#172339 = AXIS2_PLACEMENT_3D ( 'NONE', #233506, #150121, #113537 ) ;
#172340 = DIRECTION ( 'NONE',  ( 1.000000000000000000, -0.000000000000000000, -0.000000000000000000 ) ) ;
#172341 = DIRECTION ( 'NONE',  ( -1.000000000000000000, 0.000000000000000000, 0.000000000000000000 ) ) ;
#172342 = AXIS2_PLACEMENT_3D ( 'NONE', #204774, #242622, #26169 ) ;
#172343 = ORIENTED_EDGE ( 'NONE', *, *, #73923, .T. ) ;
#172345 = ORIENTED_EDGE ( 'NONE', *, *, #60269, .T. ) ;
#172344 = CARTESIAN_POINT ( 'NONE',  ( -23.25000000000000000, 77.83585931145600512, -158.5186683157258187 ) ) ;
#172346 = AXIS2_PLACEMENT_3D ( 'NONE', #93611, #216114, #253949 ) ;
#172348 = DIRECTION ( 'NONE',  ( 0.000000000000000000, -0.1350103645451876944, 0.9908441862701601321 ) ) ;
#172347 = FACE_OUTER_BOUND ( 'NONE', #215733, .T. ) ;
#172350 = ORIENTED_EDGE ( 'NONE', *, *, #214625, .T. ) ;
#172349 = DIRECTION ( 'NONE',  ( 0.000000000000000000, 6.982962677686266711E-15, -1.000000000000000000 ) ) ;
#172351 = AXIS2_PLACEMENT_3D ( 'NONE', #103361, #64261, #61691 ) ;
#172352 = AXIS2_PLACEMENT_3D ( 'NONE', #238424, #257930, #220154 ) ;
#172353 = PRODUCT ( 'Snap Open Cable Crossbars 13', 'Snap Open Cable Crossbars 13', '', ( #71807 ) ) ;
#172354 = VERTEX_POINT ( 'NONE', #236925 ) ;
#172355 = AXIS2_PLACEMENT_3D ( 'NONE', #38921, #81840, #158879 ) ;
#172356 = CARTESIAN_POINT ( 'NONE',  ( 20.94999999999999929, 68.00366762990589109, -224.2307594727497815 ) ) ;
#172357 = CARTESIAN_POINT ( 'NONE',  ( 21.04999999999999716, 67.10527618163416719, -94.53602316137545358 ) ) ;
#172358 = ORIENTED_EDGE ( 'NONE', *, *, #188461, .F. ) ;
#172359 = SPHERICAL_SURFACE ( 'NONE', #30966, 0.1000000000000000056 ) ;
#172360 = ORIENTED_EDGE ( 'NONE', *, *, #226378, .F. ) ;
#172361 = DIRECTION ( 'NONE',  ( 0.000000000000000000, 0.4721928772777345129, 0.8814952561688430555 ) ) ;
#172362 = DIRECTION ( 'NONE',  ( 1.000000000000000000, 0.000000000000000000, 0.000000000000000000 ) ) ;
#172363 = AXIS2_PLACEMENT_3D ( 'NONE', #152629, #16950, #211288 ) ;
#172364 = ORIENTED_EDGE ( 'NONE', *, *, #113359, .F. ) ;
#172365 = DIRECTION ( 'NONE',  ( 0.000000000000000000, -0.9915357197604792727, 0.1298341882520473722 ) ) ;
#172366 = CIRCLE ( 'NONE', #205611, 1.900000000000012790 ) ;
#172367 = EDGE_CURVE ( 'NONE', #5245, #196258, #133966, .T. ) ;
#172368 = CARTESIAN_POINT ( 'NONE',  ( -20.65000000000000568, 7.250000000011138646, -46.15000000000000568 ) ) ;
#172369 = AXIS2_PLACEMENT_3D ( 'NONE', #64588, #45035, #226199 ) ;
#172370 = ORIENTED_EDGE ( 'NONE', *, *, #153929, .F. ) ;
#172371 = ORIENTED_EDGE ( 'NONE', *, *, #205890, .T. ) ;
#172372 = CARTESIAN_POINT ( 'NONE',  ( 20.53930447207944354, 18.80980900407904599, -229.8058790690892010 ) ) ;
#172373 = ORIENTED_EDGE ( 'NONE', *, *, #163812, .F. ) ;
#172374 = DIRECTION ( 'NONE',  ( 1.000000000000000000, 0.000000000000000000, 0.000000000000000000 ) ) ;
#172376 = EDGE_CURVE ( 'NONE', #44715, #221017, #136522, .T. ) ;
#172375 = ORIENTED_EDGE ( 'NONE', *, *, #168149, .T. ) ;
#172378 = ORIENTED_EDGE ( 'NONE', *, *, #29266, .T. ) ;
#172377 = DIRECTION ( 'NONE',  ( 0.000000000000000000, -0.8700118002898359348, 0.4930308989875165082 ) ) ;
#172379 = ORIENTED_EDGE ( 'NONE', *, *, #140521, .F. ) ;
#172380 = ADVANCED_FACE ( 'NONE', ( #74040 ), #115349, .T. ) ;
#172381 = DIRECTION ( 'NONE',  ( 0.000000000000000000, 0.000000000000000000, 1.000000000000000000 ) ) ;
#172382 = ADVANCED_FACE ( 'NONE', ( #16616 ), #256954, .T. ) ;
#172383 = EDGE_LOOP ( 'NONE', ( #49237, #222006, #53394, #171688 ) ) ;
#172386 = VERTEX_POINT ( 'NONE', #14048 ) ;
#172385 = EDGE_LOOP ( 'NONE', ( #113952, #226325, #183930, #13272, #231283, #205450, #22290, #206003, #151842, #215005, #10987 ) ) ;
#172384 = DIRECTION ( 'NONE',  ( 0.7071067811865475727, -0.7071067811865475727, -5.142139384388981164E-15 ) ) ;
#172388 = ORIENTED_EDGE ( 'NONE', *, *, #192555, .F. ) ;
#172387 = CIRCLE ( 'NONE', #59885, 0.1999999999999987899 ) ;
#172389 = AXIS2_PLACEMENT_3D ( 'NONE', #91781, #209148, #30544 ) ;
#172390 = CIRCLE ( 'NONE', #151520, 0.09999999999999939493 ) ;
#172391 = CIRCLE ( 'NONE', #93216, 4.000000000000003553 ) ;
#172392 = DIRECTION ( 'NONE',  ( 2.952720810173289112E-16, -1.000000000000000000, 0.000000000000000000 ) ) ;
#172393 = ORIENTED_EDGE ( 'NONE', *, *, #25148, .T. ) ;
#172394 = ADVANCED_FACE ( 'NONE', ( #173158 ), #123747, .F. ) ;
#172395 = CARTESIAN_POINT ( 'NONE',  ( -16.93860193097148326, 9.993107767340401182, -154.9001383673068801 ) ) ;
#172397 = ORIENTED_EDGE ( 'NONE', *, *, #8599, .T. ) ;
#172396 = DIRECTION ( 'NONE',  ( 1.000000000000000000, 0.000000000000000000, 0.000000000000000000 ) ) ;
#172398 = LINE ( 'NONE', #173691, #208963 ) ;
#172399 = ORIENTED_EDGE ( 'NONE', *, *, #202443, .F. ) ;
#172400 = ORIENTED_EDGE ( 'NONE', *, *, #35913, .F. ) ;
#172401 = DIRECTION ( 'NONE',  ( -1.000000000000000000, 0.000000000000000000, 0.000000000000000000 ) ) ;
#172402 = CARTESIAN_POINT ( 'NONE',  ( 20.12500000000000355, 66.74195072709427734, -61.15976864738194507 ) ) ;
#172403 = VERTEX_POINT ( 'NONE', #97378 ) ;
#172405 = ORIENTED_EDGE ( 'NONE', *, *, #73337, .T. ) ;
#172404 = CARTESIAN_POINT ( 'NONE',  ( 21.05000000000000071, 40.68212387350988735, -238.0221676322813096 ) ) ;
#172406 = CARTESIAN_POINT ( 'NONE',  ( -23.15000000000000213, 11.65000000001115588, -193.9851942293460070 ) ) ;
#172408 = ORIENTED_EDGE ( 'NONE', *, *, #138632, .F. ) ;
#172407 = ORIENTED_EDGE ( 'NONE', *, *, #183283, .T. ) ;
#172409 = AXIS2_PLACEMENT_3D ( 'NONE', #71581, #6440, #85951 ) ;
#172410 = EDGE_LOOP ( 'NONE', ( #252859, #194089, #164678, #19111 ) ) ;
#172411 = DIRECTION ( 'NONE',  ( 1.000000000000000000, 0.000000000000000000, 0.000000000000000000 ) ) ;
#172413 = EDGE_LOOP ( 'NONE', ( #145543, #91311, #191367, #139950 ) ) ;
#172412 = EDGE_CURVE ( 'NONE', #29232, #12856, #44630, .T. ) ;
#172414 = VERTEX_POINT ( 'NONE', #233105 ) ;
#172415 = EDGE_CURVE ( 'NONE', #197986, #36418, #61197, .T. ) ;
#172416 = DIRECTION ( 'NONE',  ( -0.000000000000000000, 0.1350103645451807555, 0.9908441862701610203 ) ) ;
#172417 = EDGE_LOOP ( 'NONE', ( #102168, #195300, #587, #115904 ) ) ;
#172418 = DIRECTION ( 'NONE',  ( 0.000000000000000000, 8.267618268485201230E-15, -1.000000000000000000 ) ) ;
#172419 = DIRECTION ( 'NONE',  ( -3.265361837132813093E-16, 1.000000000000000000, 0.000000000000000000 ) ) ;
#172420 = ORIENTED_EDGE ( 'NONE', *, *, #185625, .F. ) ;
#172422 = ADVANCED_FACE ( 'NONE', ( #114417 ), #156140, .T. ) ;
#172421 = VERTEX_POINT ( 'NONE', #34915 ) ;
#172423 = DIRECTION ( 'NONE',  ( -2.952720810173288619E-16, 1.000000000000000000, 0.000000000000000000 ) ) ;
#172424 = AXIS2_PLACEMENT_3D ( 'NONE', #251840, #108483, #227137 ) ;
#172425 = ORIENTED_EDGE ( 'NONE', *, *, #62259, .T. ) ;
#172426 = AXIS2_PLACEMENT_3D ( 'NONE', #225638, #168314, #47007 ) ;
#172427 = DIRECTION ( 'NONE',  ( 0.000000000000000000, -0.8660254037844411501, -0.4999999999999956701 ) ) ;
#172428 = ORIENTED_EDGE ( 'NONE', *, *, #233841, .T. ) ;
#172429 = VERTEX_POINT ( 'NONE', #111855 ) ;
#172430 = CARTESIAN_POINT ( 'NONE',  ( -20.94999999999999929, 77.36242903720467723, -28.13422623660311217 ) ) ;
#172432 = ORIENTED_EDGE ( 'NONE', *, *, #91685, .T. ) ;
#172431 = CARTESIAN_POINT ( 'NONE',  ( 18.50000000000000000, 85.40000000001231228, -162.7258477248610120 ) ) ;
#172433 = CARTESIAN_POINT ( 'NONE',  ( 23.25000000000000000, -6.688413578037176066, -212.5825622730469036 ) ) ;
#172434 = CARTESIAN_POINT ( 'NONE',  ( 21.30000000000002558, 1.115600667400684642E-11, -167.4999999999999716 ) ) ;
#172435 = DIRECTION ( 'NONE',  ( -1.000000000000000000, 0.000000000000000000, 0.000000000000000000 ) ) ;
#172436 = CARTESIAN_POINT ( 'NONE',  ( -21.05000000000000071, 76.00000000001253397, -181.8231074845243711 ) ) ;
#172437 = DIRECTION ( 'NONE',  ( 1.284434275755705296E-16, -0.7071067811865471286, -0.7071067811865479058 ) ) ;
#172438 = LINE ( 'NONE', #52428, #69184 ) ;
#172439 = DIRECTION ( 'NONE',  ( 0.000000000000000000, 6.982962677686266711E-15, -1.000000000000000000 ) ) ;
#172440 = CARTESIAN_POINT ( 'NONE',  ( -21.14999999999999858, 11.65000000001115588, -140.7838656629781724 ) ) ;
#172441 = CARTESIAN_POINT ( 'NONE',  ( 18.39999999999999858, 38.27493434228539826, -261.1939574891503639 ) ) ;
#172442 = TOROIDAL_SURFACE ( 'NONE', #209819, 2.100000000000002309, 0.1000000000000000056 ) ;
#172443 = CARTESIAN_POINT ( 'NONE',  ( -18.40000000000000213, 33.92901942162173157, -235.0579290632217067 ) ) ;
#172444 = CARTESIAN_POINT ( 'NONE',  ( -23.25000000000000000, -1.835859311443637010, -45.00443916879852679 ) ) ;
#172445 = ORIENTED_EDGE ( 'NONE', *, *, #157210, .T. ) ;
#172446 = VECTOR ( 'NONE', #11293, 1000.000000000000000 ) ;
#172447 = CIRCLE ( 'NONE', #64069, 12.97500000000000320 ) ;
#172448 = EDGE_CURVE ( 'NONE', #174523, #190881, #77355, .T. ) ;
#172450 = ORIENTED_EDGE ( 'NONE', *, *, #6282, .T. ) ;
#172449 = ORIENTED_EDGE ( 'NONE', *, *, #227211, .F. ) ;
#172452 = ORIENTED_EDGE ( 'NONE', *, *, #147724, .T. ) ;
#172451 = EDGE_CURVE ( 'NONE', #217355, #161618, #125642, .T. ) ;
#172453 = DIRECTION ( 'NONE',  ( 0.000000000000000000, 0.000000000000000000, -1.000000000000000000 ) ) ;
#172454 = FACE_OUTER_BOUND ( 'NONE', #38515, .T. ) ;
#172455 = EDGE_CURVE ( 'NONE', #252694, #137777, #157065, .T. ) ;
#172456 = EDGE_CURVE ( 'NONE', #86769, #228950, #79114, .T. ) ;
#172458 = DIRECTION ( 'NONE',  ( -1.000000000000000000, 0.000000000000000000, 0.000000000000000000 ) ) ;
#172457 = PLANE ( 'NONE',  #182628 ) ;
#172459 = ORIENTED_EDGE ( 'NONE', *, *, #167949, .F. ) ;
#172460 = ORIENTED_EDGE ( 'NONE', *, *, #12626, .F. ) ;
#172461 = CIRCLE ( 'NONE', #55668, 0.09999999999999892308 ) ;
#172463 = AXIS2_PLACEMENT_3D ( 'NONE', #161026, #1916, #237969 ) ;
#172462 =( LENGTH_UNIT ( ) NAMED_UNIT ( * ) SI_UNIT ( .MILLI., .METRE. ) );
#172465 = CIRCLE ( 'NONE', #109858, 11.75000000000001066 ) ;
#172464 = CARTESIAN_POINT ( 'NONE',  ( 20.97239005616515328, 67.12515615866146845, -57.27295468237120701 ) ) ;
#172466 = ADVANCED_FACE ( 'NONE', ( #199087 ), #110698, .T. ) ;
#172467 = CARTESIAN_POINT ( 'NONE',  ( -20.05000000000000426, 66.75000000001185185, -90.67310748452436542 ) ) ;
#172469 = EDGE_LOOP ( 'NONE', ( #147840, #149538, #77541, #165957 ) ) ;
#172468 = AXIS2_PLACEMENT_3D ( 'NONE', #103321, #21268, #142457 ) ;
#172470 = ORIENTED_EDGE ( 'NONE', *, *, #153062, .F. ) ;
#172471 = EDGE_CURVE ( 'NONE', #38015, #169538, #102281, .T. ) ;
#172472 = LINE ( 'NONE', #94158, #146604 ) ;
#172474 = EDGE_CURVE ( 'NONE', #208598, #101037, #120865, .T. ) ;
#172473 = EDGE_CURVE ( 'NONE', #229500, #231654, #57065, .T. ) ;
#172475 = CARTESIAN_POINT ( 'NONE',  ( -33.72168855820451938, 9.950000000011156587, -146.6499999999999773 ) ) ;
#172476 = CIRCLE ( 'NONE', #80828, 11.65000000000000391 ) ;
#172477 = DIRECTION ( 'NONE',  ( 1.000000000000000000, -0.000000000000000000, -0.000000000000000000 ) ) ;
#172479 = VERTEX_POINT ( 'NONE', #257713 ) ;
#172478 = LINE ( 'NONE', #192014, #168800 ) ;
#172480 = EDGE_CURVE ( 'NONE', #155936, #97513, #2912, .T. ) ;
#172481 = DIRECTION ( 'NONE',  ( -0.000000000000000000, -0.000000000000000000, -1.000000000000000000 ) ) ;
#172482 = DIRECTION ( 'NONE',  ( 0.7071067811865463515, 0.7071067811865487940, 4.937700262164540154E-15 ) ) ;
#172483 = VECTOR ( 'NONE', #93732, 1000.000000000000000 ) ;
#172484 = CARTESIAN_POINT ( 'NONE',  ( 18.40000000000000568, 85.50000000001192291, -96.02374538734412113 ) ) ;
#172486 = ORIENTED_EDGE ( 'NONE', *, *, #246273, .T. ) ;
#172485 = AXIS2_PLACEMENT_3D ( 'NONE', #246648, #88845, #129285 ) ;
#172487 = CARTESIAN_POINT ( 'NONE',  ( 15.69410316191959254, 66.64325398293360081, -85.81974776316017994 ) ) ;
#172488 = DIRECTION ( 'NONE',  ( 0.000000000000000000, -1.000000000000000000, -7.105427357601001859E-15 ) ) ;
#172489 = DIRECTION ( 'NONE',  ( -0.000000000000000000, 0.000000000000000000, -1.000000000000000000 ) ) ;
#172490 = CIRCLE ( 'NONE', #18316, 3.900000000000000799 ) ;
#172491 = EDGE_CURVE ( 'NONE', #147024, #220397, #190399, .T. ) ;
#172493 = CARTESIAN_POINT ( 'NONE',  ( 18.79999999999999716, 0.000000000000000000, 0.000000000000000000 ) ) ;
#172492 = CARTESIAN_POINT ( 'NONE',  ( -16.87331047859649757, 66.05000000001255955, -182.6731074845244223 ) ) ;
#172494 = CYLINDRICAL_SURFACE ( 'NONE', #62220, 0.1000000000000028644 ) ;
#172495 = DIRECTION ( 'NONE',  ( 0.000000000000000000, -0.1332476588733448597, -0.9910827722268067408 ) ) ;
#172496 = FACE_OUTER_BOUND ( 'NONE', #71422, .T. ) ;
#172497 = CARTESIAN_POINT ( 'NONE',  ( 18.58719872626880942, 85.56664439761105712, -163.2006292881272884 ) ) ;
#172498 = CARTESIAN_POINT ( 'NONE',  ( -21.09610168723073542, 69.62104428478737361, -136.5566969914158051 ) ) ;
#172499 = EDGE_CURVE ( 'NONE', #223845, #109477, #66951, .T. ) ;
#172500 = ADVANCED_FACE ( 'NONE', ( #60844 ), #223668, .T. ) ;
#172501 = EDGE_LOOP ( 'NONE', ( #235523, #190362, #10645, #55775 ) ) ;
#172502 = ORIENTED_EDGE ( 'NONE', *, *, #158908, .T. ) ;
#172503 = EDGE_LOOP ( 'NONE', ( #60402, #92733, #14643, #166578 ) ) ;
#172504 = ADVANCED_FACE ( 'NONE', ( #47371 ), #41324, .F. ) ;
#172505 = DIRECTION ( 'NONE',  ( -1.000000000000000000, 0.000000000000000000, 0.000000000000000000 ) ) ;
#172506 = CARTESIAN_POINT ( 'NONE',  ( -23.49999999999994316, 77.85126707825561709, -47.62635315998165453 ) ) ;
#172507 = ORIENTED_EDGE ( 'NONE', *, *, #248824, .F. ) ;
#172508 = DIRECTION ( 'NONE',  ( -0.000000000000000000, 0.000000000000000000, 1.000000000000000000 ) ) ;
#172509 = EDGE_CURVE ( 'NONE', #176334, #89225, #135630, .T. ) ;
#172510 = ORIENTED_EDGE ( 'NONE', *, *, #148500, .F. ) ;
#172511 = AXIS2_PLACEMENT_3D ( 'NONE', #113740, #132022, #96717 ) ;
#172512 =( LENGTH_UNIT ( ) NAMED_UNIT ( * ) SI_UNIT ( .MILLI., .METRE. ) );
#172513 = ADVANCED_FACE ( 'NONE', ( #85193 ), #65663, .F. ) ;
#172514 = VECTOR ( 'NONE', #137610, 1000.000000000000000 ) ;
#172515 = VERTEX_POINT ( 'NONE', #145193 ) ;
#172516 = AXIS2_PLACEMENT_3D ( 'NONE', #73828, #232897, #133761 ) ;
#172517 = CARTESIAN_POINT ( 'NONE',  ( 21.05000000000000071, 76.08559286337390404, -109.4367702193939351 ) ) ;
#172518 = ORIENTED_EDGE ( 'NONE', *, *, #194129, .T. ) ;
#172519 = CARTESIAN_POINT ( 'NONE',  ( -16.83794479845802172, 30.05980643715662382, -234.7553781105508790 ) ) ;
#172520 = LINE ( 'NONE', #232463, #56852 ) ;
#172521 = CIRCLE ( 'NONE', #14269, 0.1999999999999987899 ) ;
#172522 = CARTESIAN_POINT ( 'NONE',  ( -18.79999999999999716, 4.513204987021263825, 22.10000000000000142 ) ) ;
#172523 = DIRECTION ( 'NONE',  ( 0.000000000000000000, -0.9915357197604971473, 0.1298341882519111479 ) ) ;
#172525 = ORIENTED_EDGE ( 'NONE', *, *, #15667, .F. ) ;
#172524 = CARTESIAN_POINT ( 'NONE',  ( -16.88705144915422096, 29.95864726180315429, -234.6743689137096567 ) ) ;
#172527 = CYLINDRICAL_SURFACE ( 'NONE', #254339, 0.09999999999999939493 ) ;
#172526 = CARTESIAN_POINT ( 'NONE',  ( 21.05000000000000071, 6.164605728109038729, -199.6790125993524043 ) ) ;
#172528 = ADVANCED_FACE ( 'NONE', ( #224728 ), #140271, .F. ) ;
#172529 = CARTESIAN_POINT ( 'NONE',  ( -16.91049119928363709, 9.949999999999985079, -20.88172039319084305 ) ) ;
#172530 = DIRECTION ( 'NONE',  ( 0.000000000000000000, 0.000000000000000000, -1.000000000000000000 ) ) ;
#172531 = VECTOR ( 'NONE', #194992, 1000.000000000000000 ) ;
#172532 = CARTESIAN_POINT ( 'NONE',  ( -16.97683809663753607, 66.05000000001183480, -82.79463665241381420 ) ) ;
#172533 = DIRECTION ( 'NONE',  ( 1.000000000000000000, 0.000000000000000000, 0.000000000000000000 ) ) ;
#172534 = EDGE_LOOP ( 'NONE', ( #108152, #244705, #65010, #209455 ) ) ;
#172535 = AXIS2_PLACEMENT_3D ( 'NONE', #139487, #5090, #224164 ) ;
#172536 = DIRECTION ( 'NONE',  ( -1.000000000000000000, -0.000000000000000000, -0.000000000000000000 ) ) ;
#172537 = CIRCLE ( 'NONE', #93360, 0.09999999999999414912 ) ;
#172538 = ORIENTED_EDGE ( 'NONE', *, *, #254464, .F. ) ;
#172539 = DIRECTION ( 'NONE',  ( 0.000000000000000000, 0.9126074666063770380, 0.4088369013363281068 ) ) ;
#172540 = ORIENTED_EDGE ( 'NONE', *, *, #160963, .F. ) ;
#172541 = TOROIDAL_SURFACE ( 'NONE', #26761, 0.2000000000000000111, 0.1000000000000000056 ) ;
#172542 = CARTESIAN_POINT ( 'NONE',  ( 21.72449340488910607, 65.71604372252076587, -93.77310748452438816 ) ) ;
#172543 = CARTESIAN_POINT ( 'NONE',  ( 21.05000000000000071, 1.115600667400684642E-11, -33.50000000000000000 ) ) ;
#172544 = CARTESIAN_POINT ( 'NONE',  ( -18.59999999999999787, 11.65000000001115232, -174.5148057706539930 ) ) ;
#172545 = VERTEX_POINT ( 'NONE', #225990 ) ;
#172546 = VECTOR ( 'NONE', #140730, 1000.000000000000000 ) ;
#172547 = ORIENTED_EDGE ( 'NONE', *, *, #46742, .F. ) ;
#172548 = CARTESIAN_POINT ( 'NONE',  ( -21.05000000000000071, 69.60000000001230092, -160.0926828544628222 ) ) ;
#172550 = CIRCLE ( 'NONE', #43506, 12.87500000000000178 ) ;
#172549 = CARTESIAN_POINT ( 'NONE',  ( 23.14999999999999858, 1.115600667400684642E-11, -171.5000000000000284 ) ) ;
#172551 = EDGE_CURVE ( 'NONE', #54944, #110818, #94495, .T. ) ;
#172552 = DIRECTION ( 'NONE',  ( -1.000000000000000000, 0.000000000000000000, 0.000000000000000000 ) ) ;
#172553 = DIRECTION ( 'NONE',  ( 1.000000000000000000, 1.875376730785737719E-16, 0.000000000000000000 ) ) ;
#172554 = LINE ( 'NONE', #152974, #150048 ) ;
#172555 = DIRECTION ( 'NONE',  ( 1.186688945009009831E-16, -1.000000000000000000, 0.000000000000000000 ) ) ;
#172556 = ADVANCED_FACE ( 'NONE', ( #167369 ), #58271, .F. ) ;
#172557 = CARTESIAN_POINT ( 'NONE',  ( 21.14999999999999858, 65.28660755661196902, -90.77310748452438816 ) ) ;
#172558 = CARTESIAN_POINT ( 'NONE',  ( -18.50000000000000000, 64.35000000001245724, -170.0231074845244166 ) ) ;
#172559 = ORIENTED_EDGE ( 'NONE', *, *, #18403, .T. ) ;
#172560 = CIRCLE ( 'NONE', #226662, 0.1000000000000028644 ) ;
#172562 = VERTEX_POINT ( 'NONE', #13413 ) ;
#172561 = CARTESIAN_POINT ( 'NONE',  ( -23.25000000000000000, 4.150000000011156764, -79.35000000000005116 ) ) ;
#172563 = VECTOR ( 'NONE', #30470, 1000.000000000000000 ) ;
#172564 = CARTESIAN_POINT ( 'NONE',  ( 17.74533788810829904, 10.81849979148194763, -190.6863773250524048 ) ) ;
#172565 = DIRECTION ( 'NONE',  ( 0.000000000000000000, -0.6728971962617102953, -0.7397360091702507301 ) ) ;
#172567 = CARTESIAN_POINT ( 'NONE',  ( -18.59999999999999787, -0.7124800764063081715, -242.4837965912295772 ) ) ;
#172566 = FACE_OUTER_BOUND ( 'NONE', #38724, .T. ) ;
#172568 = EDGE_CURVE ( 'NONE', #133901, #153430, #194491, .T. ) ;
#172569 = ADVANCED_FACE ( 'NONE', ( #112514 ), #182001, .T. ) ;
#172570 = DIRECTION ( 'NONE',  ( 2.465190328815662439E-32, -0.2617529984165030132, -0.9651348961777158619 ) ) ;
#172572 = EDGE_LOOP ( 'NONE', ( #137647, #105307, #51598, #21095, #62879, #96229, #145063, #175360, #43139 ) ) ;
#172571 = DIRECTION ( 'NONE',  ( 0.000000000000000000, 1.000000000000000000, 1.156482317317864980E-14 ) ) ;
#172573 = DIRECTION ( 'NONE',  ( -0.000000000000000000, -0.000000000000000000, -1.000000000000000000 ) ) ;
#172574 = FACE_OUTER_BOUND ( 'NONE', #170394, .T. ) ;
#172575 = FACE_OUTER_BOUND ( 'NONE', #142491, .T. ) ;
#172576 = DIRECTION ( 'NONE',  ( -0.000000000000000000, 0.000000000000000000, -1.000000000000000000 ) ) ;
#172577 = CARTESIAN_POINT ( 'NONE',  ( 20.85000000000000142, 6.933893972137497030, -137.7856458343736108 ) ) ;
#172578 = ORIENTED_EDGE ( 'NONE', *, *, #220377, .T. ) ;
#172579 = FACE_OUTER_BOUND ( 'NONE', #60487, .T. ) ;
#172580 = EDGE_LOOP ( 'NONE', ( #97975, #217948, #171463, #41268 ) ) ;
#172581 = DIRECTION ( 'NONE',  ( 0.000000000000000000, -0.000000000000000000, 1.000000000000000000 ) ) ;
#172582 = ORIENTED_EDGE ( 'NONE', *, *, #127990, .T. ) ;
#172583 = DIRECTION ( 'NONE',  ( 8.565286242868724116E-15, -0.1575546449569727447, 0.9875102702516478370 ) ) ;
#172584 = CIRCLE ( 'NONE', #118367, 12.87499999999999112 ) ;
#172585 = VECTOR ( 'NONE', #249373, 1000.000000000000000 ) ;
#172586 = ORIENTED_EDGE ( 'NONE', *, *, #202590, .F. ) ;
#172587 = EDGE_CURVE ( 'NONE', #121176, #62147, #128220, .T. ) ;
#172588 = DIRECTION ( 'NONE',  ( 0.000000000000000000, -1.000000000000000000, 0.000000000000000000 ) ) ;
#172589 = DIRECTION ( 'NONE',  ( 0.000000000000000000, 0.2617529984165021806, 0.9651348961777159730 ) ) ;
#172590 = CARTESIAN_POINT ( 'NONE',  ( 21.14999999999999503, 64.35000000001237197, -170.0231074845244166 ) ) ;
#172591 = ORIENTED_EDGE ( 'NONE', *, *, #18668, .F. ) ;
#172592 = CARTESIAN_POINT ( 'NONE',  ( -23.15000000000000213, -11.64999999998884483, -164.4000000000000057 ) ) ;
#172593 = DIRECTION ( 'NONE',  ( -1.000000000000000000, -3.265361837132813093E-16, 0.000000000000000000 ) ) ;
#172594 = CARTESIAN_POINT ( 'NONE',  ( -20.94999999999999929, -1.162701749926853712, -142.1000000000000227 ) ) ;
#172595 = CARTESIAN_POINT ( 'NONE',  ( -21.05000000000000071, 47.95459712139159336, -246.5019368548292675 ) ) ;
#172596 = CARTESIAN_POINT ( 'NONE',  ( -18.59999999999999787, 74.16465844978715438, -57.96795619196135618 ) ) ;
#172598 = EDGE_LOOP ( 'NONE', ( #238925, #234227, #250246, #124259 ) ) ;
#172597 = EDGE_CURVE ( 'NONE', #50827, #256542, #215310, .T. ) ;
#172599 = CARTESIAN_POINT ( 'NONE',  ( -18.52309608778507766, 85.64247632006726008, -129.8085111433545649 ) ) ;
#172600 = VERTEX_POINT ( 'NONE', #190790 ) ;
#172602 = ORIENTED_EDGE ( 'NONE', *, *, #245579, .F. ) ;
#172601 = CARTESIAN_POINT ( 'NONE',  ( 21.04999999999908411, 67.22371710472118878, -90.86519848187187165 ) ) ;
#172603 = ORIENTED_EDGE ( 'NONE', *, *, #3886, .T. ) ;
#172604 = PRESENTATION_LAYER_ASSIGNMENT (  '', '', ( #255886 ) ) ;
#172605 = DIRECTION ( 'NONE',  ( 1.000000000000000000, 2.952720810173289112E-16, -0.000000000000000000 ) ) ;
#172606 = DIRECTION ( 'NONE',  ( 0.000000000000000000, -0.4166553800442105437, 0.9090645160164456673 ) ) ;
#172607 = DIRECTION ( 'NONE',  ( 0.000000000000000000, -1.000000000000000000, 0.000000000000000000 ) ) ;
#172608 = DIRECTION ( 'NONE',  ( 0.000000000000000000, -6.938893903907222067E-15, 1.000000000000000000 ) ) ;
#172609 = EDGE_LOOP ( 'NONE', ( #132291, #133123, #31979, #127009 ) ) ;
#172610 = CARTESIAN_POINT ( 'NONE',  ( -21.05000000000000071, 14.05000000001115623, -139.5136950707610026 ) ) ;
#172611 = DIRECTION ( 'NONE',  ( 0.000000000000000000, -1.000000000000000000, 0.000000000000000000 ) ) ;
#172612 = EDGE_CURVE ( 'NONE', #168680, #93005, #136163, .T. ) ;
#172613 = ORIENTED_EDGE ( 'NONE', *, *, #59113, .T. ) ;
#172615 = VERTEX_POINT ( 'NONE', #68242 ) ;
#172614 = CARTESIAN_POINT ( 'NONE',  ( -16.94878442675511465, 66.00827089702099215, -115.6348879088864976 ) ) ;
#172617 = ADVANCED_FACE ( 'NONE', ( #231189 ), #252325, .F. ) ;
#172616 = CARTESIAN_POINT ( 'NONE',  ( -22.47071067811865319, 36.65892442174472876, -249.5511627012454596 ) ) ;
#172618 = LINE ( 'NONE', #154337, #23238 ) ;
#172620 = VECTOR ( 'NONE', #95025, 999.9999999999998863 ) ;
#172619 = CARTESIAN_POINT ( 'NONE',  ( 21.13461538461538325, 44.29694026544699170, -236.3931290369747842 ) ) ;
#172621 = ORIENTED_EDGE ( 'NONE', *, *, #192225, .T. ) ;
#172622 = VECTOR ( 'NONE', #123488, 1000.000000000000000 ) ;
#172623 = ORIENTED_EDGE ( 'NONE', *, *, #194139, .T. ) ;
#172624 = VECTOR ( 'NONE', #22045, 1000.000000000000000 ) ;
#172626 = DIRECTION ( 'NONE',  ( 1.836970198721029934E-16, 1.000000000000000000, 6.982962677686266711E-15 ) ) ;
#172625 = CIRCLE ( 'NONE', #60120, 0.09999999999999867328 ) ;
#172627 = EDGE_CURVE ( 'NONE', #254024, #111950, #2535, .T. ) ;
#172628 = DIRECTION ( 'NONE',  ( -1.000000000000000000, -0.000000000000000000, -0.000000000000000000 ) ) ;
#172629 = VERTEX_POINT ( 'NONE', #171242 ) ;
#172630 = DIRECTION ( 'NONE',  ( -1.000000000000000000, 0.000000000000000000, -0.000000000000000000 ) ) ;
#172631 = EDGE_CURVE ( 'NONE', #248447, #79198, #106573, .T. ) ;
#172632 = PLANE ( 'NONE',  #193078 ) ;
#172633 = ADVANCED_FACE ( 'NONE', ( #94208 ), #10840, .F. ) ;
#172634 = DIRECTION ( 'NONE',  ( 0.000000000000000000, 0.9229812358755983270, -0.3848449534832869001 ) ) ;
#172635 = AXIS2_PLACEMENT_3D ( 'NONE', #221943, #43347, #6776 ) ;
#172636 = EDGE_CURVE ( 'NONE', #119280, #55681, #25948, .T. ) ;
#172637 = VECTOR ( 'NONE', #100203, 1000.000000000000000 ) ;
#172638 = AXIS2_PLACEMENT_3D ( 'NONE', #108478, #168503, #69370 ) ;
#172639 = VERTEX_POINT ( 'NONE', #18540 ) ;
#172640 = CARTESIAN_POINT ( 'NONE',  ( 20.94999999999999929, 67.07338541492450190, -61.05142446530125966 ) ) ;
#172641 = AXIS2_PLACEMENT_3D ( 'NONE', #64886, #80576, #160176 ) ;
#172642 = AXIS2_PLACEMENT_3D ( 'NONE', #22450, #60259, #104500 ) ;
#172643 = ORIENTED_EDGE ( 'NONE', *, *, #88736, .T. ) ;
#172644 = CARTESIAN_POINT ( 'NONE',  ( 21.00000000000000000, 9.750000000011153745, -112.8500000000000369 ) ) ;
#172646 = EDGE_CURVE ( 'NONE', #11036, #62328, #185719, .T. ) ;
#172645 = CARTESIAN_POINT ( 'NONE',  ( 22.39999999999999503, 11.75000000001115552, -167.3999999999999773 ) ) ;
#172648 = ORIENTED_EDGE ( 'NONE', *, *, #168424, .T. ) ;
#172647 = CARTESIAN_POINT ( 'NONE',  ( -18.59999999999999787, 22.43030315632513094, -231.3223027016406093 ) ) ;
#172649 = CARTESIAN_POINT ( 'NONE',  ( 23.14999999999999503, 60.99662849158838895, -205.1669373764474642 ) ) ;
#172650 = LINE ( 'NONE', #34396, #119982 ) ;
#172651 = CARTESIAN_POINT ( 'NONE',  ( -18.59999999999999787, 77.83585931145546510, -91.41866831572575336 ) ) ;
#172652 = DIRECTION ( 'NONE',  ( 0.000000000000000000, 0.000000000000000000, 1.000000000000000000 ) ) ;
#172653 = CARTESIAN_POINT ( 'NONE',  ( 21.05000000000000071, 6.413978881499668994, -33.58579911627400350 ) ) ;
#172654 = VECTOR ( 'NONE', #198723, 1000.000000000000000 ) ;
#172655 = FACE_OUTER_BOUND ( 'NONE', #122001, .T. ) ;
#172656 = AXIS2_PLACEMENT_3D ( 'NONE', #236045, #216481, #101634 ) ;
#172657 = DIRECTION ( 'NONE',  ( 0.000000000000000000, -1.299197156476247485E-14, 1.000000000000000000 ) ) ;
#172659 = ORIENTED_EDGE ( 'NONE', *, *, #188829, .F. ) ;
#172658 = CARTESIAN_POINT ( 'NONE',  ( -22.49917693094574389, 75.91477003579036875, -114.6729032690549701 ) ) ;
#172660 = AXIS2_PLACEMENT_3D ( 'NONE', #232888, #114194, #29559 ) ;
#172661 = DIRECTION ( 'NONE',  ( -1.000000000000000000, 0.000000000000000000, 0.000000000000000000 ) ) ;
#172662 = AXIS2_PLACEMENT_3D ( 'NONE', #44031, #122287, #81829 ) ;
#172663 = CARTESIAN_POINT ( 'NONE',  ( -18.38817693311004575, 16.37893853458640692, -222.2512945466943108 ) ) ;
#172664 = CARTESIAN_POINT ( 'NONE',  ( 21.14999999999999858, 11.65000000001116298, -88.75000000000004263 ) ) ;
#172665 = TOROIDAL_SURFACE ( 'NONE', #51787, 11.65000000000000036, 0.1000000000000000056 ) ;
#172667 = ORIENTED_EDGE ( 'NONE', *, *, #33000, .F. ) ;
#172666 = AXIS2_PLACEMENT_3D ( 'NONE', #23489, #3889, #224207 ) ;
#172668 = DIRECTION ( 'NONE',  ( 0.000000000000000000, 0.000000000000000000, -1.000000000000000000 ) ) ;
#172669 = CIRCLE ( 'NONE', #192905, 0.1000000000000028644 ) ;
#172670 = DIRECTION ( 'NONE',  ( 1.000000000000000000, 0.000000000000000000, -0.000000000000000000 ) ) ;
#172671 = SPHERICAL_SURFACE ( 'NONE', #40989, 0.1000000000000000056 ) ;
#172672 = ORIENTED_EDGE ( 'NONE', *, *, #75887, .T. ) ;
#172673 = FACE_OUTER_BOUND ( 'NONE', #197475, .T. ) ;
#172674 = CARTESIAN_POINT ( 'NONE',  ( -22.47071067811866385, 59.75442326890419764, -233.9300113800878762 ) ) ;
#172675 = VERTEX_POINT ( 'NONE', #237589 ) ;
#172676 = DIRECTION ( 'NONE',  ( -1.000000000000000000, 0.000000000000000000, -0.000000000000000000 ) ) ;
#172677 = ORIENTED_EDGE ( 'NONE', *, *, #245411, .F. ) ;
#172679 = EDGE_CURVE ( 'NONE', #220385, #22057, #160795, .T. ) ;
#172678 = CARTESIAN_POINT ( 'NONE',  ( 21.04999999999999716, 65.37127968600771055, -124.3731074845243540 ) ) ;
#172681 = EDGE_LOOP ( 'NONE', ( #117367, #98429, #29006, #181252 ) ) ;
#172680 = DIRECTION ( 'NONE',  ( 1.000000000000000000, 0.000000000000000000, 0.000000000000000000 ) ) ;
#172682 = CARTESIAN_POINT ( 'NONE',  ( 18.59999999999999787, -1.835859311432481045, -112.0044391687985694 ) ) ;
#172683 = ORIENTED_EDGE ( 'NONE', *, *, #243784, .F. ) ;
#172684 = VECTOR ( 'NONE', #140820, 1000.000000000000000 ) ;
#172685 = EDGE_CURVE ( 'NONE', #234219, #168502, #198180, .T. ) ;
#172686 = CARTESIAN_POINT ( 'NONE',  ( -0.8999999999999994671, -8.250000000000005329, 30.04142135623731136 ) ) ;
#172687 = ADVANCED_FACE ( 'NONE', ( #98035 ), #176348, .T. ) ;
#172688 = VERTEX_POINT ( 'NONE', #57642 ) ;
#172689 = AXIS2_PLACEMENT_3D ( 'NONE', #18347, #256907, #23522 ) ;
#172691 = ORIENTED_EDGE ( 'NONE', *, *, #143065, .T. ) ;
#172690 = EDGE_LOOP ( 'NONE', ( #202809, #188051, #203099, #56960 ) ) ;
#172693 = VERTEX_POINT ( 'NONE', #17266 ) ;
#172692 = PLANE ( 'NONE',  #118172 ) ;
#172694 = TOROIDAL_SURFACE ( 'NONE', #31223, 11.90000000000000391, 0.1000000000000000056 ) ;
#172695 = CARTESIAN_POINT ( 'NONE',  ( 20.94999027547553894, 65.70673848566956110, -64.06382523348288771 ) ) ;
#172696 = VERTEX_POINT ( 'NONE', #39414 ) ;
#172697 = VECTOR ( 'NONE', #134750, 1000.000000000000000 ) ;
#172698 = VERTEX_POINT ( 'NONE', #253281 ) ;
#172699 = EDGE_CURVE ( 'NONE', #203823, #119804, #189989, .T. ) ;
#172700 = CARTESIAN_POINT ( 'NONE',  ( -20.54999999999999716, 73.60000000001230092, -156.7984855617622770 ) ) ;
#172701 = SPHERICAL_SURFACE ( 'NONE', #63779, 0.1000000000000000056 ) ;
#172702 = CARTESIAN_POINT ( 'NONE',  ( 21.05000000000000071, 70.50000000001158185, -57.11784146561126363 ) ) ;
#172703 = ORIENTED_EDGE ( 'NONE', *, *, #22271, .T. ) ;
#172704 = EDGE_CURVE ( 'NONE', #95681, #254324, #55065, .T. ) ;
#172705 = CARTESIAN_POINT ( 'NONE',  ( 18.39999999999999503, 64.52683809664958403, -123.8731074845243683 ) ) ;
#172706 = DIRECTION ( 'NONE',  ( -1.000000000000000000, 0.000000000000000000, 0.000000000000000000 ) ) ;
#172707 = DIRECTION ( 'NONE',  ( 0.000000000000000000, -6.982962677686266711E-15, 1.000000000000000000 ) ) ;
#172708 = AXIS2_PLACEMENT_3D ( 'NONE', #128466, #185865, #149337 ) ;
#172709 = VERTEX_POINT ( 'NONE', #137194 ) ;
#172710 = DIRECTION ( 'NONE',  ( 0.000000000000000000, 0.9998779222360096863, -0.01562500000001061998 ) ) ;
#172711 = AXIS2_PLACEMENT_3D ( 'NONE', #197238, #177712, #90735 ) ;
#172712 = DIRECTION ( 'NONE',  ( 0.000000000000000000, 1.000000000000000000, 0.000000000000000000 ) ) ;
#172713 = FILL_AREA_STYLE_COLOUR ( '', #236409 ) ;
#172714 = VERTEX_POINT ( 'NONE', #198451 ) ;
#172715 = CARTESIAN_POINT ( 'NONE',  ( 18.59999999999999076, 6.400000000000003020, -9.930424630061574831 ) ) ;
#172716 = ORIENTED_EDGE ( 'NONE', *, *, #103501, .T. ) ;
#172717 = CARTESIAN_POINT ( 'NONE',  ( -18.46093223321777899, -7.755933848802606612, -209.9397816339188125 ) ) ;
#172718 = ORIENTED_EDGE ( 'NONE', *, *, #19353, .T. ) ;
#172719 = DIRECTION ( 'NONE',  ( 1.000000000000000000, 1.541880601228652843E-16, 2.878400969107353907E-16 ) ) ;
#172720 = EDGE_CURVE ( 'NONE', #112369, #156851, #202462, .T. ) ;
#172721 = ORIENTED_EDGE ( 'NONE', *, *, #37632, .F. ) ;
#172722 = VERTEX_POINT ( 'NONE', #15997 ) ;
#172723 = CARTESIAN_POINT ( 'NONE',  ( -22.49231231312463208, 11.37015642645466684, -198.4612171126308624 ) ) ;
#172724 = EDGE_CURVE ( 'NONE', #21983, #156407, #156703, .T. ) ;
#172725 = FACE_OUTER_BOUND ( 'NONE', #205454, .T. ) ;
#172726 = EDGE_LOOP ( 'NONE', ( #106927, #15207, #121817, #81525 ) ) ;
#172727 = ADVANCED_FACE ( 'NONE', ( #173817 ), #233746, .F. ) ;
#172728 = ORIENTED_EDGE ( 'NONE', *, *, #154474, .F. ) ;
#172729 = FACE_OUTER_BOUND ( 'NONE', #248026, .T. ) ;
#172730 = ORIENTED_EDGE ( 'NONE', *, *, #132175, .T. ) ;
#172731 = AXIS2_PLACEMENT_3D ( 'NONE', #224655, #241660, #3031 ) ;
#172732 = EDGE_CURVE ( 'NONE', #57247, #11158, #134605, .T. ) ;
#172734 = ORIENTED_EDGE ( 'NONE', *, *, #150642, .T. ) ;
#172733 = CIRCLE ( 'NONE', #135254, 0.1000000000000028644 ) ;
#172735 = VECTOR ( 'NONE', #178177, 1000.000000000000000 ) ;
#172736 = VECTOR ( 'NONE', #220652, 1000.000000000000000 ) ;
#172737 = DIRECTION ( 'NONE',  ( -0.000000000000000000, -0.000000000000000000, -1.000000000000000000 ) ) ;
#172738 = CARTESIAN_POINT ( 'NONE',  ( -21.05000000000000071, 76.00000000001170974, -69.52310748452431710 ) ) ;
#172739 = CARTESIAN_POINT ( 'NONE',  ( -16.89268316805466341, 9.951721813253341153, -46.14424752145445296 ) ) ;
#172741 = ORIENTED_EDGE ( 'NONE', *, *, #1400, .F. ) ;
#172740 = DIRECTION ( 'NONE',  ( 1.000000000000000000, 0.000000000000000000, 0.000000000000000000 ) ) ;
#172742 = FACE_OUTER_BOUND ( 'NONE', #62999, .T. ) ;
#172743 = DIRECTION ( 'NONE',  ( 1.000000000000000000, 0.000000000000000000, 0.000000000000000000 ) ) ;
#172745 = EDGE_CURVE ( 'NONE', #116862, #57200, #35560, .T. ) ;
#172744 = CARTESIAN_POINT ( 'NONE',  ( 21.05000000000000071, 76.00000000001155342, -56.54810748452432279 ) ) ;
#172747 = DIRECTION ( 'NONE',  ( 0.000000000000000000, 1.000000000000000000, -1.224646799147353207E-16 ) ) ;
#172746 = CARTESIAN_POINT ( 'NONE',  ( 18.59999999999999787, -8.175168544775697654, 10.42878401658402510 ) ) ;
#172748 = DIRECTION ( 'NONE',  ( -1.000000000000000000, 0.000000000000000000, 0.000000000000000000 ) ) ;
#172749 = DIRECTION ( 'NONE',  ( 0.000000000000000000, -6.240597636138643358E-14, -1.000000000000000000 ) ) ;
#172750 = DIRECTION ( 'NONE',  ( 0.000000000000000000, 1.000000000000000000, 0.000000000000000000 ) ) ;
#172751 = DIRECTION ( 'NONE',  ( 0.000000000000000000, -1.000000000000000000, -6.982962677686265922E-15 ) ) ;
#172752 = AXIS2_PLACEMENT_3D ( 'NONE', #163118, #223062, #182679 ) ;
#172753 = ORIENTED_EDGE ( 'NONE', *, *, #57374, .T. ) ;
#172754 = EDGE_CURVE ( 'NONE', #224952, #14895, #219969, .T. ) ;
#172755 =( BOUNDED_SURFACE ( )  B_SPLINE_SURFACE ( 3, 2, ( 
 ( #96047, #115629, #196437 ),
 ( #17793, #54364, #37394 ),
 ( #178195, #175618, #19087 ),
 ( #99877, #154783, #76487 ) ),
 .UNSPECIFIED., .F., .F., .F. ) 
 B_SPLINE_SURFACE_WITH_KNOTS ( ( 4, 4 ),
 ( 3, 3 ),
 ( 0.04058434257139457990, 0.04256401539001584966 ),
 ( 0.000000000000000000, 1.000000000000000000 ),
 .UNSPECIFIED. ) 
 GEOMETRIC_REPRESENTATION_ITEM ( )  RATIONAL_B_SPLINE_SURFACE ( (
 ( 1.000000000000000000, 0.7103081912008166743, 1.000000000000000000),
 ( 1.000000000000000000, 0.7104998333555226919, 1.000000000000000000),
 ( 1.000000000000000000, 0.7107238315754937918, 1.000000000000000000),
 ( 1.000000000000000000, 0.7110073749539386201, 1.000000000000000000) ) ) 
 REPRESENTATION_ITEM ( '' )  SURFACE ( )  );
#172756 = ORIENTED_EDGE ( 'NONE', *, *, #79345, .F. ) ;
#172757 = B_SPLINE_CURVE_WITH_KNOTS ( 'NONE', 3,
 ( #241926, #24190, #26770, #145394 ),
 .UNSPECIFIED., .F., .F.,
 ( 4, 4 ),
 ( 0.000000000000000000, 7.713889350929220882E-05 ),
 .UNSPECIFIED. ) ;
#172758 = CARTESIAN_POINT ( 'NONE',  ( 20.94999999999999574, 4.252251777740766236, -211.8999245327126744 ) ) ;
#172759 = EDGE_CURVE ( 'NONE', #130702, #105736, #77525, .T. ) ;
#172760 = EDGE_CURVE ( 'NONE', #111770, #218845, #172142, .T. ) ;
#172761 = DIRECTION ( 'NONE',  ( -0.000000000000000000, -0.000000000000000000, 1.000000000000000000 ) ) ;
#172762 = EDGE_LOOP ( 'NONE', ( #24674, #254230, #125669, #180244 ) ) ;
#172763 = DIRECTION ( 'NONE',  ( 0.000000000000000000, 1.000000000000000000, 0.000000000000000000 ) ) ;
#172764 = DIRECTION ( 'NONE',  ( 1.000000000000000000, 0.000000000000000000, 0.000000000000000000 ) ) ;
#172765 = ORIENTED_EDGE ( 'NONE', *, *, #70372, .F. ) ;
#172766 = EDGE_LOOP ( 'NONE', ( #109449, #105198, #73347, #246406 ) ) ;
#172767 = EDGE_CURVE ( 'NONE', #6746, #166854, #155140, .T. ) ;
#172769 = CARTESIAN_POINT ( 'NONE',  ( -18.59999999999999787, 66.75000000001223555, -148.7731074845244166 ) ) ;
#172768 = VECTOR ( 'NONE', #113919, 1000.000000000000000 ) ;
#172770 = PRESENTATION_LAYER_ASSIGNMENT (  '', '', ( #218487 ) ) ;
#172771 = CARTESIAN_POINT ( 'NONE',  ( -23.15000000000000213, 87.65000000001269598, -203.5231074845243029 ) ) ;
#172772 = EDGE_CURVE ( 'NONE', #75809, #55862, #6645, .T. ) ;
#172773 = FACE_OUTER_BOUND ( 'NONE', #175123, .T. ) ;
#172775 = ORIENTED_EDGE ( 'NONE', *, *, #26808, .F. ) ;
#172774 = CARTESIAN_POINT ( 'NONE',  ( 17.23472005113827166, 10.30788195451192379, -89.04657686006872552 ) ) ;
#172776 = DIRECTION ( 'NONE',  ( -1.000000000000000000, 1.646408749285562691E-14, 1.149681084847720908E-28 ) ) ;
#172778 = ORIENTED_EDGE ( 'NONE', *, *, #25351, .T. ) ;
#172777 = LINE ( 'NONE', #208026, #102119 ) ;
#172779 = DIRECTION ( 'NONE',  ( -1.836970198721029934E-16, 1.000000000000000000, 0.000000000000000000 ) ) ;
#172780 = CYLINDRICAL_SURFACE ( 'NONE', #245619, 0.1000000000000124678 ) ;
#172781 = DIRECTION ( 'NONE',  ( -1.000000000000000000, -0.000000000000000000, -0.000000000000000000 ) ) ;
#172782 = DIRECTION ( 'NONE',  ( 0.000000000000000000, 0.000000000000000000, -1.000000000000000000 ) ) ;
#172783 = EDGE_CURVE ( 'NONE', #13860, #146959, #31620, .T. ) ;
#172785 = CARTESIAN_POINT ( 'NONE',  ( 20.44999100639894962, 10.43971070322319683, -108.2590757259705612 ) ) ;
#172784 = DIRECTION ( 'NONE',  ( -0.000000000000000000, -1.000000000000000000, 6.308085367188393199E-16 ) ) ;
#172786 = DIRECTION ( 'NONE',  ( 0.000000000000000000, -0.1686199900910312910, 0.9856811345164826488 ) ) ;
#172787 = VECTOR ( 'NONE', #17726, 1000.000000000000000 ) ;
#172788 = CARTESIAN_POINT ( 'NONE',  ( -19.99999999999999645, 11.61130914238355771, 16.50000000000000000 ) ) ;
#172789 = CARTESIAN_POINT ( 'NONE',  ( 18.49999999999998934, 6.550000000011156231, -121.6500000000000341 ) ) ;
#172790 = CARTESIAN_POINT ( 'NONE',  ( -23.15000000000000213, 1.115600667400684642E-11, -67.00000000000000000 ) ) ;
#172791 = DIRECTION ( 'NONE',  ( 0.000000000000000000, 0.000000000000000000, 1.000000000000000000 ) ) ;
#172792 = ADVANCED_FACE ( 'NONE', ( #173441 ), #127445, .T. ) ;
#172793 = AXIS2_PLACEMENT_3D ( 'NONE', #153257, #211926, #32013 ) ;
#172794 = VERTEX_POINT ( 'NONE', #252910 ) ;
#172795 = TOROIDAL_SURFACE ( 'NONE', #255903, 6.258578643762700899, 0.1000000000000000056 ) ;
#172796 = CARTESIAN_POINT ( 'NONE',  ( -16.87036670365549540, 9.989418819312804843, -79.52043988269798547 ) ) ;
#172797 = ORIENTED_EDGE ( 'NONE', *, *, #250955, .F. ) ;
#172798 = ORIENTED_EDGE ( 'NONE', *, *, #170377, .F. ) ;
#172799 = EDGE_CURVE ( 'NONE', #92855, #49052, #153875, .T. ) ;
#172800 = CARTESIAN_POINT ( 'NONE',  ( 20.94999999999999929, 51.66758181523423588, -231.0768342483179083 ) ) ;
#172801 = DIRECTION ( 'NONE',  ( 1.000000000000000000, -0.000000000000000000, -0.000000000000000000 ) ) ;
#172802 = ADVANCED_FACE ( 'NONE', ( #36469 ), #229513, .T. ) ;
#172803 = VERTEX_POINT ( 'NONE', #190401 ) ;
#172804 = CARTESIAN_POINT ( 'NONE',  ( 20.85000000000000142, 87.65000000001170122, -69.52310748452423184 ) ) ;
#172805 =( NAMED_UNIT ( * ) PLANE_ANGLE_UNIT ( ) SI_UNIT ( $, .RADIAN. ) );
#172806 = EDGE_CURVE ( 'NONE', #18434, #94251, #64892, .T. ) ;
#172807 = AXIS2_PLACEMENT_3D ( 'NONE', #183630, #47949, #67521 ) ;
#172808 = ORIENTED_EDGE ( 'NONE', *, *, #196909, .F. ) ;
#172809 = VECTOR ( 'NONE', #211127, 1000.000000000000000 ) ;
#172810 = EDGE_LOOP ( 'NONE', ( #4572, #95013, #6620, #29529 ) ) ;
#172811 = AXIS2_PLACEMENT_3D ( 'NONE', #243876, #80939, #105629 ) ;
#172812 = FACE_OUTER_BOUND ( 'NONE', #24316, .T. ) ;
#172813 = CARTESIAN_POINT ( 'NONE',  ( 21.05000000000000071, 10.68429367439828859, -41.02667393863730183 ) ) ;
#172814 = CARTESIAN_POINT ( 'NONE',  ( 20.73486653747088582, 7.250000000000026645, -12.65000000000000568 ) ) ;
#172815 = AXIS2_PLACEMENT_3D ( 'NONE', #118674, #160377, #179927 ) ;
#172816 = CARTESIAN_POINT ( 'NONE',  ( 12.60873083341397027, 27.26868795068922680, -233.8692014934036081 ) ) ;
#172817 = DIRECTION ( 'NONE',  ( 0.000000000000000000, 6.982962677686266711E-15, -1.000000000000000000 ) ) ;
#172819 = DIRECTION ( 'NONE',  ( 1.000000000000000000, 0.000000000000000000, -0.000000000000000000 ) ) ;
#172818 = CARTESIAN_POINT ( 'NONE',  ( 21.05000000000000071, 5.000000000011153745, -79.40526601891313874 ) ) ;
#172820 = CARTESIAN_POINT ( 'NONE',  ( -14.23072895065543264, 9.455987233623899257, -82.01153116689789613 ) ) ;
#172822 = VERTEX_POINT ( 'NONE', #35196 ) ;
#172821 = DIRECTION ( 'NONE',  ( -1.000000000000000000, 0.000000000000000000, 0.000000000000000000 ) ) ;
#172824 = DIRECTION ( 'NONE',  ( -2.952720810173289112E-16, 1.000000000000000000, 0.000000000000000000 ) ) ;
#172823 = CARTESIAN_POINT ( 'NONE',  ( -22.60000000000080789, 0.04781698046536793367, 11.75002243115275036 ) ) ;
#172825 = ADVANCED_FACE ( 'NONE', ( #131689 ), #234637, .T. ) ;
#172826 = CARTESIAN_POINT ( 'NONE',  ( -21.05000000000000071, 36.65892442174472876, -249.5511627012454596 ) ) ;
#172827 =( BOUNDED_SURFACE ( )  B_SPLINE_SURFACE ( 3, 2, ( 
 ( #141497, #16447, #236737 ),
 ( #235457, #56796, #101036 ),
 ( #257537, #60664, #140195 ),
 ( #136334, #97192, #217168 ) ),
 .UNSPECIFIED., .F., .F., .F. ) 
 B_SPLINE_SURFACE_WITH_KNOTS ( ( 4, 4 ),
 ( 3, 3 ),
 ( -5.204170427930421283E-18, 0.001979672783031571903 ),
 ( 0.000000000000000000, 1.000000000000000000 ),
 .UNSPECIFIED. ) 
 GEOMETRIC_REPRESENTATION_ITEM ( )  RATIONAL_B_SPLINE_SURFACE ( (
 ( 1.000000000000000000, 0.7103081912007942478, 1.000000000000000000),
 ( 1.000000000000000000, 0.7104998333557805967, 1.000000000000000000),
 ( 1.000000000000000000, 0.7107238315756059244, 1.000000000000000000),
 ( 1.000000000000000000, 0.7110073749539113086, 1.000000000000000000) ) ) 
 REPRESENTATION_ITEM ( '' )  SURFACE ( )  );
#172828 = EDGE_CURVE ( 'NONE', #159529, #104826, #113410, .T. ) ;
#172829 = ORIENTED_EDGE ( 'NONE', *, *, #66209, .F. ) ;
#172830 = CYLINDRICAL_SURFACE ( 'NONE', #158850, 11.80000000000000426 ) ;
#172831 = AXIS2_PLACEMENT_3D ( 'NONE', #51295, #128309, #110009 ) ;
#172832 = PLANE ( 'NONE',  #39685 ) ;
#172833 = DIRECTION ( 'NONE',  ( 1.000000000000000000, 0.000000000000000000, 0.000000000000000000 ) ) ;
#172834 = CIRCLE ( 'NONE', #185260, 0.09999999999999939493 ) ;
#172835 = ORIENTED_EDGE ( 'NONE', *, *, #126075, .F. ) ;
#172836 = VECTOR ( 'NONE', #134725, 1000.000000000000000 ) ;
#172837 = CARTESIAN_POINT ( 'NONE',  ( -18.40000000000000213, 5.650000000011139001, -154.8500000000000227 ) ) ;
#172838 = VECTOR ( 'NONE', #62771, 999.9999999999998863 ) ;
#172839 = CARTESIAN_POINT ( 'NONE',  ( -21.64999999999999858, 7.250000000011148416, -112.7500000000000284 ) ) ;
#172840 = CARTESIAN_POINT ( 'NONE',  ( -21.05000000000000071, 1.115600667400684642E-11, -134.0000000000000284 ) ) ;
#172841 = ORIENTED_EDGE ( 'NONE', *, *, #163327, .T. ) ;
#172842 = ORIENTED_EDGE ( 'NONE', *, *, #163168, .T. ) ;
#172843 = CIRCLE ( 'NONE', #76924, 0.3999999999999979683 ) ;
#172844 = CARTESIAN_POINT ( 'NONE',  ( 22.40000000000020819, 64.25313205997866817, -247.2214437328679537 ) ) ;
#172845 = CIRCLE ( 'NONE', #68744, 4.300000000000032685 ) ;
#172846 = CARTESIAN_POINT ( 'NONE',  ( -18.58222699835055280, 10.33200063080771969, -173.0931674956643178 ) ) ;
#172847 = CARTESIAN_POINT ( 'NONE',  ( -18.50000000000000000, 74.36282728704223643, -191.9409541190523498 ) ) ;
#172848 = CARTESIAN_POINT ( 'NONE',  ( -16.27683809663750480, 66.65000000001255387, -182.5731074845244279 ) ) ;
#172849 = ORIENTED_EDGE ( 'NONE', *, *, #63600, .F. ) ;
#172850 = CIRCLE ( 'NONE', #35467, 0.09999999999999939493 ) ;
#172851 = AXIS2_PLACEMENT_3D ( 'NONE', #66116, #86932, #169108 ) ;
#172852 = DIRECTION ( 'NONE',  ( 0.000000000000000000, 0.8814952561688438326, -0.4721928772777330696 ) ) ;
#172853 = DIRECTION ( 'NONE',  ( 0.000000000000000000, 0.9947597004326491632, -0.1022405907413782566 ) ) ;
#172854 = DIRECTION ( 'NONE',  ( 0.000000000000000000, 0.8814952561688437216, -0.4721928772777334582 ) ) ;
#172855 = FACE_OUTER_BOUND ( 'NONE', #143207, .T. ) ;
#172856 = EDGE_CURVE ( 'NONE', #254732, #98712, #75592, .T. ) ;
#172857 = DIRECTION ( 'NONE',  ( 1.000000000000000000, 0.000000000000000000, 0.000000000000000000 ) ) ;
#172858 =( BOUNDED_SURFACE ( )  B_SPLINE_SURFACE ( 3, 2, ( 
 ( #126174, #203156, #84444 ),
 ( #167919, #64922, #207015 ),
 ( #165320, #244841, #87035 ),
 ( #162769, #246144, #147020 ),
 ( #66222, #204429, #23271 ),
 ( #45368, #63644, #67493 ) ),
 .UNSPECIFIED., .F., .F., .F. ) 
 B_SPLINE_SURFACE_WITH_KNOTS ( ( 4, 2, 4 ),
 ( 3, 3 ),
 ( 0.0001300404313046710908, 0.0003183318589266637198, 0.0005066232865486563217 ),
 ( 0.000000000000000000, 1.000000000000000000 ),
 .UNSPECIFIED. ) 
 GEOMETRIC_REPRESENTATION_ITEM ( )  RATIONAL_B_SPLINE_SURFACE ( (
 ( 1.000000000000000000, 0.7071067811865475727, 1.000000000000000000),
 ( 1.000000000000000000, 0.7625113560541042501, 1.000000000000000000),
 ( 1.000000000000000000, 0.8126073484687571513, 1.000000000000000000),
 ( 1.000000000000000000, 0.8923049332733655747, 1.000000000000000000),
 ( 1.000000000000000000, 0.9231914937768425089, 1.000000000000000000),
 ( 1.000000000000000000, 0.9238795325112945100, 1.000000000000000000) ) ) 
 REPRESENTATION_ITEM ( '' )  SURFACE ( )  );
#172860 = ORIENTED_EDGE ( 'NONE', *, *, #196890, .T. ) ;
#172859 = CARTESIAN_POINT ( 'NONE',  ( -16.94445028196807002, 66.00793639031407167, -82.13043766294282477 ) ) ;
#172861 = CARTESIAN_POINT ( 'NONE',  ( 19.97071067811864609, 11.72071067812981404, -54.85000000000000142 ) ) ;
#172862 = DIRECTION ( 'NONE',  ( 0.000000000000000000, 0.4721928772777351790, 0.8814952561688427224 ) ) ;
#172863 = DIRECTION ( 'NONE',  ( 0.000000000000000000, -0.2128009952263602567, 0.9770955615653315052 ) ) ;
#172864 = FACE_OUTER_BOUND ( 'NONE', #94062, .T. ) ;
#172865 = CARTESIAN_POINT ( 'NONE',  ( -23.15000000000000213, 14.08768503992705057, -210.4690089352671123 ) ) ;
#172867 = ORIENTED_EDGE ( 'NONE', *, *, #162695, .T. ) ;
#172866 = CARTESIAN_POINT ( 'NONE',  ( -21.44999999999999929, 21.39776787615277343, -233.0380739262505472 ) ) ;
#172868 = CARTESIAN_POINT ( 'NONE',  ( -23.49999999999994316, 76.00000000001119815, -36.02310748452479316 ) ) ;
#172869 = CARTESIAN_POINT ( 'NONE',  ( -18.40000000000000213, 11.48667500175766953, -9.250000000000001776 ) ) ;
#172870 = ORIENTED_EDGE ( 'NONE', *, *, #197557, .T. ) ;
#172871 = DIRECTION ( 'NONE',  ( -1.000000000000000000, 0.000000000000000000, 0.000000000000000000 ) ) ;
#172872 = AXIS2_PLACEMENT_3D ( 'NONE', #62253, #182208, #24436 ) ;
#172873 = CARTESIAN_POINT ( 'NONE',  ( -18.59999999999999787, 80.78317333349157536, -192.9003134612048882 ) ) ;
#172874 = DIRECTION ( 'NONE',  ( 0.000000000000000000, 0.8814952561688476074, -0.4721928772777262417 ) ) ;
#172876 = CIRCLE ( 'NONE', #255968, 0.1000000000000106498 ) ;
#172875 = LINE ( 'NONE', #17586, #4565 ) ;
#172877 = EDGE_CURVE ( 'NONE', #60863, #51379, #210649, .T. ) ;
#172878 = CIRCLE ( 'NONE', #2116, 12.87499999999999822 ) ;
#172879 = DIRECTION ( 'NONE',  ( 0.000000000000000000, 0.000000000000000000, 1.000000000000000000 ) ) ;
#172880 = DIRECTION ( 'NONE',  ( 0.000000000000000000, 1.000000000000000000, 0.000000000000000000 ) ) ;
#172881 = ORIENTED_EDGE ( 'NONE', *, *, #38029, .T. ) ;
#172882 = ORIENTED_EDGE ( 'NONE', *, *, #183936, .F. ) ;
#172883 = VECTOR ( 'NONE', #121657, 1000.000000000000000 ) ;
#172884 = DIRECTION ( 'NONE',  ( 0.000000000000000000, -1.000000000000000000, -7.272083257015735086E-15 ) ) ;
#172885 = AXIS2_PLACEMENT_3D ( 'NONE', #31982, #209301, #57601 ) ;
#172886 = CARTESIAN_POINT ( 'NONE',  ( -16.92209698673680052, 66.05000000001201954, -115.7337430515765533 ) ) ;
#172887 = DIRECTION ( 'NONE',  ( -1.000000000000000000, -1.652117596168391700E-15, -1.153667551319263085E-29 ) ) ;
#172888 = DIRECTION ( 'NONE',  ( 1.000000000000000000, -0.000000000000000000, -0.000000000000000000 ) ) ;
#172890 = CIRCLE ( 'NONE', #206166, 4.000000000000003553 ) ;
#172889 = DIRECTION ( 'NONE',  ( -1.000000000000000000, 0.000000000000000000, 0.000000000000000000 ) ) ;
#172891 = DIRECTION ( 'NONE',  ( -0.000000000000000000, 0.9126074666063772600, 0.4088369013363276072 ) ) ;
#172892 = AXIS2_PLACEMENT_3D ( 'NONE', #125178, #204685, #165596 ) ;
#172893 = CARTESIAN_POINT ( 'NONE',  ( -21.04999999999994387, 77.16254490893143725, -43.92310748452479885 ) ) ;
#172895 = CIRCLE ( 'NONE', #139522, 0.1000000000000028644 ) ;
#172894 = DIRECTION ( 'NONE',  ( 1.000000000000000000, 0.000000000000000000, 0.000000000000000000 ) ) ;
#172896 = ORIENTED_EDGE ( 'NONE', *, *, #114845, .T. ) ;
#172897 = LINE ( 'NONE', #133713, #190297 ) ;
#172898 = VERTEX_POINT ( 'NONE', #170875 ) ;
#172899 = LINE ( 'NONE', #30799, #5429 ) ;
#172900 = CARTESIAN_POINT ( 'NONE',  ( 20.95512820512820085, 10.62384868371188062, -7.664913569087606682 ) ) ;
#172903 = ORIENTED_EDGE ( 'NONE', *, *, #69103, .T. ) ;
#172902 = AXIS2_PLACEMENT_3D ( 'NONE', #117368, #255534, #236022 ) ;
#172901 = DIRECTION ( 'NONE',  ( 0.000000000000000000, 0.2128009952263600624, -0.9770955615653316162 ) ) ;
#172904 = CARTESIAN_POINT ( 'NONE',  ( -22.50485643085238863, -3.265757507883099375, -228.2539816168355742 ) ) ;
#172905 = CARTESIAN_POINT ( 'NONE',  ( -20.54999999999999716, 87.75000000001180922, -81.87310748452422615 ) ) ;
#172906 = DIRECTION ( 'NONE',  ( -0.000000000000000000, 0.8814952561688430555, -0.4721928772777346239 ) ) ;
#172907 = DIRECTION ( 'NONE',  ( 0.000000000000000000, -0.9126074666063764829, -0.4088369013363293281 ) ) ;
#172908 = EDGE_LOOP ( 'NONE', ( #85793, #170031, #16649, #135074 ) ) ;
#172909 = CARTESIAN_POINT ( 'NONE',  ( 20.94999999999999929, 64.35000000001218723, -143.3069731475025037 ) ) ;
#172910 = CARTESIAN_POINT ( 'NONE',  ( -18.50000000000000000, 11.65000000001115232, -112.6500000000000341 ) ) ;
#172912 = EDGE_CURVE ( 'NONE', #204996, #118577, #15035, .T. ) ;
#172911 = DIRECTION ( 'NONE',  ( 1.284434275755705296E-16, -0.7071067811865471286, 0.7071067811865479058 ) ) ;
#172913 = FACE_OUTER_BOUND ( 'NONE', #196178, .T. ) ;
#172914 = CARTESIAN_POINT ( 'NONE',  ( 18.59999999999997655, 76.00000000001126921, -203.5231074845248997 ) ) ;
#172915 = AXIS2_PLACEMENT_3D ( 'NONE', #43773, #244530, #145428 ) ;
#172916 = CIRCLE ( 'NONE', #77190, 7.900000000000003908 ) ;
#172917 = ORIENTED_EDGE ( 'NONE', *, *, #169834, .T. ) ;
#172918 = DIRECTION ( 'NONE',  ( 1.000000000000000000, 0.000000000000000000, 0.000000000000000000 ) ) ;
#172920 = EDGE_CURVE ( 'NONE', #102643, #204472, #152422, .T. ) ;
#172919 = CYLINDRICAL_SURFACE ( 'NONE', #62886, 0.1000000000000028644 ) ;
#172921 = ORIENTED_EDGE ( 'NONE', *, *, #58101, .F. ) ;
#172922 = ORIENTED_EDGE ( 'NONE', *, *, #2659, .T. ) ;
#172924 = ADVANCED_FACE ( 'NONE', ( #194261 ), #92547, .T. ) ;
#172923 = CARTESIAN_POINT ( 'NONE',  ( -18.59999999999999787, 66.75000000001199396, -115.2731074845243597 ) ) ;
#172925 = CARTESIAN_POINT ( 'NONE',  ( 20.94999999999999929, 1.115624548013267999E-11, -165.6000000000000227 ) ) ;
#172926 = ORIENTED_EDGE ( 'NONE', *, *, #178984, .T. ) ;
#172927 = DIRECTION ( 'NONE',  ( 0.000000000000000000, 0.000000000000000000, 1.000000000000000000 ) ) ;
#172928 = CARTESIAN_POINT ( 'NONE',  ( -16.97683810757273193, 9.950000000011137047, -147.2635767124612869 ) ) ;
#172929 = EDGE_CURVE ( 'NONE', #59708, #222143, #211226, .T. ) ;
#172930 = ORIENTED_EDGE ( 'NONE', *, *, #241327, .F. ) ;
#172931 = AXIS2_PLACEMENT_3D ( 'NONE', #33257, #129751, #151910 ) ;
#172932 = CIRCLE ( 'NONE', #185369, 4.000000000000003553 ) ;
#172933 = VERTEX_POINT ( 'NONE', #73036 ) ;
#172934 = DIRECTION ( 'NONE',  ( 1.000000000000000000, 0.000000000000000000, 0.000000000000000000 ) ) ;
#172936 = ADVANCED_FACE ( 'NONE', ( #53436 ), #132989, .F. ) ;
#172935 = DIRECTION ( 'NONE',  ( 1.000000000000000000, 0.000000000000000000, 0.000000000000000000 ) ) ;
#172938 = ORIENTED_EDGE ( 'NONE', *, *, #74709, .F. ) ;
#172937 = DIRECTION ( 'NONE',  ( 1.000000000000000000, 0.000000000000000000, 0.000000000000000000 ) ) ;
#172940 = CARTESIAN_POINT ( 'NONE',  ( -23.15000000000000213, 4.350000000011156054, -54.85000000000000142 ) ) ;
#172939 = UNCERTAINTY_MEASURE_WITH_UNIT (LENGTH_MEASURE( 1.000000000000000082E-05 ), #26815, 'distance_accuracy_value', 'NONE');
#172941 = DIRECTION ( 'NONE',  ( -3.265361837132813586E-16, 1.000000000000000000, 0.000000000000000000 ) ) ;
#172942 = CARTESIAN_POINT ( 'NONE',  ( -18.40000000000000213, 11.48667500176882328, -76.25000000000004263 ) ) ;
#172943 = CARTESIAN_POINT ( 'NONE',  ( -18.50000000000000000, 64.35000000001205933, -124.3731074845243825 ) ) ;
#172944 = FACE_OUTER_BOUND ( 'NONE', #153519, .T. ) ;
#172945 = DIRECTION ( 'NONE',  ( 1.000000000000000000, 0.000000000000000000, 0.000000000000000000 ) ) ;
#172947 = ORIENTED_EDGE ( 'NONE', *, *, #234518, .T. ) ;
#172946 = CARTESIAN_POINT ( 'NONE',  ( 23.14999999999999858, 73.90000000001244018, -170.0231074845243882 ) ) ;
#172948 = VERTEX_POINT ( 'NONE', #196782 ) ;
#172950 = CARTESIAN_POINT ( 'NONE',  ( -16.87401514999233498, 51.55499682964786246, -231.9750802427320764 ) ) ;
#172949 = DIRECTION ( 'NONE',  ( 2.952720810173289112E-16, 1.000000000000000000, 6.982962677686266711E-15 ) ) ;
#172952 = ORIENTED_EDGE ( 'NONE', *, *, #241800, .T. ) ;
#172951 = FACE_OUTER_BOUND ( 'NONE', #44418, .T. ) ;
#172953 = ORIENTED_EDGE ( 'NONE', *, *, #32660, .F. ) ;
#172954 = CARTESIAN_POINT ( 'NONE',  ( -21.53699400387654350, 1.145497594121937190, -230.5275921506975294 ) ) ;
#172955 = DIRECTION ( 'NONE',  ( 0.000000000000000000, -1.000000000000000000, 0.000000000000000000 ) ) ;
#172956 = TOROIDAL_SURFACE ( 'NONE', #231371, 12.97499999999999787, 0.1000000000000000056 ) ;
#172957 = TOROIDAL_SURFACE ( 'NONE', #98045, 11.90000000000000391, 0.1000000000000000056 ) ;
#172958 = CARTESIAN_POINT ( 'NONE',  ( -22.39999999999999503, 7.790779598384560245, -33.39999999999999858 ) ) ;
#172959 = CARTESIAN_POINT ( 'NONE',  ( 19.80993210785492309, 11.75000000001021228, -58.26711774888664053 ) ) ;
#172960 = DIRECTION ( 'NONE',  ( 0.000000000000000000, -1.000000000000000000, -0.000000000000000000 ) ) ;
#172961 = CARTESIAN_POINT ( 'NONE',  ( 20.94999999999999574, 48.05114133249968944, -246.4758750954581785 ) ) ;
#172962 = LINE ( 'NONE', #33451, #185458 ) ;
#172963 = EDGE_LOOP ( 'NONE', ( #78508, #70154, #51900, #13275 ) ) ;
#172964 = ORIENTED_EDGE ( 'NONE', *, *, #199435, .T. ) ;
#172965 = SPHERICAL_SURFACE ( 'NONE', #244016, 0.1000000000000000056 ) ;
#172966 = AXIS2_PLACEMENT_3D ( 'NONE', #83482, #23589, #6542 ) ;
#172967 = AXIS2_PLACEMENT_3D ( 'NONE', #228085, #12905, #168147 ) ;
#172968 = ORIENTED_EDGE ( 'NONE', *, *, #241128, .T. ) ;
#172969 = FACE_OUTER_BOUND ( 'NONE', #99213, .T. ) ;
#172970 = EDGE_LOOP ( 'NONE', ( #17550, #230536, #43653, #209194 ) ) ;
#172971 = DIRECTION ( 'NONE',  ( -0.000000000000000000, -0.000000000000000000, 1.000000000000000000 ) ) ;
#172972 = AXIS2_PLACEMENT_3D ( 'NONE', #153901, #174744, #95157 ) ;
#172973 = EDGE_CURVE ( 'NONE', #254080, #175526, #15109, .T. ) ;
#172974 = CARTESIAN_POINT ( 'NONE',  ( -23.15000000000000213, 4.350000000011156054, -121.8500000000000369 ) ) ;
#172975 = CARTESIAN_POINT ( 'NONE',  ( -23.25000000000000000, 19.73066058418984170, -238.2142830767208466 ) ) ;
#172976 = VERTEX_POINT ( 'NONE', #2423 ) ;
#172978 = EDGE_CURVE ( 'NONE', #166638, #194720, #136811, .T. ) ;
#172977 = DIRECTION ( 'NONE',  ( 0.000000000000000000, 0.000000000000000000, 1.000000000000000000 ) ) ;
#172979 = EDGE_LOOP ( 'NONE', ( #238474, #125968, #60336, #190593 ) ) ;
#172980 = CARTESIAN_POINT ( 'NONE',  ( 18.59999999999999787, 72.02722222756958104, -225.1832529173024398 ) ) ;
#172981 = CARTESIAN_POINT ( 'NONE',  ( 18.54147908293618130, 8.873963602870817979, -245.4029850331302498 ) ) ;
#172982 = EDGE_CURVE ( 'NONE', #162643, #125420, #37746, .T. ) ;
#172983 = EDGE_CURVE ( 'NONE', #113, #155129, #257996, .T. ) ;
#172984 = ORIENTED_EDGE ( 'NONE', *, *, #186013, .F. ) ;
#172985 = DIRECTION ( 'NONE',  ( -1.000000000000000000, 0.000000000000000000, 0.000000000000000000 ) ) ;
#172986 = VERTEX_POINT ( 'NONE', #141947 ) ;
#172989 = ORIENTED_EDGE ( 'NONE', *, *, #59876, .T. ) ;
#172988 = FACE_OUTER_BOUND ( 'NONE', #36235, .T. ) ;
#172987 = DIRECTION ( 'NONE',  ( 0.7071067811865475727, -0.7071067811865475727, 0.000000000000000000 ) ) ;
#172990 = B_SPLINE_CURVE_WITH_KNOTS ( 'NONE', 3,
 ( #41300, #135215, #157405, #136493, #140353, #60813, #219903, #36152, #235604, #236897 ),
 .UNSPECIFIED., .F., .F.,
 ( 4, 3, 3, 4 ),
 ( 1.887726692324194669E-15, 3.877043166999659889E-05, 7.336897548475921900E-05, 7.659383120240320164E-05 ),
 .UNSPECIFIED. ) ;
#172991 = CARTESIAN_POINT ( 'NONE',  ( -21.04999999999999716, -0.08574093702224486191, -27.08617371118702977 ) ) ;
#172993 = VERTEX_POINT ( 'NONE', #22023 ) ;
#172992 = VECTOR ( 'NONE', #123578, 1000.000000000000000 ) ;
#172994 = VECTOR ( 'NONE', #233335, 1000.000000000000000 ) ;
#172995 = VERTEX_POINT ( 'NONE', #160266 ) ;
#172996 = VECTOR ( 'NONE', #46485, 1000.000000000000000 ) ;
#172998 = EDGE_CURVE ( 'NONE', #231078, #84586, #110889, .T. ) ;
#172997 = CARTESIAN_POINT ( 'NONE',  ( -21.05000000000000071, -2.576841150532142244, -189.6381168072880428 ) ) ;
#172999 = EDGE_LOOP ( 'NONE', ( #216380, #179486, #88087, #70998 ) ) ;
#173000 = EDGE_CURVE ( 'NONE', #24899, #113044, #39996, .T. ) ;
#173001 = DIRECTION ( 'NONE',  ( 1.000000000000000000, 0.000000000000000000, 0.000000000000000000 ) ) ;
#173002 = CARTESIAN_POINT ( 'NONE',  ( 22.48508240969612615, 64.13718632996433655, -247.0868454141091490 ) ) ;
#173003 = CARTESIAN_POINT ( 'NONE',  ( -23.15000000000000213, 73.50000000001205080, -123.2984855617622202 ) ) ;
#173004 = CARTESIAN_POINT ( 'NONE',  ( -21.14999999999999858, 76.00000000001195133, -103.0231074845243171 ) ) ;
#173005 = AXIS2_PLACEMENT_3D ( 'NONE', #223225, #104542, #60302 ) ;
#173006 = EDGE_CURVE ( 'NONE', #79058, #38302, #241075, .T. ) ;
#173007 = CIRCLE ( 'NONE', #114707, 0.5000000000000004441 ) ;
#173008 = CIRCLE ( 'NONE', #81349, 0.1999999999999987899 ) ;
#173009 = CARTESIAN_POINT ( 'NONE',  ( 18.59999999999999076, 5.950000000011100632, -43.80570230503486329 ) ) ;
#173010 = ORIENTED_EDGE ( 'NONE', *, *, #161338, .T. ) ;
#173011 = CARTESIAN_POINT ( 'NONE',  ( -20.94999999999999929, 48.05114133249968944, -246.4758750954581785 ) ) ;
#173012 = CARTESIAN_POINT ( 'NONE',  ( -20.96077737575320654, 64.37609936600745186, -109.8823155274178163 ) ) ;
#173013 = CARTESIAN_POINT ( 'NONE',  ( -20.94999999999999929, 11.63687328911532859, -160.6782407866750475 ) ) ;
#173014 = VERTEX_POINT ( 'NONE', #239779 ) ;
#173015 = CARTESIAN_POINT ( 'NONE',  ( -23.15000000000000213, 11.65000000001115588, -112.6500000000000341 ) ) ;
#173016 = VERTEX_POINT ( 'NONE', #81942 ) ;
#173017 = DIRECTION ( 'NONE',  ( 0.000000000000000000, -0.2128009952263604232, 0.9770955615653316162 ) ) ;
#173018 = VERTEX_POINT ( 'NONE', #220220 ) ;
#173019 = AXIS2_PLACEMENT_3D ( 'NONE', #81524, #22896, #102368 ) ;
#173020 = AXIS2_PLACEMENT_3D ( 'NONE', #2986, #139924, #81230 ) ;
#173021 = SPHERICAL_SURFACE ( 'NONE', #155945, 0.1000000000000000056 ) ;
#173022 = CARTESIAN_POINT ( 'NONE',  ( -18.59999999999999787, 64.25000000001277556, -215.2731074845244450 ) ) ;
#173023 = EDGE_CURVE ( 'NONE', #16177, #111684, #178678, .T. ) ;
#173025 = ORIENTED_EDGE ( 'NONE', *, *, #238300, .T. ) ;
#173024 = DIRECTION ( 'NONE',  ( 1.000000000000000000, -0.000000000000000000, -0.000000000000000000 ) ) ;
#173026 = EDGE_CURVE ( 'NONE', #41250, #86050, #148490, .T. ) ;
#173027 = DIRECTION ( 'NONE',  ( -1.000000000000000000, -0.000000000000000000, -0.000000000000000000 ) ) ;
#173028 = ORIENTED_EDGE ( 'NONE', *, *, #32553, .F. ) ;
#173029 = EDGE_CURVE ( 'NONE', #233085, #52293, #177263, .T. ) ;
#173030 = VECTOR ( 'NONE', #182166, 1000.000000000000000 ) ;
#173031 = DIRECTION ( 'NONE',  ( 0.000000000000000000, 0.000000000000000000, 1.000000000000000000 ) ) ;
#173032 = CARTESIAN_POINT ( 'NONE',  ( -16.87333278164142314, 9.882609784590052016, -113.6331678061527128 ) ) ;
#173033 = VERTEX_POINT ( 'NONE', #255432 ) ;
#173034 = DIRECTION ( 'NONE',  ( 0.000000000000000000, -0.3896596508880098009, -0.9209589331071360574 ) ) ;
#173035 = VERTEX_POINT ( 'NONE', #61131 ) ;
#173036 = CARTESIAN_POINT ( 'NONE',  ( -16.93583594267724379, 10.00862343506335961, -146.5593908393207982 ) ) ;
#173037 = EDGE_LOOP ( 'NONE', ( #27796, #82233, #45617, #254941, #177013 ) ) ;
#173038 = CARTESIAN_POINT ( 'NONE',  ( 12.26145404764308644, 9.351413679112543065, -117.4803435675489993 ) ) ;
#173039 = CARTESIAN_POINT ( 'NONE',  ( 18.59999999999999432, 1.162701749949165642, -41.60000000000000142 ) ) ;
#173040 = EDGE_CURVE ( 'NONE', #59053, #55818, #102649, .T. ) ;
#173041 = EDGE_CURVE ( 'NONE', #233644, #11074, #40174, .T. ) ;
#173043 = ORIENTED_EDGE ( 'NONE', *, *, #143168, .T. ) ;
#173042 = DIRECTION ( 'NONE',  ( 0.000000000000000000, 0.000000000000000000, -1.000000000000000000 ) ) ;
#173044 = AXIS2_PLACEMENT_3D ( 'NONE', #236100, #157903, #216536 ) ;
#173045 = CARTESIAN_POINT ( 'NONE',  ( -21.05000000000000071, -1.162701749926853712, -41.50000000000000000 ) ) ;
#173046 = CARTESIAN_POINT ( 'NONE',  ( -22.50000000000000000, 0.09263750062063520752, -155.8503027929592122 ) ) ;
#173047 = VECTOR ( 'NONE', #94372, 1000.000000000000000 ) ;
#173049 = ADVANCED_FACE ( 'NONE', ( #119850 ), #169374, .F. ) ;
#173048 = CARTESIAN_POINT ( 'NONE',  ( -16.93433913041102912, 10.00597842152393824, -20.93536542739516548 ) ) ;
#173051 = DIRECTION ( 'NONE',  ( 0.000000000000000000, -1.000000000000000000, 0.000000000000000000 ) ) ;
#173050 = CARTESIAN_POINT ( 'NONE',  ( 21.05000000000000071, 5.000000000011153745, -188.9947339810868812 ) ) ;
#173052 = TOROIDAL_SURFACE ( 'NONE', #60567, 2.100000000000002309, 0.1000000000000000056 ) ;
#173053 = FACE_OUTER_BOUND ( 'NONE', #172572, .T. ) ;
#173054 = DIRECTION ( 'NONE',  ( 0.000000000000000000, 0.000000000000000000, 1.000000000000000000 ) ) ;
#173055 = DIRECTION ( 'NONE',  ( 0.000000000000000000, 0.9126074666063771490, 0.4088369013363281623 ) ) ;
#173056 = ORIENTED_EDGE ( 'NONE', *, *, #224938, .T. ) ;
#173058 = ORIENTED_EDGE ( 'NONE', *, *, #54708, .F. ) ;
#173057 = CIRCLE ( 'NONE', #131497, 4.000000000000003553 ) ;
#173059 = CARTESIAN_POINT ( 'NONE',  ( -23.25000000000000000, 36.65892442174935439, -249.5511627012433848 ) ) ;
#173060 = AXIS2_PLACEMENT_3D ( 'NONE', #133017, #230844, #114727 ) ;
#173062 = ORIENTED_EDGE ( 'NONE', *, *, #57309, .T. ) ;
#173061 = CARTESIAN_POINT ( 'NONE',  ( -18.59999999999999787, 77.16412189325360771, -162.3082593989527425 ) ) ;
#173063 = ORIENTED_EDGE ( 'NONE', *, *, #77195, .T. ) ;
#173064 = CARTESIAN_POINT ( 'NONE',  ( -20.85000000000000142, 87.65000000001144542, -38.92310748452424463 ) ) ;
#173065 = VERTEX_POINT ( 'NONE', #238485 ) ;
#173066 = CARTESIAN_POINT ( 'NONE',  ( 20.95512820512820440, 43.40368376489742275, -234.8883907171572787 ) ) ;
#173067 = AXIS2_PLACEMENT_3D ( 'NONE', #99544, #457, #56562 ) ;
#173068 = AXIS2_PLACEMENT_3D ( 'NONE', #143240, #124982, #155477 ) ;
#173069 = ADVANCED_FACE ( 'NONE', ( #179816 ), #235960, .T. ) ;
#173070 = ORIENTED_EDGE ( 'NONE', *, *, #7509, .F. ) ;
#173071 = AXIS2_PLACEMENT_3D ( 'NONE', #201988, #186285, #122460 ) ;
#173072 =( NAMED_UNIT ( * ) SI_UNIT ( $, .STERADIAN. ) SOLID_ANGLE_UNIT ( ) );
#173074 = EDGE_CURVE ( 'NONE', #222383, #7645, #177560, .T. ) ;
#173073 = DIRECTION ( 'NONE',  ( 0.000000000000000000, 0.000000000000000000, -1.000000000000000000 ) ) ;
#173076 = ORIENTED_EDGE ( 'NONE', *, *, #253432, .F. ) ;
#173075 = ORIENTED_EDGE ( 'NONE', *, *, #242793, .T. ) ;
#173077 = ORIENTED_EDGE ( 'NONE', *, *, #134582, .T. ) ;
#173078 = ORIENTED_EDGE ( 'NONE', *, *, #134286, .F. ) ;
#173079 = ORIENTED_EDGE ( 'NONE', *, *, #158867, .F. ) ;
#173080 = EDGE_CURVE ( 'NONE', #5885, #221119, #27714, .T. ) ;
#173081 = CARTESIAN_POINT ( 'NONE',  ( -21.55000000000000426, 7.750000000000003553, -21.15000000000000213 ) ) ;
#173082 = CARTESIAN_POINT ( 'NONE',  ( 21.12769345151713196, 43.45362607442633873, -234.7614388166508093 ) ) ;
#173083 = CARTESIAN_POINT ( 'NONE',  ( -15.31895204843005232, 9.396533993965075382, -185.4059397791733090 ) ) ;
#173086 = EDGE_CURVE ( 'NONE', #135164, #247253, #6276, .T. ) ;
#173085 = ORIENTED_EDGE ( 'NONE', *, *, #212065, .F. ) ;
#173084 = FACE_OUTER_BOUND ( 'NONE', #34972, .T. ) ;
#173087 = CIRCLE ( 'NONE', #223101, 0.1999999999999987899 ) ;
#173088 = DIRECTION ( 'NONE',  ( 0.000000000000000000, -0.000000000000000000, -1.000000000000000000 ) ) ;
#173089 = CARTESIAN_POINT ( 'NONE',  ( 21.00023020733438273, 6.390869245278871347, -167.4999999999999432 ) ) ;
#173091 = ORIENTED_EDGE ( 'NONE', *, *, #138796, .F. ) ;
#173090 = CARTESIAN_POINT ( 'NONE',  ( -21.98333005346336932, 0.000000000000000000, 7.374075329056680950 ) ) ;
#173092 = CYLINDRICAL_SURFACE ( 'NONE', #212528, 0.09999999999999939493 ) ;
#173093 = VERTEX_POINT ( 'NONE', #165378 ) ;
#173094 = ADVANCED_FACE ( 'NONE', ( #68854 ), #7580, .F. ) ;
#173095 = DIRECTION ( 'NONE',  ( -3.265361837132813093E-16, 1.000000000000000000, 0.000000000000000000 ) ) ;
#173096 = ORIENTED_EDGE ( 'NONE', *, *, #248160, .F. ) ;
#173097 = DIRECTION ( 'NONE',  ( 1.000000000000000000, 0.000000000000000000, 0.000000000000000000 ) ) ;
#173098 = CARTESIAN_POINT ( 'NONE',  ( 21.14999999999999858, 69.74218538953603286, -136.6208977758331287 ) ) ;
#173099 = ORIENTED_EDGE ( 'NONE', *, *, #172195, .T. ) ;
#173101 = CARTESIAN_POINT ( 'NONE',  ( 18.59999999999999787, 77.73670573947921980, -58.00568489690056850 ) ) ;
#173100 = CARTESIAN_POINT ( 'NONE',  ( -18.40000000000000213, 67.23581240663841641, -214.2531594801197627 ) ) ;
#173102 = DIRECTION ( 'NONE',  ( -1.000000000000000000, 0.000000000000000000, 0.000000000000000000 ) ) ;
#173103 = ADVANCED_FACE ( 'NONE', ( #44146 ), #148375, .T. ) ;
#173104 = CARTESIAN_POINT ( 'NONE',  ( 21.72449340488910252, 65.71604372252147641, -190.8731074845244393 ) ) ;
#173105 = CIRCLE ( 'NONE', #60607, 0.1000000000000028644 ) ;
#173106 = DIRECTION ( 'NONE',  ( -0.000000000000000000, -1.000000000000000000, 6.308085367188393199E-16 ) ) ;
#173107 = ADVANCED_FACE ( 'NONE', ( #123685 ), #13589, .T. ) ;
#173108 = ORIENTED_EDGE ( 'NONE', *, *, #22513, .T. ) ;
#173109 = EDGE_LOOP ( 'NONE', ( #191347, #138185, #153509, #55288 ) ) ;
#173110 = CARTESIAN_POINT ( 'NONE',  ( -21.09096482362077651, 0.03944827878506227542, -127.6364556345950518 ) ) ;
#173111 = CARTESIAN_POINT ( 'NONE',  ( 23.14999999999999503, 64.35000000001254250, -182.2731074845244450 ) ) ;
#173112 = ORIENTED_EDGE ( 'NONE', *, *, #64866, .T. ) ;
#173113 = CARTESIAN_POINT ( 'NONE',  ( 20.94999999999999929, 10.38178547073510316, -173.0078453638842007 ) ) ;
#173114 = EDGE_LOOP ( 'NONE', ( #98934, #108422, #218862, #99880 ) ) ;
#173115 = EDGE_CURVE ( 'NONE', #135659, #172263, #35496, .T. ) ;
#173116 = DIRECTION ( 'NONE',  ( -0.000000000000000000, -0.4791956752371546169, -0.8777080977375152360 ) ) ;
#173117 = CARTESIAN_POINT ( 'NONE',  ( 21.03670563405603033, 60.20313529934050223, -221.1782316337949794 ) ) ;
#173118 = CARTESIAN_POINT ( 'NONE',  ( -20.64999999999999858, 1.115600667400684642E-11, -54.12500000000000711 ) ) ;
#173119 = ORIENTED_EDGE ( 'NONE', *, *, #83640, .T. ) ;
#173120 = DIRECTION ( 'NONE',  ( 0.000000000000000000, 0.000000000000000000, -1.000000000000000000 ) ) ;
#173121 =( NAMED_UNIT ( * ) PLANE_ANGLE_UNIT ( ) SI_UNIT ( $, .RADIAN. ) );
#173122 = ADVANCED_FACE ( 'NONE', ( #212215 ), #113099, .T. ) ;
#173123 = AXIS2_PLACEMENT_3D ( 'NONE', #125592, #180437, #184279 ) ;
#173124 = ORIENTED_EDGE ( 'NONE', *, *, #29263, .T. ) ;
#173125 = ORIENTED_EDGE ( 'NONE', *, *, #169525, .F. ) ;
#173126 = EDGE_LOOP ( 'NONE', ( #247707, #77624, #253819, #55798 ) ) ;
#173127 = EDGE_CURVE ( 'NONE', #128036, #134983, #53119, .T. ) ;
#173128 = CARTESIAN_POINT ( 'NONE',  ( -21.05000000000000071, 74.75000000001207923, -128.5231074845243029 ) ) ;
#173129 = DIRECTION ( 'NONE',  ( 0.000000000000000000, -6.853228547068871147E-15, 1.000000000000000000 ) ) ;
#173130 = AXIS2_PLACEMENT_3D ( 'NONE', #171614, #72497, #174191 ) ;
#173131 = CARTESIAN_POINT ( 'NONE',  ( -23.15000000000000213, 69.16514130714681130, -247.7543978865853660 ) ) ;
#173132 = CARTESIAN_POINT ( 'NONE',  ( -21.05000000000000071, 5.900000000011102586, -43.71909976465641989 ) ) ;
#173133 = CARTESIAN_POINT ( 'NONE',  ( 12.84435279558020149, 66.58929125296495499, -118.4538990786802941 ) ) ;
#173135 = CARTESIAN_POINT ( 'NONE',  ( -23.25000000000000000, -0.8831241301779060304, -196.9450534195053706 ) ) ;
#173134 = CARTESIAN_POINT ( 'NONE',  ( -20.54999999999999716, 1.115600667400684642E-11, -67.00000000000000000 ) ) ;
#173136 = ADVANCED_FACE ( 'NONE', ( #133932 ), #250039, .F. ) ;
#173138 = ORIENTED_EDGE ( 'NONE', *, *, #61425, .T. ) ;
#173137 = CARTESIAN_POINT ( 'NONE',  ( 23.14999999999999858, 76.00000000001213607, -136.5231074845243313 ) ) ;
#173139 = LINE ( 'NONE', #252609, #12592 ) ;
#173140 = ORIENTED_EDGE ( 'NONE', *, *, #235401, .T. ) ;
#173141 = CARTESIAN_POINT ( 'NONE',  ( -12.47155713865591764, 9.375669526436929857, -149.8677900093859705 ) ) ;
#173142 = ADVANCED_FACE ( 'NONE', ( #153560 ), #111824, .F. ) ;
#173143 = ORIENTED_EDGE ( 'NONE', *, *, #222511, .F. ) ;
#173144 = ORIENTED_EDGE ( 'NONE', *, *, #193337, .T. ) ;
#173145 = FACE_OUTER_BOUND ( 'NONE', #100481, .T. ) ;
#173146 = CARTESIAN_POINT ( 'NONE',  ( -16.93583594267724024, 10.00862343506335783, -46.05939083932076272 ) ) ;
#173147 = DIRECTION ( 'NONE',  ( -3.265361837132813093E-16, 1.000000000000000000, -0.000000000000000000 ) ) ;
#173148 = DIRECTION ( 'NONE',  ( 0.7071067811864846231, 0.2890913453341779626, -0.6453109281989296564 ) ) ;
#173149 = AXIS2_PLACEMENT_3D ( 'NONE', #160840, #176552, #155718 ) ;
#173150 = CIRCLE ( 'NONE', #155980, 12.87499999999999822 ) ;
#173151 = CARTESIAN_POINT ( 'NONE',  ( 18.49999999999999289, 6.650000000011155876, -155.1500000000000057 ) ) ;
#173152 = ORIENTED_EDGE ( 'NONE', *, *, #44573, .T. ) ;
#173153 = VERTEX_POINT ( 'NONE', #191382 ) ;
#173154 = CARTESIAN_POINT ( 'NONE',  ( -20.54999999999999716, 2.400000000011155432, -154.2753780772379173 ) ) ;
#173156 = EDGE_CURVE ( 'NONE', #45997, #207660, #244135, .T. ) ;
#173155 = VERTEX_POINT ( 'NONE', #12741 ) ;
#173157 = DIRECTION ( 'NONE',  ( 0.000000000000000000, 0.6728388485993083146, -0.7397890806274158848 ) ) ;
#173158 = FACE_OUTER_BOUND ( 'NONE', #173706, .T. ) ;
#173159 = ORIENTED_EDGE ( 'NONE', *, *, #84131, .T. ) ;
#173160 = CARTESIAN_POINT ( 'NONE',  ( 23.15000000000000213, -11.48912529306489994, -130.9000000000000341 ) ) ;
#173161 = DIRECTION ( 'NONE',  ( 0.000000000000000000, 0.2128009952263485993, -0.9770955615653341697 ) ) ;
#173162 = CARTESIAN_POINT ( 'NONE',  ( -22.48660254037843487, 64.35000000001166143, -69.57310748452438531 ) ) ;
#173163 = DIRECTION ( 'NONE',  ( 1.000000000000000000, 0.000000000000000000, 0.000000000000000000 ) ) ;
#173164 = VERTEX_POINT ( 'NONE', #192642 ) ;
#173165 = LINE ( 'NONE', #17875, #237698 ) ;
#173166 = CYLINDRICAL_SURFACE ( 'NONE', #228884, 0.09999999999999939493 ) ;
#173167 = CIRCLE ( 'NONE', #244012, 0.09999999999999538425 ) ;
#173168 = CARTESIAN_POINT ( 'NONE',  ( -21.00219873199061738, 57.83991513803482576, -226.1457439616172849 ) ) ;
#173169 = TOROIDAL_SURFACE ( 'NONE', #68905, 7.800000000000000711, 0.1000000000000000056 ) ;
#173170 = TOROIDAL_SURFACE ( 'NONE', #148163, 0.4000000000000017431, 0.1000000000000000056 ) ;
#173171 = CIRCLE ( 'NONE', #73197, 0.1000000000000000472 ) ;
#173172 = ORIENTED_EDGE ( 'NONE', *, *, #78356, .F. ) ;
#173173 = PRESENTATION_LAYER_ASSIGNMENT (  '', '', ( #23306 ) ) ;
#173175 = EDGE_CURVE ( 'NONE', #140050, #185475, #110521, .T. ) ;
#173174 = DIRECTION ( 'NONE',  ( 0.000000000000000000, -1.000000000000000000, 0.000000000000000000 ) ) ;
#173176 = EDGE_LOOP ( 'NONE', ( #29174, #122277, #166691, #244497 ) ) ;
#173177 = CARTESIAN_POINT ( 'NONE',  ( 15.15590539855245922, 66.58931770574432107, -154.5919640425761941 ) ) ;
#173178 = CARTESIAN_POINT ( 'NONE',  ( -16.93353400591625757, 14.22995845551265681, -219.3242416127272065 ) ) ;
#173179 = CARTESIAN_POINT ( 'NONE',  ( -18.59999999999999787, 11.65000000001115232, -179.6499999999999773 ) ) ;
#173180 = CARTESIAN_POINT ( 'NONE',  ( 21.05000000000000071, 77.84908441863888129, -91.36709696307717365 ) ) ;
#173181 = CARTESIAN_POINT ( 'NONE',  ( -20.54999999999999716, 1.115600667400684642E-11, -134.0000000000000284 ) ) ;
#173182 = DIRECTION ( 'NONE',  ( 1.000000000000000000, 0.000000000000000000, 0.000000000000000000 ) ) ;
#173183 = VERTEX_POINT ( 'NONE', #170561 ) ;
#173184 = CARTESIAN_POINT ( 'NONE',  ( -23.25000000000000355, 10.05000000001113847, -146.7500000000000284 ) ) ;
#173185 = CARTESIAN_POINT ( 'NONE',  ( 20.94999999999999929, 48.40874555430183790, -244.2873875965402704 ) ) ;
#173186 = DIRECTION ( 'NONE',  ( 1.020425574104004196E-15, 6.982962677686266711E-15, -1.000000000000000000 ) ) ;
#173187 = DIRECTION ( 'NONE',  ( 1.000000000000000000, 0.000000000000000000, 0.000000000000000000 ) ) ;
#173188 = EDGE_CURVE ( 'NONE', #168456, #201338, #127641, .T. ) ;
#173189 = CIRCLE ( 'NONE', #43947, 0.9000000000000014655 ) ;
#173190 = CARTESIAN_POINT ( 'NONE',  ( 20.94999999999999574, 74.16465844978745281, -91.46795619196133487 ) ) ;
#173191 =( BOUNDED_SURFACE ( )  B_SPLINE_SURFACE ( 3, 2, ( 
 ( #121796, #20123, #235296 ),
 ( #120525, #38393, #176639 ),
 ( #159627, #37131, #77485 ),
 ( #175365, #39704, #99614 ) ),
 .UNSPECIFIED., .F., .F., .T. ) 
 B_SPLINE_SURFACE_WITH_KNOTS ( ( 4, 4 ),
 ( 3, 3 ),
 ( 0.000000000000000000, 0.001979672783031562362 ),
 ( 0.000000000000000000, 1.000000000000000000 ),
 .UNSPECIFIED. ) 
 GEOMETRIC_REPRESENTATION_ITEM ( )  RATIONAL_B_SPLINE_SURFACE ( (
 ( 1.000000000000000000, 0.7103081912008196719, 1.000000000000000000),
 ( 1.000000000000000000, 0.7104998333558700807, 1.000000000000000000),
 ( 1.000000000000000000, 0.7107238315755209923, 1.000000000000000000),
 ( 1.000000000000000000, 0.7110073749539376209, 1.000000000000000000) ) ) 
 REPRESENTATION_ITEM ( '' )  SURFACE ( )  );
#173192 = AXIS2_PLACEMENT_3D ( 'NONE', #30981, #244845, #68798 ) ;
#173193 = AXIS2_PLACEMENT_3D ( 'NONE', #50698, #89842, #128995 ) ;
#173194 = ORIENTED_EDGE ( 'NONE', *, *, #174793, .F. ) ;
#173195 = ORIENTED_EDGE ( 'NONE', *, *, #235833, .T. ) ;
#173196 = DIRECTION ( 'NONE',  ( 0.000000000000000000, 0.9651348961777157509, -0.2617529984165031243 ) ) ;
#173197 = DIRECTION ( 'NONE',  ( -0.000000000000000000, -0.000000000000000000, 1.000000000000000000 ) ) ;
#173198 = CARTESIAN_POINT ( 'NONE',  ( -18.40000000000000213, 11.33174054712517886, -20.85000000000000142 ) ) ;
#173199 =( NAMED_UNIT ( * ) PLANE_ANGLE_UNIT ( ) SI_UNIT ( $, .RADIAN. ) );
#173200 = CYLINDRICAL_SURFACE ( 'NONE', #99605, 0.1000000000000028644 ) ;
#173201 = CIRCLE ( 'NONE', #206458, 4.099999999999992539 ) ;
#173202 = VERTEX_POINT ( 'NONE', #132669 ) ;
#173203 = AXIS2_PLACEMENT_3D ( 'NONE', #73187, #155293, #118719 ) ;
#173204 = ITEM_DEFINED_TRANSFORMATION ( 'NONE', 'NONE', #190248,  #2425 ) ;
#173205 = CIRCLE ( 'NONE', #42755, 0.1000000000000028644 ) ;
#173206 = EDGE_LOOP ( 'NONE', ( #204449, #250752, #191059 ) ) ;
#173207 = DIRECTION ( 'NONE',  ( 1.000000000000000000, -2.952720810173289112E-16, -2.061873921506763405E-30 ) ) ;
#173208 = VECTOR ( 'NONE', #6857, 999.9999999999998863 ) ;
#173209 = ORIENTED_EDGE ( 'NONE', *, *, #218066, .F. ) ;
#173211 = AXIS2_PLACEMENT_3D ( 'NONE', #66685, #212303, #207495 ) ;
#173210 = CARTESIAN_POINT ( 'NONE',  ( -20.94999999999999929, 12.80863705670245878, -205.3010250813005655 ) ) ;
#173212 = EDGE_LOOP ( 'NONE', ( #55792, #216259, #66414 ) ) ;
#173213 = CARTESIAN_POINT ( 'NONE',  ( -21.05000000000000071, 76.00000000001195133, -103.0231074845243171 ) ) ;
#173214 = AXIS2_PLACEMENT_3D ( 'NONE', #53551, #32744, #156537 ) ;
#173215 = DIRECTION ( 'NONE',  ( 1.000000000000000000, 0.000000000000000000, 0.000000000000000000 ) ) ;
#173216 = CARTESIAN_POINT ( 'NONE',  ( 21.04116576186302368, 10.62466307876251292, -112.8285817686274299 ) ) ;
#173217 = AXIS2_PLACEMENT_3D ( 'NONE', #1530, #122797, #22416 ) ;
#173218 = LINE ( 'NONE', #235695, #36531 ) ;
#173219 = DIRECTION ( 'NONE',  ( 1.000000000000000000, 0.000000000000000000, 0.000000000000000000 ) ) ;
#173220 = DIRECTION ( 'NONE',  ( 1.000000000000000000, 0.000000000000000000, -0.000000000000000000 ) ) ;
#173221 = DIRECTION ( 'NONE',  ( 1.000000000000000000, -0.000000000000000000, -0.000000000000000000 ) ) ;
#173222 = EDGE_CURVE ( 'NONE', #193731, #201172, #91350, .T. ) ;
#173223 = FACE_OUTER_BOUND ( 'NONE', #98379, .T. ) ;
#173225 = CARTESIAN_POINT ( 'NONE',  ( 21.30000000000002558, 1.115600667400684642E-11, -67.00000000000004263 ) ) ;
#173224 = CARTESIAN_POINT ( 'NONE',  ( 20.04999999999999716, 67.25000000001222134, -149.1731074845244223 ) ) ;
#173226 = DIRECTION ( 'NONE',  ( 1.000000000000000000, 0.000000000000000000, 0.000000000000000000 ) ) ;
#173227 = DIRECTION ( 'NONE',  ( 0.000000000000000000, -0.01562499999996560217, -0.9998779222360102414 ) ) ;
#173228 = EDGE_LOOP ( 'NONE', ( #865, #215324, #168959, #203473, #103846 ) ) ;
#173229 = CARTESIAN_POINT ( 'NONE',  ( -18.49372193242250972, -9.442484523357896009, -40.26478126003478764 ) ) ;
#173230 = CYLINDRICAL_SURFACE ( 'NONE', #66322, 0.09999999999999939493 ) ;
#173231 = CARTESIAN_POINT ( 'NONE',  ( -20.94999999999999929, 68.97833521811159585, -65.68954208262705663 ) ) ;
#173232 = ORIENTED_EDGE ( 'NONE', *, *, #14773, .T. ) ;
#173233 = CARTESIAN_POINT ( 'NONE',  ( -21.05000000000000071, 7.128833340093095217, -233.7327013124392749 ) ) ;
#173235 = EDGE_CURVE ( 'NONE', #12612, #117026, #106774, .T. ) ;
#173234 = CARTESIAN_POINT ( 'NONE',  ( -21.64999999999999858, 7.350000000011155166, -121.6500000000000341 ) ) ;
#173236 = CARTESIAN_POINT ( 'NONE',  ( -23.15000000000000213, 23.38726701055792745, -229.1122755113798632 ) ) ;
#173237 =( BOUNDED_CURVE ( )  B_SPLINE_CURVE ( 3, ( #117074, #256510, #255237, #132805 ),
 .UNSPECIFIED., .F., .F. ) 
 B_SPLINE_CURVE_WITH_KNOTS ( ( 4, 4 ),
 ( 1.570796326794895448, 3.141592653589791784 ),
 .UNSPECIFIED. ) 
 CURVE ( )  GEOMETRIC_REPRESENTATION_ITEM ( )  RATIONAL_B_SPLINE_CURVE ( ( 1.000000000000000000, 0.8047378541243650485, 0.8047378541243650485, 1.000000000000000000 ) ) 
 REPRESENTATION_ITEM ( '' )  );
#173238 = ORIENTED_EDGE ( 'NONE', *, *, #242076, .F. ) ;
#173239 = EDGE_CURVE ( 'NONE', #164655, #162415, #210913, .T. ) ;
#173240 = CIRCLE ( 'NONE', #248212, 11.80000000000000959 ) ;
#173241 = AXIS2_PLACEMENT_3D ( 'NONE', #93095, #153126, #227464 ) ;
#173242 = CYLINDRICAL_SURFACE ( 'NONE', #126461, 7.900000000000000355 ) ;
#173243 = ORIENTED_EDGE ( 'NONE', *, *, #9337, .F. ) ;
#173245 = CIRCLE ( 'NONE', #152374, 2.699999999999999289 ) ;
#173244 = DIRECTION ( 'NONE',  ( 0.000000000000000000, 0.000000000000000000, 1.000000000000000000 ) ) ;
#173246 = FACE_OUTER_BOUND ( 'NONE', #215808, .T. ) ;
#173247 = CIRCLE ( 'NONE', #6780, 0.5000000000000004441 ) ;
#173248 = EDGE_CURVE ( 'NONE', #196564, #87303, #81768, .T. ) ;
#173249 = CIRCLE ( 'NONE', #160761, 4.100000000000008527 ) ;
#173250 = EDGE_LOOP ( 'NONE', ( #189255, #100307, #81758, #8950 ) ) ;
#173251 = DIRECTION ( 'NONE',  ( -0.000000000000000000, 0.000000000000000000, -1.000000000000000000 ) ) ;
#173252 = ORIENTED_EDGE ( 'NONE', *, *, #36735, .F. ) ;
#173253 = EDGE_CURVE ( 'NONE', #220738, #245391, #56855, .T. ) ;
#173255 = AXIS2_PLACEMENT_3D ( 'NONE', #158014, #117555, #19760 ) ;
#173254 = DIRECTION ( 'NONE',  ( 1.000000000000000000, 0.000000000000000000, 0.000000000000000000 ) ) ;
#173257 = AXIS2_PLACEMENT_3D ( 'NONE', #173137, #157412, #97358 ) ;
#173256 = CARTESIAN_POINT ( 'NONE',  ( 21.05000000000000071, -11.39257802169451139, -130.9260504201681101 ) ) ;
#173259 = CARTESIAN_POINT ( 'NONE',  ( -23.25000000000000000, 70.05000000001221849, -146.8288097895591875 ) ) ;
#173258 = UNCERTAINTY_MEASURE_WITH_UNIT (LENGTH_MEASURE( 1.000000000000000082E-05 ), #7251, 'distance_accuracy_value', 'NONE');
#173260 = CARTESIAN_POINT ( 'NONE',  ( -20.64999999999999858, 20.06933876993645782, -235.7297789824848451 ) ) ;
#173261 = CARTESIAN_POINT ( 'NONE',  ( -16.83794237512074332, 9.926359221107476927, -12.80354215869896173 ) ) ;
#173262 = CARTESIAN_POINT ( 'NONE',  ( -23.25000000000000000, 76.00000000001213607, -136.5231074845243313 ) ) ;
#173263 = ADVANCED_FACE ( 'NONE', ( #109230 ), #234315, .F. ) ;
#173264 = VECTOR ( 'NONE', #243036, 1000.000000000000000 ) ;
#173265 = FACE_OUTER_BOUND ( 'NONE', #187902, .T. ) ;
#173266 = DIRECTION ( 'NONE',  ( -1.000000000000000000, -7.304098846218134667E-16, 0.000000000000000000 ) ) ;
#173268 = ORIENTED_EDGE ( 'NONE', *, *, #258032, .T. ) ;
#173267 = CARTESIAN_POINT ( 'NONE',  ( 18.50000000000000711, -0.6576273345615416543, -242.5323337003319182 ) ) ;
#173270 = CARTESIAN_POINT ( 'NONE',  ( -21.05439746398122836, 64.25000000001161027, -62.53319099703981720 ) ) ;
#173269 = CARTESIAN_POINT ( 'NONE',  ( -22.50000000000000000, 76.00000000001237765, -170.0231074845243597 ) ) ;
#173271 = ORIENTED_EDGE ( 'NONE', *, *, #169441, .F. ) ;
#173273 = ORIENTED_EDGE ( 'NONE', *, *, #117927, .T. ) ;
#173272 = CARTESIAN_POINT ( 'NONE',  ( 20.94999999999999574, 74.83729825007360148, -61.42310748452432989 ) ) ;
#173274 = B_SPLINE_CURVE_WITH_KNOTS ( 'NONE', 3,
 ( #181280, #123861, #62599, #202109, #183821, #41771, #102983, #182560, #5152, #242509, #203395, #143409, #126411, #65149, #205949, #44326, #125147, #24782, #104263 ),
 .UNSPECIFIED., .F., .F.,
 ( 4, 3, 3, 3, 3, 3, 4 ),
 ( 0.000000000000000000, 1.655171619025856859E-05, 2.773500582849416576E-05, 5.941817267376708916E-05, 0.0001114174635873553602, 0.0001914169455916492238, 0.0002627181070750875128 ),
 .UNSPECIFIED. ) ;
#173275 = EDGE_LOOP ( 'NONE', ( #224323, #75654, #129303, #169212, #151245 ) ) ;
#173276 = DIRECTION ( 'NONE',  ( 0.000000000000000000, 0.2128009952263605065, -0.9770955615653315052 ) ) ;
#173277 = DIRECTION ( 'NONE',  ( 0.000000000000000000, -1.000000000000000000, -0.000000000000000000 ) ) ;
#173278 = CARTESIAN_POINT ( 'NONE',  ( 21.05000000000000071, 62.08591502004790641, -248.5699171172615820 ) ) ;
#173279 = DIRECTION ( 'NONE',  ( -0.000000000000000000, -0.9651348961777157509, 0.2617529984165031243 ) ) ;
#173281 = DIRECTION ( 'NONE',  ( 2.952720810173289112E-16, -1.000000000000000000, -0.000000000000000000 ) ) ;
#173280 = AXIS2_PLACEMENT_3D ( 'NONE', #21949, #102726, #160195 ) ;
#173282 = CARTESIAN_POINT ( 'NONE',  ( -18.59999999999999787, 64.35000000001190301, -96.10830171387040366 ) ) ;
#173283 = CARTESIAN_POINT ( 'NONE',  ( -18.50000000000000000, 1.340746217944851715, -157.2271374945787841 ) ) ;
#173284 = EDGE_CURVE ( 'NONE', #177501, #729, #115168, .T. ) ;
#173285 = CARTESIAN_POINT ( 'NONE',  ( 20.94999999999999929, -11.64999999998883595, -100.5000000000000284 ) ) ;
#173286 = ORIENTED_EDGE ( 'NONE', *, *, #14946, .T. ) ;
#173287 = EDGE_LOOP ( 'NONE', ( #145482, #240585, #116201, #51310 ) ) ;
#173288 = DIRECTION ( 'NONE',  ( -1.000000000000000000, -0.000000000000000000, 0.000000000000000000 ) ) ;
#173289 = AXIS2_PLACEMENT_3D ( 'NONE', #251656, #11794, #233405 ) ;
#173290 = AXIS2_PLACEMENT_3D ( 'NONE', #46678, #221454, #81928 ) ;
#173291 = ORIENTED_EDGE ( 'NONE', *, *, #7022, .F. ) ;
#173292 = AXIS2_PLACEMENT_3D ( 'NONE', #164565, #61603, #65445 ) ;
#173294 = DIRECTION ( 'NONE',  ( 0.000000000000000000, -1.000000000000000000, -6.982962677686265922E-15 ) ) ;
#173293 = VECTOR ( 'NONE', #18155, 999.9999999999998863 ) ;
#173295 = VERTEX_POINT ( 'NONE', #179508 ) ;
#173296 = CARTESIAN_POINT ( 'NONE',  ( 18.58725287972291795, -9.566626910691692132, -40.32250480576551865 ) ) ;
#173297 = EDGE_CURVE ( 'NONE', #149228, #227874, #198360, .T. ) ;
#173298 = CARTESIAN_POINT ( 'NONE',  ( -20.85000000000000142, 87.65000000001192859, -105.9231074845242091 ) ) ;
#173299 = DIRECTION ( 'NONE',  ( -0.7071067811865487940, -0.7071067811865463515, -4.216150419019404490E-15 ) ) ;
#173300 = LINE ( 'NONE', #254049, #127340 ) ;
#173301 = FACE_OUTER_BOUND ( 'NONE', #163741, .T. ) ;
#173302 = ORIENTED_EDGE ( 'NONE', *, *, #162400, .T. ) ;
#173304 = EDGE_CURVE ( 'NONE', #236886, #2978, #152617, .T. ) ;
#173303 = CARTESIAN_POINT ( 'NONE',  ( -18.41809261886920623, -9.682403314745256395, -207.6568435500914234 ) ) ;
#173305 = DIRECTION ( 'NONE',  ( 1.000000000000000000, 0.000000000000000000, 0.000000000000000000 ) ) ;
#173306 = DIRECTION ( 'NONE',  ( 0.000000000000000000, -0.9941044884914571611, 0.1084263158146499262 ) ) ;
#173307 = AXIS2_PLACEMENT_3D ( 'NONE', #102506, #256757, #156469 ) ;
#173308 = CARTESIAN_POINT ( 'NONE',  ( -20.94999999999999929, 0.000000000000000000, -33.50000000000000000 ) ) ;
#173309 = EDGE_CURVE ( 'NONE', #141325, #165624, #252510, .T. ) ;
#173310 = ORIENTED_EDGE ( 'NONE', *, *, #1141, .T. ) ;
#173311 = CIRCLE ( 'NONE', #139913, 0.09999999999999892308 ) ;
#173312 = LINE ( 'NONE', #254062, #249913 ) ;
#173313 = ORIENTED_EDGE ( 'NONE', *, *, #45882, .F. ) ;
#173316 = ORIENTED_EDGE ( 'NONE', *, *, #166951, .T. ) ;
#173315 = DIRECTION ( 'NONE',  ( 1.000000000000000000, 0.000000000000000000, 0.000000000000000000 ) ) ;
#173314 = DIRECTION ( 'NONE',  ( 0.000000000000000000, 0.000000000000000000, -1.000000000000000000 ) ) ;
#173317 = EDGE_CURVE ( 'NONE', #7520, #87561, #98619, .T. ) ;
#173318 = DIRECTION ( 'NONE',  ( 0.000000000000000000, -0.000000000000000000, 1.000000000000000000 ) ) ;
#173319 = DIRECTION ( 'NONE',  ( 3.469446951953515108E-14, -1.000000000000000000, 0.000000000000000000 ) ) ;
#173320 = CIRCLE ( 'NONE', #81637, 0.1000000000000028644 ) ;
#173321 = VERTEX_POINT ( 'NONE', #235595 ) ;
#173322 = LINE ( 'NONE', #130277, #117988 ) ;
#173324 = EDGE_CURVE ( 'NONE', #171093, #121226, #240067, .T. ) ;
#173323 = CARTESIAN_POINT ( 'NONE',  ( 20.94999999999999574, 69.45000000001158469, -59.67928539484123718 ) ) ;
#173325 = CARTESIAN_POINT ( 'NONE',  ( -22.50000000000000000, -3.096576715760142484, -228.1501377515016884 ) ) ;
#173327 = ORIENTED_EDGE ( 'NONE', *, *, #205645, .T. ) ;
#173326 = FACE_OUTER_BOUND ( 'NONE', #123970, .T. ) ;
#173328 = EDGE_CURVE ( 'NONE', #88949, #12989, #58489, .T. ) ;
#173329 = EDGE_CURVE ( 'NONE', #18136, #140605, #23620, .T. ) ;
#173330 = VERTEX_POINT ( 'NONE', #137771 ) ;
#173331 = CYLINDRICAL_SURFACE ( 'NONE', #215939, 0.1000000000000046685 ) ;
#173332 = DIRECTION ( 'NONE',  ( 1.000000000000000000, 0.000000000000000000, 0.000000000000000000 ) ) ;
#173333 = CARTESIAN_POINT ( 'NONE',  ( -20.64999999999999858, 68.85000000001186038, -90.67310748452435121 ) ) ;
#173334 = VECTOR ( 'NONE', #238769, 1000.000000000000114 ) ;
#173335 = DIRECTION ( 'NONE',  ( -1.000000000000000000, -0.000000000000000000, -0.000000000000000000 ) ) ;
#173336 = ORIENTED_EDGE ( 'NONE', *, *, #224314, .F. ) ;
#173337 = CARTESIAN_POINT ( 'NONE',  ( -21.64999999999999858, 65.95000000001206786, -123.7731074845243739 ) ) ;
#173338 = EDGE_CURVE ( 'NONE', #145079, #243577, #160961, .T. ) ;
#173339 = DIRECTION ( 'NONE',  ( 0.000000000000000000, -0.1686199900910313187, 0.9856811345164828708 ) ) ;
#173340 = LINE ( 'NONE', #237112, #222597 ) ;
#173341 = EDGE_LOOP ( 'NONE', ( #255368, #167468, #79780, #151807, #77829 ) ) ;
#173342 = CARTESIAN_POINT ( 'NONE',  ( 20.12518398540832010, 59.69712022869846635, -225.5262535407554765 ) ) ;
#173343 = EDGE_CURVE ( 'NONE', #108404, #191917, #48513, .T. ) ;
#173344 = CARTESIAN_POINT ( 'NONE',  ( 18.49999999999999289, 64.25000000001161027, -61.42310748452440095 ) ) ;
#173345 = VERTEX_POINT ( 'NONE', #56931 ) ;
#173346 = AXIS2_PLACEMENT_3D ( 'NONE', #224456, #167098, #25007 ) ;
#173347 = DIRECTION ( 'NONE',  ( -1.000000000000000000, -2.952720810173289112E-16, 0.000000000000000000 ) ) ;
#173348 = DIRECTION ( 'NONE',  ( 0.000000000000000000, 0.000000000000000000, -1.000000000000000000 ) ) ;
#173349 = CIRCLE ( 'NONE', #23301, 0.1000000000000026007 ) ;
#173350 = ORIENTED_EDGE ( 'NONE', *, *, #54012, .T. ) ;
#173351 = ORIENTED_EDGE ( 'NONE', *, *, #132450, .T. ) ;
#173352 = CARTESIAN_POINT ( 'NONE',  ( 21.05000000000000071, 71.00000000001151079, -48.02837350343745015 ) ) ;
#173353 = ORIENTED_EDGE ( 'NONE', *, *, #211524, .F. ) ;
#173355 = ORIENTED_EDGE ( 'NONE', *, *, #21090, .T. ) ;
#173354 = LINE ( 'NONE', #175894, #159492 ) ;
#173356 = EDGE_CURVE ( 'NONE', #245034, #77679, #257674, .T. ) ;
#173357 = EDGE_CURVE ( 'NONE', #204919, #208058, #79074, .T. ) ;
#173360 = ORIENTED_EDGE ( 'NONE', *, *, #131031, .F. ) ;
#173359 = ORIENTED_EDGE ( 'NONE', *, *, #173852, .T. ) ;
#173358 = FACE_OUTER_BOUND ( 'NONE', #64721, .T. ) ;
#173362 = ADVANCED_FACE ( 'NONE', ( #180777 ), #81630, .F. ) ;
#173361 = CARTESIAN_POINT ( 'NONE',  ( -23.25000000000000000, -8.999999999988844479, -57.10603087734755690 ) ) ;
#173363 = CARTESIAN_POINT ( 'NONE',  ( 20.94999999999999929, 76.00000000001244871, -170.0231074845243597 ) ) ;
#173364 = CARTESIAN_POINT ( 'NONE',  ( 21.08750232978087524, 10.72486338602132250, -112.7288581729996224 ) ) ;
#173365 = CIRCLE ( 'NONE', #77604, 0.1000000000000028644 ) ;
#173366 = DIRECTION ( 'NONE',  ( 1.000000000000000000, 0.000000000000000000, 0.000000000000000000 ) ) ;
#173367 = DIRECTION ( 'NONE',  ( 0.000000000000000000, -1.000000000000000000, -6.982962677686266711E-15 ) ) ;
#173368 = CARTESIAN_POINT ( 'NONE',  ( -22.59999970745345976, 25.93914356428276591, -254.3637448099888445 ) ) ;
#173370 = ORIENTED_EDGE ( 'NONE', *, *, #133833, .F. ) ;
#173369 = AXIS2_PLACEMENT_3D ( 'NONE', #90811, #167828, #226459 ) ;
#173371 = VERTEX_POINT ( 'NONE', #55647 ) ;
#173372 = ORIENTED_EDGE ( 'NONE', *, *, #46095, .F. ) ;
#173373 = DIRECTION ( 'NONE',  ( 1.000000000000000000, 0.000000000000000000, 0.000000000000000000 ) ) ;
#173375 = ORIENTED_EDGE ( 'NONE', *, *, #50910, .T. ) ;
#173374 = CARTESIAN_POINT ( 'NONE',  ( 21.14999999999999858, 69.45934304831071415, -103.0231074845243597 ) ) ;
#173377 = CARTESIAN_POINT ( 'NONE',  ( 23.14999999999998437, 76.00000000001213607, -136.5231074845242745 ) ) ;
#173376 = CIRCLE ( 'NONE', #235853, 2.000000000000001776 ) ;
#173378 = ORIENTED_EDGE ( 'NONE', *, *, #219956, .F. ) ;
#173379 = ORIENTED_EDGE ( 'NONE', *, *, #59327, .T. ) ;
#173380 = CARTESIAN_POINT ( 'NONE',  ( -18.42637059832564717, -0.7441716900925177125, -242.2113608637883146 ) ) ;
#173381 = CIRCLE ( 'NONE', #60891, 0.09999999999998898659 ) ;
#173382 = ADVANCED_FACE ( 'NONE', ( #17828 ), #36144, .T. ) ;
#173383 = EDGE_LOOP ( 'NONE', ( #6206, #17206, #202837, #44641 ) ) ;
#173384 = DIRECTION ( 'NONE',  ( 1.000000000000000000, 0.000000000000000000, 0.000000000000000000 ) ) ;
#173386 = EDGE_CURVE ( 'NONE', #256406, #247600, #76523, .T. ) ;
#173385 = CARTESIAN_POINT ( 'NONE',  ( 20.94999999999999929, 81.91411460262999356, -215.0718681741873013 ) ) ;
#173389 = VERTEX_POINT ( 'NONE', #139033 ) ;
#173388 = EDGE_LOOP ( 'NONE', ( #166839, #118324, #117810, #190448, #14151 ) ) ;
#173387 = AXIS2_PLACEMENT_3D ( 'NONE', #2044, #234242, #116876 ) ;
#173390 = ORIENTED_EDGE ( 'NONE', *, *, #234340, .F. ) ;
#173391 = CARTESIAN_POINT ( 'NONE',  ( -22.39999999999999858, 11.75000000001115552, -66.90000000000004832 ) ) ;
#173392 = AXIS2_PLACEMENT_3D ( 'NONE', #105030, #102473, #222424 ) ;
#173393 = ORIENTED_EDGE ( 'NONE', *, *, #257421, .T. ) ;
#173394 = AXIS2_PLACEMENT_3D ( 'NONE', #153655, #14105, #59590 ) ;
#173395 = ORIENTED_EDGE ( 'NONE', *, *, #87458, .T. ) ;
#173396 = CARTESIAN_POINT ( 'NONE',  ( -28.12018973533754362, 11.62642356364895413, -347.0000000000001137 ) ) ;
#173399 = ADVANCED_FACE ( 'NONE', ( #218589 ), #176949, .T. ) ;
#173398 = ORIENTED_EDGE ( 'NONE', *, *, #153955, .F. ) ;
#173397 = LINE ( 'NONE', #212487, #210121 ) ;
#173400 = FACE_OUTER_BOUND ( 'NONE', #58577, .T. ) ;
#173401 = AXIS2_PLACEMENT_3D ( 'NONE', #37337, #25475, #162420 ) ;
#173403 = CARTESIAN_POINT ( 'NONE',  ( -23.15000000000000213, 62.08591502004791352, -248.5699171172615820 ) ) ;
#173402 = FACE_BOUND ( 'NONE', #213903, .T. ) ;
#173404 = DIRECTION ( 'NONE',  ( -1.000000000000000000, -0.000000000000000000, 0.000000000000000000 ) ) ;
#173405 = DIRECTION ( 'NONE',  ( 0.000000000000000000, 0.000000000000000000, -1.000000000000000000 ) ) ;
#173406 = FACE_BOUND ( 'NONE', #216480, .T. ) ;
#173407 = ORIENTED_EDGE ( 'NONE', *, *, #5235, .T. ) ;
#173408 = ADVANCED_FACE ( 'NONE', ( #197760 ), #65091, .T. ) ;
#173409 = ORIENTED_EDGE ( 'NONE', *, *, #81930, .F. ) ;
#173410 = CARTESIAN_POINT ( 'NONE',  ( 18.54271179734060127, 85.62408429011072997, -96.28214263182411514 ) ) ;
#173411 = DIRECTION ( 'NONE',  ( -0.000000000000000000, 0.9274965247785350586, 0.3738317757009704811 ) ) ;
#173412 = DIRECTION ( 'NONE',  ( 0.000000000000000000, 0.4099100576504394744, 0.9121259477928547188 ) ) ;
#173413 = ADVANCED_FACE ( 'NONE', ( #82918 ), #166377, .T. ) ;
#173414 = VECTOR ( 'NONE', #107241, 1000.000000000000000 ) ;
#173415 = EDGE_LOOP ( 'NONE', ( #211671, #197550, #104632 ) ) ;
#173416 = CARTESIAN_POINT ( 'NONE',  ( 18.39999999999999503, 50.99613813938697149, -230.5564200897905778 ) ) ;
#173417 = ADVANCED_FACE ( 'NONE', ( #183346 ), #124656, .F. ) ;
#173418 = DIRECTION ( 'NONE',  ( -1.000000000000000000, -2.952720810173289112E-16, 0.000000000000000000 ) ) ;
#173419 = LINE ( 'NONE', #194240, #238358 ) ;
#173421 = EDGE_CURVE ( 'NONE', #156346, #57105, #211028, .T. ) ;
#173420 = EDGE_CURVE ( 'NONE', #27566, #10248, #84172, .T. ) ;
#173422 = ORIENTED_EDGE ( 'NONE', *, *, #125456, .T. ) ;
#173423 = ORIENTED_EDGE ( 'NONE', *, *, #71642, .T. ) ;
#173424 = CARTESIAN_POINT ( 'NONE',  ( 20.85000000000000142, 80.78317333349157536, -192.9003134612049166 ) ) ;
#173425 = FACE_OUTER_BOUND ( 'NONE', #99491, .T. ) ;
#173426 = VERTEX_POINT ( 'NONE', #206750 ) ;
#173427 = DIRECTION ( 'NONE',  ( -2.940209281316621016E-16, -1.000000000000000000, -7.056502275159890832E-15 ) ) ;
#173428 = ORIENTED_EDGE ( 'NONE', *, *, #195714, .T. ) ;
#173429 = CARTESIAN_POINT ( 'NONE',  ( 18.59999999999999076, 6.650000000011155876, -88.25000000000005684 ) ) ;
#173430 = CARTESIAN_POINT ( 'NONE',  ( 18.39999999999999858, -0.7490476236415681832, -242.2033265267442061 ) ) ;
#173432 = LINE ( 'NONE', #31336, #233096 ) ;
#173431 = CARTESIAN_POINT ( 'NONE',  ( -23.25000000000000000, 1.910280373842936141, -113.1313678551989739 ) ) ;
#173433 = TOROIDAL_SURFACE ( 'NONE', #210975, 0.2000000000000000111, 0.1000000000000000056 ) ;
#173434 = CARTESIAN_POINT ( 'NONE',  ( -14.77538296656415184, 66.56333706821271790, -84.70007075222947890 ) ) ;
#173435 = DIRECTION ( 'NONE',  ( -1.000000000000000000, -0.000000000000000000, 0.000000000000000000 ) ) ;
#173436 = CIRCLE ( 'NONE', #98310, 0.1000000000000028644 ) ;
#173437 = CARTESIAN_POINT ( 'NONE',  ( 23.14999999999999858, 1.115600667400684642E-11, -67.00000000000000000 ) ) ;
#173438 = AXIS2_PLACEMENT_3D ( 'NONE', #209620, #28458, #8855 ) ;
#173439 = CIRCLE ( 'NONE', #27672, 0.1000000000000028644 ) ;
#173440 = B_SPLINE_CURVE_WITH_KNOTS ( 'NONE', 3,
 ( #197401, #77438, #99565, #201254, #240398, #22652, #61751, #21368, #155752, #180422, #98269, #141293, #219527, #81283, #39654, #116592 ),
 .UNSPECIFIED., .F., .F.,
 ( 4, 3, 3, 3, 3, 4 ),
 ( 0.000000000000000000, 2.209075297431153384E-05, 5.594258369009587762E-05, 8.979524372342081605E-05, 0.0001236472815274580067, 0.0001574990747609520314 ),
 .UNSPECIFIED. ) ;
#173441 = FACE_OUTER_BOUND ( 'NONE', #163787, .T. ) ;
#173442 = ADVANCED_FACE ( 'NONE', ( #23009 ), #46372, .T. ) ;
#173443 = EDGE_CURVE ( 'NONE', #56540, #184760, #7252, .T. ) ;
#173444 = TOROIDAL_SURFACE ( 'NONE', #60936, 0.2000000000000000111, 0.1000000000000000056 ) ;
#173446 = ORIENTED_EDGE ( 'NONE', *, *, #1970, .F. ) ;
#173445 = VERTEX_POINT ( 'NONE', #45112 ) ;
#173447 = ORIENTED_EDGE ( 'NONE', *, *, #112126, .T. ) ;
#173448 = EDGE_CURVE ( 'NONE', #1689, #90736, #61181, .T. ) ;
#173449 = CARTESIAN_POINT ( 'NONE',  ( -16.92507428761702215, 12.42752446970227176, -211.3048343277114895 ) ) ;
#173450 = CARTESIAN_POINT ( 'NONE',  ( 23.15000000000000213, 61.88149656937974896, -248.1136133839584090 ) ) ;
#173451 = DIRECTION ( 'NONE',  ( -1.000000000000000000, -0.000000000000000000, -0.000000000000000000 ) ) ;
#173452 = VECTOR ( 'NONE', #89329, 1000.000000000000000 ) ;
#173454 = CARTESIAN_POINT ( 'NONE',  ( -22.49533356619860314, 11.65000000631534149, -33.43487741967728510 ) ) ;
#173453 = DIRECTION ( 'NONE',  ( -0.000000000000000000, 6.982962677686266711E-15, -1.000000000000000000 ) ) ;
#173455 = EDGE_CURVE ( 'NONE', #204007, #41254, #64668, .T. ) ;
#173456 = DIRECTION ( 'NONE',  ( 0.000000000000000000, 6.982962677686266711E-15, -1.000000000000000000 ) ) ;
#173457 = VERTEX_POINT ( 'NONE', #51493 ) ;
#173458 = CARTESIAN_POINT ( 'NONE',  ( 20.95512820512820440, 10.62384868372303615, -74.66491356908764487 ) ) ;
#173459 = CIRCLE ( 'NONE', #165007, 0.1999999999999987899 ) ;
#173460 = ADVANCED_FACE ( 'NONE', ( #48949 ), #168955, .F. ) ;
#173461 = ORIENTED_EDGE ( 'NONE', *, *, #169020, .T. ) ;
#173462 = ORIENTED_EDGE ( 'NONE', *, *, #67050, .F. ) ;
#173463 = CARTESIAN_POINT ( 'NONE',  ( -21.05000000000000071, 1.250000000011155299, -108.5000000000000426 ) ) ;
#173464 = AXIS2_PLACEMENT_3D ( 'NONE', #48379, #228320, #163214 ) ;
#173465 = CARTESIAN_POINT ( 'NONE',  ( 21.05000000000000071, 0.000000000000000000, -12.15000000000000036 ) ) ;
#173466 = CARTESIAN_POINT ( 'NONE',  ( -23.25000000000000355, 11.75000000001113953, -54.35000000000000142 ) ) ;
#173467 = DIRECTION ( 'NONE',  ( 1.000000000000000000, 0.000000000000000000, 0.000000000000000000 ) ) ;
#173468 = CARTESIAN_POINT ( 'NONE',  ( -20.85000000000000142, 68.11287320386161070, -224.1382462126928488 ) ) ;
#173469 = ORIENTED_EDGE ( 'NONE', *, *, #66649, .T. ) ;
#173470 = ORIENTED_EDGE ( 'NONE', *, *, #138522, .F. ) ;
#173471 = CARTESIAN_POINT ( 'NONE',  ( -23.15000000000000213, -9.499999999988846255, -157.6060308773475924 ) ) ;
#173472 = VECTOR ( 'NONE', #228830, 1000.000000000000000 ) ;
#173473 = FACE_OUTER_BOUND ( 'NONE', #216622, .T. ) ;
#173474 = EDGE_CURVE ( 'NONE', #75249, #129055, #186075, .T. ) ;
#173475 = DIRECTION ( 'NONE',  ( -1.000000000000000000, 1.836970198721029934E-16, 1.282749433769087757E-30 ) ) ;
#173476 = DIRECTION ( 'NONE',  ( 1.000000000000000000, 0.000000000000000000, 0.000000000000000000 ) ) ;
#173477 = DIRECTION ( 'NONE',  ( 1.000000000000000000, 0.000000000000000000, 0.000000000000000000 ) ) ;
#173478 = DIRECTION ( 'NONE',  ( -1.000000000000000000, 0.000000000000000000, 0.000000000000000000 ) ) ;
#173479 = CARTESIAN_POINT ( 'NONE',  ( -22.00411653962166980, 7.253442868381237751, -33.40096189421771555 ) ) ;
#173481 = CARTESIAN_POINT ( 'NONE',  ( 20.10000000000000853, 4.547418889303921574, 21.90000000000000213 ) ) ;
#173480 = CARTESIAN_POINT ( 'NONE',  ( -22.44366136229477249, 0.009341569486069218817, 11.64971855747391061 ) ) ;
#173482 = LINE ( 'NONE', #250389, #112487 ) ;
#173484 = ADVANCED_FACE ( 'NONE', ( #9831 ), #93211, .T. ) ;
#173483 = CARTESIAN_POINT ( 'NONE',  ( 21.05000000000000071, 65.27628289530409234, -61.85819391543678591 ) ) ;
#173485 = DIRECTION ( 'NONE',  ( 0.000000000000000000, 0.000000000000000000, 1.000000000000000000 ) ) ;
#173486 = CARTESIAN_POINT ( 'NONE',  ( 20.94999999999999929, 10.29288807859936838, -139.4580020160122160 ) ) ;
#173487 = VECTOR ( 'NONE', #159630, 1000.000000000000000 ) ;
#173490 = ORIENTED_EDGE ( 'NONE', *, *, #241961, .F. ) ;
#173489 = AXIS2_PLACEMENT_3D ( 'NONE', #196164, #18806, #157058 ) ;
#173488 = CARTESIAN_POINT ( 'NONE',  ( -6.000000000000003553, -11.25000000000000000, 10.10000000000000142 ) ) ;
#173491 = AXIS2_PLACEMENT_3D ( 'NONE', #37903, #133133, #193116 ) ;
#173492 = AXIS2_PLACEMENT_3D ( 'NONE', #84495, #124969, #67549 ) ;
#173494 = EDGE_CURVE ( 'NONE', #212474, #225666, #223649, .T. ) ;
#173493 = DIRECTION ( 'NONE',  ( 1.000000000000000000, -3.469446951953718318E-14, 2.003086131649645455E-14 ) ) ;
#173495 = DIRECTION ( 'NONE',  ( 1.000000000000000000, 0.000000000000000000, 0.000000000000000000 ) ) ;
#173496 = FACE_OUTER_BOUND ( 'NONE', #178994, .T. ) ;
#173497 = AXIS2_PLACEMENT_3D ( 'NONE', #128530, #249760, #88082 ) ;
#173498 = CARTESIAN_POINT ( 'NONE',  ( 12.26145404764308644, 9.351413679112543065, -83.98034356754899932 ) ) ;
#173499 = CARTESIAN_POINT ( 'NONE',  ( 23.24999999999999645, 70.40000000001229807, -157.6178414656113205 ) ) ;
#173500 = CIRCLE ( 'NONE', #60998, 0.1000000000000002554 ) ;
#173501 = VECTOR ( 'NONE', #96576, 1000.000000000000000 ) ;
#173502 = B_SPLINE_CURVE_WITH_KNOTS ( 'NONE', 3,
 ( #81590, #45070, #182020, #142857, #22971, #145442, #101138, #106303, #124615, #204128, #4638, #43792, #239430, #202852, #104995, #221124, #103727, #25522, #243255 ),
 .UNSPECIFIED., .F., .F.,
 ( 4, 3, 3, 3, 3, 3, 4 ),
 ( 0.000000000000000000, 1.655171619026205498E-05, 2.773500582849481967E-05, 5.941817267378896972E-05, 0.0001114174635873639254, 0.0001914169455916358881, 0.0002627181070750633351 ),
 .UNSPECIFIED. ) ;
#173503 = FACE_OUTER_BOUND ( 'NONE', #196799, .T. ) ;
#173504 = CARTESIAN_POINT ( 'NONE',  ( -13.40000000000000036, -9.650000000000005684, 12.40000000000000391 ) ) ;
#173505 = CARTESIAN_POINT ( 'NONE',  ( 21.05000000000000071, 1.115625160336667635E-11, -132.0000000000000284 ) ) ;
#173506 = VECTOR ( 'NONE', #200479, 1000.000000000000000 ) ;
#173507 = ORIENTED_EDGE ( 'NONE', *, *, #117492, .F. ) ;
#173508 = FACE_OUTER_BOUND ( 'NONE', #103223, .T. ) ;
#173510 = EDGE_LOOP ( 'NONE', ( #192772, #68712, #86828, #110157, #78643 ) ) ;
#173509 = CARTESIAN_POINT ( 'NONE',  ( 18.59999999999999432, -1.162701749926853712, -75.00000000000004263 ) ) ;
#173511 = FACE_OUTER_BOUND ( 'NONE', #169191, .T. ) ;
#173512 = CARTESIAN_POINT ( 'NONE',  ( -21.12642695952773764, 69.62434007797720881, -170.1220107677137605 ) ) ;
#173513 = CARTESIAN_POINT ( 'NONE',  ( -22.57320508075685694, 31.85509083104292571, -238.8280249686205252 ) ) ;
#173514 = EDGE_LOOP ( 'NONE', ( #46876, #78406, #23867, #114357, #232195 ) ) ;
#173515 = CARTESIAN_POINT ( 'NONE',  ( -18.69999999999999929, -18.98805597050104410, -9.034413349721665654 ) ) ;
#173516 = PRODUCT_CONTEXT ( 'NONE', #145654, 'mechanical' ) ;
#173517 = CARTESIAN_POINT ( 'NONE',  ( 22.59999985501178799, 11.46678616150633268, -198.4355198451642650 ) ) ;
#173518 = CARTESIAN_POINT ( 'NONE',  ( 22.50927854361890113, -2.598867553876332614, -189.5410128092696311 ) ) ;
#173519 = ORIENTED_EDGE ( 'NONE', *, *, #10222, .T. ) ;
#173520 = DIRECTION ( 'NONE',  ( 1.000000000000000000, 7.304098846218134667E-16, -0.000000000000000000 ) ) ;
#173521 = CARTESIAN_POINT ( 'NONE',  ( -18.59999999999999787, 23.34004772283015328, -229.2004250369967338 ) ) ;
#173522 = AXIS2_PLACEMENT_3D ( 'NONE', #148666, #13019, #208645 ) ;
#173523 = DIRECTION ( 'NONE',  ( -3.265361837132813586E-16, 1.000000000000000000, 0.000000000000000000 ) ) ;
#173524 = VERTEX_POINT ( 'NONE', #248449 ) ;
#173525 = ORIENTED_EDGE ( 'NONE', *, *, #148579, .T. ) ;
#173526 = CIRCLE ( 'NONE', #78166, 12.87500000000000178 ) ;
#173527 = DIRECTION ( 'NONE',  ( 0.000000000000000000, -1.186135710069611419E-15, 1.000000000000000000 ) ) ;
#173528 = FACE_OUTER_BOUND ( 'NONE', #53552, .T. ) ;
#173529 = DIRECTION ( 'NONE',  ( 0.000000000000000000, 0.000000000000000000, -1.000000000000000000 ) ) ;
#173530 = CARTESIAN_POINT ( 'NONE',  ( -17.11825945287481687, 30.25354784785470841, -234.7188954791831748 ) ) ;
#173531 = EDGE_CURVE ( 'NONE', #165019, #116521, #15407, .T. ) ;
#173534 = CARTESIAN_POINT ( 'NONE',  ( -18.40000000000000213, 64.51332499825454647, -145.7731074845244450 ) ) ;
#173533 = AXIS2_PLACEMENT_3D ( 'NONE', #83329, #189842, #90725 ) ;
#173532 = FACE_OUTER_BOUND ( 'NONE', #124531, .T. ) ;
#173535 = CARTESIAN_POINT ( 'NONE',  ( -18.40000000000000213, 11.47316190337364183, -121.4500000000000313 ) ) ;
#173536 = CARTESIAN_POINT ( 'NONE',  ( -22.39999999999999858, 56.01362831242966678, -232.7091905853083347 ) ) ;
#173537 = DIRECTION ( 'NONE',  ( 0.000000000000000000, 0.000000000000000000, 1.000000000000000000 ) ) ;
#173538 = CARTESIAN_POINT ( 'NONE',  ( -17.22361732159832215, 12.52791994134343234, -209.9088836718198650 ) ) ;
#173539 = ORIENTED_EDGE ( 'NONE', *, *, #148122, .T. ) ;
#173540 = AXIS2_PLACEMENT_3D ( 'NONE', #219821, #85412, #41225 ) ;
#173541 = ORIENTED_EDGE ( 'NONE', *, *, #223110, .T. ) ;
#173542 = CARTESIAN_POINT ( 'NONE',  ( -18.59999999999999787, 85.48068669529138219, -163.0819923157664562 ) ) ;
#173543 = CARTESIAN_POINT ( 'NONE',  ( 22.39999999999999503, 29.50811709945092076, -252.6450601445781103 ) ) ;
#173545 = CARTESIAN_POINT ( 'NONE',  ( -20.64999999999999858, 29.14863708059993286, -237.4168895852561434 ) ) ;
#173544 = DIRECTION ( 'NONE',  ( 0.000000000000000000, -0.9274965247785504907, -0.3738317757009320674 ) ) ;
#173546 = ORIENTED_EDGE ( 'NONE', *, *, #148301, .F. ) ;
#173547 = CARTESIAN_POINT ( 'NONE',  ( 21.05000000000000071, -11.64999999999999147, -30.59999999999999432 ) ) ;
#173549 = EDGE_CURVE ( 'NONE', #150544, #237840, #140258, .T. ) ;
#173548 = CARTESIAN_POINT ( 'NONE',  ( 23.14999999999998792, 11.65000000001115588, -33.50000000000000000 ) ) ;
#173550 = CARTESIAN_POINT ( 'NONE',  ( 21.05000000000000071, 10.68863688179707694, -222.5873974249509217 ) ) ;
#173551 = VERTEX_POINT ( 'NONE', #129774 ) ;
#173552 = ORIENTED_EDGE ( 'NONE', *, *, #104147, .T. ) ;
#173553 = EDGE_CURVE ( 'NONE', #179315, #200421, #189754, .T. ) ;
#173554 = ORIENTED_EDGE ( 'NONE', *, *, #106997, .T. ) ;
#173555 = DIRECTION ( 'NONE',  ( 0.000000000000000000, 0.9770955615653315052, 0.2128009952263603954 ) ) ;
#173557 = EDGE_CURVE ( 'NONE', #213725, #152168, #48690, .T. ) ;
#173556 = VECTOR ( 'NONE', #90375, 1000.000000000000000 ) ;
#173558 = DIRECTION ( 'NONE',  ( 0.000000000000000000, 1.000000000000000000, 7.116814260417668513E-15 ) ) ;
#173559 = CIRCLE ( 'NONE', #169456, 0.09999999999998898659 ) ;
#173560 = DIRECTION ( 'NONE',  ( 0.000000000000000000, 6.982962677686266711E-15, -1.000000000000000000 ) ) ;
#173561 = EDGE_CURVE ( 'NONE', #5814, #31606, #91930, .T. ) ;
#173562 = AXIS2_PLACEMENT_3D ( 'NONE', #205115, #162183, #241695 ) ;
#173563 = EDGE_CURVE ( 'NONE', #230071, #199924, #252277, .T. ) ;
#173564 = ORIENTED_EDGE ( 'NONE', *, *, #143356, .F. ) ;
#173565 = LINE ( 'NONE', #253037, #76600 ) ;
#173566 =( BOUNDED_SURFACE ( )  B_SPLINE_SURFACE ( 3, 2, ( 
 ( #130933, #172678, #188340 ),
 ( #52667, #132218, #112662 ),
 ( #192211, #87927, #167522 ),
 ( #27582, #125363, #147489 ),
 ( #88773, #182779, #206180 ),
 ( #244005, #7991, #65379 ) ),
 .UNSPECIFIED., .F., .F., .F. ) 
 B_SPLINE_SURFACE_WITH_KNOTS ( ( 4, 2, 4 ),
 ( 3, 3 ),
 ( 0.0001342700090130014186, 0.0002909192928057377698, 0.0004475685765984741210 ),
 ( 0.000000000000000000, 1.000000000000000000 ),
 .UNSPECIFIED. ) 
 GEOMETRIC_REPRESENTATION_ITEM ( )  RATIONAL_B_SPLINE_SURFACE ( (
 ( 1.000000000000000000, 0.7250110520819876836, 1.000000000000000000),
 ( 1.000000000000000000, 0.7257599279135071857, 1.000000000000000000),
 ( 1.000000000000000000, 0.7137594617282845277, 1.000000000000000000),
 ( 1.000000000000000000, 0.6959270178810901264, 1.000000000000000000),
 ( 1.000000000000000000, 0.6919879549338453506, 1.000000000000000000),
 ( 1.000000000000000000, 0.7071067811865494601, 1.000000000000000000) ) ) 
 REPRESENTATION_ITEM ( '' )  SURFACE ( )  );
#173567 = AXIS2_PLACEMENT_3D ( 'NONE', #111654, #35988, #54236 ) ;
#173568 = EDGE_CURVE ( 'NONE', #60065, #151804, #123733, .T. ) ;
#173569 = FACE_OUTER_BOUND ( 'NONE', #100711, .T. ) ;
#173570 = DIRECTION ( 'NONE',  ( 1.000000000000000000, 0.000000000000000000, 0.000000000000000000 ) ) ;
#173571 = LINE ( 'NONE', #53571, #124890 ) ;
#173572 = CARTESIAN_POINT ( 'NONE',  ( 21.05000000000000071, 65.49889199258034012, -241.8691648588986425 ) ) ;
#173574 = DIRECTION ( 'NONE',  ( 0.000000000000000000, 0.000000000000000000, -1.000000000000000000 ) ) ;
#173573 = FACE_OUTER_BOUND ( 'NONE', #110471, .T. ) ;
#173575 = ADVANCED_FACE ( 'NONE', ( #230161 ), #254928, .T. ) ;
#173576 = CARTESIAN_POINT ( 'NONE',  ( -16.83233564386387471, 66.06977820342763152, -149.2985868210483318 ) ) ;
#173577 = ORIENTED_EDGE ( 'NONE', *, *, #180845, .T. ) ;
#173579 = DIRECTION ( 'NONE',  ( 0.000000000000000000, -0.8777080977375715243, 0.4791956752370512551 ) ) ;
#173578 = DIRECTION ( 'NONE',  ( 1.000000000000000000, 0.000000000000000000, 0.000000000000000000 ) ) ;
#173580 = ORIENTED_EDGE ( 'NONE', *, *, #44973, .T. ) ;
#173582 = ORIENTED_EDGE ( 'NONE', *, *, #228544, .T. ) ;
#173581 = CARTESIAN_POINT ( 'NONE',  ( -20.64999999999999858, 73.50000000001151079, -49.24772940728643533 ) ) ;
#173583 = AXIS2_PLACEMENT_3D ( 'NONE', #115282, #155732, #138663 ) ;
#173584 = ORIENTED_EDGE ( 'NONE', *, *, #64486, .T. ) ;
#173585 = CARTESIAN_POINT ( 'NONE',  ( 22.59080734064468032, 12.64999392629033359, -223.3606122593135979 ) ) ;
#173586 = VECTOR ( 'NONE', #61797, 1000.000000000000000 ) ;
#173587 = EDGE_CURVE ( 'NONE', #141245, #154382, #19502, .T. ) ;
#173588 = CARTESIAN_POINT ( 'NONE',  ( 18.56579813702275317, 10.33025634372637924, -72.58709292826388548 ) ) ;
#173589 = CIRCLE ( 'NONE', #73601, 0.9750000000000036415 ) ;
#173590 = CARTESIAN_POINT ( 'NONE',  ( -18.59999999999999787, -0.5913595841389547303, -242.4574432119242999 ) ) ;
#173591 = FACE_OUTER_BOUND ( 'NONE', #148704, .T. ) ;
#173592 = ORIENTED_EDGE ( 'NONE', *, *, #99609, .T. ) ;
#173593 = ADVANCED_FACE ( 'NONE', ( #68532, #23679 ), #182738, .F. ) ;
#173594 = LINE ( 'NONE', #117417, #122491 ) ;
#173595 = FACE_OUTER_BOUND ( 'NONE', #16656, .T. ) ;
#173596 = VERTEX_POINT ( 'NONE', #1500 ) ;
#173598 = EDGE_CURVE ( 'NONE', #118767, #111624, #23528, .T. ) ;
#173597 = CYLINDRICAL_SURFACE ( 'NONE', #15034, 0.1000000000000028644 ) ;
#173599 = CIRCLE ( 'NONE', #148432, 0.1000000000000028644 ) ;
#173600 = CARTESIAN_POINT ( 'NONE',  ( 21.05000000000000071, 13.71992543034163958, -238.5823796952984992 ) ) ;
#173601 = ORIENTED_EDGE ( 'NONE', *, *, #88905, .T. ) ;
#173602 = CARTESIAN_POINT ( 'NONE',  ( 21.14999999999999858, 45.25174493058054281, -238.5244480634700324 ) ) ;
#173603 = ORIENTED_EDGE ( 'NONE', *, *, #226370, .F. ) ;
#173604 = DIRECTION ( 'NONE',  ( -2.952720810173289112E-16, 1.000000000000000000, -0.000000000000000000 ) ) ;
#173605 = EDGE_LOOP ( 'NONE', ( #154076, #23168, #49778 ) ) ;
#173606 = CARTESIAN_POINT ( 'NONE',  ( 23.14999999999999503, 21.13195309841794867, -243.6318585593223816 ) ) ;
#173607 = ADVANCED_FACE ( 'NONE', ( #17519 ), #235197, .T. ) ;
#173608 = CARTESIAN_POINT ( 'NONE',  ( -1.739115166359751801E-14, 64.35000000001224407, -148.6731074845244507 ) ) ;
#173609 = CARTESIAN_POINT ( 'NONE',  ( 22.16821283564876666, 68.44102665923192319, -203.5231074845243882 ) ) ;
#173610 = LINE ( 'NONE', #129298, #74548 ) ;
#173611 = VECTOR ( 'NONE', #5533, 1000.000000000000000 ) ;
#173612 = AXIS2_PLACEMENT_3D ( 'NONE', #20325, #708, #75172 ) ;
#173613 = TOROIDAL_SURFACE ( 'NONE', #115289, 12.97499999999999787, 0.1000000000000000056 ) ;
#173614 = AXIS2_PLACEMENT_3D ( 'NONE', #185474, #5526, #85050 ) ;
#173615 = CARTESIAN_POINT ( 'NONE',  ( 23.14999999999998792, 31.89597452117651244, -238.9192857152811769 ) ) ;
#173616 = DIRECTION ( 'NONE',  ( 0.000000000000000000, 0.9126074666063769270, 0.4088369013363281623 ) ) ;
#173617 = DIRECTION ( 'NONE',  ( 0.000000000000000000, 0.5000000000000078826, -0.8660254037844340447 ) ) ;
#173618 = ORIENTED_EDGE ( 'NONE', *, *, #17769, .T. ) ;
#173620 = FACE_OUTER_BOUND ( 'NONE', #127983, .T. ) ;
#173619 = DIRECTION ( 'NONE',  ( -1.000000000000000000, -0.000000000000000000, -0.000000000000000000 ) ) ;
#173621 = ORIENTED_EDGE ( 'NONE', *, *, #103009, .F. ) ;
#173624 = VERTEX_POINT ( 'NONE', #240135 ) ;
#173623 = FACE_OUTER_BOUND ( 'NONE', #245501, .T. ) ;
#173622 = DIRECTION ( 'NONE',  ( -3.265361837132813093E-16, 1.000000000000000000, 0.000000000000000000 ) ) ;
#173625 = VECTOR ( 'NONE', #35150, 1000.000000000000000 ) ;
#173626 = EDGE_CURVE ( 'NONE', #46494, #120853, #61492, .T. ) ;
#173627 = EDGE_LOOP ( 'NONE', ( #72614, #70332, #204168, #196961 ) ) ;
#173628 = DIRECTION ( 'NONE',  ( 0.000000000000000000, 1.000000000000000000, 7.116814260417668513E-15 ) ) ;
#173629 = CARTESIAN_POINT ( 'NONE',  ( 21.14999999999999858, 1.115486826172573664E-11, -60.45934304829879835 ) ) ;
#173630 = CYLINDRICAL_SURFACE ( 'NONE', #73515, 12.87500000000000355 ) ;
#173631 = CARTESIAN_POINT ( 'NONE',  ( -23.15000000000000213, -8.999999999988846255, -43.39396912265245021 ) ) ;
#173632 = ORIENTED_EDGE ( 'NONE', *, *, #25985, .T. ) ;
#173634 = ORIENTED_EDGE ( 'NONE', *, *, #199661, .F. ) ;
#173633 = CARTESIAN_POINT ( 'NONE',  ( -16.87304349924914604, 66.03825492205483272, -115.6340408094791172 ) ) ;
#173636 = EDGE_CURVE ( 'NONE', #79296, #135320, #22383, .T. ) ;
#173635 = AXIS2_PLACEMENT_3D ( 'NONE', #193590, #194887, #14963 ) ;
#173638 = CARTESIAN_POINT ( 'NONE',  ( 18.49999999999999289, 10.20857864377385127, -155.3500000000000227 ) ) ;
#173637 = CARTESIAN_POINT ( 'NONE',  ( 20.94999999999999929, 10.72371710471868056, -146.1500000000000341 ) ) ;
#173639 = AXIS2_PLACEMENT_3D ( 'NONE', #109962, #166132, #228658 ) ;
#173641 = ORIENTED_EDGE ( 'NONE', *, *, #89401, .F. ) ;
#173640 = FACE_OUTER_BOUND ( 'NONE', #203838, .T. ) ;
#173642 = CIRCLE ( 'NONE', #52752, 11.80000000000000426 ) ;
#173643 = EDGE_CURVE ( 'NONE', #21068, #17724, #57047, .T. ) ;
#173644 = ADVANCED_FACE ( 'NONE', ( #56620 ), #81992, .F. ) ;
#173645 = EDGE_LOOP ( 'NONE', ( #156587, #211213, #180024, #29965 ) ) ;
#173646 = EDGE_CURVE ( 'NONE', #235108, #98003, #82301, .T. ) ;
#173647 = EDGE_CURVE ( 'NONE', #253337, #79099, #115333, .T. ) ;
#173648 = CARTESIAN_POINT ( 'NONE',  ( 20.95265033839679347, 11.88147568740731330, -206.1554567466520780 ) ) ;
#173649 = DIRECTION ( 'NONE',  ( -1.000000000000000000, -0.000000000000000000, -0.000000000000000000 ) ) ;
#173650 = VERTEX_POINT ( 'NONE', #142299 ) ;
#173651 = DIRECTION ( 'NONE',  ( 1.000000000000000000, 0.000000000000000000, 0.000000000000000000 ) ) ;
#173652 = VERTEX_POINT ( 'NONE', #221816 ) ;
#173653 = ADVANCED_FACE ( 'NONE', ( #44507 ), #122769, .F. ) ;
#173654 = CARTESIAN_POINT ( 'NONE',  ( -18.47690164073607022, -9.464844538001083052, -107.2013809398361843 ) ) ;
#173655 = CARTESIAN_POINT ( 'NONE',  ( 20.46382478191414833, 18.90138345391644847, -228.0154769769863492 ) ) ;
#173656 = ORIENTED_EDGE ( 'NONE', *, *, #44114, .F. ) ;
#173657 = CARTESIAN_POINT ( 'NONE',  ( -18.40000000000000213, 64.25000000001253397, -179.2731074845244450 ) ) ;
#173658 = VECTOR ( 'NONE', #251997, 1000.000000000000000 ) ;
#173659 = CIRCLE ( 'NONE', #98536, 0.1000000000000001305 ) ;
#173660 = DIRECTION ( 'NONE',  ( 0.000000000000000000, 0.000000000000000000, -1.000000000000000000 ) ) ;
#173661 = VECTOR ( 'NONE', #102312, 1000.000000000000000 ) ;
#173662 = CIRCLE ( 'NONE', #211203, 0.09999999999998898659 ) ;
#173663 = EDGE_CURVE ( 'NONE', #229490, #227815, #190379, .T. ) ;
#173664 = EDGE_LOOP ( 'NONE', ( #167156, #25508, #66295, #35198, #174439 ) ) ;
#173665 = VERTEX_POINT ( 'NONE', #203568 ) ;
#173666 = CARTESIAN_POINT ( 'NONE',  ( -22.94999999999999929, -11.64999999999999858, 12.09999999999999609 ) ) ;
#173667 =( BOUNDED_SURFACE ( )  B_SPLINE_SURFACE ( 3, 2, ( 
 ( #55493, #13845, #175506 ),
 ( #132507, #172959, #15134 ),
 ( #71270, #191225, #195069 ),
 ( #174244, #16431, #33447 ),
 ( #154666, #93368, #112948 ),
 ( #155948, #131213, #150783 ) ),
 .UNSPECIFIED., .F., .F., .T. ) 
 B_SPLINE_SURFACE_WITH_KNOTS ( ( 4, 2, 4 ),
 ( 3, 3 ),
 ( 4.712388980384689674, 5.497787143782137953, 6.283185307179586232 ),
 ( 0.000000000000000000, 1.000000000000000000 ),
 .UNSPECIFIED. ) 
 GEOMETRIC_REPRESENTATION_ITEM ( )  RATIONAL_B_SPLINE_SURFACE ( (
 ( 1.000000000000000000, 0.7071067811865536790, 1.000000000000000000),
 ( 1.000000000000000000, 0.7727932973488890189, 1.000000000000000000),
 ( 1.000000000000000000, 0.8282379607652868847, 1.000000000000000000),
 ( 1.000000000000000000, 0.9038128468036029650, 1.000000000000000000),
 ( 1.000000000000000000, 0.9240297172246195734, 1.000000000000000000),
 ( 1.000000000000000000, 0.9238795325112914014, 1.000000000000000000) ) ) 
 REPRESENTATION_ITEM ( '' )  SURFACE ( )  );
#173668 = ORIENTED_EDGE ( 'NONE', *, *, #210428, .T. ) ;
#173669 = CARTESIAN_POINT ( 'NONE',  ( -21.05000000000000071, 61.95000000001234497, -164.5094124137634708 ) ) ;
#173670 = VERTEX_POINT ( 'NONE', #94494 ) ;
#173672 = ORIENTED_EDGE ( 'NONE', *, *, #18240, .F. ) ;
#173671 = FACE_OUTER_BOUND ( 'NONE', #67254, .T. ) ;
#173673 = ADVANCED_FACE ( 'NONE', ( #154516 ), #115347, .F. ) ;
#173674 = ADVANCED_FACE ( 'NONE', ( #76208 ), #126599, .T. ) ;
#173675 = ORIENTED_EDGE ( 'NONE', *, *, #41970, .T. ) ;
#173676 = FACE_OUTER_BOUND ( 'NONE', #90392, .T. ) ;
#173677 = ORIENTED_EDGE ( 'NONE', *, *, #14568, .F. ) ;
#173680 = VERTEX_POINT ( 'NONE', #49628 ) ;
#173679 = ORIENTED_EDGE ( 'NONE', *, *, #167437, .T. ) ;
#173678 = CARTESIAN_POINT ( 'NONE',  ( 18.49999999999999645, -1.299733671219632791, -124.0281295228694347 ) ) ;
#173681 = CIRCLE ( 'NONE', #215309, 0.1999999999999996503 ) ;
#173682 = AXIS2_PLACEMENT_3D ( 'NONE', #217342, #29161, #70838 ) ;
#173683 = CIRCLE ( 'NONE', #40394, 0.1000000000000013933 ) ;
#173684 = ORIENTED_EDGE ( 'NONE', *, *, #132107, .T. ) ;
#173685 = AXIS2_PLACEMENT_3D ( 'NONE', #251131, #116774, #174228 ) ;
#173686 = CARTESIAN_POINT ( 'NONE',  ( -20.94999999999999929, 87.29603075034701476, -72.57100664418810254 ) ) ;
#173687 = ORIENTED_EDGE ( 'NONE', *, *, #241190, .F. ) ;
#173688 = DIRECTION ( 'NONE',  ( -1.073024830501117528E-15, 0.8814952561688430555, -0.4721928772777346239 ) ) ;
#173690 = ORIENTED_EDGE ( 'NONE', *, *, #209446, .T. ) ;
#173689 = CYLINDRICAL_SURFACE ( 'NONE', #245118, 0.1000000000000028644 ) ;
#173691 = CARTESIAN_POINT ( 'NONE',  ( -20.94999999999999929, 11.60000000001115517, -194.0717967697244717 ) ) ;
#173692 = ORIENTED_EDGE ( 'NONE', *, *, #251668, .T. ) ;
#173693 = ORIENTED_EDGE ( 'NONE', *, *, #97213, .T. ) ;
#173694 = CARTESIAN_POINT ( 'NONE',  ( -20.54999999999999716, 2.000000000011154189, -180.7246219227620543 ) ) ;
#173695 = CARTESIAN_POINT ( 'NONE',  ( 24.30000000000000071, -12.79999999999999716, 33.00000000000000000 ) ) ;
#173696 = ORIENTED_EDGE ( 'NONE', *, *, #43524, .F. ) ;
#173697 = ORIENTED_EDGE ( 'NONE', *, *, #131816, .T. ) ;
#173698 = AXIS2_PLACEMENT_3D ( 'NONE', #174686, #117230, #136776 ) ;
#173700 = VERTEX_POINT ( 'NONE', #167044 ) ;
#173699 = ORIENTED_EDGE ( 'NONE', *, *, #154628, .T. ) ;
#173701 = ORIENTED_EDGE ( 'NONE', *, *, #256549, .F. ) ;
#173702 = DIRECTION ( 'NONE',  ( -3.890533409366484652E-14, 0.1298341882520054891, 0.9915357197604850459 ) ) ;
#173703 = ORIENTED_EDGE ( 'NONE', *, *, #195440, .T. ) ;
#173704 = ORIENTED_EDGE ( 'NONE', *, *, #52095, .F. ) ;
#173705 = CARTESIAN_POINT ( 'NONE',  ( -20.94999999999999929, 77.25000000001232081, -162.0231074845243313 ) ) ;
#173706 = EDGE_LOOP ( 'NONE', ( #147688, #234627, #163561, #155324 ) ) ;
#173707 = CARTESIAN_POINT ( 'NONE',  ( -20.07928932188135107, 66.77928932189364275, -157.6731074845244223 ) ) ;
#173708 = AXIS2_PLACEMENT_3D ( 'NONE', #127586, #168036, #205836 ) ;
#173709 = CARTESIAN_POINT ( 'NONE',  ( 21.14999999999999858, 76.00000000001169553, -76.06376443622556849 ) ) ;
#173710 = ORIENTED_EDGE ( 'NONE', *, *, #16442, .T. ) ;
#173711 = ADVANCED_FACE ( 'NONE', ( #208723 ), #45771, .F. ) ;
#173712 = EDGE_LOOP ( 'NONE', ( #9156, #132878, #197666, #37664 ) ) ;
#173713 = VECTOR ( 'NONE', #221563, 1000.000000000000000 ) ;
#173714 = FACE_OUTER_BOUND ( 'NONE', #89447, .T. ) ;
#173715 = ADVANCED_FACE ( 'NONE', ( #150035 ), #68417, .F. ) ;
#173716 = ORIENTED_EDGE ( 'NONE', *, *, #242148, .T. ) ;
#173717 = AXIS2_PLACEMENT_3D ( 'NONE', #181392, #1426, #60114 ) ;
#173718 = AXIS2_PLACEMENT_3D ( 'NONE', #136788, #234615, #76819 ) ;
#173719 = ADVANCED_FACE ( 'NONE', ( #144863 ), #44622, .T. ) ;
#173720 = CARTESIAN_POINT ( 'NONE',  ( 21.05000000000000071, 8.826429739528350638, -108.9140547129437380 ) ) ;
#173721 = EDGE_CURVE ( 'NONE', #113, #84120, #164452, .T. ) ;
#173722 = ORIENTED_EDGE ( 'NONE', *, *, #176930, .T. ) ;
#173723 = VERTEX_POINT ( 'NONE', #125320 ) ;
#173724 = LINE ( 'NONE', #134522, #125327 ) ;
#173725 = VECTOR ( 'NONE', #90993, 1000.000000000000000 ) ;
#173727 = ORIENTED_EDGE ( 'NONE', *, *, #35103, .F. ) ;
#173726 = CARTESIAN_POINT ( 'NONE',  ( -16.97683809663752186, 9.950000000011138823, -120.5976359818037196 ) ) ;
#173728 = CARTESIAN_POINT ( 'NONE',  ( 18.57071067811864040, 10.17928932189250091, -88.25000000000005684 ) ) ;
#173729 = DIRECTION ( 'NONE',  ( 1.000000000000000000, 0.000000000000000000, 0.000000000000000000 ) ) ;
#173730 = CARTESIAN_POINT ( 'NONE',  ( 20.95325940946048249, 65.47660992931579926, -128.9586453552842897 ) ) ;
#173731 = FACE_OUTER_BOUND ( 'NONE', #60299, .T. ) ;
#173732 = CARTESIAN_POINT ( 'NONE',  ( -18.59999999999999787, -1.164121893241208960, -41.41484808557160591 ) ) ;
#173733 = DIRECTION ( 'NONE',  ( 0.000000000000000000, 0.000000000000000000, -1.000000000000000000 ) ) ;
#173734 = FACE_OUTER_BOUND ( 'NONE', #103657, .T. ) ;
#173735 = CARTESIAN_POINT ( 'NONE',  ( 22.16821283564877021, 33.56853718381600515, -242.6527871905703932 ) ) ;
#173736 = DIRECTION ( 'NONE',  ( 1.000000000000000000, -0.000000000000000000, -0.000000000000000000 ) ) ;
#173737 = CYLINDRICAL_SURFACE ( 'NONE', #82615, 0.09999999999999939493 ) ;
#173738 = CARTESIAN_POINT ( 'NONE',  ( 20.94999999999999929, 6.846123162363745074, -104.2377262668499043 ) ) ;
#173739 = VECTOR ( 'NONE', #60236, 1000.000000000000000 ) ;
#173740 = ORIENTED_EDGE ( 'NONE', *, *, #35076, .F. ) ;
#173741 = EDGE_CURVE ( 'NONE', #87859, #242592, #26229, .T. ) ;
#173743 = ADVANCED_FACE ( 'NONE', ( #147444 ), #86155, .F. ) ;
#173742 = VECTOR ( 'NONE', #12640, 1000.000000000000114 ) ;
#173746 = VERTEX_POINT ( 'NONE', #104435 ) ;
#173745 = ORIENTED_EDGE ( 'NONE', *, *, #14181, .T. ) ;
#173744 = VECTOR ( 'NONE', #72065, 1000.000000000000000 ) ;
#173747 = VERTEX_POINT ( 'NONE', #229563 ) ;
#173748 = AXIS2_PLACEMENT_3D ( 'NONE', #252113, #232592, #197282 ) ;
#173749 = DIRECTION ( 'NONE',  ( -0.000000000000000000, 0.2617529984165031243, 0.9651348961777157509 ) ) ;
#173750 = DIRECTION ( 'NONE',  ( -1.020425574104004196E-15, 6.982962677686266711E-15, -1.000000000000000000 ) ) ;
#173751 = AXIS2_PLACEMENT_3D ( 'NONE', #12942, #11650, #209837 ) ;
#173752 = VECTOR ( 'NONE', #64322, 1000.000000000000114 ) ;
#173754 = LINE ( 'NONE', #13345, #44657 ) ;
#173753 = DIRECTION ( 'NONE',  ( 1.000000000000000000, 0.000000000000000000, 0.000000000000000000 ) ) ;
#173755 = ORIENTED_EDGE ( 'NONE', *, *, #221902, .T. ) ;
#173756 = ORIENTED_EDGE ( 'NONE', *, *, #219693, .T. ) ;
#173757 = ADVANCED_FACE ( 'NONE', ( #206138 ), #27540, .T. ) ;
#173758 = DIRECTION ( 'NONE',  ( 0.000000000000000000, -1.000000000000000000, 0.000000000000000000 ) ) ;
#173759 = CARTESIAN_POINT ( 'NONE',  ( -18.39999999999999858, -9.599999999988849453, -207.6001893912220169 ) ) ;
#173760 = EDGE_CURVE ( 'NONE', #178267, #248809, #173662, .T. ) ;
#173761 = DIRECTION ( 'NONE',  ( 0.000000000000000000, 0.000000000000000000, -1.000000000000000000 ) ) ;
#173762 = ORIENTED_EDGE ( 'NONE', *, *, #182879, .F. ) ;
#173763 = ORIENTED_EDGE ( 'NONE', *, *, #73889, .T. ) ;
#173764 = AXIS2_PLACEMENT_3D ( 'NONE', #120165, #41898, #82244 ) ;
#173765 = CARTESIAN_POINT ( 'NONE',  ( -23.15000000000000213, -9.499999999988848032, -43.39396912265245021 ) ) ;
#173766 = CIRCLE ( 'NONE', #23896, 0.09999999999998898659 ) ;
#173767 = DIRECTION ( 'NONE',  ( 1.000000000000000000, 0.000000000000000000, 0.000000000000000000 ) ) ;
#173768 = ORIENTED_EDGE ( 'NONE', *, *, #156479, .F. ) ;
#173769 = DIRECTION ( 'NONE',  ( 0.000000000000000000, 0.000000000000000000, 1.000000000000000000 ) ) ;
#173771 = EDGE_LOOP ( 'NONE', ( #60142, #69612, #103, #122380 ) ) ;
#173770 = CARTESIAN_POINT ( 'NONE',  ( 18.40916198585723151, 77.13860745477401792, -241.8264963619319872 ) ) ;
#173772 = CARTESIAN_POINT ( 'NONE',  ( 23.24999999999999645, 67.17743825834565996, -123.8731074845243683 ) ) ;
#173773 = ADVANCED_FACE ( 'NONE', ( #207438 ), #189140, .F. ) ;
#173774 = CARTESIAN_POINT ( 'NONE',  ( -21.05000000000000071, 69.70000000001266471, -203.4231074845244223 ) ) ;
#173775 = DIRECTION ( 'NONE',  ( 1.000000000000000000, 0.000000000000000000, 0.000000000000000000 ) ) ;
#173776 = ORIENTED_EDGE ( 'NONE', *, *, #30916, .T. ) ;
#173777 = DIRECTION ( 'NONE',  ( -1.000000000000000000, -0.000000000000000000, -0.000000000000000000 ) ) ;
#173778 = ADVANCED_FACE ( 'NONE', ( #169626 ), #50884, .F. ) ;
#173779 = DIRECTION ( 'NONE',  ( -0.000000000000000000, -1.000000000000000000, 6.308085367188393199E-16 ) ) ;
#173781 = CARTESIAN_POINT ( 'NONE',  ( 18.49999999999999289, 6.846123162363745074, -70.73772626684986164 ) ) ;
#173780 = DIRECTION ( 'NONE',  ( 0.000000000000000000, 0.000000000000000000, 1.000000000000000000 ) ) ;
#173782 = DIRECTION ( 'NONE',  ( -2.827886303505249259E-16, 0.8660254037844412611, 0.4999999999999956701 ) ) ;
#173783 = AXIS2_PLACEMENT_3D ( 'NONE', #161153, #240676, #141576 ) ;
#173785 = EDGE_CURVE ( 'NONE', #23430, #94061, #184001, .T. ) ;
#173784 = DIRECTION ( 'NONE',  ( 0.000000000000000000, 0.4088369013363783999, -0.9126074666063545004 ) ) ;
#173786 = CARTESIAN_POINT ( 'NONE',  ( 18.60000000000000142, 85.52394631233008226, -163.1410794891860974 ) ) ;
#173787 = LINE ( 'NONE', #13380, #243321 ) ;
#173788 = VERTEX_POINT ( 'NONE', #250393 ) ;
#173789 = CIRCLE ( 'NONE', #252823, 0.3999999999999952482 ) ;
#173790 = VERTEX_POINT ( 'NONE', #153921 ) ;
#173791 = DIRECTION ( 'NONE',  ( 0.000000000000000000, -0.8814952561688425003, 0.4721928772777359007 ) ) ;
#173792 = CARTESIAN_POINT ( 'NONE',  ( -21.95218792049438861, 75.90097156021228386, -143.7246150457709746 ) ) ;
#173793 = ORIENTED_EDGE ( 'NONE', *, *, #144813, .F. ) ;
#173794 = ADVANCED_FACE ( 'NONE', ( #174761 ), #156470, .F. ) ;
#173795 = DIRECTION ( 'NONE',  ( 0.000000000000000000, 1.000000000000000000, -1.224646799147353207E-16 ) ) ;
#173796 = VECTOR ( 'NONE', #134157, 1000.000000000000000 ) ;
#173797 = TOROIDAL_SURFACE ( 'NONE', #15543, 0.2000000000000000111, 0.1000000000000000056 ) ;
#173798 = ORIENTED_EDGE ( 'NONE', *, *, #227585, .F. ) ;
#173799 = EDGE_CURVE ( 'NONE', #36655, #169538, #32360, .T. ) ;
#173800 =( NAMED_UNIT ( * ) SI_UNIT ( $, .STERADIAN. ) SOLID_ANGLE_UNIT ( ) );
#173801 = AXIS2_PLACEMENT_3D ( 'NONE', #101852, #100559, #86136 ) ;
#173802 = AXIS2_PLACEMENT_3D ( 'NONE', #188786, #124977, #167981 ) ;
#173803 = ORIENTED_EDGE ( 'NONE', *, *, #46805, .T. ) ;
#173804 = DIRECTION ( 'NONE',  ( -0.000000000000000000, 1.000000000000000000, 6.982962677686267499E-15 ) ) ;
#173805 = ORIENTED_EDGE ( 'NONE', *, *, #42375, .T. ) ;
#173806 = AXIS2_PLACEMENT_3D ( 'NONE', #81893, #44093, #186176 ) ;
#173807 = FACE_OUTER_BOUND ( 'NONE', #65740, .T. ) ;
#173808 = SPHERICAL_SURFACE ( 'NONE', #115846, 0.1000000000000000056 ) ;
#173809 = DIRECTION ( 'NONE',  ( -1.000000000000000000, -2.952720810173289112E-16, 0.000000000000000000 ) ) ;
#173810 = CARTESIAN_POINT ( 'NONE',  ( 18.42555734704284731, 85.49715836194880580, -129.4832769867893205 ) ) ;
#173811 = CARTESIAN_POINT ( 'NONE',  ( 21.05000000000000071, 7.554435330547283556, -235.6868924355707691 ) ) ;
#173813 = EDGE_LOOP ( 'NONE', ( #141420, #155142, #114341, #229239 ) ) ;
#173812 = CARTESIAN_POINT ( 'NONE',  ( -16.87683809663752399, 29.62235354460948500, -234.5896431630760617 ) ) ;
#173815 = DIRECTION ( 'NONE',  ( 0.000000000000000000, -1.000000000000000000, -8.609265936414504429E-15 ) ) ;
#173814 = CARTESIAN_POINT ( 'NONE',  ( 23.24999999999999289, 45.21086124044690280, -238.4331873168094091 ) ) ;
#173816 = DIRECTION ( 'NONE',  ( 1.000000000000000000, 0.000000000000000000, 0.000000000000000000 ) ) ;
#173817 = FACE_OUTER_BOUND ( 'NONE', #49028, .T. ) ;
#173818 = CARTESIAN_POINT ( 'NONE',  ( 20.04142135623730070, 11.65000000001115943, -155.3500000000000227 ) ) ;
#173819 = DIRECTION ( 'NONE',  ( -1.000000000000000000, 0.000000000000000000, 0.000000000000000000 ) ) ;
#173821 = EDGE_LOOP ( 'NONE', ( #206347, #49897, #25580, #71476 ) ) ;
#173820 = CIRCLE ( 'NONE', #39939, 4.000000000000000000 ) ;
#173822 = AXIS2_PLACEMENT_3D ( 'NONE', #231880, #70247, #130170 ) ;
#173823 = DIRECTION ( 'NONE',  ( 0.000000000000000000, 0.9126074666063773710, 0.4088369013363274962 ) ) ;
#173824 = ORIENTED_EDGE ( 'NONE', *, *, #231933, .F. ) ;
#173825 = VERTEX_POINT ( 'NONE', #131732 ) ;
#173826 = DIRECTION ( 'NONE',  ( 1.000000000000000000, -3.965082230804126670E-15, 0.000000000000000000 ) ) ;
#173827 = DIRECTION ( 'NONE',  ( 0.000000000000000000, 6.938893903907222067E-15, -1.000000000000000000 ) ) ;
#173828 = ORIENTED_EDGE ( 'NONE', *, *, #67912, .T. ) ;
#173829 = ORIENTED_EDGE ( 'NONE', *, *, #183240, .T. ) ;
#173830 = CARTESIAN_POINT ( 'NONE',  ( -20.15000000000000568, 66.70857864377528301, -191.2731074845244166 ) ) ;
#173831 = CARTESIAN_POINT ( 'NONE',  ( 23.14999999999998437, 38.31471387215685809, -253.2472229410012687 ) ) ;
#173832 = CARTESIAN_POINT ( 'NONE',  ( 20.87600722750343252, 65.66887361445387228, -164.4329845918269939 ) ) ;
#173833 = LINE ( 'NONE', #36875, #232091 ) ;
#173834 = EDGE_CURVE ( 'NONE', #41988, #94854, #200164, .T. ) ;
#173836 = LINE ( 'NONE', #194662, #8560 ) ;
#173835 = DIRECTION ( 'NONE',  ( 0.000000000000000000, 0.000000000000000000, 1.000000000000000000 ) ) ;
#173837 = CIRCLE ( 'NONE', #248816, 0.1000000000000000611 ) ;
#173838 = AXIS2_PLACEMENT_3D ( 'NONE', #174444, #71463, #231813 ) ;
#173839 = CARTESIAN_POINT ( 'NONE',  ( 21.07971444708685738, 6.329792081637700463, -167.4121765636820669 ) ) ;
#173841 = VECTOR ( 'NONE', #117759, 1000.000000000000000 ) ;
#173840 = CARTESIAN_POINT ( 'NONE',  ( 21.04999999999999716, 65.37127968600751160, -90.87310748452436826 ) ) ;
#173842 = VECTOR ( 'NONE', #212570, 1000.000000000000000 ) ;
#173843 = DIRECTION ( 'NONE',  ( -1.000000000000000000, -1.836970198721029934E-16, 0.000000000000000000 ) ) ;
#173844 = ORIENTED_EDGE ( 'NONE', *, *, #44470, .T. ) ;
#173845 = DIRECTION ( 'NONE',  ( 1.000000000000000000, 7.492892343619937423E-30, -1.073024830501117725E-15 ) ) ;
#173847 = EDGE_LOOP ( 'NONE', ( #4443, #145643, #195917, #248437 ) ) ;
#173846 = DIRECTION ( 'NONE',  ( 1.000000000000000000, 0.000000000000000000, 0.000000000000000000 ) ) ;
#173848 = DIRECTION ( 'NONE',  ( 0.000000000000000000, -1.000000000000000000, -6.982962677686265922E-15 ) ) ;
#173849 = DIRECTION ( 'NONE',  ( 1.000000000000000000, -0.000000000000000000, 0.000000000000000000 ) ) ;
#173851 = CARTESIAN_POINT ( 'NONE',  ( -18.69999999999999929, -8.350000000000004974, 10.52591260281975138 ) ) ;
#173850 = DIRECTION ( 'NONE',  ( 0.7071067811865474617, 0.7071067811865474617, 0.000000000000000000 ) ) ;
#173852 = EDGE_CURVE ( 'NONE', #255984, #177874, #170915, .T. ) ;
#173853 = VERTEX_POINT ( 'NONE', #75634 ) ;
#173854 = CARTESIAN_POINT ( 'NONE',  ( 23.25000000000000355, 98.45632476063556737, -196.7292090367925823 ) ) ;
#173855 = DIRECTION ( 'NONE',  ( -0.000000000000000000, 0.000000000000000000, 1.000000000000000000 ) ) ;
#173856 = DIRECTION ( 'NONE',  ( 0.000000000000000000, 0.9770955615653388326, 0.2128009952263264781 ) ) ;
#173857 = DIRECTION ( 'NONE',  ( -0.000000000000000000, 6.938893903907270030E-14, 1.000000000000000000 ) ) ;
#173858 = CARTESIAN_POINT ( 'NONE',  ( -23.15000000000000213, 64.35000000001222986, -148.7731074845244450 ) ) ;
#173859 = ORIENTED_EDGE ( 'NONE', *, *, #107210, .T. ) ;
#173860 = PLANE ( 'NONE',  #88803 ) ;
#173862 = EDGE_CURVE ( 'NONE', #127795, #106375, #115509, .T. ) ;
#173861 = ORIENTED_EDGE ( 'NONE', *, *, #65097, .F. ) ;
#173863 = VECTOR ( 'NONE', #62607, 1000.000000000000000 ) ;
#173865 = AXIS2_PLACEMENT_3D ( 'NONE', #110632, #11550, #231887 ) ;
#173864 = CARTESIAN_POINT ( 'NONE',  ( -20.85000000000000142, 1.115600667400684642E-11, -134.0000000000000284 ) ) ;
#173866 = EDGE_LOOP ( 'NONE', ( #55649, #118988, #173656, #111205 ) ) ;
#173867 = CARTESIAN_POINT ( 'NONE',  ( -20.91682497891422798, 46.43483777265581836, -243.0774829958280918 ) ) ;
#173868 = ORIENTED_EDGE ( 'NONE', *, *, #243343, .T. ) ;
#173870 = CARTESIAN_POINT ( 'NONE',  ( -23.25000000000000000, 71.75000000001156764, -57.37310748452435405 ) ) ;
#173869 = AXIS2_PLACEMENT_3D ( 'NONE', #237715, #42103, #176475 ) ;
#173871 = DIRECTION ( 'NONE',  ( 0.000000000000000000, 0.8660254037844419273, -0.4999999999999942824 ) ) ;
#173872 = EDGE_CURVE ( 'NONE', #253910, #113736, #119636, .T. ) ;
#173873 = ADVANCED_FACE ( 'NONE', ( #16933, #191741, #91334 ), #113451, .T. ) ;
#173874 = EDGE_LOOP ( 'NONE', ( #66816, #43387, #56850, #154037 ) ) ;
#173875 = CARTESIAN_POINT ( 'NONE',  ( -16.97683810757273193, 9.949999999999983302, -13.26357671246047687 ) ) ;
#173876 = DIRECTION ( 'NONE',  ( 0.000000000000000000, -0.2128009952263485993, 0.9770955615653341697 ) ) ;
#173877 = CARTESIAN_POINT ( 'NONE',  ( -21.05000000000000071, 1.162701749949165642, -41.50000000000000000 ) ) ;
#173878 = DIRECTION ( 'NONE',  ( 1.000000000000000000, 0.000000000000000000, 0.000000000000000000 ) ) ;
#173879 = CARTESIAN_POINT ( 'NONE',  ( -16.94445028196807002, 66.00793639031427062, -115.6304376629428106 ) ) ;
#173880 = ORIENTED_EDGE ( 'NONE', *, *, #248339, .T. ) ;
#173881 = CARTESIAN_POINT ( 'NONE',  ( -18.39999999999999858, 85.50000000001210765, -129.9229180933022576 ) ) ;
#173882 = VERTEX_POINT ( 'NONE', #151318 ) ;
#173884 = ORIENTED_EDGE ( 'NONE', *, *, #245442, .F. ) ;
#173883 = DIRECTION ( 'NONE',  ( -1.000000000000000000, 0.000000000000000000, 0.000000000000000000 ) ) ;
#173885 = VERTEX_POINT ( 'NONE', #133031 ) ;
#173886 = CARTESIAN_POINT ( 'NONE',  ( 18.50000000000000000, 85.40000000001263913, -196.2258477248609836 ) ) ;
#173887 = ADVANCED_FACE ( 'NONE', ( #33967 ), #14384, .F. ) ;
#173888 = DIRECTION ( 'NONE',  ( -3.469446951953515108E-14, 0.000000000000000000, -1.000000000000000000 ) ) ;
#173889 = CARTESIAN_POINT ( 'NONE',  ( 22.59080734064468032, 11.75000000000000000, 0.03074970809707019623 ) ) ;
#173890 = CARTESIAN_POINT ( 'NONE',  ( -22.50000000000094147, 75.89914163091312105, -81.27267460801373034 ) ) ;
#173891 = VERTEX_POINT ( 'NONE', #213836 ) ;
#173892 = DIRECTION ( 'NONE',  ( 1.000000000000000000, 0.000000000000000000, 0.000000000000000000 ) ) ;
#173893 = CIRCLE ( 'NONE', #223696, 0.1000000000000028644 ) ;
#173894 = CARTESIAN_POINT ( 'NONE',  ( 21.00000000000000000, 12.15477401631902232, -210.9923204818763622 ) ) ;
#173895 = ORIENTED_EDGE ( 'NONE', *, *, #249887, .T. ) ;
#173897 = VERTEX_POINT ( 'NONE', #233424 ) ;
#173896 = LINE ( 'NONE', #132151, #221826 ) ;
#173898 = DIRECTION ( 'NONE',  ( 1.000000000000000000, -0.000000000000000000, 0.000000000000000000 ) ) ;
#173899 = EDGE_CURVE ( 'NONE', #20074, #166706, #230858, .T. ) ;
#173900 = AXIS2_PLACEMENT_3D ( 'NONE', #223508, #224794, #128291 ) ;
#173901 = CARTESIAN_POINT ( 'NONE',  ( -20.94999999999999929, 74.16465844978787914, -158.4679561919613775 ) ) ;
#173902 = AXIS2_PLACEMENT_3D ( 'NONE', #41439, #182220, #160105 ) ;
#173903 = ORIENTED_EDGE ( 'NONE', *, *, #102361, .T. ) ;
#173904 = VECTOR ( 'NONE', #247447, 1000.000000000000000 ) ;
#173905 = ORIENTED_EDGE ( 'NONE', *, *, #137171, .F. ) ;
#173906 = PRODUCT_DEFINITION_FORMATION_WITH_SPECIFIED_SOURCE ( 'ANY', '', #257766, .NOT_KNOWN. ) ;
#173907 = CARTESIAN_POINT ( 'NONE',  ( -20.89878130938411616, 18.40663661316795441, -236.9846611508999388 ) ) ;
#173909 = ORIENTED_EDGE ( 'NONE', *, *, #156808, .T. ) ;
#173908 = CIRCLE ( 'NONE', #23854, 4.099999999999992539 ) ;
#173910 = DIRECTION ( 'NONE',  ( -3.265361837132812600E-16, -0.4088369013363246096, 0.9126074666063785923 ) ) ;
#173911 = CIRCLE ( 'NONE', #153061, 0.5000000000000004441 ) ;
#173912 = CARTESIAN_POINT ( 'NONE',  ( 15.66039659514495419, 66.63925083009641526, -52.20853734391710077 ) ) ;
#173913 = DIRECTION ( 'NONE',  ( 0.000000000000000000, 0.000000000000000000, -1.000000000000000000 ) ) ;
#173914 = EDGE_CURVE ( 'NONE', #82512, #244339, #54753, .T. ) ;
#173915 = AXIS2_PLACEMENT_3D ( 'NONE', #250139, #145885, #7685 ) ;
#173916 = AXIS2_PLACEMENT_3D ( 'NONE', #116852, #196378, #138941 ) ;
#173917 = ORIENTED_EDGE ( 'NONE', *, *, #221020, .F. ) ;
#173918 = CARTESIAN_POINT ( 'NONE',  ( 20.93284271247462414, 11.75000000001116085, -59.98519422934605672 ) ) ;
#173919 = ADVANCED_FACE ( 'NONE', ( #252950 ), #96433, .F. ) ;
#173920 = CIRCLE ( 'NONE', #182256, 0.09999999999999939493 ) ;
#173922 = EDGE_CURVE ( 'NONE', #236987, #244761, #234686, .T. ) ;
#173921 = AXIS2_PLACEMENT_3D ( 'NONE', #201502, #22901, #197647 ) ;
#173923 = ORIENTED_EDGE ( 'NONE', *, *, #22318, .F. ) ;
#173924 = CIRCLE ( 'NONE', #15692, 0.5000000000000005551 ) ;
#173925 = DIRECTION ( 'NONE',  ( 1.000000000000000000, 0.000000000000000000, 0.000000000000000000 ) ) ;
#173926 = CARTESIAN_POINT ( 'NONE',  ( -16.91256925476571027, 9.985731158139330432, -79.53235751099477113 ) ) ;
#173928 = ORIENTED_EDGE ( 'NONE', *, *, #75555, .F. ) ;
#173927 = SPHERICAL_SURFACE ( 'NONE', #224961, 0.1000000000000000056 ) ;
#173929 = DIRECTION ( 'NONE',  ( -0.000000000000000000, -0.000000000000000000, 1.000000000000000000 ) ) ;
#173930 = CYLINDRICAL_SURFACE ( 'NONE', #86595, 11.74999999999999645 ) ;
#173932 = EDGE_CURVE ( 'NONE', #53335, #176751, #227962, .T. ) ;
#173931 = DIRECTION ( 'NONE',  ( 0.000000000000000000, 0.000000000000000000, 1.000000000000000000 ) ) ;
#173934 = EDGE_CURVE ( 'NONE', #45881, #108241, #110885, .T. ) ;
#173933 = DIRECTION ( 'NONE',  ( 1.000000000000000000, 0.000000000000000000, 0.000000000000000000 ) ) ;
#173935 = FACE_OUTER_BOUND ( 'NONE', #69132, .T. ) ;
#173936 = CYLINDRICAL_SURFACE ( 'NONE', #10023, 0.1000000000000001443 ) ;
#173937 = CARTESIAN_POINT ( 'NONE',  ( -20.64999999999999858, 7.250000000011155521, -79.25000000000004263 ) ) ;
#173939 = VERTEX_POINT ( 'NONE', #11817 ) ;
#173938 = CARTESIAN_POINT ( 'NONE',  ( -13.39999999999994529, 64.35000000001120668, -23.72310748452479245 ) ) ;
#173940 = EDGE_CURVE ( 'NONE', #80924, #131461, #2472, .T. ) ;
#173941 = EDGE_CURVE ( 'NONE', #94115, #197918, #152979, .T. ) ;
#173942 = CIRCLE ( 'NONE', #182272, 0.5000000000000004441 ) ;
#173945 = EDGE_CURVE ( 'NONE', #216320, #158092, #244508, .T. ) ;
#173944 = ADVANCED_FACE ( 'NONE', ( #160309 ), #81989, .F. ) ;
#173943 = CIRCLE ( 'NONE', #98836, 0.09999999999998898659 ) ;
#173946 = AXIS2_PLACEMENT_3D ( 'NONE', #60535, #235325, #176665 ) ;
#173947 = DIRECTION ( 'NONE',  ( -0.000000000000000000, 0.9770955615653313941, 0.2128009952263603954 ) ) ;
#173948 = CARTESIAN_POINT ( 'NONE',  ( 18.59999999999999076, 65.79142135624880439, -48.17310748452439384 ) ) ;
#173949 = DIRECTION ( 'NONE',  ( 0.000000000000000000, 0.8700118002898322711, -0.4930308989875231140 ) ) ;
#173950 = ORIENTED_EDGE ( 'NONE', *, *, #6170, .T. ) ;
#173951 = DIRECTION ( 'NONE',  ( -2.602085213965226419E-14, 6.982962677686266711E-15, -1.000000000000000000 ) ) ;
#173952 = EDGE_CURVE ( 'NONE', #119072, #40566, #7170, .T. ) ;
#173953 = DIRECTION ( 'NONE',  ( 0.000000000000000000, 0.000000000000000000, -1.000000000000000000 ) ) ;
#173954 = AXIS2_PLACEMENT_3D ( 'NONE', #28786, #250349, #27496 ) ;
#173955 = CARTESIAN_POINT ( 'NONE',  ( 23.25000000000000000, -11.64999999998884483, -33.50000000000000000 ) ) ;
#173957 = ORIENTED_EDGE ( 'NONE', *, *, #243618, .T. ) ;
#173956 = CIRCLE ( 'NONE', #215583, 0.1000000000000004496 ) ;
#173958 = EDGE_CURVE ( 'NONE', #30387, #182622, #207124, .T. ) ;
#173959 = ADVANCED_FACE ( 'NONE', ( #237259 ), #3774, .T. ) ;
#173960 = CARTESIAN_POINT ( 'NONE',  ( -20.85000000000000142, 78.06784868750165174, -195.8985418047209350 ) ) ;
#173961 = CARTESIAN_POINT ( 'NONE',  ( -16.94062896051973865, 9.992719105111833144, -79.60251654211884897 ) ) ;
#173962 = EDGE_CURVE ( 'NONE', #172562, #48651, #198724, .T. ) ;
#173963 = ORIENTED_EDGE ( 'NONE', *, *, #90233, .F. ) ;
#173964 = CARTESIAN_POINT ( 'NONE',  ( -18.40000000000000213, 65.06382255409391746, -210.1412732845728897 ) ) ;
#173965 = ORIENTED_EDGE ( 'NONE', *, *, #149391, .T. ) ;
#173966 = EDGE_LOOP ( 'NONE', ( #188792, #75825, #147803, #67466 ) ) ;
#173967 = EDGE_CURVE ( 'NONE', #253024, #22668, #39072, .T. ) ;
#173968 = AXIS2_PLACEMENT_3D ( 'NONE', #86345, #100143, #256622 ) ;
#173969 = CARTESIAN_POINT ( 'NONE',  ( 22.50000000000000000, 68.25000000001236344, -170.1231074845244109 ) ) ;
#173970 = ORIENTED_EDGE ( 'NONE', *, *, #15605, .T. ) ;
#173971 = DIRECTION ( 'NONE',  ( 1.000000000000000000, -0.000000000000000000, -0.000000000000000000 ) ) ;
#173972 = VECTOR ( 'NONE', #113437, 1000.000000000000000 ) ;
#173973 = AXIS2_PLACEMENT_3D ( 'NONE', #156116, #120839, #179518 ) ;
#173974 = ORIENTED_EDGE ( 'NONE', *, *, #134636, .F. ) ;
#173976 = ORIENTED_EDGE ( 'NONE', *, *, #166267, .T. ) ;
#173975 = ORIENTED_EDGE ( 'NONE', *, *, #167549, .T. ) ;
#173977 = CARTESIAN_POINT ( 'NONE',  ( -18.59999999999999787, 7.675662554762638479, -241.7139905447625381 ) ) ;
#173978 = AXIS2_PLACEMENT_3D ( 'NONE', #234140, #157212, #214575 ) ;
#173980 = VERTEX_POINT ( 'NONE', #161589 ) ;
#173979 = CARTESIAN_POINT ( 'NONE',  ( 15.52844286134408058, 9.375669526436928081, -49.36779000938593498 ) ) ;
#173981 = CARTESIAN_POINT ( 'NONE',  ( 20.89878130938411616, 65.67252876774509218, -63.94570419949945261 ) ) ;
#173982 = ORIENTED_EDGE ( 'NONE', *, *, #103304, .T. ) ;
#173983 = AXIS2_PLACEMENT_3D ( 'NONE', #244535, #204121, #142849 ) ;
#173984 = ORIENTED_EDGE ( 'NONE', *, *, #164262, .T. ) ;
#173985 = DIRECTION ( 'NONE',  ( -0.000000000000000000, 0.000000000000000000, 1.000000000000000000 ) ) ;
#173986 = DIRECTION ( 'NONE',  ( 0.000000000000000000, -0.000000000000000000, 1.000000000000000000 ) ) ;
#173987 = CARTESIAN_POINT ( 'NONE',  ( 20.94999999999999929, 4.813084112149524252, -11.94151775652382419 ) ) ;
#173988 = ORIENTED_EDGE ( 'NONE', *, *, #2031, .T. ) ;
#173989 = DIRECTION ( 'NONE',  ( 1.020425574104004196E-15, -6.982962677686266711E-15, 1.000000000000000000 ) ) ;
#173990 = DIRECTION ( 'NONE',  ( 0.000000000000000000, 0.9126074666063805907, 0.4088369013363201132 ) ) ;
#173991 = CARTESIAN_POINT ( 'NONE',  ( -18.79999999999999716, -1.885425182446133885, -11.49641995933507843 ) ) ;
#173992 = VECTOR ( 'NONE', #106140, 1000.000000000000000 ) ;
#173993 = ORIENTED_EDGE ( 'NONE', *, *, #98559, .T. ) ;
#173994 = FACE_OUTER_BOUND ( 'NONE', #167274, .T. ) ;
#173995 = CARTESIAN_POINT ( 'NONE',  ( -18.44204374631829424, 38.01828962671714862, -261.0463112980073674 ) ) ;
#173996 = DIRECTION ( 'NONE',  ( 0.000000000000000000, -7.056502275159894776E-15, 1.000000000000000000 ) ) ;
#173997 = ORIENTED_EDGE ( 'NONE', *, *, #52047, .T. ) ;
#173998 = CARTESIAN_POINT ( 'NONE',  ( 21.05000000000000071, 87.29603075034795268, -200.4752083248604038 ) ) ;
#173999 = ORIENTED_EDGE ( 'NONE', *, *, #226229, .F. ) ;
#174001 = EDGE_LOOP ( 'NONE', ( #95795, #179935, #11327, #19216 ) ) ;
#174000 = CIRCLE ( 'NONE', #228131, 0.09999999999999939493 ) ;
#174002 = CARTESIAN_POINT ( 'NONE',  ( 20.95512820512820440, 65.37615131630076348, -195.8581939154368285 ) ) ;
#174003 = ORIENTED_EDGE ( 'NONE', *, *, #43926, .F. ) ;
#174004 = ORIENTED_EDGE ( 'NONE', *, *, #20214, .F. ) ;
#174005 = DIRECTION ( 'NONE',  ( -0.000000000000000000, 1.000000000000000000, -0.000000000000000000 ) ) ;
#174006 = CARTESIAN_POINT ( 'NONE',  ( -18.59999999999999787, 0.000000000000000000, -33.50000000000000000 ) ) ;
#174007 = ORIENTED_EDGE ( 'NONE', *, *, #149282, .F. ) ;
#174008 = ORIENTED_EDGE ( 'NONE', *, *, #26756, .T. ) ;
#174009 = FACE_OUTER_BOUND ( 'NONE', #252610, .T. ) ;
#174010 = DIRECTION ( 'NONE',  ( -1.000000000000000000, 0.000000000000000000, 0.000000000000000000 ) ) ;
#174011 = ORIENTED_EDGE ( 'NONE', *, *, #192762, .T. ) ;
#174012 = ADVANCED_FACE ( 'NONE', ( #182429 ), #62477, .F. ) ;
#174013 = AXIS2_PLACEMENT_3D ( 'NONE', #98688, #77870, #177020 ) ;
#174014 = CIRCLE ( 'NONE', #40731, 11.75000000000000000 ) ;
#174015 = ADVANCED_FACE ( 'NONE', ( #196831 ), #73861, .T. ) ;
#174016 = EDGE_LOOP ( 'NONE', ( #125857, #228192, #13855, #100421, #163307 ) ) ;
#174017 = FACE_OUTER_BOUND ( 'NONE', #86535, .T. ) ;
#174018 = EDGE_CURVE ( 'NONE', #143707, #128967, #140453, .T. ) ;
#174019 = DIRECTION ( 'NONE',  ( 1.000000000000000000, 0.000000000000000000, -0.000000000000000000 ) ) ;
#174020 = ADVANCED_FACE ( 'NONE', ( #179862 ), #85127, .T. ) ;
#174021 = CARTESIAN_POINT ( 'NONE',  ( -23.25000000000000000, 6.982009704867601307, -70.69615211825629331 ) ) ;
#174022 = DIRECTION ( 'NONE',  ( -1.000000000000000000, 0.000000000000000000, 0.000000000000000000 ) ) ;
#174023 = CARTESIAN_POINT ( 'NONE',  ( -20.54999999999999716, 7.249999999999999112, -12.25000000000000000 ) ) ;
#174024 = DIRECTION ( 'NONE',  ( 0.000000000000000000, 1.000000000000000000, 0.000000000000000000 ) ) ;
#174025 = CARTESIAN_POINT ( 'NONE',  ( 22.47071067811865319, 7.522163794833003791, -199.2603376134759117 ) ) ;
#174028 = FACE_OUTER_BOUND ( 'NONE', #119113, .T. ) ;
#174027 = AXIS2_PLACEMENT_3D ( 'NONE', #199247, #240934, #38891 ) ;
#174026 = FACE_OUTER_BOUND ( 'NONE', #243213, .T. ) ;
#174029 = CARTESIAN_POINT ( 'NONE',  ( -21.05000000000000071, -11.64999999998884483, -103.4000000000000341 ) ) ;
#174030 = DIRECTION ( 'NONE',  ( -2.952720810173288619E-16, 1.000000000000000000, 0.000000000000000000 ) ) ;
#174031 = AXIS2_PLACEMENT_3D ( 'NONE', #248233, #228685, #47438 ) ;
#174032 = CARTESIAN_POINT ( 'NONE',  ( -23.25000000000000000, 76.00000000001213607, -136.5231074845243313 ) ) ;
#174033 = CARTESIAN_POINT ( 'NONE',  ( -21.05000000000000071, 76.10000000001242881, -176.5637644362255969 ) ) ;
#174034 = VERTEX_POINT ( 'NONE', #139410 ) ;
#174035 = ADVANCED_FACE ( 'NONE', ( #218960 ), #121192, .T. ) ;
#174036 = CIRCLE ( 'NONE', #86652, 0.1000000000000124678 ) ;
#174037 = EDGE_CURVE ( 'NONE', #51264, #19031, #220274, .T. ) ;
#174039 = ORIENTED_EDGE ( 'NONE', *, *, #131008, .F. ) ;
#174038 = CARTESIAN_POINT ( 'NONE',  ( 18.59999999999999076, 6.650000000011155876, -88.35000000000003695 ) ) ;
#174040 = DIRECTION ( 'NONE',  ( 0.000000000000000000, -0.8814952561688476074, 0.4721928772777262417 ) ) ;
#174041 = LINE ( 'NONE', #230113, #244361 ) ;
#174042 = ORIENTED_EDGE ( 'NONE', *, *, #234524, .F. ) ;
#174043 =( NAMED_UNIT ( * ) PLANE_ANGLE_UNIT ( ) SI_UNIT ( $, .RADIAN. ) );
#174044 = EDGE_CURVE ( 'NONE', #235986, #118225, #206339, .T. ) ;
#174045 = CARTESIAN_POINT ( 'NONE',  ( 20.94999999999999929, 10.29288807859936838, -206.4580020160121592 ) ) ;
#174046 = AXIS2_PLACEMENT_3D ( 'NONE', #137143, #120186, #216674 ) ;
#174047 = ADVANCED_FACE ( 'NONE', ( #44200 ), #165427, .T. ) ;
#174048 = CARTESIAN_POINT ( 'NONE',  ( -23.25000000000000000, 64.25000000001206502, -124.3731074845243825 ) ) ;
#174049 = ORIENTED_EDGE ( 'NONE', *, *, #54348, .F. ) ;
#174050 = VECTOR ( 'NONE', #8146, 1000.000000000000000 ) ;
#174051 = DIRECTION ( 'NONE',  ( -1.000000000000000000, 0.000000000000000000, -0.000000000000000000 ) ) ;
#174052 = DIRECTION ( 'NONE',  ( 1.441126678808781001E-14, 0.9316174814283004757, 0.3634403228828503307 ) ) ;
#174053 = FACE_OUTER_BOUND ( 'NONE', #141682, .T. ) ;
#174055 = ORIENTED_EDGE ( 'NONE', *, *, #58797, .T. ) ;
#174054 = CARTESIAN_POINT ( 'NONE',  ( -21.14999999999999858, 11.65000000001115588, -33.50000000000000000 ) ) ;
#174056 = CARTESIAN_POINT ( 'NONE',  ( -16.87683809663752399, 66.15000000001229807, -156.6207434663281219 ) ) ;
#174057 = VECTOR ( 'NONE', #188231, 1000.000000000000000 ) ;
#174058 = EDGE_CURVE ( 'NONE', #61597, #182833, #61357, .T. ) ;
#174060 = ORIENTED_EDGE ( 'NONE', *, *, #152309, .T. ) ;
#174059 = CARTESIAN_POINT ( 'NONE',  ( -18.36527282681991124, 85.50000060000968460, -96.10095852002184813 ) ) ;
#174061 = CARTESIAN_POINT ( 'NONE',  ( 18.59999999999999076, 8.980461154494401299, -187.0187154576991304 ) ) ;
#174062 = DIRECTION ( 'NONE',  ( -1.000000000000000000, -0.000000000000000000, -0.000000000000000000 ) ) ;
#174063 = FACE_OUTER_BOUND ( 'NONE', #111389, .T. ) ;
#174064 = EDGE_CURVE ( 'NONE', #181106, #213843, #240427, .T. ) ;
#174065 = CARTESIAN_POINT ( 'NONE',  ( 20.12500000000000355, 65.75804927292921320, -95.16290375743827212 ) ) ;
#174067 = CARTESIAN_POINT ( 'NONE',  ( -23.15000000000000213, 76.00000000001213607, -136.5231074845243313 ) ) ;
#174066 = CARTESIAN_POINT ( 'NONE',  ( -16.82055514392377304, 9.950000000011137047, -154.8232019254577949 ) ) ;
#174068 = DIRECTION ( 'NONE',  ( 1.000000000000000000, -0.000000000000000000, -0.000000000000000000 ) ) ;
#174070 = EDGE_CURVE ( 'NONE', #207953, #144953, #236324, .T. ) ;
#174069 = FACE_OUTER_BOUND ( 'NONE', #40388, .T. ) ;
#174071 = DIRECTION ( 'NONE',  ( 0.000000000000000000, 0.000000000000000000, 1.000000000000000000 ) ) ;
#174072 = CIRCLE ( 'NONE', #94908, 0.2000000000000057288 ) ;
#174073 = AXIS2_PLACEMENT_3D ( 'NONE', #103448, #3066, #162186 ) ;
#174074 = DIRECTION ( 'NONE',  ( -1.000000000000000000, 0.000000000000000000, 0.000000000000000000 ) ) ;
#174075 = FACE_OUTER_BOUND ( 'NONE', #91431, .T. ) ;
#174076 = TOROIDAL_SURFACE ( 'NONE', #61610, 0.4000000000000005773, 0.1000000000000000056 ) ;
#174077 = VERTEX_POINT ( 'NONE', #222803 ) ;
#174078 = EDGE_CURVE ( 'NONE', #146439, #199102, #82172, .T. ) ;
#174079 = CARTESIAN_POINT ( 'NONE',  ( -20.07928932188135107, 66.77928932189388433, -182.3731074845244393 ) ) ;
#174080 = CIRCLE ( 'NONE', #61613, 0.5000000000000179856 ) ;
#174081 = ORIENTED_EDGE ( 'NONE', *, *, #140754, .T. ) ;
#174082 = EDGE_LOOP ( 'NONE', ( #68748, #33282, #78295, #87028 ) ) ;
#174084 = CARTESIAN_POINT ( 'NONE',  ( -23.15000000000000213, 84.66355140188075268, -59.99900636645695329 ) ) ;
#174083 = CIRCLE ( 'NONE', #98406, 0.2000000000000111688 ) ;
#174085 = CARTESIAN_POINT ( 'NONE',  ( 18.59999999999999076, 69.45000000001188312, -93.00608031408432907 ) ) ;
#174086 = ORIENTED_EDGE ( 'NONE', *, *, #222075, .F. ) ;
#174087 = EDGE_CURVE ( 'NONE', #68761, #119183, #161332, .T. ) ;
#174088 = VERTEX_POINT ( 'NONE', #184980 ) ;
#174089 = EDGE_CURVE ( 'NONE', #15679, #107177, #95069, .T. ) ;
#174090 = DIRECTION ( 'NONE',  ( 0.000000000000000000, -0.4999999999999348299, 0.8660254037844762331 ) ) ;
#174091 = PRESENTATION_STYLE_ASSIGNMENT (( #252278 ) ) ;
#174092 = VECTOR ( 'NONE', #92997, 1000.000000000000114 ) ;
#174093 = ORIENTED_EDGE ( 'NONE', *, *, #13256, .F. ) ;
#174094 = EDGE_LOOP ( 'NONE', ( #238511, #199140, #17447, #233578 ) ) ;
#174096 = FACE_OUTER_BOUND ( 'NONE', #213379, .T. ) ;
#174095 = AXIS2_PLACEMENT_3D ( 'NONE', #226571, #186189, #200614 ) ;
#174097 = CARTESIAN_POINT ( 'NONE',  ( -18.59999999999999787, -1.835341550213255957, -145.5551512925629822 ) ) ;
#174098 = DIRECTION ( 'NONE',  ( 0.000000000000000000, 0.000000000000000000, 1.000000000000000000 ) ) ;
#174099 = CIRCLE ( 'NONE', #203089, 0.09999999999999939493 ) ;
#174100 = CARTESIAN_POINT ( 'NONE',  ( 17.74533788810829904, 10.81849979148195118, -123.6863773250524616 ) ) ;
#174101 = AXIS2_PLACEMENT_3D ( 'NONE', #122272, #218783, #118432 ) ;
#174102 = EDGE_CURVE ( 'NONE', #176861, #243814, #48879, .T. ) ;
#174104 = CARTESIAN_POINT ( 'NONE',  ( 18.39999999999999858, 85.60000000001137721, -29.42291809330221142 ) ) ;
#174103 = CARTESIAN_POINT ( 'NONE',  ( 18.57071067811864040, 51.89016398296629973, -231.5736831079530020 ) ) ;
#174105 = CARTESIAN_POINT ( 'NONE',  ( -22.39999999999999858, 59.71212129423881976, -233.8158665866020272 ) ) ;
#174107 = VERTEX_POINT ( 'NONE', #85842 ) ;
#174106 = CARTESIAN_POINT ( 'NONE',  ( 20.94999999999999929, 5.850000000011105428, -177.6324972242779268 ) ) ;
#174109 = CARTESIAN_POINT ( 'NONE',  ( -20.85000000000000142, -1.263275465217258198, -41.40186466674640542 ) ) ;
#174108 = FACE_OUTER_BOUND ( 'NONE', #42201, .T. ) ;
#174110 = AXIS2_PLACEMENT_3D ( 'NONE', #129953, #70029, #88252 ) ;
#174111 = CARTESIAN_POINT ( 'NONE',  ( -23.15000000000000213, 17.01923898301589944, -224.3994341343041867 ) ) ;
#174112 = ORIENTED_EDGE ( 'NONE', *, *, #199032, .T. ) ;
#174113 = CARTESIAN_POINT ( 'NONE',  ( -23.15000000000000213, 4.350000000011156054, -54.64999999999999858 ) ) ;
#174114 = CARTESIAN_POINT ( 'NONE',  ( -18.39999999999999858, -9.399999999988850163, -21.75000000000000355 ) ) ;
#174115 = ORIENTED_EDGE ( 'NONE', *, *, #221092, .T. ) ;
#174116 = DIRECTION ( 'NONE',  ( -1.000000000000000000, -0.000000000000000000, -0.000000000000000000 ) ) ;
#174117 = AXIS2_PLACEMENT_3D ( 'NONE', #175332, #254785, #198712 ) ;
#174118 = FACE_OUTER_BOUND ( 'NONE', #205086, .T. ) ;
#174119 = AXIS2_PLACEMENT_3D ( 'NONE', #255952, #77349, #78633 ) ;
#174121 = ORIENTED_EDGE ( 'NONE', *, *, #225104, .F. ) ;
#174120 = AXIS2_PLACEMENT_3D ( 'NONE', #90371, #70852, #51223 ) ;
#174122 = EDGE_LOOP ( 'NONE', ( #105888, #154114, #1403, #149712 ) ) ;
#174123 = FACE_OUTER_BOUND ( 'NONE', #214127, .T. ) ;
#174124 = CARTESIAN_POINT ( 'NONE',  ( -22.39999999999999858, -0.1008583690875579364, -55.25043287651065782 ) ) ;
#174125 = FACE_OUTER_BOUND ( 'NONE', #177062, .T. ) ;
#174126 = DIRECTION ( 'NONE',  ( 0.000000000000000000, -0.008583690987162452199, 0.9999631594459053030 ) ) ;
#174127 = EDGE_LOOP ( 'NONE', ( #241015, #216855, #102504, #239769 ) ) ;
#174128 = DIRECTION ( 'NONE',  ( 0.000000000000000000, 1.000000000000000000, 0.000000000000000000 ) ) ;
#174129 = PRESENTATION_LAYER_ASSIGNMENT (  '', '', ( #240721 ) ) ;
#174130 = CARTESIAN_POINT ( 'NONE',  ( -22.59999985501179154, 64.25013020700939137, -170.0887061543239724 ) ) ;
#174131 = AXIS2_PLACEMENT_3D ( 'NONE', #250036, #150941, #27175 ) ;
#174132 = CARTESIAN_POINT ( 'NONE',  ( -18.44085059012131822, 11.51401249349495970, -124.7403053191215747 ) ) ;
#174133 = CARTESIAN_POINT ( 'NONE',  ( 18.59999999999999787, -1.249999999988843369, -175.3004807544151049 ) ) ;
#174134 = CIRCLE ( 'NONE', #99240, 0.1000000000000028644 ) ;
#174135 = CYLINDRICAL_SURFACE ( 'NONE', #167812, 0.09999999999998898659 ) ;
#174136 = CIRCLE ( 'NONE', #203328, 11.80000000000000426 ) ;
#174138 = ORIENTED_EDGE ( 'NONE', *, *, #129670, .T. ) ;
#174137 = DIRECTION ( 'NONE',  ( 0.000000000000000000, 0.000000000000000000, -1.000000000000000000 ) ) ;
#174139 = CARTESIAN_POINT ( 'NONE',  ( 18.60000000000000142, 85.40000000001184333, -95.72584772486095517 ) ) ;
#174140 = DIRECTION ( 'NONE',  ( -2.952720810173289112E-16, -0.9651348961777157509, 0.2617529984165031243 ) ) ;
#174141 = DIRECTION ( 'NONE',  ( 0.000000000000000000, 0.000000000000000000, -1.000000000000000000 ) ) ;
#174142 = DIRECTION ( 'NONE',  ( 0.000000000000000000, -0.6728971962617172897, 0.7397360091702445128 ) ) ;
#174143 = EDGE_CURVE ( 'NONE', #32549, #62345, #23968, .T. ) ;
#174144 = CARTESIAN_POINT ( 'NONE',  ( -20.94999999999999929, 0.000000000000000000, -33.50000000000000000 ) ) ;
#174146 = VERTEX_POINT ( 'NONE', #226659 ) ;
#174145 = DIRECTION ( 'NONE',  ( 0.000000000000000000, 0.2128009952263403282, -0.9770955615653358350 ) ) ;
#174147 = FACE_OUTER_BOUND ( 'NONE', #256044, .T. ) ;
#174148 = CIRCLE ( 'NONE', #124047, 11.80000000000000426 ) ;
#174149 = CARTESIAN_POINT ( 'NONE',  ( -20.90000000000000213, 1.899104650876408451, -11.59795743183152972 ) ) ;
#174150 = CARTESIAN_POINT ( 'NONE',  ( 23.24999999999999645, 70.40000000001150227, -48.42837350343745584 ) ) ;
#174151 = VERTEX_POINT ( 'NONE', #225370 ) ;
#174152 = DIRECTION ( 'NONE',  ( 0.000000000000000000, -0.5954378521545836689, -0.8034013718071036925 ) ) ;
#174153 = CARTESIAN_POINT ( 'NONE',  ( -21.65000000000000213, 9.950000000011140600, -180.2499999999999716 ) ) ;
#174155 = EDGE_CURVE ( 'NONE', #130783, #237011, #169735, .T. ) ;
#174154 = DIRECTION ( 'NONE',  ( -3.265361837132813093E-16, 1.000000000000000000, 0.000000000000000000 ) ) ;
#174157 = EDGE_CURVE ( 'NONE', #51518, #8358, #46737, .T. ) ;
#174156 = AXIS2_PLACEMENT_3D ( 'NONE', #174438, #36178, #93559 ) ;
#174158 = AXIS2_PLACEMENT_3D ( 'NONE', #219582, #95776, #17528 ) ;
#174159 = CARTESIAN_POINT ( 'NONE',  ( 20.94999999999999574, 70.10000000001193143, -92.80400771986793984 ) ) ;
#174160 = CIRCLE ( 'NONE', #236462, 0.09999999999999939493 ) ;
#174161 = VECTOR ( 'NONE', #127779, 1000.000000000000000 ) ;
#174162 = FACE_OUTER_BOUND ( 'NONE', #82699, .T. ) ;
#174163 = ORIENTED_EDGE ( 'NONE', *, *, #105184, .F. ) ;
#174164 = ORIENTED_EDGE ( 'NONE', *, *, #250821, .F. ) ;
#174165 = CARTESIAN_POINT ( 'NONE',  ( -20.85000000000000142, 11.75000000001115197, -160.7161343370219129 ) ) ;
#174166 = CARTESIAN_POINT ( 'NONE',  ( -23.25000000000000000, 76.00000000001165290, -69.52310748452431710 ) ) ;
#174167 = EDGE_CURVE ( 'NONE', #514, #10605, #78097, .T. ) ;
#174168 = CARTESIAN_POINT ( 'NONE',  ( 20.94999999999999929, 7.128833340094563376, -233.7327013124401276 ) ) ;
#174169 = CARTESIAN_POINT ( 'NONE',  ( 20.94999999999999574, 65.57661458509942065, -162.5310555606543232 ) ) ;
#174170 = FACE_OUTER_BOUND ( 'NONE', #238831, .T. ) ;
#174171 = VECTOR ( 'NONE', #119992, 1000.000000000000000 ) ;
#174172 = DIRECTION ( 'NONE',  ( 1.000000000000000000, 2.952720810173289112E-16, -0.000000000000000000 ) ) ;
#174173 = CYLINDRICAL_SURFACE ( 'NONE', #153729, 11.79999999999999538 ) ;
#174174 = AXIS2_PLACEMENT_3D ( 'NONE', #17040, #136963, #216501 ) ;
#174175 = CARTESIAN_POINT ( 'NONE',  ( -20.07928932188135107, 9.220710678129810489, -188.7499999999999716 ) ) ;
#174176 = EDGE_LOOP ( 'NONE', ( #71410, #62029, #165983, #252504, #42384 ) ) ;
#174177 = DIRECTION ( 'NONE',  ( 0.000000000000000000, 1.000000000000000000, -3.469446951953635015E-14 ) ) ;
#174178 = ORIENTED_EDGE ( 'NONE', *, *, #147656, .F. ) ;
#174179 = ORIENTED_EDGE ( 'NONE', *, *, #90356, .T. ) ;
#174180 = EDGE_CURVE ( 'NONE', #136982, #208398, #186452, .T. ) ;
#174181 = DIRECTION ( 'NONE',  ( -0.000000000000000000, 1.000000000000000000, 6.982962677686266711E-15 ) ) ;
#174182 = CARTESIAN_POINT ( 'NONE',  ( 20.90000000000000213, 0.000000000000000000, 0.000000000000000000 ) ) ;
#174183 = ADVANCED_FACE ( 'NONE', ( #49316 ), #94851, .F. ) ;
#174184 = CARTESIAN_POINT ( 'NONE',  ( 21.05000000000000071, 10.42338541491290549, -7.492051923870094221 ) ) ;
#174185 = ORIENTED_EDGE ( 'NONE', *, *, #101413, .F. ) ;
#174186 = DIRECTION ( 'NONE',  ( 1.000000000000000000, 7.049440681616514931E-16, -1.911869773728115948E-16 ) ) ;
#174187 = FILL_AREA_STYLE ('',( #193713 ) ) ;
#174188 = CARTESIAN_POINT ( 'NONE',  ( 18.48197441911473504, 85.51795479471654460, -62.63289584231627316 ) ) ;
#174189 = VERTEX_POINT ( 'NONE', #253921 ) ;
#174190 = CARTESIAN_POINT ( 'NONE',  ( 21.05000000000000071, 1.115600667400684642E-11, -134.0000000000000000 ) ) ;
#174191 = DIRECTION ( 'NONE',  ( 0.000000000000000000, 0.000000000000000000, -1.000000000000000000 ) ) ;
#174193 = EDGE_CURVE ( 'NONE', #106895, #4548, #207309, .T. ) ;
#174192 = CARTESIAN_POINT ( 'NONE',  ( -18.47079683080353973, 85.47166410525711910, -162.9142469435320777 ) ) ;
#174194 = AXIS2_PLACEMENT_3D ( 'NONE', #75981, #133394, #253323 ) ;
#174195 = CIRCLE ( 'NONE', #49245, 0.1000000000000028644 ) ;
#174196 = CIRCLE ( 'NONE', #120577, 0.09999999999999739653 ) ;
#174197 = TOROIDAL_SURFACE ( 'NONE', #7754, 7.791421356237335338, 0.1000000000000000056 ) ;
#174198 = DIRECTION ( 'NONE',  ( -1.000000000000000000, 0.000000000000000000, 0.000000000000000000 ) ) ;
#174199 = ORIENTED_EDGE ( 'NONE', *, *, #162181, .F. ) ;
#174200 = CYLINDRICAL_SURFACE ( 'NONE', #152129, 0.09999999999998898659 ) ;
#174201 = CARTESIAN_POINT ( 'NONE',  ( 22.39999999999999858, 7.790779598384538929, -66.90000000000004832 ) ) ;
#174202 = EDGE_LOOP ( 'NONE', ( #29653, #140079, #222415, #201133, #4556 ) ) ;
#174203 = CARTESIAN_POINT ( 'NONE',  ( 21.14250536705908345, 6.518172176891880554, -134.0000000000000000 ) ) ;
#174204 = DIRECTION ( 'NONE',  ( 0.000000000000000000, 0.000000000000000000, -1.000000000000000000 ) ) ;
#174205 = CARTESIAN_POINT ( 'NONE',  ( 20.85000000000000142, 77.73670573947940454, -91.50568489690056140 ) ) ;
#174206 = ADVANCED_FACE ( 'NONE', ( #132719 ), #229255, .T. ) ;
#174207 = ORIENTED_EDGE ( 'NONE', *, *, #207474, .T. ) ;
#174208 = CIRCLE ( 'NONE', #199114, 11.65000000000000213 ) ;
#174209 = DIRECTION ( 'NONE',  ( 0.000000000000000000, 0.9651348961777157509, -0.2617529984165031243 ) ) ;
#174210 = CARTESIAN_POINT ( 'NONE',  ( -16.87683809663752754, 9.865889849342865503, -147.2674268070695689 ) ) ;
#174211 = EDGE_LOOP ( 'NONE', ( #118887, #173058, #183298, #12641 ) ) ;
#174212 = AXIS2_PLACEMENT_3D ( 'NONE', #144463, #42827, #28436 ) ;
#174213 = EDGE_CURVE ( 'NONE', #56768, #208166, #240601, .T. ) ;
#174214 = ORIENTED_EDGE ( 'NONE', *, *, #142404, .F. ) ;
#174215 = FACE_OUTER_BOUND ( 'NONE', #72191, .T. ) ;
#174216 = CYLINDRICAL_SURFACE ( 'NONE', #208588, 0.09999999999999982514 ) ;
#174218 = ORIENTED_EDGE ( 'NONE', *, *, #22678, .F. ) ;
#174217 = LINE ( 'NONE', #256201, #79024 ) ;
#174219 = DIRECTION ( 'NONE',  ( -0.000000000000000000, 0.3848449534832963370, 0.9229812358755945523 ) ) ;
#174220 = CARTESIAN_POINT ( 'NONE',  ( -16.92507428761700439, 9.950000000011138823, -113.2133974596215893 ) ) ;
#174221 = EDGE_CURVE ( 'NONE', #22954, #118580, #36193, .T. ) ;
#174223 = EDGE_CURVE ( 'NONE', #231873, #255695, #132457, .T. ) ;
#174222 = CARTESIAN_POINT ( 'NONE',  ( -20.92356734117541706, 65.68026841930924320, -130.9725740131889893 ) ) ;
#174224 = CARTESIAN_POINT ( 'NONE',  ( -20.85000000000000142, 18.41524492703432614, -237.0006385043383546 ) ) ;
#174225 = CARTESIAN_POINT ( 'NONE',  ( -20.54999999999999716, 7.150000000011155876, -50.25000000000000000 ) ) ;
#174226 = CARTESIAN_POINT ( 'NONE',  ( -0.8999999999999437339, 64.35000000001120668, -10.02310748452479139 ) ) ;
#174227 = CARTESIAN_POINT ( 'NONE',  ( 20.85000000000000142, 75.83895117929300511, -69.80729732888453043 ) ) ;
#174229 = VERTEX_POINT ( 'NONE', #210967 ) ;
#174228 = DIRECTION ( 'NONE',  ( 0.000000000000000000, -7.304098846218139203E-15, 1.000000000000000000 ) ) ;
#174230 = ORIENTED_EDGE ( 'NONE', *, *, #86956, .F. ) ;
#174232 = CARTESIAN_POINT ( 'NONE',  ( -16.89268316805465986, 66.04827818676933759, -48.66735500597884823 ) ) ;
#174231 = DIRECTION ( 'NONE',  ( -1.000000000000000000, 3.265361837132813093E-16, 2.280189983783949500E-30 ) ) ;
#174234 = EDGE_LOOP ( 'NONE', ( #190898, #57575, #232361, #170995 ) ) ;
#174233 = CARTESIAN_POINT ( 'NONE',  ( 18.59999999999999432, 77.26178616857734482, -161.9366085209788650 ) ) ;
#174235 = TOROIDAL_SURFACE ( 'NONE', #28497, 7.800000000000000711, 0.1000000000000000056 ) ;
#174236 = VERTEX_POINT ( 'NONE', #32357 ) ;
#174237 = CARTESIAN_POINT ( 'NONE',  ( -18.57399277249657032, 10.33112638556969465, -106.0901228926975222 ) ) ;
#174239 = DIRECTION ( 'NONE',  ( 1.000000000000000000, 0.000000000000000000, 0.000000000000000000 ) ) ;
#174238 = AXIS2_PLACEMENT_3D ( 'NONE', #211475, #112384, #191944 ) ;
#174240 = VECTOR ( 'NONE', #154913, 1000.000000000000000 ) ;
#174241 = EDGE_CURVE ( 'NONE', #4255, #85481, #232259, .T. ) ;
#174242 = EDGE_CURVE ( 'NONE', #67087, #134912, #165614, .T. ) ;
#174243 = CARTESIAN_POINT ( 'NONE',  ( -22.50000000000000000, 64.35042919246716053, -103.1231074845243825 ) ) ;
#174244 = CARTESIAN_POINT ( 'NONE',  ( 19.94784844284962944, 11.71308993304009682, -58.20219871729849359 ) ) ;
#174245 = AXIS2_PLACEMENT_3D ( 'NONE', #180235, #290, #22455 ) ;
#174246 = EDGE_CURVE ( 'NONE', #200055, #72387, #219742, .T. ) ;
#174247 = DIRECTION ( 'NONE',  ( 0.000000000000000000, 0.000000000000000000, -1.000000000000000000 ) ) ;
#174248 = DIRECTION ( 'NONE',  ( 0.000000000000000000, 1.000000000000000000, 6.982962677686266711E-15 ) ) ;
#174250 = EDGE_LOOP ( 'NONE', ( #38074, #160429, #83398, #121427 ) ) ;
#174249 = EDGE_CURVE ( 'NONE', #75011, #229956, #99119, .T. ) ;
#174251 = ORIENTED_EDGE ( 'NONE', *, *, #44126, .T. ) ;
#174252 = DIRECTION ( 'NONE',  ( 0.000000000000000000, -0.9651348961777157509, 0.2617529984165031243 ) ) ;
#174253 = VECTOR ( 'NONE', #18673, 999.9999999999998863 ) ;
#174254 = CIRCLE ( 'NONE', #136787, 0.09999999999998712696 ) ;
#174255 = ORIENTED_EDGE ( 'NONE', *, *, #138600, .F. ) ;
#174256 = EDGE_CURVE ( 'NONE', #174426, #194720, #171874, .T. ) ;
#174257 = DIRECTION ( 'NONE',  ( -1.000000000000000000, -0.000000000000000000, -0.000000000000000000 ) ) ;
#174259 = EDGE_CURVE ( 'NONE', #219341, #44711, #74052, .T. ) ;
#174258 = ORIENTED_EDGE ( 'NONE', *, *, #245202, .T. ) ;
#174261 = DIRECTION ( 'NONE',  ( 0.000000000000000000, -0.2617529984165031243, -0.9651348961777157509 ) ) ;
#174260 = TOROIDAL_SURFACE ( 'NONE', #149293, 12.97499999999999609, 0.1000000000000000056 ) ;
#174262 = CIRCLE ( 'NONE', #74300, 0.1999999999999987899 ) ;
#174263 = CARTESIAN_POINT ( 'NONE',  ( -16.94389599338512298, 9.991197989766199328, -79.60764480181029512 ) ) ;
#174264 = EDGE_CURVE ( 'NONE', #71372, #123899, #244878, .T. ) ;
#174265 = ORIENTED_EDGE ( 'NONE', *, *, #164322, .F. ) ;
#174266 = CARTESIAN_POINT ( 'NONE',  ( -13.11924609551135212, 66.56831044948793874, -118.2438174522883116 ) ) ;
#174267 = ORIENTED_EDGE ( 'NONE', *, *, #256793, .F. ) ;
#174268 = DIRECTION ( 'NONE',  ( -1.000000000000000000, -0.000000000000000000, -0.000000000000000000 ) ) ;
#174269 = ORIENTED_EDGE ( 'NONE', *, *, #243030, .F. ) ;
#174270 = ADVANCED_FACE ( 'NONE', ( #154864 ), #165138, .T. ) ;
#174271 = CIRCLE ( 'NONE', #178731, 0.09999999999999520384 ) ;
#174272 = LINE ( 'NONE', #54260, #110652 ) ;
#174273 = EDGE_CURVE ( 'NONE', #201532, #7052, #149052, .T. ) ;
#174274 = FACE_OUTER_BOUND ( 'NONE', #146266, .T. ) ;
#174276 = VERTEX_POINT ( 'NONE', #177000 ) ;
#174275 = EDGE_CURVE ( 'NONE', #131987, #109174, #107327, .T. ) ;
#174277 = FACE_OUTER_BOUND ( 'NONE', #247471, .T. ) ;
#174278 = EDGE_LOOP ( 'NONE', ( #109093, #177957, #216173, #246953, #216618 ) ) ;
#174281 = ORIENTED_EDGE ( 'NONE', *, *, #226337, .F. ) ;
#174280 = PLANE ( 'NONE',  #130458 ) ;
#174279 = DIRECTION ( 'NONE',  ( 0.000000000000000000, -1.000000000000000000, -0.000000000000000000 ) ) ;
#174282 = FACE_OUTER_BOUND ( 'NONE', #56216, .T. ) ;
#174283 = CIRCLE ( 'NONE', #53438, 0.09999999999999939493 ) ;
#174284 = ORIENTED_EDGE ( 'NONE', *, *, #124699, .T. ) ;
#174285 = ORIENTED_EDGE ( 'NONE', *, *, #184144, .F. ) ;
#174286 = CIRCLE ( 'NONE', #203468, 0.09999999999998898659 ) ;
#174287 = CIRCLE ( 'NONE', #70223, 0.09999999999999781286 ) ;
#174289 = DIRECTION ( 'NONE',  ( 0.000000000000000000, 1.000000000000000000, 6.982962677686266711E-15 ) ) ;
#174288 =( BOUNDED_SURFACE ( )  B_SPLINE_SURFACE ( 3, 2, ( 
 ( #69718, #188364, #231361 ),
 ( #149259, #50126, #52693 ),
 ( #132243, #74876, #119110 ),
 ( #56527, #213055, #34463 ),
 ( #113954, #255986, #37023 ),
 ( #233910, #116541, #177820 ),
 ( #193517, #194814, #99507 ),
 ( #137365, #16175, #14887 ) ),
 .UNSPECIFIED., .F., .F., .F. ) 
 B_SPLINE_SURFACE_WITH_KNOTS ( ( 4, 2, 2, 4 ),
 ( 3, 3 ),
 ( 0.0001723339234021445073, 0.0002782939632049938328, 0.0003842540030078432124, 0.0005961740826135418633 ),
 ( 0.000000000000000000, 1.000000000000000000 ),
 .UNSPECIFIED. ) 
 GEOMETRIC_REPRESENTATION_ITEM ( )  RATIONAL_B_SPLINE_SURFACE ( (
 ( 1.000000000000000000, 0.9504532311154628710, 1.000000000000000000),
 ( 1.000000000000000000, 0.9506023220710236865, 1.000000000000000000),
 ( 1.000000000000000000, 0.9395774818181227284, 1.000000000000000000),
 ( 1.000000000000000000, 0.9079328464647767882, 1.000000000000000000),
 ( 1.000000000000000000, 0.8875702416206470158, 1.000000000000000000),
 ( 1.000000000000000000, 0.8205919608038449997, 1.000000000000000000),
 ( 1.000000000000000000, 0.7666842783599741029, 1.000000000000000000),
 ( 1.000000000000000000, 0.7071067811864506503, 1.000000000000000000) ) ) 
 REPRESENTATION_ITEM ( '' )  SURFACE ( )  );
#174290 = ORIENTED_EDGE ( 'NONE', *, *, #143343, .F. ) ;
#174291 = ADVANCED_FACE ( 'NONE', ( #141680 ), #120875, .F. ) ;
#174293 = AXIS2_PLACEMENT_3D ( 'NONE', #62840, #141574, #7184 ) ;
#174292 = CARTESIAN_POINT ( 'NONE',  ( 20.94999999999999929, 76.00000000001172396, -71.42310748452430857 ) ) ;
#174294 = CARTESIAN_POINT ( 'NONE',  ( 21.05000000000000071, 69.69548367074806094, -69.50200417646566109 ) ) ;
#174295 = DIRECTION ( 'NONE',  ( 0.000000000000000000, 0.000000000000000000, -1.000000000000000000 ) ) ;
#174296 = LINE ( 'NONE', #115542, #56064 ) ;
#174297 = DIRECTION ( 'NONE',  ( -1.000000000000000000, -0.000000000000000000, -0.000000000000000000 ) ) ;
#174298 = ORIENTED_EDGE ( 'NONE', *, *, #257091, .F. ) ;
#174299 = DIRECTION ( 'NONE',  ( 1.000000000000000000, 0.000000000000000000, 0.000000000000000000 ) ) ;
#174300 = DIRECTION ( 'NONE',  ( 1.000000000000000000, -0.000000000000000000, -0.000000000000000000 ) ) ;
#174301 = CARTESIAN_POINT ( 'NONE',  ( 18.57399277249656322, 10.33112638556969820, -139.5901228926975080 ) ) ;
#174302 = EDGE_LOOP ( 'NONE', ( #61113, #196742, #94204, #2593 ) ) ;
#174303 = CARTESIAN_POINT ( 'NONE',  ( 21.46681500593092196, 6.700443717232642982, -199.5407148005082547 ) ) ;
#174304 = ORIENTED_EDGE ( 'NONE', *, *, #93877, .F. ) ;
#174306 = CIRCLE ( 'NONE', #215924, 0.1000000000000002554 ) ;
#174305 = DIRECTION ( 'NONE',  ( -1.000000000000000000, -0.000000000000000000, -0.000000000000000000 ) ) ;
#174307 = EDGE_LOOP ( 'NONE', ( #200159, #20008, #171469, #200815 ) ) ;
#174308 = CARTESIAN_POINT ( 'NONE',  ( -20.94999999999999929, -11.64999999998884483, -70.00000000000004263 ) ) ;
#174309 = FACE_OUTER_BOUND ( 'NONE', #91152, .T. ) ;
#174311 = ORIENTED_EDGE ( 'NONE', *, *, #183283, .F. ) ;
#174310 = CARTESIAN_POINT ( 'NONE',  ( -23.15000000000000213, 76.00000000001179501, -81.32310748452431426 ) ) ;
#174312 = DIRECTION ( 'NONE',  ( 0.000000000000000000, 0.000000000000000000, -1.000000000000000000 ) ) ;
#174313 = ORIENTED_EDGE ( 'NONE', *, *, #256841, .T. ) ;
#174314 = CARTESIAN_POINT ( 'NONE',  ( -22.19999999999999929, -11.65000000000000036, 12.09999999999999609 ) ) ;
#174315 = AXIS2_PLACEMENT_3D ( 'NONE', #176026, #76887, #53488 ) ;
#174316 = CARTESIAN_POINT ( 'NONE',  ( -16.80621392010904103, 9.942202577518958861, -113.1895919654167670 ) ) ;
#174317 = CIRCLE ( 'NONE', #220057, 0.09999999999999967248 ) ;
#174318 = ORIENTED_EDGE ( 'NONE', *, *, #140843, .T. ) ;
#174319 = EDGE_CURVE ( 'NONE', #143659, #96682, #212343, .T. ) ;
#174320 = CARTESIAN_POINT ( 'NONE',  ( -21.53699400384953577, 1.355070199499284871E-11, -127.2122882067625653 ) ) ;
#174321 = CARTESIAN_POINT ( 'NONE',  ( 18.49999999999999645, 1.115600667400684642E-11, -33.50000000000000000 ) ) ;
#174322 = AXIS2_PLACEMENT_3D ( 'NONE', #65092, #164208, #222873 ) ;
#174323 = ORIENTED_EDGE ( 'NONE', *, *, #38468, .T. ) ;
#174324 = CARTESIAN_POINT ( 'NONE',  ( 18.59999999999999787, -1.835341550213255957, -45.15515129256298366 ) ) ;
#174325 = EDGE_CURVE ( 'NONE', #62507, #93087, #198902, .T. ) ;
#174326 = ORIENTED_EDGE ( 'NONE', *, *, #17536, .T. ) ;
#174327 = AXIS2_PLACEMENT_3D ( 'NONE', #165036, #86760, #248428 ) ;
#174328 = DIRECTION ( 'NONE',  ( 0.000000000000000000, -0.2617529984165152257, -0.9651348961777124202 ) ) ;
#174329 = DIRECTION ( 'NONE',  ( 0.000000000000000000, -0.03181660087581671820, 0.9994937237965574317 ) ) ;
#174330 = AXIS2_PLACEMENT_3D ( 'NONE', #23936, #121746, #83833 ) ;
#174332 = ORIENTED_EDGE ( 'NONE', *, *, #217999, .F. ) ;
#174331 = DIRECTION ( 'NONE',  ( 1.000000000000000000, -0.000000000000000000, -0.000000000000000000 ) ) ;
#174333 = CIRCLE ( 'NONE', #153488, 4.000000000000003553 ) ;
#174334 = CARTESIAN_POINT ( 'NONE',  ( -22.49072729836729678, 0.05648193274477467801, -155.8499917508450210 ) ) ;
#174335 = CIRCLE ( 'NONE', #149190, 0.6000000000000033085 ) ;
#174336 = CARTESIAN_POINT ( 'NONE',  ( 20.90000000000000213, 7.986648289447971116, -1.311673547813416718 ) ) ;
#174337 = CIRCLE ( 'NONE', #170427, 0.4000000000000114575 ) ;
#174339 = DIRECTION ( 'NONE',  ( 1.000000000000000000, 0.000000000000000000, 0.000000000000000000 ) ) ;
#174338 = CARTESIAN_POINT ( 'NONE',  ( -21.05000000000000071, -11.39257802170566691, -30.42605042016806394 ) ) ;
#174341 = ADVANCED_FACE ( 'NONE', ( #56986 ), #38748, .F. ) ;
#174340 = DIRECTION ( 'NONE',  ( -0.000000000000000000, -0.1298341882520022694, -0.9915357197604853789 ) ) ;
#174342 = CARTESIAN_POINT ( 'NONE',  ( -18.40000000000000213, 5.650000000011139001, -54.35000000000000142 ) ) ;
#174343 = CARTESIAN_POINT ( 'NONE',  ( -18.59999999999999787, 1.637172712970381694, -11.58215336547201879 ) ) ;
#174344 = VECTOR ( 'NONE', #90579, 999.9999999999998863 ) ;
#174345 = FACE_OUTER_BOUND ( 'NONE', #100085, .T. ) ;
#174346 = VERTEX_POINT ( 'NONE', #58281 ) ;
#174347 = EDGE_LOOP ( 'NONE', ( #153194, #7886 ) ) ;
#174348 = DIRECTION ( 'NONE',  ( 1.000000000000000000, 0.000000000000000000, 0.000000000000000000 ) ) ;
#174350 = ORIENTED_EDGE ( 'NONE', *, *, #49919, .T. ) ;
#174349 = SPHERICAL_SURFACE ( 'NONE', #208560, 0.1000000000000000056 ) ;
#174351 = ORIENTED_EDGE ( 'NONE', *, *, #17839, .T. ) ;
#174352 = DIRECTION ( 'NONE',  ( 0.000000000000000000, 0.5000000000000078826, 0.8660254037844340447 ) ) ;
#174353 = ORIENTED_EDGE ( 'NONE', *, *, #95387, .T. ) ;
#174354 = CARTESIAN_POINT ( 'NONE',  ( 22.00411653962185099, 33.60306640061018868, -242.9721070132476939 ) ) ;
#174355 = TOROIDAL_SURFACE ( 'NONE', #57771, 12.97499999999999787, 0.1000000000000000056 ) ;
#174356 = ORIENTED_EDGE ( 'NONE', *, *, #100838, .T. ) ;
#174357 = SHAPE_REPRESENTATION_RELATIONSHIP ( 'NONE' , 'NONE' ,  #18588, #132074 ) ;
#174358 = CARTESIAN_POINT ( 'NONE',  ( 18.59999999999999787, -10.64999999999999325, 31.59999999999999787 ) ) ;
#174360 = ORIENTED_EDGE ( 'NONE', *, *, #124966, .F. ) ;
#174359 = ORIENTED_EDGE ( 'NONE', *, *, #20520, .F. ) ;
#174361 = ORIENTED_EDGE ( 'NONE', *, *, #206247, .T. ) ;
#174362 = EDGE_LOOP ( 'NONE', ( #60292, #129881, #238490, #174527, #187982 ) ) ;
#174363 = ORIENTED_EDGE ( 'NONE', *, *, #227037, .F. ) ;
#174364 = CARTESIAN_POINT ( 'NONE',  ( 21.05000000000005400, 83.80000000001119531, -51.02310748452479316 ) ) ;
#174365 = CARTESIAN_POINT ( 'NONE',  ( 18.59999999999999787, 70.10000000001193143, -92.80400771986793984 ) ) ;
#174366 = DIRECTION ( 'NONE',  ( 1.000000000000000000, 0.000000000000000000, 0.000000000000000000 ) ) ;
#174368 = ORIENTED_EDGE ( 'NONE', *, *, #127975, .F. ) ;
#174367 = DIRECTION ( 'NONE',  ( 0.000000000000000000, -6.982962677686266711E-15, 1.000000000000000000 ) ) ;
#174369 = DIRECTION ( 'NONE',  ( 1.000000000000000000, 0.000000000000000000, 0.000000000000000000 ) ) ;
#174370 = CARTESIAN_POINT ( 'NONE',  ( -23.15000000000000213, 0.000000000000000000, -33.50000000000000000 ) ) ;
#174372 = ORIENTED_EDGE ( 'NONE', *, *, #1658, .T. ) ;
#174371 = CARTESIAN_POINT ( 'NONE',  ( -18.40000000000000213, 62.49385230547966330, -209.4698601954371213 ) ) ;
#174373 = LINE ( 'NONE', #253843, #41840 ) ;
#174374 = ORIENTED_EDGE ( 'NONE', *, *, #170471, .F. ) ;
#174375 = ADVANCED_FACE ( 'NONE', ( #158719 ), #137820, .T. ) ;
#174377 = ORIENTED_EDGE ( 'NONE', *, *, #164177, .F. ) ;
#174376 = DIRECTION ( 'NONE',  ( 2.952720810173289112E-16, -1.000000000000000000, -0.000000000000000000 ) ) ;
#174378 = DIRECTION ( 'NONE',  ( 0.000000000000000000, 0.000000000000000000, 1.000000000000000000 ) ) ;
#174379 = CYLINDRICAL_SURFACE ( 'NONE', #233073, 0.09999999999999939493 ) ;
#174380 = ADVANCED_FACE ( 'NONE', ( #98665 ), #94853, .F. ) ;
#174381 = ORIENTED_EDGE ( 'NONE', *, *, #219539, .F. ) ;
#174382 = AXIS2_PLACEMENT_3D ( 'NONE', #254289, #135634, #112251 ) ;
#174385 = CARTESIAN_POINT ( 'NONE',  ( 21.05000000000000071, 19.68370618165487329, -225.3554403480446240 ) ) ;
#174384 = AXIS2_PLACEMENT_3D ( 'NONE', #201232, #103399, #199973 ) ;
#174383 = CARTESIAN_POINT ( 'NONE',  ( -16.80891096016334529, 9.950000000011137047, -46.13233719273200251 ) ) ;
#174386 = DIRECTION ( 'NONE',  ( -1.000000000000000000, -0.000000000000000000, -0.000000000000000000 ) ) ;
#174387 = CARTESIAN_POINT ( 'NONE',  ( 21.14999999999999503, -0.09999999999999939493, 11.64957080754479968 ) ) ;
#174388 = CARTESIAN_POINT ( 'NONE',  ( -20.64999999999999858, 76.00000000001212186, -134.6231074845243256 ) ) ;
#174389 = ORIENTED_EDGE ( 'NONE', *, *, #134713, .T. ) ;
#174390 = ORIENTED_EDGE ( 'NONE', *, *, #188316, .F. ) ;
#174391 =( BOUNDED_SURFACE ( )  B_SPLINE_SURFACE ( 3, 2, ( 
 ( #143584, #124032, #206130 ),
 ( #105708, #23670, #243961 ),
 ( #82293, #203558, #24946 ),
 ( #181445, #2769, #241412 ),
 ( #104428, #65324, #122760 ),
 ( #224391, #183991, #7937 ) ),
 .UNSPECIFIED., .F., .F., .F. ) 
 B_SPLINE_SURFACE_WITH_KNOTS ( ( 4, 2, 4 ),
 ( 3, 3 ),
 ( 0.0001792624049599542341, 0.0003686986002124689049, 0.0005581347954649835486 ),
 ( 0.000000000000000000, 1.000000000000000000 ),
 .UNSPECIFIED. ) 
 GEOMETRIC_REPRESENTATION_ITEM ( )  RATIONAL_B_SPLINE_SURFACE ( (
 ( 1.000000000000000000, 0.9238795325112860723, 1.000000000000000000),
 ( 1.000000000000000000, 0.9229318695238166725, 1.000000000000000000),
 ( 1.000000000000000000, 0.8926288119231142737, 1.000000000000000000),
 ( 1.000000000000000000, 0.8123777807271115314, 1.000000000000000000),
 ( 1.000000000000000000, 0.7629087100931926102, 1.000000000000000000),
 ( 1.000000000000000000, 0.7071067811865475727, 1.000000000000000000) ) ) 
 REPRESENTATION_ITEM ( '' )  SURFACE ( )  );
#174392 = EDGE_CURVE ( 'NONE', #60331, #203538, #19865, .T. ) ;
#174393 = CARTESIAN_POINT ( 'NONE',  ( 21.05000000000000071, 70.50000000001180922, -81.92837350343744163 ) ) ;
#174394 = VECTOR ( 'NONE', #129789, 999.9999999999998863 ) ;
#174395 = CARTESIAN_POINT ( 'NONE',  ( -18.38817693311004575, 62.49759664249535263, -209.4452904435883625 ) ) ;
#174396 = ORIENTED_EDGE ( 'NONE', *, *, #159550, .T. ) ;
#174397 = CARTESIAN_POINT ( 'NONE',  ( -23.15000000000000213, 71.65000000001187175, -90.77310748452434552 ) ) ;
#174398 = VERTEX_POINT ( 'NONE', #863 ) ;
#174399 = DIRECTION ( 'NONE',  ( 0.000000000000000000, 0.000000000000000000, 1.000000000000000000 ) ) ;
#174400 = CARTESIAN_POINT ( 'NONE',  ( -20.94999999999999574, 56.21213088740040575, -228.0580413555848622 ) ) ;
#174401 = EDGE_CURVE ( 'NONE', #250992, #23181, #82352, .T. ) ;
#174402 = EDGE_CURVE ( 'NONE', #127492, #140147, #194842, .T. ) ;
#174403 = AXIS2_PLACEMENT_3D ( 'NONE', #44713, #188068, #68119 ) ;
#174404 = VECTOR ( 'NONE', #119862, 1000.000000000000000 ) ;
#174405 = ORIENTED_EDGE ( 'NONE', *, *, #101296, .F. ) ;
#174406 = AXIS2_PLACEMENT_3D ( 'NONE', #180920, #161366, #240895 ) ;
#174407 = EDGE_CURVE ( 'NONE', #163227, #126808, #3254, .T. ) ;
#174408 = CARTESIAN_POINT ( 'NONE',  ( 21.05000000000000071, 67.12338541492499644, -128.1380270056797031 ) ) ;
#174409 = EDGE_LOOP ( 'NONE', ( #228187, #59688 ) ) ;
#174410 = AXIS2_PLACEMENT_3D ( 'NONE', #110174, #89319, #132308 ) ;
#174411 = ORIENTED_EDGE ( 'NONE', *, *, #18277, .T. ) ;
#174412 = ORIENTED_EDGE ( 'NONE', *, *, #76075, .F. ) ;
#174413 = CARTESIAN_POINT ( 'NONE',  ( 21.15000000000005187, 74.25000000001119815, -47.64205752314703801 ) ) ;
#174414 = LINE ( 'NONE', #190078, #178389 ) ;
#174415 = DIRECTION ( 'NONE',  ( 1.073024830501117725E-15, -0.000000000000000000, -1.000000000000000000 ) ) ;
#174416 = CARTESIAN_POINT ( 'NONE',  ( 13.99999999999999822, 9.850000000011137402, -150.7500000000000284 ) ) ;
#174417 = LINE ( 'NONE', #196480, #84298 ) ;
#174418 = ADVANCED_FACE ( 'NONE', ( #221210 ), #20047, .F. ) ;
#174420 = DIRECTION ( 'NONE',  ( 0.000000000000000000, -6.982962677686266711E-15, 1.000000000000000000 ) ) ;
#174419 = CARTESIAN_POINT ( 'NONE',  ( 21.05000000000000071, 76.00000000001195133, -103.0231074845243171 ) ) ;
#174422 = VERTEX_POINT ( 'NONE', #62159 ) ;
#174421 = DIRECTION ( 'NONE',  ( 0.000000000000000000, -6.982962677686266711E-15, 1.000000000000000000 ) ) ;
#174423 = DIRECTION ( 'NONE',  ( -0.000000000000000000, -1.000000000000000000, -0.000000000000000000 ) ) ;
#174424 = ORIENTED_EDGE ( 'NONE', *, *, #118413, .T. ) ;
#174425 = CARTESIAN_POINT ( 'NONE',  ( -21.14999999999999858, 11.65000000001115588, -67.10000000000005116 ) ) ;
#174426 = VERTEX_POINT ( 'NONE', #66000 ) ;
#174427 = ORIENTED_EDGE ( 'NONE', *, *, #178311, .F. ) ;
#174428 = DIRECTION ( 'NONE',  ( -3.265361837132813093E-16, 1.000000000000000000, 0.000000000000000000 ) ) ;
#174429 = CARTESIAN_POINT ( 'NONE',  ( -17.11825945287481332, 10.05000000001113847, -121.2500000000000426 ) ) ;
#174430 = DIRECTION ( 'NONE',  ( 0.000000000000000000, -0.4088369013363280513, 0.9126074666063769270 ) ) ;
#174431 = CARTESIAN_POINT ( 'NONE',  ( -18.40000000000000213, 5.650000000011139001, -180.1499999999999773 ) ) ;
#174432 = CIRCLE ( 'NONE', #99336, 1.900000000000012790 ) ;
#174433 = AXIS2_PLACEMENT_3D ( 'NONE', #217561, #119792, #199316 ) ;
#174434 = CIRCLE ( 'NONE', #124311, 11.80000000000000249 ) ;
#174435 = CARTESIAN_POINT ( 'NONE',  ( -21.65000000000000213, 9.950000000011140600, -146.7500000000000284 ) ) ;
#174436 = ORIENTED_EDGE ( 'NONE', *, *, #223879, .F. ) ;
#174437 = ORIENTED_EDGE ( 'NONE', *, *, #82656, .T. ) ;
#174438 = CARTESIAN_POINT ( 'NONE',  ( 20.85000000000000142, 31.15787740146373608, -259.8205824356103903 ) ) ;
#174439 = ORIENTED_EDGE ( 'NONE', *, *, #210476, .F. ) ;
#174440 = DIRECTION ( 'NONE',  ( 0.000000000000000000, 0.000000000000000000, -1.000000000000000000 ) ) ;
#174441 = DIRECTION ( 'NONE',  ( -1.000000000000000000, 0.000000000000000000, 0.000000000000000000 ) ) ;
#174442 = ORIENTED_EDGE ( 'NONE', *, *, #17747, .F. ) ;
#174444 = CARTESIAN_POINT ( 'NONE',  ( -23.25000000000000355, 11.75000000001113953, -143.2500000000000284 ) ) ;
#174443 = AXIS2_PLACEMENT_3D ( 'NONE', #124939, #148345, #203178 ) ;
#174445 = CARTESIAN_POINT ( 'NONE',  ( 21.05000000000000071, 87.48912529308798014, -106.1231074845242262 ) ) ;
#174446 = CARTESIAN_POINT ( 'NONE',  ( -18.58735405345342784, -9.566478620325430171, -207.8227146462658652 ) ) ;
#174447 = DIRECTION ( 'NONE',  ( 1.020425574104003999E-15, 0.8814952561688430555, -0.4721928772777346239 ) ) ;
#174448 = ORIENTED_EDGE ( 'NONE', *, *, #42060, .T. ) ;
#174449 = CYLINDRICAL_SURFACE ( 'NONE', #121022, 0.09999999999999950595 ) ;
#174450 = DIRECTION ( 'NONE',  ( 0.000000000000000000, 1.000000000000000000, 6.982962677686266711E-15 ) ) ;
#174451 = VECTOR ( 'NONE', #46900, 1000.000000000000000 ) ;
#174452 = DIRECTION ( 'NONE',  ( 0.000000000000000000, 0.000000000000000000, 1.000000000000000000 ) ) ;
#174453 = CIRCLE ( 'NONE', #49500, 0.1000000000000028644 ) ;
#174454 = CIRCLE ( 'NONE', #61972, 0.1000000000000000472 ) ;
#174455 = EDGE_CURVE ( 'NONE', #56953, #194835, #202940, .T. ) ;
#174456 = ORIENTED_EDGE ( 'NONE', *, *, #128582, .T. ) ;
#174457 = AXIS2_PLACEMENT_3D ( 'NONE', #128916, #209734, #132782 ) ;
#174458 = CARTESIAN_POINT ( 'NONE',  ( 21.04999999999999716, -0.08561306079281304215, -161.0862402661896624 ) ) ;
#174459 = ORIENTED_EDGE ( 'NONE', *, *, #161251, .F. ) ;
#174460 = DIRECTION ( 'NONE',  ( 1.000000000000000000, 0.000000000000000000, 0.000000000000000000 ) ) ;
#174461 = EDGE_CURVE ( 'NONE', #131148, #103069, #203187, .T. ) ;
#174462 = DIRECTION ( 'NONE',  ( -0.000000000000000000, 6.982962677686266711E-15, -1.000000000000000000 ) ) ;
#174463 = CYLINDRICAL_SURFACE ( 'NONE', #71403, 0.09999999999999939493 ) ;
#174465 = AXIS2_PLACEMENT_3D ( 'NONE', #4358, #83863, #163452 ) ;
#174464 = DIRECTION ( 'NONE',  ( 1.000000000000000000, 0.000000000000000000, 0.000000000000000000 ) ) ;
#174466 = CARTESIAN_POINT ( 'NONE',  ( 21.05000000000000071, 76.00000000001237765, -169.9231074845243654 ) ) ;
#174467 = DIRECTION ( 'NONE',  ( 0.000000000000000000, -7.429790795770644761E-15, 1.000000000000000000 ) ) ;
#174468 = ORIENTED_EDGE ( 'NONE', *, *, #254475, .F. ) ;
#174469 = CARTESIAN_POINT ( 'NONE',  ( -16.93262454970420094, 65.99797953208170043, -123.9501837107616780 ) ) ;
#174470 = DIRECTION ( 'NONE',  ( 0.000000000000000000, 0.000000000000000000, 1.000000000000000000 ) ) ;
#174471 = EDGE_CURVE ( 'NONE', #122271, #181631, #10017, .T. ) ;
#174472 = EDGE_CURVE ( 'NONE', #173790, #27558, #103212, .T. ) ;
#174473 = CARTESIAN_POINT ( 'NONE',  ( -18.40000000000000213, 64.52683809664958403, -123.8731074845243683 ) ) ;
#174474 = CARTESIAN_POINT ( 'NONE',  ( -18.59999999999999787, 70.10000000001235776, -159.8040077198679683 ) ) ;
#174475 = CIRCLE ( 'NONE', #157898, 0.1000000000000001860 ) ;
#174476 = DIRECTION ( 'NONE',  ( 0.000000000000000000, -0.1686199900910312910, 0.9856811345164826488 ) ) ;
#174477 = AXIS2_PLACEMENT_3D ( 'NONE', #143551, #186550, #44473 ) ;
#174478 = AXIS2_PLACEMENT_3D ( 'NONE', #44554, #204883, #225719 ) ;
#174480 = ORIENTED_EDGE ( 'NONE', *, *, #245811, .F. ) ;
#174479 = CIRCLE ( 'NONE', #32819, 0.09999999999999939493 ) ;
#174481 = ORIENTED_EDGE ( 'NONE', *, *, #167983, .T. ) ;
#174482 = CARTESIAN_POINT ( 'NONE',  ( 21.05000000000000071, 76.49733069700262433, -201.6893511817872309 ) ) ;
#174483 = AXIS2_PLACEMENT_3D ( 'NONE', #198354, #100508, #19738 ) ;
#174484 = CARTESIAN_POINT ( 'NONE',  ( -21.00983514138059860, 6.346420624576638581, 11.97684634237457502 ) ) ;
#174485 = CARTESIAN_POINT ( 'NONE',  ( 18.47149038651511077, -9.671457158006703025, -40.17278633473840443 ) ) ;
#174486 = CARTESIAN_POINT ( 'NONE',  ( -20.85000000000000142, 74.83909925395606422, -233.7225145625711491 ) ) ;
#174487 = DIRECTION ( 'NONE',  ( 0.000000000000000000, -2.498001805406600196E-13, -1.000000000000000000 ) ) ;
#174488 = EDGE_CURVE ( 'NONE', #93529, #201917, #245931, .T. ) ;
#174489 = CIRCLE ( 'NONE', #191198, 0.1000000000000028644 ) ;
#174490 = EDGE_LOOP ( 'NONE', ( #55648, #163135, #63708, #183047, #94364, #208828, #104181, #249923, #13695 ) ) ;
#174491 = CARTESIAN_POINT ( 'NONE',  ( -20.94999999999994600, 66.15000000001120384, -6.023107484524794941 ) ) ;
#174492 = EDGE_CURVE ( 'NONE', #160578, #137086, #142945, .T. ) ;
#174493 = DIRECTION ( 'NONE',  ( 1.000000000000000000, -0.000000000000000000, -0.000000000000000000 ) ) ;
#174494 = ORIENTED_EDGE ( 'NONE', *, *, #179990, .T. ) ;
#174495 = DIRECTION ( 'NONE',  ( 0.000000000000000000, -0.2617529984165031243, -0.9651348961777157509 ) ) ;
#174496 = LINE ( 'NONE', #247873, #211946 ) ;
#174497 = AXIS2_PLACEMENT_3D ( 'NONE', #125815, #187110, #87954 ) ;
#174498 = VECTOR ( 'NONE', #71189, 1000.000000000000000 ) ;
#174499 = AXIS2_PLACEMENT_3D ( 'NONE', #29893, #205932, #145950 ) ;
#174500 = VERTEX_POINT ( 'NONE', #84222 ) ;
#174501 = CARTESIAN_POINT ( 'NONE',  ( -21.03571358705754335, 12.93326237266432877, -205.1683698891342829 ) ) ;
#174502 = EDGE_CURVE ( 'NONE', #258000, #136982, #178280, .T. ) ;
#174503 = ORIENTED_EDGE ( 'NONE', *, *, #176096, .F. ) ;
#174504 = ADVANCED_FACE ( 'NONE', ( #242064 ), #157443, .T. ) ;
#174505 = CARTESIAN_POINT ( 'NONE',  ( -18.59999999999999787, -1.851028230129704522, -112.1539132694225316 ) ) ;
#174506 = EDGE_CURVE ( 'NONE', #227495, #81505, #128545, .T. ) ;
#174507 = DIRECTION ( 'NONE',  ( 2.840903330521631775E-16, 0.8700118002898354908, -0.4930308989875170078 ) ) ;
#174508 = CARTESIAN_POINT ( 'NONE',  ( -20.94999999999999929, 9.685169582982728897, -235.1020606565447224 ) ) ;
#174509 = DIRECTION ( 'NONE',  ( 0.000000000000000000, 0.06835365183351375939, -0.9976611540402997580 ) ) ;
#174511 = CIRCLE ( 'NONE', #37100, 0.1000000000000028644 ) ;
#174510 = CYLINDRICAL_SURFACE ( 'NONE', #223615, 0.1000000000000028644 ) ;
#174512 = DIRECTION ( 'NONE',  ( 1.000000000000000000, 0.000000000000000000, 0.000000000000000000 ) ) ;
#174513 = B_SPLINE_CURVE_WITH_KNOTS ( 'NONE', 3,
 ( #24401, #201728, #41397, #3517, #924, #80457, #160065, #200453, #43938, #21821, #242132, #140462, #239584, #180893, #141747, #103888 ),
 .UNSPECIFIED., .F., .F.,
 ( 4, 3, 3, 3, 3, 4 ),
 ( 0.000000000000000000, 2.209075297430740031E-05, 5.594258369009624354E-05, 8.979524372342015197E-05, 0.0001236472815274586301, 0.0001574990747609555279 ),
 .UNSPECIFIED. ) ;
#174514 = DIRECTION ( 'NONE',  ( 0.000000000000000000, 1.000000000000000000, 6.982962677686266711E-15 ) ) ;
#174515 = DIRECTION ( 'NONE',  ( 1.000000000000000000, 0.000000000000000000, 0.000000000000000000 ) ) ;
#174517 = DIRECTION ( 'NONE',  ( 0.000000000000000000, 0.000000000000000000, 1.000000000000000000 ) ) ;
#174516 = DIRECTION ( 'NONE',  ( -7.304098846217608103E-16, 0.4721928772776973204, 0.8814952561688629284 ) ) ;
#174518 = CARTESIAN_POINT ( 'NONE',  ( 18.50000000000000000, -7.631834139421004970, -210.1304494778856053 ) ) ;
#174519 = AXIS2_PLACEMENT_3D ( 'NONE', #243409, #239574, #64771 ) ;
#174520 = CARTESIAN_POINT ( 'NONE',  ( 12.25000000000000000, 9.850000000011137402, -150.7500000000000284 ) ) ;
#174521 = DIRECTION ( 'NONE',  ( 1.000000000000000000, 0.000000000000000000, 0.000000000000000000 ) ) ;
#174522 = CARTESIAN_POINT ( 'NONE',  ( 20.95556889135987788, 18.88117369740709961, -227.9781925454673512 ) ) ;
#174523 = VERTEX_POINT ( 'NONE', #243350 ) ;
#174524 = CARTESIAN_POINT ( 'NONE',  ( -18.59999999999999787, 1.835341550235567887, -45.15515129256298366 ) ) ;
#174525 = CARTESIAN_POINT ( 'NONE',  ( 20.94999999999999929, 1.115600667400684642E-11, -67.00000000000004263 ) ) ;
#174526 = AXIS2_PLACEMENT_3D ( 'NONE', #16263, #31971, #90617 ) ;
#174527 = ORIENTED_EDGE ( 'NONE', *, *, #39399, .F. ) ;
#174528 = LINE ( 'NONE', #156215, #193619 ) ;
#174529 = CARTESIAN_POINT ( 'NONE',  ( -16.98495255085916611, 65.99443563401675306, -48.65772469074489948 ) ) ;
#174530 = LINE ( 'NONE', #74121, #110229 ) ;
#174531 = ORIENTED_EDGE ( 'NONE', *, *, #174143, .T. ) ;
#174532 = AXIS2_PLACEMENT_3D ( 'NONE', #145866, #45495, #25944 ) ;
#174533 = AXIS2_PLACEMENT_3D ( 'NONE', #29490, #7315, #121211 ) ;
#174534 = EDGE_CURVE ( 'NONE', #225362, #223565, #111613, .T. ) ;
#174535 = DIRECTION ( 'NONE',  ( 0.000000000000000000, -0.6728971962617102953, -0.7397360091702507301 ) ) ;
#174536 = AXIS2_PLACEMENT_3D ( 'NONE', #47538, #107527, #167540 ) ;
#174537 = ORIENTED_EDGE ( 'NONE', *, *, #63148, .T. ) ;
#174538 = CARTESIAN_POINT ( 'NONE',  ( -18.69999999999999929, 4.513204987021268266, 22.10000000000000142 ) ) ;
#174539 = DIRECTION ( 'NONE',  ( 0.000000000000000000, -1.000000000000000000, 0.000000000000000000 ) ) ;
#174540 = ORIENTED_EDGE ( 'NONE', *, *, #221857, .F. ) ;
#174541 = EDGE_CURVE ( 'NONE', #201784, #142525, #211581, .T. ) ;
#174542 = ORIENTED_EDGE ( 'NONE', *, *, #101475, .F. ) ;
#174543 = DIRECTION ( 'NONE',  ( 1.000000000000000000, 0.000000000000000000, 0.000000000000000000 ) ) ;
#174544 = FACE_OUTER_BOUND ( 'NONE', #131267, .T. ) ;
#174545 = DIRECTION ( 'NONE',  ( 0.000000000000000000, -0.2128009952261809279, 0.9770955615653705850 ) ) ;
#174546 = ADVANCED_FACE ( 'NONE', ( #127261 ), #7306, .T. ) ;
#174547 = DIRECTION ( 'NONE',  ( -4.701977403289178058E-30, 1.734723475976807094E-14, -1.000000000000000000 ) ) ;
#174548 = CYLINDRICAL_SURFACE ( 'NONE', #184728, 0.1000000000000028644 ) ;
#174549 = CARTESIAN_POINT ( 'NONE',  ( -15.39946565075089957, 47.12508421510194268, -234.5737628866445732 ) ) ;
#174550 = CARTESIAN_POINT ( 'NONE',  ( 18.59999999999999076, 55.11435547888746811, -226.8560373590520101 ) ) ;
#174551 = DIRECTION ( 'NONE',  ( -0.000000000000000000, -6.982962677686266711E-15, 1.000000000000000000 ) ) ;
#174552 = EDGE_CURVE ( 'NONE', #163287, #117533, #228330, .T. ) ;
#174554 = EDGE_LOOP ( 'NONE', ( #213707, #3921, #95585, #134252 ) ) ;
#174553 = CARTESIAN_POINT ( 'NONE',  ( 21.04999999999879279, 69.50331341424386267, -103.0084513660114993 ) ) ;
#174555 = EDGE_LOOP ( 'NONE', ( #189495, #247941, #242338, #52490 ) ) ;
#174557 = CARTESIAN_POINT ( 'NONE',  ( -20.97625342178413277, 64.39999999919147911, -62.59490425472234421 ) ) ;
#174556 = DIRECTION ( 'NONE',  ( 2.715809747126117987E-16, 1.000000000000000000, 5.431619494252235382E-15 ) ) ;
#174558 = ORIENTED_EDGE ( 'NONE', *, *, #12864, .T. ) ;
#174560 = VERTEX_POINT ( 'NONE', #64715 ) ;
#174559 = LINE ( 'NONE', #35031, #177636 ) ;
#174561 = ORIENTED_EDGE ( 'NONE', *, *, #115041, .F. ) ;
#174562 = LINE ( 'NONE', #75435, #37435 ) ;
#174563 = PLANE ( 'NONE',  #146875 ) ;
#174564 = EDGE_CURVE ( 'NONE', #85588, #80694, #95036, .T. ) ;
#174565 = ADVANCED_FACE ( 'NONE', ( #205500 ), #223777, .T. ) ;
#174566 = CARTESIAN_POINT ( 'NONE',  ( 20.96428641294277995, 62.87317279473580811, -207.0346585172396487 ) ) ;
#174567 = LINE ( 'NONE', #256550, #126753 ) ;
#174568 = LINE ( 'NONE', #171986, #223201 ) ;
#174569 = CARTESIAN_POINT ( 'NONE',  ( 21.05000000000000071, 9.997527148596393687, -228.1702915402975407 ) ) ;
#174570 = LINE ( 'NONE', #135368, #23678 ) ;
#174571 = CYLINDRICAL_SURFACE ( 'NONE', #168767, 0.8750000000000007772 ) ;
#174572 = AXIS2_PLACEMENT_3D ( 'NONE', #173231, #114489, #190193 ) ;
#174573 = ORIENTED_EDGE ( 'NONE', *, *, #252526, .F. ) ;
#174574 = ORIENTED_EDGE ( 'NONE', *, *, #108189, .T. ) ;
#174575 = AXIS2_PLACEMENT_3D ( 'NONE', #177569, #38044, #22335 ) ;
#174576 = CARTESIAN_POINT ( 'NONE',  ( 22.16821283564876666, 7.385839301279039759, -199.3914429501938343 ) ) ;
#174577 = CIRCLE ( 'NONE', #245449, 0.1000000000000024342 ) ;
#174578 = EDGE_CURVE ( 'NONE', #80026, #216286, #195019, .T. ) ;
#174579 = EDGE_LOOP ( 'NONE', ( #245752, #208914, #231660, #6237 ) ) ;
#174580 = CYLINDRICAL_SURFACE ( 'NONE', #134272, 0.1000000000000124678 ) ;
#174582 = EDGE_CURVE ( 'NONE', #144465, #208590, #53349, .T. ) ;
#174581 = VERTEX_POINT ( 'NONE', #106387 ) ;
#174583 = DIRECTION ( 'NONE',  ( -1.000000000000000000, -2.952720810173289112E-16, 0.000000000000000000 ) ) ;
#174584 = CIRCLE ( 'NONE', #49801, 0.09999999999999939493 ) ;
#174585 = SPHERICAL_SURFACE ( 'NONE', #9429, 0.1000000000000000056 ) ;
#174586 = DIRECTION ( 'NONE',  ( -0.000000000000000000, 0.3848449534832868446, 0.9229812358755982160 ) ) ;
#174587 = EDGE_CURVE ( 'NONE', #226630, #71383, #186641, .T. ) ;
#174589 = EDGE_LOOP ( 'NONE', ( #195176, #255118, #252155, #132237 ) ) ;
#174588 = CARTESIAN_POINT ( 'NONE',  ( -18.59999999999999787, 64.35000000001264198, -196.5083017138704236 ) ) ;
#174590 = DIRECTION ( 'NONE',  ( 1.000000000000000000, 0.000000000000000000, 0.000000000000000000 ) ) ;
#174591 = ORIENTED_EDGE ( 'NONE', *, *, #208411, .F. ) ;
#174592 = CARTESIAN_POINT ( 'NONE',  ( -20.64999999999999858, 68.85000000001186038, -90.67310748452435121 ) ) ;
#174594 = DIRECTION ( 'NONE',  ( 0.000000000000000000, -0.4930308989875575865, -0.8700118002898125091 ) ) ;
#174593 = AXIS2_PLACEMENT_3D ( 'NONE', #61051, #143143, #141874 ) ;
#174595 = AXIS2_PLACEMENT_3D ( 'NONE', #254223, #191738, #54751 ) ;
#174596 = CARTESIAN_POINT ( 'NONE',  ( -21.05000000000000071, 76.10000000001170406, -76.06376443622556849 ) ) ;
#174597 = EDGE_CURVE ( 'NONE', #227850, #153040, #45154, .T. ) ;
#174599 = VECTOR ( 'NONE', #20261, 999.9999999999998863 ) ;
#174598 = CARTESIAN_POINT ( 'NONE',  ( -21.76363531954647357, 75.90099812571328641, -210.5360440323960916 ) ) ;
#174600 = CYLINDRICAL_SURFACE ( 'NONE', #128199, 11.80000000000000959 ) ;
#174602 = ORIENTED_EDGE ( 'NONE', *, *, #49283, .F. ) ;
#174601 = EDGE_CURVE ( 'NONE', #148962, #9861, #224213, .T. ) ;
#174604 = CARTESIAN_POINT ( 'NONE',  ( -18.37151313414656784, 85.57101412579008581, -29.20644457528533877 ) ) ;
#174603 = CARTESIAN_POINT ( 'NONE',  ( 21.05000000000000071, 58.76097767208403866, -233.5579081436841022 ) ) ;
#174605 = ORIENTED_EDGE ( 'NONE', *, *, #73466, .T. ) ;
#174607 = VERTEX_POINT ( 'NONE', #248492 ) ;
#174606 = CARTESIAN_POINT ( 'NONE',  ( -21.05000000000000426, 64.40000000001234071, -163.0949042542488883 ) ) ;
#174608 = AXIS2_PLACEMENT_3D ( 'NONE', #89022, #126882, #249406 ) ;
#174609 = CARTESIAN_POINT ( 'NONE',  ( 18.59999999999999076, 11.75000000001115907, -125.3500000000000512 ) ) ;
#174610 = ADVANCED_FACE ( 'NONE', ( #251037 ), #134924, .T. ) ;
#174611 = CARTESIAN_POINT ( 'NONE',  ( -23.25000000000000000, 24.21659883365190069, -253.0960739854072870 ) ) ;
#174612 = EDGE_LOOP ( 'NONE', ( #35210, #47983, #24694, #50296 ) ) ;
#174613 = DIRECTION ( 'NONE',  ( 0.7071067811865388020, -0.7071067811865561215, 0.000000000000000000 ) ) ;
#174614 = CARTESIAN_POINT ( 'NONE',  ( -20.85000000000000142, 68.92903212821255465, -32.27654326265606954 ) ) ;
#174615 = CARTESIAN_POINT ( 'NONE',  ( -16.77683809663752257, 9.945835743215301505, -146.6639490191042228 ) ) ;
#174616 = EDGE_CURVE ( 'NONE', #136892, #145413, #71157, .T. ) ;
#174618 = ORIENTED_EDGE ( 'NONE', *, *, #19713, .T. ) ;
#174617 = SPHERICAL_SURFACE ( 'NONE', #101856, 0.1000000000000000056 ) ;
#174619 = ORIENTED_EDGE ( 'NONE', *, *, #184738, .F. ) ;
#174620 = DIRECTION ( 'NONE',  ( 0.000000000000000000, 0.000000000000000000, 1.000000000000000000 ) ) ;
#174621 = CYLINDRICAL_SURFACE ( 'NONE', #92005, 0.09999999999999691080 ) ;
#174622 = AXIS2_PLACEMENT_3D ( 'NONE', #83662, #227058, #245360 ) ;
#174623 = DIRECTION ( 'NONE',  ( 0.000000000000000000, 0.2128009952263403282, -0.9770955615653358350 ) ) ;
#174624 = ORIENTED_EDGE ( 'NONE', *, *, #217371, .T. ) ;
#174625 = CARTESIAN_POINT ( 'NONE',  ( 18.59999999999999432, 77.83585931145526615, -58.01866831572577610 ) ) ;
#174626 = DIRECTION ( 'NONE',  ( -0.000000000000000000, -0.000000000000000000, 1.000000000000000000 ) ) ;
#174627 = DIRECTION ( 'NONE',  ( 0.000000000000000000, 0.000000000000000000, 1.000000000000000000 ) ) ;
#174628 = ORIENTED_EDGE ( 'NONE', *, *, #249421, .T. ) ;
#174629 = CARTESIAN_POINT ( 'NONE',  ( 20.30466543256828160, 60.41185174759706911, -225.4538167435136415 ) ) ;
#174630 = DIRECTION ( 'NONE',  ( 0.000000000000000000, 0.2617529984165030132, 0.9651348961777157509 ) ) ;
#174631 = VERTEX_POINT ( 'NONE', #91975 ) ;
#174633 = AXIS2_PLACEMENT_3D ( 'NONE', #103495, #102196, #24004 ) ;
#174632 = DIRECTION ( 'NONE',  ( 1.000000000000000000, 0.000000000000000000, 0.000000000000000000 ) ) ;
#174634 = FACE_OUTER_BOUND ( 'NONE', #237987, .T. ) ;
#174635 = CARTESIAN_POINT ( 'NONE',  ( -18.79999999999999716, -1.212568896937008089, -8.000000000000000000 ) ) ;
#174636 = AXIS2_PLACEMENT_3D ( 'NONE', #87815, #199124, #124411 ) ;
#174637 = ORIENTED_EDGE ( 'NONE', *, *, #166807, .T. ) ;
#174638 = EDGE_LOOP ( 'NONE', ( #78728, #60676, #83763, #218275 ) ) ;
#174639 = AXIS2_PLACEMENT_3D ( 'NONE', #172595, #132134, #171315 ) ;
#174640 = FACE_OUTER_BOUND ( 'NONE', #61387, .T. ) ;
#174641 = EDGE_CURVE ( 'NONE', #221167, #257696, #66002, .T. ) ;
#174642 = EDGE_LOOP ( 'NONE', ( #157370, #253055, #201325, #252424 ) ) ;
#174644 = VERTEX_POINT ( 'NONE', #69876 ) ;
#174643 = DIRECTION ( 'NONE',  ( 0.000000000000000000, 2.891205793294679805E-16, -1.000000000000000000 ) ) ;
#174645 = CIRCLE ( 'NONE', #162137, 0.1000000000000024342 ) ;
#174646 = AXIS2_PLACEMENT_3D ( 'NONE', #196572, #77903, #160047 ) ;
#174649 = ORIENTED_EDGE ( 'NONE', *, *, #67450, .T. ) ;
#174648 = EDGE_LOOP ( 'NONE', ( #156595, #215900, #241285, #121627 ) ) ;
#174647 = FACE_OUTER_BOUND ( 'NONE', #145841, .T. ) ;
#174650 = DIRECTION ( 'NONE',  ( 0.000000000000000000, 0.000000000000000000, -1.000000000000000000 ) ) ;
#174651 = CARTESIAN_POINT ( 'NONE',  ( 22.20000000000000284, 6.223900101154161923, 12.09999999999999964 ) ) ;
#174653 = ADVANCED_FACE ( 'NONE', ( #149414 ), #30752, .F. ) ;
#174652 = CARTESIAN_POINT ( 'NONE',  ( 21.13507111622890022, 10.71768338700954537, -112.7491685863608382 ) ) ;
#174654 = CARTESIAN_POINT ( 'NONE',  ( 21.05000000000000071, 65.39167043205863195, -195.9314224712280748 ) ) ;
#174655 = CIRCLE ( 'NONE', #12311, 0.6000000000000033085 ) ;
#174656 = CARTESIAN_POINT ( 'NONE',  ( -21.14999999999994174, 74.94272479589878344, -3.123107484524795474 ) ) ;
#174657 = DIRECTION ( 'NONE',  ( 0.000000000000000000, 0.000000000000000000, 1.000000000000000000 ) ) ;
#174658 = ORIENTED_EDGE ( 'NONE', *, *, #174791, .F. ) ;
#174659 = ORIENTED_EDGE ( 'NONE', *, *, #213451, .F. ) ;
#174660 = TOROIDAL_SURFACE ( 'NONE', #207943, 0.2000000000000000111, 0.1000000000000000056 ) ;
#174661 = ORIENTED_EDGE ( 'NONE', *, *, #167062, .F. ) ;
#174662 = LINE ( 'NONE', #172078, #229011 ) ;
#174664 = VERTEX_POINT ( 'NONE', #52841 ) ;
#174663 = DIRECTION ( 'NONE',  ( 0.5932847527679299127, 0.8049926720990051576, 4.984624513800587583E-15 ) ) ;
#174665 = DIRECTION ( 'NONE',  ( 0.000000000000000000, -7.116814260417668513E-15, 1.000000000000000000 ) ) ;
#174666 = EDGE_LOOP ( 'NONE', ( #78059, #60599, #98043, #161181 ) ) ;
#174667 = AXIS2_PLACEMENT_3D ( 'NONE', #46666, #159272, #60136 ) ;
#174668 = FACE_OUTER_BOUND ( 'NONE', #228537, .T. ) ;
#174669 = VERTEX_POINT ( 'NONE', #213198 ) ;
#174670 = DIRECTION ( 'NONE',  ( -1.000000000000000000, -0.000000000000000000, -0.000000000000000000 ) ) ;
#174671 = ORIENTED_EDGE ( 'NONE', *, *, #12069, .T. ) ;
#174672 = PLANE ( 'NONE',  #60496 ) ;
#174673 = FACE_OUTER_BOUND ( 'NONE', #166309, .T. ) ;
#174674 = AXIS2_PLACEMENT_3D ( 'NONE', #221761, #180113, #177571 ) ;
#174676 = EDGE_LOOP ( 'NONE', ( #28172, #52418, #108208, #131099 ) ) ;
#174675 = EDGE_LOOP ( 'NONE', ( #4947, #35277, #235515, #160533 ) ) ;
#174677 = ORIENTED_EDGE ( 'NONE', *, *, #11065, .T. ) ;
#174678 = CARTESIAN_POINT ( 'NONE',  ( -23.25000000000000000, 67.49222854868494892, -195.4187676019683693 ) ) ;
#174679 = ORIENTED_EDGE ( 'NONE', *, *, #192729, .T. ) ;
#174680 = ORIENTED_EDGE ( 'NONE', *, *, #226498, .T. ) ;
#174681 = CARTESIAN_POINT ( 'NONE',  ( 23.14999999999999503, 15.92646454033040371, -219.3818586450342423 ) ) ;
#174683 = VERTEX_POINT ( 'NONE', #151988 ) ;
#174682 = CARTESIAN_POINT ( 'NONE',  ( 18.40000000000000568, -9.499999999988890664, -107.4221498493303955 ) ) ;
#174684 = DIRECTION ( 'NONE',  ( 1.000000000000000000, 3.265361837132813093E-16, -0.000000000000000000 ) ) ;
#174686 = CARTESIAN_POINT ( 'NONE',  ( 23.40000000000005542, 87.50449464844290048, -34.18759587077607165 ) ) ;
#174685 = CARTESIAN_POINT ( 'NONE',  ( -22.39999999999999503, 7.790779598384560245, -167.3999999999999773 ) ) ;
#174687 = DIRECTION ( 'NONE',  ( 1.000000000000000000, -2.952720810173289112E-16, -2.061873921506763405E-30 ) ) ;
#174688 = CARTESIAN_POINT ( 'NONE',  ( 18.59999999999999432, 77.73625713160897988, -57.95445515550681392 ) ) ;
#174689 = FACE_BOUND ( 'NONE', #162593, .T. ) ;
#174690 = ORIENTED_EDGE ( 'NONE', *, *, #79484, .F. ) ;
#174691 = CIRCLE ( 'NONE', #128867, 12.87499999999999822 ) ;
#174692 = ORIENTED_EDGE ( 'NONE', *, *, #148433, .F. ) ;
#174693 = CARTESIAN_POINT ( 'NONE',  ( -18.59999999999999787, 11.75000000001115552, -167.5000000000000284 ) ) ;
#174694 = DIRECTION ( 'NONE',  ( 0.000000000000000000, 0.000000000000000000, -1.000000000000000000 ) ) ;
#174695 = FACE_BOUND ( 'NONE', #122554, .T. ) ;
#174696 = VECTOR ( 'NONE', #194267, 1000.000000000000000 ) ;
#174697 = EDGE_CURVE ( 'NONE', #248011, #149564, #61726, .T. ) ;
#174698 = ORIENTED_EDGE ( 'NONE', *, *, #150400, .F. ) ;
#174699 = DIRECTION ( 'NONE',  ( 1.000000000000000000, -0.000000000000000000, -0.000000000000000000 ) ) ;
#174700 = DIRECTION ( 'NONE',  ( 0.000000000000000000, 1.000000000000000000, 0.000000000000000000 ) ) ;
#174701 = ORIENTED_EDGE ( 'NONE', *, *, #118809, .F. ) ;
#174702 = EDGE_LOOP ( 'NONE', ( #161634, #125232, #197224, #107039 ) ) ;
#174703 = ADVANCED_FACE ( 'NONE', ( #94534 ), #29481, .F. ) ;
#174704 = DIRECTION ( 'NONE',  ( 0.000000000000000000, 0.000000000000000000, -1.000000000000000000 ) ) ;
#174705 = CARTESIAN_POINT ( 'NONE',  ( -16.78055652883087134, 66.05322308388670649, -123.8623156469319326 ) ) ;
#174706 = ORIENTED_EDGE ( 'NONE', *, *, #146497, .F. ) ;
#174707 = CYLINDRICAL_SURFACE ( 'NONE', #218054, 0.09999999999999939493 ) ;
#174708 = ORIENTED_EDGE ( 'NONE', *, *, #225856, .T. ) ;
#174709 = FACE_OUTER_BOUND ( 'NONE', #238017, .T. ) ;
#174710 = LINE ( 'NONE', #74310, #74793 ) ;
#174712 = DIRECTION ( 'NONE',  ( -1.000000000000000000, 0.000000000000000000, 0.000000000000000000 ) ) ;
#174711 = DIRECTION ( 'NONE',  ( 0.7071067811865475727, -0.7071067811865475727, -5.142139384388981164E-15 ) ) ;
#174713 = EDGE_CURVE ( 'NONE', #222383, #178251, #192371, .T. ) ;
#174714 = VECTOR ( 'NONE', #94881, 1000.000000000000000 ) ;
#174715 = CARTESIAN_POINT ( 'NONE',  ( -21.07928932188134041, 61.09751618602744827, -234.2940654522722639 ) ) ;
#174716 = CARTESIAN_POINT ( 'NONE',  ( 21.13507111622890022, 65.28231661301347799, -90.77393889816359263 ) ) ;
#174717 = AXIS2_PLACEMENT_3D ( 'NONE', #156669, #234898, #56226 ) ;
#174718 = EDGE_CURVE ( 'NONE', #210671, #203969, #36827, .T. ) ;
#174719 = CARTESIAN_POINT ( 'NONE',  ( 20.94999999999999574, 70.53171716061257257, -228.4612385850772682 ) ) ;
#174720 = VECTOR ( 'NONE', #145005, 1000.000000000000000 ) ;
#174721 =( BOUNDED_SURFACE ( )  B_SPLINE_SURFACE ( 3, 2, ( 
 ( #17259, #96748, #255808 ),
 ( #77206, #177637, #78485 ),
 ( #198446, #219289, #236287 ),
 ( #19833, #158091, #99321 ),
 ( #178926, #79756, #159345 ),
 ( #40704, #120238, #127911 ),
 ( #87475, #105738, #226998 ),
 ( #242702, #7968, #88751 ),
 ( #125340, #246551, #224424 ),
 ( #108349, #23700, #26249 ) ),
 .UNSPECIFIED., .F., .F., .F. ) 
 B_SPLINE_SURFACE_WITH_KNOTS ( ( 4, 2, 2, 2, 4 ),
 ( 3, 3 ),
 ( 0.002161241639767248670, 0.002579950749615825267, 0.002789305304540113349, 0.002893982582002257390, 0.002998659859464401431 ),
 ( 0.000000000000000000, 1.000000000000000000 ),
 .UNSPECIFIED. ) 
 GEOMETRIC_REPRESENTATION_ITEM ( )  RATIONAL_B_SPLINE_SURFACE ( (
 ( 1.000000000000000000, 0.7071067811865536790, 1.000000000000000000),
 ( 1.000000000000000000, 0.7632447400667790038, 1.000000000000000000),
 ( 1.000000000000000000, 0.8158073005105432873, 1.000000000000000000),
 ( 1.000000000000000000, 0.8906973462398217745, 1.000000000000000000),
 ( 1.000000000000000000, 0.9149408947797255109, 1.000000000000000000),
 ( 1.000000000000000000, 0.9493368785277334077, 1.000000000000000000),
 ( 1.000000000000000000, 0.9605194247158570509, 1.000000000000000000),
 ( 1.000000000000000000, 0.9803630264779448211, 1.000000000000000000),
 ( 1.000000000000000000, 0.9900844824272494460, 1.000000000000000000),
 ( 1.000000000000000000, 0.9894588281429256282, 1.000000000000000000) ) ) 
 REPRESENTATION_ITEM ( '' )  SURFACE ( )  );
#174723 = ORIENTED_EDGE ( 'NONE', *, *, #38838, .T. ) ;
#174722 = ORIENTED_EDGE ( 'NONE', *, *, #255749, .F. ) ;
#174724 = EDGE_LOOP ( 'NONE', ( #3060, #164822, #50759 ) ) ;
#174725 = DIRECTION ( 'NONE',  ( 1.000000000000000000, 0.000000000000000000, 0.000000000000000000 ) ) ;
#174726 = CARTESIAN_POINT ( 'NONE',  ( -18.40000000000000213, 64.66825945288681510, -115.6731074845243796 ) ) ;
#174727 = DIRECTION ( 'NONE',  ( -0.000000000000000000, 0.000000000000000000, 1.000000000000000000 ) ) ;
#174728 = DIRECTION ( 'NONE',  ( 1.000000000000000000, 0.000000000000000000, 0.000000000000000000 ) ) ;
#174729 = EDGE_CURVE ( 'NONE', #35701, #109083, #75016, .T. ) ;
#174731 = CARTESIAN_POINT ( 'NONE',  ( -12.25000000000000178, 66.65000000001185754, -86.27310748452437394 ) ) ;
#174730 = DIRECTION ( 'NONE',  ( 1.000000000000000000, 0.000000000000000000, 0.000000000000000000 ) ) ;
#174732 = DIRECTION ( 'NONE',  ( 0.000000000000000000, -1.000000000000000000, 0.000000000000000000 ) ) ;
#174733 = EDGE_LOOP ( 'NONE', ( #17606, #199656, #40280, #52677, #194276, #206704, #89924 ) ) ;
#174734 = CARTESIAN_POINT ( 'NONE',  ( -18.50000000000000000, 77.16412189325330928, -128.8082593989527425 ) ) ;
#174735 = ORIENTED_EDGE ( 'NONE', *, *, #146295, .T. ) ;
#174736 = ORIENTED_EDGE ( 'NONE', *, *, #180932, .F. ) ;
#174737 = CARTESIAN_POINT ( 'NONE',  ( -21.14999999999999503, 69.45934304831041572, -69.52310748452437394 ) ) ;
#174738 = DIRECTION ( 'NONE',  ( 1.000000000000000000, -0.000000000000000000, -0.000000000000000000 ) ) ;
#174739 = DIRECTION ( 'NONE',  ( 0.000000000000000000, -6.982962677686266711E-15, 1.000000000000000000 ) ) ;
#174740 = CYLINDRICAL_SURFACE ( 'NONE', #119073, 0.09999999999999939493 ) ;
#174741 = DIRECTION ( 'NONE',  ( -5.603264701231743991E-32, 1.897661533703519897E-16, -1.000000000000000000 ) ) ;
#174742 = ORIENTED_EDGE ( 'NONE', *, *, #40458, .F. ) ;
#174743 = EDGE_LOOP ( 'NONE', ( #156654, #172132, #113469, #55961 ) ) ;
#174744 = DIRECTION ( 'NONE',  ( -1.000000000000000000, 0.000000000000000000, -0.000000000000000000 ) ) ;
#174745 = DIRECTION ( 'NONE',  ( 0.000000000000000000, 0.000000000000000000, -1.000000000000000000 ) ) ;
#174746 = DIRECTION ( 'NONE',  ( 0.000000000000000000, 0.000000000000000000, -1.000000000000000000 ) ) ;
#174747 = DIRECTION ( 'NONE',  ( 1.000000000000000000, 0.000000000000000000, 0.000000000000000000 ) ) ;
#174748 = DIRECTION ( 'NONE',  ( -1.000000000000000000, 0.000000000000000000, -0.000000000000000000 ) ) ;
#174750 = EDGE_CURVE ( 'NONE', #81073, #115527, #24333, .T. ) ;
#174749 = DIRECTION ( 'NONE',  ( 0.000000000000000000, 0.4930308989875230585, 0.8700118002898322711 ) ) ;
#174752 = FACE_OUTER_BOUND ( 'NONE', #255018, .T. ) ;
#174751 = LINE ( 'NONE', #230850, #245134 ) ;
#174753 = DIRECTION ( 'NONE',  ( -0.7070776581709311559, 4.937903618720164857E-15, -0.7071359030027479786 ) ) ;
#174754 = DIRECTION ( 'NONE',  ( 1.000000000000000000, 0.000000000000000000, -0.000000000000000000 ) ) ;
#174755 = CIRCLE ( 'NONE', #187185, 0.1000000000000013933 ) ;
#174756 = AXIS2_PLACEMENT_3D ( 'NONE', #20736, #181094, #178538 ) ;
#174757 = DIRECTION ( 'NONE',  ( 0.000000000000000000, -6.982962677686266711E-15, 1.000000000000000000 ) ) ;
#174758 = DIRECTION ( 'NONE',  ( -1.073024830501117725E-15, 0.000000000000000000, 1.000000000000000000 ) ) ;
#174759 = TOROIDAL_SURFACE ( 'NONE', #33270, 2.100000000000002309, 0.1000000000000000056 ) ;
#174760 = AXIS2_PLACEMENT_3D ( 'NONE', #216364, #40346, #195551 ) ;
#174762 = ORIENTED_EDGE ( 'NONE', *, *, #80024, .T. ) ;
#174761 = FACE_OUTER_BOUND ( 'NONE', #253013, .T. ) ;
#174763 = ADVANCED_FACE ( 'NONE', ( #172855 ), #153280, .T. ) ;
#174764 = TOROIDAL_SURFACE ( 'NONE', #128932, 11.65000000000000036, 0.1000000000000000056 ) ;
#174765 = DIRECTION ( 'NONE',  ( 0.000000000000000000, 0.000000000000000000, 1.000000000000000000 ) ) ;
#174766 = ORIENTED_EDGE ( 'NONE', *, *, #87536, .F. ) ;
#174767 = ADVANCED_FACE ( 'NONE', ( #34598 ), #3450, .T. ) ;
#174768 = DIRECTION ( 'NONE',  ( 0.000000000000000000, -1.000000000000000000, -6.982962677686265922E-15 ) ) ;
#174769 = AXIS2_PLACEMENT_3D ( 'NONE', #154742, #16509, #73930 ) ;
#174770 = AXIS2_PLACEMENT_3D ( 'NONE', #257722, #116993, #42583 ) ;
#174771 = ORIENTED_EDGE ( 'NONE', *, *, #57925, .F. ) ;
#174773 = AXIS2_PLACEMENT_3D ( 'NONE', #246993, #48797, #35377 ) ;
#174772 = DIRECTION ( 'NONE',  ( 1.000000000000000000, 7.116814260417643269E-15, 0.000000000000000000 ) ) ;
#174774 = ADVANCED_FACE ( 'NONE', ( #234053 ), #117957, .T. ) ;
#174775 = CARTESIAN_POINT ( 'NONE',  ( 12.30626653967340900, 9.356790025057035720, -84.20482650861391960 ) ) ;
#174776 = CARTESIAN_POINT ( 'NONE',  ( 22.49806830649814060, 0.07746431633666321648, -21.85011034516092465 ) ) ;
#174777 = AXIS2_PLACEMENT_3D ( 'NONE', #166391, #25574, #201626 ) ;
#174778 = CARTESIAN_POINT ( 'NONE',  ( -21.65000000000000213, 12.41403342719998548, -211.2428889513006993 ) ) ;
#174779 = CARTESIAN_POINT ( 'NONE',  ( -18.39999999999999858, 37.99112772578902764, -261.0419300540664835 ) ) ;
#174780 = CARTESIAN_POINT ( 'NONE',  ( -20.64999999999999858, -8.999999999988844479, -90.60603087734760663 ) ) ;
#174781 = VERTEX_POINT ( 'NONE', #61848 ) ;
#174782 = CYLINDRICAL_SURFACE ( 'NONE', #220509, 1.749999999999999778 ) ;
#174784 = ORIENTED_EDGE ( 'NONE', *, *, #208089, .T. ) ;
#174783 = DIRECTION ( 'NONE',  ( -1.000000000000000000, 0.000000000000000000, 0.000000000000000000 ) ) ;
#174785 = CARTESIAN_POINT ( 'NONE',  ( -20.94999999999999929, 36.65892442174935439, -249.5511627012433848 ) ) ;
#174786 = EDGE_CURVE ( 'NONE', #103882, #159242, #179245, .T. ) ;
#174787 = CARTESIAN_POINT ( 'NONE',  ( -22.01447462590972748, 68.73619979878245090, -170.1221444845839699 ) ) ;
#174788 = FACE_OUTER_BOUND ( 'NONE', #171878, .T. ) ;
#174789 = ORIENTED_EDGE ( 'NONE', *, *, #29438, .T. ) ;
#174790 = DIRECTION ( 'NONE',  ( 1.000000000000000000, 0.000000000000000000, 0.000000000000000000 ) ) ;
#174791 = EDGE_CURVE ( 'NONE', #84480, #23304, #95808, .T. ) ;
#174792 = SHAPE_DEFINITION_REPRESENTATION ( #84581, #168659 ) ;
#174793 = EDGE_CURVE ( 'NONE', #92561, #187599, #80077, .T. ) ;
#174794 = CARTESIAN_POINT ( 'NONE',  ( 21.05000000000000071, 10.72371710471867701, -112.6500000000000341 ) ) ;
#174795 = CARTESIAN_POINT ( 'NONE',  ( -5.899999999999938183, 64.35000000001120668, -21.92310748452479174 ) ) ;
#174796 = VERTEX_POINT ( 'NONE', #16318 ) ;
#174797 = CARTESIAN_POINT ( 'NONE',  ( 20.94999999999999929, 69.05648948627111849, -235.0374527038057977 ) ) ;
#174798 = CARTESIAN_POINT ( 'NONE',  ( -18.59999999999999787, 11.65000000001115232, -121.8500000000000369 ) ) ;
#174799 = CIRCLE ( 'NONE', #241399, 0.09999999999999939493 ) ;
#174800 = ADVANCED_FACE ( 'NONE', ( #196212 ), #18857, .F. ) ;
#174801 = PLANE ( 'NONE',  #186747 ) ;
#174802 = VERTEX_POINT ( 'NONE', #39741 ) ;
#174803 = AXIS2_PLACEMENT_3D ( 'NONE', #207708, #34226, #29101 ) ;
#174804 = VERTEX_POINT ( 'NONE', #254844 ) ;
#174805 = EDGE_CURVE ( 'NONE', #241985, #91860, #17563, .T. ) ;
#174806 = EDGE_CURVE ( 'NONE', #76854, #186448, #82534, .T. ) ;
#174807 = DIRECTION ( 'NONE',  ( 0.000000000000000000, 0.2128009952263403282, -0.9770955615653358350 ) ) ;
#174808 = CARTESIAN_POINT ( 'NONE',  ( -20.64999999999999858, -8.999999999988846255, -76.89396912265249284 ) ) ;
#174809 = CYLINDRICAL_SURFACE ( 'NONE', #256532, 0.09999999999999609201 ) ;
#174810 = DIRECTION ( 'NONE',  ( 0.000000000000000000, 0.000000000000000000, -1.000000000000000000 ) ) ;
#174812 = CYLINDRICAL_SURFACE ( 'NONE', #207941, 0.09999999999999939493 ) ;
#174811 = CARTESIAN_POINT ( 'NONE',  ( 23.15000000000000213, 82.22731448072437388, -214.9453318841612486 ) ) ;
#174813 = LINE ( 'NONE', #148792, #169234 ) ;
#174814 = CARTESIAN_POINT ( 'NONE',  ( -16.94389599338512298, 9.991197989766199328, -113.1076448018102809 ) ) ;
#174815 = DIRECTION ( 'NONE',  ( -1.000000000000000000, 0.000000000000000000, 0.000000000000000000 ) ) ;
#174816 = CARTESIAN_POINT ( 'NONE',  ( -21.55000000000000426, 68.29142135624888965, -57.17310748452437963 ) ) ;
#174817 = VECTOR ( 'NONE', #39141, 1000.000000000000000 ) ;
#174818 = VERTEX_POINT ( 'NONE', #155828 ) ;
#174819 = VERTEX_POINT ( 'NONE', #257411 ) ;
#174820 = FACE_OUTER_BOUND ( 'NONE', #98574, .T. ) ;
#174821 = CIRCLE ( 'NONE', #249603, 0.09999999999999939493 ) ;
#174822 = DIRECTION ( 'NONE',  ( 0.000000000000000000, -1.000000000000000000, 0.000000000000000000 ) ) ;
#174824 = DIRECTION ( 'NONE',  ( 0.000000000000000000, 0.000000000000000000, -1.000000000000000000 ) ) ;
#174823 = DIRECTION ( 'NONE',  ( 1.000000000000000000, 0.000000000000000000, 0.000000000000000000 ) ) ;
#174825 = EDGE_CURVE ( 'NONE', #85729, #229669, #245070, .T. ) ;
#174826 = CIRCLE ( 'NONE', #145710, 11.65000000000000746 ) ;
#174827 = DIRECTION ( 'NONE',  ( -1.000000000000000000, -1.836970198721029934E-16, 0.000000000000000000 ) ) ;
#174829 = EDGE_CURVE ( 'NONE', #75051, #118692, #56665, .T. ) ;
#174828 = LINE ( 'NONE', #117374, #104196 ) ;
#174830 = CARTESIAN_POINT ( 'NONE',  ( 15.73863059295127798, 12.75047551130876933, -215.6006359250795299 ) ) ;
#174831 = ORIENTED_EDGE ( 'NONE', *, *, #154816, .T. ) ;
#174832 = AXIS2_PLACEMENT_3D ( 'NONE', #179857, #182424, #59863 ) ;
#174833 = AXIS2_PLACEMENT_3D ( 'NONE', #124136, #18912, #203658 ) ;
#174834 = VERTEX_POINT ( 'NONE', #59225 ) ;
#174835 = EDGE_CURVE ( 'NONE', #138529, #257629, #120553, .T. ) ;
#174836 = DIRECTION ( 'NONE',  ( -1.000000000000000000, 2.952720810173289112E-16, 2.061873921506763405E-30 ) ) ;
#174837 = ORIENTED_EDGE ( 'NONE', *, *, #186639, .F. ) ;
#174838 = FACE_OUTER_BOUND ( 'NONE', #85526, .T. ) ;
#174839 = AXIS2_PLACEMENT_3D ( 'NONE', #174419, #175663, #199065 ) ;
#174840 = CARTESIAN_POINT ( 'NONE',  ( -21.05000000000000071, 87.29603075034775372, -173.0710066441881452 ) ) ;
#174841 = CIRCLE ( 'NONE', #216282, 11.74999999999999645 ) ;
#174843 = MECHANICAL_DESIGN_GEOMETRIC_PRESENTATION_REPRESENTATION (  '', ( #87290 ), #137349 ) ;
#174842 = CARTESIAN_POINT ( 'NONE',  ( -21.07933241753356413, 65.48460859884913532, -241.9386811690302181 ) ) ;
#174844 = AXIS2_PLACEMENT_3D ( 'NONE', #110181, #245856, #210579 ) ;
#174845 = AXIS2_PLACEMENT_3D ( 'NONE', #42690, #24440, #25700 ) ;
#174846 = ORIENTED_EDGE ( 'NONE', *, *, #5805, .F. ) ;
#174847 = LINE ( 'NONE', #134361, #43299 ) ;
#174848 = VECTOR ( 'NONE', #21687, 1000.000000000000114 ) ;
#174849 = DIRECTION ( 'NONE',  ( 1.000000000000000000, -3.265361837132813093E-16, -2.280189983783949500E-30 ) ) ;
#174850 = LINE ( 'NONE', #93965, #240874 ) ;
#174851 = CARTESIAN_POINT ( 'NONE',  ( -20.64999999999999858, 63.46669608621377279, -222.0380013001639270 ) ) ;
#174852 = EDGE_CURVE ( 'NONE', #44347, #97848, #90940, .T. ) ;
#174853 = CARTESIAN_POINT ( 'NONE',  ( -23.25000000000000000, 76.00000000001210765, -132.4731074845242915 ) ) ;
#174854 = CARTESIAN_POINT ( 'NONE',  ( 21.07954640115354294, 65.51085817920615284, -241.9464652145973957 ) ) ;
#174856 = DIRECTION ( 'NONE',  ( -1.000000000000000000, 0.000000000000000000, 0.000000000000000000 ) ) ;
#174855 = DIRECTION ( 'NONE',  ( 0.000000000000000000, 0.000000000000000000, -1.000000000000000000 ) ) ;
#174857 = LINE ( 'NONE', #229647, #107372 ) ;
#174858 = EDGE_CURVE ( 'NONE', #28425, #106299, #81366, .T. ) ;
#174859 = EDGE_LOOP ( 'NONE', ( #237954, #145064, #184950, #151557 ) ) ;
#174861 = CARTESIAN_POINT ( 'NONE',  ( -16.85312964099708566, 66.08639531794429445, -115.9202917780939686 ) ) ;
#174860 = CARTESIAN_POINT ( 'NONE',  ( -23.25000000000000000, 11.65000000000000036, -26.48519422934604961 ) ) ;
#174862 = ORIENTED_EDGE ( 'NONE', *, *, #160066, .T. ) ;
#174864 = ORIENTED_EDGE ( 'NONE', *, *, #156253, .F. ) ;
#174863 = CARTESIAN_POINT ( 'NONE',  ( 23.15000000000000213, -11.48912529307605368, -30.39999999999999503 ) ) ;
#174865 = ORIENTED_EDGE ( 'NONE', *, *, #186006, .T. ) ;
#174866 = CARTESIAN_POINT ( 'NONE',  ( -20.94999999999999929, 18.71344899777637494, -226.7788045585494103 ) ) ;
#174867 = CARTESIAN_POINT ( 'NONE',  ( -21.55000000000000426, 7.750000000011159074, -54.65000000000000568 ) ) ;
#174868 = LINE ( 'NONE', #36624, #35090 ) ;
#174869 = DIRECTION ( 'NONE',  ( -1.000000000000000000, -2.952720810173289112E-16, 0.000000000000000000 ) ) ;
#174870 = EDGE_LOOP ( 'NONE', ( #8160, #162644, #226227, #115250 ) ) ;
#174871 = ADVANCED_FACE ( 'NONE', ( #1838 ), #157626, .T. ) ;
#174872 = CARTESIAN_POINT ( 'NONE',  ( 22.57320508075688537, 31.89597452117651244, -238.9192857152811769 ) ) ;
#174873 = FACE_OUTER_BOUND ( 'NONE', #157037, .T. ) ;
#174874 = CARTESIAN_POINT ( 'NONE',  ( 22.49999999999999645, 64.35012909624849442, -203.6056273753973187 ) ) ;
#174875 = EDGE_CURVE ( 'NONE', #252537, #252512, #218318, .T. ) ;
#174876 = ORIENTED_EDGE ( 'NONE', *, *, #208493, .F. ) ;
#174877 = AXIS2_PLACEMENT_3D ( 'NONE', #227764, #146929, #49127 ) ;
#174878 = DIRECTION ( 'NONE',  ( 0.000000000000000000, 0.9654727137038715545, -0.2605042016806676242 ) ) ;
#174879 = EDGE_CURVE ( 'NONE', #246415, #22816, #182552, .T. ) ;
#174880 = CIRCLE ( 'NONE', #4124, 0.09999999999999939493 ) ;
#174881 = FACE_OUTER_BOUND ( 'NONE', #122860, .T. ) ;
#174882 = ORIENTED_EDGE ( 'NONE', *, *, #239377, .T. ) ;
#174883 = ORIENTED_EDGE ( 'NONE', *, *, #216561, .T. ) ;
#174884 = PLANE ( 'NONE',  #60311 ) ;
#174885 = AXIS2_PLACEMENT_3D ( 'NONE', #157763, #79435, #76876 ) ;
#174886 = EDGE_CURVE ( 'NONE', #159228, #183385, #124279, .T. ) ;
#174887 = EDGE_LOOP ( 'NONE', ( #118668, #235166, #26027, #135899 ) ) ;
#174888 = DIRECTION ( 'NONE',  ( -0.000000000000000000, 1.000000000000000000, 6.982962677686266711E-15 ) ) ;
#174891 = EDGE_CURVE ( 'NONE', #239804, #143336, #199099, .T. ) ;
#174890 = EDGE_CURVE ( 'NONE', #242995, #249989, #219616, .T. ) ;
#174889 = ORIENTED_EDGE ( 'NONE', *, *, #42676, .T. ) ;
#174892 = DIRECTION ( 'NONE',  ( 0.000000000000000000, -0.9770955615653318382, -0.2128009952263588411 ) ) ;
#174893 = CARTESIAN_POINT ( 'NONE',  ( -18.40000000000000213, 11.47316190337364183, -191.6740539331919990 ) ) ;
#174894 = DIRECTION ( 'NONE',  ( 0.000000000000000000, 0.9856811345164829818, 0.1686199900910294314 ) ) ;
#174895 = ADVANCED_FACE ( 'NONE', ( #63107 ), #174197, .F. ) ;
#174896 = CARTESIAN_POINT ( 'NONE',  ( 20.94999999999999574, 60.83337574417771521, -225.3422414619149095 ) ) ;
#174897 = AXIS2_PLACEMENT_3D ( 'NONE', #60575, #41054, #120587 ) ;
#174898 = VECTOR ( 'NONE', #11699, 1000.000000000000000 ) ;
#174899 = CARTESIAN_POINT ( 'NONE',  ( -21.30740335185486245, 0.09893452578700702438, -26.94334207797199809 ) ) ;
#174900 = CARTESIAN_POINT ( 'NONE',  ( 18.36493879433266940, -9.500000806178647395, -73.92214866035172349 ) ) ;
#174901 = FACE_OUTER_BOUND ( 'NONE', #85811, .T. ) ;
#174903 = ORIENTED_EDGE ( 'NONE', *, *, #32100, .F. ) ;
#174902 = ADVANCED_FACE ( 'NONE', ( #163512 ), #111993, .T. ) ;
#174907 = EDGE_CURVE ( 'NONE', #93493, #153949, #128547, .T. ) ;
#174906 = CARTESIAN_POINT ( 'NONE',  ( 23.25000000000000000, -11.64999999999999147, -30.39999999999999503 ) ) ;
#174905 = FACE_OUTER_BOUND ( 'NONE', #228236, .T. ) ;
#174904 = CIRCLE ( 'NONE', #228838, 0.1000000000000028644 ) ;
#174908 = EDGE_LOOP ( 'NONE', ( #222990, #198038, #124658, #224723 ) ) ;
#174911 = ORIENTED_EDGE ( 'NONE', *, *, #54084, .F. ) ;
#174910 = CARTESIAN_POINT ( 'NONE',  ( 18.49999999999999289, 28.91254064196106910, -237.8576372133405528 ) ) ;
#174909 = LINE ( 'NONE', #13224, #103124 ) ;
#174912 = VERTEX_POINT ( 'NONE', #5688 ) ;
#174913 = DIRECTION ( 'NONE',  ( -1.000000000000000000, 0.000000000000000000, -0.000000000000000000 ) ) ;
#174914 = FACE_OUTER_BOUND ( 'NONE', #228670, .T. ) ;
#174915 = DIRECTION ( 'NONE',  ( -0.000000000000000000, -6.982962677686266711E-15, 1.000000000000000000 ) ) ;
#174916 = EDGE_CURVE ( 'NONE', #223761, #209328, #157818, .T. ) ;
#174917 = CARTESIAN_POINT ( 'NONE',  ( -16.85939591225058365, 9.905226478398999390, -113.4600682464690777 ) ) ;
#174918 = ORIENTED_EDGE ( 'NONE', *, *, #147617, .T. ) ;
#174920 = VERTEX_POINT ( 'NONE', #106070 ) ;
#174919 = PLANE ( 'NONE',  #151140 ) ;
#174921 = EDGE_CURVE ( 'NONE', #47997, #211866, #191111, .T. ) ;
#174923 = CARTESIAN_POINT ( 'NONE',  ( 20.95556889135987788, 10.62194358773509606, -7.642394221857522929 ) ) ;
#174922 = CARTESIAN_POINT ( 'NONE',  ( 23.14999999999999858, 69.05648948627110428, -235.0374527038057977 ) ) ;
#174924 = EDGE_CURVE ( 'NONE', #15448, #105294, #143936, .T. ) ;
#174926 = EDGE_LOOP ( 'NONE', ( #196049, #128268 ) ) ;
#174925 = DIRECTION ( 'NONE',  ( 0.000000000000000000, 0.000000000000000000, -1.000000000000000000 ) ) ;
#174927 = CIRCLE ( 'NONE', #41622, 12.97499999999999964 ) ;
#174928 = AXIS2_PLACEMENT_3D ( 'NONE', #216841, #141173, #255922 ) ;
#174929 = ORIENTED_EDGE ( 'NONE', *, *, #237819, .T. ) ;
#174930 = CARTESIAN_POINT ( 'NONE',  ( 20.95496329884391784, 11.93721277456621799, -206.1520643135125397 ) ) ;
#174931 = CARTESIAN_POINT ( 'NONE',  ( -21.98333005346336577, 65.30108822512866595, -242.9721039335941555 ) ) ;
#174932 = ORIENTED_EDGE ( 'NONE', *, *, #20721, .F. ) ;
#174933 = CARTESIAN_POINT ( 'NONE',  ( 23.24999999999999645, 1.115600667400684642E-11, -100.5000000000000426 ) ) ;
#174934 = EDGE_LOOP ( 'NONE', ( #106888, #251264, #61413, #257692 ) ) ;
#174936 = ADVANCED_FACE ( 'NONE', ( #82649 ), #222167, .F. ) ;
#174935 = CARTESIAN_POINT ( 'NONE',  ( 20.04999999999999716, 8.750000000011173285, -42.75000000000000000 ) ) ;
#174937 = LINE ( 'NONE', #236134, #226512 ) ;
#174938 = EDGE_LOOP ( 'NONE', ( #125423, #40944 ) ) ;
#174939 = DIRECTION ( 'NONE',  ( -0.000000000000000000, 0.9651348961777157509, -0.2617529984165031243 ) ) ;
#174940 = EDGE_CURVE ( 'NONE', #185056, #231683, #162247, .T. ) ;
#174941 = AXIS2_PLACEMENT_3D ( 'NONE', #129583, #31797, #10926 ) ;
#174942 = AXIS2_PLACEMENT_3D ( 'NONE', #183653, #123676, #83222 ) ;
#174943 = AXIS2_PLACEMENT_3D ( 'NONE', #103736, #142865, #205419 ) ;
#174944 = CIRCLE ( 'NONE', #241527, 0.09999999999999134581 ) ;
#174945 = CARTESIAN_POINT ( 'NONE',  ( -16.85312964099708921, 9.913604682078871022, -54.10281570643046223 ) ) ;
#174946 = ORIENTED_EDGE ( 'NONE', *, *, #62855, .T. ) ;
#174947 = AXIS2_PLACEMENT_3D ( 'NONE', #132752, #111902, #253942 ) ;
#174948 = ORIENTED_EDGE ( 'NONE', *, *, #50445, .T. ) ;
#174949 = CARTESIAN_POINT ( 'NONE',  ( 20.97438252431638972, 18.81170931721642603, -229.8655759255429700 ) ) ;
#174950 = ORIENTED_EDGE ( 'NONE', *, *, #205971, .T. ) ;
#174951 = ADVANCED_FACE ( 'NONE', ( #26586 ), #123111, .F. ) ;
#174952 = ORIENTED_EDGE ( 'NONE', *, *, #186895, .T. ) ;
#174954 = EDGE_LOOP ( 'NONE', ( #164973, #85835, #93209, #47648, #232947, #29385, #103164 ) ) ;
#174953 = DIRECTION ( 'NONE',  ( 0.000000000000000000, 0.000000000000000000, -1.000000000000000000 ) ) ;
#174955 = ORIENTED_EDGE ( 'NONE', *, *, #209231, .F. ) ;
#174956 = DIRECTION ( 'NONE',  ( 0.000000000000000000, 0.9770955615653316162, 0.2128009952263604232 ) ) ;
#174957 = EDGE_LOOP ( 'NONE', ( #155290, #151359, #211375 ) ) ;
#174960 = VERTEX_POINT ( 'NONE', #184344 ) ;
#174959 = ORIENTED_EDGE ( 'NONE', *, *, #72927, .T. ) ;
#174958 = DIRECTION ( 'NONE',  ( -0.000000000000000000, -0.000000000000000000, 1.000000000000000000 ) ) ;
#174961 = CIRCLE ( 'NONE', #141572, 7.900000000000003908 ) ;
#174962 = ORIENTED_EDGE ( 'NONE', *, *, #198600, .T. ) ;
#174963 = DIRECTION ( 'NONE',  ( 0.000000000000000000, 0.8814952561688476074, -0.4721928772777262417 ) ) ;
#174964 = EDGE_CURVE ( 'NONE', #163061, #14704, #27886, .T. ) ;
#174965 = FACE_OUTER_BOUND ( 'NONE', #207809, .T. ) ;
#174966 = ORIENTED_EDGE ( 'NONE', *, *, #38611, .F. ) ;
#174967 = CARTESIAN_POINT ( 'NONE',  ( -0.8999999999999993561, -8.250000000000005329, 26.00000000000000355 ) ) ;
#174969 = VERTEX_POINT ( 'NONE', #85215 ) ;
#174968 = CARTESIAN_POINT ( 'NONE',  ( 20.85000000000000142, -1.835859311432481045, -179.0044391687985410 ) ) ;
#174970 = DIRECTION ( 'NONE',  ( 1.000000000000000000, 0.000000000000000000, 0.000000000000000000 ) ) ;
#174971 = ORIENTED_EDGE ( 'NONE', *, *, #146178, .F. ) ;
#174972 = ORIENTED_EDGE ( 'NONE', *, *, #146597, .F. ) ;
#174973 = CYLINDRICAL_SURFACE ( 'NONE', #211348, 0.5000000000000004441 ) ;
#174974 =( NAMED_UNIT ( * ) SI_UNIT ( $, .STERADIAN. ) SOLID_ANGLE_UNIT ( ) );
#174975 = ORIENTED_EDGE ( 'NONE', *, *, #234141, .F. ) ;
#174976 = ORIENTED_EDGE ( 'NONE', *, *, #203372, .F. ) ;
#174978 = AXIS2_PLACEMENT_3D ( 'NONE', #213286, #30839, #50346 ) ;
#174977 = LINE ( 'NONE', #138340, #135146 ) ;
#174979 = CARTESIAN_POINT ( 'NONE',  ( -18.59999999999999787, 64.35000000001161879, -62.50830171387040934 ) ) ;
#174981 = ORIENTED_EDGE ( 'NONE', *, *, #112784, .T. ) ;
#174980 = ORIENTED_EDGE ( 'NONE', *, *, #220058, .F. ) ;
#174982 = ORIENTED_EDGE ( 'NONE', *, *, #173636, .F. ) ;
#174983 = CARTESIAN_POINT ( 'NONE',  ( -18.59999999999999787, 77.83585931145526615, -58.01866831572577610 ) ) ;
#174984 = ORIENTED_EDGE ( 'NONE', *, *, #250436, .F. ) ;
#174985 = ORIENTED_EDGE ( 'NONE', *, *, #175943, .F. ) ;
#174986 = CARTESIAN_POINT ( 'NONE',  ( 23.15000000000000213, -4.656943609564678788, -233.1535107627236414 ) ) ;
#174987 = CIRCLE ( 'NONE', #79034, 0.09999999999999484301 ) ;
#174988 = EDGE_LOOP ( 'NONE', ( #184729, #128202, #21704, #227164 ) ) ;
#174989 = CARTESIAN_POINT ( 'NONE',  ( 20.85000000000000142, 45.99141771592758943, -256.5205054824189119 ) ) ;
#174990 = DIRECTION ( 'NONE',  ( -1.000000000000000000, -0.000000000000000000, -0.000000000000000000 ) ) ;
#174991 = ORIENTED_EDGE ( 'NONE', *, *, #64924, .T. ) ;
#174992 = EDGE_CURVE ( 'NONE', #136640, #254397, #4421, .T. ) ;
#174993 = ORIENTED_EDGE ( 'NONE', *, *, #162712, .F. ) ;
#174994 = DIRECTION ( 'NONE',  ( -6.938893903907222856E-15, 1.000000000000000000, 2.891205793294679805E-16 ) ) ;
#174996 = EDGE_LOOP ( 'NONE', ( #229974, #167146, #11507, #141421 ) ) ;
#174995 = CIRCLE ( 'NONE', #91749, 0.09999999999999939493 ) ;
#174997 = VECTOR ( 'NONE', #205910, 1000.000000000000000 ) ;
#174998 = DIRECTION ( 'NONE',  ( 7.589415207398575214E-15, -0.4721928772777346239, -0.8814952561688430555 ) ) ;
#174999 = VERTEX_POINT ( 'NONE', #164800 ) ;
#175000 = ORIENTED_EDGE ( 'NONE', *, *, #37645, .F. ) ;
#175001 = VECTOR ( 'NONE', #185624, 999.9999999999998863 ) ;
#175002 = EDGE_CURVE ( 'NONE', #7289, #218161, #28648, .T. ) ;
#175003 = CARTESIAN_POINT ( 'NONE',  ( -23.15000000000000213, 64.25000000001186606, -90.77310748452440237 ) ) ;
#175005 = VERTEX_POINT ( 'NONE', #6995 ) ;
#175004 = DIRECTION ( 'NONE',  ( 0.000000000000000000, 0.000000000000000000, -1.000000000000000000 ) ) ;
#175006 = DIRECTION ( 'NONE',  ( 0.000000000000000000, -0.000000000000000000, 1.000000000000000000 ) ) ;
#175007 = DIRECTION ( 'NONE',  ( 1.000000000000000000, 0.000000000000000000, 0.000000000000000000 ) ) ;
#175008 = ORIENTED_EDGE ( 'NONE', *, *, #153335, .F. ) ;
#175009 = AXIS2_PLACEMENT_3D ( 'NONE', #218955, #220266, #24650 ) ;
#175010 = DIRECTION ( 'NONE',  ( 0.000000000000000000, -0.5000000000000016653, 0.8660254037844377084 ) ) ;
#175012 = TOROIDAL_SURFACE ( 'NONE', #16761, 7.791421356237316687, 0.1000000000000000056 ) ;
#175011 = CARTESIAN_POINT ( 'NONE',  ( 18.49999999999907985, 33.73043529525261874, -236.3544816891452740 ) ) ;
#175013 = DIRECTION ( 'NONE',  ( -1.000000000000000000, 0.000000000000000000, 0.000000000000000000 ) ) ;
#175014 = ADVANCED_FACE ( 'NONE', ( #145214 ), #167389, .F. ) ;
#175015 = CARTESIAN_POINT ( 'NONE',  ( 20.95512820512820440, 65.37615131630040821, -157.8731074845244393 ) ) ;
#175016 = FACE_OUTER_BOUND ( 'NONE', #62954, .T. ) ;
#175017 = CARTESIAN_POINT ( 'NONE',  ( 20.94999999999999929, 6.550000000011156231, -179.7499999999999716 ) ) ;
#175018 = CARTESIAN_POINT ( 'NONE',  ( -22.01447462590972748, 68.73619979878172614, -69.62214448458389882 ) ) ;
#175019 = CARTESIAN_POINT ( 'NONE',  ( -18.40000000000000213, 33.85569253519368260, -235.0339796035492554 ) ) ;
#175020 = LINE ( 'NONE', #233670, #18181 ) ;
#175021 = ADVANCED_FACE ( 'NONE', ( #42285 ), #153540, .F. ) ;
#175022 = EDGE_LOOP ( 'NONE', ( #127704, #135769, #246399, #180124, #105904 ) ) ;
#175023 = TOROIDAL_SURFACE ( 'NONE', #191756, 12.97499999999999787, 0.1000000000000000056 ) ;
#175024 = CIRCLE ( 'NONE', #75048, 0.2000000000000057288 ) ;
#175025 = CIRCLE ( 'NONE', #45969, 0.1000000000000028644 ) ;
#175026 = CIRCLE ( 'NONE', #179281, 0.1000000000000002554 ) ;
#175027 = AXIS2_PLACEMENT_3D ( 'NONE', #9204, #169617, #50872 ) ;
#175028 = EDGE_CURVE ( 'NONE', #120409, #31046, #224748, .T. ) ;
#175030 = EDGE_LOOP ( 'NONE', ( #75805, #99115, #58986, #141639, #69160 ) ) ;
#175029 = ORIENTED_EDGE ( 'NONE', *, *, #204015, .F. ) ;
#175031 = ORIENTED_EDGE ( 'NONE', *, *, #44922, .F. ) ;
#175032 = EDGE_CURVE ( 'NONE', #237997, #212805, #99472, .T. ) ;
#175033 = CARTESIAN_POINT ( 'NONE',  ( -21.08035267497491816, 0.08268862478717949049, -94.16829316021699015 ) ) ;
#175034 = EDGE_CURVE ( 'NONE', #217417, #216635, #193396, .T. ) ;
#175036 = CARTESIAN_POINT ( 'NONE',  ( 18.49999999999998934, 10.25000000001115552, -192.1499999999999488 ) ) ;
#175035 = LINE ( 'NONE', #32945, #111691 ) ;
#175037 = ORIENTED_EDGE ( 'NONE', *, *, #196329, .T. ) ;
#175038 = ORIENTED_EDGE ( 'NONE', *, *, #241854, .F. ) ;
#175039 = CARTESIAN_POINT ( 'NONE',  ( 21.13736287352038445, 67.95335762362756782, -56.87310748452437537 ) ) ;
#175040 = DIRECTION ( 'NONE',  ( 0.000000000000000000, -0.8774096236503307056, 0.4797419643160112934 ) ) ;
#175041 = EDGE_CURVE ( 'NONE', #18414, #221149, #48683, .T. ) ;
#175042 = DIRECTION ( 'NONE',  ( -1.000000000000000000, 0.000000000000000000, 0.000000000000000000 ) ) ;
#175043 = DIRECTION ( 'NONE',  ( 0.000000000000000000, 0.000000000000000000, 1.000000000000000000 ) ) ;
#175044 = ORIENTED_EDGE ( 'NONE', *, *, #25832, .T. ) ;
#175045 = EDGE_LOOP ( 'NONE', ( #140120, #89729, #64248, #13657, #34138, #78140, #113957, #41927, #124640, #95636, #212002 ) ) ;
#175046 = DIRECTION ( 'NONE',  ( -0.000000000000000000, 6.982962677686266711E-15, -1.000000000000000000 ) ) ;
#175047 = CARTESIAN_POINT ( 'NONE',  ( 18.59999999999999787, 1.866714910057309273, -11.75267524628200633 ) ) ;
#175048 = VERTEX_POINT ( 'NONE', #169975 ) ;
#175049 = CARTESIAN_POINT ( 'NONE',  ( 23.14999999999999858, 70.50000000001158185, -57.11784146561126363 ) ) ;
#175050 = CARTESIAN_POINT ( 'NONE',  ( -20.64999999999999858, 2.500000000011154633, -53.77537807723790309 ) ) ;
#175051 = DIRECTION ( 'NONE',  ( 0.000000000000000000, -0.6728971962617102953, -0.7397360091702507301 ) ) ;
#175052 = DIRECTION ( 'NONE',  ( 1.000000000000000000, 0.000000000000000000, 0.000000000000000000 ) ) ;
#175053 = CARTESIAN_POINT ( 'NONE',  ( 23.24999999999999645, 1.115600667400684642E-11, -67.00000000000000000 ) ) ;
#175054 = EDGE_LOOP ( 'NONE', ( #239500, #6539, #136905, #10026, #136537, #96352, #152000 ) ) ;
#175055 = DIRECTION ( 'NONE',  ( 1.000000000000000000, 0.000000000000000000, 0.000000000000000000 ) ) ;
#175056 = CARTESIAN_POINT ( 'NONE',  ( -18.50000000000000000, 9.250000000011157297, -146.3500000000000227 ) ) ;
#175057 = AXIS2_PLACEMENT_3D ( 'NONE', #53651, #229720, #112354 ) ;
#175059 = ADVANCED_FACE ( 'NONE', ( #69560 ), #149099, .F. ) ;
#175058 = CARTESIAN_POINT ( 'NONE',  ( -5.899999999999938183, 64.35000000001120668, -22.12310748452479103 ) ) ;
#175061 = DIRECTION ( 'NONE',  ( 1.000000000000000000, 0.000000000000000000, 0.000000000000000000 ) ) ;
#175060 = DIRECTION ( 'NONE',  ( 0.000000000000000000, -0.000000000000000000, 1.000000000000000000 ) ) ;
#175062 = DIRECTION ( 'NONE',  ( 1.000000000000000000, 0.000000000000000000, 0.000000000000000000 ) ) ;
#175063 = CIRCLE ( 'NONE', #91797, 0.09999999999999839573 ) ;
#175064 = DIRECTION ( 'NONE',  ( 1.000000000000000000, 0.000000000000000000, 0.000000000000000000 ) ) ;
#175065 = FACE_OUTER_BOUND ( 'NONE', #87362, .T. ) ;
#175066 = CARTESIAN_POINT ( 'NONE',  ( 20.94999999999999929, -11.48912529307605546, -30.39999999999999503 ) ) ;
#175068 = ORIENTED_EDGE ( 'NONE', *, *, #69932, .T. ) ;
#175067 = AXIS2_PLACEMENT_3D ( 'NONE', #222798, #46733, #67593 ) ;
#175069 = ORIENTED_EDGE ( 'NONE', *, *, #78623, .F. ) ;
#175070 = ADVANCED_FACE ( 'NONE', ( #49974 ), #249479, .F. ) ;
#175071 = DIRECTION ( 'NONE',  ( 0.000000000000000000, 0.000000000000000000, 1.000000000000000000 ) ) ;
#175072 = ORIENTED_EDGE ( 'NONE', *, *, #206515, .T. ) ;
#175073 = DIRECTION ( 'NONE',  ( 1.000000000000000000, 0.000000000000000000, 0.000000000000000000 ) ) ;
#175074 = ORIENTED_EDGE ( 'NONE', *, *, #48403, .T. ) ;
#175075 = VECTOR ( 'NONE', #3658, 1000.000000000000114 ) ;
#175076 = SHAPE_REPRESENTATION_RELATIONSHIP ( 'NONE' , 'NONE' ,  #100031, #178764 ) ;
#175077 = FACE_OUTER_BOUND ( 'NONE', #139941, .T. ) ;
#175078 = CIRCLE ( 'NONE', #187525, 0.1000000000000060701 ) ;
#175079 = ORIENTED_EDGE ( 'NONE', *, *, #121669, .F. ) ;
#175080 = EDGE_CURVE ( 'NONE', #4874, #132890, #216009, .T. ) ;
#175081 = AXIS2_PLACEMENT_3D ( 'NONE', #57166, #158888, #23229 ) ;
#175082 = CARTESIAN_POINT ( 'NONE',  ( 18.39999999999999503, 64.25000000001253397, -179.2731074845244450 ) ) ;
#175083 = CARTESIAN_POINT ( 'NONE',  ( -12.68215100488889213, 9.396630376328872103, -51.40705739281828812 ) ) ;
#175084 = CARTESIAN_POINT ( 'NONE',  ( 21.14999999999999858, 64.25000000001165290, -69.42310748452440805 ) ) ;
#175085 = LINE ( 'NONE', #113769, #33110 ) ;
#175087 = EDGE_LOOP ( 'NONE', ( #50923, #221130, #219432, #97940 ) ) ;
#175086 = CARTESIAN_POINT ( 'NONE',  ( -16.93710578446422588, 29.96937912356857225, -234.6801176782661571 ) ) ;
#175089 = CARTESIAN_POINT ( 'NONE',  ( -20.94999999999999929, 7.128833340093095217, -233.7327013124392749 ) ) ;
#175088 = DIRECTION ( 'NONE',  ( 1.000000000000000000, 0.000000000000000000, 0.000000000000000000 ) ) ;
#175090 = CARTESIAN_POINT ( 'NONE',  ( -18.59999999999999787, 70.56573376625485139, -228.3808404818380779 ) ) ;
#175092 = EDGE_CURVE ( 'NONE', #81149, #135406, #125036, .T. ) ;
#175091 =( BOUNDED_SURFACE ( )  B_SPLINE_SURFACE ( 3, 2, ( 
 ( #236413, #16112, #153075 ),
 ( #95614, #133467, #175212 ),
 ( #254656, #216842, #155634 ),
 ( #197286, #212997, #96865 ),
 ( #18654, #240283, #182887 ),
 ( #44644, #220708, #143729 ) ),
 .UNSPECIFIED., .F., .F., .F. ) 
 B_SPLINE_SURFACE_WITH_KNOTS ( ( 4, 2, 4 ),
 ( 3, 3 ),
 ( 0.0001342700090130150253, 0.0002909192928057470397, 0.0004475685765984790000 ),
 ( 0.000000000000000000, 1.000000000000000000 ),
 .UNSPECIFIED. ) 
 GEOMETRIC_REPRESENTATION_ITEM ( )  RATIONAL_B_SPLINE_SURFACE ( (
 ( 1.000000000000000000, 0.7250110520819876836, 1.000000000000000000),
 ( 1.000000000000000000, 0.7257599279136505155, 1.000000000000000000),
 ( 1.000000000000000000, 0.7137594617280778042, 1.000000000000000000),
 ( 1.000000000000000000, 0.6959270178813201646, 1.000000000000000000),
 ( 1.000000000000000000, 0.6919879549336411806, 1.000000000000000000),
 ( 1.000000000000000000, 0.7071067811865475727, 1.000000000000000000) ) ) 
 REPRESENTATION_ITEM ( '' )  SURFACE ( )  );
#175093 = CARTESIAN_POINT ( 'NONE',  ( 20.94999999999999574, 64.37928932189329601, -109.8915241368653284 ) ) ;
#175094 = CARTESIAN_POINT ( 'NONE',  ( 18.58719872626881298, 87.01890647199485329, -199.4425935546263986 ) ) ;
#175095 = DIRECTION ( 'NONE',  ( 1.000000000000000000, -0.000000000000000000, -0.000000000000000000 ) ) ;
#175096 = ORIENTED_EDGE ( 'NONE', *, *, #204205, .T. ) ;
#175097 = ADVANCED_FACE ( 'NONE', ( #152972 ), #151685, .T. ) ;
#175098 = FILL_AREA_STYLE ('',( #95504 ) ) ;
#175099 = CARTESIAN_POINT ( 'NONE',  ( -18.59999999999999787, 77.85161776048073534, -91.41991776492061206 ) ) ;
#175100 = ADVANCED_FACE ( 'NONE', ( #73426 ), #136920, .T. ) ;
#175101 = VECTOR ( 'NONE', #127182, 1000.000000000000000 ) ;
#175102 = AXIS2_PLACEMENT_3D ( 'NONE', #165581, #63899, #66466 ) ;
#175103 = ORIENTED_EDGE ( 'NONE', *, *, #250771, .F. ) ;
#175104 = CARTESIAN_POINT ( 'NONE',  ( -2.995603634470891112E-16, -11.74999999998884448, -112.7500000000000284 ) ) ;
#175105 = EDGE_LOOP ( 'NONE', ( #182644, #107446, #139944, #148618 ) ) ;
#175106 = DIRECTION ( 'NONE',  ( 1.000000000000000000, -0.000000000000000000, -0.000000000000000000 ) ) ;
#175107 = EDGE_CURVE ( 'NONE', #81073, #217454, #16143, .T. ) ;
#175108 = CARTESIAN_POINT ( 'NONE',  ( -16.90987985657661596, 9.957807518179730977, -20.86928708888364170 ) ) ;
#175109 = CARTESIAN_POINT ( 'NONE',  ( 20.94999999999999574, 69.60000000001230092, -160.0926828544628222 ) ) ;
#175110 = ORIENTED_EDGE ( 'NONE', *, *, #220027, .T. ) ;
#175111 = ORIENTED_EDGE ( 'NONE', *, *, #234695, .F. ) ;
#175112 = DIRECTION ( 'NONE',  ( -1.000000000000000000, 2.952720810173289112E-16, 2.061873921506763405E-30 ) ) ;
#175113 = LINE ( 'NONE', #231205, #35861 ) ;
#175114 = AXIS2_PLACEMENT_3D ( 'NONE', #223222, #4178, #180267 ) ;
#175115 = CARTESIAN_POINT ( 'NONE',  ( -16.87683809663752044, 62.88879881541065942, -213.8537543555185607 ) ) ;
#175117 = CARTESIAN_POINT ( 'NONE',  ( -16.89797118371604867, 66.02361927736649250, -90.46040085208208836 ) ) ;
#175116 = CIRCLE ( 'NONE', #112532, 0.2000000000000005107 ) ;
#175119 = DIRECTION ( 'NONE',  ( 0.000000000000000000, 0.000000000000000000, -1.000000000000000000 ) ) ;
#175118 = CARTESIAN_POINT ( 'NONE',  ( -23.25000000000000000, 76.00000000001260503, -190.7481074845243256 ) ) ;
#175120 = DIRECTION ( 'NONE',  ( 0.000000000000000000, 1.734723475976998188E-13, 1.000000000000000000 ) ) ;
#175121 = CARTESIAN_POINT ( 'NONE',  ( 21.05000012384952868, 65.37127970113623121, -90.84513015448881390 ) ) ;
#175122 = CARTESIAN_POINT ( 'NONE',  ( 21.05000000000000782, 30.90959765417966665, -252.1452208208993966 ) ) ;
#175123 = EDGE_LOOP ( 'NONE', ( #26183, #73840, #146396, #137076 ) ) ;
#175124 = SPHERICAL_SURFACE ( 'NONE', #19026, 0.1000000000000000056 ) ;
#175125 = EDGE_CURVE ( 'NONE', #64347, #209723, #68266, .T. ) ;
#175127 = VERTEX_POINT ( 'NONE', #135917 ) ;
#175126 = LINE ( 'NONE', #141091, #248719 ) ;
#175128 = CIRCLE ( 'NONE', #54252, 0.1000000000000028644 ) ;
#175129 = CARTESIAN_POINT ( 'NONE',  ( 22.49999999999999645, 11.64987090376337875, 0.08251989087297323389 ) ) ;
#175130 = DIRECTION ( 'NONE',  ( 0.000000000000000000, 0.000000000000000000, 1.000000000000000000 ) ) ;
#175132 = FACE_OUTER_BOUND ( 'NONE', #67514, .T. ) ;
#175131 = CARTESIAN_POINT ( 'NONE',  ( -21.05000000000000071, 74.73821383144687047, -94.93660852097883662 ) ) ;
#175133 = ADVANCED_FACE ( 'NONE', ( #57662 ), #128579, .F. ) ;
#175135 = ORIENTED_EDGE ( 'NONE', *, *, #107365, .T. ) ;
#175134 = CARTESIAN_POINT ( 'NONE',  ( -15.06774609480954474, 62.16217865953741750, -218.5667261927900995 ) ) ;
#175137 = DIRECTION ( 'NONE',  ( 0.000000000000000000, 0.000000000000000000, -1.000000000000000000 ) ) ;
#175136 = CARTESIAN_POINT ( 'NONE',  ( -20.94999999999999929, 1.115600667400684642E-11, -167.5000000000000284 ) ) ;
#175139 = ADVANCED_FACE ( 'NONE', ( #257113 ), #198472, .T. ) ;
#175138 = CARTESIAN_POINT ( 'NONE',  ( 23.14999999999999858, 11.65000000001116298, -193.9851942293460070 ) ) ;
#175140 = DIRECTION ( 'NONE',  ( 0.000000000000000000, -6.982962677686266711E-15, 1.000000000000000000 ) ) ;
#175141 = DIRECTION ( 'NONE',  ( 1.000000000000000000, 0.000000000000000000, 0.000000000000000000 ) ) ;
#175142 = CARTESIAN_POINT ( 'NONE',  ( -18.50000000000000000, 10.29270135741298375, -139.4573618871519614 ) ) ;
#175143 = VERTEX_POINT ( 'NONE', #21155 ) ;
#175144 = DIRECTION ( 'NONE',  ( 1.000000000000000000, -0.000000000000000000, -0.000000000000000000 ) ) ;
#175146 = ORIENTED_EDGE ( 'NONE', *, *, #13916, .T. ) ;
#175145 = CIRCLE ( 'NONE', #187584, 0.09999999999998898659 ) ;
#175147 = EDGE_CURVE ( 'NONE', #62255, #207350, #99351, .T. ) ;
#175148 = FACE_OUTER_BOUND ( 'NONE', #6475, .T. ) ;
#175149 = ORIENTED_EDGE ( 'NONE', *, *, #27641, .F. ) ;
#175150 = DIRECTION ( 'NONE',  ( 0.000000000000000000, 0.1332476588733448597, -0.9910827722268067408 ) ) ;
#175151 = ORIENTED_EDGE ( 'NONE', *, *, #131737, .T. ) ;
#175152 = CARTESIAN_POINT ( 'NONE',  ( -21.12642695952773764, 6.375659922046319927, -167.4010967168105708 ) ) ;
#175153 = CARTESIAN_POINT ( 'NONE',  ( -23.25000000000000000, 76.00000000001126921, -203.5231074845248997 ) ) ;
#175154 = PLANE ( 'NONE',  #114201 ) ;
#175155 = ORIENTED_EDGE ( 'NONE', *, *, #98087, .F. ) ;
#175156 = DIRECTION ( 'NONE',  ( 1.000000000000000000, 0.000000000000000000, 0.000000000000000000 ) ) ;
#175157 = EDGE_CURVE ( 'NONE', #142715, #219313, #36874, .T. ) ;
#175158 = DIRECTION ( 'NONE',  ( 1.000000000000000000, 0.000000000000000000, 0.000000000000000000 ) ) ;
#175159 = CARTESIAN_POINT ( 'NONE',  ( 23.14999999999999858, 56.16603649944111254, -228.1013850343386480 ) ) ;
#175160 = LINE ( 'NONE', #112580, #116343 ) ;
#175162 = CARTESIAN_POINT ( 'NONE',  ( -12.25000000000000178, 9.850000000011133849, -184.2499999999999716 ) ) ;
#175161 = AXIS2_PLACEMENT_3D ( 'NONE', #135019, #15110, #56754 ) ;
#175163 = ADVANCED_FACE ( 'NONE', ( #18564 ), #98053, .F. ) ;
#175164 = ORIENTED_EDGE ( 'NONE', *, *, #209051, .T. ) ;
#175165 = CARTESIAN_POINT ( 'NONE',  ( -18.37151313414648612, 85.57101412579075372, -129.7064445752858717 ) ) ;
#175166 = ORIENTED_EDGE ( 'NONE', *, *, #197098, .F. ) ;
#175168 = ORIENTED_EDGE ( 'NONE', *, *, #123858, .F. ) ;
#175167 = DIRECTION ( 'NONE',  ( 0.000000000000000000, 0.9999631594459055250, 0.008583690987131395445 ) ) ;
#175169 = ORIENTED_EDGE ( 'NONE', *, *, #253117, .T. ) ;
#175170 = CARTESIAN_POINT ( 'NONE',  ( 18.44364597020195973, 85.49048731717491023, -196.4651295948403913 ) ) ;
#175171 = DIRECTION ( 'NONE',  ( 0.000000000000000000, 1.000000000000000000, 6.938893903907222067E-15 ) ) ;
#175172 = DIRECTION ( 'NONE',  ( -1.000000000000000000, -0.000000000000000000, -0.000000000000000000 ) ) ;
#175173 = DIRECTION ( 'NONE',  ( 0.000000000000000000, 0.2128009952263618110, -0.9770955615653311721 ) ) ;
#175174 = AXIS2_PLACEMENT_3D ( 'NONE', #220864, #235622, #136512 ) ;
#175175 = ORIENTED_EDGE ( 'NONE', *, *, #104635, .T. ) ;
#175176 = ADVANCED_FACE ( 'NONE', ( #77230 ), #24512, .F. ) ;
#175177 = DIRECTION ( 'NONE',  ( 0.000000000000000000, -1.000000000000000000, 0.000000000000000000 ) ) ;
#175178 = CARTESIAN_POINT ( 'NONE',  ( 23.14999999999999858, 76.00000000001190870, -103.0231074845243029 ) ) ;
#175179 = VERTEX_POINT ( 'NONE', #156818 ) ;
#175180 = ADVANCED_FACE ( 'NONE', ( #253305 ), #55083, .T. ) ;
#175182 = ORIENTED_EDGE ( 'NONE', *, *, #215818, .F. ) ;
#175181 = CARTESIAN_POINT ( 'NONE',  ( 11.60000000000006182, 64.25000000001119815, -23.72310748452479601 ) ) ;
#175183 = CARTESIAN_POINT ( 'NONE',  ( 20.30531438145591139, 65.90309893892202808, -128.7270896772505466 ) ) ;
#175184 = DIRECTION ( 'NONE',  ( 2.952720810173289112E-16, -1.000000000000000000, 0.000000000000000000 ) ) ;
#175185 = ADVANCED_FACE ( 'NONE', ( #154265 ), #181884, .F. ) ;
#175186 = CYLINDRICAL_SURFACE ( 'NONE', #251357, 0.1000000000000002554 ) ;
#175187 = AXIS2_PLACEMENT_3D ( 'NONE', #119641, #54514, #117065 ) ;
#175188 = ORIENTED_EDGE ( 'NONE', *, *, #23486, .T. ) ;
#175189 = AXIS2_PLACEMENT_3D ( 'NONE', #208190, #111638, #29569 ) ;
#175190 = ADVANCED_FACE ( 'NONE', ( #4122 ), #41992, .F. ) ;
#175191 = CARTESIAN_POINT ( 'NONE',  ( 21.04999999999999716, 64.25000000001195133, -109.8647081744214375 ) ) ;
#175193 = EDGE_CURVE ( 'NONE', #198825, #114655, #245315, .T. ) ;
#175192 = ORIENTED_EDGE ( 'NONE', *, *, #86411, .T. ) ;
#175194 = CARTESIAN_POINT ( 'NONE',  ( -33.72168855820451938, 9.950000000011156587, -154.8500000000000796 ) ) ;
#175195 = CIRCLE ( 'NONE', #91919, 0.1000000000000027117 ) ;
#175196 = CARTESIAN_POINT ( 'NONE',  ( 12.48201962039795809, 66.62334006147798959, -51.89491493630711716 ) ) ;
#175197 = AXIS2_PLACEMENT_3D ( 'NONE', #229891, #169960, #250725 ) ;
#175198 = CYLINDRICAL_SURFACE ( 'NONE', #242636, 0.09999999999999939493 ) ;
#175199 = CIRCLE ( 'NONE', #237696, 0.09999999999999939493 ) ;
#175200 = EDGE_CURVE ( 'NONE', #104969, #163802, #121543, .T. ) ;
#175202 = ADVANCED_FACE ( 'NONE', ( #101913 ), #240185, .F. ) ;
#175201 = CIRCLE ( 'NONE', #162690, 0.2000000000000057288 ) ;
#175203 = CIRCLE ( 'NONE', #75219, 0.1000000000000028644 ) ;
#175204 = ORIENTED_EDGE ( 'NONE', *, *, #142931, .T. ) ;
#175206 = CARTESIAN_POINT ( 'NONE',  ( -23.25000000000000000, 77.85161776048025217, -24.41991776492064758 ) ) ;
#175205 = AXIS2_PLACEMENT_3D ( 'NONE', #257700, #79102, #58264 ) ;
#175207 = CIRCLE ( 'NONE', #71119, 0.09999999999998898659 ) ;
#175208 = VERTEX_POINT ( 'NONE', #82345 ) ;
#175209 = CARTESIAN_POINT ( 'NONE',  ( -16.94107738177415712, 12.45552124806248706, -211.1315092113344463 ) ) ;
#175210 = EDGE_CURVE ( 'NONE', #77508, #122635, #74422, .T. ) ;
#175211 = LINE ( 'NONE', #136006, #199832 ) ;
#175213 = ORIENTED_EDGE ( 'NONE', *, *, #54810, .F. ) ;
#175212 = CARTESIAN_POINT ( 'NONE',  ( 21.05000000000000071, 10.72371711693665652, -146.1762396011381497 ) ) ;
#175214 = DIRECTION ( 'NONE',  ( -1.000000000000000000, 0.000000000000000000, 0.000000000000000000 ) ) ;
#175215 = DIRECTION ( 'NONE',  ( 0.000000000000000000, -2.428612866367527723E-14, -1.000000000000000000 ) ) ;
#175216 = CARTESIAN_POINT ( 'NONE',  ( -20.54999999999999716, 7.150000000011155876, -54.65000000000000568 ) ) ;
#175217 = DIRECTION ( 'NONE',  ( -0.000000000000000000, -0.000000000000000000, -1.000000000000000000 ) ) ;
#175218 = CARTESIAN_POINT ( 'NONE',  ( 15.48841904831874849, 67.43841904833035983, -56.87310748452438247 ) ) ;
#175219 = CARTESIAN_POINT ( 'NONE',  ( -21.14999999999999858, 11.65000000000000036, -3.469446951953614189E-15 ) ) ;
#175221 = ADVANCED_FACE ( 'NONE', ( #241462 ), #182783, .F. ) ;
#175220 = CARTESIAN_POINT ( 'NONE',  ( 21.08134388332232234, 6.334680580529113314, -66.92418108249302122 ) ) ;
#175222 = CIRCLE ( 'NONE', #29465, 0.09999999999999939493 ) ;
#175224 = ORIENTED_EDGE ( 'NONE', *, *, #90006, .T. ) ;
#175223 = CYLINDRICAL_SURFACE ( 'NONE', #86278, 12.87500000000000000 ) ;
#175225 = EDGE_CURVE ( 'NONE', #223079, #243012, #23728, .T. ) ;
#175227 = EDGE_CURVE ( 'NONE', #213743, #45676, #236867, .T. ) ;
#175226 = CARTESIAN_POINT ( 'NONE',  ( -18.38204789744325396, 16.37699364664935331, -222.2517181225500451 ) ) ;
#175228 = CARTESIAN_POINT ( 'NONE',  ( -18.43473496883410334, 85.49495241101196541, -196.4772359122960665 ) ) ;
#175229 = ORIENTED_EDGE ( 'NONE', *, *, #109988, .T. ) ;
#175230 = FACE_OUTER_BOUND ( 'NONE', #206676, .T. ) ;
#175231 = AXIS2_PLACEMENT_3D ( 'NONE', #79611, #198293, #17115 ) ;
#175232 = FACE_OUTER_BOUND ( 'NONE', #122139, .T. ) ;
#175233 = FACE_OUTER_BOUND ( 'NONE', #146810, .T. ) ;
#175234 = EDGE_CURVE ( 'NONE', #100848, #22587, #243234, .T. ) ;
#175235 = ORIENTED_EDGE ( 'NONE', *, *, #171094, .T. ) ;
#175236 = CIRCLE ( 'NONE', #137754, 12.97499999999999964 ) ;
#175237 = CARTESIAN_POINT ( 'NONE',  ( -23.15000000000000213, 69.16514130714681130, -247.7543978865853660 ) ) ;
#175238 = CARTESIAN_POINT ( 'NONE',  ( -16.93339986808596720, 65.99489607144667502, -190.9571138127115830 ) ) ;
#175239 = ORIENTED_EDGE ( 'NONE', *, *, #146107, .F. ) ;
#175240 = CARTESIAN_POINT ( 'NONE',  ( -18.35668295345803713, 11.47316190337363118, -124.7500000000000426 ) ) ;
#175241 = ORIENTED_EDGE ( 'NONE', *, *, #190670, .T. ) ;
#175243 = EDGE_CURVE ( 'NONE', #13199, #55509, #174496, .T. ) ;
#175242 = CARTESIAN_POINT ( 'NONE',  ( 20.94999999999999929, -9.399999999988846611, -76.89396912265249284 ) ) ;
#175245 = ORIENTED_EDGE ( 'NONE', *, *, #163360, .T. ) ;
#175244 = CARTESIAN_POINT ( 'NONE',  ( -21.05000000000000071, 1.835341550235567887, -78.55515129256302487 ) ) ;
#175246 = DIRECTION ( 'NONE',  ( 1.000000000000000000, -2.849773892568378313E-16, 7.728835255496647986E-17 ) ) ;
#175247 = ORIENTED_EDGE ( 'NONE', *, *, #84618, .T. ) ;
#175248 = AXIS2_PLACEMENT_3D ( 'NONE', #43157, #63994, #44448 ) ;
#175249 = CARTESIAN_POINT ( 'NONE',  ( 18.39999999999999858, 77.27075167199318173, -241.8768735168259241 ) ) ;
#175250 = ORIENTED_EDGE ( 'NONE', *, *, #182284, .F. ) ;
#175252 = ORIENTED_EDGE ( 'NONE', *, *, #757, .T. ) ;
#175251 = ORIENTED_EDGE ( 'NONE', *, *, #157653, .F. ) ;
#175253 = CARTESIAN_POINT ( 'NONE',  ( 18.42595409746874680, 85.49999981257707304, -129.5237451327773215 ) ) ;
#175254 = ORIENTED_EDGE ( 'NONE', *, *, #35354, .T. ) ;
#175255 = CARTESIAN_POINT ( 'NONE',  ( -21.44999999999999929, 7.150000000011155876, -188.7499999999999716 ) ) ;
#175256 = EDGE_LOOP ( 'NONE', ( #35108, #192539, #38979, #95214 ) ) ;
#175257 = CIRCLE ( 'NONE', #133518, 0.1999999999999987899 ) ;
#175258 = EDGE_LOOP ( 'NONE', ( #92196, #217680, #247188, #91190 ) ) ;
#175259 = CARTESIAN_POINT ( 'NONE',  ( -20.94999999999999929, 87.48912529308798014, -106.1231074845242262 ) ) ;
#175260 = CARTESIAN_POINT ( 'NONE',  ( -18.59999999999999787, 76.00000000001244871, -170.0231074845243597 ) ) ;
#175261 = LINE ( 'NONE', #52688, #103254 ) ;
#175262 = EDGE_LOOP ( 'NONE', ( #182006, #252472, #219665, #25709, #52380, #180021 ) ) ;
#175263 = CARTESIAN_POINT ( 'NONE',  ( 21.05000000000000071, 44.00266445878927613, -258.8505972146074896 ) ) ;
#175264 = CARTESIAN_POINT ( 'NONE',  ( 20.95512820512820795, 67.12384868372417657, -157.8229346253956749 ) ) ;
#175265 = DIRECTION ( 'NONE',  ( 1.000000000000000000, -2.824170522722115425E-14, 2.841386468225606068E-14 ) ) ;
#175266 = ORIENTED_EDGE ( 'NONE', *, *, #104062, .F. ) ;
#175267 = DIRECTION ( 'NONE',  ( 0.000000000000000000, 0.000000000000000000, -1.000000000000000000 ) ) ;
#175268 = CARTESIAN_POINT ( 'NONE',  ( -18.47130263965424390, 38.07810181029199015, -261.0557975469300800 ) ) ;
#175269 = DIRECTION ( 'NONE',  ( 4.336808689942128177E-15, 0.8660254037844330455, -0.5000000000000096589 ) ) ;
#175270 = AXIS2_PLACEMENT_3D ( 'NONE', #6160, #122279, #141828 ) ;
#175271 = ORIENTED_EDGE ( 'NONE', *, *, #120677, .F. ) ;
#175272 = CARTESIAN_POINT ( 'NONE',  ( -18.50000000000000000, 69.15387683765983695, -166.2853812176745691 ) ) ;
#175273 = VERTEX_POINT ( 'NONE', #235683 ) ;
#175274 = VERTEX_POINT ( 'NONE', #74088 ) ;
#175275 = CARTESIAN_POINT ( 'NONE',  ( -21.44999999999999929, 53.12864924257549148, -234.3382351616128858 ) ) ;
#175276 = ORIENTED_EDGE ( 'NONE', *, *, #247831, .F. ) ;
#175277 = ORIENTED_EDGE ( 'NONE', *, *, #28417, .T. ) ;
#175278 = DIRECTION ( 'NONE',  ( 1.000000000000000000, 0.000000000000000000, 0.000000000000000000 ) ) ;
#175279 = DIRECTION ( 'NONE',  ( 0.000000000000000000, 6.982962677686266711E-15, -1.000000000000000000 ) ) ;
#175280 = ORIENTED_EDGE ( 'NONE', *, *, #104654, .F. ) ;
#175281 = EDGE_LOOP ( 'NONE', ( #51786, #117796, #5248, #217068, #124071 ) ) ;
#175282 = CARTESIAN_POINT ( 'NONE',  ( -18.50000000000000000, -9.499999999988849808, -55.25000000000004974 ) ) ;
#175283 = CARTESIAN_POINT ( 'NONE',  ( -20.54999999999999716, 2.400000000011155432, -90.60603087734760663 ) ) ;
#175284 = ORIENTED_EDGE ( 'NONE', *, *, #35548, .T. ) ;
#175285 = AXIS2_PLACEMENT_3D ( 'NONE', #250826, #232595, #55169 ) ;
#175286 = VECTOR ( 'NONE', #233415, 1000.000000000000000 ) ;
#175287 = ADVANCED_FACE ( 'NONE', ( #88776 ), #57023, .T. ) ;
#175288 = CIRCLE ( 'NONE', #183636, 0.09999999999999939493 ) ;
#175289 = ORIENTED_EDGE ( 'NONE', *, *, #214298, .T. ) ;
#175290 = TOROIDAL_SURFACE ( 'NONE', #62830, 0.4000000000000005773, 0.1000000000000000056 ) ;
#175291 = DIRECTION ( 'NONE',  ( 0.000000000000000000, 0.9126074666063660468, 0.4088369013363524762 ) ) ;
#175292 = DIRECTION ( 'NONE',  ( 0.000000000000000000, 6.982962677686267499E-15, -1.000000000000000000 ) ) ;
#175293 = DIRECTION ( 'NONE',  ( 0.000000000000000000, -1.000000000000000000, 0.000000000000000000 ) ) ;
#175294 = PLANE ( 'NONE',  #180724 ) ;
#175295 = DIRECTION ( 'NONE',  ( 0.000000000000000000, 0.4999999999999689138, -0.8660254037844565822 ) ) ;
#175297 = ADVANCED_FACE ( 'NONE', ( #53205 ), #161896, .T. ) ;
#175296 = CIRCLE ( 'NONE', #162818, 0.1999999999999987899 ) ;
#175298 = CARTESIAN_POINT ( 'NONE',  ( -22.50000000000000000, 11.64957080755595520, -66.90000000000004832 ) ) ;
#175299 = LINE ( 'NONE', #177852, #231872 ) ;
#175301 = DIRECTION ( 'NONE',  ( 0.000000000000000000, 1.224646799142185182E-16, 1.000000000000000000 ) ) ;
#175300 = CARTESIAN_POINT ( 'NONE',  ( -16.86337532320262156, 9.979967204224358568, -12.55107553101719198 ) ) ;
#175302 = DIRECTION ( 'NONE',  ( -1.000000000000000000, 0.000000000000000000, 0.000000000000000000 ) ) ;
#175303 = CARTESIAN_POINT ( 'NONE',  ( -16.87683809663752399, 23.59405348476696318, -231.3784738672519836 ) ) ;
#175304 = DIRECTION ( 'NONE',  ( -1.000000000000000000, -1.394253735153569469E-16, -2.602809386958778209E-16 ) ) ;
#175305 = LINE ( 'NONE', #155741, #42678 ) ;
#175306 = ORIENTED_EDGE ( 'NONE', *, *, #71219, .T. ) ;
#175307 = EDGE_CURVE ( 'NONE', #126912, #136449, #49439, .T. ) ;
#175309 = ORIENTED_EDGE ( 'NONE', *, *, #253639, .T. ) ;
#175308 = CARTESIAN_POINT ( 'NONE',  ( 23.24999999999999289, 5.950000000011163692, -90.19429769496522908 ) ) ;
#175310 = EDGE_CURVE ( 'NONE', #129965, #241817, #232622, .T. ) ;
#175311 = AXIS2_PLACEMENT_3D ( 'NONE', #73132, #92650, #104804 ) ;
#175312 = CARTESIAN_POINT ( 'NONE',  ( 23.24999999999999289, 56.01362831242965967, -232.7091905853083347 ) ) ;
#175313 = EDGE_CURVE ( 'NONE', #38011, #226695, #45526, .T. ) ;
#175314 = CARTESIAN_POINT ( 'NONE',  ( -16.77683809663752257, 66.05416425680809311, -149.1870565036286109 ) ) ;
#175315 = ORIENTED_EDGE ( 'NONE', *, *, #195020, .F. ) ;
#175316 = CIRCLE ( 'NONE', #141967, 11.90000000000000213 ) ;
#175317 = DIRECTION ( 'NONE',  ( 0.000000000000000000, -0.2128009952263403282, 0.9770955615653358350 ) ) ;
#175318 = ADVANCED_FACE ( 'NONE', ( #153649 ), #96163, .T. ) ;
#175319 = CIRCLE ( 'NONE', #62864, 0.09999999999999939493 ) ;
#175320 = CARTESIAN_POINT ( 'NONE',  ( -17.04295772865528846, 10.02489942527129507, -54.35000000000000853 ) ) ;
#175321 = VERTEX_POINT ( 'NONE', #127935 ) ;
#175322 = CARTESIAN_POINT ( 'NONE',  ( 21.12769345151713196, 60.09153065753968548, -221.2288501437841717 ) ) ;
#175323 = CARTESIAN_POINT ( 'NONE',  ( 20.94999999999999574, 87.41227409416181615, -133.6231074845242119 ) ) ;
#175324 = EDGE_CURVE ( 'NONE', #37214, #95308, #187912, .T. ) ;
#175325 = CIRCLE ( 'NONE', #216967, 11.80000000000000426 ) ;
#175326 = CARTESIAN_POINT ( 'NONE',  ( 21.14999999999999858, 17.83900070254454562, -239.4698447713637677 ) ) ;
#175328 = VERTEX_POINT ( 'NONE', #252676 ) ;
#175327 = CYLINDRICAL_SURFACE ( 'NONE', #210090, 0.1000000000000028644 ) ;
#175330 = VERTEX_POINT ( 'NONE', #93617 ) ;
#175329 = CARTESIAN_POINT ( 'NONE',  ( -18.43459694179558639, 85.49421012500988581, -96.40610228186316988 ) ) ;
#175331 = DIRECTION ( 'NONE',  ( -0.000000000000000000, 0.4721928772777345684, 0.8814952561688429444 ) ) ;
#175332 = CARTESIAN_POINT ( 'NONE',  ( -20.64999999999999858, 4.350000000011156054, -112.8500000000000369 ) ) ;
#175334 = EDGE_CURVE ( 'NONE', #175005, #69752, #99652, .T. ) ;
#175333 = CARTESIAN_POINT ( 'NONE',  ( -23.25000000000000000, 4.350000000011156054, -146.1500000000000341 ) ) ;
#175336 = DIRECTION ( 'NONE',  ( -1.000000000000000000, 0.000000000000000000, 0.000000000000000000 ) ) ;
#175335 = CARTESIAN_POINT ( 'NONE',  ( -16.85697194749122829, 9.908543714134735225, -154.5649957323862225 ) ) ;
#175337 = LINE ( 'NONE', #91909, #28768 ) ;
#175339 = CARTESIAN_POINT ( 'NONE',  ( -23.25000000000000000, 1.115600667400684642E-11, -67.00000000000004263 ) ) ;
#175338 = CIRCLE ( 'NONE', #212739, 0.09999999999999939493 ) ;
#175340 = CARTESIAN_POINT ( 'NONE',  ( -20.00857864376270001, 9.150000000011157653, -188.7499999999999716 ) ) ;
#175341 = CARTESIAN_POINT ( 'NONE',  ( -23.25000000000000000, 76.00000000001165290, -69.52310748452431710 ) ) ;
#175342 = CIRCLE ( 'NONE', #237682, 0.09999999999998898659 ) ;
#175343 = VERTEX_POINT ( 'NONE', #108373 ) ;
#175345 = FACE_OUTER_BOUND ( 'NONE', #94929, .T. ) ;
#175344 = AXIS2_PLACEMENT_3D ( 'NONE', #99433, #224531, #108445 ) ;
#175346 = VERTEX_POINT ( 'NONE', #54482 ) ;
#175347 = AXIS2_PLACEMENT_3D ( 'NONE', #22101, #220300, #182459 ) ;
#175348 = ORIENTED_EDGE ( 'NONE', *, *, #111619, .F. ) ;
#175349 = CYLINDRICAL_SURFACE ( 'NONE', #140072, 7.900000000000010125 ) ;
#175350 = FACE_OUTER_BOUND ( 'NONE', #179652, .T. ) ;
#175351 = EDGE_LOOP ( 'NONE', ( #26171, #71705, #50811 ) ) ;
#175352 = AXIS2_PLACEMENT_3D ( 'NONE', #219300, #100603, #1529 ) ;
#175353 = VERTEX_POINT ( 'NONE', #195314 ) ;
#175354 = CARTESIAN_POINT ( 'NONE',  ( -21.45000000000000284, 7.708578643773852157, -45.85000000000000142 ) ) ;
#175355 =( LENGTH_UNIT ( ) NAMED_UNIT ( * ) SI_UNIT ( .MILLI., .METRE. ) );
#175357 = EDGE_LOOP ( 'NONE', ( #202383, #243471, #110854, #48252 ) ) ;
#175356 = AXIS2_PLACEMENT_3D ( 'NONE', #169009, #248502, #33346 ) ;
#175358 = AXIS2_PLACEMENT_3D ( 'NONE', #62615, #142138, #183836 ) ;
#175359 = TOROIDAL_SURFACE ( 'NONE', #83712, 0.2000000000000000111, 0.1000000000000000056 ) ;
#175360 = ORIENTED_EDGE ( 'NONE', *, *, #126718, .T. ) ;
#175361 = AXIS2_PLACEMENT_3D ( 'NONE', #210625, #91957, #166400 ) ;
#175362 = CIRCLE ( 'NONE', #221111, 0.1000000000000001305 ) ;
#175363 = EDGE_CURVE ( 'NONE', #221901, #80949, #231867, .T. ) ;
#175364 = CARTESIAN_POINT ( 'NONE',  ( -21.65000000000000213, 60.96553306590055854, -220.9452142459683159 ) ) ;
#175365 = CARTESIAN_POINT ( 'NONE',  ( -21.07094088545368749, 0.09889370255222154626, 6.320167221917132316 ) ) ;
#175366 = DIRECTION ( 'NONE',  ( 0.000000000000000000, 0.2617529984165031243, 0.9651348961777157509 ) ) ;
#175367 = EDGE_CURVE ( 'NONE', #248733, #79511, #213554, .T. ) ;
#175368 = DIRECTION ( 'NONE',  ( 0.000000000000000000, 0.8814952561688430555, -0.4721928772777347350 ) ) ;
#175369 = CARTESIAN_POINT ( 'NONE',  ( 16.87683809663749557, 9.950000000011131718, -121.3500000000000369 ) ) ;
#175370 = DIRECTION ( 'NONE',  ( 0.000000000000000000, 0.000000000000000000, -1.000000000000000000 ) ) ;
#175371 = CARTESIAN_POINT ( 'NONE',  ( 21.04999999999999361, 76.01759718702061264, -142.9638783781856830 ) ) ;
#175373 = ORIENTED_EDGE ( 'NONE', *, *, #64122, .T. ) ;
#175372 = CARTESIAN_POINT ( 'NONE',  ( -20.86777300164945004, 10.33200063080771969, -139.5931674956643462 ) ) ;
#175375 = CARTESIAN_POINT ( 'NONE',  ( -18.59999999999999787, 13.63177590472475487, -238.5351604075707144 ) ) ;
#175374 = CARTESIAN_POINT ( 'NONE',  ( -21.64999999999999858, 68.75000000001152500, -48.27310748452437394 ) ) ;
#175376 = ADVANCED_FACE ( 'NONE', ( #207483, #234398, #28879 ), #114461, .F. ) ;
#175377 = LINE ( 'NONE', #13698, #40224 ) ;
#175378 = EDGE_CURVE ( 'NONE', #128048, #251815, #33105, .T. ) ;
#175379 = EDGE_LOOP ( 'NONE', ( #135151, #161800, #43161, #205727 ) ) ;
#175380 = CYLINDRICAL_SURFACE ( 'NONE', #52111, 0.5000000000000004441 ) ;
#175381 = DIRECTION ( 'NONE',  ( 0.000000000000000000, -0.1575844902526687130, -0.9875055080513762684 ) ) ;
#175382 = ORIENTED_EDGE ( 'NONE', *, *, #231957, .T. ) ;
#175383 = ADVANCED_FACE ( 'NONE', ( #255198 ), #107070, .F. ) ;
#175384 = DIRECTION ( 'NONE',  ( -1.000000000000000000, -0.000000000000000000, -0.000000000000000000 ) ) ;
#175385 = EDGE_CURVE ( 'NONE', #13609, #120046, #78810, .T. ) ;
#175386 = LINE ( 'NONE', #155815, #185897 ) ;
#175387 = CARTESIAN_POINT ( 'NONE',  ( 20.85000000000000142, 1.115600667400684642E-11, -167.5000000000000284 ) ) ;
#175388 = ADVANCED_FACE ( 'NONE', ( #177034, #137856 ), #161310, .F. ) ;
#175389 = ORIENTED_EDGE ( 'NONE', *, *, #154920, .F. ) ;
#175390 = VERTEX_POINT ( 'NONE', #120912 ) ;
#175391 = LINE ( 'NONE', #75006, #236636 ) ;
#175392 = EDGE_CURVE ( 'NONE', #119943, #144042, #74602, .T. ) ;
#175393 = CARTESIAN_POINT ( 'NONE',  ( -18.31572283045012384, -0.7430829278780020086, -242.4583343033048379 ) ) ;
#175394 = PLANE ( 'NONE',  #257225 ) ;
#175395 = DIRECTION ( 'NONE',  ( -0.000000000000000000, -1.000000000000000000, 4.336808689942043611E-14 ) ) ;
#175396 = VERTEX_POINT ( 'NONE', #221244 ) ;
#175397 = DIRECTION ( 'NONE',  ( 1.000000000000000000, -0.000000000000000000, -0.000000000000000000 ) ) ;
#175398 = ADVANCED_FACE ( 'NONE', ( #17918 ), #133029, .T. ) ;
#175399 = FACE_OUTER_BOUND ( 'NONE', #8750, .T. ) ;
#175400 = DIRECTION ( 'NONE',  ( -0.000000000000000000, -0.2128009952263603677, 0.9770955615653313941 ) ) ;
#175401 = EDGE_CURVE ( 'NONE', #236185, #102720, #256473, .T. ) ;
#175402 = EDGE_CURVE ( 'NONE', #129497, #191603, #216192, .T. ) ;
#175403 = CARTESIAN_POINT ( 'NONE',  ( -23.25000000000000000, 73.40000000001185754, -89.79848556176223440 ) ) ;
#175404 = EDGE_CURVE ( 'NONE', #156098, #33432, #20597, .T. ) ;
#175405 = CIRCLE ( 'NONE', #62945, 0.09999999999999817368 ) ;
#175406 = VERTEX_POINT ( 'NONE', #140429 ) ;
#175407 = DIRECTION ( 'NONE',  ( 1.000000000000000000, 0.000000000000000000, 0.000000000000000000 ) ) ;
#175408 = CARTESIAN_POINT ( 'NONE',  ( -16.87683809663750623, 66.05000000001187743, -89.62074346632789457 ) ) ;
#175409 = CARTESIAN_POINT ( 'NONE',  ( 18.59999999999999787, 77.40560538581968331, -241.7331240221339783 ) ) ;
#175410 = CARTESIAN_POINT ( 'NONE',  ( -22.59999999999999787, 0.1008583691098682150, -122.2504328765106294 ) ) ;
#175411 = LINE ( 'NONE', #254854, #79632 ) ;
#175412 = EDGE_CURVE ( 'NONE', #131827, #127173, #21794, .T. ) ;
#175414 = EDGE_LOOP ( 'NONE', ( #101784, #66474, #73757, #211079 ) ) ;
#175413 = DIRECTION ( 'NONE',  ( -1.000000000000000000, -0.000000000000000000, 0.000000000000000000 ) ) ;
#175415 = DIRECTION ( 'NONE',  ( 0.000000000000000000, 1.000000000000000000, -6.308085367188393199E-16 ) ) ;
#175416 = EDGE_CURVE ( 'NONE', #107466, #191501, #81711, .T. ) ;
#175417 = DIRECTION ( 'NONE',  ( -1.000000000000000000, -0.000000000000000000, -0.000000000000000000 ) ) ;
#175418 = CARTESIAN_POINT ( 'NONE',  ( 21.05000000000000071, 69.35000000001231513, -160.0060803140843859 ) ) ;
#175419 = VERTEX_POINT ( 'NONE', #240833 ) ;
#175420 = FACE_OUTER_BOUND ( 'NONE', #159713, .T. ) ;
#175421 = DIRECTION ( 'NONE',  ( 1.000000000000000000, -0.000000000000000000, -0.000000000000000000 ) ) ;
#175422 = DIRECTION ( 'NONE',  ( 0.000000000000000000, 0.000000000000000000, -1.000000000000000000 ) ) ;
#175423 = CYLINDRICAL_SURFACE ( 'NONE', #204296, 0.5000000000000014433 ) ;
#175425 = AXIS2_PLACEMENT_3D ( 'NONE', #45443, #207093, #124990 ) ;
#175424 = DIRECTION ( 'NONE',  ( 0.000000000000000000, 0.8700118002898321601, -0.4930308989875230030 ) ) ;
#175427 = AXIS2_PLACEMENT_3D ( 'NONE', #210569, #33249, #233971 ) ;
#175426 = DIRECTION ( 'NONE',  ( 0.000000000000000000, -0.2128009952263479332, 0.9770955615653342807 ) ) ;
#175428 = VERTEX_POINT ( 'NONE', #160033 ) ;
#175429 = ORIENTED_EDGE ( 'NONE', *, *, #145854, .T. ) ;
#175430 = AXIS2_PLACEMENT_3D ( 'NONE', #169420, #49430, #191541 ) ;
#175431 = DIRECTION ( 'NONE',  ( -0.000000000000000000, 0.000000000000000000, -1.000000000000000000 ) ) ;
#175432 = DIRECTION ( 'NONE',  ( 0.000000000000000000, 0.2128009952263601456, -0.9770955615653316162 ) ) ;
#175433 = CARTESIAN_POINT ( 'NONE',  ( -18.50000000000000000, 11.75000000001115552, -146.1500000000000341 ) ) ;
#175434 = DIRECTION ( 'NONE',  ( 0.000000000000000000, 0.000000000000000000, -1.000000000000000000 ) ) ;
#175435 = CYLINDRICAL_SURFACE ( 'NONE', #100750, 4.000000000000003553 ) ;
#175436 = AXIS2_PLACEMENT_3D ( 'NONE', #113634, #90195, #91510 ) ;
#175437 = CARTESIAN_POINT ( 'NONE',  ( -21.05000000000000071, 36.65892442174472876, -249.5511627012454596 ) ) ;
#175438 = CARTESIAN_POINT ( 'NONE',  ( -18.59999999999999787, 61.45319073932094511, -212.2704122313080006 ) ) ;
#175439 = EDGE_LOOP ( 'NONE', ( #124489, #81945, #206395, #253403 ) ) ;
#175440 = DIRECTION ( 'NONE',  ( 1.000000000000000000, -0.000000000000000000, -0.000000000000000000 ) ) ;
#175441 = VERTEX_POINT ( 'NONE', #122174 ) ;
#175442 = ORIENTED_EDGE ( 'NONE', *, *, #144185, .T. ) ;
#175443 = DIRECTION ( 'NONE',  ( 0.000000000000000000, -6.982962677686266711E-15, 1.000000000000000000 ) ) ;
#175444 = CARTESIAN_POINT ( 'NONE',  ( -21.14999999999999858, 6.540656951712399803, -100.5000000000000284 ) ) ;
#175445 = DIRECTION ( 'NONE',  ( 1.000000000000000000, 0.000000000000000000, 0.000000000000000000 ) ) ;
#175447 = ORIENTED_EDGE ( 'NONE', *, *, #175632, .F. ) ;
#175446 = DIRECTION ( 'NONE',  ( -0.000000000000000000, 7.272083257015735086E-15, -1.000000000000000000 ) ) ;
#175448 = CARTESIAN_POINT ( 'NONE',  ( -22.50000000000000000, 11.48087284840413425, -198.4995883060917947 ) ) ;
#175449 = FACE_OUTER_BOUND ( 'NONE', #57592, .T. ) ;
#175450 = DIRECTION ( 'NONE',  ( -0.000000000000000000, 1.000000000000000000, -0.000000000000000000 ) ) ;
#175451 = ORIENTED_EDGE ( 'NONE', *, *, #237595, .F. ) ;
#175452 = DIRECTION ( 'NONE',  ( 1.000000000000000000, 0.000000000000000000, 0.000000000000000000 ) ) ;
#175453 = EDGE_CURVE ( 'NONE', #112954, #191992, #120556, .T. ) ;
#175454 = DIRECTION ( 'NONE',  ( 1.000000000000000000, -0.000000000000000000, 0.000000000000000000 ) ) ;
#175455 = CIRCLE ( 'NONE', #92213, 0.09999999999999939493 ) ;
#175456 = AXIS2_PLACEMENT_3D ( 'NONE', #204288, #25674, #187327 ) ;
#175457 = CARTESIAN_POINT ( 'NONE',  ( -23.25000000000000355, 5.650000000011139001, -76.25000000000004263 ) ) ;
#175458 = DIRECTION ( 'NONE',  ( 0.000000000000000000, -0.9908441862701782288, 0.1350103645450542456 ) ) ;
#175459 = AXIS2_PLACEMENT_3D ( 'NONE', #182117, #42600, #222492 ) ;
#175460 = EDGE_CURVE ( 'NONE', #135788, #158987, #219974, .T. ) ;
#175461 = ORIENTED_EDGE ( 'NONE', *, *, #203124, .F. ) ;
#175462 = FACE_OUTER_BOUND ( 'NONE', #202200, .T. ) ;
#175464 = ADVANCED_FACE ( 'NONE', ( #179591 ), #87197, .T. ) ;
#175463 = CARTESIAN_POINT ( 'NONE',  ( -20.94999999999999929, 11.65000000001115232, -100.5000000000000426 ) ) ;
#175466 = EDGE_CURVE ( 'NONE', #147427, #136008, #218677, .T. ) ;
#175465 = ORIENTED_EDGE ( 'NONE', *, *, #1595, .T. ) ;
#175467 = DIRECTION ( 'NONE',  ( 2.952720810173289112E-16, -1.000000000000000000, 0.000000000000000000 ) ) ;
#175468 = DIRECTION ( 'NONE',  ( 3.469446951953492389E-14, 0.9228863568391486583, 0.3850724248244262182 ) ) ;
#175469 = LINE ( 'NONE', #97144, #247217 ) ;
#175470 = AXIS2_PLACEMENT_3D ( 'NONE', #11527, #55729, #231866 ) ;
#175471 = ORIENTED_EDGE ( 'NONE', *, *, #172699, .T. ) ;
#175472 = CARTESIAN_POINT ( 'NONE',  ( 20.95263205890719149, 8.895740107905213634, -41.98950840694161712 ) ) ;
#175473 = ORIENTED_EDGE ( 'NONE', *, *, #195071, .F. ) ;
#175474 = EDGE_CURVE ( 'NONE', #25862, #235134, #141719, .T. ) ;
#175475 = EDGE_LOOP ( 'NONE', ( #132739, #6704, #118045, #194589 ) ) ;
#175476 = LINE ( 'NONE', #217119, #176712 ) ;
#175477 = DIRECTION ( 'NONE',  ( 0.000000000000000000, 0.000000000000000000, -1.000000000000000000 ) ) ;
#175478 = CIRCLE ( 'NONE', #125408, 3.999999999999996447 ) ;
#175480 = ORIENTED_EDGE ( 'NONE', *, *, #65889, .F. ) ;
#175479 = CARTESIAN_POINT ( 'NONE',  ( -21.05000000000000071, -1.162701749926853712, -41.40000000000000568 ) ) ;
#175481 = CARTESIAN_POINT ( 'NONE',  ( -20.54999999999999716, 9.350000000011156942, -188.7499999999999716 ) ) ;
#175482 = DIRECTION ( 'NONE',  ( -3.469446951953995998E-14, 0.000000000000000000, -1.000000000000000000 ) ) ;
#175483 = CARTESIAN_POINT ( 'NONE',  ( -20.94999999999999929, 65.70729864261026876, -131.0657455973724836 ) ) ;
#175484 = FACE_OUTER_BOUND ( 'NONE', #130370, .T. ) ;
#175485 = CARTESIAN_POINT ( 'NONE',  ( -21.05000000000000071, 7.128833340093095217, -233.7327013124392749 ) ) ;
#175486 = AXIS2_PLACEMENT_3D ( 'NONE', #5697, #27896, #44855 ) ;
#175487 = DIRECTION ( 'NONE',  ( 0.000000000000000000, 0.000000000000000000, -1.000000000000000000 ) ) ;
#175488 = CARTESIAN_POINT ( 'NONE',  ( 21.15000000000004476, 84.00000000001119815, -37.18565239344504647 ) ) ;
#175491 = ORIENTED_EDGE ( 'NONE', *, *, #55179, .F. ) ;
#175490 = ADVANCED_FACE ( 'NONE', ( #40093 ), #19213, .T. ) ;
#175489 = DIRECTION ( 'NONE',  ( 0.000000000000000000, 0.000000000000000000, -1.000000000000000000 ) ) ;
#175493 = EDGE_LOOP ( 'NONE', ( #39026, #9100 ) ) ;
#175492 = CARTESIAN_POINT ( 'NONE',  ( -20.94999999999999929, 87.65000000001163016, -66.42310748452423752 ) ) ;
#175495 = DIRECTION ( 'NONE',  ( 1.000000000000000000, 0.000000000000000000, 0.000000000000000000 ) ) ;
#175494 = FACE_OUTER_BOUND ( 'NONE', #19313, .T. ) ;
#175497 = ORIENTED_EDGE ( 'NONE', *, *, #240741, .F. ) ;
#175496 = CARTESIAN_POINT ( 'NONE',  ( 23.14999999999998437, 76.00000000001195133, -103.0231074845243171 ) ) ;
#175498 = AXIS2_PLACEMENT_3D ( 'NONE', #153419, #75149, #169121 ) ;
#175499 = ORIENTED_EDGE ( 'NONE', *, *, #9090, .F. ) ;
#175500 = ADVANCED_FACE ( 'NONE', ( #201698 ), #227672, .F. ) ;
#175501 = FACE_OUTER_BOUND ( 'NONE', #145759, .T. ) ;
#175502 = FACE_OUTER_BOUND ( 'NONE', #227582, .T. ) ;
#175503 = AXIS2_PLACEMENT_3D ( 'NONE', #10836, #51205, #8274 ) ;
#175504 = CARTESIAN_POINT ( 'NONE',  ( -23.25000000000000000, 64.25000000001165290, -69.52310748452440237 ) ) ;
#175505 = VECTOR ( 'NONE', #80735, 1000.000000000000000 ) ;
#175506 = CARTESIAN_POINT ( 'NONE',  ( 19.75857864376269291, 11.75000000001116263, -58.35000000000000853 ) ) ;
#175507 = CARTESIAN_POINT ( 'NONE',  ( -23.25000000000000000, 77.14957036958705316, -28.20719500002235236 ) ) ;
#175509 = ADVANCED_FACE ( 'NONE', ( #185987 ), #124739, .F. ) ;
#175508 = DIRECTION ( 'NONE',  ( 0.000000000000000000, -0.2128009952263603954, 0.9770955615653315052 ) ) ;
#175510 = CIRCLE ( 'NONE', #150554, 0.09999999999998898659 ) ;
#175511 = EDGE_CURVE ( 'NONE', #203548, #179043, #205534, .T. ) ;
#175512 = DIRECTION ( 'NONE',  ( 0.000000000000000000, -0.9371753822965326330, 0.3488585713686107592 ) ) ;
#175513 = ORIENTED_EDGE ( 'NONE', *, *, #237466, .T. ) ;
#175514 = ORIENTED_EDGE ( 'NONE', *, *, #227545, .F. ) ;
#175515 = CARTESIAN_POINT ( 'NONE',  ( -22.10000000000000142, -11.75000000000000000, 32.89999999999999858 ) ) ;
#175517 = EDGE_CURVE ( 'NONE', #61798, #256256, #165146, .T. ) ;
#175516 = AXIS2_PLACEMENT_3D ( 'NONE', #76994, #136968, #117416 ) ;
#175518 = VERTEX_POINT ( 'NONE', #184694 ) ;
#175519 = AXIS2_PLACEMENT_3D ( 'NONE', #38890, #80532, #216213 ) ;
#175520 = FACE_OUTER_BOUND ( 'NONE', #241055, .T. ) ;
#175521 = FACE_OUTER_BOUND ( 'NONE', #121436, .T. ) ;
#175522 = AXIS2_PLACEMENT_3D ( 'NONE', #17585, #116696, #137529 ) ;
#175523 = FACE_OUTER_BOUND ( 'NONE', #257567, .T. ) ;
#175524 = ORIENTED_EDGE ( 'NONE', *, *, #144821, .F. ) ;
#175525 = CARTESIAN_POINT ( 'NONE',  ( -12.92414019175886430, 66.58236703690573677, -118.3741590187920565 ) ) ;
#175526 = VERTEX_POINT ( 'NONE', #204254 ) ;
#175527 = ADVANCED_FACE ( 'NONE', ( #9913 ), #50123, .T. ) ;
#175529 = AXIS2_PLACEMENT_3D ( 'NONE', #114563, #156289, #208855 ) ;
#175528 = LINE ( 'NONE', #60669, #13004 ) ;
#175530 = ORIENTED_EDGE ( 'NONE', *, *, #88795, .F. ) ;
#175531 = FACE_OUTER_BOUND ( 'NONE', #117686, .T. ) ;
#175532 = CARTESIAN_POINT ( 'NONE',  ( -2.995603634470891112E-16, 69.35000000001222986, -148.8731074845244109 ) ) ;
#175533 = EDGE_CURVE ( 'NONE', #116556, #204714, #106421, .T. ) ;
#175534 = DIRECTION ( 'NONE',  ( -1.000000000000000000, 0.000000000000000000, 0.000000000000000000 ) ) ;
#175535 = ORIENTED_EDGE ( 'NONE', *, *, #200275, .T. ) ;
#175536 = LINE ( 'NONE', #73880, #77662 ) ;
#175538 = ORIENTED_EDGE ( 'NONE', *, *, #179562, .F. ) ;
#175537 = CARTESIAN_POINT ( 'NONE',  ( 23.40000000000005542, 77.83551161375993388, -47.52760213295649550 ) ) ;
#175539 = AXIS2_PLACEMENT_3D ( 'NONE', #203928, #240492, #3141 ) ;
#175540 = DIRECTION ( 'NONE',  ( 1.000000000000000000, 0.000000000000000000, 0.000000000000000000 ) ) ;
#175541 = CIRCLE ( 'NONE', #63074, 0.09999999999999939493 ) ;
#175543 = VERTEX_POINT ( 'NONE', #144262 ) ;
#175542 = VECTOR ( 'NONE', #160347, 1000.000000000000000 ) ;
#175544 = AXIS2_PLACEMENT_3D ( 'NONE', #81731, #223826, #910 ) ;
#175545 = ORIENTED_EDGE ( 'NONE', *, *, #81848, .F. ) ;
#175546 = FACE_BOUND ( 'NONE', #183931, .T. ) ;
#175547 = ORIENTED_EDGE ( 'NONE', *, *, #26231, .F. ) ;
#175548 = CARTESIAN_POINT ( 'NONE',  ( 20.94999999999999929, 76.00000000001141132, -34.02310748452431710 ) ) ;
#175549 = CARTESIAN_POINT ( 'NONE',  ( 21.00000000000000000, 1.410778198689825347, -7.973296578895943121 ) ) ;
#175550 = DIRECTION ( 'NONE',  ( 0.000000000000000000, -0.4930308989875170078, -0.8700118002898356018 ) ) ;
#175551 = CARTESIAN_POINT ( 'NONE',  ( -21.11927991906891577, 0.009083679485028523307, -60.55150688150853711 ) ) ;
#175552 = VERTEX_POINT ( 'NONE', #127298 ) ;
#175553 = CARTESIAN_POINT ( 'NONE',  ( -21.05000000000000071, 1.835341550235567887, -78.55515129256302487 ) ) ;
#175554 = DIRECTION ( 'NONE',  ( 0.000000000000000000, 0.000000000000000000, -1.000000000000000000 ) ) ;
#175555 = FACE_OUTER_BOUND ( 'NONE', #191413, .T. ) ;
#175556 = EDGE_LOOP ( 'NONE', ( #84237, #177814, #115696, #87435 ) ) ;
#175557 = LINE ( 'NONE', #193822, #130339 ) ;
#175558 = EDGE_LOOP ( 'NONE', ( #175733, #188284, #243265, #143527 ) ) ;
#175559 = FACE_OUTER_BOUND ( 'NONE', #75984, .T. ) ;
#175560 = ORIENTED_EDGE ( 'NONE', *, *, #176133, .T. ) ;
#175561 = DIRECTION ( 'NONE',  ( -1.000000000000000000, -0.000000000000000000, 0.000000000000000000 ) ) ;
#175563 = ORIENTED_EDGE ( 'NONE', *, *, #89946, .T. ) ;
#175562 = DIRECTION ( 'NONE',  ( -0.000000000000000000, -0.000000000000000000, -1.000000000000000000 ) ) ;
#175564 = CARTESIAN_POINT ( 'NONE',  ( -18.49719636458566896, 8.901920981062144023, -245.3987932648529693 ) ) ;
#175565 = ORIENTED_EDGE ( 'NONE', *, *, #80246, .T. ) ;
#175566 = VECTOR ( 'NONE', #248661, 1000.000000000000114 ) ;
#175567 = DIRECTION ( 'NONE',  ( -1.000000000000000000, -1.652117596168391700E-15, -1.153667551319263085E-29 ) ) ;
#175568 = CARTESIAN_POINT ( 'NONE',  ( -20.54999999999999716, 26.34635675162282098, -241.8429480539297174 ) ) ;
#175569 = ORIENTED_EDGE ( 'NONE', *, *, #32023, .T. ) ;
#175570 = FACE_OUTER_BOUND ( 'NONE', #37691, .T. ) ;
#175571 = CARTESIAN_POINT ( 'NONE',  ( -20.85000000106584750, 11.75000000001115197, -194.1555046564733971 ) ) ;
#175572 = EDGE_LOOP ( 'NONE', ( #187846, #9391, #159867, #191271, #201481 ) ) ;
#175573 = ORIENTED_EDGE ( 'NONE', *, *, #49121, .F. ) ;
#175575 = CARTESIAN_POINT ( 'NONE',  ( 22.50000000000000000, 1.115600667400684642E-11, -134.0000000000000000 ) ) ;
#175574 = CIRCLE ( 'NONE', #204595, 0.09999999999999520384 ) ;
#175576 = CARTESIAN_POINT ( 'NONE',  ( -18.39999999999999858, -9.499999999988849808, -73.60018939122203108 ) ) ;
#175577 = EDGE_CURVE ( 'NONE', #235224, #100823, #116271, .T. ) ;
#175579 = EDGE_LOOP ( 'NONE', ( #198438, #97813, #135675, #158647 ) ) ;
#175578 = DIRECTION ( 'NONE',  ( 1.000000000000000000, -7.304098846218134667E-16, -5.100424963727255829E-30 ) ) ;
#175580 = EDGE_CURVE ( 'NONE', #226215, #82768, #146221, .T. ) ;
#175581 = CARTESIAN_POINT ( 'NONE',  ( -20.64999999999999858, 7.150000000011155876, -179.8499999999999943 ) ) ;
#175582 = EDGE_CURVE ( 'NONE', #101028, #85681, #3832, .T. ) ;
#175583 = CARTESIAN_POINT ( 'NONE',  ( 20.12500000000000000, 66.25000000001189449, -94.91133620241009794 ) ) ;
#175585 = LINE ( 'NONE', #217238, #92763 ) ;
#175584 = DIRECTION ( 'NONE',  ( 0.000000000000000000, 0.4930308989875575865, 0.8700118002898125091 ) ) ;
#175586 = DIRECTION ( 'NONE',  ( 0.000000000000000000, 1.000000000000000000, 6.982962677686266711E-15 ) ) ;
#175587 = DIRECTION ( 'NONE',  ( 0.000000000000000000, -1.000000000000000000, -6.982962677686265922E-15 ) ) ;
#175588 = VECTOR ( 'NONE', #81035, 1000.000000000000000 ) ;
#175589 = CARTESIAN_POINT ( 'NONE',  ( 18.46858270002953262, -9.474202674699412796, -40.60202193470386334 ) ) ;
#175590 = AXIS2_PLACEMENT_3D ( 'NONE', #156430, #55979, #213797 ) ;
#175591 = CARTESIAN_POINT ( 'NONE',  ( -18.59999999999999787, 74.13328508995527955, -191.7704322382423641 ) ) ;
#175593 = ORIENTED_EDGE ( 'NONE', *, *, #20523, .F. ) ;
#175592 = AXIS2_PLACEMENT_3D ( 'NONE', #233486, #76947, #238594 ) ;
#175594 = ORIENTED_EDGE ( 'NONE', *, *, #75089, .F. ) ;
#175595 = CARTESIAN_POINT ( 'NONE',  ( 18.47654891039379166, 85.46527494839465078, -162.8971315793296526 ) ) ;
#175597 = ORIENTED_EDGE ( 'NONE', *, *, #85959, .F. ) ;
#175596 = CARTESIAN_POINT ( 'NONE',  ( -18.35668295345803713, 33.92263863280957281, -235.0698407953532296 ) ) ;
#175598 = ORIENTED_EDGE ( 'NONE', *, *, #54344, .F. ) ;
#175599 = ADVANCED_FACE ( 'NONE', ( #128584 ), #29517, .T. ) ;
#175600 = LINE ( 'NONE', #114327, #22867 ) ;
#175601 = ORIENTED_EDGE ( 'NONE', *, *, #215019, .F. ) ;
#175602 = CARTESIAN_POINT ( 'NONE',  ( 20.95083306685154056, 8.916842641890202259, -8.477324853258354054 ) ) ;
#175603 = ORIENTED_EDGE ( 'NONE', *, *, #44357, .T. ) ;
#175604 = AXIS2_PLACEMENT_3D ( 'NONE', #141725, #179599, #122182 ) ;
#175605 =( LENGTH_UNIT ( ) NAMED_UNIT ( * ) SI_UNIT ( .MILLI., .METRE. ) );
#175606 = CARTESIAN_POINT ( 'NONE',  ( 23.14999999999999858, 1.115600667400684642E-11, -200.9999999999999432 ) ) ;
#175608 = VERTEX_POINT ( 'NONE', #92017 ) ;
#175607 = VERTEX_POINT ( 'NONE', #222526 ) ;
#175609 = ORIENTED_EDGE ( 'NONE', *, *, #119989, .T. ) ;
#175610 = ORIENTED_EDGE ( 'NONE', *, *, #194827, .F. ) ;
#175611 = ORIENTED_EDGE ( 'NONE', *, *, #105266, .F. ) ;
#175612 = CARTESIAN_POINT ( 'NONE',  ( 20.94999999999999574, 68.48451787451661232, -224.2224406095231757 ) ) ;
#175613 = FACE_OUTER_BOUND ( 'NONE', #189459, .T. ) ;
#175615 = EDGE_LOOP ( 'NONE', ( #156841, #174735, #14284 ) ) ;
#175614 = FACE_OUTER_BOUND ( 'NONE', #126475, .T. ) ;
#175616 = EDGE_CURVE ( 'NONE', #14870, #107983, #230276, .T. ) ;
#175617 = EDGE_CURVE ( 'NONE', #113573, #10751, #191147, .T. ) ;
#175618 = CARTESIAN_POINT ( 'NONE',  ( -21.53699400384685703, 33.88385736502569756, -243.3566462376632842 ) ) ;
#175619 = CARTESIAN_POINT ( 'NONE',  ( 12.25000000000000355, 12.65163926562330410, -215.1534139431609560 ) ) ;
#175621 = ORIENTED_EDGE ( 'NONE', *, *, #74619, .F. ) ;
#175620 = CARTESIAN_POINT ( 'NONE',  ( -16.94333152886236249, 60.88942040374450215, -221.0717341904871489 ) ) ;
#175622 = CARTESIAN_POINT ( 'NONE',  ( -18.50000000000000000, -1.164121893241208960, -41.41484808557160591 ) ) ;
#175623 = EDGE_LOOP ( 'NONE', ( #233604, #197785, #13058, #230057 ) ) ;
#175624 = DIRECTION ( 'NONE',  ( 1.000000000000000000, 0.000000000000000000, 0.000000000000000000 ) ) ;
#175626 = ORIENTED_EDGE ( 'NONE', *, *, #50165, .T. ) ;
#175625 = CARTESIAN_POINT ( 'NONE',  ( -18.39999999999999858, 85.51932773110476660, -163.0501311079649440 ) ) ;
#175627 = CARTESIAN_POINT ( 'NONE',  ( -18.59999999999999787, 7.675662554762638479, -241.7139905447625381 ) ) ;
#175628 = DIRECTION ( 'NONE',  ( 0.000000000000000000, -1.000000000000000000, 0.000000000000000000 ) ) ;
#175629 = AXIS2_PLACEMENT_3D ( 'NONE', #164574, #244088, #47155 ) ;
#175630 = AXIS2_PLACEMENT_3D ( 'NONE', #229849, #169926, #48633 ) ;
#175632 = EDGE_CURVE ( 'NONE', #229722, #42531, #205317, .T. ) ;
#175631 = CARTESIAN_POINT ( 'NONE',  ( 20.01093837587850288, 11.75000000001116263, -91.75439743459725150 ) ) ;
#175633 = CIRCLE ( 'NONE', #42511, 0.1000000000000028644 ) ;
#175634 = VERTEX_POINT ( 'NONE', #52884 ) ;
#175635 = CARTESIAN_POINT ( 'NONE',  ( -16.79270642812324965, 9.946244216949034822, -46.16106672143809675 ) ) ;
#175636 = CARTESIAN_POINT ( 'NONE',  ( 18.46932045258653332, 85.67068520027807210, -163.3492471115275464 ) ) ;
#175637 = LINE ( 'NONE', #216012, #205531 ) ;
#175638 = EDGE_LOOP ( 'NONE', ( #44145, #117269, #232785, #255501 ) ) ;
#175639 = ORIENTED_EDGE ( 'NONE', *, *, #89467, .F. ) ;
#175640 = CARTESIAN_POINT ( 'NONE',  ( -20.64999999999999858, -9.000000000000001776, -24.10603087734756045 ) ) ;
#175641 = DIRECTION ( 'NONE',  ( 0.000000000000000000, -0.9908441862701782288, 0.1350103645450542456 ) ) ;
#175642 = ORIENTED_EDGE ( 'NONE', *, *, #176756, .F. ) ;
#175643 = DIRECTION ( 'NONE',  ( 0.000000000000000000, -0.1335171055202867274, 0.9910465087640865089 ) ) ;
#175644 = ORIENTED_EDGE ( 'NONE', *, *, #141587, .F. ) ;
#175645 = PLANE ( 'NONE',  #94117 ) ;
#175646 = CARTESIAN_POINT ( 'NONE',  ( -22.00356870070476489, 76.00000000000328271, -177.2773498462649968 ) ) ;
#175647 = AXIS2_PLACEMENT_3D ( 'NONE', #80425, #101258, #77888 ) ;
#175648 = ADVANCED_FACE ( 'NONE', ( #150716 ), #51574, .T. ) ;
#175649 = ORIENTED_EDGE ( 'NONE', *, *, #73348, .F. ) ;
#175650 = CARTESIAN_POINT ( 'NONE',  ( -16.87036670365548474, 65.91505003675624152, -48.57310748452439952 ) ) ;
#175651 = ORIENTED_EDGE ( 'NONE', *, *, #135049, .F. ) ;
#175652 = ORIENTED_EDGE ( 'NONE', *, *, #230271, .F. ) ;
#175653 = ORIENTED_EDGE ( 'NONE', *, *, #166800, .T. ) ;
#175654 = EDGE_CURVE ( 'NONE', #248221, #4663, #149597, .T. ) ;
#175655 = LINE ( 'NONE', #16592, #4493 ) ;
#175656 = DIRECTION ( 'NONE',  ( -0.000000000000000000, 0.1350103645451626311, 0.9908441862701635738 ) ) ;
#175657 = CARTESIAN_POINT ( 'NONE',  ( -23.15000000000000213, 76.00000000001190870, -103.0231074845243029 ) ) ;
#175658 = ADVANCED_FACE ( 'NONE', ( #94578 ), #174173, .F. ) ;
#175659 = DIRECTION ( 'NONE',  ( -7.304098846218134667E-16, -1.000000000000000000, 0.000000000000000000 ) ) ;
#175661 = B_SPLINE_CURVE_WITH_KNOTS ( 'NONE', 3,
 ( #121947, #44977, #202758, #224873, #227449, #82770, #124519, #46244, #244446, #162370 ),
 .UNSPECIFIED., .F., .F.,
 ( 4, 2, 2, 2, 4 ),
 ( 0.000000000000000000, 4.221631689684808797E-05, 8.443263379369617594E-05, 0.0001688652675874713902, 0.0003377305351750226319 ),
 .UNSPECIFIED. ) ;
#175660 = DIRECTION ( 'NONE',  ( 0.000000000000000000, -0.2617529984165031243, -0.9651348961777157509 ) ) ;
#175662 = AXIS2_PLACEMENT_3D ( 'NONE', #51075, #250591, #193212 ) ;
#175664 = DIRECTION ( 'NONE',  ( -1.000000000000000000, -3.190570557967288949E-16, -6.948722487160392945E-17 ) ) ;
#175663 = DIRECTION ( 'NONE',  ( 1.000000000000000000, 0.000000000000000000, 0.000000000000000000 ) ) ;
#175666 = ORIENTED_EDGE ( 'NONE', *, *, #160933, .F. ) ;
#175665 = LINE ( 'NONE', #92250, #139685 ) ;
#175667 = DIRECTION ( 'NONE',  ( 0.000000000000000000, 1.000000000000000000, 6.982962677686266711E-15 ) ) ;
#175668 = EDGE_LOOP ( 'NONE', ( #101745, #132158, #7572, #205875, #32394 ) ) ;
#175669 = EDGE_CURVE ( 'NONE', #12539, #139324, #131144, .T. ) ;
#175670 = CARTESIAN_POINT ( 'NONE',  ( -13.54795643572457919, 9.450668889178686527, -149.0555464902073481 ) ) ;
#175671 = EDGE_CURVE ( 'NONE', #132129, #234753, #24709, .T. ) ;
#175672 = EDGE_LOOP ( 'NONE', ( #159267, #74774, #256407, #41211 ) ) ;
#175673 = ORIENTED_EDGE ( 'NONE', *, *, #83653, .T. ) ;
#175674 = CARTESIAN_POINT ( 'NONE',  ( 18.59999999999997655, 0.000000000000000000, -33.50000000000000000 ) ) ;
#175675 = CIRCLE ( 'NONE', #229815, 0.1000000000000000749 ) ;
#175676 = DIRECTION ( 'NONE',  ( 0.000000000000000000, 0.000000000000000000, 1.000000000000000000 ) ) ;
#175677 = LINE ( 'NONE', #119557, #16956 ) ;
#175678 = VERTEX_POINT ( 'NONE', #153321 ) ;
#175679 = DIRECTION ( 'NONE',  ( -0.7071067811865475727, 0.2890913453342130457, -0.6453109281988448354 ) ) ;
#175680 = AXIS2_PLACEMENT_3D ( 'NONE', #13566, #250866, #89229 ) ;
#175681 = ADVANCED_FACE ( 'NONE', ( #234088 ), #149452, .F. ) ;
#175682 = DIRECTION ( 'NONE',  ( 1.000000000000000000, 0.000000000000000000, 0.000000000000000000 ) ) ;
#175685 = EDGE_CURVE ( 'NONE', #212201, #252532, #66375, .T. ) ;
#175684 = EDGE_CURVE ( 'NONE', #12615, #194376, #112873, .T. ) ;
#175683 = AXIS2_PLACEMENT_3D ( 'NONE', #174785, #73106, #210025 ) ;
#175686 = ORIENTED_EDGE ( 'NONE', *, *, #3574, .T. ) ;
#175687 = ORIENTED_EDGE ( 'NONE', *, *, #122426, .T. ) ;
#175688 = VECTOR ( 'NONE', #129835, 1000.000000000000000 ) ;
#175689 = FACE_OUTER_BOUND ( 'NONE', #154534, .T. ) ;
#175690 = ORIENTED_EDGE ( 'NONE', *, *, #129473, .T. ) ;
#175691 = DIRECTION ( 'NONE',  ( 0.000000000000000000, 0.000000000000000000, -1.000000000000000000 ) ) ;
#175692 = CARTESIAN_POINT ( 'NONE',  ( -1.820710678118657944, -9.929289321870186313, -192.2499999999999716 ) ) ;
#175693 = ORIENTED_EDGE ( 'NONE', *, *, #196282, .T. ) ;
#175694 = CARTESIAN_POINT ( 'NONE',  ( 21.05000000000000071, 67.17357026049469937, -94.60905277158067861 ) ) ;
#175695 = EDGE_CURVE ( 'NONE', #157545, #145044, #170326, .T. ) ;
#175696 = CARTESIAN_POINT ( 'NONE',  ( -21.05000000000000071, 6.412126976762837494, -199.7058512474018244 ) ) ;
#175697 = CARTESIAN_POINT ( 'NONE',  ( 21.05000012384952868, 65.37127970113776598, -157.8451301544894534 ) ) ;
#175698 = ORIENTED_EDGE ( 'NONE', *, *, #250324, .F. ) ;
#175699 = TOROIDAL_SURFACE ( 'NONE', #238391, 0.2000000000000000111, 0.1000000000000000056 ) ;
#175701 = AXIS2_PLACEMENT_3D ( 'NONE', #248154, #44819, #86479 ) ;
#175700 = CARTESIAN_POINT ( 'NONE',  ( 20.94999999999999574, 35.88801296822693843, -234.5558624753690538 ) ) ;
#175702 = EDGE_CURVE ( 'NONE', #30427, #40157, #232800, .T. ) ;
#175703 = CARTESIAN_POINT ( 'NONE',  ( 18.59999999999999076, 6.650000000011155876, -188.8499999999999659 ) ) ;
#175704 = AXIS2_PLACEMENT_3D ( 'NONE', #122240, #25703, #201760 ) ;
#175705 = CARTESIAN_POINT ( 'NONE',  ( -22.48479450179659977, 26.00783696130147504, -254.2712270987252339 ) ) ;
#175706 = EDGE_CURVE ( 'NONE', #6907, #16586, #7948, .T. ) ;
#175708 = EDGE_CURVE ( 'NONE', #70203, #197443, #112357, .T. ) ;
#175707 = AXIS2_PLACEMENT_3D ( 'NONE', #195096, #97201, #55516 ) ;
#175709 = ORIENTED_EDGE ( 'NONE', *, *, #40577, .T. ) ;
#175710 = VECTOR ( 'NONE', #193993, 1000.000000000000000 ) ;
#175711 = EDGE_CURVE ( 'NONE', #51418, #208604, #116456, .T. ) ;
#175712 = CARTESIAN_POINT ( 'NONE',  ( -20.64999999999999858, 85.40000000001148805, -45.91707660717669626 ) ) ;
#175713 = ORIENTED_EDGE ( 'NONE', *, *, #215305, .T. ) ;
#175714 = DIRECTION ( 'NONE',  ( 0.000000000000000000, 0.000000000000000000, 1.000000000000000000 ) ) ;
#175715 = AXIS2_PLACEMENT_3D ( 'NONE', #64209, #143734, #164600 ) ;
#175716 = CARTESIAN_POINT ( 'NONE',  ( 20.94999999999999574, -1.249999999988843369, -41.50000000000000000 ) ) ;
#175717 = CARTESIAN_POINT ( 'NONE',  ( 20.94999999999999574, -1.162701749938009677, -8.000000000000000000 ) ) ;
#175718 = ADVANCED_FACE ( 'NONE', ( #37204 ), #121870, .F. ) ;
#175719 = CARTESIAN_POINT ( 'NONE',  ( -20.85000000000000142, 87.65000000001245439, -170.0231074845242745 ) ) ;
#175720 = CARTESIAN_POINT ( 'NONE',  ( -16.89797118371614459, 9.976380722655427746, -46.06270663244127661 ) ) ;
#175721 = CARTESIAN_POINT ( 'NONE',  ( -23.15000000000000213, 1.115600667400684642E-11, -167.4999999999999716 ) ) ;
#175722 = ORIENTED_EDGE ( 'NONE', *, *, #89824, .F. ) ;
#175723 = DIRECTION ( 'NONE',  ( 0.000000000000000000, 1.000000000000000000, 0.000000000000000000 ) ) ;
#175724 = CARTESIAN_POINT ( 'NONE',  ( 21.04999999999908411, 67.22371710472138773, -124.3651984818718574 ) ) ;
#175726 = EDGE_CURVE ( 'NONE', #11088, #227300, #137280, .T. ) ;
#175725 = DIRECTION ( 'NONE',  ( 0.000000000000000000, -1.000000000000000000, 0.000000000000000000 ) ) ;
#175727 = CARTESIAN_POINT ( 'NONE',  ( -20.85000000000000142, 1.115600667400684642E-11, -100.5000000000000426 ) ) ;
#175728 = AXIS2_PLACEMENT_3D ( 'NONE', #100988, #22817, #59305 ) ;
#175729 = AXIS2_PLACEMENT_3D ( 'NONE', #58310, #33690, #97426 ) ;
#175730 = CARTESIAN_POINT ( 'NONE',  ( -23.15000000000000213, -11.64999999998884483, -21.75000000000000355 ) ) ;
#175731 = VECTOR ( 'NONE', #52905, 1000.000000000000000 ) ;
#175732 = AXIS2_PLACEMENT_3D ( 'NONE', #128849, #243647, #248796 ) ;
#175733 = ORIENTED_EDGE ( 'NONE', *, *, #186952, .F. ) ;
#175734 = ORIENTED_EDGE ( 'NONE', *, *, #47184, .T. ) ;
#175735 = CARTESIAN_POINT ( 'NONE',  ( 20.73486653747088582, 45.23934133962701765, -237.7629717664446503 ) ) ;
#175736 = DIRECTION ( 'NONE',  ( 0.000000000000000000, 0.000000000000000000, 1.000000000000000000 ) ) ;
#175737 = DIRECTION ( 'NONE',  ( -1.652117596168391700E-15, -1.000000000000000000, 0.000000000000000000 ) ) ;
#175738 = CARTESIAN_POINT ( 'NONE',  ( 18.59999999999999076, 65.79142135624930177, -115.1731074845243796 ) ) ;
#175739 = CYLINDRICAL_SURFACE ( 'NONE', #237017, 0.09999999999999939493 ) ;
#175740 = ADVANCED_FACE ( 'NONE', ( #200114 ), #18898, .F. ) ;
#175741 = EDGE_LOOP ( 'NONE', ( #111075, #167482, #98068, #210889 ) ) ;
#175742 = DIRECTION ( 'NONE',  ( 1.000000000000000000, -3.265361837132813093E-16, -2.280189983783949500E-30 ) ) ;
#175743 = CARTESIAN_POINT ( 'NONE',  ( -23.25000000000000000, 7.021664781911246322, -137.8335654018973457 ) ) ;
#175744 = VERTEX_POINT ( 'NONE', #21494 ) ;
#175745 = CYLINDRICAL_SURFACE ( 'NONE', #242075, 0.09999999999999939493 ) ;
#175746 = CARTESIAN_POINT ( 'NONE',  ( -18.59999999999999787, 0.5876173420563349792, -209.1618981382189588 ) ) ;
#175747 = VECTOR ( 'NONE', #168310, 1000.000000000000000 ) ;
#175748 = ORIENTED_EDGE ( 'NONE', *, *, #167567, .F. ) ;
#175749 = FACE_OUTER_BOUND ( 'NONE', #71024, .T. ) ;
#175750 = ORIENTED_EDGE ( 'NONE', *, *, #186996, .F. ) ;
#175751 = DIRECTION ( 'NONE',  ( -1.000000000000000000, 0.000000000000000000, 0.000000000000000000 ) ) ;
#175752 = CARTESIAN_POINT ( 'NONE',  ( 21.07928932188134397, 69.67148334361907303, -170.1220026301788266 ) ) ;
#175753 = LINE ( 'NONE', #156196, #28687 ) ;
#175754 = CARTESIAN_POINT ( 'NONE',  ( 21.22070241538126467, 75.90108096947739114, -176.4930537573939944 ) ) ;
#175755 = DIRECTION ( 'NONE',  ( 0.000000000000000000, 1.000000000000000000, 6.982962677686266711E-15 ) ) ;
#175756 = CARTESIAN_POINT ( 'NONE',  ( 20.94999999999999929, 76.00000000001142553, -36.02310748452432421 ) ) ;
#175757 = DIRECTION ( 'NONE',  ( 0.000000000000000000, -0.8814952561688390587, 0.4721928772777421734 ) ) ;
#175758 = FACE_OUTER_BOUND ( 'NONE', #167323, .T. ) ;
#175759 = ADVANCED_FACE ( 'NONE', ( #236658 ), #99692, .F. ) ;
#175760 = CARTESIAN_POINT ( 'NONE',  ( 18.44364597020196683, -7.771168315469450860, -209.9159040159132417 ) ) ;
#175761 = DIRECTION ( 'NONE',  ( -1.000000000000000000, 0.000000000000000000, 0.000000000000000000 ) ) ;
#175762 = CARTESIAN_POINT ( 'NONE',  ( -16.92507428761700083, 30.15044400021737658, -234.7771091759292688 ) ) ;
#175763 = CARTESIAN_POINT ( 'NONE',  ( 21.05000000000000071, 18.94908112497232011, -227.8991131484155517 ) ) ;
#175764 = ORIENTED_EDGE ( 'NONE', *, *, #20918, .F. ) ;
#175765 = EDGE_CURVE ( 'NONE', #153726, #66771, #62270, .T. ) ;
#175766 = CARTESIAN_POINT ( 'NONE',  ( 21.05000000000000071, 10.72371710471867701, -79.15000000000004832 ) ) ;
#175767 = DIRECTION ( 'NONE',  ( 0.000000000000000000, 0.8814952561688440547, -0.4721928772777327921 ) ) ;
#175768 = AXIS2_PLACEMENT_3D ( 'NONE', #129209, #190488, #146186 ) ;
#175769 = ORIENTED_EDGE ( 'NONE', *, *, #10222, .F. ) ;
#175770 = FACE_OUTER_BOUND ( 'NONE', #241493, .T. ) ;
#175772 = ADVANCED_FACE ( 'NONE', ( #138808 ), #174759, .T. ) ;
#175771 = LINE ( 'NONE', #96197, #171080 ) ;
#175773 = LINE ( 'NONE', #111948, #189356 ) ;
#175774 = ADVANCED_FACE ( 'NONE', ( #201386 ), #199855, .F. ) ;
#175775 = APPLICATION_CONTEXT ( 'automotive_design' ) ;
#175776 = ORIENTED_EDGE ( 'NONE', *, *, #69972, .F. ) ;
#175777 = CARTESIAN_POINT ( 'NONE',  ( 21.06025298249095457, 6.342459739380975847, 12.00000000173893078 ) ) ;
#175778 = DIRECTION ( 'NONE',  ( 0.000000000000000000, 0.000000000000000000, 1.000000000000000000 ) ) ;
#175779 = ORIENTED_EDGE ( 'NONE', *, *, #13722, .T. ) ;
#175780 = DIRECTION ( 'NONE',  ( 1.000000000000000000, 0.000000000000000000, 0.000000000000000000 ) ) ;
#175781 = DIRECTION ( 'NONE',  ( 0.000000000000000000, 0.9126074666063545004, 0.4088369013363783999 ) ) ;
#175782 = AXIS2_PLACEMENT_3D ( 'NONE', #218972, #82001, #40389 ) ;
#175783 = AXIS2_PLACEMENT_3D ( 'NONE', #143984, #5744, #226072 ) ;
#175784 = VERTEX_POINT ( 'NONE', #159708 ) ;
#175785 = CARTESIAN_POINT ( 'NONE',  ( 20.94999999999999929, 45.93587830916155212, -239.9163948487882863 ) ) ;
#175786 =( BOUNDED_SURFACE ( )  B_SPLINE_SURFACE ( 3, 2, ( 
 ( #85328, #67082, #187054 ),
 ( #164899, #127056, #147915 ),
 ( #207902, #50079, #25404 ),
 ( #166216, #84018, #227431 ),
 ( #48794, #209149, #146588 ),
 ( #65793, #47496, #103607 ),
 ( #145317, #7096, #183188 ),
 ( #206589, #128352, #46220 ) ),
 .UNSPECIFIED., .F., .F., .F. ) 
 B_SPLINE_SURFACE_WITH_KNOTS ( ( 4, 2, 2, 4 ),
 ( 3, 3 ),
 ( 0.0001723339234021411192, 0.0002782939632049912849, 0.0003842540030078414777, 0.0005961740826135418633 ),
 ( 0.000000000000000000, 1.000000000000000000 ),
 .UNSPECIFIED. ) 
 GEOMETRIC_REPRESENTATION_ITEM ( )  RATIONAL_B_SPLINE_SURFACE ( (
 ( 1.000000000000000000, 0.9504532311154628710, 1.000000000000000000),
 ( 1.000000000000000000, 0.9506023220709669541, 1.000000000000000000),
 ( 1.000000000000000000, 0.9395774818181893417, 1.000000000000000000),
 ( 1.000000000000000000, 0.9079328464647246077, 1.000000000000000000),
 ( 1.000000000000000000, 0.8875702416203912204, 1.000000000000000000),
 ( 1.000000000000000000, 0.8205919608043565905, 1.000000000000000000),
 ( 1.000000000000000000, 0.7666842783596220512, 1.000000000000000000),
 ( 1.000000000000000000, 0.7071067811864205632, 1.000000000000000000) ) ) 
 REPRESENTATION_ITEM ( '' )  SURFACE ( )  );
#175787 = EDGE_LOOP ( 'NONE', ( #174055, #64787, #89678, #162508 ) ) ;
#175788 = FACE_OUTER_BOUND ( 'NONE', #4472, .T. ) ;
#175789 = CARTESIAN_POINT ( 'NONE',  ( 20.95512820512820440, 67.12384868372393498, -124.3731074845243683 ) ) ;
#175791 = LINE ( 'NONE', #40143, #120189 ) ;
#175790 = UNCERTAINTY_MEASURE_WITH_UNIT (LENGTH_MEASURE( 1.000000000000000082E-05 ), #56340, 'distance_accuracy_value', 'NONE');
#175792 = DIRECTION ( 'NONE',  ( -1.000000000000000000, -2.952720810173289112E-16, 0.000000000000000000 ) ) ;
#175793 = CARTESIAN_POINT ( 'NONE',  ( -16.77683809663752257, 9.945835743204145984, -12.66394901910421034 ) ) ;
#175794 = CARTESIAN_POINT ( 'NONE',  ( -14.11697426661281440, 46.48157447062519765, -234.7876710066568648 ) ) ;
#175795 = AXIS2_PLACEMENT_3D ( 'NONE', #180722, #2051, #41230 ) ;
#175796 = DIRECTION ( 'NONE',  ( -0.8049926720990043805, 0.2425566999317304295, -0.5414360951997322369 ) ) ;
#175797 = CARTESIAN_POINT ( 'NONE',  ( -18.34374000495059676, 64.52683809664929981, -78.77310748452438816 ) ) ;
#175799 = EDGE_LOOP ( 'NONE', ( #198559, #32570, #41210, #46124 ) ) ;
#175798 = CARTESIAN_POINT ( 'NONE',  ( -18.44362607810620602, -9.490496158073668198, -40.55795386684712156 ) ) ;
#175800 = ORIENTED_EDGE ( 'NONE', *, *, #52665, .F. ) ;
#175802 = CARTESIAN_POINT ( 'NONE',  ( -20.54999999999999716, 74.00000000001229239, -156.7984855617622770 ) ) ;
#175801 = LINE ( 'NONE', #122231, #182748 ) ;
#175804 = VERTEX_POINT ( 'NONE', #180555 ) ;
#175803 = CARTESIAN_POINT ( 'NONE',  ( -23.25000000000000000, 1.115600667400684642E-11, -134.0000000000000284 ) ) ;
#175805 = ORIENTED_EDGE ( 'NONE', *, *, #106766, .F. ) ;
#175806 = EDGE_CURVE ( 'NONE', #226856, #236861, #1885, .T. ) ;
#175807 = CARTESIAN_POINT ( 'NONE',  ( -16.94445028196807002, 66.00793639031451221, -149.1304376629428816 ) ) ;
#175808 = FACE_OUTER_BOUND ( 'NONE', #187509, .T. ) ;
#175809 = DIRECTION ( 'NONE',  ( -0.000000000000000000, 0.6132151058540549204, -0.7899159663865520375 ) ) ;
#175810 = DIRECTION ( 'NONE',  ( -1.000000000000000000, -1.541880601228652843E-16, -2.878400969107353907E-16 ) ) ;
#175811 = CARTESIAN_POINT ( 'NONE',  ( 20.94999999999999929, 54.23099463892082639, -236.2002849323373539 ) ) ;
#175812 = LINE ( 'NONE', #255271, #143620 ) ;
#175814 = EDGE_CURVE ( 'NONE', #209877, #196735, #161971, .T. ) ;
#175813 = DIRECTION ( 'NONE',  ( -1.000000000000000000, 0.000000000000000000, -0.000000000000000000 ) ) ;
#175815 = AXIS2_PLACEMENT_3D ( 'NONE', #20922, #17063, #234808 ) ;
#175816 = AXIS2_PLACEMENT_3D ( 'NONE', #170005, #249510, #70891 ) ;
#175817 = EDGE_CURVE ( 'NONE', #42405, #21500, #198819, .T. ) ;
#175819 = CIRCLE ( 'NONE', #96654, 0.1999999999999966804 ) ;
#175818 = CARTESIAN_POINT ( 'NONE',  ( 18.59999999999999787, 1.115600667400684642E-11, -100.5000000000000284 ) ) ;
#175820 = ORIENTED_EDGE ( 'NONE', *, *, #131739, .F. ) ;
#175821 = EDGE_LOOP ( 'NONE', ( #240441, #130328, #90812, #166931 ) ) ;
#175822 = DIRECTION ( 'NONE',  ( -0.000000000000000000, 1.000000000000000000, -0.000000000000000000 ) ) ;
#175823 = ORIENTED_EDGE ( 'NONE', *, *, #206393, .F. ) ;
#175824 = CARTESIAN_POINT ( 'NONE',  ( -23.49999999999994316, 74.63923853664559260, -43.99645795275012006 ) ) ;
#175825 = ORIENTED_EDGE ( 'NONE', *, *, #50527, .T. ) ;
#175826 = DIRECTION ( 'NONE',  ( 0.000000000000000000, -4.019398425746649671E-14, 1.000000000000000000 ) ) ;
#175827 = EDGE_CURVE ( 'NONE', #127487, #22210, #145255, .T. ) ;
#175828 = CARTESIAN_POINT ( 'NONE',  ( 23.14999999999999858, 4.000000000011155521, -100.5000000000000426 ) ) ;
#175829 = CARTESIAN_POINT ( 'NONE',  ( -20.54999999999999716, 76.00000000001179501, -82.39810748452430289 ) ) ;
#175831 = VERTEX_POINT ( 'NONE', #104820 ) ;
#175830 = CARTESIAN_POINT ( 'NONE',  ( -22.39999999999999858, 0.1000000000111554016, -59.20922040162664501 ) ) ;
#175832 = EDGE_CURVE ( 'NONE', #243059, #125420, #58147, .T. ) ;
#175833 = LINE ( 'NONE', #235776, #24999 ) ;
#175834 = ORIENTED_EDGE ( 'NONE', *, *, #27402, .T. ) ;
#175835 = EDGE_CURVE ( 'NONE', #217887, #174781, #162249, .T. ) ;
#175836 = FACE_OUTER_BOUND ( 'NONE', #212789, .T. ) ;
#175837 = AXIS2_PLACEMENT_3D ( 'NONE', #86244, #182836, #245361 ) ;
#175838 = CYLINDRICAL_SURFACE ( 'NONE', #238033, 0.09999999999999976963 ) ;
#175839 = DIRECTION ( 'NONE',  ( -0.000000000000000000, -0.000000000000000000, 1.000000000000000000 ) ) ;
#175840 = CARTESIAN_POINT ( 'NONE',  ( -20.90000000000000213, -1.410778198689825347, -7.973296578895943121 ) ) ;
#175841 = EDGE_CURVE ( 'NONE', #92780, #124945, #258048, .T. ) ;
#175842 = CARTESIAN_POINT ( 'NONE',  ( -21.14999999999999858, 11.75000000000000000, -3.469446951953614189E-15 ) ) ;
#175843 = ORIENTED_EDGE ( 'NONE', *, *, #59822, .F. ) ;
#175844 = CARTESIAN_POINT ( 'NONE',  ( -18.46154800491001069, 85.48020627425343321, -29.36565664614284898 ) ) ;
#175845 = ORIENTED_EDGE ( 'NONE', *, *, #42362, .F. ) ;
#175848 = ORIENTED_EDGE ( 'NONE', *, *, #138721, .F. ) ;
#175847 = CARTESIAN_POINT ( 'NONE',  ( -21.05000000000000071, 77.26178616857662007, -61.43660852097883662 ) ) ;
#175846 = CARTESIAN_POINT ( 'NONE',  ( -20.65000000000000568, 68.75000000001233502, -160.7731074845244166 ) ) ;
#175849 = CIRCLE ( 'NONE', #188865, 2.100000000000004530 ) ;
#175850 = CARTESIAN_POINT ( 'NONE',  ( -22.42357213249529480, 0.09908696401271366305, -159.8270676136400539 ) ) ;
#175851 = CARTESIAN_POINT ( 'NONE',  ( -22.59999999999999787, 64.25043287652226809, -69.62396585362311896 ) ) ;
#175852 = EDGE_LOOP ( 'NONE', ( #241835, #101072, #232591, #71627 ) ) ;
#175853 = FACE_OUTER_BOUND ( 'NONE', #47919, .T. ) ;
#175854 = EDGE_CURVE ( 'NONE', #116279, #109234, #120746, .T. ) ;
#175855 = CARTESIAN_POINT ( 'NONE',  ( -23.15000000000000213, 2.000000000011154189, -120.7753780772379315 ) ) ;
#175856 = DIRECTION ( 'NONE',  ( 1.000000000000000000, 0.000000000000000000, 0.000000000000000000 ) ) ;
#175858 = ORIENTED_EDGE ( 'NONE', *, *, #180196, .T. ) ;
#175857 = DIRECTION ( 'NONE',  ( 0.000000000000000000, -1.000000000000000000, -6.982962677686265922E-15 ) ) ;
#175859 = VECTOR ( 'NONE', #132713, 1000.000000000000000 ) ;
#175860 = DIRECTION ( 'NONE',  ( 0.000000000000000000, 0.9893560106964510714, -0.1455152366551481502 ) ) ;
#175861 = CIRCLE ( 'NONE', #96695, 0.1000000000000028644 ) ;
#175862 = VERTEX_POINT ( 'NONE', #206532 ) ;
#175863 = TOROIDAL_SURFACE ( 'NONE', #17602, 0.6000000000000004219, 0.1000000000000000056 ) ;
#175864 = AXIS2_PLACEMENT_3D ( 'NONE', #162118, #215949, #85089 ) ;
#175865 = DIRECTION ( 'NONE',  ( -1.000000000000000000, 0.000000000000000000, 0.000000000000000000 ) ) ;
#175866 = CARTESIAN_POINT ( 'NONE',  ( 20.94999999999999574, 18.74932170447730329, -227.9057176861678613 ) ) ;
#175867 = CARTESIAN_POINT ( 'NONE',  ( 20.85000000000000142, -1.749999999988843813, -212.6189500386222164 ) ) ;
#175868 = ORIENTED_EDGE ( 'NONE', *, *, #161876, .F. ) ;
#175869 = LINE ( 'NONE', #255326, #254995 ) ;
#175871 = EDGE_LOOP ( 'NONE', ( #180209, #87101, #44060, #179664 ) ) ;
#175870 = CIRCLE ( 'NONE', #46640, 11.74999999999999822 ) ;
#175872 = LINE ( 'NONE', #152464, #147843 ) ;
#175873 = CARTESIAN_POINT ( 'NONE',  ( -20.94999999999999929, 77.84915357198811137, -124.9171408647273012 ) ) ;
#175874 = EDGE_LOOP ( 'NONE', ( #141743, #45478, #13986, #99756 ) ) ;
#175875 = CARTESIAN_POINT ( 'NONE',  ( 21.05193202509564543, 22.92263105335900164, -230.0273867217252075 ) ) ;
#175876 = B_SPLINE_CURVE_WITH_KNOTS ( 'NONE', 3,
 ( #175807, #255265, #100068, #214909, #178379, #958, #197905, #77953, #76674, #21853, #257833, #216180, #199207 ),
 .UNSPECIFIED., .F., .F.,
 ( 4, 3, 3, 3, 4 ),
 ( -3.224855718275878119E-06, -4.235164736271501695E-22, 6.199515528669195097E-06, 4.034952380127538728E-05, 7.452715123699865944E-05 ),
 .UNSPECIFIED. ) ;
#175877 = AXIS2_PLACEMENT_3D ( 'NONE', #122097, #162522, #2123 ) ;
#175878 = DIRECTION ( 'NONE',  ( -3.265361837132813093E-16, -1.000000000000000000, -6.982962677686266711E-15 ) ) ;
#175879 = AXIS2_PLACEMENT_3D ( 'NONE', #74696, #233739, #134599 ) ;
#175880 = ORIENTED_EDGE ( 'NONE', *, *, #28187, .F. ) ;
#175881 = CIRCLE ( 'NONE', #84219, 0.09999999999999854838 ) ;
#175882 = AXIS2_PLACEMENT_3D ( 'NONE', #247765, #5271, #30034 ) ;
#175883 = DIRECTION ( 'NONE',  ( 1.000000000000000000, -0.000000000000000000, 0.000000000000000000 ) ) ;
#175884 = DIRECTION ( 'NONE',  ( 1.875376730785737719E-16, -1.000000000000000000, 0.000000000000000000 ) ) ;
#175886 = CARTESIAN_POINT ( 'NONE',  ( 21.14999999999999858, 0.000000000000000000, 11.64957080754479968 ) ) ;
#175885 = AXIS2_PLACEMENT_3D ( 'NONE', #94236, #212913, #168700 ) ;
#175887 = B_SPLINE_CURVE_WITH_KNOTS ( 'NONE', 3,
 ( #152468, #130297, #28691, #231998, #91183, #250254, #208583, #29954 ),
 .UNSPECIFIED., .F., .F.,
 ( 4, 2, 2, 4 ),
 ( 0.000000000000000000, 0.0002114466876441993754, 0.0003171700314663004590, 0.0004228933752884015697 ),
 .UNSPECIFIED. ) ;
#175888 = EDGE_CURVE ( 'NONE', #109188, #201244, #145641, .T. ) ;
#175889 = ORIENTED_EDGE ( 'NONE', *, *, #24163, .T. ) ;
#175891 =( BOUNDED_CURVE ( )  B_SPLINE_CURVE ( 3, ( #13445, #92964, #172564, #252041 ),
 .UNSPECIFIED., .F., .F. ) 
 B_SPLINE_CURVE_WITH_KNOTS ( ( 4, 4 ),
 ( 3.432212674861196522, 3.693332928900581624 ),
 .UNSPECIFIED. ) 
 CURVE ( )  GEOMETRIC_REPRESENTATION_ITEM ( )  RATIONAL_B_SPLINE_CURVE ( ( 1.000000000000000000, 0.9943260843901261525, 0.9943260843901261525, 1.000000000000000000 ) ) 
 REPRESENTATION_ITEM ( '' )  );
#175890 = VECTOR ( 'NONE', #249790, 1000.000000000000000 ) ;
#175892 = CARTESIAN_POINT ( 'NONE',  ( 23.24999999999999645, 1.115600667400684642E-11, -134.0000000000000000 ) ) ;
#175893 = ORIENTED_EDGE ( 'NONE', *, *, #129478, .F. ) ;
#175895 = ORIENTED_EDGE ( 'NONE', *, *, #230443, .F. ) ;
#175894 = CARTESIAN_POINT ( 'NONE',  ( -21.37071067811865532, 12.40787673083931431, -220.0458254187771558 ) ) ;
#175897 = EDGE_CURVE ( 'NONE', #195865, #110389, #43610, .T. ) ;
#175896 = CIRCLE ( 'NONE', #213272, 0.1000000000000028644 ) ;
#175900 = EDGE_LOOP ( 'NONE', ( #201628, #25172, #20190, #37, #144519 ) ) ;
#175899 = VERTEX_POINT ( 'NONE', #123149 ) ;
#175898 = CARTESIAN_POINT ( 'NONE',  ( 21.87500000000000355, 66.25000000001151079, -48.37310748452438958 ) ) ;
#175901 = EDGE_CURVE ( 'NONE', #131047, #192117, #167431, .T. ) ;
#175902 = LINE ( 'NONE', #70713, #74621 ) ;
#175903 = ADVANCED_FACE ( 'NONE', ( #163554 ), #148390, .F. ) ;
#175904 = CARTESIAN_POINT ( 'NONE',  ( -20.85882249326303040, 65.66751761918619934, -30.42826094061123854 ) ) ;
#175905 = DIRECTION ( 'NONE',  ( 0.000000000000000000, 0.000000000000000000, -1.000000000000000000 ) ) ;
#175906 = DIRECTION ( 'NONE',  ( 0.000000000000000000, 0.000000000000000000, 1.000000000000000000 ) ) ;
#175907 = CARTESIAN_POINT ( 'NONE',  ( 23.15000000000000213, -3.770473190032740174, -225.9805569534692324 ) ) ;
#175908 = AXIS2_PLACEMENT_3D ( 'NONE', #211982, #93295, #172889 ) ;
#175909 = CARTESIAN_POINT ( 'NONE',  ( -20.94999999999999929, 1.115600667400684642E-11, -134.0000000000000284 ) ) ;
#175910 = CIRCLE ( 'NONE', #121913, 11.70000000000000284 ) ;
#175911 = CARTESIAN_POINT ( 'NONE',  ( -18.59999999999999787, 64.35000000001254250, -182.1731074845244507 ) ) ;
#175913 = CARTESIAN_POINT ( 'NONE',  ( -21.05000000000000071, 17.11694853917243364, -224.3781540347815451 ) ) ;
#175912 = TOROIDAL_SURFACE ( 'NONE', #205087, 4.099999999999999645, 0.1000000000000000056 ) ;
#175914 = VERTEX_POINT ( 'NONE', #46164 ) ;
#175915 = ORIENTED_EDGE ( 'NONE', *, *, #63221, .T. ) ;
#175916 = ORIENTED_EDGE ( 'NONE', *, *, #115887, .T. ) ;
#175917 = CARTESIAN_POINT ( 'NONE',  ( -5.900000000000003020, -11.34999999999999964, 10.10000000000000142 ) ) ;
#175919 = EDGE_LOOP ( 'NONE', ( #205215, #90763, #243576, #222266 ) ) ;
#175918 = CARTESIAN_POINT ( 'NONE',  ( -23.15000000000000213, -11.64999999998884483, -134.0000000000000000 ) ) ;
#175920 = LINE ( 'NONE', #220161, #21717 ) ;
#175921 = EDGE_LOOP ( 'NONE', ( #167767, #32632, #255709, #229220 ) ) ;
#175922 = EDGE_CURVE ( 'NONE', #154503, #202001, #49796, .T. ) ;
#175923 = FACE_OUTER_BOUND ( 'NONE', #58891, .T. ) ;
#175924 = ORIENTED_EDGE ( 'NONE', *, *, #210309, .F. ) ;
#175925 = DIRECTION ( 'NONE',  ( 1.000000000000000000, 0.000000000000000000, 0.000000000000000000 ) ) ;
#175926 = EDGE_CURVE ( 'NONE', #211251, #4726, #20792, .T. ) ;
#175928 = ORIENTED_EDGE ( 'NONE', *, *, #106158, .T. ) ;
#175927 = PRODUCT_RELATED_PRODUCT_CATEGORY ( 'part', '', ( #26382 ) ) ;
#175929 = DIRECTION ( 'NONE',  ( 0.000000000000000000, -1.000000000000000000, 0.000000000000000000 ) ) ;
#175930 = DIRECTION ( 'NONE',  ( 0.000000000000000000, 0.000000000000000000, -1.000000000000000000 ) ) ;
#175931 = AXIS2_PLACEMENT_3D ( 'NONE', #250367, #93853, #133003 ) ;
#175933 = ORIENTED_EDGE ( 'NONE', *, *, #189869, .F. ) ;
#175932 = ORIENTED_EDGE ( 'NONE', *, *, #138832, .T. ) ;
#175934 = ORIENTED_EDGE ( 'NONE', *, *, #231964, .F. ) ;
#175935 = DIRECTION ( 'NONE',  ( 1.000000000000000000, 0.000000000000000000, 0.000000000000000000 ) ) ;
#175936 = ORIENTED_EDGE ( 'NONE', *, *, #36400, .T. ) ;
#175937 = VERTEX_POINT ( 'NONE', #65734 ) ;
#175938 = EDGE_CURVE ( 'NONE', #68317, #48752, #224791, .T. ) ;
#175939 = DIRECTION ( 'NONE',  ( 0.000000000000000000, 0.000000000000000000, 1.000000000000000000 ) ) ;
#175941 = ORIENTED_EDGE ( 'NONE', *, *, #235077, .F. ) ;
#175940 = LINE ( 'NONE', #36430, #126902 ) ;
#175942 = EDGE_CURVE ( 'NONE', #140330, #141837, #166536, .T. ) ;
#175943 = EDGE_CURVE ( 'NONE', #26422, #102935, #34500, .T. ) ;
#175945 = CARTESIAN_POINT ( 'NONE',  ( 20.95052659398289308, 65.52017563223242291, -162.4478687286588183 ) ) ;
#175944 = CARTESIAN_POINT ( 'NONE',  ( 23.14999999999999858, 76.00000000001165290, -69.52310748452431710 ) ) ;
#175946 = DIRECTION ( 'NONE',  ( 0.000000000000000000, -7.086529944415893080E-15, 1.000000000000000000 ) ) ;
#175947 = DIRECTION ( 'NONE',  ( 0.000000000000000000, 1.000000000000000000, 0.000000000000000000 ) ) ;
#175948 = CARTESIAN_POINT ( 'NONE',  ( -33.72168855820452649, 64.52683809664901560, -45.27310748452439526 ) ) ;
#175949 = EDGE_LOOP ( 'NONE', ( #32984, #49725, #87898, #33191 ) ) ;
#175950 = ORIENTED_EDGE ( 'NONE', *, *, #52621, .F. ) ;
#175951 = CARTESIAN_POINT ( 'NONE',  ( 18.33683296300528198, 85.51114997114476068, -96.11740007181523993 ) ) ;
#175952 = DIRECTION ( 'NONE',  ( 0.000000000000000000, 0.2002428086779743377, -0.9797463026583749235 ) ) ;
#175953 = DIRECTION ( 'NONE',  ( 0.000000000000000000, -0.8660254037844387076, 0.4999999999999998335 ) ) ;
#175954 = ADVANCED_FACE ( 'NONE', ( #211689 ), #108075, .T. ) ;
#175955 = EDGE_LOOP ( 'NONE', ( #58458, #124301, #225865, #168562 ) ) ;
#175956 = CARTESIAN_POINT ( 'NONE',  ( 18.39999999999999503, 70.35000000001187459, -90.37310748452433984 ) ) ;
#175957 = AXIS2_PLACEMENT_3D ( 'NONE', #232827, #114128, #193685 ) ;
#175958 = DIRECTION ( 'NONE',  ( -0.000000000000000000, 1.000000000000000000, -1.224646799147352961E-16 ) ) ;
#175959 = CARTESIAN_POINT ( 'NONE',  ( 13.40000000000000036, -11.65000000000000036, 12.40000000000000391 ) ) ;
#175960 = EDGE_LOOP ( 'NONE', ( #64368, #150254, #223419, #208613 ) ) ;
#175961 = ORIENTED_EDGE ( 'NONE', *, *, #193351, .F. ) ;
#175962 = CARTESIAN_POINT ( 'NONE',  ( -23.15000000000000213, 11.65000000001115588, -155.3500000000000227 ) ) ;
#175963 = CARTESIAN_POINT ( 'NONE',  ( -20.64999999999999858, 4.350000000011156054, -155.1500000000000057 ) ) ;
#175964 = ORIENTED_EDGE ( 'NONE', *, *, #103832, .F. ) ;
#175965 = DIRECTION ( 'NONE',  ( 1.000000000000000000, -2.952720810173289112E-16, -2.061873921506763405E-30 ) ) ;
#175966 = ORIENTED_EDGE ( 'NONE', *, *, #103332, .T. ) ;
#175967 = FACE_OUTER_BOUND ( 'NONE', #235132, .T. ) ;
#175968 = LINE ( 'NONE', #213783, #187187 ) ;
#175970 = CARTESIAN_POINT ( 'NONE',  ( -23.25000000000000355, 5.650000000011139001, -87.85000000000003695 ) ) ;
#175969 = LINE ( 'NONE', #255423, #207227 ) ;
#175971 = CARTESIAN_POINT ( 'NONE',  ( -23.25000000000000000, -1.835859311443637010, -45.00443916879852679 ) ) ;
#175972 = ADVANCED_FACE ( 'NONE', ( #193409 ), #91721, .T. ) ;
#175973 = CYLINDRICAL_SURFACE ( 'NONE', #203650, 0.1000000000000028644 ) ;
#175974 = VECTOR ( 'NONE', #169326, 1000.000000000000000 ) ;
#175975 = CARTESIAN_POINT ( 'NONE',  ( 24.30000000000000071, -12.79999999999999716, -347.0000000000001137 ) ) ;
#175976 = TOROIDAL_SURFACE ( 'NONE', #63499, 0.2000000000000000111, 0.1000000000000000056 ) ;
#175978 = ORIENTED_EDGE ( 'NONE', *, *, #113230, .T. ) ;
#175977 = EDGE_LOOP ( 'NONE', ( #113509, #37145, #187526, #252868 ) ) ;
#175979 = VERTEX_POINT ( 'NONE', #150432 ) ;
#175980 = EDGE_CURVE ( 'NONE', #2240, #65925, #130842, .T. ) ;
#175981 = DIRECTION ( 'NONE',  ( -1.000000000000000000, 0.000000000000000000, 0.000000000000000000 ) ) ;
#175982 = CARTESIAN_POINT ( 'NONE',  ( -16.77828822508139694, 60.94630241056517406, -221.0305267419277868 ) ) ;
#175983 = DIRECTION ( 'NONE',  ( 1.000000000000000000, 0.000000000000000000, 0.000000000000000000 ) ) ;
#175984 = DIRECTION ( 'NONE',  ( -1.000000000000000000, 7.304098846218134667E-16, -4.217023435051678980E-16 ) ) ;
#175986 = CARTESIAN_POINT ( 'NONE',  ( -14.77738660682463312, 66.56344716000744199, -87.84515201176407118 ) ) ;
#175985 = PLANE ( 'NONE',  #224482 ) ;
#175987 = CARTESIAN_POINT ( 'NONE',  ( -16.85939681242906119, 66.09477481408619326, -48.98318552933291414 ) ) ;
#175988 = ORIENTED_EDGE ( 'NONE', *, *, #14079, .F. ) ;
#175989 = ADVANCED_FACE ( 'NONE', ( #30481 ), #195580, .F. ) ;
#175990 = DIRECTION ( 'NONE',  ( 0.000000000000000000, -0.000000000000000000, -1.000000000000000000 ) ) ;
#175991 = ORIENTED_EDGE ( 'NONE', *, *, #174992, .F. ) ;
#175992 = ORIENTED_EDGE ( 'NONE', *, *, #94177, .F. ) ;
#175993 = CARTESIAN_POINT ( 'NONE',  ( 23.14999999999998437, -4.049999999999998934, 0.000000000000000000 ) ) ;
#175995 = TOROIDAL_SURFACE ( 'NONE', #117696, 3.899999999999999467, 0.1000000000000000056 ) ;
#175994 = DIRECTION ( 'NONE',  ( 0.000000000000000000, 0.000000000000000000, -1.000000000000000000 ) ) ;
#175996 = CYLINDRICAL_SURFACE ( 'NONE', #50230, 0.09999999999998898659 ) ;
#175997 = CIRCLE ( 'NONE', #192533, 11.80000000000000426 ) ;
#175998 = CARTESIAN_POINT ( 'NONE',  ( 23.25000000000000000, 87.65000000001221281, -148.2731074845242176 ) ) ;
#175999 = EDGE_CURVE ( 'NONE', #146731, #18113, #132133, .T. ) ;
#176000 = CARTESIAN_POINT ( 'NONE',  ( 22.59999999999999432, 0.1008583691098678403, -155.7504328765105868 ) ) ;
#176001 = EDGE_CURVE ( 'NONE', #136430, #41111, #70903, .T. ) ;
#176002 = VERTEX_POINT ( 'NONE', #14783 ) ;
#176003 = VERTEX_POINT ( 'NONE', #250787 ) ;
#176004 = DIRECTION ( 'NONE',  ( 0.000000000000000000, 1.000000000000000000, 0.000000000000000000 ) ) ;
#176005 = CIRCLE ( 'NONE', #105186, 0.6000000000000033085 ) ;
#176006 = CARTESIAN_POINT ( 'NONE',  ( 18.59999999999999076, -1.835859311432481045, -179.1044391687985353 ) ) ;
#176007 = DIRECTION ( 'NONE',  ( 0.000000000000000000, 0.2617529984164955192, 0.9651348961777178603 ) ) ;
#176008 = CARTESIAN_POINT ( 'NONE',  ( 21.10000000000000142, 0.000000000000000000, -4.100000000000000533 ) ) ;
#176009 = FACE_OUTER_BOUND ( 'NONE', #58205, .T. ) ;
#176010 = CARTESIAN_POINT ( 'NONE',  ( -20.64999999999999858, 73.60000000001151932, -49.24772940728643533 ) ) ;
#176011 = FACE_OUTER_BOUND ( 'NONE', #233159, .T. ) ;
#176012 = CIRCLE ( 'NONE', #146911, 0.09999999999999939493 ) ;
#176015 = CARTESIAN_POINT ( 'NONE',  ( -21.05000000000000071, 76.10000000001276987, -215.1731074845243654 ) ) ;
#176014 = VECTOR ( 'NONE', #132521, 1000.000000000000000 ) ;
#176013 = CARTESIAN_POINT ( 'NONE',  ( -22.42253884134832020, 0.001932351135308873818, 11.64960569734842366 ) ) ;
#176017 = DIRECTION ( 'NONE',  ( -1.000000000000000000, 0.000000000000000000, 0.000000000000000000 ) ) ;
#176016 = VECTOR ( 'NONE', #138197, 1000.000000000000000 ) ;
#176018 = AXIS2_PLACEMENT_3D ( 'NONE', #89637, #169227, #190041 ) ;
#176019 = DIRECTION ( 'NONE',  ( 1.000000000000000000, 0.000000000000000000, 0.000000000000000000 ) ) ;
#176020 = CARTESIAN_POINT ( 'NONE',  ( 23.14999999999998437, 7.128833340093095217, -233.7327013124392749 ) ) ;
#176021 = CARTESIAN_POINT ( 'NONE',  ( 21.07928932188134397, 69.67148334361938566, -203.6220026301787982 ) ) ;
#176023 = VERTEX_POINT ( 'NONE', #72174 ) ;
#176022 = CARTESIAN_POINT ( 'NONE',  ( -20.54999999999999716, 70.12557831835937350, -215.6322690948981915 ) ) ;
#176024 = EDGE_CURVE ( 'NONE', #111063, #17499, #220505, .T. ) ;
#176025 = EDGE_CURVE ( 'NONE', #161437, #40449, #228869, .T. ) ;
#176026 = CARTESIAN_POINT ( 'NONE',  ( 20.85000000000000142, 1.115600667400684642E-11, -67.00000000000000000 ) ) ;
#176027 = VERTEX_POINT ( 'NONE', #94279 ) ;
#176028 = CARTESIAN_POINT ( 'NONE',  ( -18.35235881385853318, 11.47341900772405054, -109.7500000000000426 ) ) ;
#176029 = LINE ( 'NONE', #215130, #64568 ) ;
#176030 = ADVANCED_FACE ( 'NONE', ( #233811 ), #134675, .F. ) ;
#176031 = ORIENTED_EDGE ( 'NONE', *, *, #117071, .F. ) ;
#176032 = DIRECTION ( 'NONE',  ( 0.000000000000000000, 0.8068669527897009974, 0.5907332058517299478 ) ) ;
#176034 = EDGE_CURVE ( 'NONE', #82856, #147015, #52582, .T. ) ;
#176033 = CARTESIAN_POINT ( 'NONE',  ( -23.15000000000000213, 64.35000000001198828, -115.2731074845243739 ) ) ;
#176036 = CIRCLE ( 'NONE', #209308, 0.9750000000000036415 ) ;
#176035 = DIRECTION ( 'NONE',  ( 0.000000000000000000, 0.9651348961777157509, -0.2617529984165031243 ) ) ;
#176037 = AXIS2_PLACEMENT_3D ( 'NONE', #130373, #110813, #11746 ) ;
#176038 = DIRECTION ( 'NONE',  ( 0.000000000000000000, 0.9998779222360102414, 0.01562499999996356907 ) ) ;
#176039 = CARTESIAN_POINT ( 'NONE',  ( 18.52928932304149967, 10.27928932304150678, -24.67625343280360894 ) ) ;
#176040 = DIRECTION ( 'NONE',  ( -1.000000000000000000, 0.000000000000000000, 0.000000000000000000 ) ) ;
#176041 = VERTEX_POINT ( 'NONE', #231254 ) ;
#176042 = CARTESIAN_POINT ( 'NONE',  ( 18.59999999999999076, 15.24158151457507415, -223.0107194535042083 ) ) ;
#176044 = ORIENTED_EDGE ( 'NONE', *, *, #12970, .T. ) ;
#176043 = CARTESIAN_POINT ( 'NONE',  ( -21.05000000000000426, 11.60000000001115872, -40.42820323027555673 ) ) ;
#176045 = CARTESIAN_POINT ( 'NONE',  ( -21.05000000000000071, 16.44800918141279311, -240.8068063186265135 ) ) ;
#176046 = VECTOR ( 'NONE', #130996, 1000.000000000000000 ) ;
#176047 = FACE_OUTER_BOUND ( 'NONE', #179502, .T. ) ;
#176048 = EDGE_CURVE ( 'NONE', #224583, #135153, #248230, .T. ) ;
#176049 = CARTESIAN_POINT ( 'NONE',  ( -20.85000000000000142, 7.021664781900089913, -37.13356540189729316 ) ) ;
#176050 = ORIENTED_EDGE ( 'NONE', *, *, #148917, .T. ) ;
#176051 = CARTESIAN_POINT ( 'NONE',  ( -20.90000000000000213, 1.885425182446133885, -11.49641995933507843 ) ) ;
#176052 = EDGE_CURVE ( 'NONE', #213843, #239412, #133193, .T. ) ;
#176053 = AXIS2_PLACEMENT_3D ( 'NONE', #4714, #145521, #187247 ) ;
#176054 = APPLICATION_PROTOCOL_DEFINITION ( 'draft international standard', 'automotive_design', 1998, #190631 ) ;
#176055 = CARTESIAN_POINT ( 'NONE',  ( 22.48660254037843131, 11.47023279864282941, -198.4507335280135294 ) ) ;
#176057 = AXIS2_PLACEMENT_3D ( 'NONE', #16785, #216229, #15505 ) ;
#176056 = CARTESIAN_POINT ( 'NONE',  ( -18.50000000000000000, 70.22659352830977753, -197.9852579278363578 ) ) ;
#176058 = ORIENTED_EDGE ( 'NONE', *, *, #234538, .T. ) ;
#176059 = AXIS2_PLACEMENT_3D ( 'NONE', #199310, #117198, #237145 ) ;
#176060 = LINE ( 'NONE', #174797, #96138 ) ;
#176061 = FACE_OUTER_BOUND ( 'NONE', #241219, .T. ) ;
#176062 = CIRCLE ( 'NONE', #171780, 0.1000000000000013933 ) ;
#176063 = VECTOR ( 'NONE', #239638, 1000.000000000000000 ) ;
#176064 = CARTESIAN_POINT ( 'NONE',  ( -16.77779411440718604, 9.946101447118758543, -121.3369425829955048 ) ) ;
#176065 = VERTEX_POINT ( 'NONE', #51274 ) ;
#176066 = ORIENTED_EDGE ( 'NONE', *, *, #206427, .F. ) ;
#176067 = LINE ( 'NONE', #117351, #72315 ) ;
#176069 = AXIS2_PLACEMENT_3D ( 'NONE', #206452, #209023, #126921 ) ;
#176068 = CARTESIAN_POINT ( 'NONE',  ( 23.14999999999998437, 11.48087284840413425, -198.4995883060917663 ) ) ;
#176071 = CIRCLE ( 'NONE', #134325, 0.1000000000000028644 ) ;
#176070 = CARTESIAN_POINT ( 'NONE',  ( -20.94999999999999929, 11.70000000001115126, -127.2450018504814295 ) ) ;
#176072 = CYLINDRICAL_SURFACE ( 'NONE', #102824, 0.5000000000000008882 ) ;
#176073 = CARTESIAN_POINT ( 'NONE',  ( -16.93388492042257454, 30.26908302050733823, -234.7969376182378198 ) ) ;
#176075 = CARTESIAN_POINT ( 'NONE',  ( 21.14999999999999503, 30.69873658968802133, -264.9868732779115703 ) ) ;
#176074 = LINE ( 'NONE', #216444, #107753 ) ;
#176076 = AXIS2_PLACEMENT_3D ( 'NONE', #24494, #23215, #242221 ) ;
#176077 = FACE_OUTER_BOUND ( 'NONE', #139070, .T. ) ;
#176078 = CARTESIAN_POINT ( 'NONE',  ( -16.94333152886235894, 9.990342011461637028, -113.1079684689456286 ) ) ;
#176079 = CARTESIAN_POINT ( 'NONE',  ( 18.50016250449482413, 65.70233904877068198, -30.54874109119651848 ) ) ;
#176080 = DIRECTION ( 'NONE',  ( 0.000000000000000000, 0.000000000000000000, 1.000000000000000000 ) ) ;
#176081 = ORIENTED_EDGE ( 'NONE', *, *, #17025, .F. ) ;
#176082 = EDGE_CURVE ( 'NONE', #133593, #81511, #249715, .T. ) ;
#176083 = ORIENTED_EDGE ( 'NONE', *, *, #23373, .T. ) ;
#176084 = PLANE ( 'NONE',  #97816 ) ;
#176085 = CIRCLE ( 'NONE', #67723, 0.09999999999999939493 ) ;
#176086 = CARTESIAN_POINT ( 'NONE',  ( 21.05000000000000071, 76.00000000001237765, -170.0231074845243597 ) ) ;
#176088 = DIRECTION ( 'NONE',  ( 0.000000000000000000, 0.2617529984165035684, 0.9651348961777156399 ) ) ;
#176087 = CARTESIAN_POINT ( 'NONE',  ( 21.11927991906888025, 69.55150688152023974, -69.53219116399826305 ) ) ;
#176089 = AXIS2_PLACEMENT_3D ( 'NONE', #154291, #53859, #176393 ) ;
#176090 = CARTESIAN_POINT ( 'NONE',  ( -23.25000000000000000, 7.958757221477368304, -237.5433740025449083 ) ) ;
#176091 = CARTESIAN_POINT ( 'NONE',  ( 20.94999999999999929, 87.65000000001215597, -139.4231074845242802 ) ) ;
#176092 = ORIENTED_EDGE ( 'NONE', *, *, #59501, .F. ) ;
#176093 = ORIENTED_EDGE ( 'NONE', *, *, #111949, .T. ) ;
#176094 = CARTESIAN_POINT ( 'NONE',  ( 18.59999999999998366, 1.115600667400684642E-11, -200.9999999999999432 ) ) ;
#176095 = ORIENTED_EDGE ( 'NONE', *, *, #29325, .F. ) ;
#176096 = EDGE_CURVE ( 'NONE', #154148, #60110, #153919, .T. ) ;
#176097 = DIRECTION ( 'NONE',  ( 0.000000000000000000, 0.000000000000000000, 1.000000000000000000 ) ) ;
#176098 = VECTOR ( 'NONE', #199589, 1000.000000000000000 ) ;
#176099 = AXIS2_PLACEMENT_3D ( 'NONE', #165197, #204305, #141767 ) ;
#176100 = DIRECTION ( 'NONE',  ( -1.000000000000000000, 0.000000000000000000, -0.000000000000000000 ) ) ;
#176101 = VECTOR ( 'NONE', #24522, 1000.000000000000000 ) ;
#176102 = CARTESIAN_POINT ( 'NONE',  ( -23.25000000000000000, 1.148907358139439339E-11, -201.0000000000015064 ) ) ;
#176103 = ORIENTED_EDGE ( 'NONE', *, *, #219501, .T. ) ;
#176104 = CARTESIAN_POINT ( 'NONE',  ( 21.05000000000000071, 61.95000000001248708, -175.5368025552853624 ) ) ;
#176105 = ORIENTED_EDGE ( 'NONE', *, *, #30021, .T. ) ;
#176106 = DIRECTION ( 'NONE',  ( 0.000000000000000000, 0.2128009952263485993, -0.9770955615653341697 ) ) ;
#176107 = CARTESIAN_POINT ( 'NONE',  ( -18.59999999999999787, 61.57587952878036930, -212.2000740415318774 ) ) ;
#176108 = CARTESIAN_POINT ( 'NONE',  ( 21.14999999999999858, 69.45000000001186891, -90.67310748452435121 ) ) ;
#176109 = DIRECTION ( 'NONE',  ( 0.000000000000000000, 0.000000000000000000, -1.000000000000000000 ) ) ;
#176110 = CARTESIAN_POINT ( 'NONE',  ( -21.05000000000000071, 76.00000000001139711, -32.02310748452432421 ) ) ;
#176112 = CARTESIAN_POINT ( 'NONE',  ( -13.39999999999994529, 64.35000000001120668, -18.42310748452479174 ) ) ;
#176111 = DIRECTION ( 'NONE',  ( 1.000000000000000000, 0.000000000000000000, 0.000000000000000000 ) ) ;
#176113 = DIRECTION ( 'NONE',  ( 0.7071067811865463515, 0.7071067811865487940, 4.937700262164540154E-15 ) ) ;
#176114 = ORIENTED_EDGE ( 'NONE', *, *, #240635, .T. ) ;
#176115 = VECTOR ( 'NONE', #107627, 1000.000000000000000 ) ;
#176117 = DIRECTION ( 'NONE',  ( 1.000000000000000000, 0.000000000000000000, 0.000000000000000000 ) ) ;
#176116 = DIRECTION ( 'NONE',  ( 1.000000000000000000, -2.952720810173289112E-16, -2.061873921506763405E-30 ) ) ;
#176118 = ORIENTED_EDGE ( 'NONE', *, *, #32100, .T. ) ;
#176120 = ORIENTED_EDGE ( 'NONE', *, *, #113570, .F. ) ;
#176119 = CARTESIAN_POINT ( 'NONE',  ( -20.54999999999999716, 7.150000000011155876, -79.35000000000005116 ) ) ;
#176121 = ORIENTED_EDGE ( 'NONE', *, *, #140237, .F. ) ;
#176122 = FACE_OUTER_BOUND ( 'NONE', #27156, .T. ) ;
#176123 = CARTESIAN_POINT ( 'NONE',  ( -22.39999999999999503, 1.115541036281197940E-11, -25.70922040162659883 ) ) ;
#176124 = LINE ( 'NONE', #213942, #214118 ) ;
#176125 = DIRECTION ( 'NONE',  ( 0.000000000000000000, 0.000000000000000000, -1.000000000000000000 ) ) ;
#176126 = AXIS2_PLACEMENT_3D ( 'NONE', #223178, #26284, #245331 ) ;
#176127 = ORIENTED_EDGE ( 'NONE', *, *, #202970, .T. ) ;
#176128 = DIRECTION ( 'NONE',  ( 1.000000000000000000, 0.000000000000000000, 0.000000000000000000 ) ) ;
#176129 = LINE ( 'NONE', #39187, #35036 ) ;
#176130 = DIRECTION ( 'NONE',  ( 1.000000000000000000, 0.000000000000000000, 0.000000000000000000 ) ) ;
#176131 = VERTEX_POINT ( 'NONE', #175159 ) ;
#176132 = DIRECTION ( 'NONE',  ( 0.000000000000000000, -1.000000000000000000, 0.000000000000000000 ) ) ;
#176133 = EDGE_CURVE ( 'NONE', #179596, #168233, #74795, .T. ) ;
#176134 = LINE ( 'NONE', #139533, #35289 ) ;
#176135 = ORIENTED_EDGE ( 'NONE', *, *, #157635, .T. ) ;
#176136 = VERTEX_POINT ( 'NONE', #38184 ) ;
#176137 = CARTESIAN_POINT ( 'NONE',  ( -16.94878442675512886, 9.991729103002160883, -188.3882195756378337 ) ) ;
#176138 = CIRCLE ( 'NONE', #46908, 0.1000000000000032391 ) ;
#176139 = ORIENTED_EDGE ( 'NONE', *, *, #10859, .T. ) ;
#176140 = DIRECTION ( 'NONE',  ( 0.000000000000000000, 0.9998779222360096863, -0.01562500000001061998 ) ) ;
#176141 = EDGE_LOOP ( 'NONE', ( #98710, #234978, #199550, #21388 ) ) ;
#176142 = CARTESIAN_POINT ( 'NONE',  ( -21.05000000000000071, 74.83729825007462466, -195.5231074845243597 ) ) ;
#176143 = EDGE_CURVE ( 'NONE', #214669, #106265, #79187, .T. ) ;
#176144 = DIRECTION ( 'NONE',  ( 0.000000000000000000, 0.2617529984165174461, 0.9651348961777118651 ) ) ;
#176145 = LINE ( 'NONE', #77012, #101622 ) ;
#176146 = ADVANCED_FACE ( 'NONE', ( #236363 ), #120931, .T. ) ;
#176147 = CYLINDRICAL_SURFACE ( 'NONE', #95517, 0.1000000000000002554 ) ;
#176149 = CIRCLE ( 'NONE', #63690, 0.09999999999999939493 ) ;
#176148 = DIRECTION ( 'NONE',  ( 0.000000000000000000, 1.000000000000000000, -1.224646799147353207E-16 ) ) ;
#176150 = EDGE_CURVE ( 'NONE', #104084, #76475, #45891, .T. ) ;
#176151 = CARTESIAN_POINT ( 'NONE',  ( -23.15000000000000213, -4.756823075239757337, -233.1486023682345490 ) ) ;
#176152 = CARTESIAN_POINT ( 'NONE',  ( 20.94999999999999929, 1.115600667400684642E-11, -67.00000000000000000 ) ) ;
#176153 = ORIENTED_EDGE ( 'NONE', *, *, #223110, .F. ) ;
#176155 = CARTESIAN_POINT ( 'NONE',  ( 21.14999999999999858, 45.02833974712562792, -238.5149546970766892 ) ) ;
#176154 = SPHERICAL_SURFACE ( 'NONE', #174773, 0.1000000000000000056 ) ;
#176157 = ORIENTED_EDGE ( 'NONE', *, *, #16280, .T. ) ;
#176156 = AXIS2_PLACEMENT_3D ( 'NONE', #251466, #166841, #147235 ) ;
#176160 = ORIENTED_EDGE ( 'NONE', *, *, #198794, .F. ) ;
#176159 = CARTESIAN_POINT ( 'NONE',  ( -18.44362607810620958, 85.49049615809643399, -62.46515361767715291 ) ) ;
#176158 = CARTESIAN_POINT ( 'NONE',  ( -18.59999999999999787, 68.48451787451661232, -224.2224406095231757 ) ) ;
#176161 = ORIENTED_EDGE ( 'NONE', *, *, #43213, .F. ) ;
#176162 = FACE_OUTER_BOUND ( 'NONE', #98124, .T. ) ;
#176163 = CARTESIAN_POINT ( 'NONE',  ( 12.84233041328156055, 66.58946139148339682, -154.5904194873835706 ) ) ;
#176165 = FACE_OUTER_BOUND ( 'NONE', #162813, .T. ) ;
#176164 = AXIS2_PLACEMENT_3D ( 'NONE', #95476, #172508, #73388 ) ;
#176166 = CARTESIAN_POINT ( 'NONE',  ( -21.05000000000000071, 64.37928932189343811, -129.6546908321833484 ) ) ;
#176167 = ORIENTED_EDGE ( 'NONE', *, *, #190249, .T. ) ;
#176168 = CYLINDRICAL_SURFACE ( 'NONE', #55408, 0.09999999999999939493 ) ;
#176169 = EDGE_CURVE ( 'NONE', #242431, #13670, #212503, .T. ) ;
#176170 = DIRECTION ( 'NONE',  ( -1.000000000000000000, 0.000000000000000000, 0.000000000000000000 ) ) ;
#176172 = CARTESIAN_POINT ( 'NONE',  ( 20.95052659398289308, 10.47982436777990323, -7.575238755865602691 ) ) ;
#176171 = CARTESIAN_POINT ( 'NONE',  ( 21.05000000000000071, 78.47509609352879068, -238.9045489380306435 ) ) ;
#176174 = ORIENTED_EDGE ( 'NONE', *, *, #97391, .F. ) ;
#176173 = CARTESIAN_POINT ( 'NONE',  ( -21.05000000000000071, 0.000000000000000000, -4.299999999999956302 ) ) ;
#176175 = CIRCLE ( 'NONE', #209450, 0.1000000000000118433 ) ;
#176176 = AXIS2_PLACEMENT_3D ( 'NONE', #256279, #217205, #257572 ) ;
#176177 = ORIENTED_EDGE ( 'NONE', *, *, #136041, .F. ) ;
#176178 = DIRECTION ( 'NONE',  ( 1.000000000000000000, -3.265361837132813093E-16, -2.280189983783949500E-30 ) ) ;
#176179 = EDGE_LOOP ( 'NONE', ( #171054, #152344, #64233 ) ) ;
#176180 = DIRECTION ( 'NONE',  ( 1.000000000000000000, 2.952720810173289112E-16, -0.000000000000000000 ) ) ;
#176181 = ORIENTED_EDGE ( 'NONE', *, *, #148023, .F. ) ;
#176183 = AXIS2_PLACEMENT_3D ( 'NONE', #38689, #178220, #120813 ) ;
#176182 = DIRECTION ( 'NONE',  ( -0.000000000000000000, 0.000000000000000000, -1.000000000000000000 ) ) ;
#176184 = DIRECTION ( 'NONE',  ( 0.000000000000000000, 0.2617529984164915779, 0.9651348961777189706 ) ) ;
#176185 = CARTESIAN_POINT ( 'NONE',  ( 11.60000000000000320, -8.250000000000003553, 12.40000000000000391 ) ) ;
#176186 = EDGE_LOOP ( 'NONE', ( #29316, #186077, #34219, #26101 ) ) ;
#176187 = CARTESIAN_POINT ( 'NONE',  ( -21.05000000000000071, 30.73075574124490572, -252.3164853687435709 ) ) ;
#176188 = CIRCLE ( 'NONE', #109513, 0.1000000000000013933 ) ;
#176189 = AXIS2_PLACEMENT_3D ( 'NONE', #113613, #51032, #211431 ) ;
#176190 = CIRCLE ( 'NONE', #63739, 0.6000000000000033085 ) ;
#176191 = CIRCLE ( 'NONE', #59607, 0.5000000000000004441 ) ;
#176192 = CARTESIAN_POINT ( 'NONE',  ( -16.87372397896795562, 9.880599536652892922, -53.85072451003576077 ) ) ;
#176193 = EDGE_CURVE ( 'NONE', #21030, #134482, #204089, .T. ) ;
#176194 = VERTEX_POINT ( 'NONE', #310 ) ;
#176195 = EDGE_LOOP ( 'NONE', ( #163518, #13974 ) ) ;
#176196 = CARTESIAN_POINT ( 'NONE',  ( 20.12481660106788084, 18.87840997762110007, -229.2195997782433210 ) ) ;
#176197 = ORIENTED_EDGE ( 'NONE', *, *, #214449, .T. ) ;
#176198 = ORIENTED_EDGE ( 'NONE', *, *, #155678, .T. ) ;
#176200 = ORIENTED_EDGE ( 'NONE', *, *, #199562, .F. ) ;
#176199 = DIRECTION ( 'NONE',  ( -0.000000000000000000, 0.7106264324241465813, -0.7035695228903323661 ) ) ;
#176201 = EDGE_CURVE ( 'NONE', #46813, #172429, #85, .T. ) ;
#176202 = ORIENTED_EDGE ( 'NONE', *, *, #247643, .F. ) ;
#176203 = FACE_OUTER_BOUND ( 'NONE', #20246, .T. ) ;
#176205 = ORIENTED_EDGE ( 'NONE', *, *, #169195, .T. ) ;
#176204 = EDGE_LOOP ( 'NONE', ( #12348, #185315, #254496 ) ) ;
#176206 = CIRCLE ( 'NONE', #72737, 11.79999999999999716 ) ;
#176207 = EDGE_CURVE ( 'NONE', #78012, #89054, #145837, .T. ) ;
#176208 = CIRCLE ( 'NONE', #76210, 0.1000000000000001860 ) ;
#176209 = EDGE_LOOP ( 'NONE', ( #6572, #46182, #181092, #104588 ) ) ;
#176210 = DIRECTION ( 'NONE',  ( 1.000000000000000000, 3.265361837132813093E-16, -0.000000000000000000 ) ) ;
#176211 = DIRECTION ( 'NONE',  ( -0.000000000000000000, -0.1350103645451945777, 0.9908441862701590219 ) ) ;
#176212 = DIRECTION ( 'NONE',  ( -0.000000000000000000, 0.4721928772777343464, 0.8814952561688431665 ) ) ;
#176213 = ORIENTED_EDGE ( 'NONE', *, *, #113774, .T. ) ;
#176214 = AXIS2_PLACEMENT_3D ( 'NONE', #164962, #84083, #8467 ) ;
#176215 = CYLINDRICAL_SURFACE ( 'NONE', #16459, 0.09999999999999939493 ) ;
#176216 = AXIS2_PLACEMENT_3D ( 'NONE', #6887, #86394, #143818 ) ;
#176217 = EDGE_CURVE ( 'NONE', #18296, #133755, #100019, .T. ) ;
#176219 = ORIENTED_EDGE ( 'NONE', *, *, #140638, .F. ) ;
#176218 = FACE_OUTER_BOUND ( 'NONE', #81350, .T. ) ;
#176220 = DIRECTION ( 'NONE',  ( 0.000000000000000000, 0.000000000000000000, -1.000000000000000000 ) ) ;
#176222 = ORIENTED_EDGE ( 'NONE', *, *, #145605, .T. ) ;
#176221 = SPHERICAL_SURFACE ( 'NONE', #239570, 0.1000000000000000056 ) ;
#176223 = ORIENTED_EDGE ( 'NONE', *, *, #25046, .F. ) ;
#176224 = VECTOR ( 'NONE', #196207, 1000.000000000000000 ) ;
#176225 = ADVANCED_FACE ( 'NONE', ( #16067 ), #177711, .F. ) ;
#176226 = CARTESIAN_POINT ( 'NONE',  ( 22.47071067811864964, 0.09909245471376178227, -159.7799252555019223 ) ) ;
#176227 = CARTESIAN_POINT ( 'NONE',  ( -18.79999999999999716, 1.350000000000000089, 16.60000000000000142 ) ) ;
#176228 = AXIS2_PLACEMENT_3D ( 'NONE', #110099, #28033, #184491 ) ;
#176229 = CIRCLE ( 'NONE', #213610, 0.9750000000000036415 ) ;
#176231 = ORIENTED_EDGE ( 'NONE', *, *, #116503, .F. ) ;
#176230 = VECTOR ( 'NONE', #116907, 1000.000000000000000 ) ;
#176232 = VERTEX_POINT ( 'NONE', #257154 ) ;
#176233 = DIRECTION ( 'NONE',  ( 0.000000000000000000, 0.000000000000000000, -1.000000000000000000 ) ) ;
#176234 = FACE_OUTER_BOUND ( 'NONE', #78843, .T. ) ;
#176235 = CIRCLE ( 'NONE', #242847, 0.09999999999999939493 ) ;
#176236 = ADVANCED_FACE ( 'NONE', ( #78565 ), #158159, .F. ) ;
#176238 = EDGE_LOOP ( 'NONE', ( #54550, #62975, #83988, #247580, #191839 ) ) ;
#176237 = EDGE_LOOP ( 'NONE', ( #162176, #95325, #110772 ) ) ;
#176239 = ORIENTED_EDGE ( 'NONE', *, *, #241570, .T. ) ;
#176240 = VERTEX_POINT ( 'NONE', #95565 ) ;
#176241 = ORIENTED_EDGE ( 'NONE', *, *, #244313, .T. ) ;
#176242 = DIRECTION ( 'NONE',  ( 0.000000000000000000, 0.000000000000000000, -1.000000000000000000 ) ) ;
#176243 = VERTEX_POINT ( 'NONE', #176919 ) ;
#176244 = ADVANCED_FACE ( 'NONE', ( #21676 ), #12591, .F. ) ;
#176245 = CARTESIAN_POINT ( 'NONE',  ( -16.93440969289731157, 12.44567823802137241, -211.1758536839202804 ) ) ;
#176246 = EDGE_CURVE ( 'NONE', #54036, #34960, #137447, .T. ) ;
#176247 = CIRCLE ( 'NONE', #93017, 0.1000000000000002692 ) ;
#176249 = LINE ( 'NONE', #60109, #60835 ) ;
#176248 = LINE ( 'NONE', #198349, #73944 ) ;
#176251 = ORIENTED_EDGE ( 'NONE', *, *, #217371, .F. ) ;
#176250 = AXIS2_PLACEMENT_3D ( 'NONE', #39850, #60648, #240591 ) ;
#176252 = ORIENTED_EDGE ( 'NONE', *, *, #27834, .T. ) ;
#176253 = AXIS2_PLACEMENT_3D ( 'NONE', #140924, #58785, #217857 ) ;
#176254 = PLANE ( 'NONE',  #36916 ) ;
#176255 = ORIENTED_EDGE ( 'NONE', *, *, #232207, .T. ) ;
#176256 = AXIS2_PLACEMENT_3D ( 'NONE', #71345, #191307, #150858 ) ;
#176257 = TOROIDAL_SURFACE ( 'NONE', #242863, 0.2000000000000000111, 0.1000000000000000056 ) ;
#176258 = TOROIDAL_SURFACE ( 'NONE', #247134, 0.2000000000000000111, 0.1000000000000000056 ) ;
#176259 = AXIS2_PLACEMENT_3D ( 'NONE', #133368, #77223, #218004 ) ;
#176260 = DIRECTION ( 'NONE',  ( -1.000000000000000000, 0.000000000000000000, 0.000000000000000000 ) ) ;
#176261 = ORIENTED_EDGE ( 'NONE', *, *, #250772, .F. ) ;
#176262 = EDGE_CURVE ( 'NONE', #79923, #176243, #119495, .T. ) ;
#176263 = VERTEX_POINT ( 'NONE', #56906 ) ;
#176264 = ADVANCED_FACE ( 'NONE', ( #116917 ), #49977, .T. ) ;
#176265 = CARTESIAN_POINT ( 'NONE',  ( 23.14999999999998792, 55.98745301258801987, -232.8057040749261262 ) ) ;
#176267 = ORIENTED_EDGE ( 'NONE', *, *, #224227, .F. ) ;
#176266 = CARTESIAN_POINT ( 'NONE',  ( -16.90138253750127362, 9.950000000011138823, -121.2115627079046618 ) ) ;
#176268 = CARTESIAN_POINT ( 'NONE',  ( -23.15000000000000213, 76.00000000001126921, -203.5231074845248997 ) ) ;
#176269 = CARTESIAN_POINT ( 'NONE',  ( -18.41431012584570226, 33.94987820762823816, -235.0681983671880175 ) ) ;
#176270 = ORIENTED_EDGE ( 'NONE', *, *, #216228, .T. ) ;
#176271 = CARTESIAN_POINT ( 'NONE',  ( 20.99999999999998934, 7.986648289447971116, -1.311673547813416718 ) ) ;
#176272 = CARTESIAN_POINT ( 'NONE',  ( -21.05000000000000071, 67.23127455305841238, -235.8551265064783991 ) ) ;
#176273 = CYLINDRICAL_SURFACE ( 'NONE', #257044, 0.09999999999999957534 ) ;
#176274 = CARTESIAN_POINT ( 'NONE',  ( -20.64999999999999858, 84.66355140188112216, -112.5472086025915388 ) ) ;
#176275 = PLANE ( 'NONE',  #128831 ) ;
#176276 = DIRECTION ( 'NONE',  ( 0.000000000000000000, 0.000000000000000000, -1.000000000000000000 ) ) ;
#176277 = CARTESIAN_POINT ( 'NONE',  ( 21.30000000000002558, 1.115650265596050101E-11, -129.9500000000000171 ) ) ;
#176278 = EDGE_CURVE ( 'NONE', #166383, #81086, #253978, .T. ) ;
#176279 = CARTESIAN_POINT ( 'NONE',  ( 21.04999999999999716, 76.08561306081617204, -142.9368672183345552 ) ) ;
#176280 = DIRECTION ( 'NONE',  ( -1.000000000000000000, 0.000000000000000000, 0.000000000000000000 ) ) ;
#176282 = VERTEX_POINT ( 'NONE', #118202 ) ;
#176281 = AXIS2_PLACEMENT_3D ( 'NONE', #85327, #141472, #164898 ) ;
#176283 = AXIS2_PLACEMENT_3D ( 'NONE', #67424, #249918, #71301 ) ;
#176285 = EDGE_LOOP ( 'NONE', ( #222845, #41548, #120574 ) ) ;
#176284 = ORIENTED_EDGE ( 'NONE', *, *, #116228, .T. ) ;
#176286 = ORIENTED_EDGE ( 'NONE', *, *, #199348, .F. ) ;
#176287 = DIRECTION ( 'NONE',  ( 0.000000000000000000, 0.000000000000000000, -1.000000000000000000 ) ) ;
#176288 = DIRECTION ( 'NONE',  ( 1.000000000000000000, 0.000000000000000000, 0.000000000000000000 ) ) ;
#176290 = DIRECTION ( 'NONE',  ( 1.000000000000000000, -0.000000000000000000, -0.000000000000000000 ) ) ;
#176289 = DIRECTION ( 'NONE',  ( 0.000000000000000000, 0.8814952561688476074, -0.4721928772777262417 ) ) ;
#176291 = VERTEX_POINT ( 'NONE', #201578 ) ;
#176292 = EDGE_CURVE ( 'NONE', #238447, #42338, #54246, .T. ) ;
#176293 =( NAMED_UNIT ( * ) SI_UNIT ( $, .STERADIAN. ) SOLID_ANGLE_UNIT ( ) );
#176294 = DIRECTION ( 'NONE',  ( 1.000000000000000000, -0.000000000000000000, 0.000000000000000000 ) ) ;
#176295 = CARTESIAN_POINT ( 'NONE',  ( -16.89060415895970735, 9.951220762813354881, -180.1459202242704123 ) ) ;
#176296 = EDGE_CURVE ( 'NONE', #133079, #72361, #158352, .T. ) ;
#176297 = CARTESIAN_POINT ( 'NONE',  ( 18.44444291854883033, -9.490101180932070335, -73.62890396489098066 ) ) ;
#176298 = ORIENTED_EDGE ( 'NONE', *, *, #233943, .T. ) ;
#176299 = ORIENTED_EDGE ( 'NONE', *, *, #82869, .T. ) ;
#176300 = CARTESIAN_POINT ( 'NONE',  ( -22.39999999999999858, 68.20922040163927136, -203.6231074845244109 ) ) ;
#176301 = EDGE_CURVE ( 'NONE', #16177, #233882, #81600, .T. ) ;
#176302 = CIRCLE ( 'NONE', #63855, 0.1000000000000002831 ) ;
#176303 = ADVANCED_FACE ( 'NONE', ( #178201 ), #25075, .T. ) ;
#176304 = ORIENTED_EDGE ( 'NONE', *, *, #73190, .T. ) ;
#176305 = PLANE ( 'NONE',  #16348 ) ;
#176306 = DIRECTION ( 'NONE',  ( -1.000000000000000000, -0.000000000000000000, -0.000000000000000000 ) ) ;
#176307 = DIRECTION ( 'NONE',  ( 0.000000000000000000, 0.000000000000000000, 1.000000000000000000 ) ) ;
#176308 = DIRECTION ( 'NONE',  ( 0.000000000000000000, 0.000000000000000000, -1.000000000000000000 ) ) ;
#176309 = CYLINDRICAL_SURFACE ( 'NONE', #69042, 0.09999999999999939493 ) ;
#176310 = EDGE_CURVE ( 'NONE', #249247, #136022, #136453, .T. ) ;
#176311 = DIRECTION ( 'NONE',  ( 0.000000000000000000, 6.982962677686266711E-15, -1.000000000000000000 ) ) ;
#176312 = ORIENTED_EDGE ( 'NONE', *, *, #189619, .F. ) ;
#176313 = CARTESIAN_POINT ( 'NONE',  ( -21.07928932188134041, 1.115600667400684642E-11, -33.50000000000000000 ) ) ;
#176314 = DIRECTION ( 'NONE',  ( 0.000000000000000000, 0.4721928772777346239, 0.8814952561688430555 ) ) ;
#176315 = CARTESIAN_POINT ( 'NONE',  ( -21.37071067811865532, 8.070710678129811910, -54.65000000000000568 ) ) ;
#176317 = CARTESIAN_POINT ( 'NONE',  ( 21.05000000000000071, 76.00000000001244871, -170.0231074845243597 ) ) ;
#176316 = CARTESIAN_POINT ( 'NONE',  ( -16.85312841634287295, 66.08639382269184637, -123.6259343512318480 ) ) ;
#176318 = DIRECTION ( 'NONE',  ( 0.000000000000000000, 0.8814952561688430555, -0.4721928772777346239 ) ) ;
#176319 = DIRECTION ( 'NONE',  ( 0.000000000000000000, -0.7397360091702802620, 0.6728971962616779878 ) ) ;
#176320 = CARTESIAN_POINT ( 'NONE',  ( 18.52351027002947959, 85.64216290470756121, -163.3080605340145439 ) ) ;
#176321 = CARTESIAN_POINT ( 'NONE',  ( 22.49999999999999645, 75.91119002362509605, -114.6728704025562422 ) ) ;
#176322 = AXIS2_PLACEMENT_3D ( 'NONE', #241243, #26046, #202108 ) ;
#176323 = ORIENTED_EDGE ( 'NONE', *, *, #1682, .T. ) ;
#176324 = ADVANCED_FACE ( 'NONE', ( #17799 ), #87566, .T. ) ;
#176325 = TOROIDAL_SURFACE ( 'NONE', #105522, 0.4000000000000005773, 0.1000000000000000056 ) ;
#176326 = EDGE_CURVE ( 'NONE', #58209, #66400, #16685, .T. ) ;
#176327 = VERTEX_POINT ( 'NONE', #38667 ) ;
#176328 = DIRECTION ( 'NONE',  ( 0.000000000000000000, -0.8777080977375132376, 0.4791956752371582251 ) ) ;
#176329 = ORIENTED_EDGE ( 'NONE', *, *, #237813, .F. ) ;
#176330 = EDGE_CURVE ( 'NONE', #98991, #171186, #170849, .T. ) ;
#176331 = CARTESIAN_POINT ( 'NONE',  ( -20.85000000000000142, 74.74783850729542678, -233.7633982527047465 ) ) ;
#176332 = EDGE_CURVE ( 'NONE', #51404, #78551, #104135, .T. ) ;
#176333 = CARTESIAN_POINT ( 'NONE',  ( 20.94999999999999929, 1.115600667400684642E-11, -100.5000000000000426 ) ) ;
#176334 = VERTEX_POINT ( 'NONE', #20401 ) ;
#176335 = AXIS2_PLACEMENT_3D ( 'NONE', #236718, #58073, #118068 ) ;
#176336 = CARTESIAN_POINT ( 'NONE',  ( 18.59999999999999076, 64.35000000001220144, -145.1731074845244507 ) ) ;
#176337 = CARTESIAN_POINT ( 'NONE',  ( -14.87770893841226716, 9.430637101707896264, -51.76826061806094970 ) ) ;
#176338 = CARTESIAN_POINT ( 'NONE',  ( -18.59999999999999787, 66.75000000001260503, -191.1731074845244223 ) ) ;
#176339 = CIRCLE ( 'NONE', #43056, 12.87499999999999822 ) ;
#176340 = EDGE_CURVE ( 'NONE', #27168, #58719, #218411, .T. ) ;
#176341 = LINE ( 'NONE', #257086, #170479 ) ;
#176343 = ORIENTED_EDGE ( 'NONE', *, *, #207996, .F. ) ;
#176342 = CARTESIAN_POINT ( 'NONE',  ( -21.14999999999999858, 64.25000000001269029, -203.4231074845244507 ) ) ;
#176345 = DIRECTION ( 'NONE',  ( 0.000000000000000000, 0.000000000000000000, 1.000000000000000000 ) ) ;
#176344 = CARTESIAN_POINT ( 'NONE',  ( -20.64999999999999858, 74.00000000001223555, -149.7477294072864709 ) ) ;
#176346 = DIRECTION ( 'NONE',  ( 0.000000000000000000, 8.673617379884030739E-15, -1.000000000000000000 ) ) ;
#176347 = EDGE_CURVE ( 'NONE', #205644, #19990, #783, .T. ) ;
#176348 = CYLINDRICAL_SURFACE ( 'NONE', #169173, 0.09999999999999939493 ) ;
#176349 = CARTESIAN_POINT ( 'NONE',  ( -19.99999999999999645, 5.552655413246002425, 16.61686199900910310 ) ) ;
#176350 = DIRECTION ( 'NONE',  ( -0.000000000000000000, 0.8814952561688430555, -0.4721928772777346239 ) ) ;
#176351 = ORIENTED_EDGE ( 'NONE', *, *, #239012, .T. ) ;
#176352 = EDGE_CURVE ( 'NONE', #246137, #104540, #183263, .T. ) ;
#176353 = DIRECTION ( 'NONE',  ( 1.000000000000000000, 0.000000000000000000, 0.000000000000000000 ) ) ;
#176354 = CIRCLE ( 'NONE', #147096, 11.65000000000000036 ) ;
#176355 = AXIS2_PLACEMENT_3D ( 'NONE', #179015, #143691, #21217 ) ;
#176356 = EDGE_LOOP ( 'NONE', ( #189373, #238516, #40761, #80651 ) ) ;
#176357 = DIRECTION ( 'NONE',  ( 0.000000000000000000, -0.4088369013363281068, 0.9126074666063770380 ) ) ;
#176358 = ORIENTED_EDGE ( 'NONE', *, *, #250503, .F. ) ;
#176359 = LINE ( 'NONE', #172542, #63820 ) ;
#176360 = AXIS2_PLACEMENT_3D ( 'NONE', #145471, #26851, #127207 ) ;
#176361 = DIRECTION ( 'NONE',  ( -0.000000000000000000, 0.000000000000000000, -1.000000000000000000 ) ) ;
#176362 = CARTESIAN_POINT ( 'NONE',  ( -21.05000000000000071, 46.54514716347711101, -243.1111603596801842 ) ) ;
#176363 = EDGE_CURVE ( 'NONE', #152762, #74814, #88026, .T. ) ;
#176364 = ORIENTED_EDGE ( 'NONE', *, *, #113272, .T. ) ;
#176365 = EDGE_LOOP ( 'NONE', ( #106915, #207199, #215348, #84948, #248800 ) ) ;
#176366 = CIRCLE ( 'NONE', #55687, 0.09999999999998898659 ) ;
#176367 = AXIS2_PLACEMENT_3D ( 'NONE', #238695, #237417, #138287 ) ;
#176368 = AXIS2_PLACEMENT_3D ( 'NONE', #182183, #3521, #29550 ) ;
#176369 = AXIS2_PLACEMENT_3D ( 'NONE', #184355, #65701, #180526 ) ;
#176371 = EDGE_CURVE ( 'NONE', #216334, #201073, #33457, .T. ) ;
#176370 = DIRECTION ( 'NONE',  ( 0.000000000000000000, -1.776356839400271369E-15, 1.000000000000000000 ) ) ;
#176372 = CARTESIAN_POINT ( 'NONE',  ( 20.95224633520496127, 10.50403838541865831, -207.4047027453351006 ) ) ;
#176373 = CARTESIAN_POINT ( 'NONE',  ( -16.88783316861815109, 63.05896443345586277, -213.2263201824675889 ) ) ;
#176374 = CARTESIAN_POINT ( 'NONE',  ( -20.54999999999999716, 62.04503132991428060, -248.4786563706009588 ) ) ;
#176376 = CARTESIAN_POINT ( 'NONE',  ( 20.94999999999999929, 17.05609719657923407, -224.5686720499523119 ) ) ;
#176375 = DIRECTION ( 'NONE',  ( 1.000000000000000000, 0.000000000000000000, 0.000000000000000000 ) ) ;
#176377 = CARTESIAN_POINT ( 'NONE',  ( 20.85000000000000142, 64.25000000001175238, -76.30697314750248950 ) ) ;
#176378 = DIRECTION ( 'NONE',  ( 1.000000000000000000, 0.000000000000000000, 0.000000000000000000 ) ) ;
#176379 = CARTESIAN_POINT ( 'NONE',  ( 20.94999999999999929, 19.00443933019177223, -232.7770257915295531 ) ) ;
#176380 = VERTEX_POINT ( 'NONE', #26831 ) ;
#176381 = CYLINDRICAL_SURFACE ( 'NONE', #227319, 0.09999999999999939493 ) ;
#176383 = ORIENTED_EDGE ( 'NONE', *, *, #8298, .F. ) ;
#176382 = DIRECTION ( 'NONE',  ( 0.000000000000000000, -6.608470384673536035E-15, 1.000000000000000000 ) ) ;
#176384 = CARTESIAN_POINT ( 'NONE',  ( 20.94999999999999929, 63.62814136979439184, -224.4990371885399441 ) ) ;
#176385 = FACE_OUTER_BOUND ( 'NONE', #168312, .T. ) ;
#176387 = CARTESIAN_POINT ( 'NONE',  ( -23.25000000000000000, -9.682403433465239573, -73.65684337741279819 ) ) ;
#176386 = FACE_OUTER_BOUND ( 'NONE', #162931, .T. ) ;
#176388 = ADVANCED_FACE ( 'NONE', ( #145449 ), #62474, .F. ) ;
#176389 = ORIENTED_EDGE ( 'NONE', *, *, #167578, .F. ) ;
#176391 = CARTESIAN_POINT ( 'NONE',  ( 18.59999999999999787, 74.14897176987174987, -191.8691942151018850 ) ) ;
#176390 = CARTESIAN_POINT ( 'NONE',  ( 23.14999999999999503, 64.25000000001195133, -110.0379132551783243 ) ) ;
#176392 = CARTESIAN_POINT ( 'NONE',  ( -16.97683809663752186, 66.05000000001190585, -93.77310748452438816 ) ) ;
#176393 = DIRECTION ( 'NONE',  ( 0.000000000000000000, 0.000000000000000000, -1.000000000000000000 ) ) ;
#176394 = LINE ( 'NONE', #137239, #140898 ) ;
#176395 = CARTESIAN_POINT ( 'NONE',  ( -18.59117750673696889, 10.33248238083634796, -139.5948465439131780 ) ) ;
#176396 = EDGE_LOOP ( 'NONE', ( #192468, #66421, #237055 ) ) ;
#176397 = FACE_OUTER_BOUND ( 'NONE', #233337, .T. ) ;
#176398 = VERTEX_POINT ( 'NONE', #241992 ) ;
#176399 = AXIS2_PLACEMENT_3D ( 'NONE', #156746, #137150, #217945 ) ;
#176400 = CARTESIAN_POINT ( 'NONE',  ( 22.50046968639222200, 75.95483015287750561, -215.2731526389931105 ) ) ;
#176401 = ORIENTED_EDGE ( 'NONE', *, *, #15574, .T. ) ;
#176402 = ADVANCED_FACE ( 'NONE', ( #67209 ), #245851, .F. ) ;
#176403 = CARTESIAN_POINT ( 'NONE',  ( -20.89878130938411616, 46.45193731540633308, -243.0811559066744110 ) ) ;
#176404 = AXIS2_PLACEMENT_3D ( 'NONE', #171002, #208800, #147536 ) ;
#176405 = ORIENTED_EDGE ( 'NONE', *, *, #90568, .F. ) ;
#176406 = CARTESIAN_POINT ( 'NONE',  ( 20.85000000000000142, 1.115600667400684642E-11, -167.5000000000000284 ) ) ;
#176407 = AXIS2_PLACEMENT_3D ( 'NONE', #169750, #49758, #71908 ) ;
#176408 = VECTOR ( 'NONE', #44450, 999.9999999999998863 ) ;
#176409 = CARTESIAN_POINT ( 'NONE',  ( -20.64999999999999858, 68.75000000001230660, -157.7731074845244166 ) ) ;
#176410 = EDGE_LOOP ( 'NONE', ( #134260, #174389, #204428, #236732 ) ) ;
#176411 = CIRCLE ( 'NONE', #68056, 0.1000000000000058481 ) ;
#176412 = FACE_OUTER_BOUND ( 'NONE', #46914, .T. ) ;
#176414 = AXIS2_PLACEMENT_3D ( 'NONE', #85067, #207641, #6851 ) ;
#176413 = FACE_OUTER_BOUND ( 'NONE', #17268, .T. ) ;
#176415 = DIRECTION ( 'NONE',  ( 1.000000000000000000, 0.000000000000000000, -0.000000000000000000 ) ) ;
#176416 = AXIS2_PLACEMENT_3D ( 'NONE', #69451, #246769, #130680 ) ;
#176417 = AXIS2_PLACEMENT_3D ( 'NONE', #164194, #143326, #80769 ) ;
#176418 = DIRECTION ( 'NONE',  ( 0.000000000000000000, 0.000000000000000000, -1.000000000000000000 ) ) ;
#176419 = AXIS2_PLACEMENT_3D ( 'NONE', #6898, #70761, #68161 ) ;
#176420 = CARTESIAN_POINT ( 'NONE',  ( -16.94052228080551714, 66.01372026691315398, -115.6327319818549455 ) ) ;
#176421 = ORIENTED_EDGE ( 'NONE', *, *, #108436, .T. ) ;
#176422 = CARTESIAN_POINT ( 'NONE',  ( -18.44232395689948589, 85.55228255706195739, -129.6808554997166141 ) ) ;
#176423 = ORIENTED_EDGE ( 'NONE', *, *, #207560, .F. ) ;
#176425 = VERTEX_POINT ( 'NONE', #102447 ) ;
#176424 = CARTESIAN_POINT ( 'NONE',  ( 21.08832698747859169, 67.22463560659464576, -90.79439001806022702 ) ) ;
#176426 = VECTOR ( 'NONE', #87922, 1000.000000000000000 ) ;
#176427 = ORIENTED_EDGE ( 'NONE', *, *, #111064, .T. ) ;
#176428 = LINE ( 'NONE', #79842, #32334 ) ;
#176429 = DIRECTION ( 'NONE',  ( 0.000000000000000000, 0.000000000000000000, -1.000000000000000000 ) ) ;
#176430 = CARTESIAN_POINT ( 'NONE',  ( 23.15000000000000213, -11.64999999998883595, -63.89999999999999858 ) ) ;
#176431 = CARTESIAN_POINT ( 'NONE',  ( 23.14999999999999858, 5.600000000011153389, -54.59473398108690390 ) ) ;
#176432 = ORIENTED_EDGE ( 'NONE', *, *, #249196, .T. ) ;
#176433 = CARTESIAN_POINT ( 'NONE',  ( 23.24999999999999645, 8.822561741677553471, -54.34999999999999432 ) ) ;
#176435 = DIRECTION ( 'NONE',  ( 0.000000000000000000, 0.9908441862701596881, -0.1350103645451904977 ) ) ;
#176434 = CIRCLE ( 'NONE', #80710, 0.09999999999999939493 ) ;
#176436 = EDGE_LOOP ( 'NONE', ( #106059, #90228, #225746, #45003 ) ) ;
#176438 = VERTEX_POINT ( 'NONE', #106311 ) ;
#176437 = CARTESIAN_POINT ( 'NONE',  ( -23.49999999999994316, 76.00000000001119815, -36.02310748452479316 ) ) ;
#176439 = EDGE_CURVE ( 'NONE', #127497, #148843, #208215, .T. ) ;
#176440 = FACE_OUTER_BOUND ( 'NONE', #85085, .T. ) ;
#176441 = CIRCLE ( 'NONE', #209736, 0.09999999999999986677 ) ;
#176442 = CARTESIAN_POINT ( 'NONE',  ( 21.33487959338958362, 6.725558151922348848, -100.5000000000000284 ) ) ;
#176443 = ORIENTED_EDGE ( 'NONE', *, *, #87426, .F. ) ;
#176444 = AXIS2_PLACEMENT_3D ( 'NONE', #158590, #178153, #118155 ) ;
#176445 = CIRCLE ( 'NONE', #138961, 0.5000000000000014433 ) ;
#176446 = AXIS2_PLACEMENT_3D ( 'NONE', #184033, #220606, #5370 ) ;
#176447 = CARTESIAN_POINT ( 'NONE',  ( 21.05000000000000071, 64.25000000001195133, -110.0379132551783243 ) ) ;
#176448 = ORIENTED_EDGE ( 'NONE', *, *, #218391, .T. ) ;
#176449 = CARTESIAN_POINT ( 'NONE',  ( 18.59999999999999076, 46.45388641681647357, -243.1520440498138385 ) ) ;
#176450 = EDGE_CURVE ( 'NONE', #201052, #183877, #123341, .T. ) ;
#176451 = DIRECTION ( 'NONE',  ( 1.000000000000000000, -0.000000000000000000, 0.000000000000000000 ) ) ;
#176452 = LINE ( 'NONE', #79865, #51555 ) ;
#176453 = EDGE_CURVE ( 'NONE', #214434, #13316, #162428, .T. ) ;
#176454 = DIRECTION ( 'NONE',  ( -4.408576920032448588E-17, -0.1350103645451807555, -0.9908441862701609093 ) ) ;
#176456 = EDGE_CURVE ( 'NONE', #197503, #49384, #52431, .T. ) ;
#176455 = AXIS2_PLACEMENT_3D ( 'NONE', #245459, #26415, #207619 ) ;
#176457 = CIRCLE ( 'NONE', #64012, 0.1000000000000011990 ) ;
#176458 = CIRCLE ( 'NONE', #159696, 0.09999999999999939493 ) ;
#176459 = CIRCLE ( 'NONE', #138793, 11.64999999999999325 ) ;
#176460 = EDGE_LOOP ( 'NONE', ( #146224, #94380, #191962, #210797 ) ) ;
#176461 = DIRECTION ( 'NONE',  ( 6.484947573744954877E-15, -0.9274965247785555977, 0.3738317757009190223 ) ) ;
#176462 = EDGE_CURVE ( 'NONE', #207133, #133625, #124623, .T. ) ;
#176463 = ORIENTED_EDGE ( 'NONE', *, *, #35619, .T. ) ;
#176464 = CARTESIAN_POINT ( 'NONE',  ( -18.59999999999999787, -1.164121893230052995, -141.9148480855716343 ) ) ;
#176465 = PLANE ( 'NONE',  #220663 ) ;
#176467 = EDGE_LOOP ( 'NONE', ( #167161, #55093, #89374, #116627 ) ) ;
#176466 = DIRECTION ( 'NONE',  ( 1.000000000000000000, 0.000000000000000000, 0.000000000000000000 ) ) ;
#176468 = FACE_OUTER_BOUND ( 'NONE', #212790, .T. ) ;
#176469 = CARTESIAN_POINT ( 'NONE',  ( -20.64999999999999858, -8.999999999988846255, -143.3939691226524644 ) ) ;
#176470 = EDGE_CURVE ( 'NONE', #194529, #143771, #4186, .T. ) ;
#176471 = CARTESIAN_POINT ( 'NONE',  ( 19.99999999999998934, 15.90518444080776383, -219.2841490888777116 ) ) ;
#176472 = LINE ( 'NONE', #255929, #46489 ) ;
#176473 = LINE ( 'NONE', #255930, #56289 ) ;
#176474 = SPHERICAL_SURFACE ( 'NONE', #43351, 0.1000000000000000056 ) ;
#176475 = DIRECTION ( 'NONE',  ( 0.000000000000000000, 0.000000000000000000, -1.000000000000000000 ) ) ;
#176477 = ORIENTED_EDGE ( 'NONE', *, *, #18841, .T. ) ;
#176476 = DIRECTION ( 'NONE',  ( -1.000000000000000000, 0.000000000000000000, 0.000000000000000000 ) ) ;
#176478 = EDGE_CURVE ( 'NONE', #22276, #193833, #8525, .T. ) ;
#176479 = B_SPLINE_CURVE_WITH_KNOTS ( 'NONE', 3,
 ( #212714, #193154, #94024, #173633, #253098, #74523, #78311, #121347, #41795, #44348 ),
 .UNSPECIFIED., .F., .F.,
 ( 4, 3, 3, 4 ),
 ( 7.632826238681267430E-06, 4.756916949875584252E-05, 9.484459048150138379E-05, 0.0001435500935099836574 ),
 .UNSPECIFIED. ) ;
#176480 = CARTESIAN_POINT ( 'NONE',  ( -16.87683809663752399, 50.97313360171294505, -232.3453239361865315 ) ) ;
#176481 = AXIS2_PLACEMENT_3D ( 'NONE', #207542, #168458, #69317 ) ;
#176482 = DIRECTION ( 'NONE',  ( 1.000000000000000000, 0.000000000000000000, 0.000000000000000000 ) ) ;
#176483 = CARTESIAN_POINT ( 'NONE',  ( 21.53699400380198981, 69.21228820681629657, -103.0231074845243455 ) ) ;
#176484 = ORIENTED_EDGE ( 'NONE', *, *, #110658, .T. ) ;
#176485 = DIRECTION ( 'NONE',  ( -1.000000000000000000, -0.000000000000000000, 0.000000000000000000 ) ) ;
#176486 = EDGE_CURVE ( 'NONE', #161554, #97541, #204744, .T. ) ;
#176487 = CARTESIAN_POINT ( 'NONE',  ( -18.42609945526418258, 85.49999971050182523, -62.52374499427813959 ) ) ;
#176488 = ORIENTED_EDGE ( 'NONE', *, *, #120753, .T. ) ;
#176489 = CIRCLE ( 'NONE', #238842, 11.74999999999999822 ) ;
#176490 = FACE_OUTER_BOUND ( 'NONE', #19370, .T. ) ;
#176491 = AXIS2_PLACEMENT_3D ( 'NONE', #228034, #149806, #248889 ) ;
#176492 = VECTOR ( 'NONE', #94153, 1000.000000000000227 ) ;
#176493 = CARTESIAN_POINT ( 'NONE',  ( -21.14999999999999858, -11.64999999998884483, -170.3999999999999773 ) ) ;
#176494 = EDGE_CURVE ( 'NONE', #83651, #177470, #712, .T. ) ;
#176495 = ORIENTED_EDGE ( 'NONE', *, *, #29363, .F. ) ;
#176496 = DIRECTION ( 'NONE',  ( -0.000000000000000000, -0.8454177738465993297, -0.5341055959866553016 ) ) ;
#176497 = ORIENTED_EDGE ( 'NONE', *, *, #99967, .F. ) ;
#176498 = FACE_OUTER_BOUND ( 'NONE', #213034, .T. ) ;
#176500 = VERTEX_POINT ( 'NONE', #224974 ) ;
#176499 = CARTESIAN_POINT ( 'NONE',  ( 21.05000000000000071, 6.540656951712403355, -134.1000000000000227 ) ) ;
#176501 = CARTESIAN_POINT ( 'NONE',  ( -18.59999999999999787, -1.835859311443637010, -45.00443916879852679 ) ) ;
#176502 = VERTEX_POINT ( 'NONE', #22982 ) ;
#176503 = CARTESIAN_POINT ( 'NONE',  ( -20.94999999999999929, 76.00000000001189449, -95.12310748452431142 ) ) ;
#176504 = ORIENTED_EDGE ( 'NONE', *, *, #5499, .T. ) ;
#176506 = ORIENTED_EDGE ( 'NONE', *, *, #77597, .F. ) ;
#176505 = ORIENTED_EDGE ( 'NONE', *, *, #194278, .F. ) ;
#176508 = FACE_OUTER_BOUND ( 'NONE', #202138, .T. ) ;
#176507 = AXIS2_PLACEMENT_3D ( 'NONE', #50056, #93038, #171348 ) ;
#176509 = VERTEX_POINT ( 'NONE', #46347 ) ;
#176510 = ADVANCED_FACE ( 'NONE', ( #182030 ), #67391, .F. ) ;
#176511 = CARTESIAN_POINT ( 'NONE',  ( 21.05000000000000071, 71.00000000001230660, -157.6178414656113205 ) ) ;
#176512 = ORIENTED_EDGE ( 'NONE', *, *, #195180, .F. ) ;
#176513 = AXIS2_PLACEMENT_3D ( 'NONE', #150174, #233560, #189291 ) ;
#176514 = ADVANCED_FACE ( 'NONE', ( #3364 ), #179842, .T. ) ;
#176515 = AXIS2_PLACEMENT_3D ( 'NONE', #165225, #3572, #103939 ) ;
#176516 = VECTOR ( 'NONE', #222667, 999.9999999999998863 ) ;
#176517 = EDGE_LOOP ( 'NONE', ( #65214, #19817, #115301, #136339 ) ) ;
#176518 = CARTESIAN_POINT ( 'NONE',  ( 23.40000000000005187, 83.90000000001120384, -37.27310748452479316 ) ) ;
#176519 = CARTESIAN_POINT ( 'NONE',  ( 22.24259225415828567, 75.90093411655887223, -77.01504535508973959 ) ) ;
#176520 = ADVANCED_FACE ( 'NONE', ( #71082 ), #125648, .F. ) ;
#176521 = LINE ( 'NONE', #156965, #78322 ) ;
#176522 = LINE ( 'NONE', #158269, #168920 ) ;
#176523 = ORIENTED_EDGE ( 'NONE', *, *, #44465, .T. ) ;
#176524 = CARTESIAN_POINT ( 'NONE',  ( -21.14999999999999858, 64.25000000001210765, -129.7392418215462158 ) ) ;
#176525 = CARTESIAN_POINT ( 'NONE',  ( -16.87331047859651179, 9.950000000011142376, -146.6500000000000341 ) ) ;
#176526 = CARTESIAN_POINT ( 'NONE',  ( -18.40000000000000213, 67.17743825834568838, -127.2731074845243597 ) ) ;
#176527 = CIRCLE ( 'NONE', #218175, 0.5000000000000004441 ) ;
#176529 = ORIENTED_EDGE ( 'NONE', *, *, #247347, .F. ) ;
#176528 = EDGE_CURVE ( 'NONE', #134956, #16525, #238062, .T. ) ;
#176530 = VECTOR ( 'NONE', #164030, 1000.000000000000000 ) ;
#176532 = ADVANCED_FACE ( 'NONE', ( #189730 ), #149340, .T. ) ;
#176531 = LINE ( 'NONE', #35744, #67052 ) ;
#176533 = DIRECTION ( 'NONE',  ( 0.000000000000000000, 0.5000683049008540770, 0.8659859643398306606 ) ) ;
#176534 = CARTESIAN_POINT ( 'NONE',  ( 20.94999999999999929, 67.23127455305841238, -235.8551265064783991 ) ) ;
#176535 = VECTOR ( 'NONE', #61289, 1000.000000000000000 ) ;
#176536 = ORIENTED_EDGE ( 'NONE', *, *, #121171, .F. ) ;
#176537 = DIRECTION ( 'NONE',  ( 0.000000000000000000, -0.000000000000000000, -1.000000000000000000 ) ) ;
#176538 = EDGE_LOOP ( 'NONE', ( #37605, #139368, #189757, #41247 ) ) ;
#176539 = ORIENTED_EDGE ( 'NONE', *, *, #21799, .F. ) ;
#176540 = DIRECTION ( 'NONE',  ( 0.000000000000000000, 0.9126074666063769270, 0.4088369013363280513 ) ) ;
#176541 = EDGE_CURVE ( 'NONE', #105422, #214442, #167377, .T. ) ;
#176543 = EDGE_LOOP ( 'NONE', ( #198959, #43863, #47338, #116108 ) ) ;
#176542 = AXIS2_PLACEMENT_3D ( 'NONE', #64365, #225959, #223412 ) ;
#176544 = ORIENTED_EDGE ( 'NONE', *, *, #48973, .T. ) ;
#176545 = CARTESIAN_POINT ( 'NONE',  ( -22.50000000000000000, 11.36403278914770176, -198.4341430231427807 ) ) ;
#176546 = CARTESIAN_POINT ( 'NONE',  ( -23.25000000000000000, 76.00000000001170974, -69.52310748452431710 ) ) ;
#176547 = VERTEX_POINT ( 'NONE', #177592 ) ;
#176548 = ORIENTED_EDGE ( 'NONE', *, *, #189692, .F. ) ;
#176549 = CYLINDRICAL_SURFACE ( 'NONE', #239605, 11.75000000000001066 ) ;
#176550 = AXIS2_PLACEMENT_3D ( 'NONE', #130283, #204679, #49476 ) ;
#176551 = AXIS2_PLACEMENT_3D ( 'NONE', #43335, #143700, #64177 ) ;
#176552 = DIRECTION ( 'NONE',  ( 1.000000000000000000, 0.000000000000000000, 0.000000000000000000 ) ) ;
#176553 = AXIS2_PLACEMENT_3D ( 'NONE', #131465, #211011, #230579 ) ;
#176554 = EDGE_LOOP ( 'NONE', ( #130407, #121537, #17444, #86468 ) ) ;
#176555 = VERTEX_POINT ( 'NONE', #158039 ) ;
#176556 = EDGE_LOOP ( 'NONE', ( #212743, #209323, #195811, #99916 ) ) ;
#176557 = DIRECTION ( 'NONE',  ( 0.000000000000000000, -6.982962677686266711E-15, 1.000000000000000000 ) ) ;
#176558 = DIRECTION ( 'NONE',  ( 1.000000000000000000, -0.000000000000000000, 0.000000000000000000 ) ) ;
#176559 = EDGE_CURVE ( 'NONE', #45948, #206992, #63278, .T. ) ;
#176560 = ADVANCED_FACE ( 'NONE', ( #194579 ), #121594, .T. ) ;
#176561 = CARTESIAN_POINT ( 'NONE',  ( -20.94999999999999929, 74.16465844978745281, -91.46795619196133487 ) ) ;
#176562 = CARTESIAN_POINT ( 'NONE',  ( 20.85000000000000142, -1.835859311432481045, -112.0044391687985694 ) ) ;
#176563 = CARTESIAN_POINT ( 'NONE',  ( -16.94107738177415712, 10.01423928514777728, -113.0500000000000398 ) ) ;
#176564 = CARTESIAN_POINT ( 'NONE',  ( -23.15000000000000213, 64.25000000001195133, -109.8647081744214375 ) ) ;
#176565 = DIRECTION ( 'NONE',  ( -3.265361837132813093E-16, 1.000000000000000000, 0.000000000000000000 ) ) ;
#176566 = AXIS2_PLACEMENT_3D ( 'NONE', #628, #220978, #181872 ) ;
#176568 = DIRECTION ( 'NONE',  ( 0.000000000000000000, -0.000000000000000000, 1.000000000000000000 ) ) ;
#176567 = CARTESIAN_POINT ( 'NONE',  ( 20.05000000000002913, 7.250000000011171508, -146.6500000000000341 ) ) ;
#176569 = DIRECTION ( 'NONE',  ( -1.000000000000000000, 0.000000000000000000, 0.000000000000000000 ) ) ;
#176570 = DIRECTION ( 'NONE',  ( -0.5932847527679299127, -0.8049926720990051576, -6.257843056355997642E-15 ) ) ;
#176571 = CIRCLE ( 'NONE', #139101, 0.5000000000000004441 ) ;
#176572 = EDGE_CURVE ( 'NONE', #131693, #169929, #192293, .T. ) ;
#176573 = FACE_OUTER_BOUND ( 'NONE', #84763, .T. ) ;
#176575 = DIRECTION ( 'NONE',  ( 0.000000000000000000, 0.000000000000000000, -1.000000000000000000 ) ) ;
#176574 = CIRCLE ( 'NONE', #9956, 0.1000000000000028644 ) ;
#176576 = ORIENTED_EDGE ( 'NONE', *, *, #43814, .T. ) ;
#176577 = CIRCLE ( 'NONE', #26552, 0.1000000000000002554 ) ;
#176578 = AXIS2_PLACEMENT_3D ( 'NONE', #149670, #33603, #193923 ) ;
#176580 = VERTEX_POINT ( 'NONE', #175039 ) ;
#176579 = CARTESIAN_POINT ( 'NONE',  ( -18.50000000000000000, -0.5913595841389538421, -242.4574432119242999 ) ) ;
#176581 =( BOUNDED_CURVE ( )  B_SPLINE_CURVE ( 3, ( #160994, #75381, #159709, #99694 ),
 .UNSPECIFIED., .F., .F. ) 
 B_SPLINE_CURVE_WITH_KNOTS ( ( 4, 4 ),
 ( 3.141592653589793116, 4.712388980384689674 ),
 .UNSPECIFIED. ) 
 CURVE ( )  GEOMETRIC_REPRESENTATION_ITEM ( )  RATIONAL_B_SPLINE_CURVE ( ( 1.000000000000000000, 0.8047378541243649375, 0.8047378541243649375, 1.000000000000000000 ) ) 
 REPRESENTATION_ITEM ( '' )  );
#176582 = CYLINDRICAL_SURFACE ( 'NONE', #240162, 0.09999999999999939493 ) ;
#176583 = CIRCLE ( 'NONE', #134838, 0.2000000000000057288 ) ;
#176584 = CARTESIAN_POINT ( 'NONE',  ( 18.50000000000000000, -9.499999999988842703, -21.75000000000000355 ) ) ;
#176585 = VERTEX_POINT ( 'NONE', #15943 ) ;
#176586 = AXIS2_PLACEMENT_3D ( 'NONE', #247433, #187488, #227878 ) ;
#176587 =( NAMED_UNIT ( * ) PLANE_ANGLE_UNIT ( ) SI_UNIT ( $, .RADIAN. ) );
#176588 = AXIS2_PLACEMENT_3D ( 'NONE', #77904, #55747, #195328 ) ;
#176589 = CYLINDRICAL_SURFACE ( 'NONE', #24853, 0.1000000000000028644 ) ;
#176590 = CIRCLE ( 'NONE', #22480, 0.09999999999999939493 ) ;
#176591 = PRODUCT_DEFINITION_SHAPE ( 'NONE', 'NONE',  #258137 ) ;
#176592 = EDGE_CURVE ( 'NONE', #196380, #991, #242357, .T. ) ;
#176593 = CARTESIAN_POINT ( 'NONE',  ( -16.94878442675512886, 66.00827089702130479, -157.4113270601623071 ) ) ;
#176594 = VERTEX_POINT ( 'NONE', #77160 ) ;
#176595 = CARTESIAN_POINT ( 'NONE',  ( 21.05000000000000071, 65.27628289530511552, -195.8581939154368285 ) ) ;
#176596 = DIRECTION ( 'NONE',  ( -1.000000000000000000, -0.000000000000000000, -0.000000000000000000 ) ) ;
#176597 =( BOUNDED_CURVE ( )  B_SPLINE_CURVE ( 3, ( #176524, #72282, #151833, #52691 ),
 .UNSPECIFIED., .F., .F. ) 
 B_SPLINE_CURVE_WITH_KNOTS ( ( 4, 4 ),
 ( 1.570796326794895448, 3.141592653589791784 ),
 .UNSPECIFIED. ) 
 CURVE ( )  GEOMETRIC_REPRESENTATION_ITEM ( )  RATIONAL_B_SPLINE_CURVE ( ( 1.000000000000000000, 0.8047378541243650485, 0.8047378541243650485, 1.000000000000000000 ) ) 
 REPRESENTATION_ITEM ( '' )  );
#176598 = ADVANCED_FACE ( 'NONE', ( #18481, #30680 ), #254489, .T. ) ;
#176599 = DIRECTION ( 'NONE',  ( 1.224646799147353207E-16, 1.000000000000000000, 0.000000000000000000 ) ) ;
#176601 = EDGE_LOOP ( 'NONE', ( #197258, #116828, #172591, #213434 ) ) ;
#176600 = DIRECTION ( 'NONE',  ( 0.7071067811865474617, -0.7071067811865474617, -5.142139384388980375E-15 ) ) ;
#176602 = CIRCLE ( 'NONE', #160043, 0.5999999999999992006 ) ;
#176604 = ORIENTED_EDGE ( 'NONE', *, *, #120612, .T. ) ;
#176603 = CARTESIAN_POINT ( 'NONE',  ( -18.37151313414566545, 85.57101412579110900, -96.20644457528561588 ) ) ;
#176606 = EDGE_CURVE ( 'NONE', #215723, #172220, #195857, .T. ) ;
#176605 = CARTESIAN_POINT ( 'NONE',  ( -20.54999999999999716, 1.115600667400684642E-11, -132.0000000000000284 ) ) ;
#176607 = PLANE ( 'NONE',  #33266 ) ;
#176608 = CARTESIAN_POINT ( 'NONE',  ( -18.40000000000000213, 8.822561741677553471, -42.75000000000000000 ) ) ;
#176609 = CYLINDRICAL_SURFACE ( 'NONE', #106922, 1.749999999999998002 ) ;
#176610 = AXIS2_PLACEMENT_3D ( 'NONE', #226213, #51437, #47598 ) ;
#176612 = CARTESIAN_POINT ( 'NONE',  ( -21.05000000000000071, 68.49522935589659767, -224.1230159437372436 ) ) ;
#176611 = CARTESIAN_POINT ( 'NONE',  ( -22.39999999999999858, 64.35000000001166143, -69.42310748452440805 ) ) ;
#176614 = EDGE_CURVE ( 'NONE', #243325, #61948, #197104, .T. ) ;
#176613 = CYLINDRICAL_SURFACE ( 'NONE', #249488, 0.09999999999999939493 ) ;
#176615 = DIRECTION ( 'NONE',  ( 1.000000000000000000, 0.000000000000000000, 0.000000000000000000 ) ) ;
#176616 = CARTESIAN_POINT ( 'NONE',  ( -18.43459694179556152, 85.49421012501045425, -163.4061022818634683 ) ) ;
#176617 = CARTESIAN_POINT ( 'NONE',  ( 20.94999999999999929, 1.115649653272650466E-11, -130.0000000000000284 ) ) ;
#176618 =( BOUNDED_SURFACE ( )  B_SPLINE_SURFACE ( 3, 2, ( 
 ( #35081, #93726, #175851 ),
 ( #257879, #36344, #194136 ),
 ( #54593, #79274, #115862 ),
 ( #158858, #14218, #18035 ) ),
 .UNSPECIFIED., .F., .F., .F. ) 
 B_SPLINE_SURFACE_WITH_KNOTS ( ( 4, 4 ),
 ( 3, 3 ),
 ( 0.0006461284895273902403, 0.0007503702773986316125 ),
 ( 0.000000000000000000, 1.000000000000000000 ),
 .UNSPECIFIED. ) 
 GEOMETRIC_REPRESENTATION_ITEM ( )  RATIONAL_B_SPLINE_SURFACE ( (
 ( 1.000000000000000000, 0.7071067811865475727, 1.000000000000000000),
 ( 1.000000000000000000, 0.7076476444648814867, 1.000000000000000000),
 ( 1.000000000000000000, 0.7075727925191590550, 1.000000000000000000),
 ( 1.000000000000000000, 0.7071067811865581199, 1.000000000000000000) ) ) 
 REPRESENTATION_ITEM ( '' )  SURFACE ( )  );
#176620 = ORIENTED_EDGE ( 'NONE', *, *, #72883, .F. ) ;
#176619 = AXIS2_PLACEMENT_3D ( 'NONE', #52362, #152804, #74562 ) ;
#176621 = EDGE_CURVE ( 'NONE', #239496, #169204, #217204, .T. ) ;
#176622 = DIRECTION ( 'NONE',  ( -1.000000000000000000, 0.000000000000000000, 0.000000000000000000 ) ) ;
#176623 = VECTOR ( 'NONE', #124427, 1000.000000000000227 ) ;
#176625 = ADVANCED_FACE ( 'NONE', ( #168926 ), #257039, .F. ) ;
#176624 = ADVANCED_FACE ( 'NONE', ( #117577 ), #188199, .F. ) ;
#176626 = ORIENTED_EDGE ( 'NONE', *, *, #175888, .T. ) ;
#176627 = ORIENTED_EDGE ( 'NONE', *, *, #145870, .T. ) ;
#176628 = CARTESIAN_POINT ( 'NONE',  ( -23.25000000000000000, -1.835859311432481045, -78.50443916879852679 ) ) ;
#176629 = SPHERICAL_SURFACE ( 'NONE', #73600, 0.1000000000000000056 ) ;
#176630 = VERTEX_POINT ( 'NONE', #159293 ) ;
#176631 = ORIENTED_EDGE ( 'NONE', *, *, #5272, .F. ) ;
#176632 = ORIENTED_EDGE ( 'NONE', *, *, #188036, .T. ) ;
#176634 = EDGE_CURVE ( 'NONE', #237868, #154400, #60157, .T. ) ;
#176633 = CIRCLE ( 'NONE', #55771, 0.1000000000000124678 ) ;
#176635 = TOROIDAL_SURFACE ( 'NONE', #22519, 0.4000000000000009104, 0.1000000000000000056 ) ;
#176636 = ADVANCED_FACE ( 'NONE', ( #139688 ), #163143, .T. ) ;
#176637 = ORIENTED_EDGE ( 'NONE', *, *, #149231, .T. ) ;
#176638 = LINE ( 'NONE', #140034, #113020 ) ;
#176639 = CARTESIAN_POINT ( 'NONE',  ( -21.93340585898930328, -5.963111948670274387E-16, 7.324147022125356621 ) ) ;
#176640 = CARTESIAN_POINT ( 'NONE',  ( 23.15000000000000213, 79.08634564045904369, -228.8189404293001132 ) ) ;
#176641 = CARTESIAN_POINT ( 'NONE',  ( -21.14999999999999858, 11.65000000001115232, -134.0000000000000000 ) ) ;
#176642 = DIRECTION ( 'NONE',  ( -1.000000000000000000, -0.000000000000000000, 0.000000000000000000 ) ) ;
#176643 = EDGE_CURVE ( 'NONE', #96043, #14463, #104768, .T. ) ;
#176644 = DIRECTION ( 'NONE',  ( 0.000000000000000000, -6.938893903907222067E-15, 1.000000000000000000 ) ) ;
#176645 = CARTESIAN_POINT ( 'NONE',  ( -23.25000000000000000, 76.00000000001126921, -203.5231074845248997 ) ) ;
#176647 = ORIENTED_EDGE ( 'NONE', *, *, #175708, .T. ) ;
#176646 = DIRECTION ( 'NONE',  ( 0.000000000000000000, -0.9770955615653381665, -0.2128009952263304749 ) ) ;
#176649 = CYLINDRICAL_SURFACE ( 'NONE', #154271, 0.09999999999999939493 ) ;
#176648 = CARTESIAN_POINT ( 'NONE',  ( 20.85000000000000142, 77.75000000001182343, -91.40415744590204383 ) ) ;
#176650 = DIRECTION ( 'NONE',  ( 1.000000000000000000, -0.000000000000000000, 0.000000000000000000 ) ) ;
#176651 = VERTEX_POINT ( 'NONE', #180135 ) ;
#176652 = DIRECTION ( 'NONE',  ( -1.000000000000000000, 2.952720810173289112E-16, 2.061873921506763405E-30 ) ) ;
#176653 = DIRECTION ( 'NONE',  ( 0.000000000000000000, 0.8814952561688407240, -0.4721928772777390093 ) ) ;
#176654 = ORIENTED_EDGE ( 'NONE', *, *, #29598, .F. ) ;
#176655 = EDGE_CURVE ( 'NONE', #242065, #239290, #134018, .T. ) ;
#176657 = DIRECTION ( 'NONE',  ( -0.000000000000000000, 0.1350103645451835865, 0.9908441862701605762 ) ) ;
#176656 = CARTESIAN_POINT ( 'NONE',  ( 20.94999999999999574, 79.03126467873600802, -235.8703919547671717 ) ) ;
#176658 = EDGE_CURVE ( 'NONE', #6487, #197879, #1472, .T. ) ;
#176659 = CARTESIAN_POINT ( 'NONE',  ( -21.05000000000000071, -11.29603075033528548, -3.047899159663867152 ) ) ;
#176660 = ORIENTED_EDGE ( 'NONE', *, *, #224420, .F. ) ;
#176661 = ORIENTED_EDGE ( 'NONE', *, *, #248556, .T. ) ;
#176662 = AXIS2_PLACEMENT_3D ( 'NONE', #108121, #226773, #187676 ) ;
#176663 = CARTESIAN_POINT ( 'NONE',  ( 21.05000000000000071, 70.60000000001178933, -79.41707660717679573 ) ) ;
#176664 = CARTESIAN_POINT ( 'NONE',  ( 23.14999999999999503, 6.550000000011156231, -79.35000000000005116 ) ) ;
#176665 = DIRECTION ( 'NONE',  ( 0.000000000000000000, 0.000000000000000000, -1.000000000000000000 ) ) ;
#176667 = EDGE_CURVE ( 'NONE', #116965, #160646, #84833, .T. ) ;
#176666 = CARTESIAN_POINT ( 'NONE',  ( 17.74533788810830259, 10.81849979148194940, -144.3136226749475952 ) ) ;
#176668 = ORIENTED_EDGE ( 'NONE', *, *, #227153, .T. ) ;
#176669 = CARTESIAN_POINT ( 'NONE',  ( 18.59999999999999076, 6.982009704856455556, -37.19615211825629331 ) ) ;
#176670 = ADVANCED_FACE ( 'NONE', ( #120190 ), #62747, .T. ) ;
#176671 = DIRECTION ( 'NONE',  ( 1.000000000000000000, -0.000000000000000000, 0.000000000000000000 ) ) ;
#176672 = B_SPLINE_CURVE_WITH_KNOTS ( 'NONE', 3,
 ( #103667, #244484, #144085, #222327, #80240, #241911, #240636, #159837, #101071, #119419 ),
 .UNSPECIFIED., .F., .F.,
 ( 4, 3, 3, 4 ),
 ( 1.301042606982605321E-18, 0.0002000000000008467444, 0.001000000000082971845, 0.001967863649483304195 ),
 .UNSPECIFIED. ) ;
#176673 = AXIS2_PLACEMENT_3D ( 'NONE', #49788, #172362, #94047 ) ;
#176674 = CARTESIAN_POINT ( 'NONE',  ( -20.54999999999999716, 1.148907358139439339E-11, -201.0000000000015064 ) ) ;
#176675 = AXIS2_PLACEMENT_3D ( 'NONE', #42658, #20558, #122208 ) ;
#176676 = DIRECTION ( 'NONE',  ( -1.000000000000000000, 0.000000000000000000, 0.000000000000000000 ) ) ;
#176677 = AXIS2_PLACEMENT_3D ( 'NONE', #230831, #131708, #211245 ) ;
#176678 = VECTOR ( 'NONE', #173106, 1000.000000000000000 ) ;
#176680 = ORIENTED_EDGE ( 'NONE', *, *, #33820, .F. ) ;
#176679 = LINE ( 'NONE', #240483, #46269 ) ;
#176681 = FACE_OUTER_BOUND ( 'NONE', #148771, .T. ) ;
#176682 = DIRECTION ( 'NONE',  ( 1.000000000000000000, 0.000000000000000000, 0.000000000000000000 ) ) ;
#176683 = FACE_OUTER_BOUND ( 'NONE', #212485, .T. ) ;
#176684 = DIRECTION ( 'NONE',  ( 0.000000000000000000, 0.000000000000000000, -1.000000000000000000 ) ) ;
#176685 = EDGE_CURVE ( 'NONE', #47050, #163993, #225578, .T. ) ;
#176686 = CARTESIAN_POINT ( 'NONE',  ( 22.39999999999999503, 1.115600667400684642E-11, -126.2500000000000284 ) ) ;
#176688 = EDGE_LOOP ( 'NONE', ( #96083, #99622, #178400 ) ) ;
#176687 = DIRECTION ( 'NONE',  ( 1.000000000000000000, 0.000000000000000000, 0.000000000000000000 ) ) ;
#176689 = CARTESIAN_POINT ( 'NONE',  ( -23.25000000000000000, 10.33248238083634440, -106.0948465439131922 ) ) ;
#176690 = CARTESIAN_POINT ( 'NONE',  ( 20.94983749550516450, 67.49429988484537546, -195.5441618131978601 ) ) ;
#176691 = ORIENTED_EDGE ( 'NONE', *, *, #232815, .F. ) ;
#176692 = CARTESIAN_POINT ( 'NONE',  ( -21.05000000000000071, 1.162701749949165642, -74.90000000000004832 ) ) ;
#176693 = CARTESIAN_POINT ( 'NONE',  ( -26.01805557925458956, 8.624264858734566275, 33.00000000000000000 ) ) ;
#176694 = CYLINDRICAL_SURFACE ( 'NONE', #225372, 0.1000000000000028644 ) ;
#176695 = B_SPLINE_CURVE_WITH_KNOTS ( 'NONE', 3,
 ( #106673, #204498, #85809, #166705, #64994, #165394 ),
 .UNSPECIFIED., .F., .F.,
 ( 4, 2, 4 ),
 ( 0.000000000000000000, 0.0001496588209255828787, 0.0002993176418511657574 ),
 .UNSPECIFIED. ) ;
#176696 = AXIS2_PLACEMENT_3D ( 'NONE', #113579, #133146, #216526 ) ;
#176697 = CARTESIAN_POINT ( 'NONE',  ( -18.52186455169006152, 78.22055546782374336, -231.5567229729791165 ) ) ;
#176698 = DIRECTION ( 'NONE',  ( 0.000000000000000000, -6.982962677686266711E-15, 1.000000000000000000 ) ) ;
#176700 = ORIENTED_EDGE ( 'NONE', *, *, #177141, .F. ) ;
#176699 = AXIS2_PLACEMENT_3D ( 'NONE', #92755, #155346, #234856 ) ;
#176701 = ORIENTED_EDGE ( 'NONE', *, *, #129655, .T. ) ;
#176702 = AXIS2_PLACEMENT_3D ( 'NONE', #105264, #68756, #86995 ) ;
#176703 = CARTESIAN_POINT ( 'NONE',  ( 21.05000000000000071, 1.115600667400684642E-11, -134.0000000000000284 ) ) ;
#176704 = CARTESIAN_POINT ( 'NONE',  ( -23.15000000000000213, 71.65000000001253966, -182.3731074845244109 ) ) ;
#176705 = DIRECTION ( 'NONE',  ( -1.000000000000000000, 0.000000000000000000, 0.000000000000000000 ) ) ;
#176706 = DIRECTION ( 'NONE',  ( 1.000000000000000000, -0.000000000000000000, -0.000000000000000000 ) ) ;
#176707 = ORIENTED_EDGE ( 'NONE', *, *, #68793, .F. ) ;
#176708 = CARTESIAN_POINT ( 'NONE',  ( -23.25000000000000000, 78.00142589229885459, -228.9845759368473637 ) ) ;
#176709 = AXIS2_PLACEMENT_3D ( 'NONE', #119200, #63056, #121779 ) ;
#176710 = AXIS2_PLACEMENT_3D ( 'NONE', #81445, #197561, #217108 ) ;
#176711 = CARTESIAN_POINT ( 'NONE',  ( 20.21494484322213125, 10.86490356972843152, -207.1695121093801504 ) ) ;
#176712 = VECTOR ( 'NONE', #219706, 1000.000000000000114 ) ;
#176713 = CARTESIAN_POINT ( 'NONE',  ( 18.49999999999998934, 53.37395138337728895, -234.8857996415767104 ) ) ;
#176714 = AXIS2_PLACEMENT_3D ( 'NONE', #18669, #173947, #196035 ) ;
#176715 = FACE_OUTER_BOUND ( 'NONE', #38503, .T. ) ;
#176716 = VERTEX_POINT ( 'NONE', #79713 ) ;
#176717 = DIRECTION ( 'NONE',  ( -0.000000000000000000, 1.000000000000000000, 6.352154140967427193E-15 ) ) ;
#176718 = AXIS2_PLACEMENT_3D ( 'NONE', #118448, #76727, #235802 ) ;
#176719 = ORIENTED_EDGE ( 'NONE', *, *, #227022, .T. ) ;
#176720 = ORIENTED_EDGE ( 'NONE', *, *, #12428, .F. ) ;
#176721 = CARTESIAN_POINT ( 'NONE',  ( -21.05000000000000071, -0.02110330804785487402, -27.19548367073597461 ) ) ;
#176722 = CARTESIAN_POINT ( 'NONE',  ( -18.59999999999999787, 70.65875701002079268, -179.8297576910124178 ) ) ;
#176723 = FACE_OUTER_BOUND ( 'NONE', #217310, .T. ) ;
#176724 = ORIENTED_EDGE ( 'NONE', *, *, #90568, .T. ) ;
#176726 = VECTOR ( 'NONE', #252477, 1000.000000000000000 ) ;
#176725 = DIRECTION ( 'NONE',  ( -1.000000000000000000, 0.000000000000000000, 0.000000000000000000 ) ) ;
#176727 = FACE_OUTER_BOUND ( 'NONE', #30794, .T. ) ;
#176728 = DIRECTION ( 'NONE',  ( 0.000000000000000000, 0.000000000000000000, 1.000000000000000000 ) ) ;
#176729 = CIRCLE ( 'NONE', #172666, 0.09999999999999939493 ) ;
#176730 = VERTEX_POINT ( 'NONE', #23652 ) ;
#176732 = DIRECTION ( 'NONE',  ( -1.000000000000000000, -0.000000000000000000, 0.000000000000000000 ) ) ;
#176731 = AXIS2_PLACEMENT_3D ( 'NONE', #165154, #67328, #66040 ) ;
#176734 = ORIENTED_EDGE ( 'NONE', *, *, #92283, .T. ) ;
#176733 = CARTESIAN_POINT ( 'NONE',  ( 18.56308993302918964, 65.61930884468851843, -145.2838848455861580 ) ) ;
#176735 = EDGE_CURVE ( 'NONE', #230941, #163525, #5772, .T. ) ;
#176736 = DIRECTION ( 'NONE',  ( 0.000000000000000000, 0.7116622890665382783, 0.7025217336998015316 ) ) ;
#176737 = DIRECTION ( 'NONE',  ( 0.000000000000000000, 3.552713678800499352E-15, -1.000000000000000000 ) ) ;
#176738 = ORIENTED_EDGE ( 'NONE', *, *, #172978, .T. ) ;
#176739 = CARTESIAN_POINT ( 'NONE',  ( -16.77732147278574715, 9.945966932584587639, -79.66350875687584221 ) ) ;
#176740 = CARTESIAN_POINT ( 'NONE',  ( -18.59999999999999787, 66.65000000001187175, -90.77310748452437394 ) ) ;
#176741 = CARTESIAN_POINT ( 'NONE',  ( 21.14999999999999858, 1.627786319807486892, -244.0021210468063089 ) ) ;
#176742 = ORIENTED_EDGE ( 'NONE', *, *, #253422, .F. ) ;
#176743 = CARTESIAN_POINT ( 'NONE',  ( 21.07928932188134397, 6.328516656404459262, -133.9011048543456184 ) ) ;
#176744 = ADVANCED_FACE ( 'NONE', ( #188 ), #4045, .F. ) ;
#176745 = DIRECTION ( 'NONE',  ( -1.000000000000000000, 0.000000000000000000, 0.000000000000000000 ) ) ;
#176746 = DIRECTION ( 'NONE',  ( 1.000000000000000000, 2.683427030341257327E-17, -8.429776912874271752E-16 ) ) ;
#176747 = EDGE_CURVE ( 'NONE', #223317, #6603, #54903, .T. ) ;
#176748 = AXIS2_PLACEMENT_3D ( 'NONE', #36814, #233707, #74664 ) ;
#176749 = ORIENTED_EDGE ( 'NONE', *, *, #86801, .T. ) ;
#176750 = CIRCLE ( 'NONE', #89235, 0.09999999999998898659 ) ;
#176751 = VERTEX_POINT ( 'NONE', #241393 ) ;
#176752 = AXIS2_PLACEMENT_3D ( 'NONE', #50707, #155961, #91148 ) ;
#176753 = ADVANCED_FACE ( 'NONE', ( #221783 ), #142398, .F. ) ;
#176754 = AXIS2_PLACEMENT_3D ( 'NONE', #195223, #98612, #96071 ) ;
#176755 = ORIENTED_EDGE ( 'NONE', *, *, #217476, .F. ) ;
#176756 = EDGE_CURVE ( 'NONE', #189704, #140720, #42436, .T. ) ;
#176757 = PLANE ( 'NONE',  #60161 ) ;
#176758 = CARTESIAN_POINT ( 'NONE',  ( -18.34374000495059676, 64.52683809665003878, -179.2731074845244450 ) ) ;
#176760 = VERTEX_POINT ( 'NONE', #187847 ) ;
#176759 = CARTESIAN_POINT ( 'NONE',  ( 18.59999999999999076, 10.49142135624846439, -158.7500000000000284 ) ) ;
#176761 = PLANE ( 'NONE',  #57485 ) ;
#176763 = AXIS2_PLACEMENT_3D ( 'NONE', #228677, #109982, #13471 ) ;
#176762 = DIRECTION ( 'NONE',  ( 1.000000000000000000, 0.000000000000000000, 0.000000000000000000 ) ) ;
#176764 = EDGE_CURVE ( 'NONE', #224755, #114130, #206105, .T. ) ;
#176765 = CARTESIAN_POINT ( 'NONE',  ( -22.59066674512270012, 11.47438154053713966, -198.4697828622833811 ) ) ;
#176766 = CARTESIAN_POINT ( 'NONE',  ( -18.47690164073607377, 85.46484453802391101, -62.82172654468813278 ) ) ;
#176767 = DIRECTION ( 'NONE',  ( 1.000000000000000000, 0.000000000000000000, 0.000000000000000000 ) ) ;
#176768 = TOROIDAL_SURFACE ( 'NONE', #201693, 0.2000000000000000111, 0.1000000000000000056 ) ;
#176769 = CARTESIAN_POINT ( 'NONE',  ( -21.14999999999999858, 64.35000000001238618, -170.0231074845244166 ) ) ;
#176770 = AXIS2_PLACEMENT_3D ( 'NONE', #157493, #83012, #179606 ) ;
#176771 = VERTEX_POINT ( 'NONE', #6613 ) ;
#176773 = EDGE_LOOP ( 'NONE', ( #105052, #92811, #141073, #111762 ) ) ;
#176772 = CARTESIAN_POINT ( 'NONE',  ( 23.25000000000000000, -13.98128454229088291, -192.0195388455185821 ) ) ;
#176775 = DIRECTION ( 'NONE',  ( 0.000000000000000000, 0.000000000000000000, 1.000000000000000000 ) ) ;
#176774 = DIRECTION ( 'NONE',  ( -0.5932847527679298016, -0.8049926720990051576, -5.621233785078291429E-15 ) ) ;
#176776 = ADVANCED_FACE ( 'NONE', ( #91300 ), #254772, .T. ) ;
#176777 = TOROIDAL_SURFACE ( 'NONE', #255821, 2.699999999999999734, 0.1000000000000000056 ) ;
#176779 = VERTEX_POINT ( 'NONE', #209970 ) ;
#176778 = LINE ( 'NONE', #22730, #96898 ) ;
#176780 = ORIENTED_EDGE ( 'NONE', *, *, #251161, .F. ) ;
#176781 = CARTESIAN_POINT ( 'NONE',  ( -21.14999999999999858, -1.391858308744747807, -194.6091531227727955 ) ) ;
#176782 = CARTESIAN_POINT ( 'NONE',  ( -20.94999999999999929, 74.16465844978765176, -124.9679561919613207 ) ) ;
#176783 = EDGE_CURVE ( 'NONE', #240530, #221551, #146124, .T. ) ;
#176784 = CYLINDRICAL_SURFACE ( 'NONE', #67713, 0.09999999999998898659 ) ;
#176785 = PLANE ( 'NONE',  #169278 ) ;
#176786 = DIRECTION ( 'NONE',  ( -1.000000000000000000, 0.000000000000000000, 0.000000000000000000 ) ) ;
#176787 = AXIS2_PLACEMENT_3D ( 'NONE', #126655, #48393, #207498 ) ;
#176788 = CYLINDRICAL_SURFACE ( 'NONE', #182226, 0.09999999999999939493 ) ;
#176789 = EDGE_CURVE ( 'NONE', #122058, #206647, #125290, .T. ) ;
#176790 = CARTESIAN_POINT ( 'NONE',  ( -20.64999999999999858, 1.115625160336667635E-11, -202.9999999999999716 ) ) ;
#176791 = CIRCLE ( 'NONE', #22861, 0.1000000000000052097 ) ;
#176792 = VERTEX_POINT ( 'NONE', #190415 ) ;
#176793 = ORIENTED_EDGE ( 'NONE', *, *, #179608, .F. ) ;
#176794 = CYLINDRICAL_SURFACE ( 'NONE', #144045, 0.09999999999998898659 ) ;
#176795 = ORIENTED_EDGE ( 'NONE', *, *, #87811, .F. ) ;
#176796 = DIRECTION ( 'NONE',  ( 0.000000000000000000, -0.000000000000000000, -1.000000000000000000 ) ) ;
#176798 = AXIS2_PLACEMENT_3D ( 'NONE', #79358, #80635, #160228 ) ;
#176797 = DIRECTION ( 'NONE',  ( 2.694716079187273439E-16, 1.000000000000000000, 6.467318590049456648E-15 ) ) ;
#176799 = AXIS2_PLACEMENT_3D ( 'NONE', #41547, #87033, #204427 ) ;
#176800 = DIRECTION ( 'NONE',  ( 0.000000000000000000, 0.000000000000000000, -1.000000000000000000 ) ) ;
#176801 = AXIS2_PLACEMENT_3D ( 'NONE', #210385, #227364, #250778 ) ;
#176802 = CARTESIAN_POINT ( 'NONE',  ( -18.59999999999999787, 77.16412189325305349, -95.10825939895268277 ) ) ;
#176803 = VERTEX_POINT ( 'NONE', #49599 ) ;
#176804 = CARTESIAN_POINT ( 'NONE',  ( -15.15564720441981095, 66.58929125296495499, -118.4538990786802799 ) ) ;
#176805 = ORIENTED_EDGE ( 'NONE', *, *, #247632, .F. ) ;
#176806 = SPHERICAL_SURFACE ( 'NONE', #233753, 0.1000000000000000056 ) ;
#176807 = ORIENTED_EDGE ( 'NONE', *, *, #251298, .T. ) ;
#176808 = CARTESIAN_POINT ( 'NONE',  ( -20.85000000000000142, 67.23127455305835554, -235.8551265064784559 ) ) ;
#176809 = CARTESIAN_POINT ( 'NONE',  ( -17.11825945287481332, 65.95000000001181206, -82.27310748452437394 ) ) ;
#176810 = CARTESIAN_POINT ( 'NONE',  ( 23.25000000000000000, -9.600000000000003197, -9.893969122652443104 ) ) ;
#176811 = EDGE_LOOP ( 'NONE', ( #172623, #124765, #222712, #7155 ) ) ;
#176812 = FACE_OUTER_BOUND ( 'NONE', #150437, .T. ) ;
#176814 = ORIENTED_EDGE ( 'NONE', *, *, #6391, .F. ) ;
#176813 = CARTESIAN_POINT ( 'NONE',  ( 20.94999999999999929, 76.00000000001145395, -40.12310748452431852 ) ) ;
#176815 = FACE_OUTER_BOUND ( 'NONE', #21915, .T. ) ;
#176816 = CIRCLE ( 'NONE', #110156, 11.80000000000000426 ) ;
#176817 = ORIENTED_EDGE ( 'NONE', *, *, #4404, .T. ) ;
#176818 = EDGE_CURVE ( 'NONE', #33783, #15704, #117288, .T. ) ;
#176819 = VECTOR ( 'NONE', #27592, 1000.000000000000000 ) ;
#176820 = DIRECTION ( 'NONE',  ( 0.000000000000000000, 0.9274965247785529332, 0.3738317757009255171 ) ) ;
#176821 = ORIENTED_EDGE ( 'NONE', *, *, #242167, .F. ) ;
#176822 = CARTESIAN_POINT ( 'NONE',  ( 22.39999999999999858, 10.71943444926881561, -226.8179467668883547 ) ) ;
#176823 = ADVANCED_FACE ( 'NONE', ( #105687 ), #38191, .T. ) ;
#176824 = CARTESIAN_POINT ( 'NONE',  ( 22.47110162079220785, 64.15407550225560840, -247.0913484080595026 ) ) ;
#176825 = ADVANCED_FACE ( 'NONE', ( #169596 ), #249102, .F. ) ;
#176826 = CARTESIAN_POINT ( 'NONE',  ( -20.94999999999999929, 68.48451787451661232, -224.2224406095231757 ) ) ;
#176827 = DIRECTION ( 'NONE',  ( 0.000000000000000000, -6.982962677686266711E-15, 1.000000000000000000 ) ) ;
#176828 = DIRECTION ( 'NONE',  ( 1.000000000000000000, 0.000000000000000000, 0.000000000000000000 ) ) ;
#176830 = ORIENTED_EDGE ( 'NONE', *, *, #54816, .F. ) ;
#176829 = ADVANCED_FACE ( 'NONE', ( #70486 ), #165717, .F. ) ;
#176831 = EDGE_CURVE ( 'NONE', #2697, #120409, #204928, .T. ) ;
#176832 = LINE ( 'NONE', #236771, #106902 ) ;
#176833 = CARTESIAN_POINT ( 'NONE',  ( -28.12018973533754362, 11.62642356364895413, 33.00000000000000000 ) ) ;
#176834 = DIRECTION ( 'NONE',  ( 0.000000000000000000, -0.000000000000000000, -1.000000000000000000 ) ) ;
#176835 = ADVANCED_FACE ( 'NONE', ( #7921 ), #253457, .T. ) ;
#176836 = VERTEX_POINT ( 'NONE', #69190 ) ;
#176837 = CARTESIAN_POINT ( 'NONE',  ( -12.25000000000000178, 9.349999999999983658, -16.75000000000000000 ) ) ;
#176839 = EDGE_CURVE ( 'NONE', #143032, #71381, #228248, .T. ) ;
#176838 = ORIENTED_EDGE ( 'NONE', *, *, #6940, .T. ) ;
#176840 = LINE ( 'NONE', #180678, #239780 ) ;
#176841 = ORIENTED_EDGE ( 'NONE', *, *, #175854, .T. ) ;
#176842 = AXIS2_PLACEMENT_3D ( 'NONE', #256232, #77647, #135055 ) ;
#176843 = TOROIDAL_SURFACE ( 'NONE', #210158, 0.2000000000000000111, 0.1000000000000000056 ) ;
#176844 = CARTESIAN_POINT ( 'NONE',  ( 23.24999999999999289, 12.76524917372336887, -223.4223513401831269 ) ) ;
#176845 = CARTESIAN_POINT ( 'NONE',  ( 21.14999999999999858, 87.75000000001259082, -191.2731074845242745 ) ) ;
#176846 = EDGE_CURVE ( 'NONE', #182323, #235498, #104941, .T. ) ;
#176848 = ORIENTED_EDGE ( 'NONE', *, *, #98695, .F. ) ;
#176847 = LINE ( 'NONE', #58132, #48776 ) ;
#176849 = CARTESIAN_POINT ( 'NONE',  ( -17.71734398241073549, 10.84235722847571637, -123.7251382530056105 ) ) ;
#176850 = ORIENTED_EDGE ( 'NONE', *, *, #91159, .F. ) ;
#176851 = DIRECTION ( 'NONE',  ( 0.000000000000000000, 0.000000000000000000, -1.000000000000000000 ) ) ;
#176852 = CARTESIAN_POINT ( 'NONE',  ( -21.65000000000000213, 68.75000000001188027, -90.37310748452435405 ) ) ;
#176853 = ORIENTED_EDGE ( 'NONE', *, *, #146274, .T. ) ;
#176854 = VERTEX_POINT ( 'NONE', #174734 ) ;
#176855 = DIRECTION ( 'NONE',  ( -1.000000000000000000, 2.775557561562908012E-13, 5.551115123125816024E-13 ) ) ;
#176856 = CARTESIAN_POINT ( 'NONE',  ( 20.95224633520496127, 67.09947783345465666, -94.52983103660311315 ) ) ;
#176857 = ORIENTED_EDGE ( 'NONE', *, *, #96078, .F. ) ;
#176859 = CARTESIAN_POINT ( 'NONE',  ( -18.59999999999999787, 13.65786464920749843, -219.7735913778983559 ) ) ;
#176858 = CIRCLE ( 'NONE', #22740, 0.5999999999999894307 ) ;
#176860 = AXIS2_PLACEMENT_3D ( 'NONE', #254920, #215835, #76324 ) ;
#176861 = VERTEX_POINT ( 'NONE', #97680 ) ;
#176862 = VERTEX_POINT ( 'NONE', #194274 ) ;
#176863 = AXIS2_PLACEMENT_3D ( 'NONE', #60830, #196495, #137796 ) ;
#176864 = CIRCLE ( 'NONE', #180945, 1.999999999999997335 ) ;
#176865 = ADVANCED_FACE ( 'NONE', ( #114706 ), #96407, .F. ) ;
#176866 = CARTESIAN_POINT ( 'NONE',  ( -17.04295772865458858, 65.97510057475003009, -48.67310748452439384 ) ) ;
#176867 = LINE ( 'NONE', #256307, #76442 ) ;
#176868 =( GEOMETRIC_REPRESENTATION_CONTEXT ( 3 ) GLOBAL_UNCERTAINTY_ASSIGNED_CONTEXT ( ( #172939 ) ) GLOBAL_UNIT_ASSIGNED_CONTEXT ( ( #26815, #153191, #233966 ) ) REPRESENTATION_CONTEXT ( 'NONE', 'WORKASPACE' ) );
#176869 = EDGE_CURVE ( 'NONE', #12754, #246027, #238252, .T. ) ;
#176870 = EDGE_CURVE ( 'NONE', #10632, #22319, #34290, .T. ) ;
#176872 = ORIENTED_EDGE ( 'NONE', *, *, #231915, .T. ) ;
#176871 = CARTESIAN_POINT ( 'NONE',  ( 21.14999999999999858, 64.35000000001186038, -90.87310748452438247 ) ) ;
#176873 = DIRECTION ( 'NONE',  ( 0.000000000000000000, -0.6728971962616412394, -0.7397360091703134577 ) ) ;
#176874 = LINE ( 'NONE', #257604, #144091 ) ;
#176875 = CARTESIAN_POINT ( 'NONE',  ( 20.94999999999999574, 18.81166555858608902, -229.8642012822692777 ) ) ;
#176877 = CARTESIAN_POINT ( 'NONE',  ( -22.49072729836729678, 75.94351806727883059, -181.6731157336792819 ) ) ;
#176876 = DIRECTION ( 'NONE',  ( 1.000000000000000000, 0.000000000000000000, 0.000000000000000000 ) ) ;
#176878 = LINE ( 'NONE', #116880, #182112 ) ;
#176879 = CARTESIAN_POINT ( 'NONE',  ( 21.05000000000000071, 6.650000000011155876, -79.15000000000004832 ) ) ;
#176880 = DIRECTION ( 'NONE',  ( 0.000000000000000000, 0.9908441862701596881, 0.1350103645451904977 ) ) ;
#176881 = TOROIDAL_SURFACE ( 'NONE', #218522, 11.65000000000000036, 0.1000000000000000056 ) ;
#176882 = FACE_OUTER_BOUND ( 'NONE', #77404, .T. ) ;
#176883 = AXIS2_PLACEMENT_3D ( 'NONE', #75, #44365, #118768 ) ;
#176884 = VERTEX_POINT ( 'NONE', #112164 ) ;
#176885 = ORIENTED_EDGE ( 'NONE', *, *, #67547, .F. ) ;
#176886 = CIRCLE ( 'NONE', #64448, 12.87499999999999822 ) ;
#176887 = DIRECTION ( 'NONE',  ( -1.000000000000000000, -0.000000000000000000, 0.000000000000000000 ) ) ;
#176888 = AXIS2_PLACEMENT_3D ( 'NONE', #242437, #63821, #143345 ) ;
#176890 = ORIENTED_EDGE ( 'NONE', *, *, #123252, .T. ) ;
#176889 = DIRECTION ( 'NONE',  ( -0.000000000000000000, 6.982962677686266711E-15, -1.000000000000000000 ) ) ;
#176891 = VERTEX_POINT ( 'NONE', #136828 ) ;
#176892 = CARTESIAN_POINT ( 'NONE',  ( -18.59999999999999787, 69.06610602788535402, -65.73746165015079157 ) ) ;
#176893 = ORIENTED_EDGE ( 'NONE', *, *, #42483, .T. ) ;
#176894 = CARTESIAN_POINT ( 'NONE',  ( 21.72449340488910252, 65.71604372252073745, -90.37310748452436826 ) ) ;
#176895 = CIRCLE ( 'NONE', #239418, 0.1000000000000028644 ) ;
#176896 = CIRCLE ( 'NONE', #110232, 0.1000000000000028644 ) ;
#176897 = VERTEX_POINT ( 'NONE', #191711 ) ;
#176898 = AXIS2_PLACEMENT_3D ( 'NONE', #71919, #206280, #130581 ) ;
#176899 = DIRECTION ( 'NONE',  ( 1.000000000000000000, 0.000000000000000000, -0.000000000000000000 ) ) ;
#176900 = CIRCLE ( 'NONE', #93476, 12.87499999999999822 ) ;
#176902 = ORIENTED_EDGE ( 'NONE', *, *, #121254, .F. ) ;
#176901 = ORIENTED_EDGE ( 'NONE', *, *, #34634, .T. ) ;
#176903 = VERTEX_POINT ( 'NONE', #131702 ) ;
#176904 = EDGE_LOOP ( 'NONE', ( #223481, #169152, #119909, #163134 ) ) ;
#176905 = ORIENTED_EDGE ( 'NONE', *, *, #61213, .T. ) ;
#176907 = DIRECTION ( 'NONE',  ( 1.000000000000000000, 0.000000000000000000, 0.000000000000000000 ) ) ;
#176906 = CIRCLE ( 'NONE', #193645, 0.09999999999999939493 ) ;
#176908 = LINE ( 'NONE', #197721, #13567 ) ;
#176910 = ORIENTED_EDGE ( 'NONE', *, *, #99719, .T. ) ;
#176909 = DIRECTION ( 'NONE',  ( -1.000000000000000000, 0.000000000000000000, 0.000000000000000000 ) ) ;
#176911 = CIRCLE ( 'NONE', #135362, 0.09999999999998898659 ) ;
#176912 = CARTESIAN_POINT ( 'NONE',  ( 20.94999999999999929, 8.776282895303628706, -75.55862899514100661 ) ) ;
#176913 = CARTESIAN_POINT ( 'NONE',  ( 12.60053434924909688, 12.51008756600233340, -214.3176843001242275 ) ) ;
#176915 = ORIENTED_EDGE ( 'NONE', *, *, #226144, .F. ) ;
#176914 = DIRECTION ( 'NONE',  ( 0.000000000000000000, 0.000000000000000000, 1.000000000000000000 ) ) ;
#176916 = DIRECTION ( 'NONE',  ( 0.000000000000000000, 0.1568667991644863147, 0.9876197685951252359 ) ) ;
#176917 = ORIENTED_EDGE ( 'NONE', *, *, #210933, .F. ) ;
#176918 = AXIS2_PLACEMENT_3D ( 'NONE', #134467, #57499, #233603 ) ;
#176919 = CARTESIAN_POINT ( 'NONE',  ( 21.05000000000000071, -11.64999999998883595, -64.00000000000000000 ) ) ;
#176920 = AXIS2_PLACEMENT_3D ( 'NONE', #170407, #110367, #244733 ) ;
#176922 = ORIENTED_EDGE ( 'NONE', *, *, #137301, .F. ) ;
#176921 = LINE ( 'NONE', #80320, #51881 ) ;
#176923 = CARTESIAN_POINT ( 'NONE',  ( 23.15000000000000213, -8.999999999988842703, -157.6060308773475640 ) ) ;
#176925 = EDGE_CURVE ( 'NONE', #246004, #228778, #142563, .T. ) ;
#176924 = DIRECTION ( 'NONE',  ( -1.000000000000000000, -1.541880601228652843E-16, -2.878400969107353907E-16 ) ) ;
#176926 = CARTESIAN_POINT ( 'NONE',  ( -23.15000000000000213, 64.25000000001158185, -57.37310748452440379 ) ) ;
#176927 = VERTEX_POINT ( 'NONE', #15642 ) ;
#176929 = DIRECTION ( 'NONE',  ( 0.000000000000000000, -0.01283462868041947667, -0.9999176327611367654 ) ) ;
#176928 = CARTESIAN_POINT ( 'NONE',  ( -16.87401514999235275, 9.950000000011137047, -46.21998200746781293 ) ) ;
#176930 = EDGE_CURVE ( 'NONE', #82405, #58814, #76787, .T. ) ;
#176931 = CARTESIAN_POINT ( 'NONE',  ( 21.95218792049437795, 7.201507561257818324, -133.9009715602001052 ) ) ;
#176932 = DIRECTION ( 'NONE',  ( 1.000000000000000000, 0.000000000000000000, 0.000000000000000000 ) ) ;
#176933 = CARTESIAN_POINT ( 'NONE',  ( 21.05000000000000071, 74.16465844978745281, -91.46795619196133487 ) ) ;
#176934 = ORIENTED_EDGE ( 'NONE', *, *, #162221, .F. ) ;
#176935 = ORIENTED_EDGE ( 'NONE', *, *, #54911, .T. ) ;
#176936 = ORIENTED_EDGE ( 'NONE', *, *, #138214, .F. ) ;
#176937 = EDGE_CURVE ( 'NONE', #110864, #193738, #234157, .T. ) ;
#176938 = DIRECTION ( 'NONE',  ( 1.000000000000000000, 0.000000000000000000, 0.000000000000000000 ) ) ;
#176940 = EDGE_CURVE ( 'NONE', #247867, #172688, #5186, .T. ) ;
#176939 = FACE_OUTER_BOUND ( 'NONE', #254420, .T. ) ;
#176941 = VERTEX_POINT ( 'NONE', #92560 ) ;
#176942 = DIRECTION ( 'NONE',  ( 0.000000000000000000, -0.9126074666063622720, -0.4088369013363611360 ) ) ;
#176943 = VERTEX_POINT ( 'NONE', #117281 ) ;
#176944 = DIRECTION ( 'NONE',  ( -1.000000000000000000, 0.000000000000000000, -0.000000000000000000 ) ) ;
#176945 = DIRECTION ( 'NONE',  ( 0.000000000000000000, 0.8814952561688428334, -0.4721928772777350125 ) ) ;
#176946 = VECTOR ( 'NONE', #220365, 1000.000000000000227 ) ;
#176947 = AXIS2_PLACEMENT_3D ( 'NONE', #156301, #18033, #98816 ) ;
#176948 = EDGE_LOOP ( 'NONE', ( #183285, #187056, #234620, #102822 ) ) ;
#176949 = CYLINDRICAL_SURFACE ( 'NONE', #98353, 0.09999999999999939493 ) ;
#176950 = FILL_AREA_STYLE ('',( #137772 ) ) ;
#176951 = VECTOR ( 'NONE', #241558, 1000.000000000000000 ) ;
#176952 = ORIENTED_EDGE ( 'NONE', *, *, #115538, .F. ) ;
#176953 = ADVANCED_FACE ( 'NONE', ( #172159 ), #251649, .F. ) ;
#176954 = ORIENTED_EDGE ( 'NONE', *, *, #125220, .F. ) ;
#176955 = EDGE_CURVE ( 'NONE', #112934, #251883, #138286, .T. ) ;
#176956 = EDGE_LOOP ( 'NONE', ( #60514, #104575 ) ) ;
#176957 = AXIS2_PLACEMENT_3D ( 'NONE', #55203, #115213, #70984 ) ;
#176958 = CARTESIAN_POINT ( 'NONE',  ( -22.94999999999999929, 4.611773100472912112, 22.11686199900910665 ) ) ;
#176959 = FACE_OUTER_BOUND ( 'NONE', #217597, .T. ) ;
#176960 = AXIS2_PLACEMENT_3D ( 'NONE', #208709, #165732, #28819 ) ;
#176961 = CARTESIAN_POINT ( 'NONE',  ( 23.24999999999999645, 76.00000000001165290, -69.52310748452431710 ) ) ;
#176962 = DIRECTION ( 'NONE',  ( 1.000000000000000000, 0.000000000000000000, 0.000000000000000000 ) ) ;
#176963 = CARTESIAN_POINT ( 'NONE',  ( 15.31784899511110076, 66.60336962369433422, -118.6160500917061000 ) ) ;
#176965 = CARTESIAN_POINT ( 'NONE',  ( -23.25000000000000000, 11.75000000001115552, -167.4999999999999716 ) ) ;
#176964 = DIRECTION ( 'NONE',  ( 0.000000000000000000, 0.000000000000000000, 1.000000000000000000 ) ) ;
#176966 = CARTESIAN_POINT ( 'NONE',  ( -20.54999999999999716, 85.00000000001159606, -59.62913836187181715 ) ) ;
#176968 = ORIENTED_EDGE ( 'NONE', *, *, #111867, .T. ) ;
#176967 = CYLINDRICAL_SURFACE ( 'NONE', #81407, 0.09999999999999693856 ) ;
#176969 = LINE ( 'NONE', #24305, #8306 ) ;
#176970 = EDGE_LOOP ( 'NONE', ( #210931, #190246, #222742, #25114 ) ) ;
#176971 = PLANE ( 'NONE',  #15676 ) ;
#176972 = ORIENTED_EDGE ( 'NONE', *, *, #97100, .F. ) ;
#176973 = EDGE_LOOP ( 'NONE', ( #249896, #75176, #44578, #15737 ) ) ;
#176974 = CARTESIAN_POINT ( 'NONE',  ( -18.59999999999999787, 6.982009704867601307, -204.6961521182562649 ) ) ;
#176975 = CIRCLE ( 'NONE', #247678, 0.09999999999999939493 ) ;
#176976 = DIRECTION ( 'NONE',  ( -1.000000000000000000, -0.000000000000000000, -0.000000000000000000 ) ) ;
#176977 = LINE ( 'NONE', #114405, #46156 ) ;
#176978 = EDGE_LOOP ( 'NONE', ( #208899, #55569 ) ) ;
#176979 = EDGE_CURVE ( 'NONE', #35530, #210115, #167554, .T. ) ;
#176980 = AXIS2_PLACEMENT_3D ( 'NONE', #252800, #12949, #228130 ) ;
#176981 = EDGE_CURVE ( 'NONE', #22494, #164329, #55074, .T. ) ;
#176982 = CARTESIAN_POINT ( 'NONE',  ( -20.64999999999999858, 1.115600667400684642E-11, -100.5000000000000426 ) ) ;
#176983 = EDGE_LOOP ( 'NONE', ( #209487, #4208, #78933, #244787 ) ) ;
#176984 = ORIENTED_EDGE ( 'NONE', *, *, #131418, .F. ) ;
#176985 = FACE_OUTER_BOUND ( 'NONE', #56519, .T. ) ;
#176986 = EDGE_LOOP ( 'NONE', ( #215149, #193642, #24996 ) ) ;
#176987 = CARTESIAN_POINT ( 'NONE',  ( 20.10000000000000497, 5.552655413246002425, 16.61686199900910310 ) ) ;
#176988 = DIRECTION ( 'NONE',  ( 1.000000000000000000, 0.000000000000000000, 0.000000000000000000 ) ) ;
#176989 = EDGE_LOOP ( 'NONE', ( #210805, #250460, #30741, #128942 ) ) ;
#176990 = CARTESIAN_POINT ( 'NONE',  ( -18.40000000000000213, 11.47316190337364183, -158.2500000000000284 ) ) ;
#176991 = CIRCLE ( 'NONE', #31428, 0.09999999999999939493 ) ;
#176992 = DIRECTION ( 'NONE',  ( 1.000000000000000000, 0.000000000000000000, 0.000000000000000000 ) ) ;
#176994 = ADVANCED_FACE ( 'NONE', ( #16904 ), #6732, .F. ) ;
#176993 = LINE ( 'NONE', #24324, #55178 ) ;
#176995 = VERTEX_POINT ( 'NONE', #20763 ) ;
#176996 = ADVANCED_FACE ( 'NONE', ( #58562 ), #103419, .T. ) ;
#176997 = FACE_OUTER_BOUND ( 'NONE', #159705, .T. ) ;
#176998 = DIRECTION ( 'NONE',  ( 0.000000000000000000, 0.6728971962616697722, 0.7397360091702875895 ) ) ;
#176999 = EDGE_CURVE ( 'NONE', #108506, #64218, #96763, .T. ) ;
#177000 = CARTESIAN_POINT ( 'NONE',  ( -23.15000000000000213, 55.89093952297024970, -232.7795287750844579 ) ) ;
#177001 = CIRCLE ( 'NONE', #43688, 0.5000000000000004441 ) ;
#177002 = VERTEX_POINT ( 'NONE', #157736 ) ;
#177003 = CIRCLE ( 'NONE', #210303, 0.09999999999999939493 ) ;
#177004 = CARTESIAN_POINT ( 'NONE',  ( 20.94999999999999929, 1.835341550235569663, -78.55515129256303908 ) ) ;
#177005 = EDGE_LOOP ( 'NONE', ( #256342, #103275, #97147, #230859 ) ) ;
#177006 = DIRECTION ( 'NONE',  ( 0.000000000000000000, 0.000000000000000000, -1.000000000000000000 ) ) ;
#177007 = EDGE_CURVE ( 'NONE', #165391, #153112, #242350, .T. ) ;
#177008 = CARTESIAN_POINT ( 'NONE',  ( -20.94999999999999929, -10.76604040606817847, -206.3127087229280789 ) ) ;
#177009 = CARTESIAN_POINT ( 'NONE',  ( -22.19999999999999929, -11.65000000000000036, 9.900000000000002132 ) ) ;
#177010 = DIRECTION ( 'NONE',  ( 0.000000000000000000, -0.2128009952263603677, 0.9770955615653313941 ) ) ;
#177011 = DIRECTION ( 'NONE',  ( 0.000000000000000000, 6.982962677686266711E-15, -1.000000000000000000 ) ) ;
#177012 = DIRECTION ( 'NONE',  ( -1.000000000000000000, 0.000000000000000000, 0.000000000000000000 ) ) ;
#177013 = ORIENTED_EDGE ( 'NONE', *, *, #18480, .F. ) ;
#177014 = CARTESIAN_POINT ( 'NONE',  ( -16.93255653858138388, 66.00154854603491117, -123.9414641165346893 ) ) ;
#177015 = ADVANCED_FACE ( 'NONE', ( #160284 ), #241096, .F. ) ;
#177016 = CARTESIAN_POINT ( 'NONE',  ( -16.88853107394619357, 66.04912151666482600, -82.17017113763215264 ) ) ;
#177017 = DIRECTION ( 'NONE',  ( 0.000000000000000000, 2.664535259100376091E-15, 1.000000000000000000 ) ) ;
#177018 = FACE_OUTER_BOUND ( 'NONE', #238952, .T. ) ;
#177019 = CIRCLE ( 'NONE', #222759, 12.87500000000000178 ) ;
#177020 = DIRECTION ( 'NONE',  ( 0.000000000000000000, 0.000000000000000000, 1.000000000000000000 ) ) ;
#177021 = VERTEX_POINT ( 'NONE', #218927 ) ;
#177022 = VERTEX_POINT ( 'NONE', #62444 ) ;
#177023 = FACE_OUTER_BOUND ( 'NONE', #143133, .T. ) ;
#177024 = CARTESIAN_POINT ( 'NONE',  ( 21.72449340488910252, 12.74034062369345399, -211.1718227230884963 ) ) ;
#177025 = CARTESIAN_POINT ( 'NONE',  ( -23.25000000000000355, 5.650000000011139001, -54.35000000000000142 ) ) ;
#177027 = DIRECTION ( 'NONE',  ( -1.000000000000000000, 0.000000000000000000, 0.000000000000000000 ) ) ;
#177026 = AXIS2_PLACEMENT_3D ( 'NONE', #139472, #20851, #140775 ) ;
#177028 = DIRECTION ( 'NONE',  ( 1.000000000000000000, 0.000000000000000000, 0.000000000000000000 ) ) ;
#177029 = ORIENTED_EDGE ( 'NONE', *, *, #143030, .F. ) ;
#177030 = DIRECTION ( 'NONE',  ( 0.000000000000000000, 0.000000000000000000, 1.000000000000000000 ) ) ;
#177031 = DIRECTION ( 'NONE',  ( 0.000000000000000000, 0.9525900758537773072, -0.3042567129660331271 ) ) ;
#177032 = EDGE_LOOP ( 'NONE', ( #250568, #21851, #185995, #104659 ) ) ;
#177033 = CARTESIAN_POINT ( 'NONE',  ( 18.59999999999999076, 69.55000000001230376, -160.0060803140843859 ) ) ;
#177034 = FACE_BOUND ( 'NONE', #209357, .T. ) ;
#177035 = COLOUR_RGB ( '', 0.31764706, 0.68627451, 0.89019608) ;
#177036 = ORIENTED_EDGE ( 'NONE', *, *, #111081, .T. ) ;
#177037 = DIRECTION ( 'NONE',  ( 0.000000000000000000, 0.9126074666063764829, 0.4088369013363290505 ) ) ;
#177038 = ORIENTED_EDGE ( 'NONE', *, *, #135682, .T. ) ;
#177039 = DIRECTION ( 'NONE',  ( -1.000000000000000000, -0.000000000000000000, -0.000000000000000000 ) ) ;
#177040 = FACE_OUTER_BOUND ( 'NONE', #188628, .T. ) ;
#177041 = CARTESIAN_POINT ( 'NONE',  ( -21.05000000000000071, 87.39257802171802325, -166.9491579046923277 ) ) ;
#177042 = CARTESIAN_POINT ( 'NONE',  ( 20.85000000000000142, 17.16609282392354174, -224.6038045889790453 ) ) ;
#177043 = DIRECTION ( 'NONE',  ( -1.000000000000000000, 0.000000000000000000, 0.000000000000000000 ) ) ;
#177044 = CARTESIAN_POINT ( 'NONE',  ( -16.87683809663752399, 21.23804903843306491, -12.65000000000000213 ) ) ;
#177045 = FACE_OUTER_BOUND ( 'NONE', #93962, .T. ) ;
#177046 = FACE_OUTER_BOUND ( 'NONE', #83307, .T. ) ;
#177047 = DIRECTION ( 'NONE',  ( -1.000000000000000000, 0.000000000000000000, -0.000000000000000000 ) ) ;
#177048 = EDGE_CURVE ( 'NONE', #233528, #152504, #46715, .T. ) ;
#177049 = CARTESIAN_POINT ( 'NONE',  ( 21.00000000000000000, 9.750000000011153745, -88.25000000000005684 ) ) ;
#177050 = CARTESIAN_POINT ( 'NONE',  ( -23.25000000000000355, 53.98582189624752914, -228.9137301112145622 ) ) ;
#177052 = CARTESIAN_POINT ( 'NONE',  ( 18.58222699835054570, 10.33200063080772324, -206.5931674956642610 ) ) ;
#177051 = AXIS2_PLACEMENT_3D ( 'NONE', #24186, #238070, #257579 ) ;
#177053 = AXIS2_PLACEMENT_3D ( 'NONE', #153728, #173288, #134093 ) ;
#177054 = DIRECTION ( 'NONE',  ( 0.000000000000000000, -2.168404344970984413E-15, -1.000000000000000000 ) ) ;
#177056 = DIRECTION ( 'NONE',  ( -0.000000000000000000, 1.000000000000000000, -0.000000000000000000 ) ) ;
#177055 = CIRCLE ( 'NONE', #156211, 0.09999999999998898659 ) ;
#177057 = ORIENTED_EDGE ( 'NONE', *, *, #69337, .T. ) ;
#177058 = CARTESIAN_POINT ( 'NONE',  ( 21.05000000000000071, 6.257814610476131634, 0.09779029130878996723 ) ) ;
#177059 = DIRECTION ( 'NONE',  ( 0.000000000000000000, -1.000000000000000000, 1.387778780781442047E-14 ) ) ;
#177061 = ADVANCED_FACE ( 'NONE', ( #221487 ), #81960, .T. ) ;
#177060 = CARTESIAN_POINT ( 'NONE',  ( 20.41140022480507454, 10.41043084241319683, -41.11500130363457117 ) ) ;
#177062 = EDGE_LOOP ( 'NONE', ( #202686, #234166, #138028, #100931 ) ) ;
#177063 = DIRECTION ( 'NONE',  ( 1.000000000000000000, 6.938893903907222067E-15, 0.000000000000000000 ) ) ;
#177064 = EDGE_CURVE ( 'NONE', #21148, #224911, #189148, .T. ) ;
#177065 = ADVANCED_FACE ( 'NONE', ( #179834 ), #88396, .T. ) ;
#177066 = DIRECTION ( 'NONE',  ( 1.000000000000000000, 0.000000000000000000, 0.000000000000000000 ) ) ;
#177067 = EDGE_LOOP ( 'NONE', ( #149019, #201320, #184129, #168300 ) ) ;
#177068 = FACE_OUTER_BOUND ( 'NONE', #246649, .T. ) ;
#177069 = DIRECTION ( 'NONE',  ( -1.000000000000000000, 0.000000000000000000, 0.000000000000000000 ) ) ;
#177070 = ORIENTED_EDGE ( 'NONE', *, *, #12196, .F. ) ;
#177071 = VECTOR ( 'NONE', #21919, 1000.000000000000000 ) ;
#177072 = AXIS2_PLACEMENT_3D ( 'NONE', #83179, #4927, #222709 ) ;
#177073 = CIRCLE ( 'NONE', #89550, 0.09999999999998898659 ) ;
#177074 = ORIENTED_EDGE ( 'NONE', *, *, #75002, .F. ) ;
#177075 = DIRECTION ( 'NONE',  ( 1.000000000000000000, 7.304098846218105085E-16, 4.217023435051677501E-16 ) ) ;
#177076 = EDGE_CURVE ( 'NONE', #239074, #154564, #100246, .T. ) ;
#177077 = ORIENTED_EDGE ( 'NONE', *, *, #137657, .F. ) ;
#177078 = CARTESIAN_POINT ( 'NONE',  ( -22.59999999999999787, 75.89914163091405896, -215.2726746080137445 ) ) ;
#177079 = CARTESIAN_POINT ( 'NONE',  ( 21.13461538461538325, 67.11458296203758778, -124.2731074845243597 ) ) ;
#177081 = CIRCLE ( 'NONE', #127169, 0.4000000000000114575 ) ;
#177080 = DIRECTION ( 'NONE',  ( 0.000000000000000000, 0.2617529984165152257, 0.9651348961777124202 ) ) ;
#177083 = DIRECTION ( 'NONE',  ( 0.000000000000000000, 0.2128009952263485993, -0.9770955615653341697 ) ) ;
#177082 = AXIS2_PLACEMENT_3D ( 'NONE', #43346, #240268, #202407 ) ;
#177084 = AXIS2_PLACEMENT_3D ( 'NONE', #198655, #254733, #96951 ) ;
#177085 = CARTESIAN_POINT ( 'NONE',  ( -20.85000000000000142, 80.78317333349157536, -192.9003134612049166 ) ) ;
#177086 = CARTESIAN_POINT ( 'NONE',  ( -20.65000000000000568, 68.75000000001209344, -127.2731074845243597 ) ) ;
#177087 = CARTESIAN_POINT ( 'NONE',  ( 21.00000000000000000, 66.25000000001253397, -182.2731074845244450 ) ) ;
#177088 = CARTESIAN_POINT ( 'NONE',  ( 23.24999999999999289, 31.89597452117650533, -238.9192857152811484 ) ) ;
#177090 = EDGE_LOOP ( 'NONE', ( #123850, #100435, #117537 ) ) ;
#177089 = FACE_OUTER_BOUND ( 'NONE', #123607, .T. ) ;
#177091 = ORIENTED_EDGE ( 'NONE', *, *, #51935, .T. ) ;
#177093 = CARTESIAN_POINT ( 'NONE',  ( -21.05000000000000071, 64.36312671090715298, -62.70134827119954934 ) ) ;
#177092 = CARTESIAN_POINT ( 'NONE',  ( 18.58719872626879877, 38.15560524319364077, -261.2056399649021046 ) ) ;
#177095 = ORIENTED_EDGE ( 'NONE', *, *, #245146, .F. ) ;
#177094 = CARTESIAN_POINT ( 'NONE',  ( -18.59999999999999787, 11.64999999999999680, 11.75000000000000000 ) ) ;
#177096 = B_SPLINE_CURVE_WITH_KNOTS ( 'NONE', 3,
 ( #201947, #3735, #83245, #130093, #93538, #192656, #213484, #230494, #148391, #92248, #170575, #133943, #227923, #209642, #250053, #114394 ),
 .UNSPECIFIED., .F., .F.,
 ( 4, 3, 3, 3, 3, 4 ),
 ( 0.000000000000000000, 2.209833635978364789E-05, 5.595056164120505162E-05, 8.979992002657522703E-05, 0.0001236482757199150722, 0.0001574984039363133280 ),
 .UNSPECIFIED. ) ;
#177097 = ORIENTED_EDGE ( 'NONE', *, *, #214054, .F. ) ;
#177098 = FACE_OUTER_BOUND ( 'NONE', #113630, .T. ) ;
#177099 = CARTESIAN_POINT ( 'NONE',  ( 20.53930447207977039, 8.977148687535430938, -175.9425071415753621 ) ) ;
#177100 = AXIS2_PLACEMENT_3D ( 'NONE', #201204, #2991, #202494 ) ;
#177101 = ADVANCED_FACE ( 'NONE', ( #161558 ), #19466, .F. ) ;
#177102 = VECTOR ( 'NONE', #102578, 1000.000000000000000 ) ;
#177103 = CARTESIAN_POINT ( 'NONE',  ( 20.94999999999998508, 62.88396779178383156, -206.9948552354528886 ) ) ;
#177104 = DIRECTION ( 'NONE',  ( -2.978066053179069723E-16, 0.4721928772777349015, 0.8814952561688428334 ) ) ;
#177105 = FACE_OUTER_BOUND ( 'NONE', #241317, .T. ) ;
#177106 = AXIS2_PLACEMENT_3D ( 'NONE', #126021, #184714, #222545 ) ;
#177107 = CARTESIAN_POINT ( 'NONE',  ( -18.39999999999999858, 20.74413403641815989, -228.0104766523929243 ) ) ;
#177108 = AXIS2_PLACEMENT_3D ( 'NONE', #247309, #49110, #208210 ) ;
#177109 = DIRECTION ( 'NONE',  ( 0.000000000000000000, 0.9651348961776958779, -0.2617529984165761214 ) ) ;
#177110 = EDGE_CURVE ( 'NONE', #232095, #34141, #80003, .T. ) ;
#177111 = DIRECTION ( 'NONE',  ( 0.000000000000000000, 1.000000000000000000, 0.000000000000000000 ) ) ;
#177112 = EDGE_LOOP ( 'NONE', ( #81209, #72714, #45994, #212184 ) ) ;
#177113 = ORIENTED_EDGE ( 'NONE', *, *, #52191, .T. ) ;
#177114 = CYLINDRICAL_SURFACE ( 'NONE', #6510, 0.1000000000000024342 ) ;
#177115 = EDGE_LOOP ( 'NONE', ( #118703, #203491, #162587, #99519 ) ) ;
#177116 = CARTESIAN_POINT ( 'NONE',  ( -18.59999999999999787, 57.82359945636609666, -226.0354702357591350 ) ) ;
#177117 = ORIENTED_EDGE ( 'NONE', *, *, #167862, .T. ) ;
#177118 = CARTESIAN_POINT ( 'NONE',  ( -16.89021194854739960, 14.13613997954251289, -219.1501013543562522 ) ) ;
#177119 = CARTESIAN_POINT ( 'NONE',  ( -15.66061380678752535, 48.63273434562353970, -233.9299239298079840 ) ) ;
#177120 = FACE_OUTER_BOUND ( 'NONE', #166054, .T. ) ;
#177122 = ORIENTED_EDGE ( 'NONE', *, *, #155463, .F. ) ;
#177121 = DIRECTION ( 'NONE',  ( 1.000000000000000000, -3.265361837132813093E-16, -2.280189983783949500E-30 ) ) ;
#177123 = FACE_OUTER_BOUND ( 'NONE', #170582, .T. ) ;
#177124 = EDGE_LOOP ( 'NONE', ( #3105, #106513, #68766 ) ) ;
#177125 = DIRECTION ( 'NONE',  ( 0.000000000000000000, -1.000000000000000000, 0.000000000000000000 ) ) ;
#177126 = AXIS2_PLACEMENT_3D ( 'NONE', #217452, #119671, #199201 ) ;
#177127 = EDGE_CURVE ( 'NONE', #115296, #129552, #9310, .T. ) ;
#177128 = DIRECTION ( 'NONE',  ( 1.000000000000000000, 0.000000000000000000, 0.000000000000000000 ) ) ;
#177129 = DIRECTION ( 'NONE',  ( 0.000000000000000000, 1.000000000000000000, 0.000000000000000000 ) ) ;
#177130 = AXIS2_PLACEMENT_3D ( 'NONE', #21588, #81509, #157264 ) ;
#177131 = CARTESIAN_POINT ( 'NONE',  ( -22.14074124539699540, 75.90094710416866519, -210.9131853355681301 ) ) ;
#177132 = DIRECTION ( 'NONE',  ( 0.000000000000000000, 1.000000000000000000, -6.308085367188393199E-16 ) ) ;
#177133 = ORIENTED_EDGE ( 'NONE', *, *, #73316, .F. ) ;
#177134 = CARTESIAN_POINT ( 'NONE',  ( -23.15000000000000213, 36.65892442174935439, -249.5511627012433848 ) ) ;
#177135 = ORIENTED_EDGE ( 'NONE', *, *, #165586, .T. ) ;
#177138 = ORIENTED_EDGE ( 'NONE', *, *, #34975, .T. ) ;
#177137 = CARTESIAN_POINT ( 'NONE',  ( -18.59999999999999787, 45.93315328338058379, -256.6017782078560003 ) ) ;
#177136 = CARTESIAN_POINT ( 'NONE',  ( 20.95512820512820440, 62.54007867304706281, -212.5651857150171224 ) ) ;
#177139 = DIRECTION ( 'NONE',  ( 1.000000000000000000, 0.000000000000000000, 0.000000000000000000 ) ) ;
#177140 = AXIS2_PLACEMENT_3D ( 'NONE', #167216, #104600, #146320 ) ;
#177141 = EDGE_CURVE ( 'NONE', #123153, #211510, #66294, .T. ) ;
#177142 = CARTESIAN_POINT ( 'NONE',  ( -18.50000000000000711, 57.72708596674832648, -226.0092949359174952 ) ) ;
#177143 = VECTOR ( 'NONE', #3759, 1000.000000000000000 ) ;
#177144 = ORIENTED_EDGE ( 'NONE', *, *, #39106, .F. ) ;
#177146 = ADVANCED_FACE ( 'NONE', ( #164114 ), #150971, .F. ) ;
#177145 = CARTESIAN_POINT ( 'NONE',  ( 18.41815437325351823, 85.49870985315352812, -129.9191616457220277 ) ) ;
#177147 = FACE_OUTER_BOUND ( 'NONE', #63910, .T. ) ;
#177148 = EDGE_CURVE ( 'NONE', #220110, #63695, #225336, .T. ) ;
#177149 = CARTESIAN_POINT ( 'NONE',  ( -16.93388492042258875, 9.988541822515902169, -12.59945487681382836 ) ) ;
#177151 = EDGE_CURVE ( 'NONE', #39117, #32631, #144520, .T. ) ;
#177150 = AXIS2_PLACEMENT_3D ( 'NONE', #34495, #72327, #91871 ) ;
#177153 = ORIENTED_EDGE ( 'NONE', *, *, #214807, .T. ) ;
#177152 = CARTESIAN_POINT ( 'NONE',  ( -22.94999999999999929, -11.75000000000000178, 0.000000000000000000 ) ) ;
#177154 = CIRCLE ( 'NONE', #222896, 0.09999999999998708533 ) ;
#177155 = DIRECTION ( 'NONE',  ( 0.000000000000000000, 0.000000000000000000, -1.000000000000000000 ) ) ;
#177157 = VERTEX_POINT ( 'NONE', #243636 ) ;
#177156 = ADVANCED_FACE ( 'NONE', ( #7595 ), #224061, .T. ) ;
#177158 = CARTESIAN_POINT ( 'NONE',  ( -16.85718274719485166, 9.976142314632857833, -180.0633463321825616 ) ) ;
#177159 = CARTESIAN_POINT ( 'NONE',  ( 18.51997666896878059, -9.392332131507778570, -74.14340618748370559 ) ) ;
#177160 = CARTESIAN_POINT ( 'NONE',  ( -16.80438519320023616, 44.13624578021552480, -235.2988313683356409 ) ) ;
#177161 = ADVANCED_FACE ( 'NONE', ( #25893 ), #180022, .T. ) ;
#177162 = ORIENTED_EDGE ( 'NONE', *, *, #149128, .T. ) ;
#177163 = LINE ( 'NONE', #217519, #59210 ) ;
#177166 = EDGE_CURVE ( 'NONE', #189338, #11593, #75956, .T. ) ;
#177165 = EDGE_CURVE ( 'NONE', #4043, #255700, #227929, .T. ) ;
#177164 = ORIENTED_EDGE ( 'NONE', *, *, #246360, .F. ) ;
#177167 = CARTESIAN_POINT ( 'NONE',  ( 18.49999999999999289, 7.021664781911246322, -104.3335654018973315 ) ) ;
#177168 = CARTESIAN_POINT ( 'NONE',  ( 18.39999999999999858, -9.399999999988843058, -55.25000000000004974 ) ) ;
#177169 = CARTESIAN_POINT ( 'NONE',  ( -17.11825945287482753, 10.05000000001113847, -46.14999999999999858 ) ) ;
#177170 = CIRCLE ( 'NONE', #64707, 11.75000000000000000 ) ;
#177171 = ORIENTED_EDGE ( 'NONE', *, *, #116110, .T. ) ;
#177172 = DIRECTION ( 'NONE',  ( -0.000000000000000000, -0.000000000000000000, -1.000000000000000000 ) ) ;
#177173 = PLANE ( 'NONE',  #93099 ) ;
#177174 = EDGE_CURVE ( 'NONE', #72109, #254577, #30182, .T. ) ;
#177175 = FACE_OUTER_BOUND ( 'NONE', #38042, .T. ) ;
#177176 = ORIENTED_EDGE ( 'NONE', *, *, #242572, .T. ) ;
#177177 = DIRECTION ( 'NONE',  ( -1.000000000000000000, -0.000000000000000000, -0.000000000000000000 ) ) ;
#177178 = DIRECTION ( 'NONE',  ( 6.938893903907222856E-15, 0.4088369013363281068, -0.9126074666063770380 ) ) ;
#177179 = EDGE_CURVE ( 'NONE', #85475, #27168, #124987, .T. ) ;
#177181 = EDGE_CURVE ( 'NONE', #16604, #61134, #176695, .T. ) ;
#177180 = DIRECTION ( 'NONE',  ( 0.000000000000000000, -6.982962677686266711E-15, 1.000000000000000000 ) ) ;
#177182 = TOROIDAL_SURFACE ( 'NONE', #35708, 0.2000000000000000111, 0.1000000000000000056 ) ;
#177183 = AXIS2_PLACEMENT_3D ( 'NONE', #195015, #78874, #95879 ) ;
#177184 = ORIENTED_EDGE ( 'NONE', *, *, #130371, .T. ) ;
#177185 = EDGE_CURVE ( 'NONE', #225500, #70632, #84261, .T. ) ;
#177186 = CYLINDRICAL_SURFACE ( 'NONE', #112649, 2.000000000000001776 ) ;
#177187 = EDGE_LOOP ( 'NONE', ( #140750, #78687, #155001 ) ) ;
#177189 = ORIENTED_EDGE ( 'NONE', *, *, #113998, .F. ) ;
#177188 = DIRECTION ( 'NONE',  ( 0.000000000000000000, 0.4088369013363287729, -0.9126074666063767049 ) ) ;
#177190 = EDGE_CURVE ( 'NONE', #45677, #38476, #184093, .T. ) ;
#177193 = ORIENTED_EDGE ( 'NONE', *, *, #72059, .T. ) ;
#177192 = ORIENTED_EDGE ( 'NONE', *, *, #163640, .T. ) ;
#177191 = CARTESIAN_POINT ( 'NONE',  ( -20.54999999999999716, -8.999999999988846255, -110.3939691226524786 ) ) ;
#177194 = CARTESIAN_POINT ( 'NONE',  ( 18.49999999999998934, 56.14960075277838314, -100.7428044267230973 ) ) ;
#177195 = CARTESIAN_POINT ( 'NONE',  ( -16.77683809663752257, 52.34166666667851331, -86.27310748452447342 ) ) ;
#177196 = CARTESIAN_POINT ( 'NONE',  ( -16.83558968593874994, 12.41665198337125098, -211.2549122955051359 ) ) ;
#177197 = LINE ( 'NONE', #205699, #257439 ) ;
#177198 = AXIS2_PLACEMENT_3D ( 'NONE', #82883, #106313, #127193 ) ;
#177199 = DIRECTION ( 'NONE',  ( 0.000000000000000000, 0.000000000000000000, -1.000000000000000000 ) ) ;
#177200 = CARTESIAN_POINT ( 'NONE',  ( -37.88850191057539973, -9.849999999999994316, 30.09999999999999076 ) ) ;
#177202 = FACE_OUTER_BOUND ( 'NONE', #137621, .T. ) ;
#177201 = DIRECTION ( 'NONE',  ( -1.000000000000000000, -0.000000000000000000, -0.000000000000000000 ) ) ;
#177203 = ORIENTED_EDGE ( 'NONE', *, *, #186846, .T. ) ;
#177204 = ORIENTED_EDGE ( 'NONE', *, *, #256516, .T. ) ;
#177205 = ORIENTED_EDGE ( 'NONE', *, *, #124761, .F. ) ;
#177206 = DIRECTION ( 'NONE',  ( -1.000000000000000000, 0.000000000000000000, 0.000000000000000000 ) ) ;
#177207 = AXIS2_PLACEMENT_3D ( 'NONE', #28251, #226391, #243406 ) ;
#177209 = ORIENTED_EDGE ( 'NONE', *, *, #35244, .T. ) ;
#177208 = DIRECTION ( 'NONE',  ( -0.000000000000000000, -0.8814952561688430555, 0.4721928772777346239 ) ) ;
#177210 = DIRECTION ( 'NONE',  ( -0.000000000000000000, 1.000000000000000000, -0.000000000000000000 ) ) ;
#177211 = VERTEX_POINT ( 'NONE', #188795 ) ;
#177212 = CARTESIAN_POINT ( 'NONE',  ( 18.39999999999999858, 77.17949092533254429, -241.9177572069595783 ) ) ;
#177213 = ORIENTED_EDGE ( 'NONE', *, *, #189302, .F. ) ;
#177214 = LINE ( 'NONE', #138033, #54538 ) ;
#177215 = ORIENTED_EDGE ( 'NONE', *, *, #238624, .F. ) ;
#177216 = LINE ( 'NONE', #237166, #172994 ) ;
#177217 = DIRECTION ( 'NONE',  ( -1.000000000000000000, 0.000000000000000000, 0.000000000000000000 ) ) ;
#177219 = EDGE_LOOP ( 'NONE', ( #64620, #216516, #218997, #9396, #13243 ) ) ;
#177218 = ORIENTED_EDGE ( 'NONE', *, *, #133215, .F. ) ;
#177220 = AXIS2_PLACEMENT_3D ( 'NONE', #237273, #22084, #101567 ) ;
#177221 = ORIENTED_EDGE ( 'NONE', *, *, #196069, .F. ) ;
#177222 = DIRECTION ( 'NONE',  ( -1.000000000000000000, 0.000000000000000000, 0.000000000000000000 ) ) ;
#177223 = ORIENTED_EDGE ( 'NONE', *, *, #197709, .F. ) ;
#177224 = ORIENTED_EDGE ( 'NONE', *, *, #6391, .T. ) ;
#177225 = DIRECTION ( 'NONE',  ( 0.7071067811865475727, 0.7071067811865475727, -0.000000000000000000 ) ) ;
#177227 = ORIENTED_EDGE ( 'NONE', *, *, #163174, .T. ) ;
#177226 = CARTESIAN_POINT ( 'NONE',  ( 18.40916198585730967, -9.499999999988844479, -107.1001896318234543 ) ) ;
#177229 = CARTESIAN_POINT ( 'NONE',  ( 20.95265033839679347, 65.48774916754517506, -162.4573437284944646 ) ) ;
#177228 = CARTESIAN_POINT ( 'NONE',  ( 19.58285714285715073, 60.73471314953822997, -225.3683569544359671 ) ) ;
#177230 = CARTESIAN_POINT ( 'NONE',  ( 21.15000000000005187, 77.83551161375991967, -47.62760213295649692 ) ) ;
#177231 = CARTESIAN_POINT ( 'NONE',  ( -18.39999999999999858, 11.47867410001043709, -42.77469321634066546 ) ) ;
#177232 = LINE ( 'NONE', #256685, #105196 ) ;
#177233 = ORIENTED_EDGE ( 'NONE', *, *, #108050, .T. ) ;
#177234 = VERTEX_POINT ( 'NONE', #149702 ) ;
#177235 = CARTESIAN_POINT ( 'NONE',  ( -20.65000000000000568, 28.93140779147704933, -237.1870821964559184 ) ) ;
#177236 = CARTESIAN_POINT ( 'NONE',  ( -18.59999999999999787, 64.35000000001234355, -163.0083017138704236 ) ) ;
#177238 = ADVANCED_FACE ( 'NONE', ( #10173 ), #248785, .F. ) ;
#177237 = DIRECTION ( 'NONE',  ( 1.000000000000000000, 0.000000000000000000, 0.000000000000000000 ) ) ;
#177239 = AXIS2_PLACEMENT_3D ( 'NONE', #207965, #244492, #29347 ) ;
#177240 = ORIENTED_EDGE ( 'NONE', *, *, #191899, .T. ) ;
#177241 = CARTESIAN_POINT ( 'NONE',  ( 20.94999999999999574, 74.83729825007388570, -94.92310748452432279 ) ) ;
#177242 = EDGE_CURVE ( 'NONE', #33031, #195816, #104103, .T. ) ;
#177243 = VECTOR ( 'NONE', #9998, 1000.000000000000000 ) ;
#177244 = CIRCLE ( 'NONE', #210532, 0.09999999999999520384 ) ;
#177245 = AXIS2_PLACEMENT_3D ( 'NONE', #173363, #129059, #113337 ) ;
#177246 = CARTESIAN_POINT ( 'NONE',  ( -16.93211319090181632, 51.66459555148166061, -231.8712077822809761 ) ) ;
#177247 = DIRECTION ( 'NONE',  ( 0.000000000000000000, -0.4930308989875248349, -0.8700118002898312719 ) ) ;
#177248 = ORIENTED_EDGE ( 'NONE', *, *, #211216, .F. ) ;
#177249 = EDGE_LOOP ( 'NONE', ( #231098, #233979, #205020, #159725 ) ) ;
#177250 = EDGE_CURVE ( 'NONE', #132941, #147015, #11463, .T. ) ;
#177251 = DIRECTION ( 'NONE',  ( 0.000000000000000000, 0.000000000000000000, 1.000000000000000000 ) ) ;
#177253 = ADVANCED_FACE ( 'NONE', ( #252611 ), #171845, .T. ) ;
#177252 = LINE ( 'NONE', #114679, #252856 ) ;
#177254 = ORIENTED_EDGE ( 'NONE', *, *, #103779, .T. ) ;
#177255 = CARTESIAN_POINT ( 'NONE',  ( -20.64999999999999858, 74.00000000001151079, -48.74772940728643533 ) ) ;
#177256 = VERTEX_POINT ( 'NONE', #74027 ) ;
#177257 = FACE_OUTER_BOUND ( 'NONE', #100758, .T. ) ;
#177258 = DIRECTION ( 'NONE',  ( 0.7071067811865388020, -0.7071067811865561215, 0.000000000000000000 ) ) ;
#177260 = CARTESIAN_POINT ( 'NONE',  ( -22.48660254037844552, 55.87785187304944401, -232.8277855198933253 ) ) ;
#177259 = LINE ( 'NONE', #136804, #111530 ) ;
#177261 = LINE ( 'NONE', #152566, #69687 ) ;
#177262 = CARTESIAN_POINT ( 'NONE',  ( -20.54999999999999716, 68.85000000001259934, -191.2731074845244166 ) ) ;
#177263 = LINE ( 'NONE', #175975, #210834 ) ;
#177264 = VECTOR ( 'NONE', #20333, 1000.000000000000000 ) ;
#177265 = PRESENTATION_LAYER_ASSIGNMENT (  '', '', ( #185604 ) ) ;
#177266 = EDGE_CURVE ( 'NONE', #132961, #175526, #170580, .T. ) ;
#177268 = ORIENTED_EDGE ( 'NONE', *, *, #70279, .F. ) ;
#177267 = VERTEX_POINT ( 'NONE', #114399 ) ;
#177269 = ORIENTED_EDGE ( 'NONE', *, *, #205051, .F. ) ;
#177271 = EDGE_CURVE ( 'NONE', #31535, #203363, #2547, .T. ) ;
#177270 = AXIS2_PLACEMENT_3D ( 'NONE', #243796, #82124, #63878 ) ;
#177272 = CARTESIAN_POINT ( 'NONE',  ( -18.47653818581422058, -7.732071902224467941, -209.9769657719527629 ) ) ;
#177273 = DIRECTION ( 'NONE',  ( -1.000000000000000000, -0.000000000000000000, -0.000000000000000000 ) ) ;
#177274 = TOROIDAL_SURFACE ( 'NONE', #85607, 0.4000000000000003553, 0.1000000000000000056 ) ;
#177275 = FACE_OUTER_BOUND ( 'NONE', #181191, .T. ) ;
#177277 = DIRECTION ( 'NONE',  ( 0.000000000000000000, -1.000000000000000000, 0.000000000000000000 ) ) ;
#177276 = CARTESIAN_POINT ( 'NONE',  ( 20.13684514580102913, 9.495855392750403468, -8.143031685684873011 ) ) ;
#177278 = CARTESIAN_POINT ( 'NONE',  ( -21.45000000000000284, 7.708578643773852157, -179.7499999999999716 ) ) ;
#177279 = ORIENTED_EDGE ( 'NONE', *, *, #153278, .T. ) ;
#177280 = CIRCLE ( 'NONE', #168904, 14.30833333333333890 ) ;
#177281 = CARTESIAN_POINT ( 'NONE',  ( -21.14999999999999858, 76.00000000001267608, -203.5231074845243597 ) ) ;
#177282 = CIRCLE ( 'NONE', #214641, 0.1000000000000028644 ) ;
#177283 = TOROIDAL_SURFACE ( 'NONE', #148017, 0.2000000000000000111, 0.1000000000000000056 ) ;
#177284 = VERTEX_POINT ( 'NONE', #12757 ) ;
#177285 = ORIENTED_EDGE ( 'NONE', *, *, #225449, .F. ) ;
#177286 = CARTESIAN_POINT ( 'NONE',  ( -20.64999999999999858, 74.00000000001254818, -183.2477294072864709 ) ) ;
#177287 = CARTESIAN_POINT ( 'NONE',  ( -22.44366136229477249, 0.009341569497225227225, -88.85028144252612492 ) ) ;
#177288 = DIRECTION ( 'NONE',  ( 0.000000000000000000, 1.000000000000000000, 6.982962677686266711E-15 ) ) ;
#177289 = CARTESIAN_POINT ( 'NONE',  ( 21.05000000000000071, 5.850000000011105428, -43.63249722427796939 ) ) ;
#177290 = EDGE_CURVE ( 'NONE', #34419, #82189, #28137, .T. ) ;
#177291 = VECTOR ( 'NONE', #84424, 1000.000000000000000 ) ;
#177292 = CARTESIAN_POINT ( 'NONE',  ( -20.85000000000000497, 56.11297552314564285, -227.9607914937810733 ) ) ;
#177293 = ORIENTED_EDGE ( 'NONE', *, *, #170498, .T. ) ;
#177294 = VERTEX_POINT ( 'NONE', #16605 ) ;
#177295 = VECTOR ( 'NONE', #65534, 1000.000000000000000 ) ;
#177296 = DIRECTION ( 'NONE',  ( 0.000000000000000000, -3.469446951953635015E-14, 1.000000000000000000 ) ) ;
#177297 = CARTESIAN_POINT ( 'NONE',  ( -16.97683809663752186, 61.03587125567668181, -221.0679030354277188 ) ) ;
#177298 = ORIENTED_EDGE ( 'NONE', *, *, #227507, .T. ) ;
#177299 = DIRECTION ( 'NONE',  ( -1.000000000000000000, -0.000000000000000000, -0.000000000000000000 ) ) ;
#177300 = DIRECTION ( 'NONE',  ( 0.000000000000000000, 6.938893903907222067E-15, -1.000000000000000000 ) ) ;
#177301 = AXIS2_PLACEMENT_3D ( 'NONE', #88798, #247894, #69278 ) ;
#177302 = FACE_OUTER_BOUND ( 'NONE', #194465, .T. ) ;
#177303 = VECTOR ( 'NONE', #172226, 1000.000000000000000 ) ;
#177305 = EDGE_CURVE ( 'NONE', #88949, #176903, #148926, .T. ) ;
#177304 = DIRECTION ( 'NONE',  ( 1.000000000000000000, -0.000000000000000000, -0.000000000000000000 ) ) ;
#177306 = CARTESIAN_POINT ( 'NONE',  ( -21.04999999999999716, -0.08574093703340139594, 6.413826288812968457 ) ) ;
#177308 = CARTESIAN_POINT ( 'NONE',  ( -13.40000000000000036, -8.250000000000007105, 17.60000000000000497 ) ) ;
#177307 = DIRECTION ( 'NONE',  ( 0.000000000000000000, -1.000000000000000000, 0.000000000000000000 ) ) ;
#177309 = CARTESIAN_POINT ( 'NONE',  ( -23.25000000000000000, 76.00000000001234923, -165.9731074845243768 ) ) ;
#177310 = ADVANCED_FACE ( 'NONE', ( #255133 ), #140514, .T. ) ;
#177311 = CARTESIAN_POINT ( 'NONE',  ( -21.05000000000000071, 5.899999999999947065, -10.21909976465641456 ) ) ;
#177312 = DIRECTION ( 'NONE',  ( 0.000000000000000000, -1.000000000000000000, 0.000000000000000000 ) ) ;
#177313 = LINE ( 'NONE', #97705, #252521 ) ;
#177314 = B_SPLINE_CURVE_WITH_KNOTS ( 'NONE', 3,
 ( #141648, #99926, #823, #101194 ),
 .UNSPECIFIED., .F., .F.,
 ( 4, 4 ),
 ( 0.000000000000000000, 0.0001048066582182725291 ),
 .UNSPECIFIED. ) ;
#177316 = ORIENTED_EDGE ( 'NONE', *, *, #241478, .T. ) ;
#177315 = CARTESIAN_POINT ( 'NONE',  ( -23.25000000000000000, 14.80545736607782814, -235.9842437978701639 ) ) ;
#177317 = B_SPLINE_CURVE_WITH_KNOTS ( 'NONE', 3,
 ( #7226, #106317, #183318, #50203, #185874, #47627, #5933, #245858, #146723, #68508 ),
 .UNSPECIFIED., .F., .F.,
 ( 4, 2, 2, 2, 4 ),
 ( 0.000000000000000000, 0.0003916577441626822214, 0.0005874866162440240368, 0.0006854010522846949987, 0.0007833154883253658522 ),
 .UNSPECIFIED. ) ;
#177318 = EDGE_CURVE ( 'NONE', #70602, #237528, #32223, .T. ) ;
#177319 = DIRECTION ( 'NONE',  ( 0.000000000000000000, 0.000000000000000000, 1.000000000000000000 ) ) ;
#177320 = ORIENTED_EDGE ( 'NONE', *, *, #189619, .T. ) ;
#177321 = APPLICATION_CONTEXT ( 'automotive_design' ) ;
#177322 = EDGE_CURVE ( 'NONE', #108947, #41838, #11825, .T. ) ;
#177324 = AXIS2_PLACEMENT_3D ( 'NONE', #189285, #92726, #229691 ) ;
#177323 = CARTESIAN_POINT ( 'NONE',  ( -18.40000000000000213, 54.09347887257330711, -229.1540424707546322 ) ) ;
#177325 = CARTESIAN_POINT ( 'NONE',  ( -23.25000000000000000, 0.000000000000000000, 0.000000000000000000 ) ) ;
#177327 = EDGE_LOOP ( 'NONE', ( #16109, #153110, #108742, #68129 ) ) ;
#177326 = AXIS2_PLACEMENT_3D ( 'NONE', #57810, #35730, #253450 ) ;
#177328 = CARTESIAN_POINT ( 'NONE',  ( -21.05000000000000071, 86.58125133469155799, -209.3975964148341973 ) ) ;
#177329 = EDGE_CURVE ( 'NONE', #94706, #151867, #2135, .T. ) ;
#177330 = DIRECTION ( 'NONE',  ( 1.000000000000000000, 0.000000000000000000, 0.000000000000000000 ) ) ;
#177331 = CARTESIAN_POINT ( 'NONE',  ( 22.44352723754029810, 0.009277095054436624438, -21.85027865465129437 ) ) ;
#177332 = CARTESIAN_POINT ( 'NONE',  ( -20.94999999999999929, 1.115600667400684642E-11, -67.00000000000004263 ) ) ;
#177333 = DIRECTION ( 'NONE',  ( 0.000000000000000000, 0.000000000000000000, -1.000000000000000000 ) ) ;
#177334 = DIRECTION ( 'NONE',  ( 1.000000000000000000, 0.000000000000000000, 0.000000000000000000 ) ) ;
#177335 = ORIENTED_EDGE ( 'NONE', *, *, #160699, .T. ) ;
#177336 = LINE ( 'NONE', #56038, #237262 ) ;
#177338 = VERTEX_POINT ( 'NONE', #242039 ) ;
#177337 = FACE_OUTER_BOUND ( 'NONE', #210881, .T. ) ;
#177339 = FACE_OUTER_BOUND ( 'NONE', #171791, .T. ) ;
#177340 = EDGE_CURVE ( 'NONE', #50990, #251678, #245105, .T. ) ;
#177341 =( BOUNDED_SURFACE ( )  B_SPLINE_SURFACE ( 3, 2, ( 
 ( #139099, #137837, #879 ),
 ( #217373, #2176, #102540 ),
 ( #37490, #40073, #136552 ),
 ( #140410, #3467, #256447 ),
 ( #257744, #117013, #119600 ),
 ( #219959, #158736, #118303 ),
 ( #21774, #141697, #197819 ),
 ( #200401, #201674, #199115 ),
 ( #60874, #236957, #157458 ),
 ( #160013, #20496, #19193 ) ),
 .UNSPECIFIED., .F., .F., .F. ) 
 B_SPLINE_SURFACE_WITH_KNOTS ( ( 4, 2, 2, 2, 4 ),
 ( 3, 3 ),
 ( 0.0001836757140118967866, 0.0004000170051583450668, 0.0005081876507315692204, 0.0005622729735181812702, 0.0006163582963047933199 ),
 ( 0.000000000000000000, 1.000000000000000000 ),
 .UNSPECIFIED. ) 
 GEOMETRIC_REPRESENTATION_ITEM ( )  RATIONAL_B_SPLINE_SURFACE ( (
 ( 1.000000000000000000, 0.7071067811865475727, 1.000000000000000000),
 ( 1.000000000000000000, 0.6461995200041559251, 1.000000000000000000),
 ( 1.000000000000000000, 0.5776453529532865616, 1.000000000000000000),
 ( 1.000000000000000000, 0.4585233068360237696, 1.000000000000000000),
 ( 1.000000000000000000, 0.4154092989944294656, 1.000000000000000000),
 ( 1.000000000000000000, 0.3550093145832801111, 1.000000000000000000),
 ( 1.000000000000000000, 0.3354498651690954736, 1.000000000000000000),
 ( 1.000000000000000000, 0.3060347992252003824, 1.000000000000000000),
 ( 1.000000000000000000, 0.2963555829628572447, 1.000000000000000000),
 ( 1.000000000000000000, 0.2966190024561997651, 1.000000000000000000) ) ) 
 REPRESENTATION_ITEM ( '' )  SURFACE ( )  );
#177342 = DIRECTION ( 'NONE',  ( -1.000000000000000000, -0.000000000000000000, -0.000000000000000000 ) ) ;
#177343 = DIRECTION ( 'NONE',  ( 1.000000000000000000, -0.000000000000000000, -0.000000000000000000 ) ) ;
#177344 = CIRCLE ( 'NONE', #64862, 0.1000000000000028644 ) ;
#177345 = ORIENTED_EDGE ( 'NONE', *, *, #152182, .T. ) ;
#177346 = CARTESIAN_POINT ( 'NONE',  ( -16.83558968593882099, 66.05000000001261640, -190.8608022969076785 ) ) ;
#177347 = AXIS2_PLACEMENT_3D ( 'NONE', #209322, #129790, #170260 ) ;
#177348 = PRODUCT_CONTEXT ( 'NONE', #190631, 'mechanical' ) ;
#177349 = CARTESIAN_POINT ( 'NONE',  ( -18.47079683080346513, 85.47166410525677804, -95.91424694353177927 ) ) ;
#177350 = AXIS2_PLACEMENT_3D ( 'NONE', #167388, #68264, #244312 ) ;
#177351 = VERTEX_POINT ( 'NONE', #101203 ) ;
#177352 = DIRECTION ( 'NONE',  ( 1.000000000000000000, 0.000000000000000000, 0.000000000000000000 ) ) ;
#177353 = LINE ( 'NONE', #117345, #46543 ) ;
#177354 = SURFACE_STYLE_FILL_AREA ( #116073 ) ;
#177355 = ORIENTED_EDGE ( 'NONE', *, *, #113697, .F. ) ;
#177356 = CIRCLE ( 'NONE', #152220, 4.299999999999970512 ) ;
#177357 = VERTEX_POINT ( 'NONE', #80371 ) ;
#177358 = DIRECTION ( 'NONE',  ( -1.000000000000000000, -7.709882115452463178E-15, 0.000000000000000000 ) ) ;
#177359 = CARTESIAN_POINT ( 'NONE',  ( 21.05281448260627641, 8.776010158548784190, -45.67355791181142166 ) ) ;
#177360 = CARTESIAN_POINT ( 'NONE',  ( -18.50000000000000000, 14.80545736607782814, -235.9842437978701639 ) ) ;
#177361 = DIRECTION ( 'NONE',  ( -0.000000000000000000, 0.9126074666063770380, 0.4088369013363281068 ) ) ;
#177362 = CARTESIAN_POINT ( 'NONE',  ( 18.49999999999999289, 10.37342005529114886, -125.2657881246251037 ) ) ;
#177364 = DIRECTION ( 'NONE',  ( 0.000000000000000000, 1.000000000000000000, 0.000000000000000000 ) ) ;
#177363 = CARTESIAN_POINT ( 'NONE',  ( 21.04999999999999716, -1.391858308744753359, -194.6091531227728524 ) ) ;
#177365 = DIRECTION ( 'NONE',  ( 0.000000000000000000, 0.000000000000000000, 1.000000000000000000 ) ) ;
#177366 = PLANE ( 'NONE',  #43710 ) ;
#177367 = CARTESIAN_POINT ( 'NONE',  ( 18.57399277249656322, 65.66887361445283489, -30.43298459182692639 ) ) ;
#177368 = DIRECTION ( 'NONE',  ( -1.000000000000000000, -0.000000000000000000, -0.000000000000000000 ) ) ;
#177369 = ORIENTED_EDGE ( 'NONE', *, *, #15029, .T. ) ;
#177370 = AXIS2_PLACEMENT_3D ( 'NONE', #40006, #119527, #199049 ) ;
#177371 = ADVANCED_FACE ( 'NONE', ( #17850 ), #176971, .F. ) ;
#177372 = EDGE_LOOP ( 'NONE', ( #4437, #51714, #138998, #193244 ) ) ;
#177373 = CIRCLE ( 'NONE', #119076, 0.1000000000000028644 ) ;
#177375 = DIRECTION ( 'NONE',  ( 0.000000000000000000, 1.000000000000000000, 0.000000000000000000 ) ) ;
#177374 = VECTOR ( 'NONE', #75947, 1000.000000000000000 ) ;
#177376 = CARTESIAN_POINT ( 'NONE',  ( 21.05000000000000071, 1.115600667400684642E-11, -163.1999999999999602 ) ) ;
#177378 = LINE ( 'NONE', #44262, #257648 ) ;
#177377 = FACE_OUTER_BOUND ( 'NONE', #46053, .T. ) ;
#177379 = CYLINDRICAL_SURFACE ( 'NONE', #147643, 0.1000000000000078187 ) ;
#177380 = DIRECTION ( 'NONE',  ( 1.000000000000000000, 0.000000000000000000, 0.000000000000000000 ) ) ;
#177382 = ADVANCED_FACE ( 'NONE', ( #217325 ), #256405, .F. ) ;
#177381 = CARTESIAN_POINT ( 'NONE',  ( 13.12229106158773639, 13.10213769539062412, -216.8429874065679144 ) ) ;
#177383 = EDGE_LOOP ( 'NONE', ( #137059, #245474, #64933, #205660 ) ) ;
#177384 = EDGE_LOOP ( 'NONE', ( #103980, #11688, #110124, #70899 ) ) ;
#177385 = EDGE_CURVE ( 'NONE', #203793, #256334, #115582, .T. ) ;
#177386 = EDGE_CURVE ( 'NONE', #165923, #220397, #94733, .T. ) ;
#177387 = LINE ( 'NONE', #134352, #176016 ) ;
#177388 = EDGE_LOOP ( 'NONE', ( #74844, #77272, #173844, #113575 ) ) ;
#177389 = AXIS2_PLACEMENT_3D ( 'NONE', #83854, #81296, #121768 ) ;
#177390 = CARTESIAN_POINT ( 'NONE',  ( -33.72168855820452649, 64.52683809664941350, -93.77310748452440237 ) ) ;
#177391 = CIRCLE ( 'NONE', #98028, 0.9750000000000036415 ) ;
#177392 = ORIENTED_EDGE ( 'NONE', *, *, #245653, .F. ) ;
#177393 = CARTESIAN_POINT ( 'NONE',  ( -17.11825945287482753, 66.05000000001260219, -190.8731074845243825 ) ) ;
#177394 = EDGE_CURVE ( 'NONE', #118040, #178378, #36523, .T. ) ;
#177395 = VERTEX_POINT ( 'NONE', #196490 ) ;
#177396 = DIRECTION ( 'NONE',  ( 1.000000000000000000, 0.000000000000000000, 0.000000000000000000 ) ) ;
#177397 = CARTESIAN_POINT ( 'NONE',  ( 21.05000000000000071, -0.09999999998884338825, -26.95934304829875927 ) ) ;
#177398 = DIRECTION ( 'NONE',  ( 0.000000000000000000, 6.982962677686266711E-15, -1.000000000000000000 ) ) ;
#177399 = DIRECTION ( 'NONE',  ( 1.000000000000000000, 0.000000000000000000, -0.000000000000000000 ) ) ;
#177400 = CARTESIAN_POINT ( 'NONE',  ( 21.04999999999978755, 65.55631946098660023, -241.9747880272848022 ) ) ;
#177402 = CARTESIAN_POINT ( 'NONE',  ( -20.54999999999999716, 74.00000000001259082, -190.2984855617622770 ) ) ;
#177401 = FACE_OUTER_BOUND ( 'NONE', #240362, .T. ) ;
#177403 = CARTESIAN_POINT ( 'NONE',  ( 18.59999999999999076, 6.650000000011155876, -155.2500000000000284 ) ) ;
#177404 = ORIENTED_EDGE ( 'NONE', *, *, #157665, .T. ) ;
#177406 = DIRECTION ( 'NONE',  ( 0.000000000000000000, -0.9651348961780373825, 0.2617529984153167399 ) ) ;
#177405 = DIRECTION ( 'NONE',  ( 0.000000000000000000, 0.000000000000000000, -1.000000000000000000 ) ) ;
#177407 = ORIENTED_EDGE ( 'NONE', *, *, #212202, .F. ) ;
#177409 = ORIENTED_EDGE ( 'NONE', *, *, #197116, .T. ) ;
#177408 = DIRECTION ( 'NONE',  ( 1.000000000000000000, 0.000000000000000000, 0.000000000000000000 ) ) ;
#177410 = AXIS2_PLACEMENT_3D ( 'NONE', #129394, #128116, #13304 ) ;
#177411 = VERTEX_POINT ( 'NONE', #58258 ) ;
#177412 = FACE_OUTER_BOUND ( 'NONE', #25825, .T. ) ;
#177413 = CARTESIAN_POINT ( 'NONE',  ( -21.53699400385237794, 1.034126895667923527E-11, -26.71228820676542526 ) ) ;
#177414 = CARTESIAN_POINT ( 'NONE',  ( -23.15000000000000213, 85.00000000001179501, -78.81707660717668773 ) ) ;
#177415 = CARTESIAN_POINT ( 'NONE',  ( -17.27223548802031061, 22.03327853370796419, -229.9804127912456693 ) ) ;
#177416 = VERTEX_POINT ( 'NONE', #182082 ) ;
#177417 = EDGE_CURVE ( 'NONE', #239144, #104754, #116968, .T. ) ;
#177419 = EDGE_CURVE ( 'NONE', #158708, #134756, #44686, .T. ) ;
#177418 = CARTESIAN_POINT ( 'NONE',  ( -23.15000000000000213, 76.00000000001213607, -136.5231074845243313 ) ) ;
#177420 = CARTESIAN_POINT ( 'NONE',  ( 21.04105312098514347, 8.875332623054768888, -112.8285067472120602 ) ) ;
#177421 = CARTESIAN_POINT ( 'NONE',  ( 22.59066674512274986, 64.25000000001267608, -203.5536116081545970 ) ) ;
#177422 = ORIENTED_EDGE ( 'NONE', *, *, #105509, .F. ) ;
#177423 = LINE ( 'NONE', #251789, #210833 ) ;
#177424 = ADVANCED_FACE ( 'NONE', ( #98640 ), #21969, .T. ) ;
#177426 = TOROIDAL_SURFACE ( 'NONE', #35763, 11.90000000000000213, 0.1000000000000000056 ) ;
#177425 = DIRECTION ( 'NONE',  ( -1.000000000000000000, -0.000000000000000000, -0.000000000000000000 ) ) ;
#177427 = ORIENTED_EDGE ( 'NONE', *, *, #185841, .T. ) ;
#177428 = VERTEX_POINT ( 'NONE', #85496 ) ;
#177430 = CARTESIAN_POINT ( 'NONE',  ( -23.15000000000000213, 1.148907358139439339E-11, -201.0000000000015064 ) ) ;
#177429 = VECTOR ( 'NONE', #217159, 1000.000000000000000 ) ;
#177431 = CIRCLE ( 'NONE', #193980, 0.5000000000000004441 ) ;
#177432 = AXIS2_PLACEMENT_3D ( 'NONE', #72964, #148633, #49520 ) ;
#177433 = ORIENTED_EDGE ( 'NONE', *, *, #126812, .F. ) ;
#177434 = CARTESIAN_POINT ( 'NONE',  ( -18.44085059012131822, 11.51401249348379530, -9.259694680878462592 ) ) ;
#177435 = ORIENTED_EDGE ( 'NONE', *, *, #257364, .T. ) ;
#177436 = FACE_OUTER_BOUND ( 'NONE', #137383, .T. ) ;
#177437 =( BOUNDED_CURVE ( )  B_SPLINE_CURVE ( 3, ( #151461, #251819, #250534, #190589 ),
 .UNSPECIFIED., .F., .T. ) 
 B_SPLINE_CURVE_WITH_KNOTS ( ( 4, 4 ),
 ( 0.3000847527772366186, 0.5497968875596810356 ),
 .UNSPECIFIED. ) 
 CURVE ( )  GEOMETRIC_REPRESENTATION_ITEM ( )  RATIONAL_B_SPLINE_CURVE ( ( 1.000000000000000000, 0.9948104011409419911, 0.9948104011409419911, 1.000000000000000000 ) ) 
 REPRESENTATION_ITEM ( '' )  );
#177438 = COLOUR_RGB ( '', 0.08235294, 0.09019608, 0.10196078) ;
#177439 = CARTESIAN_POINT ( 'NONE',  ( -20.65000000000000568, 7.250000000011138646, -79.65000000000004832 ) ) ;
#177440 = CARTESIAN_POINT ( 'NONE',  ( -20.94999999999999929, 77.26178616857734482, -161.9366085209788650 ) ) ;
#177441 = PLANE ( 'NONE',  #103871 ) ;
#177442 = EDGE_CURVE ( 'NONE', #236989, #208046, #119701, .T. ) ;
#177443 = DIRECTION ( 'NONE',  ( 0.000000000000000000, 0.9651348961777157509, -0.2617529984165031243 ) ) ;
#177444 = CARTESIAN_POINT ( 'NONE',  ( -21.08198257630413508, 0.07264332379574613141, -27.16340326598493604 ) ) ;
#177445 = PLANE ( 'NONE',  #193322 ) ;
#177446 = ORIENTED_EDGE ( 'NONE', *, *, #179705, .T. ) ;
#177448 = CARTESIAN_POINT ( 'NONE',  ( 23.14999999999999858, 53.62064951147646497, -235.8162552129080609 ) ) ;
#177447 = CARTESIAN_POINT ( 'NONE',  ( -23.25000000000000000, 87.75000000001192291, -99.92310748452422331 ) ) ;
#177449 = ORIENTED_EDGE ( 'NONE', *, *, #17876, .T. ) ;
#177452 = ORIENTED_EDGE ( 'NONE', *, *, #32247, .F. ) ;
#177451 = DIRECTION ( 'NONE',  ( -1.000000000000000000, -1.541880601228652843E-16, -2.878400969107353907E-16 ) ) ;
#177450 = CARTESIAN_POINT ( 'NONE',  ( -18.59999999999999787, 66.65000000001222702, -148.6731074845244223 ) ) ;
#177453 = VERTEX_POINT ( 'NONE', #165076 ) ;
#177454 = DIRECTION ( 'NONE',  ( -1.000000000000000000, 0.000000000000000000, 0.000000000000000000 ) ) ;
#177455 = AXIS2_PLACEMENT_3D ( 'NONE', #172975, #152112, #37293 ) ;
#177456 = DIRECTION ( 'NONE',  ( 0.000000000000000000, 0.2617529984165031243, 0.9651348961777157509 ) ) ;
#177457 = ADVANCED_FACE ( 'NONE', ( #67257 ), #47674, .T. ) ;
#177458 = DIRECTION ( 'NONE',  ( 0.000000000000000000, 0.000000000000000000, 1.000000000000000000 ) ) ;
#177459 = ORIENTED_EDGE ( 'NONE', *, *, #6445, .T. ) ;
#177460 = CARTESIAN_POINT ( 'NONE',  ( -23.15000000000000213, -11.41227409413852811, -131.0000000000000284 ) ) ;
#177461 = CIRCLE ( 'NONE', #19205, 0.09999999999998898659 ) ;
#177462 = CYLINDRICAL_SURFACE ( 'NONE', #190284, 0.09999999999998898659 ) ;
#177463 = AXIS2_PLACEMENT_3D ( 'NONE', #186061, #248599, #25704 ) ;
#177464 = EDGE_CURVE ( 'NONE', #22716, #107478, #123389, .T. ) ;
#177466 = CARTESIAN_POINT ( 'NONE',  ( 20.95265033839679347, 10.51225083246715819, -7.565763756029960874 ) ) ;
#177465 = LINE ( 'NONE', #256915, #67909 ) ;
#177467 = EDGE_CURVE ( 'NONE', #254486, #246750, #215546, .T. ) ;
#177468 = AXIS2_PLACEMENT_3D ( 'NONE', #186502, #249052, #152536 ) ;
#177470 = VERTEX_POINT ( 'NONE', #226307 ) ;
#177469 = CARTESIAN_POINT ( 'NONE',  ( 20.94999999999999929, 1.835341550235569663, -112.0551512925630249 ) ) ;
#177471 = VERTEX_POINT ( 'NONE', #168974 ) ;
#177474 = EDGE_CURVE ( 'NONE', #163992, #163656, #225025, .T. ) ;
#177473 = EDGE_CURVE ( 'NONE', #15038, #212171, #173911, .T. ) ;
#177472 = B_SPLINE_CURVE_WITH_KNOTS ( 'NONE', 3,
 ( #38049, #194559, #97965, #160565, #134531, #96673, #177574, #78421, #158019, #237517, #217917, #101813, #242631, #121446, #6592, #144806 ),
 .UNSPECIFIED., .F., .F.,
 ( 4, 3, 3, 3, 3, 4 ),
 ( 0.000000000000000000, 3.357088238235017585E-05, 6.714213034886951743E-05, 0.0001007408646120965597, 0.0001343627955914321564, 0.0001573956632896059723 ),
 .UNSPECIFIED. ) ;
#177475 = TOROIDAL_SURFACE ( 'NONE', #210753, 11.70000000000000639, 0.1000000000000000056 ) ;
#177476 = DIRECTION ( 'NONE',  ( -1.000000000000000000, -0.000000000000000000, 0.000000000000000000 ) ) ;
#177478 = EDGE_CURVE ( 'NONE', #120061, #24865, #187230, .T. ) ;
#177477 = EDGE_LOOP ( 'NONE', ( #166448, #52440, #211877, #103073 ) ) ;
#177479 = DIRECTION ( 'NONE',  ( 0.000000000000000000, 0.000000000000000000, -1.000000000000000000 ) ) ;
#177480 = ORIENTED_EDGE ( 'NONE', *, *, #123595, .T. ) ;
#177481 = TOROIDAL_SURFACE ( 'NONE', #139832, 1.900000000000002576, 0.1000000000000000056 ) ;
#177482 = DIRECTION ( 'NONE',  ( 0.7071067811865493491, -0.7071067811865456854, -4.937700262164518065E-15 ) ) ;
#177483 = DIRECTION ( 'NONE',  ( -2.952720810173288619E-16, 0.4721928772777346239, 0.8814952561688430555 ) ) ;
#177484 = LINE ( 'NONE', #79, #68340 ) ;
#177485 = ADVANCED_FACE ( 'NONE', ( #107663 ), #77979, .F. ) ;
#177487 = VERTEX_POINT ( 'NONE', #163806 ) ;
#177486 = AXIS2_PLACEMENT_3D ( 'NONE', #81547, #21619, #161127 ) ;
#177488 = CYLINDRICAL_SURFACE ( 'NONE', #125313, 11.80000000000000426 ) ;
#177489 = EDGE_CURVE ( 'NONE', #257228, #162975, #82236, .T. ) ;
#177490 = AXIS2_PLACEMENT_3D ( 'NONE', #181364, #28401, #120122 ) ;
#177491 = CARTESIAN_POINT ( 'NONE',  ( 20.94999999999999929, -11.64999999998883595, -167.5000000000000000 ) ) ;
#177492 = EDGE_CURVE ( 'NONE', #139895, #116521, #65510, .T. ) ;
#177493 = EDGE_CURVE ( 'NONE', #23304, #200329, #182236, .T. ) ;
#177494 = ORIENTED_EDGE ( 'NONE', *, *, #98510, .F. ) ;
#177495 = ORIENTED_EDGE ( 'NONE', *, *, #100397, .F. ) ;
#177496 = DIRECTION ( 'NONE',  ( 0.000000000000000000, -1.000000000000000000, -1.734723475976807292E-15 ) ) ;
#177497 = ORIENTED_EDGE ( 'NONE', *, *, #240113, .F. ) ;
#177498 = EDGE_CURVE ( 'NONE', #108264, #65247, #68551, .T. ) ;
#177499 = ORIENTED_EDGE ( 'NONE', *, *, #21791, .F. ) ;
#177501 = VERTEX_POINT ( 'NONE', #245907 ) ;
#177500 = CARTESIAN_POINT ( 'NONE',  ( 18.59999999999998721, 6.846123162363745074, -171.2377262668498759 ) ) ;
#177503 = EDGE_CURVE ( 'NONE', #241360, #57517, #219631, .T. ) ;
#177502 = ORIENTED_EDGE ( 'NONE', *, *, #185848, .T. ) ;
#177504 = AXIS2_PLACEMENT_3D ( 'NONE', #41470, #6148, #85661 ) ;
#177505 = EDGE_CURVE ( 'NONE', #120691, #154671, #227608, .T. ) ;
#177506 = CIRCLE ( 'NONE', #227522, 11.75000000000000178 ) ;
#177509 = ORIENTED_EDGE ( 'NONE', *, *, #178791, .T. ) ;
#177508 = ORIENTED_EDGE ( 'NONE', *, *, #55907, .T. ) ;
#177507 = SPHERICAL_SURFACE ( 'NONE', #27081, 0.1000000000000000056 ) ;
#177510 = CIRCLE ( 'NONE', #194258, 0.1000000000000003525 ) ;
#177511 = AXIS2_PLACEMENT_3D ( 'NONE', #257545, #241888, #159807 ) ;
#177512 = EDGE_CURVE ( 'NONE', #232566, #219655, #223749, .T. ) ;
#177513 = ORIENTED_EDGE ( 'NONE', *, *, #218457, .T. ) ;
#177514 = DIRECTION ( 'NONE',  ( 0.000000000000000000, 0.000000000000000000, -1.000000000000000000 ) ) ;
#177515 = CARTESIAN_POINT ( 'NONE',  ( -18.59999999999999787, 74.25000000001229239, -158.3535959266227451 ) ) ;
#177516 = CIRCLE ( 'NONE', #252283, 3.900000000000000799 ) ;
#177517 = CARTESIAN_POINT ( 'NONE',  ( -16.80621392010919735, 14.14295755150341627, -219.2180467217198725 ) ) ;
#177518 = VERTEX_POINT ( 'NONE', #205474 ) ;
#177519 = FACE_OUTER_BOUND ( 'NONE', #244042, .T. ) ;
#177521 = ORIENTED_EDGE ( 'NONE', *, *, #129763, .F. ) ;
#177520 = DIRECTION ( 'NONE',  ( 1.000000000000000000, 0.000000000000000000, 0.000000000000000000 ) ) ;
#177522 = DIRECTION ( 'NONE',  ( 1.000000000000000000, -0.000000000000000000, -0.000000000000000000 ) ) ;
#177524 = VERTEX_POINT ( 'NONE', #5984 ) ;
#177523 = DIRECTION ( 'NONE',  ( 1.000000000000000000, 0.000000000000000000, 0.000000000000000000 ) ) ;
#177525 = EDGE_CURVE ( 'NONE', #250352, #210177, #252958, .T. ) ;
#177526 = CIRCLE ( 'NONE', #123321, 0.1000000000000028644 ) ;
#177527 = ORIENTED_EDGE ( 'NONE', *, *, #185221, .F. ) ;
#177528 = ADVANCED_FACE ( 'NONE', ( #26879 ), #24033, .T. ) ;
#177529 = AXIS2_PLACEMENT_3D ( 'NONE', #61862, #64431, #141383 ) ;
#177530 = CARTESIAN_POINT ( 'NONE',  ( 23.14999999999999147, 0.000000000000000000, 0.000000000000000000 ) ) ;
#177531 = DIRECTION ( 'NONE',  ( 0.000000000000000000, 0.000000000000000000, -1.000000000000000000 ) ) ;
#177532 = TOROIDAL_SURFACE ( 'NONE', #165009, 11.65000000000000036, 0.1000000000000000056 ) ;
#177533 = ORIENTED_EDGE ( 'NONE', *, *, #244501, .T. ) ;
#177534 = ORIENTED_EDGE ( 'NONE', *, *, #252009, .T. ) ;
#177535 = DIRECTION ( 'NONE',  ( -1.000000000000000000, 0.000000000000000000, 0.000000000000000000 ) ) ;
#177536 = DIRECTION ( 'NONE',  ( -1.000000000000000000, 0.000000000000000000, 0.000000000000000000 ) ) ;
#177538 = ORIENTED_EDGE ( 'NONE', *, *, #124477, .F. ) ;
#177537 = VERTEX_POINT ( 'NONE', #30732 ) ;
#177539 = ORIENTED_EDGE ( 'NONE', *, *, #185193, .F. ) ;
#177540 = CARTESIAN_POINT ( 'NONE',  ( 21.12802099929860944, 61.96285729424215560, -221.7356349687620138 ) ) ;
#177541 = ORIENTED_EDGE ( 'NONE', *, *, #29759, .T. ) ;
#177542 = ORIENTED_EDGE ( 'NONE', *, *, #173421, .F. ) ;
#177543 = FACE_OUTER_BOUND ( 'NONE', #132531, .T. ) ;
#177544 = AXIS2_PLACEMENT_3D ( 'NONE', #118491, #139292, #179741 ) ;
#177545 = ORIENTED_EDGE ( 'NONE', *, *, #168214, .F. ) ;
#177546 = CARTESIAN_POINT ( 'NONE',  ( -18.40000000000000213, 5.649999999999983480, -20.85000000000000142 ) ) ;
#177548 = FACE_OUTER_BOUND ( 'NONE', #223411, .T. ) ;
#177547 = CARTESIAN_POINT ( 'NONE',  ( 23.14999999999998437, 1.115600667400684642E-11, -167.4999999999999716 ) ) ;
#177549 = EDGE_LOOP ( 'NONE', ( #191086, #183906, #65962, #44333 ) ) ;
#177551 = VERTEX_POINT ( 'NONE', #133649 ) ;
#177550 = ORIENTED_EDGE ( 'NONE', *, *, #216681, .T. ) ;
#177552 = CARTESIAN_POINT ( 'NONE',  ( -21.05000000000000071, 76.10000000001272724, -210.0637644362255969 ) ) ;
#177554 = ADVANCED_FACE ( 'NONE', ( #210619 ), #61429, .T. ) ;
#177553 = DIRECTION ( 'NONE',  ( 0.000000000000000000, -1.000000000000000000, 0.000000000000000000 ) ) ;
#177555 = ORIENTED_EDGE ( 'NONE', *, *, #81865, .F. ) ;
#177556 = VECTOR ( 'NONE', #103478, 1000.000000000000000 ) ;
#177557 = AXIS2_PLACEMENT_3D ( 'NONE', #34868, #253866, #154814 ) ;
#177558 = EDGE_CURVE ( 'NONE', #164661, #250321, #161396, .T. ) ;
#177559 = CIRCLE ( 'NONE', #10941, 11.89999999999999858 ) ;
#177560 = CIRCLE ( 'NONE', #135991, 0.09999999999998898659 ) ;
#177561 = DIRECTION ( 'NONE',  ( -1.000000000000000000, 2.952720810173289112E-16, 2.061873921506763405E-30 ) ) ;
#177562 = EDGE_LOOP ( 'NONE', ( #189153, #105247, #41311, #26184 ) ) ;
#177563 = ORIENTED_EDGE ( 'NONE', *, *, #171593, .F. ) ;
#177564 = DIRECTION ( 'NONE',  ( 0.000000000000000000, -0.5341055959866798375, 0.8454177738465836756 ) ) ;
#177565 = VERTEX_POINT ( 'NONE', #131078 ) ;
#177566 = CARTESIAN_POINT ( 'NONE',  ( -21.05000000000000071, 0.000000000000000000, 0.000000000000000000 ) ) ;
#177567 = ORIENTED_EDGE ( 'NONE', *, *, #53986, .T. ) ;
#177568 = DIRECTION ( 'NONE',  ( 1.000000000000000000, 0.000000000000000000, 0.000000000000000000 ) ) ;
#177569 = CARTESIAN_POINT ( 'NONE',  ( -20.94999999999999929, -1.835341550213255957, -145.5551512925629822 ) ) ;
#177571 = DIRECTION ( 'NONE',  ( -1.000000000000000000, -0.000000000000000000, 0.000000000000000000 ) ) ;
#177570 = CARTESIAN_POINT ( 'NONE',  ( -20.54999999999999716, 1.925233644870972816, -46.23024353312612789 ) ) ;
#177572 = FACE_OUTER_BOUND ( 'NONE', #55777, .T. ) ;
#177573 = LINE ( 'NONE', #154162, #224665 ) ;
#177574 = CARTESIAN_POINT ( 'NONE',  ( 21.07189867249812210, 65.27501972991913703, -157.8106560422477003 ) ) ;
#177575 = CARTESIAN_POINT ( 'NONE',  ( -16.85312964099708566, 66.08639531794450761, -149.4202917780939686 ) ) ;
#177576 = DIRECTION ( 'NONE',  ( 0.000000000000000000, 0.000000000000000000, -1.000000000000000000 ) ) ;
#177577 = CARTESIAN_POINT ( 'NONE',  ( 20.95000000000005258, 64.25000000001119815, -6.123107484524794586 ) ) ;
#177578 = TOROIDAL_SURFACE ( 'NONE', #181643, 3.899999999999999467, 0.1000000000000000056 ) ;
#177579 = EDGE_CURVE ( 'NONE', #138331, #201908, #169801, .T. ) ;
#177580 = CIRCLE ( 'NONE', #252348, 0.1999999999999987899 ) ;
#177581 = ORIENTED_EDGE ( 'NONE', *, *, #201790, .F. ) ;
#177583 = ORIENTED_EDGE ( 'NONE', *, *, #75736, .T. ) ;
#177582 = ORIENTED_EDGE ( 'NONE', *, *, #166259, .T. ) ;
#177584 = CIRCLE ( 'NONE', #2555, 0.09999999999999939493 ) ;
#177585 = ORIENTED_EDGE ( 'NONE', *, *, #178669, .F. ) ;
#177586 = VERTEX_POINT ( 'NONE', #150651 ) ;
#177587 = CYLINDRICAL_SURFACE ( 'NONE', #82110, 0.09999999999999939493 ) ;
#177588 = DIRECTION ( 'NONE',  ( -1.000000000000000000, 0.000000000000000000, 0.000000000000000000 ) ) ;
#177590 = CARTESIAN_POINT ( 'NONE',  ( 18.59999999999999076, 63.62814136979439184, -224.4990371885399441 ) ) ;
#177589 = CARTESIAN_POINT ( 'NONE',  ( -21.55000000000000426, 68.29142135624881860, -48.37310748452437537 ) ) ;
#177591 = ORIENTED_EDGE ( 'NONE', *, *, #93729, .F. ) ;
#177592 = CARTESIAN_POINT ( 'NONE',  ( -23.15000000000000213, 85.00000000001149658, -45.41707660717669626 ) ) ;
#177593 = PRESENTATION_STYLE_ASSIGNMENT (( #38066 ) ) ;
#177594 = DIRECTION ( 'NONE',  ( 1.186688945009009831E-16, 1.000000000000000000, 6.982962677686266711E-15 ) ) ;
#177595 = DIRECTION ( 'NONE',  ( 1.000000000000000000, 0.000000000000000000, -0.000000000000000000 ) ) ;
#177596 = DIRECTION ( 'NONE',  ( 0.000000000000000000, 0.000000000000000000, -1.000000000000000000 ) ) ;
#177597 = ORIENTED_EDGE ( 'NONE', *, *, #244473, .T. ) ;
#177598 = AXIS2_PLACEMENT_3D ( 'NONE', #106942, #108249, #186504 ) ;
#177599 = EDGE_LOOP ( 'NONE', ( #222085, #165787, #147772, #205850 ) ) ;
#177600 = CYLINDRICAL_SURFACE ( 'NONE', #245476, 0.1000000000000028644 ) ;
#177601 = CARTESIAN_POINT ( 'NONE',  ( 20.05000000000002913, 7.250000000000015099, -12.65000000000000391 ) ) ;
#177602 = DIRECTION ( 'NONE',  ( 0.000000000000000000, -7.086529944415886769E-15, 1.000000000000000000 ) ) ;
#177603 = CYLINDRICAL_SURFACE ( 'NONE', #158519, 1.749999999999998002 ) ;
#177604 = ORIENTED_EDGE ( 'NONE', *, *, #209430, .F. ) ;
#177605 = LINE ( 'NONE', #56320, #219457 ) ;
#177607 = EDGE_CURVE ( 'NONE', #50042, #138896, #190456, .T. ) ;
#177606 = DIRECTION ( 'NONE',  ( -1.000000000000000000, -0.000000000000000000, 0.000000000000000000 ) ) ;
#177608 = DIRECTION ( 'NONE',  ( -1.000000000000000000, -0.000000000000000000, -0.000000000000000000 ) ) ;
#177609 = CARTESIAN_POINT ( 'NONE',  ( 23.24999999999999645, 67.17743825834622839, -194.2731074845244166 ) ) ;
#177610 = LINE ( 'NONE', #135860, #41392 ) ;
#177611 = EDGE_CURVE ( 'NONE', #7452, #197017, #194929, .T. ) ;
#177612 = TOROIDAL_SURFACE ( 'NONE', #77587, 0.2000000000000000111, 0.1000000000000000056 ) ;
#177613 = CARTESIAN_POINT ( 'NONE',  ( -21.44999999999999929, 63.37018259659601682, -222.0118260003222872 ) ) ;
#177614 = DIRECTION ( 'NONE',  ( 0.000000000000000000, 0.2128009952263485993, -0.9770955615653341697 ) ) ;
#177615 = DIRECTION ( 'NONE',  ( 0.000000000000000000, -0.1495327102803078179, 0.9887567792719429427 ) ) ;
#177616 = AXIS2_PLACEMENT_3D ( 'NONE', #191130, #175421, #72457 ) ;
#177617 = VERTEX_POINT ( 'NONE', #230180 ) ;
#177618 = CIRCLE ( 'NONE', #90076, 0.09999999999999976963 ) ;
#177620 = VERTEX_POINT ( 'NONE', #90660 ) ;
#177619 = PRESENTATION_LAYER_ASSIGNMENT (  '', '', ( #256625 ) ) ;
#177621 = EDGE_CURVE ( 'NONE', #121432, #211306, #157311, .T. ) ;
#177622 = LINE ( 'NONE', #257069, #90383 ) ;
#177623 = VERTEX_POINT ( 'NONE', #171527 ) ;
#177624 = EDGE_CURVE ( 'NONE', #75581, #86050, #175377, .T. ) ;
#177625 = DIRECTION ( 'NONE',  ( -0.000000000000000000, 0.4088369013363281623, -0.9126074666063771490 ) ) ;
#177626 = CARTESIAN_POINT ( 'NONE',  ( -18.58693740092132884, -9.406432150241801793, -174.6248164565013496 ) ) ;
#177627 = ADVANCED_FACE ( 'NONE', ( #149392 ), #91953, .T. ) ;
#177628 = LINE ( 'NONE', #216714, #133589 ) ;
#177629 = CIRCLE ( 'NONE', #73575, 0.1000000000000009492 ) ;
#177630 = VERTEX_POINT ( 'NONE', #251006 ) ;
#177631 = PLANE ( 'NONE',  #155604 ) ;
#177632 = VECTOR ( 'NONE', #55208, 1000.000000000000000 ) ;
#177633 = DIRECTION ( 'NONE',  ( 1.000000000000000000, 0.000000000000000000, -0.000000000000000000 ) ) ;
#177634 = CARTESIAN_POINT ( 'NONE',  ( -20.85000000000000142, 1.115600667400684642E-11, -167.5000000000000284 ) ) ;
#177635 = CARTESIAN_POINT ( 'NONE',  ( -21.05000000000000071, 76.10000000001245724, -181.6726782920691505 ) ) ;
#177638 = ORIENTED_EDGE ( 'NONE', *, *, #30353, .F. ) ;
#177637 = CARTESIAN_POINT ( 'NONE',  ( -16.89155683852479228, 9.950000000011138823, -187.7226281504588599 ) ) ;
#177636 = VECTOR ( 'NONE', #229355, 1000.000000000000000 ) ;
#177640 = CARTESIAN_POINT ( 'NONE',  ( 20.85000000000000142, 11.75000000001115907, -200.9999999999999432 ) ) ;
#177639 = FACE_OUTER_BOUND ( 'NONE', #73422, .T. ) ;
#177641 = EDGE_CURVE ( 'NONE', #121114, #81429, #65702, .T. ) ;
#177642 = PLANE ( 'NONE',  #44494 ) ;
#177643 = DIRECTION ( 'NONE',  ( -1.000000000000000000, -0.000000000000000000, -0.000000000000000000 ) ) ;
#177644 = CIRCLE ( 'NONE', #181889, 0.09999999999999939493 ) ;
#177645 = DIRECTION ( 'NONE',  ( -3.265361837132813093E-16, -1.000000000000000000, -6.982962677686266711E-15 ) ) ;
#177646 = LINE ( 'NONE', #55067, #4241 ) ;
#177648 = ORIENTED_EDGE ( 'NONE', *, *, #62336, .F. ) ;
#177647 = AXIS2_PLACEMENT_3D ( 'NONE', #16855, #96353, #179456 ) ;
#177649 =( NAMED_UNIT ( * ) PLANE_ANGLE_UNIT ( ) SI_UNIT ( $, .RADIAN. ) );
#177650 = CARTESIAN_POINT ( 'NONE',  ( -23.25000000000000000, 78.57160958314655375, -238.9307242378722833 ) ) ;
#177651 = VERTEX_POINT ( 'NONE', #50243 ) ;
#177652 = LINE ( 'NONE', #237599, #248623 ) ;
#177653 = ORIENTED_EDGE ( 'NONE', *, *, #95664, .T. ) ;
#177654 = CIRCLE ( 'NONE', #115259, 4.000000000000002665 ) ;
#177655 = CARTESIAN_POINT ( 'NONE',  ( 18.53691006697114929, 54.99043569302317280, -230.0501718883048738 ) ) ;
#177656 = AXIS2_PLACEMENT_3D ( 'NONE', #145477, #46369, #202891 ) ;
#177657 = AXIS2_PLACEMENT_3D ( 'NONE', #118332, #197845, #137860 ) ;
#177658 = FACE_OUTER_BOUND ( 'NONE', #23230, .T. ) ;
#177659 = DIRECTION ( 'NONE',  ( -0.000000000000000000, -0.4088369013363283844, 0.9126074666063769270 ) ) ;
#177660 = ORIENTED_EDGE ( 'NONE', *, *, #40866, .F. ) ;
#177661 = VERTEX_POINT ( 'NONE', #114075 ) ;
#177662 = DIRECTION ( 'NONE',  ( 0.000000000000000000, -0.4999999999999478195, -0.8660254037844686836 ) ) ;
#177663 = CYLINDRICAL_SURFACE ( 'NONE', #60950, 0.09999999999999939493 ) ;
#177664 = CARTESIAN_POINT ( 'NONE',  ( 18.39999999999999503, 70.35000000001261355, -190.8731074845244109 ) ) ;
#177665 = CARTESIAN_POINT ( 'NONE',  ( 21.00000000000000000, 0.000000000000000000, 0.000000000000000000 ) ) ;
#177666 = CIRCLE ( 'NONE', #206855, 0.09999999999999939493 ) ;
#177668 = CARTESIAN_POINT ( 'NONE',  ( -21.00000000000000000, 6.644425182197215562, 9.641788261573355001 ) ) ;
#177667 = CARTESIAN_POINT ( 'NONE',  ( -20.85000000000000142, 7.021664781911246322, -137.8335654018973457 ) ) ;
#177669 = LINE ( 'NONE', #2829, #156585 ) ;
#177670 = B_SPLINE_CURVE_WITH_KNOTS ( 'NONE', 3,
 ( #203472, #27437, #165638, #26123, #105615, #185186, #16835, #53376, #93775, #229451, #170812, #211167, #194192, #32569, #172079, #114631 ),
 .UNSPECIFIED., .F., .F.,
 ( 4, 3, 3, 3, 3, 4 ),
 ( 0.000000000000000000, 1.810570668010599751E-05, 2.740575833570006129E-05, 4.256816319434536945E-05, 5.213463471025743496E-05, 6.641585710718904932E-05 ),
 .UNSPECIFIED. ) ;
#177671 = CARTESIAN_POINT ( 'NONE',  ( 21.13461538461538325, 65.38541703798631488, -90.77310748452440237 ) ) ;
#177672 = DIRECTION ( 'NONE',  ( 0.000000000000000000, 4.440892098500570153E-15, -1.000000000000000000 ) ) ;
#177673 = ORIENTED_EDGE ( 'NONE', *, *, #25746, .F. ) ;
#177674 = LINE ( 'NONE', #182795, #202391 ) ;
#177675 = EDGE_CURVE ( 'NONE', #145277, #219574, #206793, .T. ) ;
#177677 = ORIENTED_EDGE ( 'NONE', *, *, #45405, .T. ) ;
#177676 = DIRECTION ( 'NONE',  ( 0.000000000000000000, -6.982962677686266711E-15, 1.000000000000000000 ) ) ;
#177678 = DIRECTION ( 'NONE',  ( 0.000000000000000000, 0.000000000000000000, 1.000000000000000000 ) ) ;
#177679 = DIRECTION ( 'NONE',  ( 0.000000000000000000, 0.000000000000000000, -1.000000000000000000 ) ) ;
#177680 = DIRECTION ( 'NONE',  ( 1.000000000000000000, 0.000000000000000000, 0.000000000000000000 ) ) ;
#177681 = ORIENTED_EDGE ( 'NONE', *, *, #185943, .T. ) ;
#177683 = DIRECTION ( 'NONE',  ( -1.000000000000000000, 0.000000000000000000, 0.000000000000000000 ) ) ;
#177682 = FACE_OUTER_BOUND ( 'NONE', #111159, .T. ) ;
#177684 = DIRECTION ( 'NONE',  ( -0.000000000000000000, -0.000000000000000000, -1.000000000000000000 ) ) ;
#177685 = DIRECTION ( 'NONE',  ( -0.000000000000000000, 0.1332476588733589318, -0.9910827722268049644 ) ) ;
#177686 = DIRECTION ( 'NONE',  ( -1.000000000000000000, 0.000000000000000000, -0.000000000000000000 ) ) ;
#177688 = ADVANCED_FACE ( 'NONE', ( #34572, #33309 ), #112809, .T. ) ;
#177687 = CARTESIAN_POINT ( 'NONE',  ( -18.54148534481894472, 10.32532329027886320, -139.5699343018359855 ) ) ;
#177689 = ORIENTED_EDGE ( 'NONE', *, *, #255406, .F. ) ;
#177690 = CARTESIAN_POINT ( 'NONE',  ( -22.49806830649814415, 31.82532512087596288, -238.9510566881495777 ) ) ;
#177691 = CIRCLE ( 'NONE', #52731, 0.09999999999999939493 ) ;
#177692 = ORIENTED_EDGE ( 'NONE', *, *, #166379, .F. ) ;
#177693 = EDGE_CURVE ( 'NONE', #113100, #40685, #252563, .T. ) ;
#177695 = ADVANCED_FACE ( 'NONE', ( #69851 ), #153254, .F. ) ;
#177694 = AXIS2_PLACEMENT_3D ( 'NONE', #26512, #85145, #65614 ) ;
#177696 = CIRCLE ( 'NONE', #181752, 12.77500000000000036 ) ;
#177697 = CARTESIAN_POINT ( 'NONE',  ( -18.46907102845853998, -9.473727364764107151, -40.17603473873652575 ) ) ;
#177698 = ORIENTED_EDGE ( 'NONE', *, *, #53569, .F. ) ;
#177699 = DIRECTION ( 'NONE',  ( 2.915501640297155269E-16, -1.000000000000000000, 0.000000000000000000 ) ) ;
#177700 = ORIENTED_EDGE ( 'NONE', *, *, #233901, .T. ) ;
#177701 = AXIS2_PLACEMENT_3D ( 'NONE', #174979, #30296, #109805 ) ;
#177702 = DIRECTION ( 'NONE',  ( -0.000000000000000000, -2.891205793294679805E-16, 1.000000000000000000 ) ) ;
#177703 = VERTEX_POINT ( 'NONE', #228906 ) ;
#177704 = EDGE_CURVE ( 'NONE', #108030, #28028, #130092, .T. ) ;
#177705 = CIRCLE ( 'NONE', #169522, 0.09999999999999939493 ) ;
#177706 = EDGE_CURVE ( 'NONE', #51884, #210178, #85954, .T. ) ;
#177708 = AXIS2_PLACEMENT_3D ( 'NONE', #146073, #130359, #28759 ) ;
#177707 = DIRECTION ( 'NONE',  ( 1.000000000000000000, 0.000000000000000000, 0.000000000000000000 ) ) ;
#177709 = DIRECTION ( 'NONE',  ( -0.000000000000000000, 1.000000000000000000, 6.982962677686266711E-15 ) ) ;
#177710 = AXIS2_PLACEMENT_3D ( 'NONE', #19547, #8958, #226706 ) ;
#177711 = PLANE ( 'NONE',  #141555 ) ;
#177712 = DIRECTION ( 'NONE',  ( -0.000000000000000000, 0.1350103645451649625, -0.9908441862701631297 ) ) ;
#177713 = CARTESIAN_POINT ( 'NONE',  ( 23.15000000000000213, 28.50120599808395028, -258.2149742250584268 ) ) ;
#177714 = ORIENTED_EDGE ( 'NONE', *, *, #180856, .T. ) ;
#177715 = DIRECTION ( 'NONE',  ( 0.000000000000000000, -0.4166553800442105437, 0.9090645160164456673 ) ) ;
#177716 = ORIENTED_EDGE ( 'NONE', *, *, #192182, .F. ) ;
#177718 = ORIENTED_EDGE ( 'NONE', *, *, #41232, .T. ) ;
#177717 = CARTESIAN_POINT ( 'NONE',  ( -23.15000000000000213, 17.01923898301589944, -224.3994341343041867 ) ) ;
#177719 = VERTEX_POINT ( 'NONE', #180487 ) ;
#177720 = FACE_OUTER_BOUND ( 'NONE', #223616, .T. ) ;
#177721 = DIRECTION ( 'NONE',  ( 1.000000000000000000, 2.952720810173289112E-16, -0.000000000000000000 ) ) ;
#177722 = CARTESIAN_POINT ( 'NONE',  ( -18.59999999999999787, 66.85000000001254250, -182.3731074845244393 ) ) ;
#177723 = EDGE_CURVE ( 'NONE', #208046, #246187, #94343, .T. ) ;
#177724 = DIRECTION ( 'NONE',  ( 0.000000000000000000, 0.000000000000000000, 1.000000000000000000 ) ) ;
#177726 = ORIENTED_EDGE ( 'NONE', *, *, #60144, .T. ) ;
#177725 = VECTOR ( 'NONE', #4616, 1000.000000000000000 ) ;
#177727 = EDGE_CURVE ( 'NONE', #95913, #185684, #98994, .T. ) ;
#177728 = EDGE_CURVE ( 'NONE', #185953, #224921, #78787, .T. ) ;
#177729 = FACE_OUTER_BOUND ( 'NONE', #5030, .T. ) ;
#177730 = DIRECTION ( 'NONE',  ( 1.000000000000000000, -2.952720810173289112E-16, -2.061873921506763405E-30 ) ) ;
#177731 = ORIENTED_EDGE ( 'NONE', *, *, #102143, .F. ) ;
#177733 = VERTEX_POINT ( 'NONE', #102188 ) ;
#177732 = FACE_OUTER_BOUND ( 'NONE', #221377, .T. ) ;
#177734 = DIRECTION ( 'NONE',  ( 0.000000000000000000, -0.8740096314914906905, 0.4859085964048265316 ) ) ;
#177735 = CARTESIAN_POINT ( 'NONE',  ( -16.97683809663752186, 9.950000000011137047, -80.40236401819653622 ) ) ;
#177736 = VECTOR ( 'NONE', #252969, 1000.000000000000114 ) ;
#177737 = EDGE_LOOP ( 'NONE', ( #153452, #223985, #6230 ) ) ;
#177738 = CIRCLE ( 'NONE', #144340, 0.09999999999999939493 ) ;
#177739 = VECTOR ( 'NONE', #106184, 1000.000000000000000 ) ;
#177740 = AXIS2_PLACEMENT_3D ( 'NONE', #157395, #195231, #255115 ) ;
#177741 = ORIENTED_EDGE ( 'NONE', *, *, #8687, .F. ) ;
#177742 = CARTESIAN_POINT ( 'NONE',  ( 23.24999999999997513, 64.25000000001219291, -143.5379132551784096 ) ) ;
#177743 = DIRECTION ( 'NONE',  ( -1.000000000000000000, 0.000000000000000000, 0.000000000000000000 ) ) ;
#177744 = CARTESIAN_POINT ( 'NONE',  ( 14.22916352759893321, 66.54258906972138732, -51.02319157577811382 ) ) ;
#177745 = CYLINDRICAL_SURFACE ( 'NONE', #221944, 11.75000000000000178 ) ;
#177746 = ADVANCED_FACE ( 'NONE', ( #217021 ), #22719, .F. ) ;
#177747 = VECTOR ( 'NONE', #13710, 1000.000000000000000 ) ;
#177748 = AXIS2_PLACEMENT_3D ( 'NONE', #233414, #251665, #177300 ) ;
#177749 = VECTOR ( 'NONE', #65168, 1000.000000000000227 ) ;
#177750 = ORIENTED_EDGE ( 'NONE', *, *, #181352, .F. ) ;
#177751 = CARTESIAN_POINT ( 'NONE',  ( -17.11825945287482753, 9.950000000011138823, -79.75000000000004263 ) ) ;
#177752 = VERTEX_POINT ( 'NONE', #57943 ) ;
#177753 = DIRECTION ( 'NONE',  ( 1.000000000000000000, 0.000000000000000000, 0.000000000000000000 ) ) ;
#177754 = EDGE_CURVE ( 'NONE', #86704, #182014, #161009, .T. ) ;
#177755 = DIRECTION ( 'NONE',  ( 0.000000000000000000, -0.2617529984165031243, -0.9651348961777157509 ) ) ;
#177757 = ORIENTED_EDGE ( 'NONE', *, *, #80032, .F. ) ;
#177756 = DIRECTION ( 'NONE',  ( 0.000000000000000000, 7.086529944415894657E-15, -1.000000000000000000 ) ) ;
#177758 = DIRECTION ( 'NONE',  ( 1.000000000000000000, 0.000000000000000000, -0.000000000000000000 ) ) ;
#177759 = DIRECTION ( 'NONE',  ( -1.836970198721029441E-16, 0.4721928772777346239, 0.8814952561688430555 ) ) ;
#177760 = DIRECTION ( 'NONE',  ( 0.000000000000000000, -1.000000000000000000, -6.982962677686266711E-15 ) ) ;
#177761 = DIRECTION ( 'NONE',  ( -0.000000000000000000, 0.1298341882519953583, 0.9915357197604862671 ) ) ;
#177762 = ADVANCED_FACE ( 'NONE', ( #116653 ), #159639, .T. ) ;
#177763 = CARTESIAN_POINT ( 'NONE',  ( -18.49719636458551264, 85.44636535924043130, -129.4514936146411799 ) ) ;
#177765 = ORIENTED_EDGE ( 'NONE', *, *, #254957, .T. ) ;
#177764 = DIRECTION ( 'NONE',  ( -1.000000000000000000, 3.854941057726231589E-15, 0.000000000000000000 ) ) ;
#177766 = ADVANCED_FACE ( 'NONE', ( #18831 ), #140131, .T. ) ;
#177767 = AXIS2_PLACEMENT_3D ( 'NONE', #200615, #203172, #61097 ) ;
#177768 = EDGE_CURVE ( 'NONE', #60425, #95061, #32428, .T. ) ;
#177769 = EDGE_CURVE ( 'NONE', #193142, #88353, #173526, .T. ) ;
#177770 = ORIENTED_EDGE ( 'NONE', *, *, #233308, .F. ) ;
#177771 = CARTESIAN_POINT ( 'NONE',  ( -18.46919391072063021, 85.67072438828941472, -62.84930395272471060 ) ) ;
#177772 = CARTESIAN_POINT ( 'NONE',  ( -18.51555513499479844, 85.35265705451605811, -196.3279375888288030 ) ) ;
#177773 = AXIS2_PLACEMENT_3D ( 'NONE', #17891, #117006, #76587 ) ;
#177774 = VERTEX_POINT ( 'NONE', #38404 ) ;
#177775 = FACE_OUTER_BOUND ( 'NONE', #153715, .T. ) ;
#177776 = DIRECTION ( 'NONE',  ( 1.000000000000000000, 2.952720810173289112E-16, -0.000000000000000000 ) ) ;
#177777 = AXIS2_PLACEMENT_3D ( 'NONE', #170328, #131145, #224147 ) ;
#177778 = ORIENTED_EDGE ( 'NONE', *, *, #98384, .F. ) ;
#177779 = AXIS2_PLACEMENT_3D ( 'NONE', #16738, #79235, #17992 ) ;
#177780 = CIRCLE ( 'NONE', #173718, 0.8750000000000007772 ) ;
#177782 = ADVANCED_FACE ( 'NONE', ( #235308 ), #98327, .T. ) ;
#177781 = DIRECTION ( 'NONE',  ( 1.000000000000000000, 0.000000000000000000, 0.000000000000000000 ) ) ;
#177783 = EDGE_CURVE ( 'NONE', #239427, #82199, #40801, .T. ) ;
#177784 = DIRECTION ( 'NONE',  ( 0.000000000000000000, 0.000000000000000000, -1.000000000000000000 ) ) ;
#177785 = AXIS2_PLACEMENT_3D ( 'NONE', #57646, #137198, #216732 ) ;
#177786 = ORIENTED_EDGE ( 'NONE', *, *, #191581, .T. ) ;
#177787 = DIRECTION ( 'NONE',  ( -1.000000000000000000, 0.000000000000000000, 0.000000000000000000 ) ) ;
#177788 = VERTEX_POINT ( 'NONE', #117925 ) ;
#177789 = EDGE_CURVE ( 'NONE', #228775, #134584, #165100, .T. ) ;
#177790 = CARTESIAN_POINT ( 'NONE',  ( 23.30000000000000426, -11.79999999999999538, -347.0000000000001137 ) ) ;
#177791 = CIRCLE ( 'NONE', #161211, 0.09999999999999574507 ) ;
#177793 = ORIENTED_EDGE ( 'NONE', *, *, #95951, .F. ) ;
#177792 = CARTESIAN_POINT ( 'NONE',  ( 21.05000000000000071, -1.835341550213257733, -78.55515129256303908 ) ) ;
#177794 = CYLINDRICAL_SURFACE ( 'NONE', #27847, 0.09999999999999939493 ) ;
#177795 = ORIENTED_EDGE ( 'NONE', *, *, #210680, .T. ) ;
#177796 = DIRECTION ( 'NONE',  ( -1.000000000000000000, 0.000000000000000000, 0.000000000000000000 ) ) ;
#177798 = ORIENTED_EDGE ( 'NONE', *, *, #243225, .F. ) ;
#177797 = EDGE_CURVE ( 'NONE', #169204, #103163, #86521, .T. ) ;
#177800 = ORIENTED_EDGE ( 'NONE', *, *, #197010, .T. ) ;
#177799 = ORIENTED_EDGE ( 'NONE', *, *, #30699, .T. ) ;
#177801 = CARTESIAN_POINT ( 'NONE',  ( -23.15000000000000213, 87.65000000001215597, -139.5231074845243029 ) ) ;
#177802 = VERTEX_POINT ( 'NONE', #237883 ) ;
#177803 = EDGE_CURVE ( 'NONE', #247369, #129910, #52649, .T. ) ;
#177804 = CARTESIAN_POINT ( 'NONE',  ( -18.59999999999999787, 47.95459712139159336, -246.5019368548292675 ) ) ;
#177806 = VERTEX_POINT ( 'NONE', #254823 ) ;
#177805 = CIRCLE ( 'NONE', #194563, 0.1000000000000043771 ) ;
#177807 = VECTOR ( 'NONE', #177496, 1000.000000000000000 ) ;
#177808 = EDGE_CURVE ( 'NONE', #207476, #147427, #76229, .T. ) ;
#177809 = AXIS2_PLACEMENT_3D ( 'NONE', #217955, #159314, #219255 ) ;
#177810 = ORIENTED_EDGE ( 'NONE', *, *, #254404, .F. ) ;
#177811 = VECTOR ( 'NONE', #12253, 1000.000000000000000 ) ;
#177812 = CARTESIAN_POINT ( 'NONE',  ( -23.25000000000000000, 36.65892442174935439, -249.5511627012433848 ) ) ;
#177814 = ORIENTED_EDGE ( 'NONE', *, *, #19898, .T. ) ;
#177813 = DIRECTION ( 'NONE',  ( 0.000000000000000000, 0.2617529984165030688, 0.9651348961777157509 ) ) ;
#177815 = DIRECTION ( 'NONE',  ( -0.000000000000000000, 0.000000000000000000, -1.000000000000000000 ) ) ;
#177816 = VERTEX_POINT ( 'NONE', #206464 ) ;
#177817 = AXIS2_PLACEMENT_3D ( 'NONE', #65175, #239982, #80874 ) ;
#177818 = CARTESIAN_POINT ( 'NONE',  ( -18.40000000000000213, 11.47316190337362762, -180.1499999999999773 ) ) ;
#177819 = CIRCLE ( 'NONE', #165322, 0.09999999999999939493 ) ;
#177820 = CARTESIAN_POINT ( 'NONE',  ( -18.58693740092145319, -9.406432150241773371, -74.12481645650147755 ) ) ;
#177821 = EDGE_CURVE ( 'NONE', #140961, #102291, #224726, .T. ) ;
#177822 = DIRECTION ( 'NONE',  ( 0.000000000000000000, 0.9126074666063769270, 0.4088369013363280513 ) ) ;
#177823 = ORIENTED_EDGE ( 'NONE', *, *, #96295, .F. ) ;
#177824 = DIRECTION ( 'NONE',  ( 0.000000000000000000, 0.000000000000000000, 1.000000000000000000 ) ) ;
#177825 = CARTESIAN_POINT ( 'NONE',  ( -18.41809261886955085, 37.95493855205511835, -261.2294694010199692 ) ) ;
#177826 = EDGE_LOOP ( 'NONE', ( #212771, #194471, #7004, #53421 ) ) ;
#177827 = CARTESIAN_POINT ( 'NONE',  ( -17.11825945287481687, 14.13772148853350252, -219.1573629999798527 ) ) ;
#177828 = EDGE_LOOP ( 'NONE', ( #43007, #189005, #21176, #236822 ) ) ;
#177829 = ORIENTED_EDGE ( 'NONE', *, *, #246622, .T. ) ;
#177830 = CIRCLE ( 'NONE', #231992, 0.09999999999999939493 ) ;
#177831 = AXIS2_PLACEMENT_3D ( 'NONE', #162205, #5640, #104732 ) ;
#177832 = FACE_OUTER_BOUND ( 'NONE', #155458, .T. ) ;
#177833 = ORIENTED_EDGE ( 'NONE', *, *, #91399, .T. ) ;
#177834 = ORIENTED_EDGE ( 'NONE', *, *, #120212, .T. ) ;
#177835 = CARTESIAN_POINT ( 'NONE',  ( -16.87683809663752399, 66.05000000001187743, -90.37310748452438247 ) ) ;
#177836 = DIRECTION ( 'NONE',  ( 0.000000000000000000, 0.000000000000000000, 1.000000000000000000 ) ) ;
#177837 = EDGE_LOOP ( 'NONE', ( #78198, #25355, #187585, #114277 ) ) ;
#177838 = ORIENTED_EDGE ( 'NONE', *, *, #38561, .F. ) ;
#177839 = CARTESIAN_POINT ( 'NONE',  ( 18.59999999999999787, -11.75000000000000000, 30.09999999999999787 ) ) ;
#177840 = DIRECTION ( 'NONE',  ( 0.000000000000000000, 0.000000000000000000, 1.000000000000000000 ) ) ;
#177841 = ORIENTED_EDGE ( 'NONE', *, *, #164502, .T. ) ;
#177842 = VECTOR ( 'NONE', #16220, 1000.000000000000000 ) ;
#177843 = VERTEX_POINT ( 'NONE', #107352 ) ;
#177844 = ORIENTED_EDGE ( 'NONE', *, *, #167238, .T. ) ;
#177845 = EDGE_CURVE ( 'NONE', #227071, #24822, #125640, .T. ) ;
#177846 = CARTESIAN_POINT ( 'NONE',  ( -21.07928932188134041, 76.00000000001165290, -69.52310748452431710 ) ) ;
#177847 = CARTESIAN_POINT ( 'NONE',  ( 21.13736287352038445, 67.95335762362829257, -157.3731074845244109 ) ) ;
#177848 = DIRECTION ( 'NONE',  ( 0.000000000000000000, -6.938893903907222067E-15, 1.000000000000000000 ) ) ;
#177849 = CYLINDRICAL_SURFACE ( 'NONE', #245068, 0.09999999999999939493 ) ;
#177850 = DIRECTION ( 'NONE',  ( 0.000000000000000000, 0.000000000000000000, 1.000000000000000000 ) ) ;
#177851 = CIRCLE ( 'NONE', #148814, 0.09999999999999781286 ) ;
#177852 = CARTESIAN_POINT ( 'NONE',  ( -20.54999999999999716, -9.399999999988846611, -191.1060308773475356 ) ) ;
#177854 = DIRECTION ( 'NONE',  ( 1.000000000000000000, 0.000000000000000000, -0.000000000000000000 ) ) ;
#177853 = CARTESIAN_POINT ( 'NONE',  ( -23.15000000000000213, -11.74999999998884448, -33.50000000000000000 ) ) ;
#177856 = VECTOR ( 'NONE', #84845, 1000.000000000000000 ) ;
#177855 = CARTESIAN_POINT ( 'NONE',  ( -20.94999999999999929, 67.23127455305835554, -235.8551265064784559 ) ) ;
#177857 = AXIS2_PLACEMENT_3D ( 'NONE', #113106, #130090, #90969 ) ;
#177858 = CARTESIAN_POINT ( 'NONE',  ( -18.59999999999999787, 72.05339752741123505, -225.0867394276846483 ) ) ;
#177859 = DIRECTION ( 'NONE',  ( -1.000000000000000000, 0.000000000000000000, 0.000000000000000000 ) ) ;
#177860 = EDGE_CURVE ( 'NONE', #154701, #77148, #186521, .T. ) ;
#177861 = CARTESIAN_POINT ( 'NONE',  ( 18.59999999999999076, 69.60000000001230092, -160.0926828544628222 ) ) ;
#177863 = VERTEX_POINT ( 'NONE', #202611 ) ;
#177862 = VECTOR ( 'NONE', #208630, 1000.000000000000000 ) ;
#177865 = ORIENTED_EDGE ( 'NONE', *, *, #27113, .T. ) ;
#177864 = DIRECTION ( 'NONE',  ( 0.000000000000000000, 0.9579639084728132081, 0.2868887416116073785 ) ) ;
#177866 = DIRECTION ( 'NONE',  ( -1.000000000000000000, 0.000000000000000000, 0.000000000000000000 ) ) ;
#177867 = AXIS2_PLACEMENT_3D ( 'NONE', #130379, #30035, #89964 ) ;
#177868 = PLANE ( 'NONE',  #11326 ) ;
#177869 = VERTEX_POINT ( 'NONE', #23998 ) ;
#177870 = VECTOR ( 'NONE', #175755, 1000.000000000000000 ) ;
#177871 = SHAPE_REPRESENTATION_RELATIONSHIP ( 'NONE' , 'NONE' ,  #141939, #157027 ) ;
#177872 = SPHERICAL_SURFACE ( 'NONE', #45668, 0.1000000000000000056 ) ;
#177873 = DIRECTION ( 'NONE',  ( 1.000000000000000000, 0.000000000000000000, -0.000000000000000000 ) ) ;
#177874 = VERTEX_POINT ( 'NONE', #65661 ) ;
#177875 = CIRCLE ( 'NONE', #77892, 0.1000000000000055705 ) ;
#177876 = DIRECTION ( 'NONE',  ( 0.000000000000000000, -1.000000000000000000, 0.000000000000000000 ) ) ;
#177877 = LINE ( 'NONE', #213128, #250867 ) ;
#177878 = CARTESIAN_POINT ( 'NONE',  ( 20.01715728752538936, 5.586869315528661062, 16.41686199900910736 ) ) ;
#177879 = CARTESIAN_POINT ( 'NONE',  ( 21.05000000000000071, 10.42338541492406279, -141.4920519238701218 ) ) ;
#177881 = EDGE_LOOP ( 'NONE', ( #78183, #93402 ) ) ;
#177880 = CARTESIAN_POINT ( 'NONE',  ( -20.99142135623731065, 64.40000000001194280, -109.9513107147998880 ) ) ;
#177883 = ORIENTED_EDGE ( 'NONE', *, *, #214757, .T. ) ;
#177882 = CARTESIAN_POINT ( 'NONE',  ( -18.52309608778508832, 85.64247632006711797, -96.30851114335470697 ) ) ;
#177884 = DIRECTION ( 'NONE',  ( -1.000000000000000000, 0.000000000000000000, -0.000000000000000000 ) ) ;
#177885 = DIRECTION ( 'NONE',  ( 1.000000000000000000, 0.000000000000000000, 0.000000000000000000 ) ) ;
#177886 = EDGE_CURVE ( 'NONE', #8263, #135203, #61028, .T. ) ;
#177887 = CARTESIAN_POINT ( 'NONE',  ( -21.65000000000000213, 7.250000000011138646, -76.25000000000004263 ) ) ;
#177888 = CARTESIAN_POINT ( 'NONE',  ( -18.59999999999999787, -1.149570369564537842, -175.3159124845019790 ) ) ;
#177890 = LINE ( 'NONE', #256063, #41721 ) ;
#177889 = FACE_OUTER_BOUND ( 'NONE', #142862, .T. ) ;
#177891 = DIRECTION ( 'NONE',  ( 0.000000000000000000, -6.982962677686266711E-15, 1.000000000000000000 ) ) ;
#177893 = ADVANCED_FACE ( 'NONE', ( #186931 ), #87777, .F. ) ;
#177892 = CARTESIAN_POINT ( 'NONE',  ( -21.00857864376268935, 11.60000000001115161, -40.42820323027555673 ) ) ;
#177894 = CARTESIAN_POINT ( 'NONE',  ( 21.13736287352038445, 8.046642376395153562, -76.25000000000004263 ) ) ;
#177895 = CARTESIAN_POINT ( 'NONE',  ( 22.24259225415828922, 0.09906588346399246292, -160.0080621294345633 ) ) ;
#177896 = CIRCLE ( 'NONE', #82168, 0.5000000000000004441 ) ;
#177897 = VECTOR ( 'NONE', #98658, 1000.000000000000000 ) ;
#177898 = CARTESIAN_POINT ( 'NONE',  ( 21.09813707148777340, 10.11617798928880063, -228.0894954011192794 ) ) ;
#177899 = AXIS2_PLACEMENT_3D ( 'NONE', #181605, #159465, #242841 ) ;
#177900 = EDGE_LOOP ( 'NONE', ( #228693, #72506, #136955 ) ) ;
#177901 = CARTESIAN_POINT ( 'NONE',  ( 21.05000000000000071, -0.09999993529482512078, -94.02192177890532321 ) ) ;
#177902 = ORIENTED_EDGE ( 'NONE', *, *, #209585, .F. ) ;
#177903 = ORIENTED_EDGE ( 'NONE', *, *, #235673, .T. ) ;
#177904 = ADVANCED_FACE ( 'NONE', ( #146469 ), #106051, .F. ) ;
#177905 = DIRECTION ( 'NONE',  ( 0.000000000000000000, 0.9770955615653548199, 0.2128009952262535920 ) ) ;
#177906 = CYLINDRICAL_SURFACE ( 'NONE', #127556, 12.87499999999999822 ) ;
#177907 = ORIENTED_EDGE ( 'NONE', *, *, #121669, .T. ) ;
#177908 = ADVANCED_FACE ( 'NONE', ( #29159 ), #48600, .F. ) ;
#177909 = ORIENTED_EDGE ( 'NONE', *, *, #230815, .F. ) ;
#177910 =( NAMED_UNIT ( * ) PLANE_ANGLE_UNIT ( ) SI_UNIT ( $, .RADIAN. ) );
#177911 = AXIS2_PLACEMENT_3D ( 'NONE', #59537, #200374, #197791 ) ;
#177912 = AXIS2_PLACEMENT_3D ( 'NONE', #140398, #243356, #64723 ) ;
#177913 = EDGE_CURVE ( 'NONE', #195513, #42095, #219252, .T. ) ;
#177914 = ORIENTED_EDGE ( 'NONE', *, *, #22089, .T. ) ;
#177915 = ORIENTED_EDGE ( 'NONE', *, *, #184766, .T. ) ;
#177916 = CARTESIAN_POINT ( 'NONE',  ( -23.25000000000000000, 11.65000000001115588, -88.75000000000004263 ) ) ;
#177917 = DIRECTION ( 'NONE',  ( 1.000000000000000000, -0.000000000000000000, -0.000000000000000000 ) ) ;
#177918 = AXIS2_PLACEMENT_3D ( 'NONE', #37262, #196304, #33431 ) ;
#177919 = CARTESIAN_POINT ( 'NONE',  ( -20.94999999999999929, 1.115600667400684642E-11, -167.5000000000000284 ) ) ;
#177920 = CYLINDRICAL_SURFACE ( 'NONE', #228104, 0.09999999999998898659 ) ;
#177921 = LINE ( 'NONE', #1815, #177556 ) ;
#177922 = CARTESIAN_POINT ( 'NONE',  ( 21.08479644141221954, 65.51392872348355922, -241.9636179317403162 ) ) ;
#177923 = CARTESIAN_POINT ( 'NONE',  ( 21.05000000000000071, 76.09999993531927487, -143.0011857056192639 ) ) ;
#177925 = EDGE_LOOP ( 'NONE', ( #105245, #64645, #125711, #38723, #39319, #21290, #220370, #103807, #242241, #137454, #25478, #225886 ) ) ;
#177924 = CARTESIAN_POINT ( 'NONE',  ( -23.15000000000000213, 47.70572087816298534, -241.8629305864830030 ) ) ;
#177927 = CARTESIAN_POINT ( 'NONE',  ( -20.85000000000000142, 80.82423061532404063, -192.8091306798888525 ) ) ;
#177926 = CARTESIAN_POINT ( 'NONE',  ( -22.39999999999999858, -0.1008583690987139431, 11.74956712348939192 ) ) ;
#177928 = ADVANCED_FACE ( 'NONE', ( #104757, #184319, #181770 ), #43550, .F. ) ;
#177929 = DIRECTION ( 'NONE',  ( -1.000000000000000000, 1.652117596168391700E-15, 0.000000000000000000 ) ) ;
#177930 = ORIENTED_EDGE ( 'NONE', *, *, #71271, .T. ) ;
#177931 = CARTESIAN_POINT ( 'NONE',  ( -16.93301857435210422, 63.06970463974469254, -213.0862067822817778 ) ) ;
#177932 = CARTESIAN_POINT ( 'NONE',  ( -18.59999999999999787, 79.16909458115064524, -196.2854372848902926 ) ) ;
#177933 = ORIENTED_EDGE ( 'NONE', *, *, #225840, .F. ) ;
#177935 = CARTESIAN_POINT ( 'NONE',  ( -23.15000000000000213, 4.250000000011156409, -146.3500000000000227 ) ) ;
#177934 = DIRECTION ( 'NONE',  ( 0.000000000000000000, -0.8660254037844384856, 0.5000000000000002220 ) ) ;
#177936 = AXIS2_PLACEMENT_3D ( 'NONE', #242948, #63024, #186857 ) ;
#177937 = PLANE ( 'NONE',  #73688 ) ;
#177938 = CARTESIAN_POINT ( 'NONE',  ( 19.75857864376268935, 16.76897757977919312, -222.7804130109902871 ) ) ;
#177939 = ORIENTED_EDGE ( 'NONE', *, *, #52197, .F. ) ;
#177940 = CARTESIAN_POINT ( 'NONE',  ( -18.50000000000000355, 77.26327546522891510, -61.62124281777789037 ) ) ;
#177941 = FACE_OUTER_BOUND ( 'NONE', #25841, .T. ) ;
#177942 = CYLINDRICAL_SURFACE ( 'NONE', #232359, 0.1999999999999987899 ) ;
#177943 = CARTESIAN_POINT ( 'NONE',  ( -21.65000000000000213, 68.25000000001185185, -90.67310748452436542 ) ) ;
#177944 = ORIENTED_EDGE ( 'NONE', *, *, #57762, .T. ) ;
#177945 = AXIS2_PLACEMENT_3D ( 'NONE', #68592, #7323, #226347 ) ;
#177946 = EDGE_CURVE ( 'NONE', #247064, #79682, #190627, .T. ) ;
#177947 = LINE ( 'NONE', #97064, #117079 ) ;
#177948 = CIRCLE ( 'NONE', #236194, 0.09999999999999939493 ) ;
#177949 = FACE_OUTER_BOUND ( 'NONE', #5353, .T. ) ;
#177950 = DIRECTION ( 'NONE',  ( -4.239556034732056743E-17, -0.9579639084728132081, -0.2868887416116073230 ) ) ;
#177951 = TOROIDAL_SURFACE ( 'NONE', #61419, 0.2000000000000000111, 0.1000000000000000056 ) ;
#177952 = CIRCLE ( 'NONE', #211276, 0.09999999999999939493 ) ;
#177953 = CARTESIAN_POINT ( 'NONE',  ( -18.39999999999999858, 85.50000000001233502, -162.9910380878246201 ) ) ;
#177954 = PRODUCT_DEFINITION_FORMATION_WITH_SPECIFIED_SOURCE ( 'ANY', '', #211859, .NOT_KNOWN. ) ;
#177955 = EDGE_CURVE ( 'NONE', #44054, #182258, #244292, .T. ) ;
#177957 = ORIENTED_EDGE ( 'NONE', *, *, #12277, .F. ) ;
#177956 = CARTESIAN_POINT ( 'NONE',  ( 20.94999999999999929, 6.450000000011156587, -77.01702717044007329 ) ) ;
#177958 = FACE_OUTER_BOUND ( 'NONE', #24356, .T. ) ;
#177959 = VECTOR ( 'NONE', #97623, 1000.000000000000000 ) ;
#177960 = CARTESIAN_POINT ( 'NONE',  ( -16.84981964351479178, 66.08268176591317911, -90.15350587050488684 ) ) ;
#177961 = PLANE ( 'NONE',  #171035 ) ;
#177962 = CARTESIAN_POINT ( 'NONE',  ( 23.14999999999999147, 1.115600667400684642E-11, -100.5000000000000284 ) ) ;
#177963 = AXIS2_PLACEMENT_3D ( 'NONE', #140365, #161239, #119552 ) ;
#177964 = CARTESIAN_POINT ( 'NONE',  ( 21.04999999999914806, 10.54375127550720137, -175.0563878086650504 ) ) ;
#177966 = ORIENTED_EDGE ( 'NONE', *, *, #233088, .F. ) ;
#177965 = DIRECTION ( 'NONE',  ( -0.000000000000000000, 1.000000000000000000, -0.000000000000000000 ) ) ;
#177967 = CARTESIAN_POINT ( 'NONE',  ( -20.85000000000000142, 7.021664781911246322, -204.6335654018972434 ) ) ;
#177968 = DIRECTION ( 'NONE',  ( 1.000000000000000000, 0.000000000000000000, 0.000000000000000000 ) ) ;
#177969 = CARTESIAN_POINT ( 'NONE',  ( 20.86777300164945004, 67.49225400653517681, -195.4205142095401868 ) ) ;
#177970 = EDGE_CURVE ( 'NONE', #55636, #239248, #174083, .T. ) ;
#177971 = EDGE_LOOP ( 'NONE', ( #157650, #38602, #118872, #113395 ) ) ;
#177972 = CARTESIAN_POINT ( 'NONE',  ( -12.26136940704872202, 66.64859682587062650, -153.0435770476858579 ) ) ;
#177973 = CARTESIAN_POINT ( 'NONE',  ( 21.05000000000000071, 76.02138556594995578, -176.3280685972093806 ) ) ;
#177974 = CARTESIAN_POINT ( 'NONE',  ( 18.59999999999999787, 1.115600667400684642E-11, -134.0000000000000000 ) ) ;
#177975 = CARTESIAN_POINT ( 'NONE',  ( -18.59999999999999787, 77.13501884592227498, -128.8061306010920362 ) ) ;
#177976 = EDGE_CURVE ( 'NONE', #56834, #195949, #4398, .T. ) ;
#177977 = CARTESIAN_POINT ( 'NONE',  ( -18.49346865148359598, 78.22586126723579980, -231.3921957456194889 ) ) ;
#177978 = CIRCLE ( 'NONE', #32438, 0.1000000000000013933 ) ;
#177979 = CARTESIAN_POINT ( 'NONE',  ( 23.14999999999999503, 6.450000000011156587, -112.8500000000000369 ) ) ;
#177980 = CIRCLE ( 'NONE', #186354, 0.1999999999999987899 ) ;
#177981 = ORIENTED_EDGE ( 'NONE', *, *, #66520, .T. ) ;
#177982 = ORIENTED_EDGE ( 'NONE', *, *, #99711, .F. ) ;
#177983 = AXIS2_PLACEMENT_3D ( 'NONE', #138352, #178827, #217890 ) ;
#177984 = CARTESIAN_POINT ( 'NONE',  ( 22.00411653889225860, -1.446770167443869104, -193.8916177604842517 ) ) ;
#177985 = CARTESIAN_POINT ( 'NONE',  ( -20.94999999999999929, 46.50671693017397246, -243.2369495081682942 ) ) ;
#177986 = VECTOR ( 'NONE', #160454, 1000.000000000000000 ) ;
#177987 = EDGE_CURVE ( 'NONE', #24865, #133198, #158319, .T. ) ;
#177988 = LINE ( 'NONE', #78847, #107992 ) ;
#177989 = DIRECTION ( 'NONE',  ( 0.000000000000000000, -1.000000000000000000, 0.000000000000000000 ) ) ;
#177990 = ORIENTED_EDGE ( 'NONE', *, *, #90332, .T. ) ;
#177991 = VECTOR ( 'NONE', #248970, 1000.000000000000000 ) ;
#177992 = CARTESIAN_POINT ( 'NONE',  ( 20.95017935633852346, 10.47548927963648246, -175.0774397973904399 ) ) ;
#177993 = EDGE_CURVE ( 'NONE', #43053, #81086, #14570, .T. ) ;
#177995 = ADVANCED_FACE ( 'NONE', ( #109917 ), #184941, .T. ) ;
#177994 = CARTESIAN_POINT ( 'NONE',  ( 20.22516295850462598, 11.35589477125217250, -206.6222955247963000 ) ) ;
#177996 = CARTESIAN_POINT ( 'NONE',  ( 20.94999999999999574, 87.41227409416133298, -66.62310748452424036 ) ) ;
#177997 = LINE ( 'NONE', #41066, #127885 ) ;
#177998 = AXIS2_PLACEMENT_3D ( 'NONE', #115983, #33918, #192945 ) ;
#177999 = TOROIDAL_SURFACE ( 'NONE', #65550, 0.9750000000000019762, 0.1000000000000000056 ) ;
#178000 = VECTOR ( 'NONE', #7619, 999.9999999999998863 ) ;
#178001 = VERTEX_POINT ( 'NONE', #94207 ) ;
#178002 = DIRECTION ( 'NONE',  ( 0.000000000000000000, 0.9651348961777157509, -0.2617529984165031243 ) ) ;
#178003 = EDGE_CURVE ( 'NONE', #129778, #206320, #189476, .T. ) ;
#178004 = ORIENTED_EDGE ( 'NONE', *, *, #160778, .T. ) ;
#178005 = DIRECTION ( 'NONE',  ( 1.000000000000000000, 0.000000000000000000, 0.000000000000000000 ) ) ;
#178006 = ORIENTED_EDGE ( 'NONE', *, *, #68505, .F. ) ;
#178007 = CARTESIAN_POINT ( 'NONE',  ( -21.05000000000000071, 0.01485563490482383515, -27.15564095795645727 ) ) ;
#178008 = CARTESIAN_POINT ( 'NONE',  ( -6.000000000000002665, -11.34999999999999964, 14.00000000000000178 ) ) ;
#178009 = DIRECTION ( 'NONE',  ( 0.000000000000000000, 1.000000000000000000, 6.982962677686266711E-15 ) ) ;
#178010 = VERTEX_POINT ( 'NONE', #34282 ) ;
#178011 = EDGE_CURVE ( 'NONE', #165206, #243103, #257193, .T. ) ;
#178012 = EDGE_CURVE ( 'NONE', #88661, #254615, #23665, .T. ) ;
#178013 = FACE_OUTER_BOUND ( 'NONE', #10691, .T. ) ;
#178014 = CARTESIAN_POINT ( 'NONE',  ( 18.52928932188133970, 10.27928932189250411, -155.3500000000000227 ) ) ;
#178015 = CARTESIAN_POINT ( 'NONE',  ( -16.78805706634180339, 30.20034948041843492, -234.8058246103456383 ) ) ;
#178016 = VERTEX_POINT ( 'NONE', #92921 ) ;
#178017 = FACE_OUTER_BOUND ( 'NONE', #131565, .T. ) ;
#178019 = VERTEX_POINT ( 'NONE', #73406 ) ;
#178018 = CARTESIAN_POINT ( 'NONE',  ( -23.15000000000000213, 5.082284216461513184E-16, 4.149999999999999467 ) ) ;
#178020 = DIRECTION ( 'NONE',  ( 1.000000000000000000, -0.000000000000000000, -0.000000000000000000 ) ) ;
#178021 = AXIS2_PLACEMENT_3D ( 'NONE', #142253, #200947, #41902 ) ;
#178022 = DIRECTION ( 'NONE',  ( 0.000000000000000000, -0.2617529984165031243, -0.9651348961777157509 ) ) ;
#178023 = VERTEX_POINT ( 'NONE', #209033 ) ;
#178024 = AXIS2_PLACEMENT_3D ( 'NONE', #25202, #125562, #162144 ) ;
#178025 = DIRECTION ( 'NONE',  ( 0.000000000000000000, -0.1350103645451807555, -0.9908441862701610203 ) ) ;
#178026 = DIRECTION ( 'NONE',  ( -7.304098846217948299E-16, -1.000000000000000000, 0.000000000000000000 ) ) ;
#178027 = CARTESIAN_POINT ( 'NONE',  ( 18.59999999999997655, 74.93036000061670165, -233.6816308724374949 ) ) ;
#178028 = ORIENTED_EDGE ( 'NONE', *, *, #182613, .F. ) ;
#178029 = DIRECTION ( 'NONE',  ( 1.000000000000000000, 0.000000000000000000, -0.000000000000000000 ) ) ;
#178030 = EDGE_CURVE ( 'NONE', #44801, #236473, #130773, .T. ) ;
#178031 = ADVANCED_FACE ( 'NONE', ( #52508 ), #102703, .T. ) ;
#178032 = CARTESIAN_POINT ( 'NONE',  ( 15.75000000000000000, 48.22810253856975038, -234.1229447132332950 ) ) ;
#178033 = FACE_OUTER_BOUND ( 'NONE', #93659, .T. ) ;
#178034 = AXIS2_PLACEMENT_3D ( 'NONE', #22567, #79917, #219449 ) ;
#178035 = AXIS2_PLACEMENT_3D ( 'NONE', #46615, #8800, #199644 ) ;
#178036 = ORIENTED_EDGE ( 'NONE', *, *, #221862, .T. ) ;
#178037 = AXIS2_PLACEMENT_3D ( 'NONE', #41627, #160296, #140697 ) ;
#178038 = VECTOR ( 'NONE', #102489, 1000.000000000000000 ) ;
#178039 = EDGE_CURVE ( 'NONE', #210147, #161922, #248486, .T. ) ;
#178040 = AXIS2_PLACEMENT_3D ( 'NONE', #92063, #89488, #189891 ) ;
#178041 = VERTEX_POINT ( 'NONE', #231188 ) ;
#178042 = AXIS2_PLACEMENT_3D ( 'NONE', #23275, #124922, #127479 ) ;
#178043 = ORIENTED_EDGE ( 'NONE', *, *, #218752, .T. ) ;
#178044 = CARTESIAN_POINT ( 'NONE',  ( -18.59999999999999787, 45.93315328338058379, -256.6017782078560003 ) ) ;
#178045 = CARTESIAN_POINT ( 'NONE',  ( -17.22361732159831149, 65.65484434141011150, -181.3938920103915677 ) ) ;
#178047 = ORIENTED_EDGE ( 'NONE', *, *, #191486, .F. ) ;
#178046 = CARTESIAN_POINT ( 'NONE',  ( 18.52928932188133970, 10.27928932189249878, -158.7085786437627064 ) ) ;
#178048 = CARTESIAN_POINT ( 'NONE',  ( 19.75857864376268935, 11.75000000000000355, -24.85000000000000142 ) ) ;
#178049 = DIRECTION ( 'NONE',  ( 1.000000000000000000, 0.000000000000000000, -0.000000000000000000 ) ) ;
#178050 = CARTESIAN_POINT ( 'NONE',  ( -22.49544290803762792, 11.46684760846028084, -198.4357998940973573 ) ) ;
#178051 = FACE_OUTER_BOUND ( 'NONE', #215617, .T. ) ;
#178052 = LINE ( 'NONE', #77618, #196000 ) ;
#178053 = AXIS2_PLACEMENT_3D ( 'NONE', #10930, #108731, #69620 ) ;
#178054 = EDGE_CURVE ( 'NONE', #3957, #50671, #69439, .T. ) ;
#178055 = CARTESIAN_POINT ( 'NONE',  ( -18.59999999999999787, 57.82359945636609666, -226.0354702357591350 ) ) ;
#178057 = ORIENTED_EDGE ( 'NONE', *, *, #233075, .T. ) ;
#178056 = CARTESIAN_POINT ( 'NONE',  ( 23.14999999999999503, 17.11694853917244075, -224.3781540347815451 ) ) ;
#178059 = EDGE_LOOP ( 'NONE', ( #175079, #122822, #112624, #123884 ) ) ;
#178058 = FACE_OUTER_BOUND ( 'NONE', #183579, .T. ) ;
#178061 = CARTESIAN_POINT ( 'NONE',  ( 23.15000000000000213, 81.77808381374872226, -227.1078217596952697 ) ) ;
#178060 = CARTESIAN_POINT ( 'NONE',  ( 23.14999999999999503, 61.95000000001146390, -41.53680255528533394 ) ) ;
#178062 = ORIENTED_EDGE ( 'NONE', *, *, #251837, .T. ) ;
#178063 = EDGE_CURVE ( 'NONE', #142820, #215945, #211609, .T. ) ;
#178064 = ORIENTED_EDGE ( 'NONE', *, *, #65821, .F. ) ;
#178065 = DIRECTION ( 'NONE',  ( 0.000000000000000000, 0.1575844902526835067, 0.9875055080513738259 ) ) ;
#178066 = DIRECTION ( 'NONE',  ( -0.000000000000000000, -0.9651348961777157509, 0.2617529984165031243 ) ) ;
#178067 = CIRCLE ( 'NONE', #111413, 0.1000000000000028644 ) ;
#178068 = CARTESIAN_POINT ( 'NONE',  ( 20.04142135623730070, 11.65000000001115943, -88.75000000000004263 ) ) ;
#178069 = CARTESIAN_POINT ( 'NONE',  ( -23.15000000000000213, 1.115600667400684642E-11, -67.00000000000004263 ) ) ;
#178070 = EDGE_CURVE ( 'NONE', #119326, #182152, #108646, .T. ) ;
#178071 = FACE_OUTER_BOUND ( 'NONE', #19386, .T. ) ;
#178072 = EDGE_CURVE ( 'NONE', #123338, #51281, #219420, .T. ) ;
#178073 = LINE ( 'NONE', #209165, #156461 ) ;
#178074 = EDGE_LOOP ( 'NONE', ( #185674, #15826, #94594, #69441 ) ) ;
#178075 = ORIENTED_EDGE ( 'NONE', *, *, #233302, .T. ) ;
#178076 = EDGE_CURVE ( 'NONE', #105460, #104983, #169418, .T. ) ;
#178077 = CARTESIAN_POINT ( 'NONE',  ( 18.49999999999999289, 10.49142135624846439, -192.3499999999999659 ) ) ;
#178078 = AXIS2_PLACEMENT_3D ( 'NONE', #192095, #255850, #112550 ) ;
#178079 = AXIS2_PLACEMENT_3D ( 'NONE', #48014, #108002, #198431 ) ;
#178080 = ORIENTED_EDGE ( 'NONE', *, *, #27298, .F. ) ;
#178081 = DIRECTION ( 'NONE',  ( -1.000000000000000000, 0.000000000000000000, 0.000000000000000000 ) ) ;
#178082 = CARTESIAN_POINT ( 'NONE',  ( -17.11825945287481687, 51.52760218553060412, -231.9873527057832234 ) ) ;
#178084 = EDGE_CURVE ( 'NONE', #135481, #202597, #52836, .T. ) ;
#178083 = CARTESIAN_POINT ( 'NONE',  ( -12.84409460144754078, 66.58931770574362474, -54.09196404257613722 ) ) ;
#178086 = EDGE_CURVE ( 'NONE', #171525, #55518, #198587, .T. ) ;
#178085 = EDGE_CURVE ( 'NONE', #8900, #196464, #117633, .T. ) ;
#178087 = ORIENTED_EDGE ( 'NONE', *, *, #200606, .F. ) ;
#178088 = DIRECTION ( 'NONE',  ( -0.000000000000000000, 0.6922311945860614157, 0.7216758089626911232 ) ) ;
#178089 = EDGE_LOOP ( 'NONE', ( #237864, #68853, #72686, #106869 ) ) ;
#178090 = CARTESIAN_POINT ( 'NONE',  ( -18.37013991200266005, 11.49974761622313224, -91.29302301051716029 ) ) ;
#178091 = ORIENTED_EDGE ( 'NONE', *, *, #72833, .T. ) ;
#178092 = FACE_OUTER_BOUND ( 'NONE', #171677, .T. ) ;
#178093 = DIRECTION ( 'NONE',  ( 0.000000000000000000, 0.2128009952263485993, -0.9770955615653341697 ) ) ;
#178094 = DIRECTION ( 'NONE',  ( -0.000000000000000000, -0.9868171638914224886, -0.1618390714546072695 ) ) ;
#178095 = AXIS2_PLACEMENT_3D ( 'NONE', #24024, #239195, #63109 ) ;
#178096 = ORIENTED_EDGE ( 'NONE', *, *, #43789, .T. ) ;
#178098 = DIRECTION ( 'NONE',  ( 1.000000000000000000, 0.000000000000000000, 0.000000000000000000 ) ) ;
#178097 = CIRCLE ( 'NONE', #69768, 12.97499999999998721 ) ;
#178100 = EDGE_LOOP ( 'NONE', ( #30317, #52935, #164647, #153861 ) ) ;
#178099 = CARTESIAN_POINT ( 'NONE',  ( -22.01447462590972748, 7.263800201241075172, -100.4009629999405036 ) ) ;
#178101 = EDGE_CURVE ( 'NONE', #180643, #112954, #11159, .T. ) ;
#178102 = LINE ( 'NONE', #95960, #222883 ) ;
#178103 = ADVANCED_FACE ( 'NONE', ( #257092 ), #78489, .T. ) ;
#178104 = EDGE_LOOP ( 'NONE', ( #10375, #219312, #228596, #135442, #246335 ) ) ;
#178105 = AXIS2_PLACEMENT_3D ( 'NONE', #36977, #371, #138572 ) ;
#178106 = EDGE_CURVE ( 'NONE', #230546, #254598, #140309, .T. ) ;
#178107 = FACE_OUTER_BOUND ( 'NONE', #106656, .T. ) ;
#178108 = ORIENTED_EDGE ( 'NONE', *, *, #85473, .T. ) ;
#178109 = DIRECTION ( 'NONE',  ( 1.000000000000000000, 0.000000000000000000, 0.000000000000000000 ) ) ;
#178110 = CARTESIAN_POINT ( 'NONE',  ( 22.44352723754029810, 64.17297141203522415, -247.0962508001766480 ) ) ;
#178111 =( BOUNDED_CURVE ( )  B_SPLINE_CURVE ( 3, ( #163916, #243442, #240889, #123504 ),
 .UNSPECIFIED., .F., .F. ) 
 B_SPLINE_CURVE_WITH_KNOTS ( ( 4, 4 ),
 ( 3.752122642744613046, 4.712388980384671910 ),
 .UNSPECIFIED. ) 
 CURVE ( )  GEOMETRIC_REPRESENTATION_ITEM ( )  RATIONAL_B_SPLINE_CURVE ( ( 1.000000000000000000, 0.9246222802177266331, 0.9246222802177266331, 1.000000000000000000 ) ) 
 REPRESENTATION_ITEM ( '' )  );
#178113 = EDGE_CURVE ( 'NONE', #76073, #241619, #231937, .T. ) ;
#178112 = DIRECTION ( 'NONE',  ( 0.000000000000000000, -0.2617529984165031243, -0.9651348961777157509 ) ) ;
#178114 = DIRECTION ( 'NONE',  ( 0.000000000000000000, -0.1350103645451835865, -0.9908441862701605762 ) ) ;
#178115 = DIRECTION ( 'NONE',  ( 0.000000000000000000, -0.5041370733442398500, -0.8636236514129894681 ) ) ;
#178116 = EDGE_CURVE ( 'NONE', #195772, #46245, #38114, .T. ) ;
#178117 = VERTEX_POINT ( 'NONE', #235023 ) ;
#178118 = DIRECTION ( 'NONE',  ( 0.000000000000000000, -0.7397360091702823714, 0.6728971962616756564 ) ) ;
#178119 = CARTESIAN_POINT ( 'NONE',  ( 23.25000000000000000, -7.761787541757068531, -236.6467894636467975 ) ) ;
#178120 = DIRECTION ( 'NONE',  ( -0.000000000000000000, 3.469446951953635015E-14, 1.000000000000000000 ) ) ;
#178121 = VERTEX_POINT ( 'NONE', #139742 ) ;
#178122 = CARTESIAN_POINT ( 'NONE',  ( 22.47007471830798409, 7.543872110139020037, -199.3570250894167941 ) ) ;
#178123 = ORIENTED_EDGE ( 'NONE', *, *, #220577, .F. ) ;
#178124 = DIRECTION ( 'NONE',  ( -1.000000000000000000, 0.000000000000000000, -0.000000000000000000 ) ) ;
#178125 = VECTOR ( 'NONE', #13590, 1000.000000000000000 ) ;
#178126 = ORIENTED_EDGE ( 'NONE', *, *, #80610, .T. ) ;
#178127 =( BOUNDED_CURVE ( )  B_SPLINE_CURVE ( 3, ( #88902, #71938, #173655, #70671 ),
 .UNSPECIFIED., .F., .F. ) 
 B_SPLINE_CURVE_WITH_KNOTS ( ( 4, 4 ),
 ( 4.712388980384689674, 6.231880751915386263 ),
 .UNSPECIFIED. ) 
 CURVE ( )  GEOMETRIC_REPRESENTATION_ITEM ( )  RATIONAL_B_SPLINE_CURVE ( ( 1.000000000000000000, 0.8166740347213228279, 0.8166740347213228279, 1.000000000000000000 ) ) 
 REPRESENTATION_ITEM ( '' )  );
#178128 = DIRECTION ( 'NONE',  ( 1.000000000000000000, 0.000000000000000000, 0.000000000000000000 ) ) ;
#178129 = DIRECTION ( 'NONE',  ( 1.000000000000000000, 3.265361837132813093E-16, -0.000000000000000000 ) ) ;
#178131 = ORIENTED_EDGE ( 'NONE', *, *, #113389, .T. ) ;
#178130 = CARTESIAN_POINT ( 'NONE',  ( -21.04999999999994387, 84.00000000001119815, -37.18565239344504647 ) ) ;
#178132 = EDGE_CURVE ( 'NONE', #117921, #51613, #238246, .T. ) ;
#178133 = CARTESIAN_POINT ( 'NONE',  ( -18.46946985241266503, 8.797311384861430383, -245.4141716383250866 ) ) ;
#178134 = EDGE_LOOP ( 'NONE', ( #106930, #214870, #141789, #168790 ) ) ;
#178135 = AXIS2_PLACEMENT_3D ( 'NONE', #223486, #83938, #125682 ) ;
#178136 = DIRECTION ( 'NONE',  ( 0.000000000000000000, 6.577889128801576950E-15, -1.000000000000000000 ) ) ;
#178137 = LINE ( 'NONE', #198953, #185388 ) ;
#178138 = ORIENTED_EDGE ( 'NONE', *, *, #158945, .T. ) ;
#178139 = AXIS2_PLACEMENT_3D ( 'NONE', #93970, #5, #216493 ) ;
#178141 = ORIENTED_EDGE ( 'NONE', *, *, #5902, .T. ) ;
#178140 = ADVANCED_FACE ( 'NONE', ( #197158 ), #177642, .F. ) ;
#178142 = DIRECTION ( 'NONE',  ( 0.000000000000000000, 0.000000000000000000, -1.000000000000000000 ) ) ;
#178143 = CARTESIAN_POINT ( 'NONE',  ( 20.95483826173900255, 67.12383379524190730, -94.47683193162485793 ) ) ;
#178144 = ORIENTED_EDGE ( 'NONE', *, *, #136276, .T. ) ;
#178145 = CARTESIAN_POINT ( 'NONE',  ( -20.54999999999999716, 6.703231349641842307, -231.7785101893094577 ) ) ;
#178146 = AXIS2_PLACEMENT_3D ( 'NONE', #14848, #94341, #192192 ) ;
#178147 = CIRCLE ( 'NONE', #111487, 0.09999999999998898659 ) ;
#178149 = EDGE_LOOP ( 'NONE', ( #134761, #30216, #52438, #45679 ) ) ;
#178148 = CIRCLE ( 'NONE', #36695, 0.1000000000000054040 ) ;
#178150 = ORIENTED_EDGE ( 'NONE', *, *, #189145, .T. ) ;
#178151 =( BOUNDED_CURVE ( )  B_SPLINE_CURVE ( 3, ( #70584, #129247, #208789, #225748 ),
 .UNSPECIFIED., .F., .T. ) 
 B_SPLINE_CURVE_WITH_KNOTS ( ( 4, 4 ),
 ( 3.141592653589793116, 4.712388980384689674 ),
 .UNSPECIFIED. ) 
 CURVE ( )  GEOMETRIC_REPRESENTATION_ITEM ( )  RATIONAL_B_SPLINE_CURVE ( ( 1.000000000000000000, 0.8047378541243649375, 0.8047378541243649375, 1.000000000000000000 ) ) 
 REPRESENTATION_ITEM ( '' )  );
#178153 = DIRECTION ( 'NONE',  ( 0.000000000000000000, 6.982962677686266711E-15, -1.000000000000000000 ) ) ;
#178152 = CIRCLE ( 'NONE', #86516, 0.1000000000000028644 ) ;
#178154 = ADVANCED_FACE ( 'NONE', ( #120243 ), #115069, .F. ) ;
#178155 = AXIS2_PLACEMENT_3D ( 'NONE', #39715, #119235, #21435 ) ;
#178157 = VERTEX_POINT ( 'NONE', #77211 ) ;
#178156 = CARTESIAN_POINT ( 'NONE',  ( -18.59999999999999787, -9.400000000000005684, -40.38204184817266906 ) ) ;
#178158 = CARTESIAN_POINT ( 'NONE',  ( 22.39999999999999503, -1.232296663996729880, -194.8718726406955568 ) ) ;
#178159 = DIRECTION ( 'NONE',  ( 1.000000000000000000, 7.304098846218134667E-16, -0.000000000000000000 ) ) ;
#178160 = CARTESIAN_POINT ( 'NONE',  ( -16.81453563122428463, 63.08009114446584675, -213.1900633619857501 ) ) ;
#178162 = DIRECTION ( 'NONE',  ( 0.000000000000000000, 0.000000000000000000, -1.000000000000000000 ) ) ;
#178161 = CARTESIAN_POINT ( 'NONE',  ( -22.50000000000000000, 11.64957080755595520, -66.90000000000004832 ) ) ;
#178163 = CARTESIAN_POINT ( 'NONE',  ( -22.59999999999999787, 0.1000000000111554016, -55.35042919245524473 ) ) ;
#178164 = CARTESIAN_POINT ( 'NONE',  ( -20.54999999999999716, 2.500000000011154633, -120.7753780772379315 ) ) ;
#178165 = CIRCLE ( 'NONE', #211287, 0.09999999999999080458 ) ;
#178166 = CARTESIAN_POINT ( 'NONE',  ( 18.44364597020196328, -9.490487317151108826, -40.55797788968387607 ) ) ;
#178167 = EDGE_CURVE ( 'NONE', #17846, #182491, #75945, .T. ) ;
#178168 = DIRECTION ( 'NONE',  ( 1.000000000000000000, -4.851622311275599093E-17, 1.082981191754466866E-16 ) ) ;
#178169 = VECTOR ( 'NONE', #216918, 1000.000000000000000 ) ;
#178170 = ORIENTED_EDGE ( 'NONE', *, *, #93152, .T. ) ;
#178171 = AXIS2_PLACEMENT_3D ( 'NONE', #184893, #7542, #126196 ) ;
#178172 = AXIS2_PLACEMENT_3D ( 'NONE', #65543, #164663, #125526 ) ;
#178174 = VERTEX_POINT ( 'NONE', #175090 ) ;
#178173 = DIRECTION ( 'NONE',  ( 0.000000000000000000, -1.224646799147353207E-16, 1.000000000000000000 ) ) ;
#178175 = AXIS2_PLACEMENT_3D ( 'NONE', #109417, #188976, #130267 ) ;
#178176 = ORIENTED_EDGE ( 'NONE', *, *, #3827, .T. ) ;
#178177 = DIRECTION ( 'NONE',  ( 1.000000000000000000, 0.000000000000000000, 0.000000000000000000 ) ) ;
#178178 = ORIENTED_EDGE ( 'NONE', *, *, #158772, .T. ) ;
#178179 = DIRECTION ( 'NONE',  ( 0.000000000000000000, 0.000000000000000000, -1.000000000000000000 ) ) ;
#178180 = CIRCLE ( 'NONE', #119937, 14.30833333333333890 ) ;
#178181 = ORIENTED_EDGE ( 'NONE', *, *, #106210, .F. ) ;
#178182 =( LENGTH_UNIT ( ) NAMED_UNIT ( * ) SI_UNIT ( .MILLI., .METRE. ) );
#178183 = DIRECTION ( 'NONE',  ( -1.284434275755705296E-16, 0.7071067811865471286, 0.7071067811865479058 ) ) ;
#178186 = VERTEX_POINT ( 'NONE', #56354 ) ;
#178185 = ORIENTED_EDGE ( 'NONE', *, *, #216023, .T. ) ;
#178184 = AXIS2_PLACEMENT_3D ( 'NONE', #242971, #163449, #86439 ) ;
#178187 = ORIENTED_EDGE ( 'NONE', *, *, #46954, .T. ) ;
#178188 = AXIS2_PLACEMENT_3D ( 'NONE', #189797, #75009, #133665 ) ;
#178189 = ORIENTED_EDGE ( 'NONE', *, *, #98935, .T. ) ;
#178190 = CARTESIAN_POINT ( 'NONE',  ( 5.899999999999997691, -11.34999999999999964, 13.90000000000000213 ) ) ;
#178192 = CLOSED_SHELL ( 'NONE', ( #74397, #72955, #150457, #33294, #125485, #143630, #243946, #129442, #38174, #33425, #98540, #14566, #67778, #63392, #255925, #87329, #149367, #120916, #141996, #28839, #208736, #205251, #226561, #249508, #65870, #58515, #209960, #26691, #115269, #169972, #181308, #211486, #5952, #249318, #181218, #95356, #1428, #140628, #143854, #116612, #17882, #238862, #158834, #210437, #73868, #207482, #211798, #130886, #34381, #177746, #38747, #12341, #8942, #231585, #128976, #1253, #6488, #2581, #137501, #73485, #195492, #127122, #240460, #245124, #252982, #156767, #126489, #144950, #91852, #249156, #126188, #231393, #15077, #194204, #180173, #136092, #80391, #212478, #173919, #25072, #114804, #181830, #17670, #140276, #205458, #253559, #141632, #170983, #165323, #59325, #159702, #52975, #182934, #152072, #181196, #203681, #104311, #69659, #223958, #108617, #92167, #164181, #108269, #32430, #149230, #79341, #40883, #52965, #41686, #176953, #118788, #228928, #239040, #181491, #33659, #150993, #183559, #81444, #75896, #16581, #190481, #129165, #31042, #254302, #217781, #216296, #13810, #192231, #9746, #46861, #21898, #35720, #253033, #29016, #121968, #175287, #152375, #240698, #254060, #88369, #253076, #56265, #215635, #100285, #125055, #102103, #108753, #101190, #119337, #69776, #22735, #199927, #20098, #232470, #179209, #48274, #18217, #240333, #141945, #189069, #79111, #205480, #39990, #33280, #9872, #32347, #239360, #117623, #129694, #131037, #115543, #70143, #142302, #123423, #186543, #246542, #141294, #12549, #12120, #217505, #11120, #93482, #67463, #115120, #2068, #201911, #38780, #150970, #13460, #37601, #76030, #51814, #64297, #251683, #158061, #210049, #96978, #241291, #147048, #223959, #167164, #32312, #164000, #162214, #81358, #196278, #73617, #29854, #58354, #36575, #45582, #21149, #82338, #140114, #150415, #66384, #200703, #69604, #58680, #217226, #75442, #43492, #81742, #95855, #253466, #83410, #145455, #13620, #103820, #248739, #48727, #46248, #113220, #63945, #125803, #234417, #196509, #20443, #177627, #11729, #198818, #130576, #237797, #28342, #253854, #127784, #230143, #216311, #181911, #30724, #220555, #154622, #196960, #183907, #161226, #86161, #95073, #12291, #102961, #70835, #256546, #23696, #92849, #37274, #7547, #18800, #95867, #25558, #50098, #109157, #246666, #192984, #234882, #213118, #52581, #25921, #174610, #3104, #163759, #113566, #165002, #191856, #15846, #35046, #148853, #75754, #49964, #202756, #80749, #106198, #216513, #208328, #106404, #43700, #50919, #62153, #99902, #94215, #127297, #96249, #144559, #87075, #104852, #121684, #36870, #52874, #32171, #182372, #71678, #136724, #11300, #25666, #29402, #114462, #96818, #140230, #133742, #181762, #152319, #195910, #255935, #112709, #106737, #125666, #191611, #64532, #179847, #19673, #128769, #91560, #56678, #185018, #76841, #140051, #169574, #248455, #255691, #115348, #27880, #32574, #58245, #71347, #25817, #49312, #108330, #227860, #117372, #243063, #40423, #118613, #201729, #184459, #199822, #97836, #138803, #233622, #58233, #171598, #197718, #136131, #20828, #14147, #200187, #75506, #74391, #110070, #62881, #164410, #37583, #140342, #185068, #86603, #193985, #54661, #224867, #197717, #195504, #56207, #117910, #75664, #202895, #167784, #173069, #163506, #122814, #117966, #77179, #178717, #182467, #53471, #188395, #127607, #168527, #235893, #21827, #92044, #96888, #164113, #245729, #238848, #235365, #11960, #109145, #194614, #70736, #206321, #312, #28712, #239394, #32359, #208316, #215382, #99852, #184154, #11940, #35078, #175954, #59695, #81918, #39578, #184182, #56749, #96382, #71957, #144811, #140957, #28250, #88885, #206281, #6911, #151063, #247123, #230379, #23625, #148250, #229648, #23121, #179855, #208527, #183005, #171620, #32010, #25657, #187031, #231225, #15755, #101797, #142422, #138655, #152632, #59354, #186258, #97619, #156387, #65244, #54441, #176996, #221310, #51417, #177253, #68023, #92706, #191372, #105223, #180681, #67873, #208299, #158469, #137594, #112661, #135130, #47009, #195602, #75244, #185179, #222810, #223774, #175648 ) ) ;
#178191 = DIRECTION ( 'NONE',  ( 0.000000000000000000, 0.000000000000000000, -1.000000000000000000 ) ) ;
#178194 = ORIENTED_EDGE ( 'NONE', *, *, #238036, .T. ) ;
#178193 = CARTESIAN_POINT ( 'NONE',  ( 18.59999999999999076, 64.25000000001148237, -44.67310748452440095 ) ) ;
#178195 = CARTESIAN_POINT ( 'NONE',  ( -21.46681500593987479, 33.85532080846552816, -243.2929468148609260 ) ) ;
#178196 = CARTESIAN_POINT ( 'NONE',  ( 13.22261339317536155, 12.45029792656131562, -213.8222050902127478 ) ) ;
#178198 = ORIENTED_EDGE ( 'NONE', *, *, #153013, .F. ) ;
#178197 = DIRECTION ( 'NONE',  ( 1.000000000000000000, 0.000000000000000000, 0.000000000000000000 ) ) ;
#178199 = CARTESIAN_POINT ( 'NONE',  ( -21.14999999999999858, -11.64999999998884483, -167.4999999999999716 ) ) ;
#178200 = VERTEX_POINT ( 'NONE', #215446 ) ;
#178201 = FACE_OUTER_BOUND ( 'NONE', #241264, .T. ) ;
#178203 = ORIENTED_EDGE ( 'NONE', *, *, #29896, .T. ) ;
#178202 = CARTESIAN_POINT ( 'NONE',  ( -20.64999999999999858, 66.33592547490526670, -222.9197737850312251 ) ) ;
#178204 = AXIS2_PLACEMENT_3D ( 'NONE', #80681, #242340, #100235 ) ;
#178205 = CARTESIAN_POINT ( 'NONE',  ( 23.14999999999999503, 64.35000000001146248, -43.03791325517834565 ) ) ;
#178206 = DIRECTION ( 'NONE',  ( 0.000000000000000000, -0.9998779222360104635, -0.01562499999996343723 ) ) ;
#178207 = EDGE_CURVE ( 'NONE', #172822, #242007, #240299, .T. ) ;
#178208 = CIRCLE ( 'NONE', #253185, 0.09999999999998898659 ) ;
#178209 = CARTESIAN_POINT ( 'NONE',  ( 20.99551997958364424, 11.75000000001111644, -60.15165913768996120 ) ) ;
#178210 = EDGE_LOOP ( 'NONE', ( #117899, #86966, #201099, #174952, #57428, #120745 ) ) ;
#178212 = CARTESIAN_POINT ( 'NONE',  ( -20.94999999999999929, 14.88773611405353314, -236.3451124650200370 ) ) ;
#178211 = CARTESIAN_POINT ( 'NONE',  ( -16.88783316861810135, 9.950000000011137047, -46.25226404197980656 ) ) ;
#178213 = CARTESIAN_POINT ( 'NONE',  ( -12.30589683808040391, 66.64325398293358660, -85.81974776316017994 ) ) ;
#178214 = CARTESIAN_POINT ( 'NONE',  ( 18.39999999999999858, 85.50000000001240608, -163.4229180933022576 ) ) ;
#178215 = DIRECTION ( 'NONE',  ( 0.000000000000000000, -0.8660254037844468122, -0.4999999999999859557 ) ) ;
#178216 = CARTESIAN_POINT ( 'NONE',  ( 18.39999999999997371, 16.37079970714665933, -222.2530670965321349 ) ) ;
#178217 = VERTEX_POINT ( 'NONE', #39413 ) ;
#178218 = VERTEX_POINT ( 'NONE', #19838 ) ;
#178219 = ORIENTED_EDGE ( 'NONE', *, *, #154906, .F. ) ;
#178220 = DIRECTION ( 'NONE',  ( 0.000000000000000000, -0.8814952561688430555, 0.4721928772777346239 ) ) ;
#178221 = ORIENTED_EDGE ( 'NONE', *, *, #22934, .F. ) ;
#178222 = FACE_OUTER_BOUND ( 'NONE', #82868, .T. ) ;
#178223 = ORIENTED_EDGE ( 'NONE', *, *, #253778, .T. ) ;
#178224 = ADVANCED_FACE ( 'NONE', ( #48039 ), #125516, .T. ) ;
#178225 = LINE ( 'NONE', #216024, #223120 ) ;
#178226 = CARTESIAN_POINT ( 'NONE',  ( -20.94999999999999929, 1.115600667400684642E-11, -134.0000000000000284 ) ) ;
#178227 = AXIS2_PLACEMENT_3D ( 'NONE', #142818, #67162, #146668 ) ;
#178228 = EDGE_CURVE ( 'NONE', #217875, #101660, #246253, .T. ) ;
#178229 = AXIS2_PLACEMENT_3D ( 'NONE', #178266, #62146, #142933 ) ;
#178230 = AXIS2_PLACEMENT_3D ( 'NONE', #193320, #73397, #248148 ) ;
#178231 = ORIENTED_EDGE ( 'NONE', *, *, #30374, .T. ) ;
#178232 = VECTOR ( 'NONE', #150479, 1000.000000000000000 ) ;
#178233 = DIRECTION ( 'NONE',  ( 1.000000000000000000, 0.000000000000000000, 0.000000000000000000 ) ) ;
#178234 = EDGE_CURVE ( 'NONE', #105532, #46813, #152845, .T. ) ;
#178235 = AXIS2_PLACEMENT_3D ( 'NONE', #59448, #75234, #77750 ) ;
#178236 = VERTEX_POINT ( 'NONE', #207132 ) ;
#178237 = VERTEX_POINT ( 'NONE', #110583 ) ;
#178238 = VERTEX_POINT ( 'NONE', #11506 ) ;
#178239 = EDGE_CURVE ( 'NONE', #96541, #244617, #148443, .T. ) ;
#178240 = CARTESIAN_POINT ( 'NONE',  ( 21.30000000000002558, 1.115650265596050101E-11, -171.5499999999999829 ) ) ;
#178241 = CARTESIAN_POINT ( 'NONE',  ( -21.14999999999999858, 11.40444339177023814, -198.6185779617709670 ) ) ;
#178243 = EDGE_CURVE ( 'NONE', #155345, #237838, #32030, .T. ) ;
#178242 = CARTESIAN_POINT ( 'NONE',  ( 18.39999999999999858, 85.60000000001137721, -29.42291809330221142 ) ) ;
#178244 = CARTESIAN_POINT ( 'NONE',  ( -20.54999999999999716, 68.85000000001205933, -124.1731074845243370 ) ) ;
#178246 = DIRECTION ( 'NONE',  ( -0.000000000000000000, 0.8814952561688430555, -0.4721928772777346239 ) ) ;
#178245 = FACE_OUTER_BOUND ( 'NONE', #155973, .T. ) ;
#178247 = FACE_OUTER_BOUND ( 'NONE', #188410, .T. ) ;
#178249 = ORIENTED_EDGE ( 'NONE', *, *, #256873, .T. ) ;
#178248 = CARTESIAN_POINT ( 'NONE',  ( 21.76363531954645936, 68.98706345214023372, -103.1221093588238062 ) ) ;
#178250 = CARTESIAN_POINT ( 'NONE',  ( -22.50000000000000000, 64.25000000001237765, -170.0231074845244166 ) ) ;
#178251 = VERTEX_POINT ( 'NONE', #227970 ) ;
#178252 = EDGE_CURVE ( 'NONE', #84962, #88954, #49326, .T. ) ;
#178253 = CARTESIAN_POINT ( 'NONE',  ( -18.47079683080349710, -9.471664105233697839, -141.1088605409922536 ) ) ;
#178254 = VERTEX_POINT ( 'NONE', #220595 ) ;
#178255 = VERTEX_POINT ( 'NONE', #128880 ) ;
#178256 = CARTESIAN_POINT ( 'NONE',  ( -21.05000000000000071, 1.162701749949165642, -142.0000000000000284 ) ) ;
#178257 = VECTOR ( 'NONE', #136949, 1000.000000000000000 ) ;
#178258 = FACE_OUTER_BOUND ( 'NONE', #165436, .T. ) ;
#178259 = CARTESIAN_POINT ( 'NONE',  ( -21.05000000000000071, 64.23744694032046709, -224.5446448091673233 ) ) ;
#178260 = ORIENTED_EDGE ( 'NONE', *, *, #245462, .F. ) ;
#178261 = ADVANCED_FACE ( 'NONE', ( #188837 ), #36115, .T. ) ;
#178262 = CIRCLE ( 'NONE', #224000, 0.1000000000000055844 ) ;
#178263 = CARTESIAN_POINT ( 'NONE',  ( 23.24999999999999645, 64.25000000001161027, -60.27310748452440947 ) ) ;
#178264 = ORIENTED_EDGE ( 'NONE', *, *, #249532, .F. ) ;
#178265 = VERTEX_POINT ( 'NONE', #10220 ) ;
#178266 = CARTESIAN_POINT ( 'NONE',  ( 21.05000000000000071, 69.55000000001187743, -93.00608031408432907 ) ) ;
#178267 = VERTEX_POINT ( 'NONE', #74063 ) ;
#178268 = CARTESIAN_POINT ( 'NONE',  ( -16.93772744219066340, 60.88373978801495667, -221.0804579231064793 ) ) ;
#178269 = CARTESIAN_POINT ( 'NONE',  ( 19.99999999999998934, 11.75000000001115552, -121.8500000000000369 ) ) ;
#178270 = ORIENTED_EDGE ( 'NONE', *, *, #211636, .F. ) ;
#178271 = DIRECTION ( 'NONE',  ( 1.000000000000000000, 0.000000000000000000, 0.000000000000000000 ) ) ;
#178272 = SPHERICAL_SURFACE ( 'NONE', #152898, 0.1000000000000000056 ) ;
#178273 = DIRECTION ( 'NONE',  ( 0.000000000000000000, 0.1335171055202901413, -0.9910465087640860649 ) ) ;
#178274 = ORIENTED_EDGE ( 'NONE', *, *, #96210, .F. ) ;
#178275 = EDGE_CURVE ( 'NONE', #257831, #58706, #111112, .T. ) ;
#178276 = DIRECTION ( 'NONE',  ( 1.000000000000000000, 0.000000000000000000, -0.000000000000000000 ) ) ;
#178277 = DIRECTION ( 'NONE',  ( 0.000000000000000000, 0.000000000000000000, -1.000000000000000000 ) ) ;
#178278 = CIRCLE ( 'NONE', #99112, 4.049999999999998046 ) ;
#178279 = AXIS2_PLACEMENT_3D ( 'NONE', #209345, #192360, #51525 ) ;
#178280 = CIRCLE ( 'NONE', #11675, 0.1000000000000054040 ) ;
#178281 = ORIENTED_EDGE ( 'NONE', *, *, #62555, .T. ) ;
#178282 = EDGE_CURVE ( 'NONE', #255102, #133253, #61224, .T. ) ;
#178284 = ORIENTED_EDGE ( 'NONE', *, *, #70383, .T. ) ;
#178283 = LINE ( 'NONE', #257728, #8691 ) ;
#178285 = ORIENTED_EDGE ( 'NONE', *, *, #202136, .T. ) ;
#178286 = CARTESIAN_POINT ( 'NONE',  ( 20.95512820512820440, 67.12384868372393498, -124.3229346253956038 ) ) ;
#178287 = CARTESIAN_POINT ( 'NONE',  ( -22.47071067811865319, 1.115600667400684642E-11, -100.5000000000000284 ) ) ;
#178288 = DIRECTION ( 'NONE',  ( 0.000000000000000000, -1.000000000000000000, -6.982962677686265922E-15 ) ) ;
#178289 = DIRECTION ( 'NONE',  ( 0.000000000000000000, -0.9654727137038715545, 0.2605042016806676242 ) ) ;
#178290 = DIRECTION ( 'NONE',  ( 0.000000000000000000, 0.9126074666063769270, 0.4088369013363280513 ) ) ;
#178291 = FACE_OUTER_BOUND ( 'NONE', #20113, .T. ) ;
#178292 = ORIENTED_EDGE ( 'NONE', *, *, #14391, .T. ) ;
#178293 = CARTESIAN_POINT ( 'NONE',  ( 21.08489247129321242, 61.89576995986235630, -221.6119524385055399 ) ) ;
#178294 = DIRECTION ( 'NONE',  ( -1.000000000000000000, 7.492892343619937423E-30, -1.073024830501117725E-15 ) ) ;
#178295 = CIRCLE ( 'NONE', #224226, 4.049999999999998046 ) ;
#178296 = CARTESIAN_POINT ( 'NONE',  ( -22.50000000000094502, 0.1008583690986050579, 11.74956712348940613 ) ) ;
#178297 = DIRECTION ( 'NONE',  ( 0.000000000000000000, 1.096314854800262720E-14, -1.000000000000000000 ) ) ;
#178298 = EDGE_CURVE ( 'NONE', #135423, #228990, #14072, .T. ) ;
#178299 = AXIS2_PLACEMENT_3D ( 'NONE', #118534, #181070, #217583 ) ;
#178300 = ORIENTED_EDGE ( 'NONE', *, *, #51374, .T. ) ;
#178301 = ORIENTED_EDGE ( 'NONE', *, *, #220877, .T. ) ;
#178302 = DIRECTION ( 'NONE',  ( 0.000000000000000000, 0.2128009952263603677, -0.9770955615653313941 ) ) ;
#178303 = CARTESIAN_POINT ( 'NONE',  ( -20.94999999999999929, 28.67750504931771616, -258.3094128005139396 ) ) ;
#178304 = CARTESIAN_POINT ( 'NONE',  ( -21.64999999999999858, 9.350000000011133849, -146.6500000000000341 ) ) ;
#178305 = CARTESIAN_POINT ( 'NONE',  ( -20.90000000000000213, 0.000000000000000000, 0.000000000000000000 ) ) ;
#178306 = CARTESIAN_POINT ( 'NONE',  ( -18.59999999999999787, 1.162701749938009677, -8.099999999999999645 ) ) ;
#178307 = EDGE_CURVE ( 'NONE', #210461, #85043, #211073, .T. ) ;
#178308 = ORIENTED_EDGE ( 'NONE', *, *, #29878, .F. ) ;
#178309 = LINE ( 'NONE', #98700, #93164 ) ;
#178310 = PLANE ( 'NONE',  #55228 ) ;
#178311 = EDGE_CURVE ( 'NONE', #25605, #249684, #253931, .T. ) ;
#178313 = EDGE_CURVE ( 'NONE', #119379, #153971, #244376, .T. ) ;
#178312 = DIRECTION ( 'NONE',  ( 1.000000000000000000, 0.000000000000000000, 0.000000000000000000 ) ) ;
#178314 = DIRECTION ( 'NONE',  ( 0.000000000000000000, -0.9126074666063763718, -0.4088369013363293836 ) ) ;
#178315 = CIRCLE ( 'NONE', #211618, 4.150000000000001243 ) ;
#178316 = ADVANCED_FACE ( 'NONE', ( #152313 ), #127876, .F. ) ;
#178317 = AXIS2_PLACEMENT_3D ( 'NONE', #205025, #9409, #87657 ) ;
#178318 = AXIS2_PLACEMENT_3D ( 'NONE', #224139, #123774, #162918 ) ;
#178319 = EDGE_LOOP ( 'NONE', ( #208053, #89667, #27268, #5561 ) ) ;
#178320 = FACE_OUTER_BOUND ( 'NONE', #107812, .T. ) ;
#178321 = ADVANCED_FACE ( 'NONE', ( #93592 ), #19544, .F. ) ;
#178322 = ORIENTED_EDGE ( 'NONE', *, *, #151356, .T. ) ;
#178323 = CARTESIAN_POINT ( 'NONE',  ( 21.09096482362048874, 69.63645563460823951, -170.0625557632986613 ) ) ;
#178324 = TOROIDAL_SURFACE ( 'NONE', #82577, 0.2000000000000000111, 0.1000000000000000056 ) ;
#178325 = DIRECTION ( 'NONE',  ( -0.000000000000000000, -0.4088369013363283844, 0.9126074666063769270 ) ) ;
#178326 = CARTESIAN_POINT ( 'NONE',  ( 18.50000324121758055, 65.70692517833191459, -64.06446533783041275 ) ) ;
#178327 = CARTESIAN_POINT ( 'NONE',  ( -20.94999999999999929, -11.29603075032412640, -197.9521008403361009 ) ) ;
#178328 = CARTESIAN_POINT ( 'NONE',  ( 21.13461538461538325, 65.38541703798705385, -191.1731074845244223 ) ) ;
#178329 = PLANE ( 'NONE',  #199746 ) ;
#178330 = CARTESIAN_POINT ( 'NONE',  ( -20.85000000000000142, 74.44087353924872730, -232.6253149859214773 ) ) ;
#178331 = FACE_OUTER_BOUND ( 'NONE', #166038, .T. ) ;
#178332 = CARTESIAN_POINT ( 'NONE',  ( 23.14999999999999858, 71.00000000001205080, -124.1178414656112352 ) ) ;
#178333 = DIRECTION ( 'NONE',  ( -1.000000000000000000, 0.000000000000000000, 0.000000000000000000 ) ) ;
#178334 = DIRECTION ( 'NONE',  ( 0.000000000000000000, 0.000000000000000000, 1.000000000000000000 ) ) ;
#178335 = CIRCLE ( 'NONE', #99171, 0.1000000000000028644 ) ;
#178336 = CIRCLE ( 'NONE', #153411, 0.5000000000000004441 ) ;
#178337 = DIRECTION ( 'NONE',  ( -1.000000000000000000, -0.000000000000000000, 0.000000000000000000 ) ) ;
#178338 = CARTESIAN_POINT ( 'NONE',  ( -24.30000000000000071, 3.175288713399619933, -347.0000000000001137 ) ) ;
#178339 = EDGE_CURVE ( 'NONE', #220552, #136488, #15454, .T. ) ;
#178340 = ORIENTED_EDGE ( 'NONE', *, *, #136688, .T. ) ;
#178341 = CARTESIAN_POINT ( 'NONE',  ( 21.04999999999999716, 6.344359042043513419, 0.01485563489366281686 ) ) ;
#178342 = DIRECTION ( 'NONE',  ( 0.000000000000000000, 0.000000000000000000, -1.000000000000000000 ) ) ;
#178343 = CARTESIAN_POINT ( 'NONE',  ( 20.12518398540832365, 9.975088720679844201, -41.49666825246991664 ) ) ;
#178344 = EDGE_CURVE ( 'NONE', #1569, #106796, #48750, .T. ) ;
#178345 = EDGE_CURVE ( 'NONE', #147959, #214102, #230545, .T. ) ;
#178346 = VERTEX_POINT ( 'NONE', #33672 ) ;
#178347 = PLANE ( 'NONE',  #159622 ) ;
#178348 = ORIENTED_EDGE ( 'NONE', *, *, #149847, .T. ) ;
#178349 = CARTESIAN_POINT ( 'NONE',  ( 22.48660254037845263, 31.80946045771257502, -238.8484668136873381 ) ) ;
#178350 = CIRCLE ( 'NONE', #119921, 0.1999999999999987899 ) ;
#178351 = ORIENTED_EDGE ( 'NONE', *, *, #249232, .T. ) ;
#178352 = AXIS2_PLACEMENT_3D ( 'NONE', #232363, #195806, #231079 ) ;
#178353 = AXIS2_PLACEMENT_3D ( 'NONE', #98582, #233034, #217268 ) ;
#178354 = VECTOR ( 'NONE', #210469, 1000.000000000000000 ) ;
#178355 = AXIS2_PLACEMENT_3D ( 'NONE', #40638, #199695, #21059 ) ;
#178357 = ORIENTED_EDGE ( 'NONE', *, *, #20206, .F. ) ;
#178356 = AXIS2_PLACEMENT_3D ( 'NONE', #105218, #107835, #89541 ) ;
#178358 = CARTESIAN_POINT ( 'NONE',  ( -21.65000000000000213, 30.11817903451004952, -234.7598257170722889 ) ) ;
#178359 = ORIENTED_EDGE ( 'NONE', *, *, #203143, .T. ) ;
#178360 = VECTOR ( 'NONE', #115116, 1000.000000000000114 ) ;
#178361 = CARTESIAN_POINT ( 'NONE',  ( -20.64999999999999858, 7.250000000011155521, -54.65000000000000568 ) ) ;
#178362 = CARTESIAN_POINT ( 'NONE',  ( -20.94999999999999929, 1.115600667400684642E-11, -100.5000000000000426 ) ) ;
#178364 = CYLINDRICAL_SURFACE ( 'NONE', #16121, 0.09999999999999986677 ) ;
#178363 = PRODUCT_DEFINITION_CONTEXT ( 'detailed design', #137289, 'design' ) ;
#178365 = CARTESIAN_POINT ( 'NONE',  ( 18.49999999999999289, 6.450000000011156587, -55.25000000000004974 ) ) ;
#178366 = CARTESIAN_POINT ( 'NONE',  ( 20.94999999999999574, 74.83729825007431202, -161.9231074845243654 ) ) ;
#178367 = EDGE_CURVE ( 'NONE', #38559, #48342, #227806, .T. ) ;
#178368 = CARTESIAN_POINT ( 'NONE',  ( -13.22483237240078680, 46.65138127958493897, -234.7343221152025023 ) ) ;
#178369 = PLANE ( 'NONE',  #221660 ) ;
#178370 = CARTESIAN_POINT ( 'NONE',  ( -21.65000000000000213, 52.80902093404626640, -233.8693558107618173 ) ) ;
#178372 = ORIENTED_EDGE ( 'NONE', *, *, #178072, .F. ) ;
#178371 = DIRECTION ( 'NONE',  ( -7.304098846218201720E-16, 1.000000000000000000, 0.000000000000000000 ) ) ;
#178373 = ORIENTED_EDGE ( 'NONE', *, *, #175684, .T. ) ;
#178375 = LINE ( 'NONE', #40154, #181024 ) ;
#178374 = CARTESIAN_POINT ( 'NONE',  ( 22.50046968638104516, 0.04516984714028955683, 11.75004515447417930 ) ) ;
#178377 = ORIENTED_EDGE ( 'NONE', *, *, #150224, .F. ) ;
#178376 = CARTESIAN_POINT ( 'NONE',  ( -16.77431908686105544, 60.94711240597669644, -221.0291585267142125 ) ) ;
#178378 = VERTEX_POINT ( 'NONE', #133994 ) ;
#178379 = CARTESIAN_POINT ( 'NONE',  ( -16.94165728009536664, 66.01213024408845342, -149.1320524760142234 ) ) ;
#178380 = AXIS2_PLACEMENT_3D ( 'NONE', #257890, #121037, #83113 ) ;
#178381 = CIRCLE ( 'NONE', #45067, 0.09999999999999939493 ) ;
#178382 = FACE_OUTER_BOUND ( 'NONE', #254525, .T. ) ;
#178383 = TOROIDAL_SURFACE ( 'NONE', #65923, 6.258578643762712446, 0.1000000000000000056 ) ;
#178384 = CARTESIAN_POINT ( 'NONE',  ( -18.59999999999999787, 74.16465844978765176, -124.9679561919613207 ) ) ;
#178385 =( NAMED_UNIT ( * ) SI_UNIT ( $, .STERADIAN. ) SOLID_ANGLE_UNIT ( ) );
#178386 = LINE ( 'NONE', #222589, #69294 ) ;
#178387 = DIRECTION ( 'NONE',  ( -0.000000000000000000, 0.8814952561688430555, -0.4721928772777346239 ) ) ;
#178388 = CARTESIAN_POINT ( 'NONE',  ( 20.94999999999999574, 65.52661458509869874, -61.94445302027585143 ) ) ;
#178389 = VECTOR ( 'NONE', #154824, 1000.000000000000000 ) ;
#178390 = EDGE_CURVE ( 'NONE', #86933, #162629, #2764, .T. ) ;
#178391 = AXIS2_PLACEMENT_3D ( 'NONE', #85156, #4361, #8242 ) ;
#178392 = CARTESIAN_POINT ( 'NONE',  ( 18.79999999999999716, -11.65000000000000036, 32.89999999999999858 ) ) ;
#178393 = ORIENTED_EDGE ( 'NONE', *, *, #44129, .T. ) ;
#178394 = VERTEX_POINT ( 'NONE', #32372 ) ;
#178395 = EDGE_CURVE ( 'NONE', #211067, #197295, #34938, .T. ) ;
#178396 = CARTESIAN_POINT ( 'NONE',  ( 21.33487959338958362, 6.571513019293449887, -199.5687945318220500 ) ) ;
#178397 = CIRCLE ( 'NONE', #182485, 0.1000000000000028644 ) ;
#178398 = ORIENTED_EDGE ( 'NONE', *, *, #30896, .T. ) ;
#178399 = DIRECTION ( 'NONE',  ( 1.000000000000000000, 0.000000000000000000, 0.000000000000000000 ) ) ;
#178400 = ORIENTED_EDGE ( 'NONE', *, *, #228940, .F. ) ;
#178401 = FACE_OUTER_BOUND ( 'NONE', #141205, .T. ) ;
#178402 = AXIS2_PLACEMENT_3D ( 'NONE', #87702, #224653, #8200 ) ;
#178403 = ADVANCED_FACE ( 'NONE', ( #94864 ), #182029, .T. ) ;
#178404 = ADVANCED_FACE ( 'NONE', ( #214814 ), #111308, .T. ) ;
#178405 = CARTESIAN_POINT ( 'NONE',  ( -12.48127053791144903, 48.91191486804444111, -233.7874788057928868 ) ) ;
#178406 = DIRECTION ( 'NONE',  ( 0.000000000000000000, -8.881784197000871698E-16, -1.000000000000000000 ) ) ;
#178407 = FACE_OUTER_BOUND ( 'NONE', #89684, .T. ) ;
#178408 = CARTESIAN_POINT ( 'NONE',  ( -22.39999999999999858, 11.65000000000000036, 0.09999999999999592548 ) ) ;
#178409 = ORIENTED_EDGE ( 'NONE', *, *, #175453, .T. ) ;
#178410 = AXIS2_PLACEMENT_3D ( 'NONE', #161997, #143682, #126697 ) ;
#178411 = DIRECTION ( 'NONE',  ( 0.000000000000000000, -1.000000000000000000, 0.000000000000000000 ) ) ;
#178412 = DIRECTION ( 'NONE',  ( -1.000000000000000000, 0.000000000000000000, 0.000000000000000000 ) ) ;
#178413 = CIRCLE ( 'NONE', #61871, 0.1000000000000028644 ) ;
#178415 = DIRECTION ( 'NONE',  ( 0.000000000000000000, 0.000000000000000000, -1.000000000000000000 ) ) ;
#178414 = CIRCLE ( 'NONE', #65956, 0.09999999999999939493 ) ;
#178416 = CARTESIAN_POINT ( 'NONE',  ( -22.32929514600008503, 75.90092432189882743, -211.1017550499008735 ) ) ;
#178417 = AXIS2_PLACEMENT_3D ( 'NONE', #234696, #162391, #99800 ) ;
#178418 = CARTESIAN_POINT ( 'NONE',  ( -20.85000000000000142, 77.83585931145600512, -158.5186683157258187 ) ) ;
#178419 = ORIENTED_EDGE ( 'NONE', *, *, #248022, .T. ) ;
#178420 = ORIENTED_EDGE ( 'NONE', *, *, #192803, .T. ) ;
#178423 = VERTEX_POINT ( 'NONE', #96137 ) ;
#178422 = CARTESIAN_POINT ( 'NONE',  ( -23.15000000000000213, 61.88149656937975607, -248.1136133839584090 ) ) ;
#178421 = LINE ( 'NONE', #158853, #57510 ) ;
#178424 = TOROIDAL_SURFACE ( 'NONE', #132606, 11.90000000000000391, 0.1000000000000000056 ) ;
#178425 = ADVANCED_FACE ( 'NONE', ( #56998 ), #72781, .F. ) ;
#178426 = DIRECTION ( 'NONE',  ( 0.000000000000000000, 0.000000000000000000, -1.000000000000000000 ) ) ;
#178427 = EDGE_CURVE ( 'NONE', #15533, #1348, #252937, .T. ) ;
#178428 = CARTESIAN_POINT ( 'NONE',  ( -20.94999999999994245, 67.75000000001118394, -3.123107484524795474 ) ) ;
#178429 = ORIENTED_EDGE ( 'NONE', *, *, #393, .T. ) ;
#178430 = LINE ( 'NONE', #2306, #138790 ) ;
#178431 = CARTESIAN_POINT ( 'NONE',  ( -16.93860193097148326, 9.993107767340401182, -54.40013836730685881 ) ) ;
#178432 = CARTESIAN_POINT ( 'NONE',  ( -16.87242674293850797, 9.949999999999983302, -12.64890975362765424 ) ) ;
#178434 = VERTEX_POINT ( 'NONE', #2170 ) ;
#178433 = DIRECTION ( 'NONE',  ( 0.000000000000000000, -0.9651348961777157509, 0.2617529984165031243 ) ) ;
#178435 = AXIS2_PLACEMENT_3D ( 'NONE', #122219, #103905, #28285 ) ;
#178436 = CARTESIAN_POINT ( 'NONE',  ( 23.14999999999999858, 76.00000000001142553, -36.02310748452432421 ) ) ;
#178437 = ADVANCED_FACE ( 'NONE', ( #79140 ), #61409, .F. ) ;
#178438 = ORIENTED_EDGE ( 'NONE', *, *, #19572, .F. ) ;
#178440 = EDGE_CURVE ( 'NONE', #16800, #221298, #160500, .T. ) ;
#178439 = FACE_OUTER_BOUND ( 'NONE', #105150, .T. ) ;
#178441 = CYLINDRICAL_SURFACE ( 'NONE', #136836, 0.09999999999998898659 ) ;
#178442 = CYLINDRICAL_SURFACE ( 'NONE', #129611, 0.1000000000000050432 ) ;
#178443 = ORIENTED_EDGE ( 'NONE', *, *, #76171, .F. ) ;
#178444 = CARTESIAN_POINT ( 'NONE',  ( -23.25000000000000000, -11.74999999998884448, -167.4999999999999432 ) ) ;
#178445 = ORIENTED_EDGE ( 'NONE', *, *, #65886, .T. ) ;
#178446 = DIRECTION ( 'NONE',  ( 1.652117596168391700E-15, 1.000000000000000000, -0.000000000000000000 ) ) ;
#178447 = FACE_OUTER_BOUND ( 'NONE', #135425, .T. ) ;
#178448 = DIRECTION ( 'NONE',  ( 1.000000000000000000, 1.387778780781454006E-13, 0.000000000000000000 ) ) ;
#178449 = ORIENTED_EDGE ( 'NONE', *, *, #60452, .T. ) ;
#178450 = ADVANCED_FACE ( 'NONE', ( #178291 ), #82973, .T. ) ;
#178451 = CARTESIAN_POINT ( 'NONE',  ( -17.11825945287481332, 65.95000000001201101, -115.6731074845243796 ) ) ;
#178452 = CARTESIAN_POINT ( 'NONE',  ( 23.24999999999997513, 17.11694853917244075, -224.3781540347815451 ) ) ;
#178453 = CARTESIAN_POINT ( 'NONE',  ( -11.60000000000000320, -9.650000000000005684, 12.40000000000000391 ) ) ;
#178454 = EDGE_LOOP ( 'NONE', ( #96875, #41015, #1118, #110233 ) ) ;
#178455 = EDGE_CURVE ( 'NONE', #7443, #154279, #60870, .T. ) ;
#178456 = CIRCLE ( 'NONE', #36821, 0.1000000000000028644 ) ;
#178458 = CIRCLE ( 'NONE', #7752, 0.09999999999999939493 ) ;
#178457 = CARTESIAN_POINT ( 'NONE',  ( -20.05000000000000426, 9.250000000011157297, -121.6500000000000341 ) ) ;
#178459 = DIRECTION ( 'NONE',  ( 0.000000000000000000, 0.9915357197604862671, -0.1298341882519953583 ) ) ;
#178460 = AXIS2_PLACEMENT_3D ( 'NONE', #111548, #133674, #15030 ) ;
#178461 = DIRECTION ( 'NONE',  ( -1.000000000000000000, -0.000000000000000000, -0.000000000000000000 ) ) ;
#178462 = EDGE_LOOP ( 'NONE', ( #211362, #242749, #247705, #124389 ) ) ;
#178463 = DIRECTION ( 'NONE',  ( 1.000000000000000000, 0.000000000000000000, 0.000000000000000000 ) ) ;
#178464 = CIRCLE ( 'NONE', #82722, 0.1000000000000000472 ) ;
#178465 = EDGE_LOOP ( 'NONE', ( #248644, #14959, #114646, #20698 ) ) ;
#178467 = ORIENTED_EDGE ( 'NONE', *, *, #90946, .F. ) ;
#178466 = CARTESIAN_POINT ( 'NONE',  ( -23.25000000000000000, 11.65000000001115588, -33.50000000000000000 ) ) ;
#178468 = EDGE_CURVE ( 'NONE', #69713, #48052, #82217, .T. ) ;
#178470 = ORIENTED_EDGE ( 'NONE', *, *, #37920, .F. ) ;
#178469 = ORIENTED_EDGE ( 'NONE', *, *, #99325, .T. ) ;
#178472 = CIRCLE ( 'NONE', #124479, 0.1000000000000046685 ) ;
#178471 = DIRECTION ( 'NONE',  ( 0.000000000000000000, 0.000000000000000000, -1.000000000000000000 ) ) ;
#178473 = CIRCLE ( 'NONE', #224410, 0.09999999999999939493 ) ;
#178474 = CYLINDRICAL_SURFACE ( 'NONE', #114962, 1.749999999999998002 ) ;
#178475 = AXIS2_PLACEMENT_3D ( 'NONE', #159418, #22483, #238950 ) ;
#178476 = CARTESIAN_POINT ( 'NONE',  ( -16.87683809663752754, 12.46323881132462397, -211.8640726678501380 ) ) ;
#178477 = DIRECTION ( 'NONE',  ( 0.000000000000000000, -0.8814952561688430555, 0.4721928772777347350 ) ) ;
#178478 = LINE ( 'NONE', #59753, #197263 ) ;
#178479 = CARTESIAN_POINT ( 'NONE',  ( -21.00000000000000000, 6.258114003436814343, 11.90000000000000036 ) ) ;
#178480 = AXIS2_PLACEMENT_3D ( 'NONE', #39974, #253840, #217269 ) ;
#178482 = CARTESIAN_POINT ( 'NONE',  ( 21.05000000000000071, 67.92720994251783395, -214.1870976236629929 ) ) ;
#178481 = DIRECTION ( 'NONE',  ( 0.000000000000000000, 0.2128009952263603399, -0.9770955615653315052 ) ) ;
#178483 = EDGE_LOOP ( 'NONE', ( #172691, #133142, #175593 ) ) ;
#178484 = EDGE_LOOP ( 'NONE', ( #61759, #187593, #87116, #196730, #184277 ) ) ;
#178485 = DIRECTION ( 'NONE',  ( 0.000000000000000000, -0.9999176327611369874, 0.01283462868041984617 ) ) ;
#178487 = VERTEX_POINT ( 'NONE', #38759 ) ;
#178486 = CARTESIAN_POINT ( 'NONE',  ( 18.49999999999999645, 76.00000000001190870, -103.0231074845243029 ) ) ;
#178488 = LINE ( 'NONE', #215013, #46626 ) ;
#178489 = ORIENTED_EDGE ( 'NONE', *, *, #219388, .T. ) ;
#178490 = CARTESIAN_POINT ( 'NONE',  ( -18.39999999999999858, 85.50000000001242029, -163.4229180933022576 ) ) ;
#178491 = ORIENTED_EDGE ( 'NONE', *, *, #185825, .T. ) ;
#178492 = DIRECTION ( 'NONE',  ( -0.7071067811865456854, -0.7071067811865493491, -4.937700262164544098E-15 ) ) ;
#178493 = VERTEX_POINT ( 'NONE', #140403 ) ;
#178494 = DIRECTION ( 'NONE',  ( 1.000000000000000000, -0.000000000000000000, -0.000000000000000000 ) ) ;
#178495 = CARTESIAN_POINT ( 'NONE',  ( -21.14999999999999858, -0.09999999999999939493, 11.64957080754479968 ) ) ;
#178496 = AXIS2_PLACEMENT_3D ( 'NONE', #122102, #201625, #26874 ) ;
#178497 = AXIS2_PLACEMENT_3D ( 'NONE', #255685, #172396, #134479 ) ;
#178498 = TOROIDAL_SURFACE ( 'NONE', #207711, 11.70000000000000639, 0.1000000000000000056 ) ;
#178500 = ORIENTED_EDGE ( 'NONE', *, *, #33761, .T. ) ;
#178499 = ORIENTED_EDGE ( 'NONE', *, *, #14271, .F. ) ;
#178501 = ORIENTED_EDGE ( 'NONE', *, *, #90687, .F. ) ;
#178502 = CARTESIAN_POINT ( 'NONE',  ( -23.25000000000000000, 36.65892442174472876, -249.5511627012454596 ) ) ;
#178504 = VERTEX_POINT ( 'NONE', #219954 ) ;
#178503 = B_SPLINE_CURVE_WITH_KNOTS ( 'NONE', 3,
 ( #236283, #94198, #115061, #154235, #156781, #194628, #198441, #36842, #175083, #254535, #75937, #155506, #58901, #18528, #235013, #56346, #96745, #216719, #176337, #78481, #118926, #38104, #139734, #19831, #99318, #117626, #60207, #197150, #158087, #223134 ),
 .UNSPECIFIED., .F., .F.,
 ( 4, 2, 2, 2, 2, 2, 2, 2, 2, 2, 2, 2, 2, 2, 4 ),
 ( 0.000000000000000000, 0.0003422764154113409332, 0.0006845528308226818664, 0.001026829246234022908, 0.001369105661645363733, 0.002053658492468026734, 0.002738211323290689735, 0.003080487738702024272, 0.003422764154113357941, 0.003765040569524692477, 0.004107316984936026580, 0.004449593400347361116, 0.004791869815758694785, 0.005134146231170027587, 0.005476422646581360389 ),
 .UNSPECIFIED. ) ;
#178505 = ORIENTED_EDGE ( 'NONE', *, *, #34341, .F. ) ;
#178506 = CYLINDRICAL_SURFACE ( 'NONE', #38848, 0.09999999999998898659 ) ;
#178508 = ORIENTED_EDGE ( 'NONE', *, *, #210309, .T. ) ;
#178507 = DIRECTION ( 'NONE',  ( 1.000000000000000000, 0.000000000000000000, 0.000000000000000000 ) ) ;
#178509 = TOROIDAL_SURFACE ( 'NONE', #66041, 3.899999999999999467, 0.1000000000000000056 ) ;
#178511 = CARTESIAN_POINT ( 'NONE',  ( 21.14999999999999503, 87.75000000001202238, -114.7731074845242318 ) ) ;
#178510 = CARTESIAN_POINT ( 'NONE',  ( 21.87500000000000355, 66.25000000001227818, -157.6731074845244223 ) ) ;
#178512 = CARTESIAN_POINT ( 'NONE',  ( -23.25000000000000000, 76.00000000001142553, -36.02310748452432421 ) ) ;
#178513 = CARTESIAN_POINT ( 'NONE',  ( 20.94999999999999929, 1.115600667400684642E-11, -134.0000000000000284 ) ) ;
#178514 = DIRECTION ( 'NONE',  ( -1.000000000000000000, 0.000000000000000000, 0.000000000000000000 ) ) ;
#178515 = ORIENTED_EDGE ( 'NONE', *, *, #105016, .T. ) ;
#178516 = EDGE_LOOP ( 'NONE', ( #154654, #57455, #195687, #84695 ) ) ;
#178517 = DIRECTION ( 'NONE',  ( 0.000000000000000000, -1.000000000000000000, -7.272083257015735086E-15 ) ) ;
#178518 = CARTESIAN_POINT ( 'NONE',  ( -16.86578989773640913, 66.01519019875343020, -149.0584425979022001 ) ) ;
#178519 = CARTESIAN_POINT ( 'NONE',  ( -18.50000000000000000, 64.35000000001205933, -124.2731074845243882 ) ) ;
#178520 = ADVANCED_FACE ( 'NONE', ( #161284 ), #201669, .T. ) ;
#178521 = EDGE_LOOP ( 'NONE', ( #239812, #90572, #48679, #78284 ) ) ;
#178522 = AXIS2_PLACEMENT_3D ( 'NONE', #238702, #202149, #100444 ) ;
#178524 = DIRECTION ( 'NONE',  ( 1.000000000000000000, -3.151514657663852580E-16, 8.547182517843351137E-17 ) ) ;
#178523 = AXIS2_PLACEMENT_3D ( 'NONE', #11808, #67899, #164446 ) ;
#178525 = CIRCLE ( 'NONE', #37056, 0.5000000000000004441 ) ;
#178526 = DIRECTION ( 'NONE',  ( 0.000000000000000000, -0.9579639084728132081, -0.2868887416116073785 ) ) ;
#178527 = CARTESIAN_POINT ( 'NONE',  ( 18.59999999999999432, 77.86671491006887891, -57.77043223824230722 ) ) ;
#178528 = AXIS2_PLACEMENT_3D ( 'NONE', #170656, #247569, #89766 ) ;
#178529 = VERTEX_POINT ( 'NONE', #103835 ) ;
#178530 = ORIENTED_EDGE ( 'NONE', *, *, #8665, .F. ) ;
#178531 = FACE_OUTER_BOUND ( 'NONE', #135249, .T. ) ;
#178532 = DIRECTION ( 'NONE',  ( 0.7071067811865475727, 0.6824534298470373850, -0.1850873201762210096 ) ) ;
#178533 = ORIENTED_EDGE ( 'NONE', *, *, #38761, .T. ) ;
#178534 = FACE_OUTER_BOUND ( 'NONE', #851, .T. ) ;
#178535 = EDGE_LOOP ( 'NONE', ( #68809, #80494, #9725 ) ) ;
#178536 = LINE ( 'NONE', #80664, #252144 ) ;
#178538 = DIRECTION ( 'NONE',  ( 0.000000000000000000, 0.000000000000000000, 1.000000000000000000 ) ) ;
#178537 = SHAPE_REPRESENTATION ( 'Injection Molded Chain Links 14', ( #2425 ), #185415 ) ;
#178539 = FILL_AREA_STYLE ('',( #98939 ) ) ;
#178540 = AXIS2_PLACEMENT_3D ( 'NONE', #13374, #208994, #91617 ) ;
#178541 = EDGE_CURVE ( 'NONE', #77793, #233092, #244552, .T. ) ;
#178542 = CARTESIAN_POINT ( 'NONE',  ( 22.49806830649814060, 0.07746431633666323036, -55.35011034516096373 ) ) ;
#178543 = DIRECTION ( 'NONE',  ( -1.000000000000000000, 0.000000000000000000, 0.000000000000000000 ) ) ;
#178544 = AXIS2_PLACEMENT_3D ( 'NONE', #37877, #39162, #54830 ) ;
#178545 = CARTESIAN_POINT ( 'NONE',  ( -19.95857864376268509, 4.513204987021262937, 22.00000000000000355 ) ) ;
#178548 = ORIENTED_EDGE ( 'NONE', *, *, #189856, .F. ) ;
#178547 = ORIENTED_EDGE ( 'NONE', *, *, #186812, .F. ) ;
#178546 = AXIS2_PLACEMENT_3D ( 'NONE', #148709, #49595, #202252 ) ;
#178549 = EDGE_LOOP ( 'NONE', ( #242162, #93088, #78501, #239811 ) ) ;
#178550 = CIRCLE ( 'NONE', #61998, 0.1000000000000008937 ) ;
#178551 = AXIS2_PLACEMENT_3D ( 'NONE', #130368, #108256, #52107 ) ;
#178552 = EDGE_CURVE ( 'NONE', #105294, #192091, #90438, .T. ) ;
#178553 = CARTESIAN_POINT ( 'NONE',  ( -18.69999999999999929, 7.799999999999999822, 1.212568896937007867 ) ) ;
#178554 = CARTESIAN_POINT ( 'NONE',  ( -22.60000000000080789, 75.95218301954636786, -81.27312991567707456 ) ) ;
#178556 = ADVANCED_FACE ( 'NONE', ( #120886 ), #202951, .T. ) ;
#178555 = DIRECTION ( 'NONE',  ( 0.000000000000000000, 0.000000000000000000, -1.000000000000000000 ) ) ;
#178557 = DIRECTION ( 'NONE',  ( 0.000000000000000000, 0.000000000000000000, -1.000000000000000000 ) ) ;
#178558 = AXIS2_PLACEMENT_3D ( 'NONE', #48586, #70757, #151580 ) ;
#178560 = CARTESIAN_POINT ( 'NONE',  ( -20.64999999999999858, -8.730841121484171907, -177.0980747189843214 ) ) ;
#178559 = DIRECTION ( 'NONE',  ( 0.000000000000000000, -6.938893903907222067E-15, 1.000000000000000000 ) ) ;
#178561 = VERTEX_POINT ( 'NONE', #62173 ) ;
#178562 = DIRECTION ( 'NONE',  ( 0.000000000000000000, -0.8814952561688430555, 0.4721928772777346239 ) ) ;
#178563 = ORIENTED_EDGE ( 'NONE', *, *, #102024, .T. ) ;
#178564 = ADVANCED_FACE ( 'NONE', ( #20491 ), #183405, .F. ) ;
#178565 = DIRECTION ( 'NONE',  ( -1.000000000000000000, 0.000000000000000000, -0.000000000000000000 ) ) ;
#178566 = VERTEX_POINT ( 'NONE', #123426 ) ;
#178567 = ORIENTED_EDGE ( 'NONE', *, *, #151533, .T. ) ;
#178568 = DIRECTION ( 'NONE',  ( 1.000000000000000000, 0.000000000000000000, 0.000000000000000000 ) ) ;
#178569 = CARTESIAN_POINT ( 'NONE',  ( -22.39999999999999858, -1.330006220153263641, -194.8931527402181700 ) ) ;
#178570 = CARTESIAN_POINT ( 'NONE',  ( 21.05000000000000071, 65.27628289530404970, -57.37310748452439668 ) ) ;
#178571 = CIRCLE ( 'NONE', #66103, 0.09999999999999939493 ) ;
#178572 = CIRCLE ( 'NONE', #149330, 2.000000000000001776 ) ;
#178573 = DIRECTION ( 'NONE',  ( -1.000000000000000000, -3.190570557967288949E-16, -6.948722487160392945E-17 ) ) ;
#178574 = ORIENTED_EDGE ( 'NONE', *, *, #46303, .T. ) ;
#178576 = EDGE_LOOP ( 'NONE', ( #32383, #225319, #136401, #82464 ) ) ;
#178575 = EDGE_CURVE ( 'NONE', #229356, #240051, #240471, .T. ) ;
#178577 = DIRECTION ( 'NONE',  ( 0.000000000000000000, 0.4999999999999994449, 0.8660254037844390407 ) ) ;
#178578 = CARTESIAN_POINT ( 'NONE',  ( -18.59999999999999787, 30.36376046184471988, -235.5720385971402493 ) ) ;
#178579 = EDGE_LOOP ( 'NONE', ( #73495, #80727, #10670, #181417, #152255 ) ) ;
#178580 = CARTESIAN_POINT ( 'NONE',  ( 18.50000000000000000, -9.399999999988843058, -40.49928567783884858 ) ) ;
#178581 = CARTESIAN_POINT ( 'NONE',  ( -21.14999999999999858, 64.35000000001166143, -69.42310748452440805 ) ) ;
#178582 = CARTESIAN_POINT ( 'NONE',  ( 23.14999999999999858, 76.00000000001126921, -203.5231074845248997 ) ) ;
#178583 = CARTESIAN_POINT ( 'NONE',  ( 21.10000000000000142, 0.000000000000000000, 0.000000000000000000 ) ) ;
#178584 = CARTESIAN_POINT ( 'NONE',  ( -16.77683809663752257, 66.05416425680770942, -90.35915846542016538 ) ) ;
#178585 = DIRECTION ( 'NONE',  ( 0.000000000000000000, -0.4999999999999478195, -0.8660254037844686836 ) ) ;
#178587 = FACE_OUTER_BOUND ( 'NONE', #168160, .T. ) ;
#178586 = CARTESIAN_POINT ( 'NONE',  ( -16.94445028196807002, 30.26380394232451465, -234.7901145182196956 ) ) ;
#178588 = CARTESIAN_POINT ( 'NONE',  ( 20.94999999999999929, 76.00000000001213607, -136.5231074845242745 ) ) ;
#178589 = AXIS2_PLACEMENT_3D ( 'NONE', #217515, #139253, #214964 ) ;
#178590 = ADVANCED_FACE ( 'NONE', ( #137832 ), #30768, .F. ) ;
#178591 = CARTESIAN_POINT ( 'NONE',  ( 18.49999999999999289, 65.50857864377520912, -178.6731074845244223 ) ) ;
#178592 = DIRECTION ( 'NONE',  ( 0.000000000000000000, 0.2617529984164915779, 0.9651348961777187485 ) ) ;
#178593 = CIRCLE ( 'NONE', #191049, 3.899999999999993694 ) ;
#178594 = CARTESIAN_POINT ( 'NONE',  ( -17.22767730082241044, 10.34924421247839454, -55.64242869057007113 ) ) ;
#178595 = ORIENTED_EDGE ( 'NONE', *, *, #350, .F. ) ;
#178596 = CARTESIAN_POINT ( 'NONE',  ( -18.40000000000000213, 23.66963324290564685, -229.6440402155210734 ) ) ;
#178597 = ORIENTED_EDGE ( 'NONE', *, *, #143868, .T. ) ;
#178598 = CARTESIAN_POINT ( 'NONE',  ( -23.25000000000000000, 1.115649040949250830E-11, -96.60000000000005116 ) ) ;
#178599 = CARTESIAN_POINT ( 'NONE',  ( -20.94999999999999929, 74.16465844978745281, -91.46795619196133487 ) ) ;
#178600 = CARTESIAN_POINT ( 'NONE',  ( -23.15000000000000213, 69.09936979046463534, -247.6075824278584605 ) ) ;
#178601 = AXIS2_PLACEMENT_3D ( 'NONE', #235981, #78188, #136890 ) ;
#178602 = AXIS2_PLACEMENT_3D ( 'NONE', #251049, #50277, #13738 ) ;
#178603 = ORIENTED_EDGE ( 'NONE', *, *, #5338, .T. ) ;
#178604 = FACE_OUTER_BOUND ( 'NONE', #236448, .T. ) ;
#178605 = CIRCLE ( 'NONE', #103704, 0.09999999999999939493 ) ;
#178606 = DIRECTION ( 'NONE',  ( -0.000000000000000000, 6.982962677686266711E-15, -1.000000000000000000 ) ) ;
#178607 = DIRECTION ( 'NONE',  ( 1.000000000000000000, 0.000000000000000000, 0.000000000000000000 ) ) ;
#178608 = FACE_OUTER_BOUND ( 'NONE', #123923, .T. ) ;
#178609 = CARTESIAN_POINT ( 'NONE',  ( 18.49999999999998934, 10.37342005527971800, -24.76578812462619794 ) ) ;
#178610 = FACE_OUTER_BOUND ( 'NONE', #60018, .T. ) ;
#178611 = EDGE_CURVE ( 'NONE', #58070, #45271, #53019, .T. ) ;
#178612 = EDGE_CURVE ( 'NONE', #63069, #131644, #48920, .T. ) ;
#178613 = EDGE_LOOP ( 'NONE', ( #182439, #81574, #240063, #143865 ) ) ;
#178614 = DIRECTION ( 'NONE',  ( -1.000000000000000000, 0.000000000000000000, -0.000000000000000000 ) ) ;
#178616 = ORIENTED_EDGE ( 'NONE', *, *, #55401, .F. ) ;
#178615 = LINE ( 'NONE', #36543, #130239 ) ;
#178617 = CYLINDRICAL_SURFACE ( 'NONE', #30126, 2.000000000000001776 ) ;
#178618 = CARTESIAN_POINT ( 'NONE',  ( 20.85000000000000142, 7.783179459866048866, -245.3643104511423019 ) ) ;
#178620 = ADVANCED_FACE ( 'NONE', ( #127276 ), #204234, .T. ) ;
#178619 = FACE_OUTER_BOUND ( 'NONE', #12033, .T. ) ;
#178621 = ADVANCED_FACE ( 'NONE', ( #29496 ), #148730, .T. ) ;
#178622 = ORIENTED_EDGE ( 'NONE', *, *, #50018, .F. ) ;
#178623 = CARTESIAN_POINT ( 'NONE',  ( -22.44366136229477249, 75.99065843052615321, -148.1728260419982064 ) ) ;
#178624 = CIRCLE ( 'NONE', #136894, 0.1999999999999987343 ) ;
#178625 = APPLICATION_PROTOCOL_DEFINITION ( 'draft international standard', 'automotive_design', 1998, #2476 ) ;
#178626 = CARTESIAN_POINT ( 'NONE',  ( 20.84999999999998721, -11.74999999998884448, -134.0000000000000284 ) ) ;
#178627 = EDGE_CURVE ( 'NONE', #149274, #182870, #256987, .T. ) ;
#178628 = ORIENTED_EDGE ( 'NONE', *, *, #75288, .F. ) ;
#178629 = CARTESIAN_POINT ( 'NONE',  ( 23.15000000000000213, -9.599999999988845900, -177.3939691226524076 ) ) ;
#178630 = DIRECTION ( 'NONE',  ( 0.000000000000000000, 0.2128009952263604232, -0.9770955615653316162 ) ) ;
#178631 = EDGE_CURVE ( 'NONE', #108582, #183834, #190434, .T. ) ;
#178633 = EDGE_CURVE ( 'NONE', #170631, #44131, #23839, .T. ) ;
#178632 = ADVANCED_FACE ( 'NONE', ( #129829 ), #144245, .F. ) ;
#178634 = FACE_OUTER_BOUND ( 'NONE', #104733, .T. ) ;
#178635 = ORIENTED_EDGE ( 'NONE', *, *, #95700, .F. ) ;
#178636 = EDGE_LOOP ( 'NONE', ( #246682, #18419 ) ) ;
#178637 = DIRECTION ( 'NONE',  ( 1.000000000000000000, 0.000000000000000000, 0.000000000000000000 ) ) ;
#178638 = CARTESIAN_POINT ( 'NONE',  ( 21.05000000000000071, 8.776282895303632259, -45.65000000000000568 ) ) ;
#178639 = CARTESIAN_POINT ( 'NONE',  ( -20.64999999999999858, 71.65000000001259650, -191.2731074845243882 ) ) ;
#178640 = CARTESIAN_POINT ( 'NONE',  ( -22.50000000000000000, 64.25000000001215028, -136.5231074845243597 ) ) ;
#178641 = ADVANCED_FACE ( 'NONE', ( #243361 ), #89419, .F. ) ;
#178642 = CARTESIAN_POINT ( 'NONE',  ( 20.94999999999999574, -11.64999999998883595, -103.4000000000000341 ) ) ;
#178643 = DIRECTION ( 'NONE',  ( 1.000000000000000000, 0.000000000000000000, 0.000000000000000000 ) ) ;
#178645 = DIRECTION ( 'NONE',  ( 0.000000000000000000, 0.000000000000000000, -1.000000000000000000 ) ) ;
#178644 = DIRECTION ( 'NONE',  ( 0.000000000000000000, 0.000000000000000000, 1.000000000000000000 ) ) ;
#178646 = CIRCLE ( 'NONE', #91126, 2.000000000000009326 ) ;
#178648 = LINE ( 'NONE', #258099, #40425 ) ;
#178647 = AXIS2_PLACEMENT_3D ( 'NONE', #82242, #79691, #216650 ) ;
#178650 = ADVANCED_FACE ( 'NONE', ( #247211 ), #69891, .T. ) ;
#178649 = CARTESIAN_POINT ( 'NONE',  ( -21.05000000000000071, 70.44746257310249860, -228.4383880063670347 ) ) ;
#178651 = DIRECTION ( 'NONE',  ( 0.000000000000000000, 1.000000000000000000, 0.000000000000000000 ) ) ;
#178652 = VECTOR ( 'NONE', #142345, 1000.000000000000000 ) ;
#178655 = ADVANCED_FACE ( 'NONE', ( #165120 ), #149427, .T. ) ;
#178654 = DIRECTION ( 'NONE',  ( -1.000000000000000000, 0.000000000000000000, 0.000000000000000000 ) ) ;
#178653 = AXIS2_PLACEMENT_3D ( 'NONE', #22979, #199021, #179476 ) ;
#178656 = B_SPLINE_CURVE_WITH_KNOTS ( 'NONE', 3,
 ( #200375, #165096, #128536, #226323, #127254, #106380, #247186, #67275, #206790, #26899 ),
 .UNSPECIFIED., .F., .F.,
 ( 4, 2, 2, 2, 4 ),
 ( 0.000000000000000000, 0.0001660831991682119001, 0.0002491247987523189885, 0.0002906455985443902866, 0.0003321663983364616930 ),
 .UNSPECIFIED. ) ;
#178657 = ORIENTED_EDGE ( 'NONE', *, *, #218, .F. ) ;
#178658 = ORIENTED_EDGE ( 'NONE', *, *, #182096, .F. ) ;
#178659 = FACE_OUTER_BOUND ( 'NONE', #86415, .T. ) ;
#178661 = CARTESIAN_POINT ( 'NONE',  ( 21.08832698747859169, 67.22463560659538473, -191.2943900180602554 ) ) ;
#178660 = FACE_OUTER_BOUND ( 'NONE', #168012, .T. ) ;
#178662 = EDGE_CURVE ( 'NONE', #245418, #99200, #244642, .T. ) ;
#178663 = AXIS2_PLACEMENT_3D ( 'NONE', #112214, #169645, #168362 ) ;
#178664 = DIRECTION ( 'NONE',  ( 1.000000000000000000, 0.000000000000000000, 0.000000000000000000 ) ) ;
#178665 = DIRECTION ( 'NONE',  ( 1.073024830501117725E-15, 0.000000000000000000, 1.000000000000000000 ) ) ;
#178666 = CARTESIAN_POINT ( 'NONE',  ( -17.78043020864320667, 10.85359211201684637, -90.16304916572026684 ) ) ;
#178667 = ADVANCED_FACE ( 'NONE', ( #166436 ), #44665, .T. ) ;
#178668 = VERTEX_POINT ( 'NONE', #228949 ) ;
#178669 = EDGE_CURVE ( 'NONE', #41121, #104038, #77958, .T. ) ;
#178670 = FACE_OUTER_BOUND ( 'NONE', #112999, .T. ) ;
#178671 = EDGE_LOOP ( 'NONE', ( #139311, #1336, #50640, #234798, #7596 ) ) ;
#178672 = CIRCLE ( 'NONE', #128566, 0.09999999999998898659 ) ;
#178673 = AXIS2_PLACEMENT_3D ( 'NONE', #14347, #92556, #249097 ) ;
#178675 = CIRCLE ( 'NONE', #232825, 0.09999999999999939493 ) ;
#178674 = CARTESIAN_POINT ( 'NONE',  ( -22.94999999999999929, 8.000000000000000000, 1.212568896937007867 ) ) ;
#178676 = EDGE_LOOP ( 'NONE', ( #7294, #183915, #43327, #142731 ) ) ;
#178677 = CARTESIAN_POINT ( 'NONE',  ( 21.14999999999999503, 26.06832281015329755, -254.4051978787608732 ) ) ;
#178678 = B_SPLINE_CURVE_WITH_KNOTS ( 'NONE', 3,
 ( #221463, #101497, #181100, #161538, #78116, #218907, #237214, #16892 ),
 .UNSPECIFIED., .F., .F.,
 ( 4, 2, 2, 4 ),
 ( 0.000000000000000000, 0.0001094981963948503753, 0.0002189963927897007505, 0.0004379927855793972185 ),
 .UNSPECIFIED. ) ;
#178679 = CIRCLE ( 'NONE', #203579, 7.900000000000000355 ) ;
#178680 = LINE ( 'NONE', #216474, #221281 ) ;
#178681 = ORIENTED_EDGE ( 'NONE', *, *, #18326, .T. ) ;
#178682 = CARTESIAN_POINT ( 'NONE',  ( -1.739115166359751801E-14, 11.65000000001114699, -112.7500000000000284 ) ) ;
#178683 = ORIENTED_EDGE ( 'NONE', *, *, #86576, .F. ) ;
#178684 = DIRECTION ( 'NONE',  ( 0.000000000000000000, 0.000000000000000000, 1.000000000000000000 ) ) ;
#178685 = LINE ( 'NONE', #7238, #207567 ) ;
#178686 = DIRECTION ( 'NONE',  ( -1.000000000000000000, 0.000000000000000000, 0.000000000000000000 ) ) ;
#178687 = CARTESIAN_POINT ( 'NONE',  ( -21.05000000000000071, 7.219003623157315808, -233.4904674204326227 ) ) ;
#178688 = CARTESIAN_POINT ( 'NONE',  ( -22.50000000000000000, 1.115600667400684642E-11, -133.9000000000000057 ) ) ;
#178690 = CARTESIAN_POINT ( 'NONE',  ( -21.14999999999999858, 1.115600667400684642E-11, -67.00000000000004263 ) ) ;
#178689 = DIRECTION ( 'NONE',  ( 0.000000000000000000, 0.000000000000000000, -1.000000000000000000 ) ) ;
#178691 = CARTESIAN_POINT ( 'NONE',  ( -23.15000000000000213, 76.00000000001165290, -69.52310748452431710 ) ) ;
#178692 = ORIENTED_EDGE ( 'NONE', *, *, #183659, .T. ) ;
#178694 = CARTESIAN_POINT ( 'NONE',  ( -20.94999999999999929, 3.047642603966940200, -208.5984958277594785 ) ) ;
#178693 = CARTESIAN_POINT ( 'NONE',  ( -16.88593481969334675, 9.950560090095464716, -188.3518722569444606 ) ) ;
#178696 = ORIENTED_EDGE ( 'NONE', *, *, #176262, .F. ) ;
#178695 = AXIS2_PLACEMENT_3D ( 'NONE', #20690, #158918, #238432 ) ;
#178698 = ORIENTED_EDGE ( 'NONE', *, *, #194612, .F. ) ;
#178697 = DIRECTION ( 'NONE',  ( -7.304098846218134667E-16, 1.000000000000000000, 6.982962677686267499E-15 ) ) ;
#178699 = CIRCLE ( 'NONE', #241220, 0.5000000000000004441 ) ;
#178700 = VERTEX_POINT ( 'NONE', #9885 ) ;
#178701 = CARTESIAN_POINT ( 'NONE',  ( -21.05000000000000071, 7.872214528623314500, -209.6555322433423783 ) ) ;
#178702 = CARTESIAN_POINT ( 'NONE',  ( -21.14999999999999858, 64.25000000001237765, -169.9231074845244507 ) ) ;
#178703 = CARTESIAN_POINT ( 'NONE',  ( 19.97071067811864609, 11.72071067812981404, -158.6500000000000057 ) ) ;
#178704 = CARTESIAN_POINT ( 'NONE',  ( -18.37013991200266005, 20.67483879484485954, -227.9431972973032998 ) ) ;
#178705 = ORIENTED_EDGE ( 'NONE', *, *, #250878, .T. ) ;
#178706 = DIRECTION ( 'NONE',  ( 1.000000000000000000, -0.000000000000000000, 0.000000000000000000 ) ) ;
#178707 = CARTESIAN_POINT ( 'NONE',  ( 18.49999999999999289, 10.20857864377384239, -125.2671572875254071 ) ) ;
#178708 = CIRCLE ( 'NONE', #37213, 0.1000000000000089567 ) ;
#178709 = CARTESIAN_POINT ( 'NONE',  ( 18.39999999999999858, 37.99112772578902764, -261.0419300540664835 ) ) ;
#178710 = ORIENTED_EDGE ( 'NONE', *, *, #45812, .F. ) ;
#178711 = CARTESIAN_POINT ( 'NONE',  ( -20.94999999999999929, 77.25000000001209344, -128.5231074845242745 ) ) ;
#178712 = EDGE_CURVE ( 'NONE', #254860, #54914, #173893, .T. ) ;
#178713 = CARTESIAN_POINT ( 'NONE',  ( 21.08884785362045378, 6.357193367425240105, 0.04978309506684791552 ) ) ;
#178714 = ORIENTED_EDGE ( 'NONE', *, *, #188224, .T. ) ;
#178715 = ORIENTED_EDGE ( 'NONE', *, *, #107932, .T. ) ;
#178716 = CIRCLE ( 'NONE', #149657, 0.1000000000000124678 ) ;
#178717 = ADVANCED_FACE ( 'NONE', ( #12483 ), #194974, .T. ) ;
#178718 = CARTESIAN_POINT ( 'NONE',  ( 21.05000000000000071, 11.65000000001116298, -146.1500000000000341 ) ) ;
#178719 = CIRCLE ( 'NONE', #257725, 0.09999999999999986677 ) ;
#178720 = ORIENTED_EDGE ( 'NONE', *, *, #104326, .F. ) ;
#178721 = DIRECTION ( 'NONE',  ( 0.000000000000000000, -0.1298341882520022694, -0.9915357197604852679 ) ) ;
#178723 = ORIENTED_EDGE ( 'NONE', *, *, #165052, .T. ) ;
#178722 = AXIS2_PLACEMENT_3D ( 'NONE', #44893, #243082, #47436 ) ;
#178724 = CARTESIAN_POINT ( 'NONE',  ( 20.86777300164945004, 10.33200063080771969, -173.0931674956643178 ) ) ;
#178725 = EDGE_CURVE ( 'NONE', #145261, #217224, #111567, .T. ) ;
#178726 = EDGE_CURVE ( 'NONE', #154195, #218718, #211962, .T. ) ;
#178727 = CYLINDRICAL_SURFACE ( 'NONE', #1024, 0.1000000000000013933 ) ;
#178728 = CARTESIAN_POINT ( 'NONE',  ( 20.95512820512820440, 60.90483797576755620, -225.2715357783924333 ) ) ;
#178729 = DIRECTION ( 'NONE',  ( 0.000000000000000000, -1.000000000000000000, 0.000000000000000000 ) ) ;
#178730 = TOROIDAL_SURFACE ( 'NONE', #62171, 11.70000000000000107, 0.1000000000000000056 ) ;
#178731 = AXIS2_PLACEMENT_3D ( 'NONE', #63799, #22125, #41684 ) ;
#178732 = DIRECTION ( 'NONE',  ( 0.000000000000000000, -1.000000000000000000, -6.982962677686265922E-15 ) ) ;
#178733 = CARTESIAN_POINT ( 'NONE',  ( 18.49999999999999645, 1.866714910068465239, -45.25267524628200988 ) ) ;
#178734 = DIRECTION ( 'NONE',  ( -1.000000000000000000, 0.000000000000000000, 0.000000000000000000 ) ) ;
#178735 = ORIENTED_EDGE ( 'NONE', *, *, #148218, .F. ) ;
#178737 = DIRECTION ( 'NONE',  ( 1.000000000000000000, 0.000000000000000000, 0.000000000000000000 ) ) ;
#178736 = CARTESIAN_POINT ( 'NONE',  ( 23.14999999999999858, -11.74999999998883560, -155.7499999999999716 ) ) ;
#178738 = VERTEX_POINT ( 'NONE', #56684 ) ;
#178741 = ORIENTED_EDGE ( 'NONE', *, *, #220206, .F. ) ;
#178740 = CARTESIAN_POINT ( 'NONE',  ( -18.50000000000000000, -7.558719773525646168, -210.9360835033311332 ) ) ;
#178739 = CARTESIAN_POINT ( 'NONE',  ( 20.95000000000005969, 61.64150943397345372, -36.51839050339276582 ) ) ;
#178742 = EDGE_CURVE ( 'NONE', #129819, #2197, #119682, .T. ) ;
#178743 = TOROIDAL_SURFACE ( 'NONE', #87096, 0.2000000000000000111, 0.1000000000000000056 ) ;
#178744 = ORIENTED_EDGE ( 'NONE', *, *, #192496, .F. ) ;
#178745 = DIRECTION ( 'NONE',  ( 0.7071067811865474617, 0.7071067811865474617, 0.000000000000000000 ) ) ;
#178747 = ADVANCED_FACE ( 'NONE', ( #51551 ), #251057, .T. ) ;
#178746 = AXIS2_PLACEMENT_3D ( 'NONE', #41688, #46786, #225419 ) ;
#178748 = MECHANICAL_DESIGN_GEOMETRIC_PRESENTATION_REPRESENTATION (  '', ( #253690 ), #207942 ) ;
#178749 = DIRECTION ( 'NONE',  ( 2.952720810173289112E-16, 0.9651348961777157509, -0.2617529984165031243 ) ) ;
#178750 = CIRCLE ( 'NONE', #66078, 0.1000000000000072220 ) ;
#178751 = CARTESIAN_POINT ( 'NONE',  ( 21.05000000000000071, 77.16270174995010223, -128.4231074845242802 ) ) ;
#178752 = CARTESIAN_POINT ( 'NONE',  ( -16.79139129368504157, 9.944944162472831195, -113.1702446328258560 ) ) ;
#178753 = ORIENTED_EDGE ( 'NONE', *, *, #103012, .F. ) ;
#178754 = CARTESIAN_POINT ( 'NONE',  ( 19.99999999738088974, 16.73432760861077995, -222.6213144456777400 ) ) ;
#178755 = CIRCLE ( 'NONE', #237158, 0.2000000000000005107 ) ;
#178756 = DIRECTION ( 'NONE',  ( 0.000000000000000000, 0.9579639084728132081, 0.2868887416116073785 ) ) ;
#178758 = CARTESIAN_POINT ( 'NONE',  ( 20.95035502843362707, 10.47763832677646789, -7.576299708736373262 ) ) ;
#178757 = CARTESIAN_POINT ( 'NONE',  ( -23.25000000000000000, 1.115600667400684642E-11, -175.4000000000000341 ) ) ;
#178760 = EDGE_LOOP ( 'NONE', ( #97154, #187623, #194285, #110725 ) ) ;
#178759 = CARTESIAN_POINT ( 'NONE',  ( 18.59999999999999787, 1.851028230152016674, -112.1539132694225316 ) ) ;
#178761 = EDGE_CURVE ( 'NONE', #75249, #44800, #236380, .T. ) ;
#178762 = PRODUCT_DEFINITION_SHAPE ( 'NONE', 'NONE',  #258110 ) ;
#178763 = ORIENTED_EDGE ( 'NONE', *, *, #95373, .T. ) ;
#178764 = ADVANCED_BREP_SHAPE_REPRESENTATION ( '', ( #110136, #2425 ), #77591 ) ;
#178765 = EDGE_CURVE ( 'NONE', #137793, #151535, #240652, .T. ) ;
#178766 = CARTESIAN_POINT ( 'NONE',  ( -16.92570016628985030, 44.10510403810827995, -235.3029098272679107 ) ) ;
#178767 = ORIENTED_EDGE ( 'NONE', *, *, #159858, .T. ) ;
#178768 = DIRECTION ( 'NONE',  ( 1.000000000000000000, -0.000000000000000000, 0.000000000000000000 ) ) ;
#178769 = VERTEX_POINT ( 'NONE', #210661 ) ;
#178770 = CARTESIAN_POINT ( 'NONE',  ( -18.40000000000000213, 11.33174054713631662, -146.6500000000000341 ) ) ;
#178771 = DIRECTION ( 'NONE',  ( 0.000000000000000000, 0.000000000000000000, -1.000000000000000000 ) ) ;
#178772 = DIRECTION ( 'NONE',  ( 0.000000000000000000, 1.897661533703519897E-16, -1.000000000000000000 ) ) ;
#178773 = VERTEX_POINT ( 'NONE', #214503 ) ;
#178774 = ADVANCED_FACE ( 'NONE', ( #16335 ), #52859, .T. ) ;
#178775 = DIRECTION ( 'NONE',  ( 0.000000000000000000, 0.8814952561688444987, -0.4721928772777320149 ) ) ;
#178776 = AXIS2_PLACEMENT_3D ( 'NONE', #36198, #156154, #92291 ) ;
#178777 = EDGE_CURVE ( 'NONE', #179358, #46322, #219795, .T. ) ;
#178778 = CIRCLE ( 'NONE', #245386, 0.09999999999999939493 ) ;
#178779 = VECTOR ( 'NONE', #230598, 1000.000000000000114 ) ;
#178780 = EDGE_CURVE ( 'NONE', #18436, #168199, #37180, .T. ) ;
#178781 = DIRECTION ( 'NONE',  ( -1.000000000000000000, 0.000000000000000000, 0.000000000000000000 ) ) ;
#178782 = B_SPLINE_CURVE_WITH_KNOTS ( 'NONE', 3,
 ( #153135, #175264, #254709, #214350, #77387, #218173 ),
 .UNSPECIFIED., .F., .F.,
 ( 4, 2, 4 ),
 ( 0.000000000000000000, 0.0001496588209255797074, 0.0002993176418511594148 ),
 .UNSPECIFIED. ) ;
#178783 = VECTOR ( 'NONE', #74954, 1000.000000000000000 ) ;
#178784 = EDGE_LOOP ( 'NONE', ( #121975, #144669, #229398, #194863 ) ) ;
#178785 = ORIENTED_EDGE ( 'NONE', *, *, #95466, .T. ) ;
#178786 = ORIENTED_EDGE ( 'NONE', *, *, #58664, .F. ) ;
#178787 = CYLINDRICAL_SURFACE ( 'NONE', #41757, 0.09999999999998898659 ) ;
#178788 = ORIENTED_EDGE ( 'NONE', *, *, #47806, .F. ) ;
#178790 = ORIENTED_EDGE ( 'NONE', *, *, #160611, .T. ) ;
#178789 = DIRECTION ( 'NONE',  ( 0.000000000000000000, 0.000000000000000000, -1.000000000000000000 ) ) ;
#178791 = EDGE_CURVE ( 'NONE', #152802, #158579, #225549, .T. ) ;
#178792 = ORIENTED_EDGE ( 'NONE', *, *, #204477, .T. ) ;
#178793 = CIRCLE ( 'NONE', #212080, 0.1000000000000075273 ) ;
#178796 = ORIENTED_EDGE ( 'NONE', *, *, #18802, .F. ) ;
#178795 = VERTEX_POINT ( 'NONE', #73745 ) ;
#178794 = LINE ( 'NONE', #173678, #143578 ) ;
#178797 = EDGE_CURVE ( 'NONE', #220173, #148410, #215529, .T. ) ;
#178798 = AXIS2_PLACEMENT_3D ( 'NONE', #232344, #173688, #190649 ) ;
#178799 = ORIENTED_EDGE ( 'NONE', *, *, #183040, .F. ) ;
#178800 = CARTESIAN_POINT ( 'NONE',  ( -18.50000000000000000, 31.98723526783714988, -238.8784020251475511 ) ) ;
#178801 = AXIS2_PLACEMENT_3D ( 'NONE', #212497, #36440, #57232 ) ;
#178802 = DIRECTION ( 'NONE',  ( 0.000000000000000000, -0.4930308989875313852, -0.8700118002898274971 ) ) ;
#178803 = CARTESIAN_POINT ( 'NONE',  ( -16.87333278164155104, 13.99033631766475416, -218.7973121421632641 ) ) ;
#178804 = VERTEX_POINT ( 'NONE', #232817 ) ;
#178805 = FACE_OUTER_BOUND ( 'NONE', #193287, .T. ) ;
#178807 = ORIENTED_EDGE ( 'NONE', *, *, #57903, .T. ) ;
#178806 = CARTESIAN_POINT ( 'NONE',  ( 21.95218792049437795, 7.201507561257818324, -167.4009715602000483 ) ) ;
#178808 = DIRECTION ( 'NONE',  ( 0.000000000000000000, -8.717686153663073805E-15, 1.000000000000000000 ) ) ;
#178810 = ORIENTED_EDGE ( 'NONE', *, *, #162566, .T. ) ;
#178809 = FACE_OUTER_BOUND ( 'NONE', #101880, .T. ) ;
#178811 = ORIENTED_EDGE ( 'NONE', *, *, #201831, .T. ) ;
#178812 = DIRECTION ( 'NONE',  ( 0.7071067811865463515, -0.7071067811865487940, 4.930380657631324879E-32 ) ) ;
#178813 = FACE_OUTER_BOUND ( 'NONE', #201894, .T. ) ;
#178814 = ORIENTED_EDGE ( 'NONE', *, *, #36906, .T. ) ;
#178815 = ORIENTED_EDGE ( 'NONE', *, *, #98935, .F. ) ;
#178816 = CARTESIAN_POINT ( 'NONE',  ( -23.15000000000000213, 1.115600667400684642E-11, -33.50000000000000000 ) ) ;
#178817 = DIRECTION ( 'NONE',  ( 0.000000000000000000, -0.9770955615653316162, -0.2128009952263604232 ) ) ;
#178819 = ORIENTED_EDGE ( 'NONE', *, *, #158046, .F. ) ;
#178818 = VERTEX_POINT ( 'NONE', #174150 ) ;
#178820 = EDGE_LOOP ( 'NONE', ( #43013, #82803, #60448, #33968 ) ) ;
#178821 = LINE ( 'NONE', #63974, #15471 ) ;
#178822 = EDGE_LOOP ( 'NONE', ( #90591, #128794, #250774, #75239 ) ) ;
#178823 = EDGE_LOOP ( 'NONE', ( #21609, #93791, #116848, #124972 ) ) ;
#178824 = CARTESIAN_POINT ( 'NONE',  ( -18.59999999999999787, 7.120270961697594103, -37.15956304183931991 ) ) ;
#178825 = ORIENTED_EDGE ( 'NONE', *, *, #238410, .T. ) ;
#178826 = CARTESIAN_POINT ( 'NONE',  ( -18.59999999999999787, 76.00000000001237765, -170.0231074845243597 ) ) ;
#178828 = CARTESIAN_POINT ( 'NONE',  ( -18.59999999999999787, 4.252251777740764460, -211.8999245327126744 ) ) ;
#178827 = DIRECTION ( 'NONE',  ( 0.000000000000000000, -1.000000000000000000, -6.982962677686265922E-15 ) ) ;
#178829 = ORIENTED_EDGE ( 'NONE', *, *, #24457, .F. ) ;
#178831 = ORIENTED_EDGE ( 'NONE', *, *, #87636, .T. ) ;
#178830 = EDGE_LOOP ( 'NONE', ( #81790, #132942, #42773, #234331 ) ) ;
#178833 = CIRCLE ( 'NONE', #66371, 0.1000000000000028644 ) ;
#178832 = DIRECTION ( 'NONE',  ( 0.000000000000000000, 6.982962677686266711E-15, -1.000000000000000000 ) ) ;
#178834 = DIRECTION ( 'NONE',  ( 0.000000000000000000, 0.000000000000000000, -1.000000000000000000 ) ) ;
#178835 = CIRCLE ( 'NONE', #20594, 3.900000000000000799 ) ;
#178836 = AXIS2_PLACEMENT_3D ( 'NONE', #206836, #107728, #148142 ) ;
#178837 = AXIS2_PLACEMENT_3D ( 'NONE', #163141, #242648, #44475 ) ;
#178838 = ORIENTED_EDGE ( 'NONE', *, *, #56196, .T. ) ;
#178839 = AXIS2_PLACEMENT_3D ( 'NONE', #104457, #86175, #4099 ) ;
#178840 = CARTESIAN_POINT ( 'NONE',  ( 21.00000000000000000, 9.750000000011153745, -88.15000000000004832 ) ) ;
#178841 = VERTEX_POINT ( 'NONE', #175418 ) ;
#178842 = ORIENTED_EDGE ( 'NONE', *, *, #198651, .F. ) ;
#178843 = CARTESIAN_POINT ( 'NONE',  ( 23.14999999999999858, 11.65000000001116298, -59.98519422934606382 ) ) ;
#178844 = EDGE_CURVE ( 'NONE', #226785, #68814, #253618, .T. ) ;
#178845 = VERTEX_POINT ( 'NONE', #76273 ) ;
#178846 = CARTESIAN_POINT ( 'NONE',  ( -22.59999999999999787, -2.401771312552908544, -189.4980873520049727 ) ) ;
#178847 = DIRECTION ( 'NONE',  ( 0.000000000000000000, -0.4088369013363283289, 0.9126074666063768159 ) ) ;
#178848 = ORIENTED_EDGE ( 'NONE', *, *, #98856, .T. ) ;
#178849 = CARTESIAN_POINT ( 'NONE',  ( -23.25000000000000000, -1.835859311432481045, -145.6044391687985637 ) ) ;
#178850 = CARTESIAN_POINT ( 'NONE',  ( 18.60000000000000497, 85.52394631232981226, -129.6410794891860974 ) ) ;
#178852 = CARTESIAN_POINT ( 'NONE',  ( -16.87401514999228525, 9.950000000011137047, -121.2800179925321231 ) ) ;
#178851 = CYLINDRICAL_SURFACE ( 'NONE', #44721, 0.1000000000000026007 ) ;
#178853 = DIRECTION ( 'NONE',  ( 0.000000000000000000, 0.2617529984165152257, 0.9651348961777124202 ) ) ;
#178854 = EDGE_CURVE ( 'NONE', #40625, #96347, #134942, .T. ) ;
#178856 = CARTESIAN_POINT ( 'NONE',  ( 18.49999999999999289, 69.55000000001230376, -160.0060803140843859 ) ) ;
#178855 = AXIS2_PLACEMENT_3D ( 'NONE', #30954, #70074, #53044 ) ;
#178859 = EDGE_CURVE ( 'NONE', #110910, #88904, #182182, .T. ) ;
#178858 = DIRECTION ( 'NONE',  ( 0.000000000000000000, 0.8660254037844411501, 0.4999999999999956701 ) ) ;
#178857 = CIRCLE ( 'NONE', #95427, 0.09999999999999939493 ) ;
#178860 = CARTESIAN_POINT ( 'NONE',  ( -22.39999999999999858, 11.65000000001115588, -33.40000000000000568 ) ) ;
#178861 = AXIS2_PLACEMENT_3D ( 'NONE', #183487, #167800, #103914 ) ;
#178862 = CARTESIAN_POINT ( 'NONE',  ( 21.05000000000000426, 75.93429838969011314, -142.7814235418563271 ) ) ;
#178863 = CARTESIAN_POINT ( 'NONE',  ( -20.54999999999999716, 1.115600667400684642E-11, -100.5000000000000284 ) ) ;
#178864 = ORIENTED_EDGE ( 'NONE', *, *, #234766, .F. ) ;
#178865 = AXIS2_PLACEMENT_3D ( 'NONE', #92876, #216686, #53761 ) ;
#178867 = VERTEX_POINT ( 'NONE', #198793 ) ;
#178866 = VERTEX_POINT ( 'NONE', #121846 ) ;
#178868 = VERTEX_POINT ( 'NONE', #78829 ) ;
#178869 = ORIENTED_EDGE ( 'NONE', *, *, #141710, .T. ) ;
#178870 = ADVANCED_FACE ( 'NONE', ( #63125 ), #157131, .F. ) ;
#178871 = CARTESIAN_POINT ( 'NONE',  ( -18.59999999999999787, 9.250000000011157297, -121.6500000000000341 ) ) ;
#178872 =( BOUNDED_SURFACE ( )  B_SPLINE_SURFACE ( 3, 2, ( 
 ( #242081, #24350, #204238 ),
 ( #139100, #218661, #63441 ),
 ( #41353, #2177, #42606 ),
 ( #120893, #201675, #200402 ) ),
 .UNSPECIFIED., .F., .F., .F. ) 
 B_SPLINE_SURFACE_WITH_KNOTS ( ( 4, 4 ),
 ( 3, 3 ),
 ( 0.04058434257139475337, 0.04256401539001599538 ),
 ( 0.000000000000000000, 1.000000000000000000 ),
 .UNSPECIFIED. ) 
 GEOMETRIC_REPRESENTATION_ITEM ( )  RATIONAL_B_SPLINE_SURFACE ( (
 ( 1.000000000000000000, 0.7103081912007809251, 1.000000000000000000),
 ( 1.000000000000000000, 0.7104998333556791223, 1.000000000000000000),
 ( 1.000000000000000000, 0.7107238315754067504, 1.000000000000000000),
 ( 1.000000000000000000, 0.7110073749539717047, 1.000000000000000000) ) ) 
 REPRESENTATION_ITEM ( '' )  SURFACE ( )  );
#178873 = SPHERICAL_SURFACE ( 'NONE', #56958, 0.1000000000000000056 ) ;
#178875 = CARTESIAN_POINT ( 'NONE',  ( -23.15000000000000213, 0.000000000000000000, 0.000000000000000000 ) ) ;
#178874 = DIRECTION ( 'NONE',  ( -1.000000000000000000, 0.000000000000000000, 0.000000000000000000 ) ) ;
#178876 = DIRECTION ( 'NONE',  ( 0.000000000000000000, -0.9654727137038715545, 0.2605042016806676242 ) ) ;
#178877 = EDGE_LOOP ( 'NONE', ( #63019, #11769, #142206, #46878 ) ) ;
#178878 = DIRECTION ( 'NONE',  ( 0.000000000000000000, 0.000000000000000000, 1.000000000000000000 ) ) ;
#178879 =( LENGTH_UNIT ( ) NAMED_UNIT ( * ) SI_UNIT ( .MILLI., .METRE. ) );
#178880 = CARTESIAN_POINT ( 'NONE',  ( 23.04999999999999716, 67.17743825834591576, -160.7731074845244166 ) ) ;
#178881 = DIRECTION ( 'NONE',  ( -0.000000000000000000, -6.982962677686266711E-15, 1.000000000000000000 ) ) ;
#178882 = DIRECTION ( 'NONE',  ( 1.000000000000000000, 0.000000000000000000, 0.000000000000000000 ) ) ;
#178883 = ORIENTED_EDGE ( 'NONE', *, *, #99740, .F. ) ;
#178884 = CIRCLE ( 'NONE', #62316, 7.800000000000001599 ) ;
#178885 = DIRECTION ( 'NONE',  ( 0.000000000000000000, 0.000000000000000000, -1.000000000000000000 ) ) ;
#178886 = CARTESIAN_POINT ( 'NONE',  ( 20.94999999999999929, 69.35000000001231513, -160.0060803140843859 ) ) ;
#178887 = EDGE_LOOP ( 'NONE', ( #110027, #139257, #108534, #55923 ) ) ;
#178888 = EDGE_CURVE ( 'NONE', #136601, #38380, #40786, .T. ) ;
#178889 = LINE ( 'NONE', #62756, #195419 ) ;
#178890 = EDGE_CURVE ( 'NONE', #165926, #223519, #220913, .T. ) ;
#178891 = VECTOR ( 'NONE', #35516, 1000.000000000000000 ) ;
#178892 = CYLINDRICAL_SURFACE ( 'NONE', #98684, 0.9000000000000014655 ) ;
#178893 = DIRECTION ( 'NONE',  ( -1.000000000000000000, 0.000000000000000000, 0.000000000000000000 ) ) ;
#178894 = DIRECTION ( 'NONE',  ( 0.000000000000000000, 1.000000000000000000, 6.982962677686266711E-15 ) ) ;
#178895 = ORIENTED_EDGE ( 'NONE', *, *, #144772, .F. ) ;
#178896 = CARTESIAN_POINT ( 'NONE',  ( 21.05000000000000071, 11.77895973109482952, -206.1023438919106070 ) ) ;
#178897 = CARTESIAN_POINT ( 'NONE',  ( -18.59999999999999787, -1.162701749926853712, -41.60000000000000142 ) ) ;
#178898 = FACE_OUTER_BOUND ( 'NONE', #72650, .T. ) ;
#178900 = LINE ( 'NONE', #121487, #245340 ) ;
#178899 = DIRECTION ( 'NONE',  ( 0.000000000000000000, 0.000000000000000000, -1.000000000000000000 ) ) ;
#178901 = CARTESIAN_POINT ( 'NONE',  ( 23.14999999999999858, 34.77015291263840169, -253.0771437259187167 ) ) ;
#178902 = ADVANCED_FACE ( 'NONE', ( #236631 ), #140701, .F. ) ;
#178903 = CARTESIAN_POINT ( 'NONE',  ( 21.05000000000000071, 76.00000000001126921, -203.5231074845248997 ) ) ;
#178904 = CARTESIAN_POINT ( 'NONE',  ( -23.49999999999994316, 74.16448838626247664, -47.62760213295649692 ) ) ;
#178905 = CYLINDRICAL_SURFACE ( 'NONE', #205906, 0.09999999999999939493 ) ;
#178906 = CIRCLE ( 'NONE', #87259, 0.09999999999998898659 ) ;
#178907 = ORIENTED_EDGE ( 'NONE', *, *, #222749, .F. ) ;
#178908 = CIRCLE ( 'NONE', #95639, 0.09999999999999939493 ) ;
#178909 = VERTEX_POINT ( 'NONE', #180534 ) ;
#178910 = ORIENTED_EDGE ( 'NONE', *, *, #70904, .T. ) ;
#178911 = LINE ( 'NONE', #237571, #147075 ) ;
#178912 = CIRCLE ( 'NONE', #103836, 4.900000000000003020 ) ;
#178913 = EDGE_CURVE ( 'NONE', #233299, #48831, #149095, .T. ) ;
#178914 = LINE ( 'NONE', #111526, #142257 ) ;
#178915 = CYLINDRICAL_SURFACE ( 'NONE', #37959, 0.09999999999999939493 ) ;
#178916 = ORIENTED_EDGE ( 'NONE', *, *, #76235, .F. ) ;
#178917 = AXIS2_PLACEMENT_3D ( 'NONE', #28158, #129787, #11135 ) ;
#178918 = DIRECTION ( 'NONE',  ( 0.000000000000000000, 1.000000000000000000, 0.000000000000000000 ) ) ;
#178919 = VECTOR ( 'NONE', #18914, 1000.000000000000000 ) ;
#178920 = VECTOR ( 'NONE', #218264, 1000.000000000000000 ) ;
#178921 = CARTESIAN_POINT ( 'NONE',  ( 18.59999999999999076, 7.128833340094563376, -233.7327013124401276 ) ) ;
#178922 = CARTESIAN_POINT ( 'NONE',  ( -18.53317502108577131, 65.67736539654943329, -97.46251168765716955 ) ) ;
#178923 = ADVANCED_FACE ( 'NONE', ( #119279 ), #123965, .T. ) ;
#178924 = ADVANCED_FACE ( 'NONE', ( #98366, #59240, #39759 ), #20176, .T. ) ;
#178925 = CARTESIAN_POINT ( 'NONE',  ( -0.8999999999999437339, 64.25000000001119815, -7.323107484524790323 ) ) ;
#178927 = ORIENTED_EDGE ( 'NONE', *, *, #256871, .T. ) ;
#178926 = CARTESIAN_POINT ( 'NONE',  ( -16.84981964351507600, 9.917318234109812281, -188.1303983859795892 ) ) ;
#178929 = DIRECTION ( 'NONE',  ( 1.000000000000000000, 0.000000000000000000, 0.000000000000000000 ) ) ;
#178928 = CARTESIAN_POINT ( 'NONE',  ( -18.59999999999999787, 1.866714910057309273, -11.75267524628200633 ) ) ;
#178930 = AXIS2_PLACEMENT_3D ( 'NONE', #43811, #123350, #142877 ) ;
#178931 = CARTESIAN_POINT ( 'NONE',  ( -18.50000000000000000, -26.43935341558978891, -118.6415086075074896 ) ) ;
#178932 = CARTESIAN_POINT ( 'NONE',  ( -20.00857864376270001, 9.250000000011157297, -121.7500000000000426 ) ) ;
#178933 = EDGE_CURVE ( 'NONE', #140838, #257284, #190609, .T. ) ;
#178934 = EDGE_CURVE ( 'NONE', #170816, #70703, #21471, .T. ) ;
#178935 = ORIENTED_EDGE ( 'NONE', *, *, #153507, .T. ) ;
#178936 = DIRECTION ( 'NONE',  ( 0.000000000000000000, 0.000000000000000000, 1.000000000000000000 ) ) ;
#178937 = CARTESIAN_POINT ( 'NONE',  ( 22.47071067811865319, 0.09909245471376171288, -92.77992525550199332 ) ) ;
#178938 = ORIENTED_EDGE ( 'NONE', *, *, #103283, .T. ) ;
#178939 = DIRECTION ( 'NONE',  ( 0.000000000000000000, -1.000000000000000000, 2.771150684185008344E-14 ) ) ;
#178940 = CARTESIAN_POINT ( 'NONE',  ( 21.05000000000000071, 76.00000000001213607, -136.5231074845243313 ) ) ;
#178942 = ORIENTED_EDGE ( 'NONE', *, *, #2091, .T. ) ;
#178941 = STYLED_ITEM ( 'NONE', ( #123143 ), #110572 ) ;
#178943 = EDGE_CURVE ( 'NONE', #170466, #39339, #111475, .T. ) ;
#178944 = CARTESIAN_POINT ( 'NONE',  ( 23.15000000000000213, 61.88149656937974896, -248.1136133839584090 ) ) ;
#178945 = EDGE_CURVE ( 'NONE', #76954, #43436, #3148, .T. ) ;
#178946 = DIRECTION ( 'NONE',  ( 1.000000000000000000, 0.000000000000000000, 0.000000000000000000 ) ) ;
#178947 = DIRECTION ( 'NONE',  ( 1.000000000000000000, -0.000000000000000000, -0.000000000000000000 ) ) ;
#178948 = ORIENTED_EDGE ( 'NONE', *, *, #56616, .T. ) ;
#178949 = ADVANCED_FACE ( 'NONE', ( #89127 ), #203937, .T. ) ;
#178950 = ORIENTED_EDGE ( 'NONE', *, *, #207793, .F. ) ;
#178951 = AXIS2_PLACEMENT_3D ( 'NONE', #255951, #148230, #194771 ) ;
#178952 = CARTESIAN_POINT ( 'NONE',  ( 20.95512820512820795, 8.876151316299273120, -112.7001728591287844 ) ) ;
#178953 = CARTESIAN_POINT ( 'NONE',  ( -20.85000000000000142, 71.99422445362657186, -246.4870034924427671 ) ) ;
#178954 = ADVANCED_FACE ( 'NONE', ( #29207 ), #8327, .T. ) ;
#178955 = CARTESIAN_POINT ( 'NONE',  ( -16.87683809663752399, 63.00529667655239763, -213.7455378284023482 ) ) ;
#178956 = CARTESIAN_POINT ( 'NONE',  ( -22.94999999999999929, -1.885425182446134107, -11.49641995933507843 ) ) ;
#178957 = AXIS2_PLACEMENT_3D ( 'NONE', #99414, #21215, #324 ) ;
#178959 = LINE ( 'NONE', #197189, #145179 ) ;
#178958 = LINE ( 'NONE', #268, #82596 ) ;
#178960 = DIRECTION ( 'NONE',  ( -1.000000000000000000, 0.000000000000000000, 0.000000000000000000 ) ) ;
#178962 = ADVANCED_FACE ( 'NONE', ( #48706 ), #25326, .T. ) ;
#178961 = LINE ( 'NONE', #62823, #118570 ) ;
#178964 = EDGE_CURVE ( 'NONE', #73870, #695, #257174, .T. ) ;
#178963 = FACE_OUTER_BOUND ( 'NONE', #108020, .T. ) ;
#178965 = VERTEX_POINT ( 'NONE', #207825 ) ;
#178966 = CARTESIAN_POINT ( 'NONE',  ( 20.94999999999999929, 14.80545736607782814, -235.9842437978701639 ) ) ;
#178968 = ORIENTED_EDGE ( 'NONE', *, *, #69926, .T. ) ;
#178967 = FACE_OUTER_BOUND ( 'NONE', #251215, .T. ) ;
#178969 = CARTESIAN_POINT ( 'NONE',  ( 20.95035502843362707, 65.52236167323616201, -195.9468077757880451 ) ) ;
#178970 = DIRECTION ( 'NONE',  ( 1.000000000000000000, 0.000000000000000000, 0.000000000000000000 ) ) ;
#178972 = PLANE ( 'NONE',  #132453 ) ;
#178971 = DIRECTION ( 'NONE',  ( 0.000000000000000000, -1.000000000000000000, 0.000000000000000000 ) ) ;
#178973 =( BOUNDED_CURVE ( )  B_SPLINE_CURVE ( 3, ( #223162, #25003, #104482, #198473 ),
 .UNSPECIFIED., .F., .F. ) 
 B_SPLINE_CURVE_WITH_KNOTS ( ( 4, 4 ),
 ( 1.570796326794885012, 3.141592653589794448 ),
 .UNSPECIFIED. ) 
 CURVE ( )  GEOMETRIC_REPRESENTATION_ITEM ( )  RATIONAL_B_SPLINE_CURVE ( ( 1.000000000000000000, 0.8047378541243619399, 0.8047378541243619399, 1.000000000000000000 ) ) 
 REPRESENTATION_ITEM ( '' )  );
#178974 = ADVANCED_FACE ( 'NONE', ( #47416 ), #68291, .F. ) ;
#178975 = ORIENTED_EDGE ( 'NONE', *, *, #123934, .F. ) ;
#178977 = CARTESIAN_POINT ( 'NONE',  ( -23.25000000000000000, -3.770473190032741062, -225.9805569534692324 ) ) ;
#178976 = CARTESIAN_POINT ( 'NONE',  ( 19.99999999999998934, 16.02417409648692725, -219.3605785455116006 ) ) ;
#178978 = LINE ( 'NONE', #81100, #158071 ) ;
#178979 = LINE ( 'NONE', #82369, #134516 ) ;
#178980 = CARTESIAN_POINT ( 'NONE',  ( -20.54999999999999716, 76.00000000001190870, -103.0231074845243029 ) ) ;
#178981 = DIRECTION ( 'NONE',  ( 0.000000000000000000, 0.9421926911474418631, -0.3350715337779995862 ) ) ;
#178982 = ORIENTED_EDGE ( 'NONE', *, *, #211314, .F. ) ;
#178983 = CARTESIAN_POINT ( 'NONE',  ( -22.48660254037843487, 31.85034414784621148, -238.9397275603479898 ) ) ;
#178984 = EDGE_CURVE ( 'NONE', #75869, #15594, #46144, .T. ) ;
#178986 = ORIENTED_EDGE ( 'NONE', *, *, #133462, .T. ) ;
#178985 = VECTOR ( 'NONE', #220930, 1000.000000000000000 ) ;
#178987 = EDGE_CURVE ( 'NONE', #172986, #14889, #85238, .T. ) ;
#178988 = AXIS2_PLACEMENT_3D ( 'NONE', #97601, #181042, #216287 ) ;
#178989 = ADVANCED_FACE ( 'NONE', ( #205205 ), #26609, .F. ) ;
#178990 = CARTESIAN_POINT ( 'NONE',  ( 20.05000000000002913, 7.250000000000015099, -20.85000000000000142 ) ) ;
#178991 = ORIENTED_EDGE ( 'NONE', *, *, #18236, .T. ) ;
#178992 = CARTESIAN_POINT ( 'NONE',  ( 23.25000000000000000, 79.08634564045904369, -228.8189404293001132 ) ) ;
#178993 = AXIS2_PLACEMENT_3D ( 'NONE', #68488, #171472, #172763 ) ;
#178994 = EDGE_LOOP ( 'NONE', ( #132822, #118524, #254793, #99530 ) ) ;
#178995 = LINE ( 'NONE', #255869, #97648 ) ;
#178996 = DIRECTION ( 'NONE',  ( 0.000000000000000000, -6.982962677686266711E-15, 1.000000000000000000 ) ) ;
#178997 = ORIENTED_EDGE ( 'NONE', *, *, #243975, .T. ) ;
#178998 = EDGE_CURVE ( 'NONE', #2004, #13565, #182418, .T. ) ;
#178999 = CARTESIAN_POINT ( 'NONE',  ( -18.49513951962167368, -9.437725026666546668, -174.2780725750291424 ) ) ;
#179000 = CARTESIAN_POINT ( 'NONE',  ( 21.07928932188134397, 76.00000000001237765, -170.0231074845243597 ) ) ;
#179001 = DIRECTION ( 'NONE',  ( 0.000000000000000000, 0.000000000000000000, -1.000000000000000000 ) ) ;
#179002 = CARTESIAN_POINT ( 'NONE',  ( 18.49999999999999289, 65.79142135624880439, -48.17310748452439384 ) ) ;
#179004 = CIRCLE ( 'NONE', #141528, 0.1000000000000028644 ) ;
#179003 = CARTESIAN_POINT ( 'NONE',  ( 21.00000000000000000, 51.97441255244040548, -232.0063394385699667 ) ) ;
#179005 = CARTESIAN_POINT ( 'NONE',  ( 19.99999999738033551, 62.35288080320960802, -208.9530776385553850 ) ) ;
#179006 = ORIENTED_EDGE ( 'NONE', *, *, #64611, .F. ) ;
#179007 = CARTESIAN_POINT ( 'NONE',  ( 20.04999999999999716, 67.25000000001205080, -123.8731074845243683 ) ) ;
#179008 = EDGE_LOOP ( 'NONE', ( #124159, #188566, #228180, #191620 ) ) ;
#179010 = VERTEX_POINT ( 'NONE', #107400 ) ;
#179009 = LINE ( 'NONE', #79839, #2435 ) ;
#179011 = EDGE_LOOP ( 'NONE', ( #220489, #194144, #63246 ) ) ;
#179012 = CARTESIAN_POINT ( 'NONE',  ( 18.43565242384934422, -9.519327731092435130, -6.972976376559337552 ) ) ;
#179013 = CARTESIAN_POINT ( 'NONE',  ( 23.14999999999998437, 1.115600667400684642E-11, -67.00000000000004263 ) ) ;
#179014 = DIRECTION ( 'NONE',  ( -1.000000000000000000, -0.000000000000000000, -0.000000000000000000 ) ) ;
#179015 = CARTESIAN_POINT ( 'NONE',  ( -20.64999999999999858, 73.60000000001259934, -190.2984855617622770 ) ) ;
#179016 = LINE ( 'NONE', #57727, #100014 ) ;
#179017 = ORIENTED_EDGE ( 'NONE', *, *, #142822, .F. ) ;
#179018 = DIRECTION ( 'NONE',  ( -2.952720810173289112E-16, 0.9770955615653316162, 0.2128009952263604232 ) ) ;
#179019 = CARTESIAN_POINT ( 'NONE',  ( -21.05000000000000071, -11.48912529307605901, -3.100000000000000533 ) ) ;
#179021 = ORIENTED_EDGE ( 'NONE', *, *, #14881, .T. ) ;
#179020 = FACE_OUTER_BOUND ( 'NONE', #125783, .T. ) ;
#179022 = DIRECTION ( 'NONE',  ( 1.000000000000000000, 0.000000000000000000, 0.000000000000000000 ) ) ;
#179023 = AXIS2_PLACEMENT_3D ( 'NONE', #142700, #24081, #222226 ) ;
#179024 = EDGE_CURVE ( 'NONE', #110447, #19933, #86498, .T. ) ;
#179025 = VECTOR ( 'NONE', #23954, 1000.000000000000000 ) ;
#179026 = VECTOR ( 'NONE', #147855, 1000.000000000000000 ) ;
#179028 = AXIS2_PLACEMENT_3D ( 'NONE', #20760, #179832, #35209 ) ;
#179027 = LINE ( 'NONE', #337, #242969 ) ;
#179029 = EDGE_LOOP ( 'NONE', ( #242881, #26485, #2755, #169737, #54858 ) ) ;
#179030 = EDGE_CURVE ( 'NONE', #8351, #180099, #165668, .T. ) ;
#179031 = AXIS2_PLACEMENT_3D ( 'NONE', #187890, #92608, #47059 ) ;
#179032 = CARTESIAN_POINT ( 'NONE',  ( -20.94999999999999929, 74.83729825007388570, -94.92310748452432279 ) ) ;
#179033 = VERTEX_POINT ( 'NONE', #27905 ) ;
#179034 = LINE ( 'NONE', #138551, #141992 ) ;
#179035 = ADVANCED_FACE ( 'NONE', ( #104800 ), #124414, .F. ) ;
#179036 = EDGE_CURVE ( 'NONE', #219596, #19771, #86528, .T. ) ;
#179037 = CARTESIAN_POINT ( 'NONE',  ( -21.05000000000000071, 0.09779029130879170195, 6.257814610476114758 ) ) ;
#179038 = CARTESIAN_POINT ( 'NONE',  ( 21.04386569057619027, 64.25000000001250555, -176.8802701327446698 ) ) ;
#179039 = DIRECTION ( 'NONE',  ( -0.000000000000000000, -0.000000000000000000, 1.000000000000000000 ) ) ;
#179040 = AXIS2_PLACEMENT_3D ( 'NONE', #168027, #6326, #165424 ) ;
#179041 = AXIS2_PLACEMENT_3D ( 'NONE', #105540, #9046, #5161 ) ;
#179042 = AXIS2_PLACEMENT_3D ( 'NONE', #129154, #229543, #50864 ) ;
#179043 = VERTEX_POINT ( 'NONE', #164820 ) ;
#179044 = LINE ( 'NONE', #162034, #127910 ) ;
#179045 = ADVANCED_BREP_SHAPE_REPRESENTATION ( '', ( #26097, #2425 ), #164577 ) ;
#179046 = ORIENTED_EDGE ( 'NONE', *, *, #87635, .T. ) ;
#179047 = DIRECTION ( 'NONE',  ( 0.000000000000000000, -8.905812670947865054E-15, 1.000000000000000000 ) ) ;
#179048 = DIRECTION ( 'NONE',  ( 1.000000000000000000, 0.000000000000000000, 0.000000000000000000 ) ) ;
#179050 = EDGE_LOOP ( 'NONE', ( #217379, #106931, #9517 ) ) ;
#179049 = CARTESIAN_POINT ( 'NONE',  ( -18.59999999999999787, 76.00000000001170974, -69.52310748452431710 ) ) ;
#179051 = DIRECTION ( 'NONE',  ( -1.000000000000000000, 0.000000000000000000, -0.000000000000000000 ) ) ;
#179052 = DIRECTION ( 'NONE',  ( 0.000000000000000000, 1.000000000000000000, 0.000000000000000000 ) ) ;
#179053 = CARTESIAN_POINT ( 'NONE',  ( -22.50000000000000000, 64.35000000001214460, -136.5231074845243597 ) ) ;
#179054 = CARTESIAN_POINT ( 'NONE',  ( -16.77683809663752257, 9.945835743215301505, -79.66394901910425119 ) ) ;
#179055 = LINE ( 'NONE', #141182, #134885 ) ;
#179056 = DIRECTION ( 'NONE',  ( 1.000000000000000000, -0.000000000000000000, -0.000000000000000000 ) ) ;
#179058 = ORIENTED_EDGE ( 'NONE', *, *, #226798, .F. ) ;
#179057 = CARTESIAN_POINT ( 'NONE',  ( 23.50000000000005684, 74.94272479589878344, -8.023107484524793165 ) ) ;
#179059 = CIRCLE ( 'NONE', #162461, 0.09999999999999939493 ) ;
#179060 = EDGE_CURVE ( 'NONE', #21468, #224619, #66995, .T. ) ;
#179061 = FACE_OUTER_BOUND ( 'NONE', #238029, .T. ) ;
#179062 = ORIENTED_EDGE ( 'NONE', *, *, #127898, .F. ) ;
#179063 = ORIENTED_EDGE ( 'NONE', *, *, #29158, .T. ) ;
#179064 = AXIS2_PLACEMENT_3D ( 'NONE', #162850, #61158, #140690 ) ;
#179065 = LINE ( 'NONE', #120379, #174253 ) ;
#179066 = DIRECTION ( 'NONE',  ( 1.000000000000000000, 0.000000000000000000, 0.000000000000000000 ) ) ;
#179067 = ORIENTED_EDGE ( 'NONE', *, *, #148283, .T. ) ;
#179068 = EDGE_CURVE ( 'NONE', #240580, #75284, #207355, .T. ) ;
#179069 = CARTESIAN_POINT ( 'NONE',  ( 21.14999999999999858, 1.115600667400684642E-11, -33.60000000000000142 ) ) ;
#179070 = EDGE_CURVE ( 'NONE', #91550, #239682, #128238, .T. ) ;
#179071 = PRESENTATION_STYLE_ASSIGNMENT (( #180325 ) ) ;
#179072 = ORIENTED_EDGE ( 'NONE', *, *, #86583, .T. ) ;
#179073 = AXIS2_PLACEMENT_3D ( 'NONE', #49392, #131486, #228027 ) ;
#179074 = CARTESIAN_POINT ( 'NONE',  ( 23.24999999999999289, 6.450000000011156587, -54.65000000000000568 ) ) ;
#179075 = VECTOR ( 'NONE', #226757, 1000.000000000000000 ) ;
#179076 = LINE ( 'NONE', #79903, #51458 ) ;
#179077 = EDGE_CURVE ( 'NONE', #175552, #24921, #49106, .T. ) ;
#179078 = VERTEX_POINT ( 'NONE', #209079 ) ;
#179079 = CARTESIAN_POINT ( 'NONE',  ( 21.15000000000003055, 84.00000000001119815, -37.18565239344504647 ) ) ;
#179080 = TOROIDAL_SURFACE ( 'NONE', #170918, 0.2000000000000000111, 0.1000000000000000056 ) ;
#179081 = VERTEX_POINT ( 'NONE', #35612 ) ;
#179082 = DIRECTION ( 'NONE',  ( 1.000000000000000000, -1.207181226542539700E-16, 2.694675058168174199E-16 ) ) ;
#179084 = ORIENTED_EDGE ( 'NONE', *, *, #241675, .T. ) ;
#179083 = FACE_OUTER_BOUND ( 'NONE', #225563, .T. ) ;
#179085 = ADVANCED_FACE ( 'NONE', ( #194686 ), #82413, .T. ) ;
#179086 = VECTOR ( 'NONE', #6322, 1000.000000000000000 ) ;
#179087 = EDGE_CURVE ( 'NONE', #168244, #169705, #153397, .T. ) ;
#179088 = CIRCLE ( 'NONE', #137336, 0.09999999999998898659 ) ;
#179089 = DIRECTION ( 'NONE',  ( 7.304098846218134667E-16, -1.000000000000000000, 0.000000000000000000 ) ) ;
#179090 = VERTEX_POINT ( 'NONE', #189528 ) ;
#179091 = CARTESIAN_POINT ( 'NONE',  ( 23.15000000000000213, 87.75000000001259082, -191.2731074845242745 ) ) ;
#179092 = EDGE_LOOP ( 'NONE', ( #250817, #102093, #31033 ) ) ;
#179094 = ORIENTED_EDGE ( 'NONE', *, *, #29765, .F. ) ;
#179093 = ORIENTED_EDGE ( 'NONE', *, *, #125702, .T. ) ;
#179095 = FACE_OUTER_BOUND ( 'NONE', #249273, .T. ) ;
#179096 = ADVANCED_FACE ( 'NONE', ( #16042 ), #10888, .T. ) ;
#179097 = EDGE_LOOP ( 'NONE', ( #181315, #52020, #125246, #232551, #179402 ) ) ;
#179098 = CARTESIAN_POINT ( 'NONE',  ( 23.14999999999999858, 54.36558989155976462, -236.3448031251562327 ) ) ;
#179099 = ORIENTED_EDGE ( 'NONE', *, *, #228398, .F. ) ;
#179100 = AXIS2_PLACEMENT_3D ( 'NONE', #27856, #248151, #69534 ) ;
#179101 = AXIS2_PLACEMENT_3D ( 'NONE', #236670, #73790, #58022 ) ;
#179102 = TOROIDAL_SURFACE ( 'NONE', #224839, 0.2000000000000000111, 0.1000000000000000056 ) ;
#179103 = CIRCLE ( 'NONE', #41538, 0.09999999999999600875 ) ;
#179104 = CIRCLE ( 'NONE', #174845, 0.5000000000000013323 ) ;
#179105 = ORIENTED_EDGE ( 'NONE', *, *, #26071, .F. ) ;
#179106 = DIRECTION ( 'NONE',  ( 1.186688945009010077E-16, -1.000000000000000000, -0.000000000000000000 ) ) ;
#179107 = EDGE_CURVE ( 'NONE', #50215, #159227, #195072, .T. ) ;
#179108 = CARTESIAN_POINT ( 'NONE',  ( 20.94999999999999574, 1.162701749949165642, -41.50000000000000000 ) ) ;
#179110 = VERTEX_POINT ( 'NONE', #254595 ) ;
#179109 = DIRECTION ( 'NONE',  ( 1.000000000000000000, 0.000000000000000000, 0.000000000000000000 ) ) ;
#179111 = CARTESIAN_POINT ( 'NONE',  ( -21.05000000000000071, 1.250000000011155299, -142.0000000000000284 ) ) ;
#179112 = ORIENTED_EDGE ( 'NONE', *, *, #55966, .F. ) ;
#179113 = CARTESIAN_POINT ( 'NONE',  ( -18.50000000000000000, 65.70729864261028297, -131.0657455973724836 ) ) ;
#179114 = CARTESIAN_POINT ( 'NONE',  ( 21.05000000000000071, 76.00000000001189449, -101.0231074845243029 ) ) ;
#179115 = ORIENTED_EDGE ( 'NONE', *, *, #207845, .F. ) ;
#179116 = DIRECTION ( 'NONE',  ( 0.000000000000000000, 7.056502275159890832E-15, -1.000000000000000000 ) ) ;
#179117 = DIRECTION ( 'NONE',  ( -1.000000000000000000, -0.000000000000000000, 0.000000000000000000 ) ) ;
#179118 = CARTESIAN_POINT ( 'NONE',  ( -23.25000000000000000, 76.00000000001267608, -203.5231074845243597 ) ) ;
#179119 = ORIENTED_EDGE ( 'NONE', *, *, #147731, .T. ) ;
#179120 = CARTESIAN_POINT ( 'NONE',  ( -16.94333152886235894, 66.00965798856138633, -90.41513901557878796 ) ) ;
#179121 = ORIENTED_EDGE ( 'NONE', *, *, #139144, .T. ) ;
#179122 = ORIENTED_EDGE ( 'NONE', *, *, #186067, .T. ) ;
#179123 = DIRECTION ( 'NONE',  ( 0.000000000000000000, 0.000000000000000000, 1.000000000000000000 ) ) ;
#179124 = ORIENTED_EDGE ( 'NONE', *, *, #236877, .F. ) ;
#179125 = ORIENTED_EDGE ( 'NONE', *, *, #183711, .T. ) ;
#179126 = CARTESIAN_POINT ( 'NONE',  ( -21.05000000000000071, 5.900000000011162093, -190.7809002353436085 ) ) ;
#179127 = DIRECTION ( 'NONE',  ( 1.000000000000000000, -0.000000000000000000, -0.000000000000000000 ) ) ;
#179128 = ORIENTED_EDGE ( 'NONE', *, *, #141580, .F. ) ;
#179129 = VERTEX_POINT ( 'NONE', #231232 ) ;
#179130 = DIRECTION ( 'NONE',  ( -0.7070776581708964059, -0.6909393522475117955, -0.1504792239192832004 ) ) ;
#179131 = DIRECTION ( 'NONE',  ( 1.000000000000000000, 7.304098846218134667E-16, -4.607487905232622991E-31 ) ) ;
#179132 = VERTEX_POINT ( 'NONE', #115115 ) ;
#179133 = AXIS2_PLACEMENT_3D ( 'NONE', #99181, #20987, #63935 ) ;
#179134 = ORIENTED_EDGE ( 'NONE', *, *, #222171, .T. ) ;
#179135 = ORIENTED_EDGE ( 'NONE', *, *, #25504, .F. ) ;
#179136 = AXIS2_PLACEMENT_3D ( 'NONE', #113447, #251671, #109582 ) ;
#179137 = ADVANCED_FACE ( 'NONE', ( #111268 ), #178324, .T. ) ;
#179138 = DIRECTION ( 'NONE',  ( 0.000000000000000000, 0.000000000000000000, 1.000000000000000000 ) ) ;
#179139 = DIRECTION ( 'NONE',  ( 0.000000000000000000, 0.4088369013363280513, -0.9126074666063769270 ) ) ;
#179140 = EDGE_CURVE ( 'NONE', #15539, #199092, #112559, .T. ) ;
#179141 = DIRECTION ( 'NONE',  ( 1.000000000000000000, -0.000000000000000000, 0.000000000000000000 ) ) ;
#179142 = CARTESIAN_POINT ( 'NONE',  ( -37.88850191057539973, -10.80884033489985363, 6.000000000000001776 ) ) ;
#179143 = DIRECTION ( 'NONE',  ( 1.000000000000000000, 0.000000000000000000, -0.000000000000000000 ) ) ;
#179144 = AXIS2_PLACEMENT_3D ( 'NONE', #167422, #170015, #46159 ) ;
#179145 = CARTESIAN_POINT ( 'NONE',  ( -22.49436431346200038, 11.64995094766461392, -66.93309647027778908 ) ) ;
#179146 = CARTESIAN_POINT ( 'NONE',  ( 20.95512820512820440, 8.876151316288115822, -8.558628995140949769 ) ) ;
#179147 = VECTOR ( 'NONE', #154757, 1000.000000000000114 ) ;
#179148 = EDGE_CURVE ( 'NONE', #8640, #199333, #249053, .T. ) ;
#179150 = CARTESIAN_POINT ( 'NONE',  ( 21.05000000000000071, -11.39257802169451139, -63.92605042016806749 ) ) ;
#179149 = CARTESIAN_POINT ( 'NONE',  ( -16.78805706634180694, 66.05174750694105512, -149.1789542764925898 ) ) ;
#179152 = EDGE_CURVE ( 'NONE', #109264, #71691, #65865, .T. ) ;
#179151 = LINE ( 'NONE', #257311, #198846 ) ;
#179153 = CARTESIAN_POINT ( 'NONE',  ( -16.82055514392384765, 23.00168983512579146, -230.9477172710467414 ) ) ;
#179154 = CARTESIAN_POINT ( 'NONE',  ( -21.64999999999999858, 29.19585636832770348, -237.3287400596392445 ) ) ;
#179155 = CARTESIAN_POINT ( 'NONE',  ( -18.59999999999999787, 66.65000000001180069, -81.87310748452438247 ) ) ;
#179156 = CIRCLE ( 'NONE', #54209, 4.049999999999998046 ) ;
#179157 = ORIENTED_EDGE ( 'NONE', *, *, #209584, .T. ) ;
#179158 = MECHANICAL_DESIGN_GEOMETRIC_PRESENTATION_REPRESENTATION (  '', ( #145793 ), #212646 ) ;
#179160 = ORIENTED_EDGE ( 'NONE', *, *, #56156, .T. ) ;
#179159 = CARTESIAN_POINT ( 'NONE',  ( 21.30000000000002558, 66.17117490947157421, -239.7639228359981303 ) ) ;
#179161 = EDGE_CURVE ( 'NONE', #148418, #226515, #203244, .T. ) ;
#179162 = DIRECTION ( 'NONE',  ( 0.000000000000000000, 0.000000000000000000, -1.000000000000000000 ) ) ;
#179163 = EDGE_CURVE ( 'NONE', #161742, #9710, #211629, .T. ) ;
#179164 = FACE_OUTER_BOUND ( 'NONE', #120071, .T. ) ;
#179165 = VERTEX_POINT ( 'NONE', #51255 ) ;
#179166 = PRODUCT_DEFINITION ( 'UNKNOWN', '', #119697, #238298 ) ;
#179168 = AXIS2_PLACEMENT_3D ( 'NONE', #63334, #137735, #180741 ) ;
#179167 = CARTESIAN_POINT ( 'NONE',  ( 20.95512820512820440, 10.62384868372303615, -141.6649135690876165 ) ) ;
#179169 = AXIS2_PLACEMENT_3D ( 'NONE', #251508, #149876, #169459 ) ;
#179170 = CARTESIAN_POINT ( 'NONE',  ( -16.86445178670581058, 66.03778837089642195, -157.4138849226412731 ) ) ;
#179171 = ORIENTED_EDGE ( 'NONE', *, *, #23764, .F. ) ;
#179172 = CARTESIAN_POINT ( 'NONE',  ( -21.04999999999999361, 11.75000000001115374, -140.7838656629781724 ) ) ;
#179173 = DIRECTION ( 'NONE',  ( 0.000000000000000000, -0.9908441862701596881, 0.1350103645451904977 ) ) ;
#179174 = CARTESIAN_POINT ( 'NONE',  ( -18.50000000000000000, 11.65000000001115232, -79.25000000000004263 ) ) ;
#179175 = EDGE_CURVE ( 'NONE', #51105, #19454, #90794, .T. ) ;
#179176 = EDGE_CURVE ( 'NONE', #231943, #76888, #40954, .T. ) ;
#179177 = DIRECTION ( 'NONE',  ( -1.000000000000000000, -0.000000000000000000, 0.000000000000000000 ) ) ;
#179179 = ORIENTED_EDGE ( 'NONE', *, *, #233784, .F. ) ;
#179178 = CARTESIAN_POINT ( 'NONE',  ( -20.94999999999999929, 67.49463558145296815, -195.5618716440587548 ) ) ;
#179180 = ADVANCED_FACE ( 'NONE', ( #13455 ), #57478, .F. ) ;
#179182 = ORIENTED_EDGE ( 'NONE', *, *, #5388, .T. ) ;
#179181 = DIRECTION ( 'NONE',  ( 0.000000000000000000, -0.2617529984165030132, -0.9651348961777157509 ) ) ;
#179183 = CARTESIAN_POINT ( 'NONE',  ( 20.85000000000000142, -1.149570369564537842, -74.81591248450196474 ) ) ;
#179184 = CARTESIAN_POINT ( 'NONE',  ( -20.64999999999999858, 7.249999999999999112, -21.15000000000000213 ) ) ;
#179185 = CARTESIAN_POINT ( 'NONE',  ( -23.25000000000000000, 64.35000000001198828, -115.1731074845243938 ) ) ;
#179186 = CARTESIAN_POINT ( 'NONE',  ( -21.65000000000000213, 10.05000000001113847, -87.85000000000003695 ) ) ;
#179187 = AXIS2_PLACEMENT_3D ( 'NONE', #207859, #12222, #248242 ) ;
#179190 = FACE_OUTER_BOUND ( 'NONE', #136075, .T. ) ;
#179189 = AXIS2_PLACEMENT_3D ( 'NONE', #58876, #81014, #139707 ) ;
#179188 = CARTESIAN_POINT ( 'NONE',  ( -16.93589915522258948, 63.05285544833442657, -213.0248735350789389 ) ) ;
#179191 = CARTESIAN_POINT ( 'NONE',  ( -18.40000000000000213, 67.17743825834611471, -179.2731074845244166 ) ) ;
#179192 = CARTESIAN_POINT ( 'NONE',  ( 20.04142135623730070, 64.35000000001180354, -81.67310748452439384 ) ) ;
#179193 = AXIS2_PLACEMENT_3D ( 'NONE', #115139, #176415, #195974 ) ;
#179194 = VECTOR ( 'NONE', #202915, 1000.000000000000000 ) ;
#179195 = CARTESIAN_POINT ( 'NONE',  ( 20.90000000000000213, 1.885425182446133885, -11.49641995933507843 ) ) ;
#179196 = CYLINDRICAL_SURFACE ( 'NONE', #93554, 0.09999999999999939493 ) ;
#179197 = DIRECTION ( 'NONE',  ( 1.000000000000000000, 0.000000000000000000, 1.073024830501117725E-15 ) ) ;
#179198 = ORIENTED_EDGE ( 'NONE', *, *, #39746, .F. ) ;
#179199 = DIRECTION ( 'NONE',  ( 1.000000000000000000, -3.265361837132813093E-16, -2.280189983783949500E-30 ) ) ;
#179200 = CIRCLE ( 'NONE', #229063, 14.30833333333333890 ) ;
#179201 = ORIENTED_EDGE ( 'NONE', *, *, #91621, .F. ) ;
#179202 = VERTEX_POINT ( 'NONE', #212933 ) ;
#179203 = CYLINDRICAL_SURFACE ( 'NONE', #73674, 0.09999999999999939493 ) ;
#179204 = DIRECTION ( 'NONE',  ( 0.000000000000000000, 1.000000000000000000, 0.000000000000000000 ) ) ;
#179205 = ORIENTED_EDGE ( 'NONE', *, *, #116270, .T. ) ;
#179206 = APPLICATION_CONTEXT ( 'automotive_design' ) ;
#179207 = AXIS2_PLACEMENT_3D ( 'NONE', #149411, #132392, #12462 ) ;
#179209 = ADVANCED_FACE ( 'NONE', ( #170000 ), #154292, .F. ) ;
#179208 = VERTEX_POINT ( 'NONE', #34321 ) ;
#179210 = VECTOR ( 'NONE', #233038, 1000.000000000000114 ) ;
#179211 = ORIENTED_EDGE ( 'NONE', *, *, #203750, .T. ) ;
#179212 = ORIENTED_EDGE ( 'NONE', *, *, #92427, .T. ) ;
#179213 = CARTESIAN_POINT ( 'NONE',  ( 18.60000000000000497, 76.00000000001165290, -69.52310748452431710 ) ) ;
#179214 = DIRECTION ( 'NONE',  ( -1.000000000000000000, 0.000000000000000000, 0.000000000000000000 ) ) ;
#179215 = DIRECTION ( 'NONE',  ( 0.000000000000000000, 0.000000000000000000, -1.000000000000000000 ) ) ;
#179216 = LINE ( 'NONE', #535, #65085 ) ;
#179217 = EDGE_CURVE ( 'NONE', #88284, #51883, #99374, .T. ) ;
#179218 = LINE ( 'NONE', #155804, #187277 ) ;
#179219 = DIRECTION ( 'NONE',  ( 0.000000000000000000, -6.454785026890406770E-15, 1.000000000000000000 ) ) ;
#179221 = ORIENTED_EDGE ( 'NONE', *, *, #166321, .T. ) ;
#179220 = DIRECTION ( 'NONE',  ( 0.000000000000000000, 1.000000000000000000, -1.224646799147353207E-16 ) ) ;
#179223 = CARTESIAN_POINT ( 'NONE',  ( -20.64999999999999858, 68.85000000001151932, -48.37310748452436826 ) ) ;
#179222 = FACE_OUTER_BOUND ( 'NONE', #70385, .T. ) ;
#179224 = DIRECTION ( 'NONE',  ( -0.000000000000000000, -0.9770955615653316162, -0.2128009952263604232 ) ) ;
#179225 = EDGE_LOOP ( 'NONE', ( #86156, #71697, #187085, #122725 ) ) ;
#179227 = EDGE_CURVE ( 'NONE', #201062, #41849, #176394, .T. ) ;
#179226 = DIRECTION ( 'NONE',  ( 0.7071067811865474617, -0.7071067811865474617, -5.142139384388980375E-15 ) ) ;
#179228 = ORIENTED_EDGE ( 'NONE', *, *, #56498, .T. ) ;
#179230 = CARTESIAN_POINT ( 'NONE',  ( 20.73486653747088937, 7.750000000011182166, -180.1499999999999773 ) ) ;
#179229 = CARTESIAN_POINT ( 'NONE',  ( 20.85000000000000142, 76.00000000001170974, -69.52310748452431710 ) ) ;
#179231 = AXIS2_PLACEMENT_3D ( 'NONE', #78612, #193456, #53928 ) ;
#179232 = CARTESIAN_POINT ( 'NONE',  ( 21.07928932188134397, 75.90110485435778287, -142.8516241409176075 ) ) ;
#179233 = DIRECTION ( 'NONE',  ( -1.000000000000000000, -0.000000000000000000, -0.000000000000000000 ) ) ;
#179234 = EDGE_LOOP ( 'NONE', ( #68706, #180570, #156018, #27448 ) ) ;
#179235 = EDGE_CURVE ( 'NONE', #42010, #98991, #244934, .T. ) ;
#179237 = EDGE_CURVE ( 'NONE', #84318, #230992, #120075, .T. ) ;
#179236 = LINE ( 'NONE', #38417, #124233 ) ;
#179239 = CARTESIAN_POINT ( 'NONE',  ( -18.41817142474042157, -0.7469768386996047393, -242.2067401450736668 ) ) ;
#179238 = AXIS2_PLACEMENT_3D ( 'NONE', #12763, #92261, #184305 ) ;
#179240 = CARTESIAN_POINT ( 'NONE',  ( -23.25000000000000000, 19.84582043097491422, -235.7234899326461743 ) ) ;
#179241 = PLANE ( 'NONE',  #242650 ) ;
#179242 = ORIENTED_EDGE ( 'NONE', *, *, #178395, .F. ) ;
#179243 = CYLINDRICAL_SURFACE ( 'NONE', #104570, 0.09999999999999781286 ) ;
#179244 = FACE_OUTER_BOUND ( 'NONE', #197716, .T. ) ;
#179245 = LINE ( 'NONE', #240475, #203385 ) ;
#179246 = DIRECTION ( 'NONE',  ( 0.000000000000000000, 1.069579021796876340E-15, 1.000000000000000000 ) ) ;
#179247 = AXIS2_PLACEMENT_3D ( 'NONE', #143013, #140458, #85590 ) ;
#179248 = CARTESIAN_POINT ( 'NONE',  ( -20.54999999999999716, 71.65000000001151648, -48.37310748452435405 ) ) ;
#179249 = ADVANCED_FACE ( 'NONE', ( #19881 ), #1567, .F. ) ;
#179252 = ADVANCED_FACE ( 'NONE', ( #98080 ), #57688, .T. ) ;
#179251 = LINE ( 'NONE', #198777, #234223 ) ;
#179250 = CIRCLE ( 'NONE', #150203, 0.1000000000000028644 ) ;
#179254 = ORIENTED_EDGE ( 'NONE', *, *, #231466, .T. ) ;
#179253 = DIRECTION ( 'NONE',  ( 0.7071067811865474617, 0.7071067811865474617, -0.000000000000000000 ) ) ;
#179255 = CARTESIAN_POINT ( 'NONE',  ( -16.92280123533699410, 66.05000000001187743, -90.17247517043927019 ) ) ;
#179256 = CARTESIAN_POINT ( 'NONE',  ( 18.58719872626879877, 77.36871634755026150, -241.7964367688455241 ) ) ;
#179257 = AXIS2_PLACEMENT_3D ( 'NONE', #62799, #4105, #220596 ) ;
#179258 = DIRECTION ( 'NONE',  ( -0.8660254037844724584, -0.1308764992082773471, -0.4825674480887902629 ) ) ;
#179259 = ADVANCED_FACE ( 'NONE', ( #21181 ), #28510, .T. ) ;
#179260 = DIRECTION ( 'NONE',  ( -0.000000000000000000, -0.9126074666063771490, -0.4088369013363281623 ) ) ;
#179262 = ORIENTED_EDGE ( 'NONE', *, *, #98804, .F. ) ;
#179261 = DIRECTION ( 'NONE',  ( -0.000000000000000000, -1.000000000000000000, 0.000000000000000000 ) ) ;
#179263 = CARTESIAN_POINT ( 'NONE',  ( 23.14999999999999858, 7.244009986534929446, -211.6437749090809177 ) ) ;
#179264 = AXIS2_PLACEMENT_3D ( 'NONE', #8283, #68248, #147793 ) ;
#179265 = DIRECTION ( 'NONE',  ( -1.000000000000000000, -0.000000000000000000, -0.000000000000000000 ) ) ;
#179266 = DIRECTION ( 'NONE',  ( 1.000000000000000000, 0.000000000000000000, 0.000000000000000000 ) ) ;
#179267 = CIRCLE ( 'NONE', #66812, 0.1000000000000052097 ) ;
#179268 = ORIENTED_EDGE ( 'NONE', *, *, #101136, .T. ) ;
#179269 = DIRECTION ( 'NONE',  ( -3.469446951953501855E-14, 0.1575546449569757979, -0.9875102702516471709 ) ) ;
#179270 = DIRECTION ( 'NONE',  ( 0.000000000000000000, 0.000000000000000000, 1.000000000000000000 ) ) ;
#179271 = ADVANCED_FACE ( 'NONE', ( #181526 ), #190806, .F. ) ;
#179272 = CARTESIAN_POINT ( 'NONE',  ( 21.04999999999998650, 69.35000000001156195, -57.27310748452436684 ) ) ;
#179273 = EDGE_CURVE ( 'NONE', #85043, #97414, #160694, .T. ) ;
#179274 = DIRECTION ( 'NONE',  ( 0.000000000000000000, 6.982962677686266711E-15, -1.000000000000000000 ) ) ;
#179276 = DIRECTION ( 'NONE',  ( -1.000000000000000000, 0.000000000000000000, 0.000000000000000000 ) ) ;
#179275 = CIRCLE ( 'NONE', #196013, 0.5999999999999894307 ) ;
#179277 = AXIS2_PLACEMENT_3D ( 'NONE', #146290, #206275, #107163 ) ;
#179279 = VERTEX_POINT ( 'NONE', #121568 ) ;
#179278 = CIRCLE ( 'NONE', #208303, 0.1000000000000028644 ) ;
#179280 = ORIENTED_EDGE ( 'NONE', *, *, #125274, .F. ) ;
#179281 = AXIS2_PLACEMENT_3D ( 'NONE', #112763, #37101, #157038 ) ;
#179282 = CIRCLE ( 'NONE', #37625, 0.1000000000000026007 ) ;
#179283 = CARTESIAN_POINT ( 'NONE',  ( -21.05000000000000071, 70.10000000001220144, -146.7422072491807796 ) ) ;
#179284 = FACE_OUTER_BOUND ( 'NONE', #240076, .T. ) ;
#179285 = CARTESIAN_POINT ( 'NONE',  ( -20.54999999999999716, 1.940186915899009490, -113.3291192110533672 ) ) ;
#179286 = CARTESIAN_POINT ( 'NONE',  ( 18.49999999999999289, 6.650000000011155876, -54.85000000000000142 ) ) ;
#179287 = ORIENTED_EDGE ( 'NONE', *, *, #244879, .F. ) ;
#179288 = EDGE_CURVE ( 'NONE', #214183, #88756, #124157, .T. ) ;
#179289 = EDGE_CURVE ( 'NONE', #118763, #98142, #115950, .T. ) ;
#179290 = FACE_OUTER_BOUND ( 'NONE', #213793, .T. ) ;
#179291 = CARTESIAN_POINT ( 'NONE',  ( 20.77766267348356166, 11.82544895625581738, -206.1952355620770732 ) ) ;
#179292 = AXIS2_PLACEMENT_3D ( 'NONE', #215636, #94410, #136084 ) ;
#179293 = CARTESIAN_POINT ( 'NONE',  ( 20.95496329884391784, 10.56743320610419445, -108.0743099322848479 ) ) ;
#179294 = CARTESIAN_POINT ( 'NONE',  ( 21.05000000000000071, 76.00000000001188027, -99.02310748452428868 ) ) ;
#179295 = ORIENTED_EDGE ( 'NONE', *, *, #195351, .T. ) ;
#179296 = DIRECTION ( 'NONE',  ( -1.000000000000000000, -0.000000000000000000, -0.000000000000000000 ) ) ;
#179297 = ORIENTED_EDGE ( 'NONE', *, *, #52512, .T. ) ;
#179298 = CARTESIAN_POINT ( 'NONE',  ( -20.64999999999999858, 4.250000000011156409, -54.64999999999999858 ) ) ;
#179299 = VERTEX_POINT ( 'NONE', #78540 ) ;
#179300 = CARTESIAN_POINT ( 'NONE',  ( -17.11825945287481687, 9.950000000011138823, -154.7500000000000284 ) ) ;
#179301 = CYLINDRICAL_SURFACE ( 'NONE', #84522, 0.5000000000000004441 ) ;
#179302 = CARTESIAN_POINT ( 'NONE',  ( 18.49999999999998934, 69.45000000001149942, -48.27310748452436684 ) ) ;
#179303 = VERTEX_POINT ( 'NONE', #219336 ) ;
#179304 = CYLINDRICAL_SURFACE ( 'NONE', #132245, 0.1000000000000124678 ) ;
#179305 = CARTESIAN_POINT ( 'NONE',  ( -23.25000000000000000, 11.65000000001115588, -100.5000000000000284 ) ) ;
#179307 = ORIENTED_EDGE ( 'NONE', *, *, #132367, .T. ) ;
#179306 = TOROIDAL_SURFACE ( 'NONE', #175231, 11.65000000000000036, 0.1000000000000000056 ) ;
#179308 = CARTESIAN_POINT ( 'NONE',  ( 22.49999999999999645, 11.74956712350054744, -100.3991416309013402 ) ) ;
#179310 = ORIENTED_EDGE ( 'NONE', *, *, #70519, .T. ) ;
#179309 = CARTESIAN_POINT ( 'NONE',  ( 18.59999999999999076, 6.550000000011156231, -88.25000000000005684 ) ) ;
#179311 = AXIS2_PLACEMENT_3D ( 'NONE', #143135, #240979, #160184 ) ;
#179312 = DIRECTION ( 'NONE',  ( 0.000000000000000000, 0.000000000000000000, -1.000000000000000000 ) ) ;
#179313 = CARTESIAN_POINT ( 'NONE',  ( -18.42609945526433535, 85.49999971050328895, -163.0237449942759156 ) ) ;
#179314 = EDGE_CURVE ( 'NONE', #13384, #149370, #61768, .T. ) ;
#179315 = VERTEX_POINT ( 'NONE', #77255 ) ;
#179316 = CARTESIAN_POINT ( 'NONE',  ( -20.85000000000000142, 76.00000000001142553, -36.02310748452432421 ) ) ;
#179317 = CARTESIAN_POINT ( 'NONE',  ( 21.05000000000000071, 10.72371710471867701, -79.16119029412749342 ) ) ;
#179318 = CIRCLE ( 'NONE', #208536, 0.5000000000000008882 ) ;
#179319 = CARTESIAN_POINT ( 'NONE',  ( 23.04999999999999716, 8.822561741677553471, -109.7500000000000426 ) ) ;
#179320 = ORIENTED_EDGE ( 'NONE', *, *, #141105, .T. ) ;
#179321 = CARTESIAN_POINT ( 'NONE',  ( 13.99999999999999822, 66.15000000001155911, -52.77310748452440237 ) ) ;
#179322 = DIRECTION ( 'NONE',  ( -1.000000000000000000, -0.000000000000000000, -0.000000000000000000 ) ) ;
#179323 = FACE_OUTER_BOUND ( 'NONE', #99221, .T. ) ;
#179324 = AXIS2_PLACEMENT_3D ( 'NONE', #1440, #83521, #163115 ) ;
#179325 = EDGE_LOOP ( 'NONE', ( #174537, #98471, #51756, #145270 ) ) ;
#179326 = EDGE_CURVE ( 'NONE', #64541, #17866, #103267, .T. ) ;
#179327 = ORIENTED_EDGE ( 'NONE', *, *, #200770, .F. ) ;
#179328 = VECTOR ( 'NONE', #92232, 1000.000000000000000 ) ;
#179330 = ORIENTED_EDGE ( 'NONE', *, *, #247066, .F. ) ;
#179329 = TOROIDAL_SURFACE ( 'NONE', #158488, 0.6000000000000004219, 0.1000000000000000056 ) ;
#179331 = EDGE_LOOP ( 'NONE', ( #2080, #230500, #138802, #8865 ) ) ;
#179332 = CARTESIAN_POINT ( 'NONE',  ( -23.39999999999994529, 76.00000000001119815, -36.02310748452479316 ) ) ;
#179333 = CARTESIAN_POINT ( 'NONE',  ( 21.09787244211750945, 8.775370707348422172, -45.73925338431762810 ) ) ;
#179335 = EDGE_LOOP ( 'NONE', ( #99857, #100491 ) ) ;
#179334 = LINE ( 'NONE', #158493, #137487 ) ;
#179336 = CARTESIAN_POINT ( 'NONE',  ( 20.85000000000000142, 11.75000000001115907, -93.71613433702195550 ) ) ;
#179337 = DIRECTION ( 'NONE',  ( 2.952720810173289112E-16, 1.000000000000000000, 6.982962677686266711E-15 ) ) ;
#179338 = CARTESIAN_POINT ( 'NONE',  ( -21.05000000000000071, -11.41227409413852989, -103.5000000000000426 ) ) ;
#179339 = CARTESIAN_POINT ( 'NONE',  ( -16.87665923198281348, 51.61886293219124155, -231.9464690156495692 ) ) ;
#179340 = DIRECTION ( 'NONE',  ( 0.000000000000000000, 0.9553114395362780620, -0.2956011730205483912 ) ) ;
#179341 = DIRECTION ( 'NONE',  ( -1.000000000000000000, 0.000000000000000000, 0.000000000000000000 ) ) ;
#179343 = ORIENTED_EDGE ( 'NONE', *, *, #143036, .T. ) ;
#179342 = CARTESIAN_POINT ( 'NONE',  ( -16.89797118371505036, 66.02361927736811253, -182.5858141169664179 ) ) ;
#179345 = ORIENTED_EDGE ( 'NONE', *, *, #12485, .F. ) ;
#179344 = DIRECTION ( 'NONE',  ( 0.000000000000000000, 0.000000000000000000, -1.000000000000000000 ) ) ;
#179346 = DIRECTION ( 'NONE',  ( -1.186688945009010077E-16, -0.9651348961777154178, 0.2617529984165037904 ) ) ;
#179347 = CIRCLE ( 'NONE', #225086, 7.800000000000002487 ) ;
#179348 = ORIENTED_EDGE ( 'NONE', *, *, #78800, .T. ) ;
#179349 = EDGE_LOOP ( 'NONE', ( #94661, #45680, #129982 ) ) ;
#179350 = CARTESIAN_POINT ( 'NONE',  ( -21.04999999999999716, 6.307425219576570541, -167.5168198683856247 ) ) ;
#179351 = CARTESIAN_POINT ( 'NONE',  ( 18.39999999999999503, 11.74999999999998224, -24.25000000000001066 ) ) ;
#179352 = DIRECTION ( 'NONE',  ( 0.000000000000000000, 1.000000000000000000, 6.688090509790097607E-15 ) ) ;
#179353 = CARTESIAN_POINT ( 'NONE',  ( 18.49999999999999645, 7.128833340094563376, -233.7327013124401276 ) ) ;
#179354 = DIRECTION ( 'NONE',  ( -0.000000000000000000, -0.000000000000000000, -1.000000000000000000 ) ) ;
#179355 = CARTESIAN_POINT ( 'NONE',  ( 21.05000000000000071, 18.82290990851282331, -233.3604470821920529 ) ) ;
#179356 = DIRECTION ( 'NONE',  ( 0.000000000000000000, 0.9126074666063753726, 0.4088369013363320481 ) ) ;
#179357 = CIRCLE ( 'NONE', #16865, 0.09999999999998898659 ) ;
#179358 = VERTEX_POINT ( 'NONE', #118978 ) ;
#179359 = ORIENTED_EDGE ( 'NONE', *, *, #55559, .T. ) ;
#179360 = VECTOR ( 'NONE', #65014, 1000.000000000000000 ) ;
#179361 = DIRECTION ( 'NONE',  ( -0.000000000000000000, 0.8660254037844502539, 0.4999999999999799050 ) ) ;
#179362 = EDGE_CURVE ( 'NONE', #158102, #17245, #7616, .T. ) ;
#179363 = CIRCLE ( 'NONE', #166913, 0.1000000000000060146 ) ;
#179364 = ORIENTED_EDGE ( 'NONE', *, *, #239345, .T. ) ;
#179365 = DIRECTION ( 'NONE',  ( 1.000000000000000000, 0.000000000000000000, 0.000000000000000000 ) ) ;
#179366 = CARTESIAN_POINT ( 'NONE',  ( -20.94999999999999929, 76.00000000001213607, -136.5231074845243313 ) ) ;
#179367 = CARTESIAN_POINT ( 'NONE',  ( -20.54999999999999716, 2.000000000011154189, -46.72462192276210402 ) ) ;
#179368 = AXIS2_PLACEMENT_3D ( 'NONE', #13740, #213204, #174141 ) ;
#179369 = CARTESIAN_POINT ( 'NONE',  ( -23.15000000000000213, 87.65000000001246860, -181.7731074845242745 ) ) ;
#179370 = EDGE_CURVE ( 'NONE', #217909, #103588, #235071, .T. ) ;
#179371 = VERTEX_POINT ( 'NONE', #120288 ) ;
#179372 = CARTESIAN_POINT ( 'NONE',  ( -18.59999999999999787, 70.37092869010230345, -198.1237041667535550 ) ) ;
#179373 = ORIENTED_EDGE ( 'NONE', *, *, #91088, .T. ) ;
#179374 = CARTESIAN_POINT ( 'NONE',  ( 19.97071067811864609, 64.27928932189357170, -148.6731074845244507 ) ) ;
#179375 = ORIENTED_EDGE ( 'NONE', *, *, #48994, .F. ) ;
#179376 = EDGE_CURVE ( 'NONE', #34176, #41259, #56403, .T. ) ;
#179377 = CIRCLE ( 'NONE', #212694, 0.2000000000000057288 ) ;
#179378 = CARTESIAN_POINT ( 'NONE',  ( -21.65000000000000213, 22.97806745954241947, -230.9350634111226270 ) ) ;
#179379 = CARTESIAN_POINT ( 'NONE',  ( -21.45000000000000284, 7.708578643773852157, -79.25000000000004263 ) ) ;
#179380 = ORIENTED_EDGE ( 'NONE', *, *, #95209, .F. ) ;
#179381 = DIRECTION ( 'NONE',  ( 0.000000000000000000, 0.000000000000000000, -1.000000000000000000 ) ) ;
#179382 = ADVANCED_FACE ( 'NONE', ( #199807 ), #116408, .F. ) ;
#179384 = EDGE_LOOP ( 'NONE', ( #199401, #60613, #70854, #114950 ) ) ;
#179383 = CARTESIAN_POINT ( 'NONE',  ( 22.39999999999999503, 64.35000000001164722, -69.52310748452438816 ) ) ;
#179385 = CARTESIAN_POINT ( 'NONE',  ( 20.94999999999999929, 77.34915357198741503, -28.23561014893443044 ) ) ;
#179386 = ORIENTED_EDGE ( 'NONE', *, *, #137908, .T. ) ;
#179387 = DIRECTION ( 'NONE',  ( 0.000000000000000000, 0.000000000000000000, -1.000000000000000000 ) ) ;
#179388 = ORIENTED_EDGE ( 'NONE', *, *, #99475, .T. ) ;
#179389 = CARTESIAN_POINT ( 'NONE',  ( 21.14999999999999858, 1.115600667400684642E-11, -122.3504291924552234 ) ) ;
#179390 = ADVANCED_FACE ( 'NONE', ( #23749 ), #95092, .T. ) ;
#179392 = DIRECTION ( 'NONE',  ( 0.7070776581708965169, 4.937903618720407826E-15, -0.7071359030027827286 ) ) ;
#179391 = AXIS2_PLACEMENT_3D ( 'NONE', #180538, #241779, #81388 ) ;
#179393 = DIRECTION ( 'NONE',  ( 0.000000000000000000, 0.000000000000000000, -1.000000000000000000 ) ) ;
#179394 = CARTESIAN_POINT ( 'NONE',  ( -16.89268316805465986, 9.951721813253337601, -121.3557524785455826 ) ) ;
#179395 = DIRECTION ( 'NONE',  ( -1.000000000000000000, 0.000000000000000000, -0.000000000000000000 ) ) ;
#179396 = AXIS2_PLACEMENT_3D ( 'NONE', #220902, #256123, #119268 ) ;
#179397 = ORIENTED_EDGE ( 'NONE', *, *, #217176, .T. ) ;
#179398 = FACE_OUTER_BOUND ( 'NONE', #240181, .T. ) ;
#179399 = PLANE ( 'NONE',  #236776 ) ;
#179400 = CARTESIAN_POINT ( 'NONE',  ( 23.14999999999999503, 11.65000000001116298, -55.25000000000004974 ) ) ;
#179401 = AXIS2_PLACEMENT_3D ( 'NONE', #21255, #42094, #141174 ) ;
#179402 = ORIENTED_EDGE ( 'NONE', *, *, #73390, .F. ) ;
#179403 = DIRECTION ( 'NONE',  ( 0.000000000000000000, 0.1350103645451807555, 0.9908441862701609093 ) ) ;
#179404 = ORIENTED_EDGE ( 'NONE', *, *, #24774, .F. ) ;
#179405 = PLANE ( 'NONE',  #194002 ) ;
#179406 = ORIENTED_EDGE ( 'NONE', *, *, #167872, .T. ) ;
#179407 = CARTESIAN_POINT ( 'NONE',  ( 23.14999999999999503, 11.65000000001116298, -126.9851942293460922 ) ) ;
#179408 = DIRECTION ( 'NONE',  ( 1.000000000000000000, 0.000000000000000000, 0.000000000000000000 ) ) ;
#179409 = EDGE_LOOP ( 'NONE', ( #56308, #176197, #172667, #71557, #249230 ) ) ;
#179410 = AXIS2_PLACEMENT_3D ( 'NONE', #48351, #88739, #33977 ) ;
#179412 = ORIENTED_EDGE ( 'NONE', *, *, #169208, .T. ) ;
#179411 = DIRECTION ( 'NONE',  ( 0.000000000000000000, 0.000000000000000000, 1.000000000000000000 ) ) ;
#179413 = CARTESIAN_POINT ( 'NONE',  ( 20.94999999999999929, 5.500000000011153745, -88.09473398108696074 ) ) ;
#179414 = EDGE_LOOP ( 'NONE', ( #24206, #172345, #180905, #123663 ) ) ;
#179415 = DIRECTION ( 'NONE',  ( 0.000000000000000000, 1.000000000000000000, 0.000000000000000000 ) ) ;
#179416 = CARTESIAN_POINT ( 'NONE',  ( -21.05000000000000071, -1.249999999988843369, -75.00000000000004263 ) ) ;
#179417 = ORIENTED_EDGE ( 'NONE', *, *, #169021, .F. ) ;
#179418 = ORIENTED_EDGE ( 'NONE', *, *, #26784, .F. ) ;
#179419 = FACE_OUTER_BOUND ( 'NONE', #217425, .T. ) ;
#179420 = DIRECTION ( 'NONE',  ( 0.000000000000000000, 0.000000000000000000, 1.000000000000000000 ) ) ;
#179421 = B_SPLINE_CURVE_WITH_KNOTS ( 'NONE', 3,
 ( #181034, #83155, #246132, #124902, #203144, #162755 ),
 .UNSPECIFIED., .F., .F.,
 ( 4, 2, 4 ),
 ( 0.000000000000000000, 0.0001568709654583398281, 0.0003137419309166796563 ),
 .UNSPECIFIED. ) ;
#179422 = EDGE_LOOP ( 'NONE', ( #239738, #4115, #98624, #102610 ) ) ;
#179423 = CARTESIAN_POINT ( 'NONE',  ( 20.94999999999999929, 77.36242903720467723, -28.13422623660311217 ) ) ;
#179424 = VECTOR ( 'NONE', #161696, 1000.000000000000000 ) ;
#179425 = AXIS2_PLACEMENT_3D ( 'NONE', #136994, #239962, #61317 ) ;
#179426 = ORIENTED_EDGE ( 'NONE', *, *, #62120, .T. ) ;
#179427 = ORIENTED_EDGE ( 'NONE', *, *, #162307, .F. ) ;
#179428 = EDGE_CURVE ( 'NONE', #225825, #24660, #240843, .T. ) ;
#179429 = VECTOR ( 'NONE', #79862, 1000.000000000000000 ) ;
#179430 = DIRECTION ( 'NONE',  ( -1.000000000000000000, -0.000000000000000000, -0.000000000000000000 ) ) ;
#179431 = CIRCLE ( 'NONE', #166986, 0.1000000000000026007 ) ;
#179432 = AXIS2_PLACEMENT_3D ( 'NONE', #102728, #84427, #143148 ) ;
#179433 = EDGE_CURVE ( 'NONE', #201875, #5985, #224078, .T. ) ;
#179435 = ORIENTED_EDGE ( 'NONE', *, *, #204222, .T. ) ;
#179434 = FACE_BOUND ( 'NONE', #66537, .T. ) ;
#179436 = DIRECTION ( 'NONE',  ( 1.000000000000000000, -0.000000000000000000, 0.000000000000000000 ) ) ;
#179437 = CARTESIAN_POINT ( 'NONE',  ( -16.85939681242906119, 63.04778223063582487, -213.4386086703495948 ) ) ;
#179439 = CARTESIAN_POINT ( 'NONE',  ( -22.41119224318417125, 76.00000000001246292, -181.6726782920691505 ) ) ;
#179438 = CARTESIAN_POINT ( 'NONE',  ( -20.54999999999999716, -8.730841121484173684, -143.5980747189843783 ) ) ;
#179441 = EDGE_CURVE ( 'NONE', #137676, #77226, #144968, .T. ) ;
#179440 = CARTESIAN_POINT ( 'NONE',  ( 23.15000000000000213, 85.60000000001177511, -79.41707660717668205 ) ) ;
#179442 = CARTESIAN_POINT ( 'NONE',  ( -21.05000000000000426, 11.60000000001115872, -73.92820323027559937 ) ) ;
#179443 = DIRECTION ( 'NONE',  ( 0.000000000000000000, 6.982962677686266711E-15, -1.000000000000000000 ) ) ;
#179444 = AXIS2_PLACEMENT_3D ( 'NONE', #84232, #146815, #28207 ) ;
#179445 = DIRECTION ( 'NONE',  ( 1.000000000000000000, 0.000000000000000000, 0.000000000000000000 ) ) ;
#179446 = AXIS2_PLACEMENT_3D ( 'NONE', #147584, #48475, #129307 ) ;
#179447 = AXIS2_PLACEMENT_3D ( 'NONE', #248813, #50575, #149730 ) ;
#179448 = AXIS2_PLACEMENT_3D ( 'NONE', #136509, #80376, #75307 ) ;
#179449 = VERTEX_POINT ( 'NONE', #65403 ) ;
#179450 = ORIENTED_EDGE ( 'NONE', *, *, #194553, .F. ) ;
#179451 = ORIENTED_EDGE ( 'NONE', *, *, #139898, .T. ) ;
#179452 = DIRECTION ( 'NONE',  ( -1.000000000000000000, -0.000000000000000000, 0.000000000000000000 ) ) ;
#179453 = ADVANCED_FACE ( 'NONE', ( #142370 ), #69988, .T. ) ;
#179454 = EDGE_LOOP ( 'NONE', ( #197739, #11464, #36004 ) ) ;
#179455 = CARTESIAN_POINT ( 'NONE',  ( 21.14999999999999858, 69.45934304831114048, -170.0231074845243882 ) ) ;
#179456 = DIRECTION ( 'NONE',  ( 0.000000000000000000, 0.8814952561688428334, -0.4721928772777349570 ) ) ;
#179457 = EDGE_CURVE ( 'NONE', #241787, #71101, #32597, .T. ) ;
#179458 = EDGE_CURVE ( 'NONE', #24563, #104087, #232489, .T. ) ;
#179459 = ORIENTED_EDGE ( 'NONE', *, *, #232758, .T. ) ;
#179460 =( LENGTH_UNIT ( ) NAMED_UNIT ( * ) SI_UNIT ( .MILLI., .METRE. ) );
#179461 = CARTESIAN_POINT ( 'NONE',  ( -17.78043020864320667, 65.14640788800619475, -92.68615665024458394 ) ) ;
#179463 = ORIENTED_EDGE ( 'NONE', *, *, #60824, .F. ) ;
#179462 = ORIENTED_EDGE ( 'NONE', *, *, #165434, .T. ) ;
#179464 = ORIENTED_EDGE ( 'NONE', *, *, #185059, .F. ) ;
#179465 = ORIENTED_EDGE ( 'NONE', *, *, #78103, .F. ) ;
#179466 = EDGE_CURVE ( 'NONE', #165951, #5557, #223185, .T. ) ;
#179467 = CARTESIAN_POINT ( 'NONE',  ( 23.50000000000005684, 82.64476912853859858, -26.37791261425322986 ) ) ;
#179468 = DIRECTION ( 'NONE',  ( 0.000000000000000000, -0.2617529984165031243, -0.9651348961777157509 ) ) ;
#179470 = ORIENTED_EDGE ( 'NONE', *, *, #145265, .T. ) ;
#179469 = DIRECTION ( 'NONE',  ( 0.000000000000000000, -0.9126074666063545004, -0.4088369013363783999 ) ) ;
#179471 = DIRECTION ( 'NONE',  ( 1.000000000000000000, 0.000000000000000000, 0.000000000000000000 ) ) ;
#179472 = EDGE_CURVE ( 'NONE', #34831, #192857, #128595, .T. ) ;
#179473 = CARTESIAN_POINT ( 'NONE',  ( -20.54999999999999716, 68.75000000001199396, -115.3731074845243540 ) ) ;
#179475 = ORIENTED_EDGE ( 'NONE', *, *, #178933, .T. ) ;
#179474 = FACE_OUTER_BOUND ( 'NONE', #45364, .T. ) ;
#179476 = DIRECTION ( 'NONE',  ( 0.000000000000000000, 0.000000000000000000, 1.000000000000000000 ) ) ;
#179478 = ADVANCED_FACE ( 'NONE', ( #47103 ), #83646, .F. ) ;
#179477 = ORIENTED_EDGE ( 'NONE', *, *, #7672, .T. ) ;
#179479 = CARTESIAN_POINT ( 'NONE',  ( 20.12500000000000000, 9.750000000011153745, -175.6117712821142618 ) ) ;
#179480 = AXIS2_PLACEMENT_3D ( 'NONE', #187420, #145695, #205669 ) ;
#179482 = ORIENTED_EDGE ( 'NONE', *, *, #15983, .T. ) ;
#179481 = DIRECTION ( 'NONE',  ( -1.000000000000000000, -3.265361837132813093E-16, 0.000000000000000000 ) ) ;
#179483 = CARTESIAN_POINT ( 'NONE',  ( 21.00000000000000000, 66.25000000001260503, -191.1731074845244223 ) ) ;
#179484 = DIRECTION ( 'NONE',  ( 0.000000000000000000, 0.9915357197604794948, -0.1298341882520470392 ) ) ;
#179485 = CARTESIAN_POINT ( 'NONE',  ( 20.96428641294217954, 11.75000000001150013, -60.17489317794084513 ) ) ;
#179486 = ORIENTED_EDGE ( 'NONE', *, *, #132277, .T. ) ;
#179488 = CARTESIAN_POINT ( 'NONE',  ( -16.87487986503753845, 44.13545556447066076, -235.2989350391281391 ) ) ;
#179487 = CARTESIAN_POINT ( 'NONE',  ( -16.87683809663752399, 9.850000000011123191, -46.90236401819647938 ) ) ;
#179489 = DIRECTION ( 'NONE',  ( 0.000000000000000000, 0.2617529984165035128, 0.9651348961777155289 ) ) ;
#179490 = CARTESIAN_POINT ( 'NONE',  ( 18.31572054635728009, 85.54847543579103331, -163.1725373197758415 ) ) ;
#179491 = AXIS2_PLACEMENT_3D ( 'NONE', #257276, #117815, #17432 ) ;
#179492 = DIRECTION ( 'NONE',  ( -1.000000000000000000, 0.000000000000000000, 0.000000000000000000 ) ) ;
#179493 = DIRECTION ( 'NONE',  ( 0.000000000000000000, 0.000000000000000000, 1.000000000000000000 ) ) ;
#179494 = ORIENTED_EDGE ( 'NONE', *, *, #83882, .T. ) ;
#179495 = ORIENTED_EDGE ( 'NONE', *, *, #57533, .T. ) ;
#179496 = EDGE_LOOP ( 'NONE', ( #135193, #214504, #99577, #18248 ) ) ;
#179498 = AXIS2_PLACEMENT_3D ( 'NONE', #185906, #67243, #8565 ) ;
#179497 = CARTESIAN_POINT ( 'NONE',  ( -21.11833042828115481, 0.007100509070730082022, -127.5543553061452542 ) ) ;
#179500 = EDGE_LOOP ( 'NONE', ( #229804, #41572, #92570 ) ) ;
#179499 = ADVANCED_FACE ( 'NONE', ( #108393 ), #90996, .F. ) ;
#179501 = CARTESIAN_POINT ( 'NONE',  ( 21.05000000000000071, 87.29603075034775372, -173.0710066441881452 ) ) ;
#179502 = EDGE_LOOP ( 'NONE', ( #199088, #103931, #134634, #230122 ) ) ;
#179503 = ADVANCED_FACE ( 'NONE', ( #187933 ), #124115, .T. ) ;
#179504 = CARTESIAN_POINT ( 'NONE',  ( 23.14999999999999858, 1.148907358139439339E-11, -201.0000000000015064 ) ) ;
#179505 = DIRECTION ( 'NONE',  ( 0.000000000000000000, 0.000000000000000000, 1.000000000000000000 ) ) ;
#179507 = EDGE_CURVE ( 'NONE', #178218, #18361, #82370, .T. ) ;
#179506 = VERTEX_POINT ( 'NONE', #224470 ) ;
#179508 = CARTESIAN_POINT ( 'NONE',  ( 19.97071067811864609, 34.39212750349580006, -235.0405048756463486 ) ) ;
#179509 = CIRCLE ( 'NONE', #233671, 0.2000000000000057288 ) ;
#179511 = VERTEX_POINT ( 'NONE', #25025 ) ;
#179510 = CIRCLE ( 'NONE', #83770, 0.09999999999998898659 ) ;
#179512 = ORIENTED_EDGE ( 'NONE', *, *, #166072, .T. ) ;
#179513 = ORIENTED_EDGE ( 'NONE', *, *, #87881, .T. ) ;
#179514 = AXIS2_PLACEMENT_3D ( 'NONE', #108562, #90259, #169868 ) ;
#179515 = DIRECTION ( 'NONE',  ( -0.000000000000000000, 7.272083257015735086E-15, -1.000000000000000000 ) ) ;
#179516 = CARTESIAN_POINT ( 'NONE',  ( 22.41477678272288188, 75.99917613424982221, -215.1726927690397702 ) ) ;
#179517 = CARTESIAN_POINT ( 'NONE',  ( 20.95512820512820440, 8.876151316299271343, -142.5586289951409640 ) ) ;
#179518 = DIRECTION ( 'NONE',  ( 1.000000000000000000, 0.000000000000000000, 0.000000000000000000 ) ) ;
#179519 = DIRECTION ( 'NONE',  ( -0.000000000000000000, 0.8660254037844411501, 0.4999999999999956701 ) ) ;
#179520 = FACE_OUTER_BOUND ( 'NONE', #242779, .T. ) ;
#179521 = DIRECTION ( 'NONE',  ( -0.000000000000000000, -0.000000000000000000, -1.000000000000000000 ) ) ;
#179522 = CARTESIAN_POINT ( 'NONE',  ( 23.14999999999999858, 78.00000000001213607, -136.5231074845243029 ) ) ;
#179524 = VERTEX_POINT ( 'NONE', #241484 ) ;
#179523 = FACE_OUTER_BOUND ( 'NONE', #246613, .T. ) ;
#179525 = DIRECTION ( 'NONE',  ( 1.000000000000000000, 0.000000000000000000, 0.000000000000000000 ) ) ;
#179526 = ORIENTED_EDGE ( 'NONE', *, *, #117088, .T. ) ;
#179527 = CARTESIAN_POINT ( 'NONE',  ( -16.88495309932522304, 22.96663205285974385, -230.9236886748582549 ) ) ;
#179528 = ORIENTED_EDGE ( 'NONE', *, *, #240402, .T. ) ;
#179529 = ORIENTED_EDGE ( 'NONE', *, *, #142522, .T. ) ;
#179530 = SPHERICAL_SURFACE ( 'NONE', #4847, 0.1000000000000000056 ) ;
#179531 = CARTESIAN_POINT ( 'NONE',  ( 18.59999999999999076, 10.49142135624846439, -58.35000000000000142 ) ) ;
#179533 = EDGE_CURVE ( 'NONE', #232829, #89128, #104503, .T. ) ;
#179532 = CARTESIAN_POINT ( 'NONE',  ( -16.89268316805466341, 66.04827818676939444, -56.87885996306994230 ) ) ;
#179534 = VERTEX_POINT ( 'NONE', #125392 ) ;
#179535 = VECTOR ( 'NONE', #162072, 1000.000000000000000 ) ;
#179536 = EDGE_CURVE ( 'NONE', #157888, #197596, #16194, .T. ) ;
#179537 = CARTESIAN_POINT ( 'NONE',  ( -23.15000000000000213, -11.64999999998884483, -130.9000000000000341 ) ) ;
#179538 = ORIENTED_EDGE ( 'NONE', *, *, #255333, .T. ) ;
#179539 = ORIENTED_EDGE ( 'NONE', *, *, #195915, .T. ) ;
#179540 = EDGE_CURVE ( 'NONE', #208712, #35508, #57441, .T. ) ;
#179542 = EDGE_CURVE ( 'NONE', #86021, #205324, #93951, .T. ) ;
#179541 = CARTESIAN_POINT ( 'NONE',  ( -16.92778301347286884, 10.00094491683533526, -12.57148189203151034 ) ) ;
#179543 = ORIENTED_EDGE ( 'NONE', *, *, #104198, .F. ) ;
#179544 = CARTESIAN_POINT ( 'NONE',  ( 19.97071067811865319, 64.27928932189330169, -111.8145288407616817 ) ) ;
#179545 = CARTESIAN_POINT ( 'NONE',  ( -20.94999999999999929, 26.25728039895700050, -243.9792867493661106 ) ) ;
#179546 = VERTEX_POINT ( 'NONE', #90088 ) ;
#179547 = DIRECTION ( 'NONE',  ( 1.000000000000000000, -0.000000000000000000, -0.000000000000000000 ) ) ;
#179548 = DIRECTION ( 'NONE',  ( 1.000000000000000000, 0.000000000000000000, 0.000000000000000000 ) ) ;
#179549 = VERTEX_POINT ( 'NONE', #191805 ) ;
#179550 = EDGE_CURVE ( 'NONE', #230716, #130418, #24378, .T. ) ;
#179551 = CYLINDRICAL_SURFACE ( 'NONE', #21065, 11.80000000000000426 ) ;
#179552 = AXIS2_PLACEMENT_3D ( 'NONE', #128341, #44942, #4511 ) ;
#179554 = DIRECTION ( 'NONE',  ( 0.000000000000000000, 0.000000000000000000, -1.000000000000000000 ) ) ;
#179553 = CIRCLE ( 'NONE', #208764, 0.1000000000000008937 ) ;
#179555 = CIRCLE ( 'NONE', #92037, 0.2000000000000057288 ) ;
#179556 = DIRECTION ( 'NONE',  ( 0.000000000000000000, 0.000000000000000000, 1.000000000000000000 ) ) ;
#179557 = EDGE_CURVE ( 'NONE', #140913, #78910, #116145, .T. ) ;
#179558 = ORIENTED_EDGE ( 'NONE', *, *, #171932, .F. ) ;
#179559 = EDGE_CURVE ( 'NONE', #192753, #82161, #130506, .T. ) ;
#179560 = VERTEX_POINT ( 'NONE', #30155 ) ;
#179561 = CARTESIAN_POINT ( 'NONE',  ( -23.49999999999994316, 76.00000000001119815, -36.02310748452479316 ) ) ;
#179562 = EDGE_CURVE ( 'NONE', #150648, #127380, #14450, .T. ) ;
#179563 = DIRECTION ( 'NONE',  ( 0.000000000000000000, -0.9126074666063660468, -0.4088369013363524762 ) ) ;
#179564 = DIRECTION ( 'NONE',  ( 0.000000000000000000, -0.9371753822965316338, 0.3488585713686134793 ) ) ;
#179565 = DIRECTION ( 'NONE',  ( -1.000000000000000000, 0.000000000000000000, 0.000000000000000000 ) ) ;
#179566 = CARTESIAN_POINT ( 'NONE',  ( 18.59999999999999787, 77.36242903720540198, -128.6342262366031548 ) ) ;
#179567 = VECTOR ( 'NONE', #252990, 1000.000000000000000 ) ;
#179568 = ORIENTED_EDGE ( 'NONE', *, *, #65569, .T. ) ;
#179569 = CARTESIAN_POINT ( 'NONE',  ( 20.94999999999999929, 5.400000000011154988, -112.9052660189131245 ) ) ;
#179570 = CARTESIAN_POINT ( 'NONE',  ( -16.81744102076749314, 9.950000000011142376, -146.6500000000000341 ) ) ;
#179571 = DIRECTION ( 'NONE',  ( 0.000000000000000000, -0.9651348961777157509, 0.2617529984165031243 ) ) ;
#179572 = ADVANCED_FACE ( 'NONE', ( #92666 ), #73146, .F. ) ;
#179573 = EDGE_CURVE ( 'NONE', #24454, #182190, #11880, .T. ) ;
#179574 = CARTESIAN_POINT ( 'NONE',  ( 20.54374330479327426, 65.49498968578859603, -61.79742384963523705 ) ) ;
#179575 = EDGE_LOOP ( 'NONE', ( #75784, #70120, #123878, #31102 ) ) ;
#179576 = ORIENTED_EDGE ( 'NONE', *, *, #118304, .T. ) ;
#179577 = CARTESIAN_POINT ( 'NONE',  ( -18.69999999999999929, 1.350000000000000089, 16.39999999999999858 ) ) ;
#179578 = DIRECTION ( 'NONE',  ( 0.000000000000000000, 0.000000000000000000, 1.000000000000000000 ) ) ;
#179579 = ADVANCED_FACE ( 'NONE', ( #70576 ), #13148, .T. ) ;
#179580 = DIRECTION ( 'NONE',  ( -0.7071067811865475727, 0.7071067811865475727, 4.937700262164531476E-15 ) ) ;
#179581 =( BOUNDED_SURFACE ( )  B_SPLINE_SURFACE ( 3, 2, ( 
 ( #51557, #32061, #131128 ),
 ( #191136, #91998, #253627 ),
 ( #50291, #248509, #129837 ),
 ( #209382, #110275, #189829 ),
 ( #11189, #90711, #33359 ),
 ( #170309, #71180, #171577 ) ),
 .UNSPECIFIED., .F., .F., .F. ) 
 B_SPLINE_SURFACE_WITH_KNOTS ( ( 4, 2, 4 ),
 ( 3, 3 ),
 ( 0.0001792624049599819626, 0.0003686986002124877700, 0.0005581347954649935232 ),
 ( 0.000000000000000000, 1.000000000000000000 ),
 .UNSPECIFIED. ) 
 GEOMETRIC_REPRESENTATION_ITEM ( )  RATIONAL_B_SPLINE_SURFACE ( (
 ( 1.000000000000000000, 0.9238795325112830747, 1.000000000000000000),
 ( 1.000000000000000000, 0.9229318695232786585, 1.000000000000000000),
 ( 1.000000000000000000, 0.8926288119238298124, 1.000000000000000000),
 ( 1.000000000000000000, 0.8123777807263558026, 1.000000000000000000),
 ( 1.000000000000000000, 0.7629087100937371746, 1.000000000000000000),
 ( 1.000000000000000000, 0.7071067811865475727, 1.000000000000000000) ) ) 
 REPRESENTATION_ITEM ( '' )  SURFACE ( )  );
#179582 = DIRECTION ( 'NONE',  ( -1.000000000000000000, 0.000000000000000000, 0.000000000000000000 ) ) ;
#179583 = TOROIDAL_SURFACE ( 'NONE', #133753, 4.099999999999999645, 0.1000000000000000056 ) ;
#179584 = ORIENTED_EDGE ( 'NONE', *, *, #71412, .F. ) ;
#179586 = ADVANCED_FACE ( 'NONE', ( #229624 ), #135408, .T. ) ;
#179585 = CARTESIAN_POINT ( 'NONE',  ( 18.59999999999999076, 11.75000000001115907, -41.60000000000000142 ) ) ;
#179587 = EDGE_CURVE ( 'NONE', #63066, #8158, #106623, .T. ) ;
#179588 = CARTESIAN_POINT ( 'NONE',  ( -18.39999999999999858, 85.50000000001189449, -96.02382180668539036 ) ) ;
#179589 = AXIS2_PLACEMENT_3D ( 'NONE', #33048, #231219, #194673 ) ;
#179590 = CARTESIAN_POINT ( 'NONE',  ( 23.15000000000000213, -8.663551401857999323, -191.4758988819326646 ) ) ;
#179591 = FACE_OUTER_BOUND ( 'NONE', #177005, .T. ) ;
#179592 = AXIS2_PLACEMENT_3D ( 'NONE', #81501, #140199, #157252 ) ;
#179593 = ORIENTED_EDGE ( 'NONE', *, *, #23832, .F. ) ;
#179594 = DIRECTION ( 'NONE',  ( 0.000000000000000000, -7.056502275159890832E-15, 1.000000000000000000 ) ) ;
#179595 = AXIS2_PLACEMENT_3D ( 'NONE', #145856, #164157, #45485 ) ;
#179596 = VERTEX_POINT ( 'NONE', #227882 ) ;
#179597 = EDGE_CURVE ( 'NONE', #253941, #153829, #143197, .T. ) ;
#179598 = FACE_OUTER_BOUND ( 'NONE', #205014, .T. ) ;
#179599 = DIRECTION ( 'NONE',  ( -1.000000000000000000, 0.000000000000000000, 0.000000000000000000 ) ) ;
#179600 = DIRECTION ( 'NONE',  ( 2.952720810173289112E-16, -1.000000000000000000, -0.000000000000000000 ) ) ;
#179601 = CARTESIAN_POINT ( 'NONE',  ( 18.49999999999998934, 65.70711192142341872, -64.06510546851222898 ) ) ;
#179602 = CARTESIAN_POINT ( 'NONE',  ( 18.54999999999999716, 67.25000000001197975, -115.6731074845243654 ) ) ;
#179603 = CARTESIAN_POINT ( 'NONE',  ( 5.551115123125782702E-14, 64.75000000001119815, -25.92310748452479174 ) ) ;
#179605 = DIRECTION ( 'NONE',  ( -4.391705002472921695E-16, 0.4721928772777337913, 0.8814952561688434995 ) ) ;
#179604 = AXIS2_PLACEMENT_3D ( 'NONE', #211868, #127181, #8518 ) ;
#179606 = DIRECTION ( 'NONE',  ( 0.7071067811865127117, 0.7071067811865821007, 0.000000000000000000 ) ) ;
#179607 = LINE ( 'NONE', #114478, #145551 ) ;
#179608 = EDGE_CURVE ( 'NONE', #7786, #166275, #203438, .T. ) ;
#179609 = FACE_OUTER_BOUND ( 'NONE', #217738, .T. ) ;
#179610 = LINE ( 'NONE', #256495, #23163 ) ;
#179611 = CIRCLE ( 'NONE', #33713, 11.80000000000000426 ) ;
#179612 = CARTESIAN_POINT ( 'NONE',  ( 18.49999999999999289, 10.29270135741298731, -105.9573618871519756 ) ) ;
#179613 = CARTESIAN_POINT ( 'NONE',  ( -20.54999999999999716, 1.115600667400684642E-11, -134.0000000000000284 ) ) ;
#179614 = ORIENTED_EDGE ( 'NONE', *, *, #12329, .F. ) ;
#179615 = AXIS2_PLACEMENT_3D ( 'NONE', #250618, #193234, #208936 ) ;
#179616 = CARTESIAN_POINT ( 'NONE',  ( 23.14999999999999503, 11.75000000001116263, -55.25000000000004974 ) ) ;
#179617 = DIRECTION ( 'NONE',  ( -1.000000000000000000, -0.000000000000000000, -0.000000000000000000 ) ) ;
#179618 = EDGE_CURVE ( 'NONE', #196505, #37339, #207721, .T. ) ;
#179619 = CARTESIAN_POINT ( 'NONE',  ( 20.86036036209909383, 10.62104277658211871, -41.16634841850498816 ) ) ;
#179620 = AXIS2_PLACEMENT_3D ( 'NONE', #68367, #84011, #86609 ) ;
#179621 = ORIENTED_EDGE ( 'NONE', *, *, #235995, .F. ) ;
#179622 = DIRECTION ( 'NONE',  ( 0.000000000000000000, 0.9908441862701605762, 0.1350103645451835310 ) ) ;
#179623 = CARTESIAN_POINT ( 'NONE',  ( -18.59999999999999787, -1.164121893241208960, -41.31484808557160449 ) ) ;
#179624 = ORIENTED_EDGE ( 'NONE', *, *, #131929, .T. ) ;
#179625 = DIRECTION ( 'NONE',  ( 1.000000000000000000, 0.000000000000000000, 0.000000000000000000 ) ) ;
#179626 = CARTESIAN_POINT ( 'NONE',  ( 18.49999999999998934, 6.550000000011156231, -88.25000000000005684 ) ) ;
#179627 = EDGE_CURVE ( 'NONE', #77258, #163063, #170155, .T. ) ;
#179628 = CIRCLE ( 'NONE', #67184, 0.09999999999999939493 ) ;
#179629 = ORIENTED_EDGE ( 'NONE', *, *, #188983, .F. ) ;
#179630 = AXIS2_PLACEMENT_3D ( 'NONE', #24797, #80864, #165574 ) ;
#179631 = VECTOR ( 'NONE', #112827, 1000.000000000000000 ) ;
#179632 = VECTOR ( 'NONE', #107533, 1000.000000000000000 ) ;
#179633 = VERTEX_POINT ( 'NONE', #47947 ) ;
#179634 = FACE_OUTER_BOUND ( 'NONE', #39005, .T. ) ;
#179635 = EDGE_LOOP ( 'NONE', ( #93085, #163710, #232061, #195500 ) ) ;
#179637 =( BOUNDED_SURFACE ( )  B_SPLINE_SURFACE ( 3, 2, ( 
 ( #167622, #111478, #9805 ),
 ( #203199, #151913, #231442 ),
 ( #230138, #129754, #250968 ),
 ( #162815, #128475, #191042 ),
 ( #242323, #108901, #29412 ),
 ( #30686, #88031, #110182 ) ),
 .UNSPECIFIED., .F., .F., .F. ) 
 B_SPLINE_SURFACE_WITH_KNOTS ( ( 4, 2, 4 ),
 ( 3, 3 ),
 ( -1.776356839400250465E-15, 0.7853981633974468357, 1.570796326794895448 ),
 ( 0.000000000000000000, 1.000000000000000000 ),
 .UNSPECIFIED. ) 
 GEOMETRIC_REPRESENTATION_ITEM ( )  RATIONAL_B_SPLINE_SURFACE ( (
 ( 1.000000000000000000, 0.5000000000000456302, 1.000000000000000000),
 ( 1.000000000000000000, 0.4993418825331401578, 1.000000000000000000),
 ( 1.000000000000000000, 0.5278258667061684895, 1.000000000000000000),
 ( 1.000000000000000000, 0.6092287576692355655, 1.000000000000000000),
 ( 1.000000000000000000, 0.6611148371781849775, 1.000000000000000000),
 ( 1.000000000000000000, 0.7071067811865597852, 1.000000000000000000) ) ) 
 REPRESENTATION_ITEM ( '' )  SURFACE ( )  );
#179636 = CARTESIAN_POINT ( 'NONE',  ( 21.05000000000000071, -0.01759718700860490523, 6.440770893661947660 ) ) ;
#179638 = DIRECTION ( 'NONE',  ( 1.000000000000000000, 0.000000000000000000, 0.000000000000000000 ) ) ;
#179639 = CARTESIAN_POINT ( 'NONE',  ( 21.10320863425824811, 34.01941935407060669, -243.7204517896670382 ) ) ;
#179640 = DIRECTION ( 'NONE',  ( 1.000000000000000000, 0.000000000000000000, 0.000000000000000000 ) ) ;
#179641 = CYLINDRICAL_SURFACE ( 'NONE', #155911, 0.1000000000000033362 ) ;
#179642 = DIRECTION ( 'NONE',  ( -0.000000000000000000, -0.000000000000000000, 1.000000000000000000 ) ) ;
#179643 = CARTESIAN_POINT ( 'NONE',  ( -20.85000000000000142, 64.75617845954087670, -200.4736850529726269 ) ) ;
#179644 = CARTESIAN_POINT ( 'NONE',  ( 22.47007471830798053, 0.3230635261676697012, -230.0870367350772767 ) ) ;
#179646 = VERTEX_POINT ( 'NONE', #85761 ) ;
#179645 = CARTESIAN_POINT ( 'NONE',  ( 18.41815437325352534, 86.89613897263180320, -199.6357246881775040 ) ) ;
#179647 = VERTEX_POINT ( 'NONE', #244868 ) ;
#179649 = CYLINDRICAL_SURFACE ( 'NONE', #85474, 0.09999999999999939493 ) ;
#179648 = CARTESIAN_POINT ( 'NONE',  ( 22.40000000000010516, -9.465491541613135773E-13, 11.64957080754511232 ) ) ;
#179652 = EDGE_LOOP ( 'NONE', ( #241234, #23535, #218558, #41616 ) ) ;
#179651 = CARTESIAN_POINT ( 'NONE',  ( -16.87401514999236696, 60.95767576634881380, -220.9741856580743331 ) ) ;
#179650 = CARTESIAN_POINT ( 'NONE',  ( 20.95512840106816199, 65.37615130623927939, -191.3206282637256663 ) ) ;
#179653 = ORIENTED_EDGE ( 'NONE', *, *, #250360, .F. ) ;
#179654 = FACE_OUTER_BOUND ( 'NONE', #188577, .T. ) ;
#179655 = DIRECTION ( 'NONE',  ( 1.000000000000000000, 2.379049338482476317E-14, 0.000000000000000000 ) ) ;
#179656 = DIRECTION ( 'NONE',  ( 0.000000000000000000, 0.000000000000000000, 1.000000000000000000 ) ) ;
#179657 = DIRECTION ( 'NONE',  ( -1.000000000000000000, 0.000000000000000000, 0.000000000000000000 ) ) ;
#179658 = FACE_OUTER_BOUND ( 'NONE', #110508, .T. ) ;
#179659 = DIRECTION ( 'NONE',  ( 0.000000000000000000, 0.4721928772777346239, 0.8814952561688430555 ) ) ;
#179660 = CIRCLE ( 'NONE', #195858, 0.3999999999999970801 ) ;
#179661 = EDGE_CURVE ( 'NONE', #18809, #214666, #95281, .T. ) ;
#179662 = DIRECTION ( 'NONE',  ( 0.000000000000000000, 0.9651348961777157509, -0.2617529984165031243 ) ) ;
#179663 = VERTEX_POINT ( 'NONE', #165347 ) ;
#179664 = ORIENTED_EDGE ( 'NONE', *, *, #164755, .T. ) ;
#179665 = DIRECTION ( 'NONE',  ( -1.000000000000000000, 9.012599976028471648E-15, 6.882867235861662930E-14 ) ) ;
#179666 = ORIENTED_EDGE ( 'NONE', *, *, #48407, .T. ) ;
#179667 = DIRECTION ( 'NONE',  ( -1.000000000000000000, -0.000000000000000000, -0.000000000000000000 ) ) ;
#179668 = ORIENTED_EDGE ( 'NONE', *, *, #80030, .F. ) ;
#179669 = CARTESIAN_POINT ( 'NONE',  ( -16.97048361161166952, 14.05449168777968261, -218.7752056288641427 ) ) ;
#179670 =( BOUNDED_SURFACE ( )  B_SPLINE_SURFACE ( 3, 2, ( 
 ( #85989, #24801, #188979 ),
 ( #63895, #187714, #165578 ),
 ( #48172, #69051, #226812 ),
 ( #183839, #208559, #247666 ) ),
 .UNSPECIFIED., .F., .F., .F. ) 
 B_SPLINE_SURFACE_WITH_KNOTS ( ( 4, 4 ),
 ( 3, 3 ),
 ( 4.712388980384689674, 5.765869716888531116 ),
 ( 0.000000000000000000, 1.000000000000000000 ),
 .UNSPECIFIED. ) 
 GEOMETRIC_REPRESENTATION_ITEM ( )  RATIONAL_B_SPLINE_SURFACE ( (
 ( 1.000000000000000000, 0.7071067811864985009, 1.000000000000000000),
 ( 1.000000000000000000, 0.7953136715912955124, 1.000000000000000000),
 ( 1.000000000000000000, 0.8646876308615905060, 1.000000000000000000),
 ( 1.000000000000000000, 0.8984936768950610997, 1.000000000000000000) ) ) 
 REPRESENTATION_ITEM ( '' )  SURFACE ( )  );
#179671 = CARTESIAN_POINT ( 'NONE',  ( -12.92414019175885720, 49.37151442406710800, -233.5366006881135092 ) ) ;
#179672 = DIRECTION ( 'NONE',  ( -1.000000000000000000, 0.000000000000000000, -0.000000000000000000 ) ) ;
#179673 = EDGE_CURVE ( 'NONE', #64025, #50939, #3684, .T. ) ;
#179674 = DIRECTION ( 'NONE',  ( 0.000000000000000000, -0.4930308989875324399, -0.8700118002898268310 ) ) ;
#179675 = EDGE_LOOP ( 'NONE', ( #176114, #254725, #250288, #148499 ) ) ;
#179676 = FACE_OUTER_BOUND ( 'NONE', #113259, .T. ) ;
#179677 = ORIENTED_EDGE ( 'NONE', *, *, #133235, .T. ) ;
#179678 = EDGE_CURVE ( 'NONE', #52856, #66806, #149461, .T. ) ;
#179679 = CYLINDRICAL_SURFACE ( 'NONE', #88363, 12.87499999999999822 ) ;
#179680 = DIRECTION ( 'NONE',  ( 0.000000000000000000, 0.000000000000000000, -1.000000000000000000 ) ) ;
#179681 = DIRECTION ( 'NONE',  ( 1.000000000000000000, -0.000000000000000000, -0.000000000000000000 ) ) ;
#179682 = FACE_OUTER_BOUND ( 'NONE', #7483, .T. ) ;
#179683 = EDGE_LOOP ( 'NONE', ( #57175, #186614, #74386, #34339 ) ) ;
#179685 = CARTESIAN_POINT ( 'NONE',  ( -18.59999999999999787, -1.249999999988843369, -175.3004807544151049 ) ) ;
#179684 = CIRCLE ( 'NONE', #233843, 7.800000000000000711 ) ;
#179686 = ADVANCED_FACE ( 'NONE', ( #25839 ), #84468, .F. ) ;
#179687 = EDGE_LOOP ( 'NONE', ( #144744, #122364 ) ) ;
#179690 = ORIENTED_EDGE ( 'NONE', *, *, #35431, .F. ) ;
#179689 = CARTESIAN_POINT ( 'NONE',  ( 18.60000000000000142, -9.523946312306552642, -107.3820279953382624 ) ) ;
#179688 = DIRECTION ( 'NONE',  ( 0.000000000000000000, 0.8700118002898322711, -0.4930308989875231696 ) ) ;
#179691 = CIRCLE ( 'NONE', #117322, 0.09999999999998898659 ) ;
#179692 = CARTESIAN_POINT ( 'NONE',  ( -20.64999999999999858, 2.000000000011154189, -147.2246219227621111 ) ) ;
#179693 = VECTOR ( 'NONE', #153978, 1000.000000000000000 ) ;
#179694 = EDGE_CURVE ( 'NONE', #11008, #70163, #207040, .T. ) ;
#179695 = DIRECTION ( 'NONE',  ( 0.000000000000000000, -1.000000000000000000, 0.000000000000000000 ) ) ;
#179696 = ORIENTED_EDGE ( 'NONE', *, *, #112399, .F. ) ;
#179697 = CARTESIAN_POINT ( 'NONE',  ( 18.43630871534878324, 85.67980087481501528, -129.8624754165401498 ) ) ;
#179698 = EDGE_CURVE ( 'NONE', #61007, #8158, #82757, .T. ) ;
#179699 = CARTESIAN_POINT ( 'NONE',  ( -16.93658211146644987, 9.994108662352344297, -54.40429506995567976 ) ) ;
#179700 = ADVANCED_FACE ( 'NONE', ( #45391 ), #184901, .F. ) ;
#179701 = DIRECTION ( 'NONE',  ( -1.000000000000000000, 0.000000000000000000, 0.000000000000000000 ) ) ;
#179703 = ORIENTED_EDGE ( 'NONE', *, *, #169526, .F. ) ;
#179702 = DIRECTION ( 'NONE',  ( -0.000000000000000000, 0.000000000000000000, 1.000000000000000000 ) ) ;
#179704 = CARTESIAN_POINT ( 'NONE',  ( -18.79999999999999716, 2.168342339202985247, -13.59640602015278432 ) ) ;
#179705 = EDGE_CURVE ( 'NONE', #141418, #36387, #61962, .T. ) ;
#179706 = AXIS2_PLACEMENT_3D ( 'NONE', #110619, #94894, #134023 ) ;
#179707 = ORIENTED_EDGE ( 'NONE', *, *, #97100, .T. ) ;
#179708 = CARTESIAN_POINT ( 'NONE',  ( 21.07094088545304444, 61.10557489434067691, -234.2962495489933872 ) ) ;
#179709 = FACE_BOUND ( 'NONE', #247621, .T. ) ;
#179710 = ORIENTED_EDGE ( 'NONE', *, *, #152688, .T. ) ;
#179711 = DIRECTION ( 'NONE',  ( 1.000000000000000000, -0.000000000000000000, -0.000000000000000000 ) ) ;
#179712 = EDGE_LOOP ( 'NONE', ( #47131, #15611, #47528, #115940 ) ) ;
#179713 = CARTESIAN_POINT ( 'NONE',  ( 21.72449340488909897, 10.28395627750227703, -121.3500000000000227 ) ) ;
#179714 = CYLINDRICAL_SURFACE ( 'NONE', #72547, 0.1000000000000024342 ) ;
#179715 = DIRECTION ( 'NONE',  ( 1.000000000000000000, 0.000000000000000000, 0.000000000000000000 ) ) ;
#179716 = ORIENTED_EDGE ( 'NONE', *, *, #185625, .T. ) ;
#179717 = CARTESIAN_POINT ( 'NONE',  ( 21.07888907270776002, 22.96605880254024612, -230.0493642421780862 ) ) ;
#179718 = ADVANCED_FACE ( 'NONE', ( #145760 ), #187493, .F. ) ;
#179719 = DIRECTION ( 'NONE',  ( -1.652117596168391700E-15, 1.000000000000000000, 6.982962677686266711E-15 ) ) ;
#179720 = CIRCLE ( 'NONE', #100569, 0.09999999999998898659 ) ;
#179721 = AXIS2_PLACEMENT_3D ( 'NONE', #93282, #210668, #208125 ) ;
#179722 = DIRECTION ( 'NONE',  ( 0.000000000000000000, 0.000000000000000000, 1.000000000000000000 ) ) ;
#179723 = ORIENTED_EDGE ( 'NONE', *, *, #202432, .T. ) ;
#179724 = AXIS2_PLACEMENT_3D ( 'NONE', #204231, #24341, #23064 ) ;
#179725 = DIRECTION ( 'NONE',  ( 0.000000000000000000, 0.000000000000000000, -1.000000000000000000 ) ) ;
#179726 = CARTESIAN_POINT ( 'NONE',  ( -23.15000000000000213, 7.128833340094563376, -233.7327013124401276 ) ) ;
#179727 = VERTEX_POINT ( 'NONE', #128793 ) ;
#179728 = CARTESIAN_POINT ( 'NONE',  ( 21.05000000000000071, 85.00000000001197975, -112.9170766071766820 ) ) ;
#179729 = ORIENTED_EDGE ( 'NONE', *, *, #246068, .F. ) ;
#179730 = EDGE_CURVE ( 'NONE', #23218, #39881, #182776, .T. ) ;
#179731 = CARTESIAN_POINT ( 'NONE',  ( -20.94999999999999929, 77.36087058720364951, -61.45010955743335046 ) ) ;
#179732 = ORIENTED_EDGE ( 'NONE', *, *, #219423, .F. ) ;
#179734 = ORIENTED_EDGE ( 'NONE', *, *, #75687, .F. ) ;
#179733 = DIRECTION ( 'NONE',  ( 1.000000000000000000, 0.000000000000000000, 0.000000000000000000 ) ) ;
#179735 = VECTOR ( 'NONE', #250127, 1000.000000000000000 ) ;
#179738 = ORIENTED_EDGE ( 'NONE', *, *, #154906, .T. ) ;
#179737 = ORIENTED_EDGE ( 'NONE', *, *, #52830, .F. ) ;
#179736 = DIRECTION ( 'NONE',  ( 1.000000000000000000, 0.000000000000000000, 0.000000000000000000 ) ) ;
#179739 = CARTESIAN_POINT ( 'NONE',  ( 21.05000000000000071, 65.57661458509899433, -95.53105556065429482 ) ) ;
#179740 = CYLINDRICAL_SURFACE ( 'NONE', #202386, 0.09999999999999939493 ) ;
#179741 = DIRECTION ( 'NONE',  ( 0.000000000000000000, 0.000000000000000000, -1.000000000000000000 ) ) ;
#179742 = CARTESIAN_POINT ( 'NONE',  ( -16.93710578446436088, 12.47123518247324725, -211.5055361308018576 ) ) ;
#179744 = EDGE_CURVE ( 'NONE', #103735, #16503, #74475, .T. ) ;
#179743 = DIRECTION ( 'NONE',  ( 1.000000000000000000, 0.000000000000000000, 0.000000000000000000 ) ) ;
#179745 = CARTESIAN_POINT ( 'NONE',  ( 21.05000000000005400, 66.25000000001119815, -5.923107484524795296 ) ) ;
#179746 = EDGE_CURVE ( 'NONE', #253445, #187280, #224267, .T. ) ;
#179747 = CARTESIAN_POINT ( 'NONE',  ( 23.15000000000000213, -8.999999999988842703, -90.60603087734760663 ) ) ;
#179749 = DIRECTION ( 'NONE',  ( 0.000000000000000000, 0.8660254037844377084, 0.5000000000000015543 ) ) ;
#179748 = DIRECTION ( 'NONE',  ( 0.000000000000000000, 1.000000000000000000, 2.891205793294679805E-16 ) ) ;
#179750 = EDGE_LOOP ( 'NONE', ( #52599, #68309, #123601, #120139, #186610 ) ) ;
#179751 = ORIENTED_EDGE ( 'NONE', *, *, #168166, .F. ) ;
#179752 = CARTESIAN_POINT ( 'NONE',  ( -16.94445028196808778, 66.00793639031384430, -56.91577730610593733 ) ) ;
#179754 = ORIENTED_EDGE ( 'NONE', *, *, #29502, .T. ) ;
#179753 = FACE_OUTER_BOUND ( 'NONE', #35825, .T. ) ;
#179755 = DIRECTION ( 'NONE',  ( 0.000000000000000000, -1.000000000000000000, 0.000000000000000000 ) ) ;
#179756 = ORIENTED_EDGE ( 'NONE', *, *, #257013, .T. ) ;
#179758 = DIRECTION ( 'NONE',  ( 1.000000000000000000, 0.000000000000000000, 0.000000000000000000 ) ) ;
#179757 = VECTOR ( 'NONE', #222382, 1000.000000000000000 ) ;
#179759 = EDGE_CURVE ( 'NONE', #143316, #83250, #133904, .T. ) ;
#179760 = ORIENTED_EDGE ( 'NONE', *, *, #216766, .F. ) ;
#179761 = CARTESIAN_POINT ( 'NONE',  ( -20.64999999999999858, 23.68770167995059595, -252.8127582590406348 ) ) ;
#179762 = VECTOR ( 'NONE', #226973, 1000.000000000000000 ) ;
#179763 = ADVANCED_FACE ( 'NONE', ( #71396 ), #230451, .T. ) ;
#179764 = EDGE_CURVE ( 'NONE', #71322, #157401, #93498, .T. ) ;
#179765 = ORIENTED_EDGE ( 'NONE', *, *, #60193, .F. ) ;
#179767 = AXIS2_PLACEMENT_3D ( 'NONE', #202322, #126639, #242723 ) ;
#179766 = CARTESIAN_POINT ( 'NONE',  ( -16.93301857435212199, 66.02369064527634634, -82.13733191336294226 ) ) ;
#179768 = DIRECTION ( 'NONE',  ( -0.000000000000000000, -0.000000000000000000, 1.000000000000000000 ) ) ;
#179770 = ORIENTED_EDGE ( 'NONE', *, *, #177723, .T. ) ;
#179769 = ORIENTED_EDGE ( 'NONE', *, *, #239869, .T. ) ;
#179771 = ORIENTED_EDGE ( 'NONE', *, *, #208854, .T. ) ;
#179773 = CARTESIAN_POINT ( 'NONE',  ( 20.05000000000002913, 68.75000000001186606, -93.77310748452435973 ) ) ;
#179772 = CIRCLE ( 'NONE', #67322, 0.1000000000000043771 ) ;
#179774 = ORIENTED_EDGE ( 'NONE', *, *, #47315, .F. ) ;
#179775 = ORIENTED_EDGE ( 'NONE', *, *, #148849, .T. ) ;
#179776 = ADVANCED_FACE ( 'NONE', ( #209605 ), #178509, .T. ) ;
#179777 = CARTESIAN_POINT ( 'NONE',  ( -23.15000000000000213, -11.48912529306489816, -164.4000000000000057 ) ) ;
#179778 = AXIS2_PLACEMENT_3D ( 'NONE', #81691, #131125, #90710 ) ;
#179780 = ORIENTED_EDGE ( 'NONE', *, *, #157529, .F. ) ;
#179779 = DIRECTION ( 'NONE',  ( -3.265361837132813093E-16, -1.000000000000000000, -7.086529944415894657E-15 ) ) ;
#179782 = CARTESIAN_POINT ( 'NONE',  ( 20.95545211741311320, 65.41358668846837077, -162.4369606249361198 ) ) ;
#179781 = DIRECTION ( 'NONE',  ( 0.000000000000000000, -6.938893903907222067E-15, 1.000000000000000000 ) ) ;
#179783 = DIRECTION ( 'NONE',  ( -0.000000000000000000, -0.3896596508880098009, -0.9209589331071360574 ) ) ;
#179784 = DIRECTION ( 'NONE',  ( -1.000000000000000000, -0.000000000000000000, -0.000000000000000000 ) ) ;
#179785 = CARTESIAN_POINT ( 'NONE',  ( -16.87036670365549540, 9.989418819312804843, -180.0204398826979286 ) ) ;
#179786 = ORIENTED_EDGE ( 'NONE', *, *, #152786, .T. ) ;
#179787 = ORIENTED_EDGE ( 'NONE', *, *, #14254, .F. ) ;
#179788 = DIRECTION ( 'NONE',  ( 0.000000000000000000, -1.687538997430242044E-14, -1.000000000000000000 ) ) ;
#179789 = AXIS2_PLACEMENT_3D ( 'NONE', #159635, #100889, #137476 ) ;
#179790 = CARTESIAN_POINT ( 'NONE',  ( -23.25000000000000000, 76.00000000001126921, -203.5231074845248997 ) ) ;
#179792 = ORIENTED_EDGE ( 'NONE', *, *, #244532, .T. ) ;
#179791 = AXIS2_PLACEMENT_3D ( 'NONE', #60964, #154971, #57096 ) ;
#179793 = DIRECTION ( 'NONE',  ( -1.000000000000000000, 0.000000000000000000, 0.000000000000000000 ) ) ;
#179794 = AXIS2_PLACEMENT_3D ( 'NONE', #184794, #45293, #42720 ) ;
#179795 = FACE_OUTER_BOUND ( 'NONE', #167385, .T. ) ;
#179796 = DIRECTION ( 'NONE',  ( -1.000000000000000000, 0.000000000000000000, 0.000000000000000000 ) ) ;
#179797 = EDGE_LOOP ( 'NONE', ( #10230, #2707, #170647, #100311 ) ) ;
#179798 = EDGE_LOOP ( 'NONE', ( #105664, #211060, #110614, #55908 ) ) ;
#179799 = AXIS2_PLACEMENT_3D ( 'NONE', #137831, #874, #80401 ) ;
#179800 = DIRECTION ( 'NONE',  ( -1.836970198721029934E-16, -0.4088369013363280513, 0.9126074666063769270 ) ) ;
#179801 = CARTESIAN_POINT ( 'NONE',  ( -18.59999999999999787, 66.65000000001198543, -115.1731074845243654 ) ) ;
#179803 = EDGE_LOOP ( 'NONE', ( #78951, #205691, #116974, #57500 ) ) ;
#179802 = EDGE_CURVE ( 'NONE', #60767, #4454, #149651, .T. ) ;
#179804 = LINE ( 'NONE', #257986, #197228 ) ;
#179805 = VERTEX_POINT ( 'NONE', #31001 ) ;
#179806 = EDGE_CURVE ( 'NONE', #145808, #138726, #154789, .T. ) ;
#179807 = DIRECTION ( 'NONE',  ( -1.000000000000000000, -0.000000000000000000, -0.000000000000000000 ) ) ;
#179809 = CIRCLE ( 'NONE', #71483, 0.1000000000000040579 ) ;
#179808 = CARTESIAN_POINT ( 'NONE',  ( 20.04142135623730070, 64.25000000001173817, -81.27310748452440237 ) ) ;
#179811 = CARTESIAN_POINT ( 'NONE',  ( -22.50014994443974103, 55.86946353937208443, -232.8597856945306432 ) ) ;
#179810 = CARTESIAN_POINT ( 'NONE',  ( -16.81744102076749314, 66.05000000001230376, -157.3731074845244393 ) ) ;
#179812 = CARTESIAN_POINT ( 'NONE',  ( 22.40736611211992368, 1.115600667400684642E-11, -55.35042919245524473 ) ) ;
#179813 = DIRECTION ( 'NONE',  ( 0.000000000000000000, 0.000000000000000000, -1.000000000000000000 ) ) ;
#179815 = EDGE_CURVE ( 'NONE', #23611, #12539, #131342, .T. ) ;
#179814 = ORIENTED_EDGE ( 'NONE', *, *, #158202, .T. ) ;
#179816 = FACE_OUTER_BOUND ( 'NONE', #25937, .T. ) ;
#179817 = VECTOR ( 'NONE', #203344, 1000.000000000000000 ) ;
#179818 = VECTOR ( 'NONE', #230890, 1000.000000000000000 ) ;
#179819 = AXIS2_PLACEMENT_3D ( 'NONE', #69934, #206853, #169049 ) ;
#179821 = ORIENTED_EDGE ( 'NONE', *, *, #34479, .F. ) ;
#179820 = ORIENTED_EDGE ( 'NONE', *, *, #19361, .T. ) ;
#179823 = ORIENTED_EDGE ( 'NONE', *, *, #175854, .F. ) ;
#179822 = AXIS2_PLACEMENT_3D ( 'NONE', #26207, #105695, #28812 ) ;
#179824 = DIRECTION ( 'NONE',  ( 0.000000000000000000, -0.9126074666063602736, -0.4088369013363654103 ) ) ;
#179825 = CARTESIAN_POINT ( 'NONE',  ( -18.42554971533679264, -7.781550387048931761, -209.8995886608980470 ) ) ;
#179826 = FACE_OUTER_BOUND ( 'NONE', #50119, .T. ) ;
#179827 = CARTESIAN_POINT ( 'NONE',  ( 18.49999999999999645, -1.164121893230052995, -141.9148480855716343 ) ) ;
#179828 = FACE_OUTER_BOUND ( 'NONE', #36423, .T. ) ;
#179830 = CARTESIAN_POINT ( 'NONE',  ( -13.22483237240078147, 66.56332574816900660, -87.84624555352516495 ) ) ;
#179829 = CARTESIAN_POINT ( 'NONE',  ( 20.97565083910961548, 10.47461740127880958, -7.577943176588548546 ) ) ;
#179831 = EDGE_LOOP ( 'NONE', ( #191742, #100650, #169802, #167618 ) ) ;
#179832 = DIRECTION ( 'NONE',  ( 1.000000000000000000, 0.000000000000000000, 0.000000000000000000 ) ) ;
#179833 = EDGE_LOOP ( 'NONE', ( #223627, #213270, #243923 ) ) ;
#179834 = FACE_OUTER_BOUND ( 'NONE', #214036, .T. ) ;
#179835 = EDGE_LOOP ( 'NONE', ( #183526, #109645, #133542, #29870 ) ) ;
#179836 = ORIENTED_EDGE ( 'NONE', *, *, #47655, .T. ) ;
#179837 = CARTESIAN_POINT ( 'NONE',  ( 21.14999999999999503, 1.115600667400684642E-11, -167.4999999999999716 ) ) ;
#179838 = CARTESIAN_POINT ( 'NONE',  ( 20.94999999999999574, 87.41227409416161720, -100.0231074845242318 ) ) ;
#179839 = CARTESIAN_POINT ( 'NONE',  ( -23.15000000000000213, 87.48912529308749697, -39.12310748452424747 ) ) ;
#179840 = CARTESIAN_POINT ( 'NONE',  ( 13.54556439290363379, 9.450592112144859058, -82.05618831880843800 ) ) ;
#179841 = EDGE_CURVE ( 'NONE', #187769, #85468, #28692, .T. ) ;
#179842 = TOROIDAL_SURFACE ( 'NONE', #88204, 11.89999999999999858, 0.1000000000000000056 ) ;
#179843 = CARTESIAN_POINT ( 'NONE',  ( 20.94999999999999929, 68.01331835486308819, -224.1288211375801609 ) ) ;
#179844 = EDGE_LOOP ( 'NONE', ( #165330, #87626, #34270, #153779 ) ) ;
#179845 = ORIENTED_EDGE ( 'NONE', *, *, #209904, .T. ) ;
#179847 = ADVANCED_FACE ( 'NONE', ( #15270 ), #32965, .T. ) ;
#179846 = DIRECTION ( 'NONE',  ( 1.000000000000000000, 0.000000000000000000, 0.000000000000000000 ) ) ;
#179848 = ORIENTED_EDGE ( 'NONE', *, *, #66108, .T. ) ;
#179849 = DIRECTION ( 'NONE',  ( -1.000000000000000000, 0.000000000000000000, 0.000000000000000000 ) ) ;
#179850 = CARTESIAN_POINT ( 'NONE',  ( -16.94445028196808778, 9.992063609708889516, -46.10733017841845793 ) ) ;
#179851 = LINE ( 'NONE', #256748, #166910 ) ;
#179852 = CARTESIAN_POINT ( 'NONE',  ( -21.14999999999999858, 76.10000000001276987, -215.1726782920691505 ) ) ;
#179853 = CARTESIAN_POINT ( 'NONE',  ( -16.81095280782811230, 66.05000000001187743, -90.37310748452526354 ) ) ;
#179854 = DIRECTION ( 'NONE',  ( 1.000000000000000000, 3.265361837132813093E-16, -0.000000000000000000 ) ) ;
#179855 = ADVANCED_FACE ( 'NONE', ( #11414 ), #150913, .F. ) ;
#179857 = CARTESIAN_POINT ( 'NONE',  ( 22.60000000000000142, 0.000000000000000000, 0.000000000000000000 ) ) ;
#179856 = CARTESIAN_POINT ( 'NONE',  ( -18.58735405345342784, 85.56647862034870400, -129.7003928382583524 ) ) ;
#179858 = DIRECTION ( 'NONE',  ( 0.000000000000000000, 0.2128009952263568427, -0.9770955615653322823 ) ) ;
#179859 = DIRECTION ( 'NONE',  ( -1.000000000000000000, -0.000000000000000000, -0.000000000000000000 ) ) ;
#179861 = ADVANCED_FACE ( 'NONE', ( #90929 ), #171794, .F. ) ;
#179860 = CARTESIAN_POINT ( 'NONE',  ( -21.05000000000000071, 1.115600667400684642E-11, -122.3000000000000398 ) ) ;
#179862 = FACE_OUTER_BOUND ( 'NONE', #124104, .T. ) ;
#179863 = EDGE_CURVE ( 'NONE', #139652, #105004, #20445, .T. ) ;
#179865 = ORIENTED_EDGE ( 'NONE', *, *, #192850, .T. ) ;
#179864 = CIRCLE ( 'NONE', #217416, 0.1000000000000028644 ) ;
#179867 = EDGE_CURVE ( 'NONE', #135153, #41243, #53087, .T. ) ;
#179866 = EDGE_CURVE ( 'NONE', #69624, #60014, #91184, .T. ) ;
#179868 = ORIENTED_EDGE ( 'NONE', *, *, #100280, .F. ) ;
#179869 = CARTESIAN_POINT ( 'NONE',  ( 18.39999999999999858, 85.50000000001209344, -129.4910380878245633 ) ) ;
#179870 = CARTESIAN_POINT ( 'NONE',  ( 21.05000000000000071, 11.60000000001116227, -93.57179676972454274 ) ) ;
#179871 = CARTESIAN_POINT ( 'NONE',  ( -20.54999999999999716, 2.000000000011154189, -187.7753780772378889 ) ) ;
#179872 = ORIENTED_EDGE ( 'NONE', *, *, #26493, .F. ) ;
#179873 = CARTESIAN_POINT ( 'NONE',  ( -18.59999999999999787, 11.65000000001115232, -74.01480577065404987 ) ) ;
#179874 = DIRECTION ( 'NONE',  ( 0.000000000000000000, 1.776356839400306474E-15, 1.000000000000000000 ) ) ;
#179875 = PLANE ( 'NONE',  #100443 ) ;
#179876 = CIRCLE ( 'NONE', #246494, 11.65000000000000036 ) ;
#179877 = CIRCLE ( 'NONE', #67426, 0.6000000000000033085 ) ;
#179878 = EDGE_CURVE ( 'NONE', #239900, #242842, #253656, .T. ) ;
#179879 = DIRECTION ( 'NONE',  ( 0.000000000000000000, 0.000000000000000000, -1.000000000000000000 ) ) ;
#179880 = EDGE_CURVE ( 'NONE', #121418, #194615, #132889, .T. ) ;
#179881 = CARTESIAN_POINT ( 'NONE',  ( 23.14999999999999858, 1.115600667400684642E-11, -134.0000000000000284 ) ) ;
#179883 = DIRECTION ( 'NONE',  ( 1.000000000000000000, 0.000000000000000000, 0.000000000000000000 ) ) ;
#179882 = AXIS2_PLACEMENT_3D ( 'NONE', #195988, #96831, #223219 ) ;
#179884 = EDGE_LOOP ( 'NONE', ( #147087, #154786, #182956, #76912, #25920 ) ) ;
#179885 = CARTESIAN_POINT ( 'NONE',  ( 18.50000000000000000, -9.399999999988843058, -174.7972597596632625 ) ) ;
#179887 = EDGE_LOOP ( 'NONE', ( #174981, #7337, #149921, #116951 ) ) ;
#179886 = DIRECTION ( 'NONE',  ( 0.000000000000000000, 0.2617529984165031243, 0.9651348961777157509 ) ) ;
#179888 = DIRECTION ( 'NONE',  ( 0.000000000000000000, 3.552713678800413366E-15, -1.000000000000000000 ) ) ;
#179889 = EDGE_CURVE ( 'NONE', #110818, #54944, #257715, .T. ) ;
#179890 = DIRECTION ( 'NONE',  ( 0.000000000000000000, -7.086529944415894657E-15, 1.000000000000000000 ) ) ;
#179891 = DIRECTION ( 'NONE',  ( 0.000000000000000000, 0.000000000000000000, -1.000000000000000000 ) ) ;
#179892 = EDGE_LOOP ( 'NONE', ( #58266, #96434, #234561, #36598 ) ) ;
#179893 = CARTESIAN_POINT ( 'NONE',  ( -22.49756042579671700, 75.92195366299505110, -148.1729724456266410 ) ) ;
#179894 = APPLICATION_PROTOCOL_DEFINITION ( 'draft international standard', 'automotive_design', 1998, #114050 ) ;
#179895 = ADVANCED_FACE ( 'NONE', ( #93173 ), #28873, .T. ) ;
#179896 = CYLINDRICAL_SURFACE ( 'NONE', #117266, 0.09999999999999939493 ) ;
#179897 = CIRCLE ( 'NONE', #34344, 0.09999999999999939493 ) ;
#179898 = EDGE_LOOP ( 'NONE', ( #8149, #130632, #69721, #113752, #231346, #207041, #226699 ) ) ;
#179899 = CARTESIAN_POINT ( 'NONE',  ( -23.25000000000000000, 11.75000000001115552, -100.5000000000000426 ) ) ;
#179900 = CARTESIAN_POINT ( 'NONE',  ( 16.87683809663749557, 66.05000000001183480, -82.17310748452439384 ) ) ;
#179901 = EDGE_CURVE ( 'NONE', #45529, #71933, #116324, .T. ) ;
#179902 = CYLINDRICAL_SURFACE ( 'NONE', #216120, 0.09999999999999939493 ) ;
#179903 = ORIENTED_EDGE ( 'NONE', *, *, #149185, .T. ) ;
#179904 = VERTEX_POINT ( 'NONE', #34516 ) ;
#179905 = ADVANCED_FACE ( 'NONE', ( #192292 ), #210565, .F. ) ;
#179906 = CARTESIAN_POINT ( 'NONE',  ( -20.54999999999999716, 73.60000000001224407, -149.7477294072864709 ) ) ;
#179907 = CARTESIAN_POINT ( 'NONE',  ( -21.55000000000000426, 7.750000000011155521, -79.35000000000005116 ) ) ;
#179908 = DIRECTION ( 'NONE',  ( 0.000000000000000000, 0.000000000000000000, -1.000000000000000000 ) ) ;
#179909 = PLANE ( 'NONE',  #23769 ) ;
#179911 = LINE ( 'NONE', #157810, #161969 ) ;
#179910 = VECTOR ( 'NONE', #230656, 1000.000000000000000 ) ;
#179912 = AXIS2_PLACEMENT_3D ( 'NONE', #76279, #157138, #217064 ) ;
#179913 = DIRECTION ( 'NONE',  ( 0.000000000000000000, -7.172728831056617961E-15, 1.000000000000000000 ) ) ;
#179916 = CARTESIAN_POINT ( 'NONE',  ( 20.94999999999999574, 1.249999999999999334, -7.900000000000000355 ) ) ;
#179915 = AXIS2_PLACEMENT_3D ( 'NONE', #54142, #213210, #157129 ) ;
#179914 = DIRECTION ( 'NONE',  ( 0.000000000000000000, 0.9770955615653323934, 0.2128009952263564264 ) ) ;
#179917 = EDGE_CURVE ( 'NONE', #45940, #195803, #149644, .T. ) ;
#179918 = DIRECTION ( 'NONE',  ( -1.000000000000000000, 0.000000000000000000, 0.000000000000000000 ) ) ;
#179919 = DIRECTION ( 'NONE',  ( 0.000000000000000000, 0.8814952561688430555, -0.4721928772777346239 ) ) ;
#179920 = CARTESIAN_POINT ( 'NONE',  ( 21.05000000000000071, 0.000000000000000000, -33.50000000000000000 ) ) ;
#179921 = CARTESIAN_POINT ( 'NONE',  ( -18.50000000000000355, -1.263275465206102233, -108.4018646667464481 ) ) ;
#179922 = ORIENTED_EDGE ( 'NONE', *, *, #116193, .F. ) ;
#179923 = VERTEX_POINT ( 'NONE', #71071 ) ;
#179924 = DIRECTION ( 'NONE',  ( 1.000000000000000000, 0.000000000000000000, 0.000000000000000000 ) ) ;
#179926 = DIRECTION ( 'NONE',  ( 0.000000000000000000, 0.000000000000000000, 1.000000000000000000 ) ) ;
#179925 = DIRECTION ( 'NONE',  ( 2.952720810173289112E-16, -1.000000000000000000, 0.000000000000000000 ) ) ;
#179927 = DIRECTION ( 'NONE',  ( 1.000000000000000000, 7.304098846218134667E-16, 0.000000000000000000 ) ) ;
#179928 = CARTESIAN_POINT ( 'NONE',  ( -21.06715728752538652, 12.97363049771892207, -205.3537238898406656 ) ) ;
#179929 = EDGE_CURVE ( 'NONE', #201029, #120342, #178708, .T. ) ;
#179930 = CARTESIAN_POINT ( 'NONE',  ( 13.99999999999999822, 26.54497872210689735, -232.9592037335782209 ) ) ;
#179931 = ORIENTED_EDGE ( 'NONE', *, *, #218081, .F. ) ;
#179932 = DIRECTION ( 'NONE',  ( 1.000000000000000000, -0.000000000000000000, -0.000000000000000000 ) ) ;
#179933 = EDGE_LOOP ( 'NONE', ( #152588, #162406, #78692, #28984 ) ) ;
#179934 = CARTESIAN_POINT ( 'NONE',  ( -16.94107738177414291, 51.68386028857255354, -231.8469600742508305 ) ) ;
#179935 = ORIENTED_EDGE ( 'NONE', *, *, #101725, .T. ) ;
#179936 = FACE_OUTER_BOUND ( 'NONE', #195849, .T. ) ;
#179937 = CARTESIAN_POINT ( 'NONE',  ( 18.31325810956384359, 85.53638847601837369, -29.15466727821959836 ) ) ;
#179938 = EDGE_LOOP ( 'NONE', ( #36422, #96787, #246247, #127268, #9293, #149512, #174722 ) ) ;
#179939 = CARTESIAN_POINT ( 'NONE',  ( -23.15000000000000213, 28.37802281961254636, -258.4449340416662722 ) ) ;
#179940 = AXIS2_PLACEMENT_3D ( 'NONE', #238434, #119794, #100173 ) ;
#179941 = ORIENTED_EDGE ( 'NONE', *, *, #256061, .F. ) ;
#179942 = CARTESIAN_POINT ( 'NONE',  ( 23.14999999999999858, 76.00000000001213607, -136.5231074845243313 ) ) ;
#179943 = DIRECTION ( 'NONE',  ( 1.000000000000000000, -0.000000000000000000, 0.000000000000000000 ) ) ;
#179945 = CIRCLE ( 'NONE', #34220, 0.1000000000000028644 ) ;
#179944 = DIRECTION ( 'NONE',  ( 1.000000000000000000, 0.000000000000000000, 0.000000000000000000 ) ) ;
#179946 = CYLINDRICAL_SURFACE ( 'NONE', #83350, 0.09999999999999781286 ) ;
#179947 = DIRECTION ( 'NONE',  ( -1.000000000000000000, 0.000000000000000000, 0.000000000000000000 ) ) ;
#179949 = FACE_OUTER_BOUND ( 'NONE', #32184, .T. ) ;
#179948 = FACE_OUTER_BOUND ( 'NONE', #92208, .T. ) ;
#179951 = CYLINDRICAL_SURFACE ( 'NONE', #215537, 0.09999999999999560629 ) ;
#179950 = AXIS2_PLACEMENT_3D ( 'NONE', #41681, #40417, #56065 ) ;
#179952 = CIRCLE ( 'NONE', #155026, 0.09999999999999635569 ) ;
#179954 = ORIENTED_EDGE ( 'NONE', *, *, #154474, .T. ) ;
#179953 = CARTESIAN_POINT ( 'NONE',  ( 21.05000000000000071, 65.27628289530507288, -191.3619171903970084 ) ) ;
#179956 = LINE ( 'NONE', #56120, #151639 ) ;
#179955 = CARTESIAN_POINT ( 'NONE',  ( 21.15000000000005187, 76.00000000001119815, -31.87310748452479459 ) ) ;
#179957 = ORIENTED_EDGE ( 'NONE', *, *, #75939, .T. ) ;
#179959 = ORIENTED_EDGE ( 'NONE', *, *, #248590, .F. ) ;
#179958 = CARTESIAN_POINT ( 'NONE',  ( -23.15000000000000213, 19.80622355348251418, -246.0044611956074618 ) ) ;
#179960 = ORIENTED_EDGE ( 'NONE', *, *, #43630, .F. ) ;
#179961 = DIRECTION ( 'NONE',  ( -3.265361837132813093E-16, -1.000000000000000000, -6.982962677686266711E-15 ) ) ;
#179962 = CIRCLE ( 'NONE', #146598, 12.87500000000000711 ) ;
#179963 = DIRECTION ( 'NONE',  ( 0.000000000000000000, -1.000000000000000000, 0.000000000000000000 ) ) ;
#179964 = CYLINDRICAL_SURFACE ( 'NONE', #239060, 0.09999999999998898659 ) ;
#179965 = ORIENTED_EDGE ( 'NONE', *, *, #78665, .F. ) ;
#179966 = CARTESIAN_POINT ( 'NONE',  ( -20.85000000000000142, 76.00000000001170974, -69.52310748452431710 ) ) ;
#179967 = CARTESIAN_POINT ( 'NONE',  ( 22.50000000000000000, 1.115600667400684642E-11, -134.0000000000000000 ) ) ;
#179968 = CARTESIAN_POINT ( 'NONE',  ( 20.94999999999999929, 76.00000000001213607, -136.5231074845243313 ) ) ;
#179969 = FACE_OUTER_BOUND ( 'NONE', #125119, .T. ) ;
#179970 = AXIS2_PLACEMENT_3D ( 'NONE', #107975, #164102, #6286 ) ;
#179971 = CARTESIAN_POINT ( 'NONE',  ( -18.55121869061588669, 46.45193731540634019, -243.0811559066744110 ) ) ;
#179972 = AXIS2_PLACEMENT_3D ( 'NONE', #35260, #133053, #70531 ) ;
#179973 = ADVANCED_FACE ( 'NONE', ( #129737 ), #193572, .T. ) ;
#179974 = CARTESIAN_POINT ( 'NONE',  ( 21.08035267497491105, 69.66829316022912622, -136.6057961093004849 ) ) ;
#179975 = AXIS2_PLACEMENT_3D ( 'NONE', #88209, #132506, #187357 ) ;
#179976 = ORIENTED_EDGE ( 'NONE', *, *, #198164, .F. ) ;
#179977 = EDGE_LOOP ( 'NONE', ( #200775, #45423, #113329 ) ) ;
#179978 = DIRECTION ( 'NONE',  ( -0.000000000000000000, 0.8660254037844411501, 0.4999999999999956701 ) ) ;
#179979 = AXIS2_PLACEMENT_3D ( 'NONE', #123387, #244601, #19481 ) ;
#179980 = ORIENTED_EDGE ( 'NONE', *, *, #41723, .T. ) ;
#179981 = FACE_OUTER_BOUND ( 'NONE', #251849, .T. ) ;
#179982 = EDGE_LOOP ( 'NONE', ( #83214, #166963, #155387, #186055 ) ) ;
#179983 = CARTESIAN_POINT ( 'NONE',  ( 23.14999999999999858, 1.115600667400684642E-11, -79.87500000000004263 ) ) ;
#179984 = CIRCLE ( 'NONE', #5149, 0.09999999999998898659 ) ;
#179985 = CARTESIAN_POINT ( 'NONE',  ( 20.94999999999999929, 1.115600667400684642E-11, -100.5000000000000426 ) ) ;
#179986 = DIRECTION ( 'NONE',  ( 4.377807931758639578E-15, -0.9876013379310922824, -0.1569827930593562515 ) ) ;
#179987 = AXIS2_PLACEMENT_3D ( 'NONE', #102211, #239193, #145215 ) ;
#179988 = CARTESIAN_POINT ( 'NONE',  ( -20.94999999999994600, 65.19115966511134275, -30.12310748452479103 ) ) ;
#179989 = DIRECTION ( 'NONE',  ( 0.000000000000000000, 0.9651348961777157509, -0.2617529984165031243 ) ) ;
#179990 = EDGE_CURVE ( 'NONE', #30528, #70015, #12097, .T. ) ;
#179991 = EDGE_CURVE ( 'NONE', #122858, #60637, #69787, .T. ) ;
#179992 = DIRECTION ( 'NONE',  ( 0.000000000000000000, 0.2617529984165031243, 0.9651348961777157509 ) ) ;
#179993 = CARTESIAN_POINT ( 'NONE',  ( -20.85000000000000142, 64.25000000001215028, -136.5231074845244166 ) ) ;
#179994 = DIRECTION ( 'NONE',  ( -1.000000000000000000, 2.849773892568378313E-16, -7.728835255496647986E-17 ) ) ;
#179995 = VERTEX_POINT ( 'NONE', #227550 ) ;
#179997 = CARTESIAN_POINT ( 'NONE',  ( 22.49436431346199683, 64.35004905235869899, -136.5900110142466417 ) ) ;
#179996 = FACE_OUTER_BOUND ( 'NONE', #133249, .T. ) ;
#179998 = CIRCLE ( 'NONE', #242332, 12.87499999999999822 ) ;
#179999 = EDGE_LOOP ( 'NONE', ( #13223, #63747, #19181, #243693 ) ) ;
#180003 = VERTEX_POINT ( 'NONE', #150594 ) ;
#180002 = FACE_OUTER_BOUND ( 'NONE', #52283, .T. ) ;
#180001 =( BOUNDED_CURVE ( )  B_SPLINE_CURVE ( 3, ( #123521, #84332, #58378, #197910 ),
 .UNSPECIFIED., .F., .T. ) 
 B_SPLINE_CURVE_WITH_KNOTS ( ( 4, 4 ),
 ( 3.192897208853993085, 4.712388980384689674 ),
 .UNSPECIFIED. ) 
 CURVE ( )  GEOMETRIC_REPRESENTATION_ITEM ( )  RATIONAL_B_SPLINE_CURVE ( ( 1.000000000000000000, 0.8166740347213228279, 0.8166740347213228279, 1.000000000000000000 ) ) 
 REPRESENTATION_ITEM ( '' )  );
#180000 = DIRECTION ( 'NONE',  ( 1.000000000000000000, 0.000000000000000000, 0.000000000000000000 ) ) ;
#180004 = CIRCLE ( 'NONE', #4981, 0.1000000000000002554 ) ;
#180005 = ORIENTED_EDGE ( 'NONE', *, *, #136879, .F. ) ;
#180006 = CARTESIAN_POINT ( 'NONE',  ( -18.59999999999999787, -1.164121893230052995, -141.9148480855716343 ) ) ;
#180007 = CIRCLE ( 'NONE', #96574, 0.1000000000000067224 ) ;
#180008 = CARTESIAN_POINT ( 'NONE',  ( 11.60000000000000320, -11.65000000000000036, 12.30000000000000426 ) ) ;
#180009 = ADVANCED_FACE ( 'NONE', ( #13646 ), #14944, .T. ) ;
#180010 = DIRECTION ( 'NONE',  ( 1.000000000000000000, 1.836970198721029934E-16, -0.000000000000000000 ) ) ;
#180011 = ORIENTED_EDGE ( 'NONE', *, *, #16963, .T. ) ;
#180012 = FACE_OUTER_BOUND ( 'NONE', #88681, .T. ) ;
#180013 = ADVANCED_FACE ( 'NONE', ( #132300 ), #87055, .F. ) ;
#180014 = DIRECTION ( 'NONE',  ( -1.000000000000000000, -0.000000000000000000, 0.000000000000000000 ) ) ;
#180015 = ADVANCED_FACE ( 'NONE', ( #114015 ), #90595, .F. ) ;
#180017 = DIRECTION ( 'NONE',  ( 1.000000000000000000, -0.000000000000000000, -0.000000000000000000 ) ) ;
#180016 = CARTESIAN_POINT ( 'NONE',  ( -22.16821283564876666, 7.558973340791935058, -167.4999999999999716 ) ) ;
#180019 = ORIENTED_EDGE ( 'NONE', *, *, #70596, .T. ) ;
#180018 = CARTESIAN_POINT ( 'NONE',  ( 22.88900146558018989, 67.29609520889925989, -127.2731074845243597 ) ) ;
#180020 = ADVANCED_FACE ( 'NONE', ( #188422 ), #230120, .T. ) ;
#180021 = ORIENTED_EDGE ( 'NONE', *, *, #67663, .F. ) ;
#180022 = TOROIDAL_SURFACE ( 'NONE', #42626, 3.899999999999999467, 0.1000000000000000056 ) ;
#180023 = DIRECTION ( 'NONE',  ( -0.7071067811865474617, -0.7071067811865474617, -0.000000000000000000 ) ) ;
#180024 = ORIENTED_EDGE ( 'NONE', *, *, #253272, .T. ) ;
#180025 = DIRECTION ( 'NONE',  ( -1.000000000000000000, 0.000000000000000000, 0.000000000000000000 ) ) ;
#180026 = EDGE_CURVE ( 'NONE', #221652, #147354, #120443, .T. ) ;
#180027 = ORIENTED_EDGE ( 'NONE', *, *, #161371, .F. ) ;
#180028 = CARTESIAN_POINT ( 'NONE',  ( 21.00000000000000000, 9.750000000011153745, -112.8500000000000369 ) ) ;
#180029 = CARTESIAN_POINT ( 'NONE',  ( 22.40000000000010516, 76.00000000001297451, -114.6726782920694205 ) ) ;
#180030 = CARTESIAN_POINT ( 'NONE',  ( 20.73486653747090003, 68.75000000001149658, -48.67310748452437963 ) ) ;
#180031 = EDGE_LOOP ( 'NONE', ( #17901, #244402 ) ) ;
#180032 = LINE ( 'NONE', #138296, #250199 ) ;
#180033 = EDGE_CURVE ( 'NONE', #123853, #139130, #80002, .T. ) ;
#180034 = CARTESIAN_POINT ( 'NONE',  ( -21.05000000000000071, 11.65000000001115232, -73.78386566297820082 ) ) ;
#180036 = VERTEX_POINT ( 'NONE', #120482 ) ;
#180035 = AXIS2_PLACEMENT_3D ( 'NONE', #191137, #252350, #128572 ) ;
#180037 = ORIENTED_EDGE ( 'NONE', *, *, #224787, .F. ) ;
#180038 = VERTEX_POINT ( 'NONE', #39659 ) ;
#180039 = DIRECTION ( 'NONE',  ( 0.000000000000000000, 0.000000000000000000, 1.000000000000000000 ) ) ;
#180040 = ORIENTED_EDGE ( 'NONE', *, *, #118738, .F. ) ;
#180042 = ORIENTED_EDGE ( 'NONE', *, *, #114312, .T. ) ;
#180041 = CARTESIAN_POINT ( 'NONE',  ( 15.51872946208853143, 66.62341902196861554, -185.8961612375124446 ) ) ;
#180043 = ORIENTED_EDGE ( 'NONE', *, *, #212912, .F. ) ;
#180046 = VERTEX_POINT ( 'NONE', #60457 ) ;
#180045 = ORIENTED_EDGE ( 'NONE', *, *, #1111, .T. ) ;
#180044 = CARTESIAN_POINT ( 'NONE',  ( 18.60000000000000142, 78.12133356376091342, -231.3112718935514636 ) ) ;
#180047 = CIRCLE ( 'NONE', #121790, 0.09999999999999363565 ) ;
#180048 = ORIENTED_EDGE ( 'NONE', *, *, #127301, .F. ) ;
#180049 = FACE_OUTER_BOUND ( 'NONE', #255577, .T. ) ;
#180050 = CARTESIAN_POINT ( 'NONE',  ( 18.59999999999999076, 77.83585931145526615, -58.01866831572577610 ) ) ;
#180051 = VECTOR ( 'NONE', #113556, 999.9999999999998863 ) ;
#180052 = ADVANCED_FACE ( 'NONE', ( #78733 ), #235251, .F. ) ;
#180053 = FACE_OUTER_BOUND ( 'NONE', #88263, .T. ) ;
#180054 = EDGE_CURVE ( 'NONE', #19886, #216520, #154478, .T. ) ;
#180055 = EDGE_LOOP ( 'NONE', ( #185845, #87218, #200588, #175315 ) ) ;
#180056 = FACE_OUTER_BOUND ( 'NONE', #208890, .T. ) ;
#180058 = VERTEX_POINT ( 'NONE', #219533 ) ;
#180057 = DIRECTION ( 'NONE',  ( 0.000000000000000000, -0.9651348961777028723, 0.2617529984165503087 ) ) ;
#180059 = DIRECTION ( 'NONE',  ( -0.000000000000000000, -0.000000000000000000, -1.000000000000000000 ) ) ;
#180061 = ORIENTED_EDGE ( 'NONE', *, *, #32043, .T. ) ;
#180060 = CARTESIAN_POINT ( 'NONE',  ( 20.94999999999999574, 69.65000000001262492, -193.6792853948412869 ) ) ;
#180062 = EDGE_CURVE ( 'NONE', #102074, #161516, #20470, .T. ) ;
#180063 = EDGE_CURVE ( 'NONE', #91092, #151216, #45384, .T. ) ;
#180064 = ORIENTED_EDGE ( 'NONE', *, *, #5201, .F. ) ;
#180065 = CARTESIAN_POINT ( 'NONE',  ( -21.05000000000000071, 62.00000000001249134, -175.4502000149069261 ) ) ;
#180066 = SURFACE_SIDE_STYLE ('',( #60093 ) ) ;
#180067 = AXIS2_PLACEMENT_3D ( 'NONE', #116885, #39943, #59435 ) ;
#180068 = EDGE_CURVE ( 'NONE', #196564, #159137, #103809, .T. ) ;
#180069 = CIRCLE ( 'NONE', #121814, 0.1000000000000000472 ) ;
#180070 = ORIENTED_EDGE ( 'NONE', *, *, #226546, .T. ) ;
#180071 = ORIENTED_EDGE ( 'NONE', *, *, #211019, .T. ) ;
#180073 = ADVANCED_FACE ( 'NONE', ( #233969 ), #55419, .T. ) ;
#180072 = CARTESIAN_POINT ( 'NONE',  ( -18.69999999999999929, 1.350000000000000089, 21.90000000000000213 ) ) ;
#180074 = ADVANCED_FACE ( 'NONE', ( #99569 ), #10537, .T. ) ;
#180076 = ORIENTED_EDGE ( 'NONE', *, *, #28311, .T. ) ;
#180075 = ORIENTED_EDGE ( 'NONE', *, *, #189999, .F. ) ;
#180077 = EDGE_LOOP ( 'NONE', ( #208894, #236057, #96940, #251039 ) ) ;
#180078 = CARTESIAN_POINT ( 'NONE',  ( 21.14999999999999858, 61.95748721176698126, -221.7323031544521541 ) ) ;
#180079 = ORIENTED_EDGE ( 'NONE', *, *, #1029, .F. ) ;
#180080 = ORIENTED_EDGE ( 'NONE', *, *, #227660, .F. ) ;
#180081 = B_SPLINE_CURVE_WITH_KNOTS ( 'NONE', 3,
 ( #196087, #156978, #17437, #197354, #96939, #158279, #237774, #179120, #222030, #182953 ),
 .UNSPECIFIED., .F., .F.,
 ( 4, 3, 3, 4 ),
 ( 1.891637802867244836E-15, 3.877043166999269576E-05, 7.336897548475566824E-05, 7.659383120239756379E-05 ),
 .UNSPECIFIED. ) ;
#180082 = EDGE_CURVE ( 'NONE', #22794, #7849, #241228, .T. ) ;
#180084 = CARTESIAN_POINT ( 'NONE',  ( 21.05000000000000071, 3.047642603966940200, -208.5984958277594785 ) ) ;
#180083 = AXIS2_PLACEMENT_3D ( 'NONE', #192813, #174583, #169432 ) ;
#180085 = ORIENTED_EDGE ( 'NONE', *, *, #54126, .F. ) ;
#180086 = CARTESIAN_POINT ( 'NONE',  ( 23.15000000000000213, 87.48912529308749697, -39.12310748452424747 ) ) ;
#180088 = CARTESIAN_POINT ( 'NONE',  ( 23.14999999999999503, 11.65000000001116298, -160.4851942293460922 ) ) ;
#180087 = CARTESIAN_POINT ( 'NONE',  ( 18.59999999999999432, 77.13501884592227498, -128.8061306010920362 ) ) ;
#180089 = ORIENTED_EDGE ( 'NONE', *, *, #237248, .T. ) ;
#180090 = EDGE_CURVE ( 'NONE', #258053, #88402, #78925, .T. ) ;
#180091 = AXIS2_PLACEMENT_3D ( 'NONE', #122252, #124823, #201772 ) ;
#180092 = AXIS2_PLACEMENT_3D ( 'NONE', #132120, #228669, #211669 ) ;
#180094 = ORIENTED_EDGE ( 'NONE', *, *, #246258, .F. ) ;
#180093 = EDGE_LOOP ( 'NONE', ( #1019, #231340, #150133, #168930 ) ) ;
#180095 = AXIS2_PLACEMENT_3D ( 'NONE', #37718, #178514, #134209 ) ;
#180096 = CYLINDRICAL_SURFACE ( 'NONE', #236018, 0.09999999999998898659 ) ;
#180097 = CARTESIAN_POINT ( 'NONE',  ( 21.05000000000000071, 87.48912529308822172, -139.5231074845243029 ) ) ;
#180098 = EDGE_CURVE ( 'NONE', #63775, #48019, #136970, .T. ) ;
#180099 = VERTEX_POINT ( 'NONE', #43487 ) ;
#180100 = EDGE_CURVE ( 'NONE', #18030, #68437, #61758, .T. ) ;
#180101 = DIRECTION ( 'NONE',  ( 0.000000000000000000, 0.000000000000000000, -1.000000000000000000 ) ) ;
#180102 = EDGE_LOOP ( 'NONE', ( #138102, #249586, #21946 ) ) ;
#180103 = ORIENTED_EDGE ( 'NONE', *, *, #242615, .F. ) ;
#180104 = CYLINDRICAL_SURFACE ( 'NONE', #37862, 1.749999999999998002 ) ;
#180106 = EDGE_CURVE ( 'NONE', #232077, #125708, #27806, .T. ) ;
#180105 = ORIENTED_EDGE ( 'NONE', *, *, #244028, .T. ) ;
#180107 = DIRECTION ( 'NONE',  ( 1.000000000000000000, 0.000000000000000000, -0.000000000000000000 ) ) ;
#180108 = CYLINDRICAL_SURFACE ( 'NONE', #26982, 0.1000000000000028644 ) ;
#180109 = ORIENTED_EDGE ( 'NONE', *, *, #155728, .T. ) ;
#180110 = EDGE_CURVE ( 'NONE', #209328, #255664, #249592, .T. ) ;
#180111 = FACE_OUTER_BOUND ( 'NONE', #139286, .T. ) ;
#180112 = CARTESIAN_POINT ( 'NONE',  ( -17.27223548803219444, 10.34539739140581815, -44.86639382081585836 ) ) ;
#180113 = DIRECTION ( 'NONE',  ( 0.000000000000000000, 0.9126074666063770380, 0.4088369013363281068 ) ) ;
#180114 = DIRECTION ( 'NONE',  ( 3.265361837132812600E-16, -0.4721928772777346239, -0.8814952561688430555 ) ) ;
#180115 = CARTESIAN_POINT ( 'NONE',  ( 18.59999999999999076, 6.650000000011155876, -188.6499999999999488 ) ) ;
#180116 = CARTESIAN_POINT ( 'NONE',  ( -23.15000000000000213, 87.65000000001246860, -173.0231074845243029 ) ) ;
#180117 = CARTESIAN_POINT ( 'NONE',  ( 22.39999999999999503, 76.00000000001243450, -177.8138870828977360 ) ) ;
#180118 = DIRECTION ( 'NONE',  ( 1.000000000000000000, 0.000000000000000000, 0.000000000000000000 ) ) ;
#180119 = DIRECTION ( 'NONE',  ( 0.000000000000000000, 0.000000000000000000, -1.000000000000000000 ) ) ;
#180120 = VECTOR ( 'NONE', #59443, 1000.000000000000000 ) ;
#180121 = ORIENTED_EDGE ( 'NONE', *, *, #179176, .T. ) ;
#180122 = CIRCLE ( 'NONE', #176037, 0.09999999999999939493 ) ;
#180124 = ORIENTED_EDGE ( 'NONE', *, *, #136095, .F. ) ;
#180123 = ORIENTED_EDGE ( 'NONE', *, *, #257779, .T. ) ;
#180125 = ORIENTED_EDGE ( 'NONE', *, *, #189917, .F. ) ;
#180126 = ORIENTED_EDGE ( 'NONE', *, *, #155723, .F. ) ;
#180127 = CARTESIAN_POINT ( 'NONE',  ( -17.04761207306820125, 10.02645087340892971, -79.65000000000004832 ) ) ;
#180128 = AXIS2_PLACEMENT_3D ( 'NONE', #147996, #166307, #85406 ) ;
#180129 = DIRECTION ( 'NONE',  ( 0.000000000000000000, -0.1455152366551522025, -0.9893560106964505163 ) ) ;
#180131 = CARTESIAN_POINT ( 'NONE',  ( -23.25000000000000000, 76.00000000001267608, -203.5231074845243597 ) ) ;
#180130 = CARTESIAN_POINT ( 'NONE',  ( 21.05000000000000071, -3.363022478626109368, -226.2703567425896267 ) ) ;
#180132 = DIRECTION ( 'NONE',  ( 1.000000000000000000, -0.000000000000000000, -0.000000000000000000 ) ) ;
#180133 = EDGE_LOOP ( 'NONE', ( #34441, #58816, #44154, #217677 ) ) ;
#180134 = VECTOR ( 'NONE', #174447, 1000.000000000000000 ) ;
#180135 = CARTESIAN_POINT ( 'NONE',  ( 23.15000000000000213, 87.39257802171783851, -139.5970570643562212 ) ) ;
#180136 = SURFACE_STYLE_FILL_AREA ( #60158 ) ;
#180137 = CYLINDRICAL_SURFACE ( 'NONE', #75282, 2.000000000000001776 ) ;
#180138 = AXIS2_PLACEMENT_3D ( 'NONE', #257883, #256597, #98824 ) ;
#180139 = DIRECTION ( 'NONE',  ( -1.000000000000000000, -0.000000000000000000, -0.000000000000000000 ) ) ;
#180140 = CIRCLE ( 'NONE', #67692, 0.09999999999998898659 ) ;
#180141 = CARTESIAN_POINT ( 'NONE',  ( -16.94333152882355975, 9.990342011468824168, -87.89203153110153721 ) ) ;
#180142 = VERTEX_POINT ( 'NONE', #47308 ) ;
#180143 = AXIS2_PLACEMENT_3D ( 'NONE', #195950, #117673, #38157 ) ;
#180144 = DIRECTION ( 'NONE',  ( 0.000000000000000000, -0.9126074666063773710, -0.4088369013363271631 ) ) ;
#180145 = AXIS2_PLACEMENT_3D ( 'NONE', #160440, #18327, #239957 ) ;
#180146 = CARTESIAN_POINT ( 'NONE',  ( -21.04999999999999716, -0.01465611850212083199, -94.00331341423238030 ) ) ;
#180147 = EDGE_LOOP ( 'NONE', ( #74240, #136314, #184173, #219057, #250071 ) ) ;
#180148 = DIRECTION ( 'NONE',  ( 1.000000000000000000, 0.000000000000000000, 0.000000000000000000 ) ) ;
#180149 = DIRECTION ( 'NONE',  ( 0.000000000000000000, -7.086529944415894657E-15, 1.000000000000000000 ) ) ;
#180150 = CARTESIAN_POINT ( 'NONE',  ( -20.54999999999999716, 76.49733069700262433, -201.6893511817872309 ) ) ;
#180151 = DIRECTION ( 'NONE',  ( 0.000000000000000000, -0.000000000000000000, 1.000000000000000000 ) ) ;
#180152 = VECTOR ( 'NONE', #120838, 1000.000000000000000 ) ;
#180153 = ORIENTED_EDGE ( 'NONE', *, *, #176478, .F. ) ;
#180154 = DIRECTION ( 'NONE',  ( -0.000000000000000000, 1.000000000000000000, 6.982962677686266711E-15 ) ) ;
#180155 = DIRECTION ( 'NONE',  ( -1.652117596168391700E-15, 1.000000000000000000, 6.982962677686266711E-15 ) ) ;
#180156 = CARTESIAN_POINT ( 'NONE',  ( 22.47071067811865319, 0.3704148268517115650, -229.9999874772931037 ) ) ;
#180157 = TOROIDAL_SURFACE ( 'NONE', #5135, 11.70000000000000107, 0.1000000000000000056 ) ;
#180158 = ADVANCED_FACE ( 'NONE', ( #166024 ), #121754, .F. ) ;
#180160 = FACE_OUTER_BOUND ( 'NONE', #61800, .T. ) ;
#180159 = DIRECTION ( 'NONE',  ( -0.7071067811865475727, 0.7071067811865475727, 4.937700262164531476E-15 ) ) ;
#180161 = DIRECTION ( 'NONE',  ( 0.000000000000000000, 1.000000000000000000, -1.224646799147353207E-16 ) ) ;
#180162 = CARTESIAN_POINT ( 'NONE',  ( -20.64999999999999858, 71.65000000001222702, -148.8731074845244109 ) ) ;
#180163 = CIRCLE ( 'NONE', #242493, 0.2000000000000005107 ) ;
#180165 = EDGE_CURVE ( 'NONE', #127078, #182882, #41325, .T. ) ;
#180164 = DIRECTION ( 'NONE',  ( 0.000000000000000000, -7.056502275159890832E-15, 1.000000000000000000 ) ) ;
#180166 = DIRECTION ( 'NONE',  ( 0.000000000000000000, 0.000000000000000000, 1.000000000000000000 ) ) ;
#180168 = ORIENTED_EDGE ( 'NONE', *, *, #224264, .T. ) ;
#180167 = CARTESIAN_POINT ( 'NONE',  ( -16.91256925476571027, 9.985731158139333985, -146.5323575109947569 ) ) ;
#180169 = CIRCLE ( 'NONE', #38878, 0.1000000000000028644 ) ;
#180170 = VECTOR ( 'NONE', #28209, 1000.000000000000114 ) ;
#180171 = ORIENTED_EDGE ( 'NONE', *, *, #18411, .T. ) ;
#180172 = EDGE_CURVE ( 'NONE', #200313, #110820, #203606, .T. ) ;
#180173 = ADVANCED_FACE ( 'NONE', ( #181711 ), #107299, .F. ) ;
#180174 = ORIENTED_EDGE ( 'NONE', *, *, #183813, .F. ) ;
#180175 = CIRCLE ( 'NONE', #179604, 0.09999999999999939493 ) ;
#180176 = DIRECTION ( 'NONE',  ( 0.000000000000000000, -2.428612866367527723E-14, -1.000000000000000000 ) ) ;
#180177 = SURFACE_SIDE_STYLE ('',( #133643 ) ) ;
#180178 = DIRECTION ( 'NONE',  ( 0.000000000000000000, -0.9770955615653312831, -0.2128009952263615612 ) ) ;
#180179 = DIRECTION ( 'NONE',  ( 0.000000000000000000, 0.000000000000000000, -1.000000000000000000 ) ) ;
#180180 = ORIENTED_EDGE ( 'NONE', *, *, #96331, .F. ) ;
#180181 = TOROIDAL_SURFACE ( 'NONE', #80164, 12.97499999999999609, 0.1000000000000000056 ) ;
#180183 = CARTESIAN_POINT ( 'NONE',  ( 20.94999999999999929, 5.000000000011153745, -112.9052660189131245 ) ) ;
#180182 = TOROIDAL_SURFACE ( 'NONE', #121914, 0.2000000000000000111, 0.1000000000000000056 ) ;
#180184 = EDGE_CURVE ( 'NONE', #82520, #175518, #244228, .T. ) ;
#180185 = CARTESIAN_POINT ( 'NONE',  ( -18.59999999999999787, 7.021664781911246322, -104.1335654018973287 ) ) ;
#180186 = CARTESIAN_POINT ( 'NONE',  ( 21.14999999999999858, 11.65000000001116298, -79.15000000000004832 ) ) ;
#180188 = EDGE_LOOP ( 'NONE', ( #54087, #148882, #144181, #120062 ) ) ;
#180187 = DIRECTION ( 'NONE',  ( 0.000000000000000000, 0.8814952561688428334, -0.4721928772777350125 ) ) ;
#180190 = CARTESIAN_POINT ( 'NONE',  ( -18.37013991200266005, 11.49974761622313224, -158.2930230105171461 ) ) ;
#180189 = DIRECTION ( 'NONE',  ( 0.000000000000000000, 0.000000000000000000, -1.000000000000000000 ) ) ;
#180191 = DIRECTION ( 'NONE',  ( -1.000000000000000000, 2.849773892568378313E-16, -7.728835255496647986E-17 ) ) ;
#180192 = CARTESIAN_POINT ( 'NONE',  ( -20.94999999999999929, 64.35000000001191722, -103.0231074845243882 ) ) ;
#180193 = ORIENTED_EDGE ( 'NONE', *, *, #90536, .T. ) ;
#180194 = DIRECTION ( 'NONE',  ( 1.000000000000000000, 0.000000000000000000, 0.000000000000000000 ) ) ;
#180195 = CARTESIAN_POINT ( 'NONE',  ( -18.59999999999999787, 11.65000000001115232, -122.2500000000000284 ) ) ;
#180196 = EDGE_CURVE ( 'NONE', #116181, #154736, #99524, .T. ) ;
#180197 = CARTESIAN_POINT ( 'NONE',  ( 21.05000000000000071, 0.000000000000000000, -35.50000000000000711 ) ) ;
#180198 = VERTEX_POINT ( 'NONE', #104694 ) ;
#180199 = DIRECTION ( 'NONE',  ( 0.000000000000000000, 0.000000000000000000, 1.000000000000000000 ) ) ;
#180200 = CARTESIAN_POINT ( 'NONE',  ( 21.05000000000000071, -11.48912529306490349, -36.39999999999999858 ) ) ;
#180201 = EDGE_CURVE ( 'NONE', #40310, #143511, #237113, .T. ) ;
#180202 = CIRCLE ( 'NONE', #38729, 0.1000000000000064587 ) ;
#180203 = EDGE_LOOP ( 'NONE', ( #100895, #184194, #89567, #233572, #24685, #32773, #196770, #187391, #171317, #149536, #212302 ) ) ;
#180204 = CARTESIAN_POINT ( 'NONE',  ( 18.49999999999999289, 66.34920340998563404, -213.7018660128499334 ) ) ;
#180205 = CIRCLE ( 'NONE', #159361, 7.800000000000001599 ) ;
#180206 = DIRECTION ( 'NONE',  ( 0.000000000000000000, -0.1298341882520022694, -0.9915357197604852679 ) ) ;
#180207 = DIRECTION ( 'NONE',  ( -0.000000000000000000, -0.2814428106787469352, -0.9595780032479105381 ) ) ;
#180208 = VERTEX_POINT ( 'NONE', #225933 ) ;
#180209 = ORIENTED_EDGE ( 'NONE', *, *, #236285, .T. ) ;
#180210 = EDGE_CURVE ( 'NONE', #223586, #159037, #13377, .T. ) ;
#180211 = ADVANCED_FACE ( 'NONE', ( #241681 ), #63030, .F. ) ;
#180212 = CARTESIAN_POINT ( 'NONE',  ( -20.00857864376270001, 66.85000000001222986, -148.8731074845244393 ) ) ;
#180213 = CARTESIAN_POINT ( 'NONE',  ( -2.995603634470884209E-16, -11.75000000000000000, -21.25000000000000000 ) ) ;
#180214 = CARTESIAN_POINT ( 'NONE',  ( 21.09696443733127325, 13.08195529389994860, -210.6724668423044307 ) ) ;
#180215 = CARTESIAN_POINT ( 'NONE',  ( -18.59999999999999787, -9.321008403350132809, -141.2359382490778899 ) ) ;
#180217 = LINE ( 'NONE', #176376, #194920 ) ;
#180216 = DIRECTION ( 'NONE',  ( 0.000000000000000000, 0.000000000000000000, 1.000000000000000000 ) ) ;
#180218 = EDGE_CURVE ( 'NONE', #257097, #163312, #20648, .T. ) ;
#180219 = CARTESIAN_POINT ( 'NONE',  ( -18.60000000000000142, -9.523954320752791247, -40.38201705682730847 ) ) ;
#180220 = DIRECTION ( 'NONE',  ( 1.000000000000000000, 0.000000000000000000, 0.000000000000000000 ) ) ;
#180221 = CARTESIAN_POINT ( 'NONE',  ( 22.49999999999999645, 75.89914163091350474, -148.2726746080136877 ) ) ;
#180222 = ORIENTED_EDGE ( 'NONE', *, *, #242174, .F. ) ;
#180223 = CARTESIAN_POINT ( 'NONE',  ( 20.85000000000000142, 11.65000000001115943, -200.9999999999999432 ) ) ;
#180224 = AXIS2_PLACEMENT_3D ( 'NONE', #162275, #241784, #63135 ) ;
#180226 = VERTEX_POINT ( 'NONE', #143847 ) ;
#180225 = CARTESIAN_POINT ( 'NONE',  ( -20.54999999999999716, 76.00000000001213607, -136.5231074845243313 ) ) ;
#180227 = CARTESIAN_POINT ( 'NONE',  ( 20.95568717954149562, 65.39800594612081852, -195.9205991162557723 ) ) ;
#180228 = DIRECTION ( 'NONE',  ( 0.000000000000000000, -1.000000000000000000, 0.000000000000000000 ) ) ;
#180229 = DIRECTION ( 'NONE',  ( 1.000000000000000000, 0.000000000000000000, 0.000000000000000000 ) ) ;
#180230 = VERTEX_POINT ( 'NONE', #44770 ) ;
#180231 = CARTESIAN_POINT ( 'NONE',  ( -16.87683809663750623, 66.05000000001157900, -56.12074346632790878 ) ) ;
#180232 = DIRECTION ( 'NONE',  ( 0.000000000000000000, -0.000000000000000000, -1.000000000000000000 ) ) ;
#180233 = EDGE_CURVE ( 'NONE', #112332, #220164, #124308, .T. ) ;
#180234 = FACE_OUTER_BOUND ( 'NONE', #195217, .T. ) ;
#180235 = CARTESIAN_POINT ( 'NONE',  ( -20.94999999999999929, 87.48912529308769592, -66.42310748452423752 ) ) ;
#180236 = DIRECTION ( 'NONE',  ( 1.000000000000000000, 3.265361837132813093E-16, -0.000000000000000000 ) ) ;
#180237 = ORIENTED_EDGE ( 'NONE', *, *, #210676, .T. ) ;
#180238 = CARTESIAN_POINT ( 'NONE',  ( -14.00000000000000178, 9.850000000011133849, -117.2500000000000284 ) ) ;
#180239 = EDGE_LOOP ( 'NONE', ( #234024, #235380, #62225, #137519 ) ) ;
#180240 = EDGE_CURVE ( 'NONE', #174781, #61278, #171185, .T. ) ;
#180241 = CARTESIAN_POINT ( 'NONE',  ( -16.77828822459933633, 9.946229375067616729, -54.33737174908105771 ) ) ;
#180242 = EDGE_LOOP ( 'NONE', ( #59188, #257680, #150226, #155704 ) ) ;
#180243 = DIRECTION ( 'NONE',  ( 0.000000000000000000, 0.9770955615653315052, 0.2128009952263605065 ) ) ;
#180244 = ORIENTED_EDGE ( 'NONE', *, *, #33597, .T. ) ;
#180245 = VECTOR ( 'NONE', #145627, 1000.000000000000000 ) ;
#180246 = DIRECTION ( 'NONE',  ( -1.000000000000000000, -1.186688945009010077E-16, -0.000000000000000000 ) ) ;
#180247 = DIRECTION ( 'NONE',  ( 0.000000000000000000, 0.000000000000000000, 1.000000000000000000 ) ) ;
#180248 = ORIENTED_EDGE ( 'NONE', *, *, #90594, .T. ) ;
#180249 = DIRECTION ( 'NONE',  ( -1.000000000000000000, -1.836970198721029934E-16, 0.000000000000000000 ) ) ;
#180250 = DIRECTION ( 'NONE',  ( 0.000000000000000000, 6.982962677686266711E-15, -1.000000000000000000 ) ) ;
#180251 = CARTESIAN_POINT ( 'NONE',  ( -18.50000000000000000, 66.75000000001223555, -148.8731074845244393 ) ) ;
#180252 = AXIS2_PLACEMENT_3D ( 'NONE', #164997, #103710, #107583 ) ;
#180253 = CARTESIAN_POINT ( 'NONE',  ( 11.60000000000006182, 63.75000000001119815, -21.02310748452479316 ) ) ;
#180254 = DIRECTION ( 'NONE',  ( 0.000000000000000000, -6.467318590049456648E-15, 1.000000000000000000 ) ) ;
#180255 = DIRECTION ( 'NONE',  ( 1.000000000000000000, 0.000000000000000000, 0.000000000000000000 ) ) ;
#180256 = EDGE_LOOP ( 'NONE', ( #119585, #117797, #39921, #8404 ) ) ;
#180257 = CARTESIAN_POINT ( 'NONE',  ( -20.94999999999999929, 87.75000000001163869, -66.62310748452424036 ) ) ;
#180258 = ORIENTED_EDGE ( 'NONE', *, *, #28637, .T. ) ;
#180260 = ORIENTED_EDGE ( 'NONE', *, *, #252316, .F. ) ;
#180259 = CARTESIAN_POINT ( 'NONE',  ( -16.87368910959167678, 66.03872618332046329, -90.41061438788379689 ) ) ;
#180261 = ORIENTED_EDGE ( 'NONE', *, *, #40436, .T. ) ;
#180262 = CARTESIAN_POINT ( 'NONE',  ( -23.25000000000000000, -11.74999999998884448, -167.5000000000000000 ) ) ;
#180263 = DIRECTION ( 'NONE',  ( 0.000000000000000000, 1.000000000000000000, 0.000000000000000000 ) ) ;
#180264 = CARTESIAN_POINT ( 'NONE',  ( -18.59999999999999787, 11.65000000001115232, -174.5148057706539930 ) ) ;
#180265 = CARTESIAN_POINT ( 'NONE',  ( 23.24999999999999289, 69.55000000001223270, -148.8731074845244109 ) ) ;
#180266 = CIRCLE ( 'NONE', #167611, 0.1000000000000028644 ) ;
#180267 = DIRECTION ( 'NONE',  ( -1.000000000000000000, 0.000000000000000000, 0.000000000000000000 ) ) ;
#180268 = EDGE_LOOP ( 'NONE', ( #93752, #119764, #53198, #129384 ) ) ;
#180269 = DIRECTION ( 'NONE',  ( 0.000000000000000000, 1.000000000000000000, 0.000000000000000000 ) ) ;
#180270 = CARTESIAN_POINT ( 'NONE',  ( -16.79139129368505934, 66.05505583755062560, -157.3528628516985748 ) ) ;
#180271 = TOROIDAL_SURFACE ( 'NONE', #5258, 0.4000000000000009104, 0.1000000000000000056 ) ;
#180272 = EDGE_LOOP ( 'NONE', ( #215102, #11237, #253229, #51486 ) ) ;
#180273 = VECTOR ( 'NONE', #35051, 1000.000000000000000 ) ;
#180274 = CIRCLE ( 'NONE', #88467, 0.09999999999999867328 ) ;
#180275 = CARTESIAN_POINT ( 'NONE',  ( 18.51997666896878059, -9.392332131507652448, -174.6434061874831514 ) ) ;
#180276 = CIRCLE ( 'NONE', #67833, 0.1999999999999890476 ) ;
#180277 = ADVANCED_FACE ( 'NONE', ( #73352 ), #48608, .T. ) ;
#180278 = CARTESIAN_POINT ( 'NONE',  ( 21.93642651522410603, 7.327166239336949438, -100.5000000000000284 ) ) ;
#180279 = ORIENTED_EDGE ( 'NONE', *, *, #3501, .F. ) ;
#180280 = FACE_OUTER_BOUND ( 'NONE', #144927, .T. ) ;
#180281 = FACE_OUTER_BOUND ( 'NONE', #65570, .T. ) ;
#180282 = ORIENTED_EDGE ( 'NONE', *, *, #207320, .T. ) ;
#180283 = DIRECTION ( 'NONE',  ( 0.000000000000000000, 0.4721928772777551075, 0.8814952561688320642 ) ) ;
#180284 = EDGE_CURVE ( 'NONE', #248091, #247920, #31657, .T. ) ;
#180285 = LINE ( 'NONE', #119033, #256100 ) ;
#180286 = DIRECTION ( 'NONE',  ( 2.952720810173289605E-16, -0.9770955615653315052, -0.2128009952263610061 ) ) ;
#180287 = CARTESIAN_POINT ( 'NONE',  ( -23.15000000000000213, 4.250000000011156409, -79.25000000000004263 ) ) ;
#180288 = EDGE_CURVE ( 'NONE', #155942, #196105, #87724, .T. ) ;
#180289 = EDGE_CURVE ( 'NONE', #25668, #221833, #41496, .T. ) ;
#180290 = AXIS2_PLACEMENT_3D ( 'NONE', #167313, #244236, #125585 ) ;
#180291 = CARTESIAN_POINT ( 'NONE',  ( -18.59999999999999787, -1.162701749926853712, -41.60000000000000142 ) ) ;
#180292 = ORIENTED_EDGE ( 'NONE', *, *, #251668, .F. ) ;
#180293 = VERTEX_POINT ( 'NONE', #251953 ) ;
#180294 = CIRCLE ( 'NONE', #246920, 0.2000000000000057288 ) ;
#180295 = CARTESIAN_POINT ( 'NONE',  ( -18.45140287520618472, 85.48607773954195466, -163.3825843578381978 ) ) ;
#180296 = EDGE_CURVE ( 'NONE', #72158, #163070, #91374, .T. ) ;
#180297 = DIRECTION ( 'NONE',  ( -0.7071067811865487940, -0.6824534298470361637, 0.1850873201762206766 ) ) ;
#180298 = CIRCLE ( 'NONE', #26365, 11.74999999999999645 ) ;
#180300 = ORIENTED_EDGE ( 'NONE', *, *, #228889, .T. ) ;
#180299 = CARTESIAN_POINT ( 'NONE',  ( -18.79999999999999716, 1.350000000000000089, 22.00000000000000355 ) ) ;
#180301 = CARTESIAN_POINT ( 'NONE',  ( 20.95512828230159030, 67.12384868768627655, -57.32067721902129875 ) ) ;
#180302 = DIRECTION ( 'NONE',  ( 0.000000000000000000, -0.2617529984165031243, -0.9651348961777157509 ) ) ;
#180303 = DIRECTION ( 'NONE',  ( 0.000000000000000000, 0.2617529984164996826, 0.9651348961777166391 ) ) ;
#180304 = DIRECTION ( 'NONE',  ( 0.000000000000000000, 0.000000000000000000, 1.000000000000000000 ) ) ;
#180305 = AXIS2_PLACEMENT_3D ( 'NONE', #65363, #59218, #60536 ) ;
#180306 = CARTESIAN_POINT ( 'NONE',  ( 21.05000000000000071, 28.56975825374500388, -258.1421690862028413 ) ) ;
#180307 = DIRECTION ( 'NONE',  ( 0.000000000000000000, -0.2128009952263403282, 0.9770955615653358350 ) ) ;
#180309 = EDGE_LOOP ( 'NONE', ( #181251, #257205, #151589, #129474 ) ) ;
#180308 = DIRECTION ( 'NONE',  ( 1.000000000000000000, 0.000000000000000000, 0.000000000000000000 ) ) ;
#180310 = AXIS2_PLACEMENT_3D ( 'NONE', #67433, #226486, #88254 ) ;
#180311 = CIRCLE ( 'NONE', #117935, 6.329289321881356400 ) ;
#180312 = AXIS2_PLACEMENT_3D ( 'NONE', #192598, #11403, #15257 ) ;
#180313 = VECTOR ( 'NONE', #192498, 1000.000000000000114 ) ;
#180314 = DIRECTION ( 'NONE',  ( -1.000000000000000000, 0.000000000000000000, -0.000000000000000000 ) ) ;
#180315 = ORIENTED_EDGE ( 'NONE', *, *, #248990, .T. ) ;
#180316 = EDGE_CURVE ( 'NONE', #205348, #256826, #212178, .T. ) ;
#180317 = ORIENTED_EDGE ( 'NONE', *, *, #85972, .T. ) ;
#180318 = ADVANCED_FACE ( 'NONE', ( #228551 ), #150301, .F. ) ;
#180319 = CARTESIAN_POINT ( 'NONE',  ( -21.06715728752537942, 11.75000000001115019, -107.5148057706540357 ) ) ;
#180320 = CARTESIAN_POINT ( 'NONE',  ( -18.49719636458550553, 85.44636535924099974, -196.4514936146412367 ) ) ;
#180321 = CIRCLE ( 'NONE', #63602, 0.09999999999999967248 ) ;
#180322 = EDGE_LOOP ( 'NONE', ( #234263, #173984, #97808, #63960 ) ) ;
#180323 = DIRECTION ( 'NONE',  ( 0.000000000000000000, 0.000000000000000000, -1.000000000000000000 ) ) ;
#180324 = AXIS2_PLACEMENT_3D ( 'NONE', #18232, #235978, #61205 ) ;
#180326 = ADVANCED_FACE ( 'NONE', ( #49895 ), #128974, .T. ) ;
#180325 = SURFACE_STYLE_USAGE ( .BOTH. , #1664 ) ;
#180327 = CIRCLE ( 'NONE', #246956, 12.87499999999999822 ) ;
#180328 = ORIENTED_EDGE ( 'NONE', *, *, #224312, .T. ) ;
#180329 = DIRECTION ( 'NONE',  ( 0.000000000000000000, 0.000000000000000000, 1.000000000000000000 ) ) ;
#180330 = CIRCLE ( 'NONE', #117780, 0.09999999999999939493 ) ;
#180331 = AXIS2_PLACEMENT_3D ( 'NONE', #231231, #215491, #19880 ) ;
#180333 = AXIS2_PLACEMENT_3D ( 'NONE', #217816, #238686, #237409 ) ;
#180332 = CARTESIAN_POINT ( 'NONE',  ( -16.94180778212363236, 66.00755694428045217, -190.9189239139911649 ) ) ;
#180334 = ORIENTED_EDGE ( 'NONE', *, *, #125775, .T. ) ;
#180335 = AXIS2_PLACEMENT_3D ( 'NONE', #57654, #135904, #216739 ) ;
#180336 = ORIENTED_EDGE ( 'NONE', *, *, #25375, .T. ) ;
#180337 = DIRECTION ( 'NONE',  ( 0.000000000000000000, -7.272083257015735086E-15, 1.000000000000000000 ) ) ;
#180338 = VERTEX_POINT ( 'NONE', #231136 ) ;
#180339 = CARTESIAN_POINT ( 'NONE',  ( -14.00000000000000178, 47.91805600923872532, -233.7139610577891631 ) ) ;
#180340 = ORIENTED_EDGE ( 'NONE', *, *, #50436, .F. ) ;
#180342 = ORIENTED_EDGE ( 'NONE', *, *, #229000, .F. ) ;
#180341 = DIRECTION ( 'NONE',  ( -1.000000000000000000, 0.000000000000000000, 0.000000000000000000 ) ) ;
#180343 = CARTESIAN_POINT ( 'NONE',  ( -20.64999999999999858, 11.43341603104965110, -245.8667934851861787 ) ) ;
#180344 = ORIENTED_EDGE ( 'NONE', *, *, #115519, .F. ) ;
#180345 = DIRECTION ( 'NONE',  ( 1.476360405086644309E-16, -1.000000000000000000, -0.000000000000000000 ) ) ;
#180346 = ORIENTED_EDGE ( 'NONE', *, *, #203898, .F. ) ;
#180348 = ORIENTED_EDGE ( 'NONE', *, *, #192481, .F. ) ;
#180347 = VERTEX_POINT ( 'NONE', #68184 ) ;
#180349 = DIRECTION ( 'NONE',  ( 0.000000000000000000, -0.9651348961777157509, 0.2617529984165031243 ) ) ;
#180350 = FACE_OUTER_BOUND ( 'NONE', #168186, .T. ) ;
#180352 = ORIENTED_EDGE ( 'NONE', *, *, #187402, .F. ) ;
#180351 = AXIS2_PLACEMENT_3D ( 'NONE', #254369, #171059, #15819 ) ;
#180353 = VECTOR ( 'NONE', #135349, 1000.000000000000000 ) ;
#180354 = CIRCLE ( 'NONE', #209572, 0.09999999999999895084 ) ;
#180355 = VECTOR ( 'NONE', #141870, 1000.000000000000000 ) ;
#180356 = ADVANCED_FACE ( 'NONE', ( #130717 ), #169902, .F. ) ;
#180357 = EDGE_CURVE ( 'NONE', #120974, #160249, #227245, .T. ) ;
#180358 = EDGE_LOOP ( 'NONE', ( #90951, #201723, #167083, #2947 ) ) ;
#180359 = CARTESIAN_POINT ( 'NONE',  ( 18.39999999999998082, 40.40989152675300033, -235.2989281452919954 ) ) ;
#180360 = CARTESIAN_POINT ( 'NONE',  ( 18.59999999999999076, 65.79142135624930177, -115.1731074845243796 ) ) ;
#180361 =( BOUNDED_SURFACE ( )  B_SPLINE_SURFACE ( 3, 2, ( 
 ( #203231, #161564, #205797 ),
 ( #27202, #106679, #7600 ),
 ( #87123, #166710, #200674 ),
 ( #22047, #181124, #92260 ),
 ( #208391, #167997, #51838 ),
 ( #31056, #252617, #171850 ) ),
 .UNSPECIFIED., .F., .F., .F. ) 
 B_SPLINE_SURFACE_WITH_KNOTS ( ( 4, 2, 4 ),
 ( 3, 3 ),
 ( 0.0001792624049599621759, 0.0003686986002124819695, 0.0005581347954650017632 ),
 ( 0.000000000000000000, 1.000000000000000000 ),
 .UNSPECIFIED. ) 
 GEOMETRIC_REPRESENTATION_ITEM ( )  RATIONAL_B_SPLINE_SURFACE ( (
 ( 1.000000000000000000, 0.9238795325112516554, 1.000000000000000000),
 ( 1.000000000000000000, 0.9229318695242004766, 1.000000000000000000),
 ( 1.000000000000000000, 0.8926288119226696294, 1.000000000000000000),
 ( 1.000000000000000000, 0.8123777807275355256, 1.000000000000000000),
 ( 1.000000000000000000, 0.7629087100928401144, 1.000000000000000000),
 ( 1.000000000000000000, 0.7071067811865352493, 1.000000000000000000) ) ) 
 REPRESENTATION_ITEM ( '' )  SURFACE ( )  );
#180362 = VERTEX_POINT ( 'NONE', #108591 ) ;
#180363 = DIRECTION ( 'NONE',  ( 0.000000000000000000, 0.8814952561688437216, -0.4721928772777334582 ) ) ;
#180364 = ORIENTED_EDGE ( 'NONE', *, *, #61654, .T. ) ;
#180365 = ADVANCED_FACE ( 'NONE', ( #8220 ), #232419, .T. ) ;
#180367 = EDGE_CURVE ( 'NONE', #54023, #213186, #188132, .T. ) ;
#180366 = CARTESIAN_POINT ( 'NONE',  ( -18.51024323315077424, 65.68895814178263493, -131.0026557862138645 ) ) ;
#180368 = DIRECTION ( 'NONE',  ( 0.000000000000000000, 0.000000000000000000, 1.000000000000000000 ) ) ;
#180369 = EDGE_LOOP ( 'NONE', ( #166860, #4797, #239157, #49211, #227149 ) ) ;
#180370 = CARTESIAN_POINT ( 'NONE',  ( -21.05000000000000071, 74.16465844978765176, -124.9679561919613207 ) ) ;
#180371 = CARTESIAN_POINT ( 'NONE',  ( 21.05000000000000071, 67.12338541492449906, -61.13802700567970305 ) ) ;
#180372 = CARTESIAN_POINT ( 'NONE',  ( 23.14999999999999858, 76.00000000001213607, -136.5231074845242745 ) ) ;
#180373 = ADVANCED_FACE ( 'NONE', ( #248095 ), #109859, .T. ) ;
#180374 = ORIENTED_EDGE ( 'NONE', *, *, #235679, .T. ) ;
#180375 = DIRECTION ( 'NONE',  ( 1.000000000000000000, -3.265361837132813093E-16, -2.280189983783949500E-30 ) ) ;
#180376 = EDGE_LOOP ( 'NONE', ( #93841, #213464, #256213, #81202 ) ) ;
#180377 = ORIENTED_EDGE ( 'NONE', *, *, #81118, .F. ) ;
#180378 = ADVANCED_FACE ( 'NONE', ( #229818 ), #120609, .T. ) ;
#180380 = ADVANCED_FACE ( 'NONE', ( #74648 ), #87249, .F. ) ;
#180379 = EDGE_CURVE ( 'NONE', #218126, #214994, #12087, .T. ) ;
#180381 = FACE_OUTER_BOUND ( 'NONE', #241056, .T. ) ;
#180382 = ORIENTED_EDGE ( 'NONE', *, *, #29377, .T. ) ;
#180383 = AXIS2_PLACEMENT_3D ( 'NONE', #106142, #240540, #206549 ) ;
#180384 = ORIENTED_EDGE ( 'NONE', *, *, #14686, .F. ) ;
#180385 = CARTESIAN_POINT ( 'NONE',  ( -18.37160782347004329, 11.47561641481354044, -42.75000000000000000 ) ) ;
#180386 = CARTESIAN_POINT ( 'NONE',  ( -23.25000000000000000, 76.00000000001190870, -103.0231074845243029 ) ) ;
#180387 = ORIENTED_EDGE ( 'NONE', *, *, #172099, .T. ) ;
#180388 = EDGE_CURVE ( 'NONE', #114189, #129693, #154190, .T. ) ;
#180389 = EDGE_LOOP ( 'NONE', ( #130111, #210226, #4581, #164341 ) ) ;
#180390 = PLANE ( 'NONE',  #85430 ) ;
#180391 = CARTESIAN_POINT ( 'NONE',  ( 22.50497660315937765, 76.07871793023828388, -215.2729029894197197 ) ) ;
#180392 = ORIENTED_EDGE ( 'NONE', *, *, #179901, .T. ) ;
#180393 = EDGE_CURVE ( 'NONE', #5367, #14621, #198404, .T. ) ;
#180394 = ORIENTED_EDGE ( 'NONE', *, *, #231951, .T. ) ;
#180395 = EDGE_CURVE ( 'NONE', #43175, #12448, #58015, .T. ) ;
#180396 = EDGE_CURVE ( 'NONE', #70888, #3673, #40661, .T. ) ;
#180397 = ORIENTED_EDGE ( 'NONE', *, *, #147890, .F. ) ;
#180398 = ADVANCED_FACE ( 'NONE', ( #115013 ), #95627, .F. ) ;
#180399 = CARTESIAN_POINT ( 'NONE',  ( 21.14999999999999858, 69.45934304831143891, -203.5231074845243882 ) ) ;
#180400 = CARTESIAN_POINT ( 'NONE',  ( 18.43473516226069364, 85.49494228277087871, -196.4772088011747826 ) ) ;
#180401 = DIRECTION ( 'NONE',  ( -1.000000000000000000, 0.000000000000000000, -0.000000000000000000 ) ) ;
#180402 = DIRECTION ( 'NONE',  ( -1.000000000000000000, 0.000000000000000000, -0.000000000000000000 ) ) ;
#180403 = EDGE_CURVE ( 'NONE', #47601, #228369, #183143, .T. ) ;
#180404 = PLANE ( 'NONE',  #174384 ) ;
#180405 = CARTESIAN_POINT ( 'NONE',  ( -20.54999999999999716, 2.500000000011154633, -187.7753780772378889 ) ) ;
#180407 = CARTESIAN_POINT ( 'NONE',  ( 21.05000000000001137, 33.99373157816871327, -243.8426824212976953 ) ) ;
#180406 = DIRECTION ( 'NONE',  ( 1.000000000000000000, 0.000000000000000000, 0.000000000000000000 ) ) ;
#180408 = DIRECTION ( 'NONE',  ( 0.000000000000000000, 0.000000000000000000, 1.000000000000000000 ) ) ;
#180410 = EDGE_CURVE ( 'NONE', #162073, #48041, #55015, .T. ) ;
#180409 = LINE ( 'NONE', #229797, #123662 ) ;
#180411 = AXIS2_PLACEMENT_3D ( 'NONE', #38165, #139795, #96801 ) ;
#180412 = CARTESIAN_POINT ( 'NONE',  ( 23.14999999999999503, 42.94327155031035659, -233.8606566173841372 ) ) ;
#180413 = CYLINDRICAL_SURFACE ( 'NONE', #21841, 0.1000000000000065836 ) ;
#180414 = AXIS2_PLACEMENT_3D ( 'NONE', #98458, #97173, #56776 ) ;
#180415 = EDGE_LOOP ( 'NONE', ( #64930, #90631, #54976 ) ) ;
#180416 = VECTOR ( 'NONE', #29961, 1000.000000000000000 ) ;
#180418 = ORIENTED_EDGE ( 'NONE', *, *, #205661, .T. ) ;
#180417 = DIRECTION ( 'NONE',  ( -1.000000000000000000, 0.000000000000000000, 0.000000000000000000 ) ) ;
#180419 = EDGE_CURVE ( 'NONE', #38476, #128403, #12275, .T. ) ;
#180420 = CARTESIAN_POINT ( 'NONE',  ( -23.25000000000000355, 5.650000000011139001, -176.7499999999999716 ) ) ;
#180421 = DIRECTION ( 'NONE',  ( -1.000000000000000000, 0.000000000000000000, 0.000000000000000000 ) ) ;
#180422 = CARTESIAN_POINT ( 'NONE',  ( -22.46246831459151494, 64.16073937605142419, -247.0930817548480150 ) ) ;
#180423 = ORIENTED_EDGE ( 'NONE', *, *, #220382, .F. ) ;
#180424 = AXIS2_PLACEMENT_3D ( 'NONE', #199359, #183641, #241052 ) ;
#180425 = AXIS2_PLACEMENT_3D ( 'NONE', #146652, #188372, #29342 ) ;
#180427 = CIRCLE ( 'NONE', #67999, 12.77500000000000036 ) ;
#180426 = DIRECTION ( 'NONE',  ( -0.7071067811865475727, 0.2890913453342130457, -0.6453109281988448354 ) ) ;
#180428 = CARTESIAN_POINT ( 'NONE',  ( -23.25000000000000000, 1.115600667400684642E-11, -100.5000000000000426 ) ) ;
#180429 = ORIENTED_EDGE ( 'NONE', *, *, #228070, .F. ) ;
#180430 = DIRECTION ( 'NONE',  ( 0.000000000000000000, -1.000000000000000000, 0.000000000000000000 ) ) ;
#180431 = DIRECTION ( 'NONE',  ( 1.000000000000000000, 0.000000000000000000, 0.000000000000000000 ) ) ;
#180432 = CARTESIAN_POINT ( 'NONE',  ( 19.90000000000000568, 5.586869315528661062, 16.41686199900910736 ) ) ;
#180433 = VECTOR ( 'NONE', #13997, 1000.000000000000114 ) ;
#180434 = CARTESIAN_POINT ( 'NONE',  ( 21.04999999999651905, 40.80806194774932294, -237.9707170097019855 ) ) ;
#180436 = ORIENTED_EDGE ( 'NONE', *, *, #27090, .T. ) ;
#180435 = LINE ( 'NONE', #139997, #201877 ) ;
#180438 = ORIENTED_EDGE ( 'NONE', *, *, #229920, .T. ) ;
#180437 = DIRECTION ( 'NONE',  ( 1.000000000000000000, -0.000000000000000000, 0.000000000000000000 ) ) ;
#180439 = AXIS2_PLACEMENT_3D ( 'NONE', #41022, #180515, #103517 ) ;
#180440 = SPHERICAL_SURFACE ( 'NONE', #199933, 0.1000000000000000056 ) ;
#180442 = DIRECTION ( 'NONE',  ( -0.000000000000000000, 1.000000000000000000, 0.000000000000000000 ) ) ;
#180441 = AXIS2_PLACEMENT_3D ( 'NONE', #20284, #66785, #27698 ) ;
#180443 = AXIS2_PLACEMENT_3D ( 'NONE', #85916, #165505, #29859 ) ;
#180444 = CARTESIAN_POINT ( 'NONE',  ( 19.90000000000000568, 11.61130914238355771, 16.60000000000000142 ) ) ;
#180445 = DIRECTION ( 'NONE',  ( 0.000000000000000000, 0.2617529984165152257, 0.9651348961777124202 ) ) ;
#180446 = AXIS2_PLACEMENT_3D ( 'NONE', #20169, #60553, #99663 ) ;
#180447 = EDGE_CURVE ( 'NONE', #190117, #130981, #117585, .T. ) ;
#180449 = DIRECTION ( 'NONE',  ( 0.000000000000000000, -1.000000000000000000, -6.982962677686266711E-15 ) ) ;
#180448 = CARTESIAN_POINT ( 'NONE',  ( 23.14999999999999503, 21.17283678855157802, -243.7231193059830048 ) ) ;
#180450 = DIRECTION ( 'NONE',  ( 0.000000000000000000, -0.4930308989874653269, -0.8700118002898649117 ) ) ;
#180451 = CARTESIAN_POINT ( 'NONE',  ( 20.94999999999999929, 61.95000000001175522, -75.03680255528533394 ) ) ;
#180452 = ADVANCED_FACE ( 'NONE', ( #197108 ), #135841, .T. ) ;
#180453 = CARTESIAN_POINT ( 'NONE',  ( 21.08198257630413508, 10.05689443876789468, -228.1127196910771318 ) ) ;
#180454 = EDGE_LOOP ( 'NONE', ( #28406, #158324, #223487, #26062 ) ) ;
#180455 = CARTESIAN_POINT ( 'NONE',  ( -21.05000000000000071, 1.148907358139439339E-11, -201.0000000000015064 ) ) ;
#180456 = ORIENTED_EDGE ( 'NONE', *, *, #116803, .T. ) ;
#180457 =( BOUNDED_SURFACE ( )  B_SPLINE_SURFACE ( 3, 2, ( 
 ( #246859, #188191, #207770 ),
 ( #149077, #111215, #106049 ),
 ( #249457, #66948, #130772 ),
 ( #70834, #9535, #51206 ),
 ( #185617, #150353, #229882 ),
 ( #168674, #190786, #46091 ) ),
 .UNSPECIFIED., .F., .F., .F. ) 
 B_SPLINE_SURFACE_WITH_KNOTS ( ( 4, 2, 4 ),
 ( 3, 3 ),
 ( 0.0001381104793128061785, 0.0002947094729387644179, 0.0004513084665647226030 ),
 ( 0.000000000000000000, 1.000000000000000000 ),
 .UNSPECIFIED. ) 
 GEOMETRIC_REPRESENTATION_ITEM ( )  RATIONAL_B_SPLINE_SURFACE ( (
 ( 1.000000000000000000, 0.7071067811865494601, 1.000000000000000000),
 ( 1.000000000000000000, 0.6919563088099165427, 1.000000000000000000),
 ( 1.000000000000000000, 0.6959445945717444015, 1.000000000000000000),
 ( 1.000000000000000000, 0.7137882985313115380, 1.000000000000000000),
 ( 1.000000000000000000, 0.7257496306096496985, 1.000000000000000000),
 ( 1.000000000000000000, 0.7250110520819876836, 1.000000000000000000) ) ) 
 REPRESENTATION_ITEM ( '' )  SURFACE ( )  );
#180458 = ORIENTED_EDGE ( 'NONE', *, *, #42067, .F. ) ;
#180459 = EDGE_CURVE ( 'NONE', #49802, #14341, #137148, .T. ) ;
#180460 = DIRECTION ( 'NONE',  ( 0.000000000000000000, 0.000000000000000000, -1.000000000000000000 ) ) ;
#180461 = EDGE_CURVE ( 'NONE', #234918, #163063, #107232, .T. ) ;
#180462 = DIRECTION ( 'NONE',  ( 0.000000000000000000, -0.1350103645451876666, 0.9908441862701600211 ) ) ;
#180463 = VERTEX_POINT ( 'NONE', #195861 ) ;
#180464 = EDGE_CURVE ( 'NONE', #171125, #101473, #162853, .T. ) ;
#180465 = ORIENTED_EDGE ( 'NONE', *, *, #247179, .T. ) ;
#180466 = AXIS2_PLACEMENT_3D ( 'NONE', #220653, #38177, #257149 ) ;
#180467 =( LENGTH_UNIT ( ) NAMED_UNIT ( * ) SI_UNIT ( .MILLI., .METRE. ) );
#180468 = CIRCLE ( 'NONE', #101295, 4.000000000000003553 ) ;
#180469 = ORIENTED_EDGE ( 'NONE', *, *, #84734, .T. ) ;
#180470 = VECTOR ( 'NONE', #45560, 1000.000000000000000 ) ;
#180471 = B_SPLINE_CURVE_WITH_KNOTS ( 'NONE', 3,
 ( #32777, #131832, #229657, #133125, #93980, #212669, #207538, #28936, #253057, #11915, #150138, #168453, #14485, #52277, #250489, #108427, #34058, #247923, #191842, #69312, #50983, #208811, #73182, #74470, #9318, #187969, #31486, #88831, #151418, #130544 ),
 .UNSPECIFIED., .F., .F.,
 ( 4, 2, 2, 2, 2, 2, 2, 2, 2, 2, 2, 2, 2, 2, 4 ),
 ( 0.000000000000000000, 0.0003422764154113498236, 0.0006845528308226996473, 0.001026829246234049579, 0.001369105661645399295, 0.002053658492468046683, 0.002738211323290694072, 0.003080487738702019935, 0.003422764154113346231, 0.003765040569524672528, 0.004107316984935998824, 0.004449593400347324687, 0.004791869815758650550, 0.005134146231169977280, 0.005476422646581303143 ),
 .UNSPECIFIED. ) ;
#180472 = CARTESIAN_POINT ( 'NONE',  ( 21.05000000000000071, 82.09643798151613225, -215.4278993322501208 ) ) ;
#180473 = ORIENTED_EDGE ( 'NONE', *, *, #10164, .T. ) ;
#180474 = EDGE_CURVE ( 'NONE', #25563, #163036, #208092, .T. ) ;
#180475 = CARTESIAN_POINT ( 'NONE',  ( 20.94999999999999929, -10.38870553492056104, -206.3818953267866902 ) ) ;
#180476 = CARTESIAN_POINT ( 'NONE',  ( -20.65000000000000568, 7.250000000011138646, -42.75000000000000000 ) ) ;
#180477 = FACE_OUTER_BOUND ( 'NONE', #14850, .T. ) ;
#180478 = CARTESIAN_POINT ( 'NONE',  ( -20.85000000000000142, -4.969162394454528453, -233.3995358778103935 ) ) ;
#180479 = DIRECTION ( 'NONE',  ( 0.000000000000000000, -0.2558827019434435912, 0.9667078373770033872 ) ) ;
#180480 = AXIS2_PLACEMENT_3D ( 'NONE', #78682, #254724, #196090 ) ;
#180481 = DIRECTION ( 'NONE',  ( -1.000000000000000000, 7.304098846218163263E-16, -4.217023435051627211E-16 ) ) ;
#180482 = DIRECTION ( 'NONE',  ( 0.000000000000000000, 0.000000000000000000, 1.000000000000000000 ) ) ;
#180484 = ORIENTED_EDGE ( 'NONE', *, *, #16576, .F. ) ;
#180483 = DIRECTION ( 'NONE',  ( 0.000000000000000000, 1.000000000000000000, 0.000000000000000000 ) ) ;
#180486 = FACE_OUTER_BOUND ( 'NONE', #84499, .T. ) ;
#180485 = CARTESIAN_POINT ( 'NONE',  ( -16.92989507731676824, 66.05000000001224691, -149.4056085539143055 ) ) ;
#180487 = CARTESIAN_POINT ( 'NONE',  ( -21.05000000000000071, 11.65000000001115232, -73.78386566297820082 ) ) ;
#180488 = ORIENTED_EDGE ( 'NONE', *, *, #98909, .F. ) ;
#180489 = CIRCLE ( 'NONE', #172346, 0.1000000000000054040 ) ;
#180490 = LINE ( 'NONE', #77499, #147989 ) ;
#180491 = VERTEX_POINT ( 'NONE', #159301 ) ;
#180492 = CIRCLE ( 'NONE', #34765, 0.09999999999999062417 ) ;
#180495 = DIRECTION ( 'NONE',  ( 0.000000000000000000, 1.000000000000000000, 0.000000000000000000 ) ) ;
#180494 = CARTESIAN_POINT ( 'NONE',  ( -18.50000000000000000, -9.499999999988849808, -21.75000000000000355 ) ) ;
#180493 = AXIS2_PLACEMENT_3D ( 'NONE', #238783, #60121, #139648 ) ;
#180496 = CIRCLE ( 'NONE', #122228, 0.09999999999999982514 ) ;
#180497 = CIRCLE ( 'NONE', #14099, 2.000000000000013323 ) ;
#180498 = CARTESIAN_POINT ( 'NONE',  ( -21.07928932188134041, 75.90110485435759813, -109.3516241409176075 ) ) ;
#180499 = ADVANCED_FACE ( 'NONE', ( #238820 ), #4049, .F. ) ;
#180500 = EDGE_LOOP ( 'NONE', ( #189573, #180126, #110865, #209847 ) ) ;
#180501 = AXIS2_PLACEMENT_3D ( 'NONE', #176493, #177784, #21283 ) ;
#180502 = FACE_OUTER_BOUND ( 'NONE', #167242, .T. ) ;
#180503 = DIRECTION ( 'NONE',  ( -1.000000000000000000, 0.000000000000000000, 0.000000000000000000 ) ) ;
#180504 = DIRECTION ( 'NONE',  ( 0.000000000000000000, 0.000000000000000000, -1.000000000000000000 ) ) ;
#180505 = CARTESIAN_POINT ( 'NONE',  ( 20.94999999999999574, 1.736257131608553550, -145.5686523290175387 ) ) ;
#180506 = VERTEX_POINT ( 'NONE', #82274 ) ;
#180507 = AXIS2_PLACEMENT_3D ( 'NONE', #219282, #181467, #40700 ) ;
#180508 = EDGE_CURVE ( 'NONE', #6622, #236967, #37393, .T. ) ;
#180509 = ADVANCED_FACE ( 'NONE', ( #83559 ), #86125, .F. ) ;
#180510 = FACE_OUTER_BOUND ( 'NONE', #126784, .T. ) ;
#180511 = TOROIDAL_SURFACE ( 'NONE', #221983, 2.100000000000002309, 0.1000000000000000056 ) ;
#180512 = CARTESIAN_POINT ( 'NONE',  ( 18.59999999999999787, 74.86109765932729943, -233.8067614591677454 ) ) ;
#180513 = DIRECTION ( 'NONE',  ( -1.000000000000000000, -0.000000000000000000, -0.000000000000000000 ) ) ;
#180514 = DIRECTION ( 'NONE',  ( 0.000000000000000000, -0.7071067811865479058, -0.7071067811865472397 ) ) ;
#180515 = DIRECTION ( 'NONE',  ( 1.000000000000000000, 0.000000000000000000, -0.000000000000000000 ) ) ;
#180516 = AXIS2_PLACEMENT_3D ( 'NONE', #237129, #21941, #200562 ) ;
#180517 = VECTOR ( 'NONE', #104502, 1000.000000000000227 ) ;
#180518 = AXIS2_PLACEMENT_3D ( 'NONE', #145997, #89870, #246395 ) ;
#180519 = ADVANCED_FACE ( 'NONE', ( #221789 ), #145518, .F. ) ;
#180521 = VERTEX_POINT ( 'NONE', #161873 ) ;
#180520 = CARTESIAN_POINT ( 'NONE',  ( 21.05995757104869170, 8.775389244732430427, -179.6949051229912016 ) ) ;
#180522 = MECHANICAL_DESIGN_GEOMETRIC_PRESENTATION_REPRESENTATION (  '', ( #184605 ), #43153 ) ;
#180523 = DIRECTION ( 'NONE',  ( 0.000000000000000000, 0.000000000000000000, -1.000000000000000000 ) ) ;
#180524 = CARTESIAN_POINT ( 'NONE',  ( -21.05000000000000071, -1.851028230129704522, -45.15391326942249606 ) ) ;
#180525 = DIRECTION ( 'NONE',  ( 1.186688945009010077E-16, 1.000000000000000000, 6.982962677686266711E-15 ) ) ;
#180526 = DIRECTION ( 'NONE',  ( -0.7071067811865388020, 0.7071067811865561215, 0.000000000000000000 ) ) ;
#180527 = FACE_OUTER_BOUND ( 'NONE', #245675, .T. ) ;
#180528 = EDGE_CURVE ( 'NONE', #172220, #47223, #47064, .T. ) ;
#180530 = EDGE_LOOP ( 'NONE', ( #231692, #105840, #222113, #233636, #46350, #237044, #160157, #239306 ) ) ;
#180529 = DIRECTION ( 'NONE',  ( 0.000000000000000000, -0.4999999999999689138, 0.8660254037844565822 ) ) ;
#180531 = CARTESIAN_POINT ( 'NONE',  ( -21.55000000000000426, 68.25000000001151079, -48.27310748452437394 ) ) ;
#180532 = EDGE_CURVE ( 'NONE', #164528, #90248, #101844, .T. ) ;
#180533 = LINE ( 'NONE', #220912, #92829 ) ;
#180534 = CARTESIAN_POINT ( 'NONE',  ( -21.05000000000000071, -3.187427350888460076, -228.3200064793908837 ) ) ;
#180535 = EDGE_LOOP ( 'NONE', ( #54543, #120725, #181355, #7966 ) ) ;
#180536 = CARTESIAN_POINT ( 'NONE',  ( 23.14999999999999858, 65.72352950616313194, -223.1694128933794730 ) ) ;
#180537 = CYLINDRICAL_SURFACE ( 'NONE', #244192, 0.1000000000000028644 ) ;
#180538 = CARTESIAN_POINT ( 'NONE',  ( -23.15000000000000213, 71.65000000001199965, -115.3731074845243256 ) ) ;
#180539 = EDGE_CURVE ( 'NONE', #232805, #17316, #128363, .T. ) ;
#180540 = FACE_OUTER_BOUND ( 'NONE', #202879, .T. ) ;
#180541 = AXIS2_PLACEMENT_3D ( 'NONE', #170110, #249611, #70991 ) ;
#180542 = DIRECTION ( 'NONE',  ( 1.000000000000000000, 0.000000000000000000, 0.000000000000000000 ) ) ;
#180543 = AXIS2_PLACEMENT_3D ( 'NONE', #121960, #257551, #20304 ) ;
#180544 = AXIS2_PLACEMENT_3D ( 'NONE', #739, #137696, #80274 ) ;
#180545 = ORIENTED_EDGE ( 'NONE', *, *, #243441, .F. ) ;
#180546 = EDGE_LOOP ( 'NONE', ( #116011, #16876, #10725, #730 ) ) ;
#180547 = FACE_OUTER_BOUND ( 'NONE', #99161, .T. ) ;
#180548 = DIRECTION ( 'NONE',  ( 0.000000000000000000, 0.000000000000000000, -1.000000000000000000 ) ) ;
#180549 = EDGE_CURVE ( 'NONE', #204625, #252057, #223094, .T. ) ;
#180550 = CARTESIAN_POINT ( 'NONE',  ( -21.05000000000000071, 64.27847795353595473, -247.1247091181747066 ) ) ;
#180551 = LINE ( 'NONE', #59260, #168434 ) ;
#180552 = VERTEX_POINT ( 'NONE', #160596 ) ;
#180553 = DIRECTION ( 'NONE',  ( 1.000000000000000000, 0.000000000000000000, 0.000000000000000000 ) ) ;
#180554 = DIRECTION ( 'NONE',  ( 0.000000000000000000, -0.000000000000000000, 1.000000000000000000 ) ) ;
#180555 = CARTESIAN_POINT ( 'NONE',  ( -21.05000000000000071, 11.60000000001115517, -160.5717967697245285 ) ) ;
#180556 = CARTESIAN_POINT ( 'NONE',  ( 20.95568717954149562, 10.60199405390297400, -108.1025083682686869 ) ) ;
#180557 = CARTESIAN_POINT ( 'NONE',  ( -16.84981964351497652, 9.917318234098841501, -20.63039838598054843 ) ) ;
#180558 = ORIENTED_EDGE ( 'NONE', *, *, #80833, .T. ) ;
#180559 = ORIENTED_EDGE ( 'NONE', *, *, #10075, .T. ) ;
#180560 = ORIENTED_EDGE ( 'NONE', *, *, #165170, .T. ) ;
#180561 = AXIS2_PLACEMENT_3D ( 'NONE', #42055, #6757, #62882 ) ;
#180562 = DIRECTION ( 'NONE',  ( -1.000000000000000000, -0.000000000000000000, 0.000000000000000000 ) ) ;
#180563 = ORIENTED_EDGE ( 'NONE', *, *, #184534, .T. ) ;
#180564 = DIRECTION ( 'NONE',  ( 0.000000000000000000, 1.000000000000000000, 0.000000000000000000 ) ) ;
#180565 = LINE ( 'NONE', #184401, #92931 ) ;
#180566 = CARTESIAN_POINT ( 'NONE',  ( 18.50000000000000000, 85.50000000001276135, -215.2731074845243029 ) ) ;
#180567 = ORIENTED_EDGE ( 'NONE', *, *, #3630, .T. ) ;
#180568 = CARTESIAN_POINT ( 'NONE',  ( -23.25000000000000000, 87.65000000001192859, -106.0231074845242176 ) ) ;
#180569 = DIRECTION ( 'NONE',  ( 0.000000000000000000, 0.000000000000000000, -1.000000000000000000 ) ) ;
#180570 = ORIENTED_EDGE ( 'NONE', *, *, #167990, .T. ) ;
#180571 = DIRECTION ( 'NONE',  ( 0.000000000000000000, 1.000000000000000000, 6.938893903907222067E-15 ) ) ;
#180573 = ORIENTED_EDGE ( 'NONE', *, *, #198084, .F. ) ;
#180572 = CARTESIAN_POINT ( 'NONE',  ( -23.15000000000000213, 2.600000000011154278, -154.2753780772379173 ) ) ;
#180574 = CARTESIAN_POINT ( 'NONE',  ( -20.54999999999999716, 36.65892442174935439, -249.5511627012433848 ) ) ;
#180575 = DIRECTION ( 'NONE',  ( 0.000000000000000000, -7.086529944415894657E-15, 1.000000000000000000 ) ) ;
#180576 = VECTOR ( 'NONE', #231904, 1000.000000000000000 ) ;
#180577 = ORIENTED_EDGE ( 'NONE', *, *, #66429, .F. ) ;
#180578 = CIRCLE ( 'NONE', #9878, 0.5000000000000004441 ) ;
#180579 = CARTESIAN_POINT ( 'NONE',  ( 21.13461538461538325, 65.38541703798705385, -191.1731074845244223 ) ) ;
#180580 = CARTESIAN_POINT ( 'NONE',  ( 21.12769345151713196, 10.71928767695172624, -79.24748034619751991 ) ) ;
#180581 = DIRECTION ( 'NONE',  ( -1.020425574104004196E-15, -6.982962677686266711E-15, 1.000000000000000000 ) ) ;
#180582 = ORIENTED_EDGE ( 'NONE', *, *, #79596, .F. ) ;
#180583 = SPHERICAL_SURFACE ( 'NONE', #67366, 0.1000000000000000056 ) ;
#180584 = EDGE_CURVE ( 'NONE', #72588, #42134, #225640, .T. ) ;
#180585 = CARTESIAN_POINT ( 'NONE',  ( 15.07585980824113747, 49.37151442406710089, -233.5366006881135945 ) ) ;
#180586 = CARTESIAN_POINT ( 'NONE',  ( -21.52071067811865746, 68.22071067813045886, -81.87310748452436826 ) ) ;
#180587 = ADVANCED_FACE ( 'NONE', ( #21083 ), #220543, .T. ) ;
#180588 = ORIENTED_EDGE ( 'NONE', *, *, #203998, .T. ) ;
#180589 = EDGE_CURVE ( 'NONE', #221704, #199924, #181432, .T. ) ;
#180590 = VECTOR ( 'NONE', #155621, 1000.000000000000000 ) ;
#180591 = VECTOR ( 'NONE', #21764, 1000.000000000000000 ) ;
#180592 = VECTOR ( 'NONE', #251974, 1000.000000000000000 ) ;
#180593 = ORIENTED_EDGE ( 'NONE', *, *, #212530, .T. ) ;
#180594 = AXIS2_PLACEMENT_3D ( 'NONE', #129041, #207307, #127760 ) ;
#180595 = ORIENTED_EDGE ( 'NONE', *, *, #97624, .F. ) ;
#180596 = DIRECTION ( 'NONE',  ( 0.5000000000001141309, 0.000000000000000000, -0.8660254037843729824 ) ) ;
#180597 = EDGE_CURVE ( 'NONE', #253651, #254124, #191538, .T. ) ;
#180598 = LINE ( 'NONE', #81457, #216925 ) ;
#180600 = ORIENTED_EDGE ( 'NONE', *, *, #234988, .T. ) ;
#180599 = CARTESIAN_POINT ( 'NONE',  ( 12.47034474403012716, 25.54511595760792630, -232.9618513057392875 ) ) ;
#180601 = CARTESIAN_POINT ( 'NONE',  ( 19.92426406871192412, 11.75000000000000711, -24.85000000000000142 ) ) ;
#180602 = CARTESIAN_POINT ( 'NONE',  ( 21.14999999999999858, 64.35000000001214460, -136.4231074845243938 ) ) ;
#180603 = FACE_OUTER_BOUND ( 'NONE', #68765, .T. ) ;
#180604 = DIRECTION ( 'NONE',  ( 0.000000000000000000, 0.9998779222360102414, 0.01562499999996356907 ) ) ;
#180605 = DIRECTION ( 'NONE',  ( 0.000000000000000000, -0.4999999999999689138, -0.8660254037844565822 ) ) ;
#180606 = AXIS2_PLACEMENT_3D ( 'NONE', #207050, #66255, #187505 ) ;
#180607 = CARTESIAN_POINT ( 'NONE',  ( 21.05000000000000071, 74.63912941282003999, -128.4501095574333647 ) ) ;
#180608 = AXIS2_PLACEMENT_3D ( 'NONE', #139300, #220156, #80605 ) ;
#180610 = ORIENTED_EDGE ( 'NONE', *, *, #91803, .F. ) ;
#180609 = CARTESIAN_POINT ( 'NONE',  ( -16.85718274719425125, 66.02385768539068067, -182.5864538167065518 ) ) ;
#180612 = VERTEX_POINT ( 'NONE', #200974 ) ;
#180611 = DIRECTION ( 'NONE',  ( 0.7071067811865462405, -0.6909108974501249056, -0.1504730267678058564 ) ) ;
#180614 = DIRECTION ( 'NONE',  ( 1.000000000000000000, -0.000000000000000000, -0.000000000000000000 ) ) ;
#180613 = AXIS2_PLACEMENT_3D ( 'NONE', #199845, #104537, #182853 ) ;
#180615 = VERTEX_POINT ( 'NONE', #243942 ) ;
#180616 = ORIENTED_EDGE ( 'NONE', *, *, #6017, .F. ) ;
#180617 = DIRECTION ( 'NONE',  ( 0.000000000000000000, -0.9868171638914228216, 0.1618390714546044939 ) ) ;
#180618 = DIRECTION ( 'NONE',  ( 0.000000000000000000, 0.2868887416115947775, -0.9579639084728169829 ) ) ;
#180619 = CARTESIAN_POINT ( 'NONE',  ( -21.05000000000000071, 1.851028230152016674, -145.6539132694225032 ) ) ;
#180620 = VECTOR ( 'NONE', #208043, 1000.000000000000000 ) ;
#180621 = DIRECTION ( 'NONE',  ( 1.000000000000000000, 0.000000000000000000, -0.000000000000000000 ) ) ;
#180622 = EDGE_CURVE ( 'NONE', #255696, #207631, #112408, .T. ) ;
#180623 = ADVANCED_FACE ( 'NONE', ( #6617 ), #172168, .T. ) ;
#180624 = LINE ( 'NONE', #662, #234473 ) ;
#180625 = CARTESIAN_POINT ( 'NONE',  ( 20.75572585718184015, 67.11768327161523473, -195.0258490858114158 ) ) ;
#180626 = VECTOR ( 'NONE', #158123, 1000.000000000000000 ) ;
#180627 = AXIS2_PLACEMENT_3D ( 'NONE', #14811, #252098, #26977 ) ;
#180629 = AXIS2_PLACEMENT_3D ( 'NONE', #243711, #105445, #164188 ) ;
#180628 = CARTESIAN_POINT ( 'NONE',  ( 21.05000000000000071, 10.40519331719241336, -207.3517860968744628 ) ) ;
#180630 = ORIENTED_EDGE ( 'NONE', *, *, #206377, .T. ) ;
#180631 = EDGE_LOOP ( 'NONE', ( #237866, #241312, #216437, #23077 ) ) ;
#180632 = CARTESIAN_POINT ( 'NONE',  ( -18.50000000000000000, -1.687074390080403941, -121.1854270334583674 ) ) ;
#180633 = EDGE_CURVE ( 'NONE', #233882, #129578, #66613, .T. ) ;
#180634 = ORIENTED_EDGE ( 'NONE', *, *, #43279, .F. ) ;
#180635 = CARTESIAN_POINT ( 'NONE',  ( -18.59999999999999787, 9.250000000011157297, -146.2500000000000284 ) ) ;
#180636 = FACE_OUTER_BOUND ( 'NONE', #106272, .T. ) ;
#180637 = CARTESIAN_POINT ( 'NONE',  ( 22.47071067811864964, 75.90090754530983475, -177.7431822290224090 ) ) ;
#180638 = FACE_OUTER_BOUND ( 'NONE', #253198, .T. ) ;
#180639 = EDGE_LOOP ( 'NONE', ( #6313, #165606, #28735, #23955 ) ) ;
#180640 = CARTESIAN_POINT ( 'NONE',  ( -16.87036670365548474, 14.31214069770892472, -219.3240646258064430 ) ) ;
#180641 = VERTEX_POINT ( 'NONE', #189117 ) ;
#180642 = CARTESIAN_POINT ( 'NONE',  ( -17.80356949363834218, 10.87673139701198011, -90.21307302422357566 ) ) ;
#180643 = VERTEX_POINT ( 'NONE', #126575 ) ;
#180644 = PLANE ( 'NONE',  #194063 ) ;
#180645 = EDGE_CURVE ( 'NONE', #221804, #22186, #87439, .T. ) ;
#180646 = AXIS2_PLACEMENT_3D ( 'NONE', #192445, #174204, #136284 ) ;
#180647 = LINE ( 'NONE', #231344, #51306 ) ;
#180648 = ORIENTED_EDGE ( 'NONE', *, *, #244919, .T. ) ;
#180649 = CARTESIAN_POINT ( 'NONE',  ( -18.69999999999999929, -1.212568896937008089, -7.800000000000000711 ) ) ;
#180651 = ORIENTED_EDGE ( 'NONE', *, *, #215098, .F. ) ;
#180650 = DIRECTION ( 'NONE',  ( 0.000000000000000000, 0.000000000000000000, -1.000000000000000000 ) ) ;
#180652 = CIRCLE ( 'NONE', #68226, 0.09999999999999993616 ) ;
#180653 = LINE ( 'NONE', #236754, #81389 ) ;
#180654 = VERTEX_POINT ( 'NONE', #27518 ) ;
#180655 = VECTOR ( 'NONE', #202415, 1000.000000000000000 ) ;
#180656 = EDGE_CURVE ( 'NONE', #143950, #177267, #246512, .T. ) ;
#180657 = AXIS2_PLACEMENT_3D ( 'NONE', #186213, #167958, #246184 ) ;
#180658 = CARTESIAN_POINT ( 'NONE',  ( 18.59999999999999076, 69.45000000001252261, -182.2731074845244166 ) ) ;
#180659 = ORIENTED_EDGE ( 'NONE', *, *, #184566, .T. ) ;
#180660 = LINE ( 'NONE', #102362, #257437 ) ;
#180661 = CARTESIAN_POINT ( 'NONE',  ( 19.87657994472028378, 64.25000000001250555, -178.7573193598975649 ) ) ;
#180662 = DIRECTION ( 'NONE',  ( -1.000000000000000000, 0.000000000000000000, 0.000000000000000000 ) ) ;
#180663 = CARTESIAN_POINT ( 'NONE',  ( -18.40000000000000213, 64.25000000001159606, -56.87310748452440379 ) ) ;
#180664 = VECTOR ( 'NONE', #58000, 1000.000000000000000 ) ;
#180665 = EDGE_CURVE ( 'NONE', #18995, #82481, #71755, .T. ) ;
#180666 = EDGE_CURVE ( 'NONE', #27038, #61955, #158224, .T. ) ;
#180667 = CARTESIAN_POINT ( 'NONE',  ( -23.25000000000000000, 1.115600667400684642E-11, -100.5000000000000284 ) ) ;
#180668 = CIRCLE ( 'NONE', #197403, 0.09999999999998898659 ) ;
#180669 = EDGE_LOOP ( 'NONE', ( #229438, #149253, #204126, #186167 ) ) ;
#180670 = AXIS2_PLACEMENT_3D ( 'NONE', #93630, #131474, #136588 ) ;
#180671 = CARTESIAN_POINT ( 'NONE',  ( 23.14999999999999858, 76.00000000001237765, -170.0231074845243597 ) ) ;
#180672 = DIRECTION ( 'NONE',  ( 1.000000000000000000, 7.304098846218134667E-16, 0.000000000000000000 ) ) ;
#180674 = CARTESIAN_POINT ( 'NONE',  ( 20.94999999999999574, 74.16465844978745281, -91.36795619196134055 ) ) ;
#180673 = VECTOR ( 'NONE', #51136, 1000.000000000000000 ) ;
#180675 = ORIENTED_EDGE ( 'NONE', *, *, #176450, .F. ) ;
#180676 = DIRECTION ( 'NONE',  ( 1.000000000000000000, -0.000000000000000000, 0.000000000000000000 ) ) ;
#180677 = EDGE_LOOP ( 'NONE', ( #159283, #194408, #104286, #205537 ) ) ;
#180678 = CARTESIAN_POINT ( 'NONE',  ( -20.54999999999999716, 65.40605961984559258, -236.6728003091511425 ) ) ;
#180680 = ORIENTED_EDGE ( 'NONE', *, *, #95847, .F. ) ;
#180679 = CIRCLE ( 'NONE', #9987, 0.2000000000000057288 ) ;
#180681 = ADVANCED_FACE ( 'NONE', ( #206109 ), #168315, .F. ) ;
#180682 = EDGE_CURVE ( 'NONE', #177416, #250872, #211246, .T. ) ;
#180683 = LINE ( 'NONE', #97239, #10184 ) ;
#180684 = CARTESIAN_POINT ( 'NONE',  ( -20.94403535211772294, 10.30632246271647467, -72.50418367788957141 ) ) ;
#180685 = ORIENTED_EDGE ( 'NONE', *, *, #64005, .F. ) ;
#180687 = EDGE_LOOP ( 'NONE', ( #89245, #116590, #129097, #27416 ) ) ;
#180686 = DIRECTION ( 'NONE',  ( -1.000000000000000000, 0.000000000000000000, 0.000000000000000000 ) ) ;
#180688 = CARTESIAN_POINT ( 'NONE',  ( 18.39999999999999858, -0.8254770802754703984, -242.3223161824233500 ) ) ;
#180689 = ORIENTED_EDGE ( 'NONE', *, *, #164477, .T. ) ;
#180690 = CARTESIAN_POINT ( 'NONE',  ( -23.15000000000000213, 1.115600667400684642E-11, -167.5000000000000284 ) ) ;
#180691 = FACE_OUTER_BOUND ( 'NONE', #106090, .T. ) ;
#180692 = EDGE_LOOP ( 'NONE', ( #209044, #34115, #161160, #37978, #150248, #245866, #173519, #150855 ) ) ;
#180693 = ORIENTED_EDGE ( 'NONE', *, *, #104171, .F. ) ;
#180694 = VECTOR ( 'NONE', #221399, 1000.000000000000000 ) ;
#180695 = EDGE_CURVE ( 'NONE', #61013, #237888, #224808, .T. ) ;
#180696 = CARTESIAN_POINT ( 'NONE',  ( 18.59999999999999787, 76.00000000001267608, -203.5231074845243597 ) ) ;
#180697 = CARTESIAN_POINT ( 'NONE',  ( -16.94107738177414291, 14.24304960796391128, -219.3391119284832484 ) ) ;
#180698 = CARTESIAN_POINT ( 'NONE',  ( 19.92426406871192412, 64.25000000001148237, -44.67310748452439384 ) ) ;
#180699 = EDGE_CURVE ( 'NONE', #223089, #83188, #241568, .T. ) ;
#180700 = ADVANCED_FACE ( 'NONE', ( #207410 ), #170506, .T. ) ;
#180702 = ORIENTED_EDGE ( 'NONE', *, *, #201813, .F. ) ;
#180701 = AXIS2_PLACEMENT_3D ( 'NONE', #239392, #3316, #181987 ) ;
#180703 = ORIENTED_EDGE ( 'NONE', *, *, #77210, .F. ) ;
#180704 = AXIS2_PLACEMENT_3D ( 'NONE', #197318, #78651, #96908 ) ;
#180705 = CIRCLE ( 'NONE', #238976, 0.1999999999999987899 ) ;
#180706 = DIRECTION ( 'NONE',  ( 1.000000000000000000, 0.000000000000000000, 0.000000000000000000 ) ) ;
#180707 = EDGE_CURVE ( 'NONE', #74558, #108824, #90473, .T. ) ;
#180708 = APPLICATION_CONTEXT ( 'automotive_design' ) ;
#180710 = ORIENTED_EDGE ( 'NONE', *, *, #181470, .F. ) ;
#180709 = PLANE ( 'NONE',  #230615 ) ;
#180711 = EDGE_CURVE ( 'NONE', #241355, #143362, #198625, .T. ) ;
#180712 = DIRECTION ( 'NONE',  ( -1.000000000000000000, -0.000000000000000000, -0.000000000000000000 ) ) ;
#180713 = PLANE ( 'NONE',  #173387 ) ;
#180714 = ADVANCED_FACE ( 'NONE', ( #87430 ), #75008, .F. ) ;
#180715 = CARTESIAN_POINT ( 'NONE',  ( 20.04142135623730070, 11.65000000001115943, -54.85000000000000142 ) ) ;
#180716 = DIRECTION ( 'NONE',  ( -1.000000000000000000, -0.000000000000000000, -0.000000000000000000 ) ) ;
#180717 = CARTESIAN_POINT ( 'NONE',  ( -21.15000000000000213, 76.00000000001219291, -143.0637644362255401 ) ) ;
#180719 = EDGE_CURVE ( 'NONE', #75223, #211866, #174987, .T. ) ;
#180718 = FACE_OUTER_BOUND ( 'NONE', #24884, .T. ) ;
#180720 = DIRECTION ( 'NONE',  ( 0.000000000000000000, 0.000000000000000000, 1.000000000000000000 ) ) ;
#180721 = VECTOR ( 'NONE', #219409, 1000.000000000000000 ) ;
#180722 = CARTESIAN_POINT ( 'NONE',  ( 23.14999999999999858, 5.600000000011153389, -121.5947339810869465 ) ) ;
#180723 = CIRCLE ( 'NONE', #5904, 11.65000000000000036 ) ;
#180724 = AXIS2_PLACEMENT_3D ( 'NONE', #236506, #233947, #174022 ) ;
#180725 = ORIENTED_EDGE ( 'NONE', *, *, #83754, .F. ) ;
#180726 = EDGE_LOOP ( 'NONE', ( #51364, #127548, #94769, #113355 ) ) ;
#180727 = FACE_OUTER_BOUND ( 'NONE', #214206, .T. ) ;
#180728 = ORIENTED_EDGE ( 'NONE', *, *, #105065, .T. ) ;
#180729 = EDGE_CURVE ( 'NONE', #174819, #245138, #33324, .T. ) ;
#180730 = ADVANCED_FACE ( 'NONE', ( #232111 ), #99876, .F. ) ;
#180731 = CARTESIAN_POINT ( 'NONE',  ( -16.88219499860498374, 9.950206425438745228, -146.6493096901073443 ) ) ;
#180732 = ORIENTED_EDGE ( 'NONE', *, *, #255995, .F. ) ;
#180733 = CARTESIAN_POINT ( 'NONE',  ( 20.94999999999999929, 65.70711192142388768, -131.0651054685122574 ) ) ;
#180735 = ORIENTED_EDGE ( 'NONE', *, *, #122048, .F. ) ;
#180734 = VERTEX_POINT ( 'NONE', #178570 ) ;
#180736 = VERTEX_POINT ( 'NONE', #18180 ) ;
#180737 = ORIENTED_EDGE ( 'NONE', *, *, #37713, .T. ) ;
#180738 = DIRECTION ( 'NONE',  ( 0.000000000000000000, -0.9126074666063771490, -0.4088369013363281623 ) ) ;
#180739 = COLOUR_RGB ( '', 0.09019608, 0.27058824, 0.51372549) ;
#180740 = DIRECTION ( 'NONE',  ( 1.186688945009010077E-16, 1.000000000000000000, 6.982962677686266711E-15 ) ) ;
#180742 = ORIENTED_EDGE ( 'NONE', *, *, #122673, .F. ) ;
#180741 = DIRECTION ( 'NONE',  ( 0.000000000000000000, 0.4088369013363304383, -0.9126074666063759278 ) ) ;
#180743 = CARTESIAN_POINT ( 'NONE',  ( -23.15000000000000213, 74.00000000001223555, -149.7477294072864709 ) ) ;
#180744 = FACE_OUTER_BOUND ( 'NONE', #35565, .T. ) ;
#180746 = ORIENTED_EDGE ( 'NONE', *, *, #114081, .T. ) ;
#180745 = CARTESIAN_POINT ( 'NONE',  ( 23.14999999999999503, 69.55000000001199112, -115.3731074845243398 ) ) ;
#180747 = SPHERICAL_SURFACE ( 'NONE', #187587, 0.1000000000000000056 ) ;
#180748 = EDGE_LOOP ( 'NONE', ( #77218, #139596, #133950, #39240, #226429 ) ) ;
#180749 = DIRECTION ( 'NONE',  ( 0.000000000000000000, 0.000000000000000000, -1.000000000000000000 ) ) ;
#180750 = VERTEX_POINT ( 'NONE', #177289 ) ;
#180751 = DIRECTION ( 'NONE',  ( -1.000000000000000000, 0.000000000000000000, 0.000000000000000000 ) ) ;
#180752 = CARTESIAN_POINT ( 'NONE',  ( -15.39126916658603328, 27.26868795068923390, -233.8692014934036365 ) ) ;
#180753 = CYLINDRICAL_SURFACE ( 'NONE', #110846, 0.09999999999998898659 ) ;
#180754 = VERTEX_POINT ( 'NONE', #96413 ) ;
#180755 = EDGE_CURVE ( 'NONE', #122594, #17724, #225263, .T. ) ;
#180757 = CARTESIAN_POINT ( 'NONE',  ( -16.87331047859651179, 44.13548170601895038, -235.2989316066074821 ) ) ;
#180756 = CARTESIAN_POINT ( 'NONE',  ( 18.79999999999999361, -11.75000000000000000, 5.900000000000001243 ) ) ;
#180758 = CARTESIAN_POINT ( 'NONE',  ( -12.60829076262180237, 66.61047060254509233, -85.20599957163069860 ) ) ;
#180759 = AXIS2_PLACEMENT_3D ( 'NONE', #216570, #75786, #217831 ) ;
#180760 = CARTESIAN_POINT ( 'NONE',  ( 18.47135592147665406, 85.47108861327795637, -163.3395125446803320 ) ) ;
#180761 = EDGE_CURVE ( 'NONE', #6106, #86933, #78136, .T. ) ;
#180762 = CIRCLE ( 'NONE', #176675, 0.1000000000000028644 ) ;
#180763 = DIRECTION ( 'NONE',  ( -0.000000000000000000, 0.8814952561688430555, -0.4721928772777346239 ) ) ;
#180764 = ORIENTED_EDGE ( 'NONE', *, *, #104725, .F. ) ;
#180766 = ORIENTED_EDGE ( 'NONE', *, *, #41890, .T. ) ;
#180765 = CIRCLE ( 'NONE', #210001, 0.1000000000000028644 ) ;
#180767 = ORIENTED_EDGE ( 'NONE', *, *, #169488, .T. ) ;
#180768 = VECTOR ( 'NONE', #154805, 1000.000000000000000 ) ;
#180769 = CARTESIAN_POINT ( 'NONE',  ( -21.05000000000000071, -0.09999996528894476711, -127.5224478175062472 ) ) ;
#180770 = ORIENTED_EDGE ( 'NONE', *, *, #162737, .F. ) ;
#180771 = DIRECTION ( 'NONE',  ( 1.000000000000000000, 0.000000000000000000, 0.000000000000000000 ) ) ;
#180772 = VERTEX_POINT ( 'NONE', #195559 ) ;
#180773 = DIRECTION ( 'NONE',  ( 1.000000000000000000, -1.875376730785737719E-16, -1.309568571767809260E-30 ) ) ;
#180774 = DIRECTION ( 'NONE',  ( 1.000000000000000000, 7.304098846218134667E-16, -0.000000000000000000 ) ) ;
#180775 = ORIENTED_EDGE ( 'NONE', *, *, #80788, .T. ) ;
#180776 = AXIS2_PLACEMENT_3D ( 'NONE', #251803, #152739, #138255 ) ;
#180777 = FACE_OUTER_BOUND ( 'NONE', #167558, .T. ) ;
#180778 = FILL_AREA_STYLE_COLOUR ( '', #131420 ) ;
#180779 = EDGE_CURVE ( 'NONE', #124163, #239652, #254031, .T. ) ;
#180780 = TOROIDAL_SURFACE ( 'NONE', #47475, 3.899999999999999467, 0.1000000000000000056 ) ;
#180781 = VERTEX_POINT ( 'NONE', #173466 ) ;
#180782 = VERTEX_POINT ( 'NONE', #116015 ) ;
#180783 = CIRCLE ( 'NONE', #230684, 0.1000000000000012546 ) ;
#180784 = EDGE_LOOP ( 'NONE', ( #219175, #131946, #86718, #199274, #110713 ) ) ;
#180785 = CIRCLE ( 'NONE', #85063, 0.09999999999999939493 ) ;
#180786 = DIRECTION ( 'NONE',  ( -0.000000000000000000, -0.9910827722268049644, 0.1332476588733589318 ) ) ;
#180787 = FACE_OUTER_BOUND ( 'NONE', #245436, .T. ) ;
#180788 = DIRECTION ( 'NONE',  ( 0.000000000000000000, 1.000000000000000000, 6.688090509790097607E-15 ) ) ;
#180789 = CIRCLE ( 'NONE', #97542, 4.299999999999945643 ) ;
#180790 = CARTESIAN_POINT ( 'NONE',  ( 23.24999999999999645, 8.212522512469060842, -212.1579332307740344 ) ) ;
#180791 = LINE ( 'NONE', #195561, #131537 ) ;
#180792 = FACE_OUTER_BOUND ( 'NONE', #122341, .T. ) ;
#180794 = CARTESIAN_POINT ( 'NONE',  ( -18.79999999999999716, -11.65000000000000036, -15.00000000000000000 ) ) ;
#180793 = DIRECTION ( 'NONE',  ( -0.000000000000000000, -0.000000000000000000, -1.000000000000000000 ) ) ;
#180795 = DIRECTION ( 'NONE',  ( -1.000000000000000000, 0.000000000000000000, 0.000000000000000000 ) ) ;
#180797 = ORIENTED_EDGE ( 'NONE', *, *, #176925, .F. ) ;
#180796 = CARTESIAN_POINT ( 'NONE',  ( 21.14999999999999858, 69.35000000001186038, -90.87310748452435405 ) ) ;
#180798 = LINE ( 'NONE', #60823, #249895 ) ;
#180799 = DIRECTION ( 'NONE',  ( -2.342056488767301376E-15, -0.1350103645451904977, 0.9908441862701596881 ) ) ;
#180800 = VERTEX_POINT ( 'NONE', #255455 ) ;
#180801 = ORIENTED_EDGE ( 'NONE', *, *, #52973, .F. ) ;
#180802 = DIRECTION ( 'NONE',  ( 0.000000000000000000, 0.000000000000000000, 1.000000000000000000 ) ) ;
#180804 = VECTOR ( 'NONE', #37112, 1000.000000000000000 ) ;
#180803 = DIRECTION ( 'NONE',  ( 0.000000000000000000, -0.2617529984165034573, -0.9651348961777156399 ) ) ;
#180805 = VECTOR ( 'NONE', #61265, 1000.000000000000000 ) ;
#180806 = ORIENTED_EDGE ( 'NONE', *, *, #230488, .F. ) ;
#180807 = VECTOR ( 'NONE', #43016, 1000.000000000000000 ) ;
#180808 = AXIS2_PLACEMENT_3D ( 'NONE', #375, #244122, #141187 ) ;
#180809 = DIRECTION ( 'NONE',  ( -1.000000000000000000, 0.000000000000000000, 0.000000000000000000 ) ) ;
#180810 = ORIENTED_EDGE ( 'NONE', *, *, #99429, .F. ) ;
#180811 = ORIENTED_EDGE ( 'NONE', *, *, #231423, .T. ) ;
#180812 = AXIS2_PLACEMENT_3D ( 'NONE', #47340, #222114, #205127 ) ;
#180813 = CARTESIAN_POINT ( 'NONE',  ( -16.91256925476571382, 9.985731158128174911, -12.53235751099473205 ) ) ;
#180814 = ORIENTED_EDGE ( 'NONE', *, *, #6709, .F. ) ;
#180815 = FACE_OUTER_BOUND ( 'NONE', #107165, .T. ) ;
#180816 = DIRECTION ( 'NONE',  ( 0.000000000000000000, 1.000000000000000000, 2.891205793294679805E-16 ) ) ;
#180817 = CARTESIAN_POINT ( 'NONE',  ( -16.81931177881023132, 9.936996059515065483, -121.2732178786172597 ) ) ;
#180818 = DIRECTION ( 'NONE',  ( -3.265361837132813586E-16, 0.9770955615653357240, 0.2128009952263412996 ) ) ;
#180819 = EDGE_LOOP ( 'NONE', ( #84493, #108800, #141220, #138852 ) ) ;
#180820 = CIRCLE ( 'NONE', #39188, 4.049999999999998934 ) ;
#180821 = VECTOR ( 'NONE', #86273, 1000.000000000000114 ) ;
#180822 = EDGE_CURVE ( 'NONE', #55121, #212737, #195810, .T. ) ;
#180823 = CIRCLE ( 'NONE', #197372, 0.09999999999998898659 ) ;
#180824 = CARTESIAN_POINT ( 'NONE',  ( 23.14999999999999858, 70.50000000001223555, -148.9283735034374843 ) ) ;
#180825 = CARTESIAN_POINT ( 'NONE',  ( -20.85000000000000142, 7.120270961697594103, -37.15956304183931991 ) ) ;
#180826 = ADVANCED_FACE ( 'NONE', ( #213814 ), #117151, .F. ) ;
#180827 = CARTESIAN_POINT ( 'NONE',  ( -20.64999999999999858, 1.115600667400684642E-11, -100.5000000000000426 ) ) ;
#180828 = VERTEX_POINT ( 'NONE', #234661 ) ;
#180829 = EDGE_CURVE ( 'NONE', #115361, #170560, #233225, .T. ) ;
#180831 = ORIENTED_EDGE ( 'NONE', *, *, #120706, .F. ) ;
#180830 = DIRECTION ( 'NONE',  ( 0.000000000000000000, -7.086529944415894657E-15, 1.000000000000000000 ) ) ;
#180832 = DIRECTION ( 'NONE',  ( 1.000000000000000000, -0.000000000000000000, -0.000000000000000000 ) ) ;
#180833 = CARTESIAN_POINT ( 'NONE',  ( -18.59999999999999787, 11.75000000001115552, -155.2500000000000284 ) ) ;
#180834 = CARTESIAN_POINT ( 'NONE',  ( -21.05000000000000071, 76.00000000001195133, -103.0231074845243171 ) ) ;
#180835 = EDGE_CURVE ( 'NONE', #74064, #38688, #252862, .T. ) ;
#180836 = CARTESIAN_POINT ( 'NONE',  ( -21.04999999999994387, 67.75000000001119815, -30.12310748452479459 ) ) ;
#180837 = CARTESIAN_POINT ( 'NONE',  ( -18.59999999999999787, 68.97833521811179480, -99.18954208262705663 ) ) ;
#180838 = DIRECTION ( 'NONE',  ( 0.000000000000000000, 0.3848449534832868446, 0.9229812358755983270 ) ) ;
#180839 = ORIENTED_EDGE ( 'NONE', *, *, #6371, .T. ) ;
#180840 = SPHERICAL_SURFACE ( 'NONE', #225799, 0.1000000000000000056 ) ;
#180841 = VECTOR ( 'NONE', #131824, 1000.000000000000000 ) ;
#180842 = DIRECTION ( 'NONE',  ( -1.000000000000000000, 0.000000000000000000, -0.000000000000000000 ) ) ;
#180843 = CARTESIAN_POINT ( 'NONE',  ( -21.05000000000000071, 76.00000000001216449, -140.8231074845242574 ) ) ;
#180844 = AXIS2_PLACEMENT_3D ( 'NONE', #125164, #6476, #26065 ) ;
#180845 = EDGE_CURVE ( 'NONE', #227113, #23245, #203968, .T. ) ;
#180846 = CARTESIAN_POINT ( 'NONE',  ( 22.59999999999999432, 11.45898712536580177, -198.4011321578509524 ) ) ;
#180847 = CARTESIAN_POINT ( 'NONE',  ( 20.97217846901851956, 67.12455827530190788, -61.02187980058715766 ) ) ;
#180848 = ORIENTED_EDGE ( 'NONE', *, *, #190693, .T. ) ;
#180849 = ORIENTED_EDGE ( 'NONE', *, *, #50257, .F. ) ;
#180850 = LINE ( 'NONE', #202967, #54079 ) ;
#180851 = CIRCLE ( 'NONE', #97417, 0.09999999999999939493 ) ;
#180852 = LINE ( 'NONE', #199123, #146781 ) ;
#180853 = DIRECTION ( 'NONE',  ( 0.000000000000000000, -0.8814952561688430555, 0.4721928772777346239 ) ) ;
#180854 = AXIS2_PLACEMENT_3D ( 'NONE', #168946, #30703, #8547 ) ;
#180855 = DIRECTION ( 'NONE',  ( 0.000000000000000000, 0.000000000000000000, -1.000000000000000000 ) ) ;
#180856 = EDGE_CURVE ( 'NONE', #115854, #116101, #249946, .T. ) ;
#180857 = ORIENTED_EDGE ( 'NONE', *, *, #69577, .T. ) ;
#180858 = DIRECTION ( 'NONE',  ( -1.000000000000000000, 0.000000000000000000, 0.000000000000000000 ) ) ;
#180859 = AXIS2_PLACEMENT_3D ( 'NONE', #137545, #97108, #177989 ) ;
#180861 = VECTOR ( 'NONE', #158636, 1000.000000000000000 ) ;
#180860 = CARTESIAN_POINT ( 'NONE',  ( -0.8999999999999437339, 67.75000000001118394, -7.423107484524793520 ) ) ;
#180862 = CARTESIAN_POINT ( 'NONE',  ( -18.59999999999999787, 80.78317333349157536, -192.9003134612049166 ) ) ;
#180863 = TOROIDAL_SURFACE ( 'NONE', #101716, 0.2000000000000000111, 0.1000000000000000056 ) ;
#180864 = VECTOR ( 'NONE', #169240, 1000.000000000000000 ) ;
#180865 = CARTESIAN_POINT ( 'NONE',  ( 23.14999999999999858, 76.00000000001126921, -203.5231074845248997 ) ) ;
#180866 = AXIS2_PLACEMENT_3D ( 'NONE', #19027, #80248, #20337 ) ;
#180867 = VERTEX_POINT ( 'NONE', #144529 ) ;
#180868 = LINE ( 'NONE', #219978, #194216 ) ;
#180869 = ORIENTED_EDGE ( 'NONE', *, *, #73637, .F. ) ;
#180870 = DIRECTION ( 'NONE',  ( 1.000000000000000000, 0.000000000000000000, 0.000000000000000000 ) ) ;
#180871 = CARTESIAN_POINT ( 'NONE',  ( -21.65000000000000213, 65.95000000001152785, -48.67310748452439384 ) ) ;
#180873 = VECTOR ( 'NONE', #186295, 1000.000000000000000 ) ;
#180872 = CARTESIAN_POINT ( 'NONE',  ( -21.13435531349824004, 10.19512217334964888, -228.0085169999992161 ) ) ;
#180874 = DIRECTION ( 'NONE',  ( 0.000000000000000000, 0.000000000000000000, -1.000000000000000000 ) ) ;
#180875 = DIRECTION ( 'NONE',  ( 0.000000000000000000, 0.9998779222360102414, 0.01562499999996356907 ) ) ;
#180876 = DIRECTION ( 'NONE',  ( -1.000000000000000000, -0.000000000000000000, 0.000000000000000000 ) ) ;
#180877 = CYLINDRICAL_SURFACE ( 'NONE', #176770, 0.1000000000000026007 ) ;
#180878 = CARTESIAN_POINT ( 'NONE',  ( -18.59999999999999787, 64.35000000001205933, -124.3731074845243825 ) ) ;
#180879 = CIRCLE ( 'NONE', #55949, 0.09999999999999847899 ) ;
#180880 = CARTESIAN_POINT ( 'NONE',  ( -20.64999999999999858, 1.925233644870967487, -87.76975646687391475 ) ) ;
#180881 = CARTESIAN_POINT ( 'NONE',  ( -23.25000000000000000, 87.75000000001212186, -133.4231074845242233 ) ) ;
#180882 = CARTESIAN_POINT ( 'NONE',  ( 20.94999999999999929, -8.999999999988842703, -90.60603087734760663 ) ) ;
#180883 = AXIS2_PLACEMENT_3D ( 'NONE', #230090, #110140, #16206 ) ;
#180884 = DIRECTION ( 'NONE',  ( 1.000000000000000000, 0.000000000000000000, 0.000000000000000000 ) ) ;
#180885 = CIRCLE ( 'NONE', #176619, 0.09999999999999939493 ) ;
#180886 = EDGE_CURVE ( 'NONE', #68947, #145361, #12456, .T. ) ;
#180887 = CIRCLE ( 'NONE', #68460, 14.20833333333333748 ) ;
#180888 = ORIENTED_EDGE ( 'NONE', *, *, #50248, .F. ) ;
#180889 = CARTESIAN_POINT ( 'NONE',  ( -21.14999999999994174, 83.90000000001120384, -34.77310748452479316 ) ) ;
#180890 = DIRECTION ( 'NONE',  ( 1.000000000000000000, 0.000000000000000000, 0.000000000000000000 ) ) ;
#180891 = EDGE_CURVE ( 'NONE', #157279, #48836, #123710, .T. ) ;
#180892 = ORIENTED_EDGE ( 'NONE', *, *, #58639, .F. ) ;
#180893 = CARTESIAN_POINT ( 'NONE',  ( -22.42253884134832020, 0.001932351146464880492, -55.35039430265162252 ) ) ;
#180894 = CARTESIAN_POINT ( 'NONE',  ( -17.27223548804059661, 10.34539739140874381, -189.6336061792289627 ) ) ;
#180895 = ADVANCED_FACE ( 'NONE', ( #184956 ), #221493, .F. ) ;
#180896 = ORIENTED_EDGE ( 'NONE', *, *, #168346, .F. ) ;
#180898 = EDGE_CURVE ( 'NONE', #35141, #7738, #45755, .T. ) ;
#180897 = DIRECTION ( 'NONE',  ( 0.000000000000000000, 1.483188571960168804E-13, -1.000000000000000000 ) ) ;
#180899 = CARTESIAN_POINT ( 'NONE',  ( 20.94999999999999574, 87.39257802171779588, -133.4491579046922709 ) ) ;
#180900 = ORIENTED_EDGE ( 'NONE', *, *, #41796, .F. ) ;
#180901 = VECTOR ( 'NONE', #237506, 1000.000000000000000 ) ;
#180902 = ORIENTED_EDGE ( 'NONE', *, *, #128684, .F. ) ;
#180903 = CARTESIAN_POINT ( 'NONE',  ( 21.05000000000000071, 69.35000000001187459, -93.00608031408432907 ) ) ;
#180904 = AXIS2_PLACEMENT_3D ( 'NONE', #32377, #191453, #55707 ) ;
#180905 = ORIENTED_EDGE ( 'NONE', *, *, #3437, .T. ) ;
#180906 = EDGE_CURVE ( 'NONE', #140623, #24438, #220725, .T. ) ;
#180907 = DIRECTION ( 'NONE',  ( 0.7071359030027593029, -0.7070776581709197206, 0.000000000000000000 ) ) ;
#180908 = DIRECTION ( 'NONE',  ( 0.000000000000000000, 0.000000000000000000, 1.000000000000000000 ) ) ;
#180910 = CARTESIAN_POINT ( 'NONE',  ( 21.08198257630413508, 34.00199500830718335, -243.7980364803085820 ) ) ;
#180909 = PRODUCT_DEFINITION_CONTEXT ( 'detailed design', #250762, 'design' ) ;
#180911 = EDGE_CURVE ( 'NONE', #43643, #20715, #116666, .T. ) ;
#180912 = CARTESIAN_POINT ( 'NONE',  ( 21.05000000000000071, -11.29603075033528548, -3.047899159663867152 ) ) ;
#180913 = FACE_OUTER_BOUND ( 'NONE', #25877, .T. ) ;
#180914 = DIRECTION ( 'NONE',  ( 0.000000000000000000, -6.982962677686266711E-15, 1.000000000000000000 ) ) ;
#180915 = CARTESIAN_POINT ( 'NONE',  ( 20.04142135623730070, 11.65000000001115943, -58.15000000000000568 ) ) ;
#180916 = LINE ( 'NONE', #195366, #141359 ) ;
#180918 = ORIENTED_EDGE ( 'NONE', *, *, #96816, .F. ) ;
#180917 = CARTESIAN_POINT ( 'NONE',  ( -18.50000000000000355, -9.399999999988818189, -40.79725975966328377 ) ) ;
#180919 = EDGE_LOOP ( 'NONE', ( #231764, #16489, #115774, #186794 ) ) ;
#180921 = DIRECTION ( 'NONE',  ( -0.000000000000000000, 1.000000000000000000, -0.000000000000000000 ) ) ;
#180920 = CARTESIAN_POINT ( 'NONE',  ( -18.59999999999999787, 1.835341550235567887, -179.0551512925629538 ) ) ;
#180923 = ORIENTED_EDGE ( 'NONE', *, *, #250813, .F. ) ;
#180922 = CARTESIAN_POINT ( 'NONE',  ( 21.11701782572533048, 10.72160911601861244, -146.2450374295112283 ) ) ;
#180924 = VERTEX_POINT ( 'NONE', #2452 ) ;
#180925 = CARTESIAN_POINT ( 'NONE',  ( -23.15000000000000213, -7.274670914976377745, -212.7102428701827250 ) ) ;
#180926 = CARTESIAN_POINT ( 'NONE',  ( 21.00000000000000000, 61.05385884576949707, -221.3836188041226762 ) ) ;
#180927 = AXIS2_PLACEMENT_3D ( 'NONE', #190910, #171363, #93053 ) ;
#180929 = EDGE_CURVE ( 'NONE', #125507, #98827, #81968, .T. ) ;
#180928 = LINE ( 'NONE', #23158, #163219 ) ;
#180930 = DIRECTION ( 'NONE',  ( 0.000000000000000000, -0.8814952561688429444, 0.4721928772777345684 ) ) ;
#180931 = EDGE_CURVE ( 'NONE', #142111, #102643, #84521, .T. ) ;
#180932 = EDGE_CURVE ( 'NONE', #132836, #215608, #65001, .T. ) ;
#180933 = DIRECTION ( 'NONE',  ( 0.000000000000000000, 0.000000000000000000, -1.000000000000000000 ) ) ;
#180934 = DIRECTION ( 'NONE',  ( 0.000000000000000000, -0.8814952561688437216, 0.4721928772777334582 ) ) ;
#180935 = FACE_OUTER_BOUND ( 'NONE', #71952, .T. ) ;
#180936 = ORIENTED_EDGE ( 'NONE', *, *, #202981, .F. ) ;
#180937 = ORIENTED_EDGE ( 'NONE', *, *, #243049, .T. ) ;
#180938 = CARTESIAN_POINT ( 'NONE',  ( 18.39999999999998082, 58.57934086597919077, -223.9244941873113817 ) ) ;
#180939 = CIRCLE ( 'NONE', #114293, 0.09999999999998898659 ) ;
#180940 = ORIENTED_EDGE ( 'NONE', *, *, #174, .F. ) ;
#180941 = CARTESIAN_POINT ( 'NONE',  ( -21.05000000000000071, 7.939498413483247141, -209.7295111514051200 ) ) ;
#180942 = ORIENTED_EDGE ( 'NONE', *, *, #153350, .T. ) ;
#180943 = DIRECTION ( 'NONE',  ( 0.000000000000000000, -6.982962677686266711E-15, 1.000000000000000000 ) ) ;
#180944 = CIRCLE ( 'NONE', #80963, 0.5000000000000004441 ) ;
#180945 = AXIS2_PLACEMENT_3D ( 'NONE', #170053, #207877, #249555 ) ;
#180946 = EDGE_CURVE ( 'NONE', #155807, #225917, #159008, .T. ) ;
#180947 = CARTESIAN_POINT ( 'NONE',  ( -12.25000000000000178, 48.12247445990688988, -234.1702647910923361 ) ) ;
#180948 = STYLED_ITEM ( 'NONE', ( #224958 ), #13839 ) ;
#180949 = ADVANCED_FACE ( 'NONE', ( #225343 ), #128847, .T. ) ;
#180950 = CARTESIAN_POINT ( 'NONE',  ( -11.60000000000000320, -8.279289321881350361, 15.00000000000000355 ) ) ;
#180951 = CARTESIAN_POINT ( 'NONE',  ( -16.90202395485723486, 22.93886501610722917, -230.8959756691647272 ) ) ;
#180952 = VERTEX_POINT ( 'NONE', #186252 ) ;
#180953 = DIRECTION ( 'NONE',  ( -1.000000000000000000, 0.000000000000000000, 0.000000000000000000 ) ) ;
#180954 = ORIENTED_EDGE ( 'NONE', *, *, #188389, .F. ) ;
#180955 = CARTESIAN_POINT ( 'NONE',  ( -20.54999999999999716, 76.00000000001195133, -103.0231074845243171 ) ) ;
#180956 = DIRECTION ( 'NONE',  ( -1.000000000000000000, 0.000000000000000000, 0.000000000000000000 ) ) ;
#180957 = ADVANCED_FACE ( 'NONE', ( #50552 ), #167999, .F. ) ;
#180959 = AXIS2_PLACEMENT_3D ( 'NONE', #40501, #179986, #102981 ) ;
#180958 = DIRECTION ( 'NONE',  ( 0.7071067811865475727, -0.7071067811865475727, -4.937700262164531476E-15 ) ) ;
#180960 = CARTESIAN_POINT ( 'NONE',  ( 21.15000000000005542, 65.15000000001120384, -3.023107484524792277 ) ) ;
#180961 = ORIENTED_EDGE ( 'NONE', *, *, #239080, .T. ) ;
#180962 = LINE ( 'NONE', #66141, #65035 ) ;
#180964 = ORIENTED_EDGE ( 'NONE', *, *, #30682, .T. ) ;
#180963 = CIRCLE ( 'NONE', #22767, 0.1000000000000028644 ) ;
#180967 = ORIENTED_EDGE ( 'NONE', *, *, #227998, .F. ) ;
#180966 = DIRECTION ( 'NONE',  ( -1.000000000000000000, -0.000000000000000000, 0.000000000000000000 ) ) ;
#180965 = DIRECTION ( 'NONE',  ( -1.000000000000000000, 0.000000000000000000, 0.000000000000000000 ) ) ;
#180968 = DIRECTION ( 'NONE',  ( 0.000000000000000000, 0.000000000000000000, 1.000000000000000000 ) ) ;
#180970 = ORIENTED_EDGE ( 'NONE', *, *, #251587, .F. ) ;
#180969 = AXIS2_PLACEMENT_3D ( 'NONE', #165911, #68069, #146309 ) ;
#180971 = CIRCLE ( 'NONE', #139431, 3.999999999999994671 ) ;
#180972 = CARTESIAN_POINT ( 'NONE',  ( -23.15000000000000213, 76.00000000001143974, -38.12310748452432563 ) ) ;
#180973 = ORIENTED_EDGE ( 'NONE', *, *, #141925, .F. ) ;
#180975 = CARTESIAN_POINT ( 'NONE',  ( 18.39999999999999147, 67.17743825834520521, -60.27310748452438816 ) ) ;
#180974 = CIRCLE ( 'NONE', #56036, 0.09999999999999939493 ) ;
#180976 = PLANE ( 'NONE',  #232161 ) ;
#180977 = DIRECTION ( 'NONE',  ( 0.000000000000000000, 0.000000000000000000, -1.000000000000000000 ) ) ;
#180979 = ORIENTED_EDGE ( 'NONE', *, *, #150705, .T. ) ;
#180978 = CARTESIAN_POINT ( 'NONE',  ( -18.59999999999999787, 9.105964803472822666, -245.3658845043482586 ) ) ;
#180980 = VECTOR ( 'NONE', #72834, 1000.000000000000114 ) ;
#180981 = AXIS2_PLACEMENT_3D ( 'NONE', #111191, #190757, #12114 ) ;
#180982 = ADVANCED_FACE ( 'NONE', ( #107990 ), #62513, .T. ) ;
#180983 = DIRECTION ( 'NONE',  ( 0.000000000000000000, 0.4088369013363281068, -0.9126074666063770380 ) ) ;
#180984 = CIRCLE ( 'NONE', #18485, 0.1000000000000072220 ) ;
#180985 = VERTEX_POINT ( 'NONE', #7602 ) ;
#180986 = EDGE_CURVE ( 'NONE', #133804, #98230, #237300, .T. ) ;
#180987 = DIRECTION ( 'NONE',  ( -1.000000000000000000, 0.000000000000000000, -0.000000000000000000 ) ) ;
#180988 = CARTESIAN_POINT ( 'NONE',  ( -16.94389599337536012, 9.991197989767877985, -188.3923551982015852 ) ) ;
#180989 = VECTOR ( 'NONE', #194463, 1000.000000000000114 ) ;
#180990 = CARTESIAN_POINT ( 'NONE',  ( -18.39999999999999503, -9.499999999988849808, -140.9221498493304239 ) ) ;
#180991 = EDGE_LOOP ( 'NONE', ( #44762, #214603, #82140 ) ) ;
#180992 = LINE ( 'NONE', #205659, #142791 ) ;
#180993 = VERTEX_POINT ( 'NONE', #51839 ) ;
#180994 = FACE_OUTER_BOUND ( 'NONE', #190474, .T. ) ;
#180995 = EDGE_CURVE ( 'NONE', #178394, #176, #237670, .T. ) ;
#180996 = AXIS2_PLACEMENT_3D ( 'NONE', #36026, #155984, #212098 ) ;
#180997 = EDGE_CURVE ( 'NONE', #50892, #97606, #166776, .T. ) ;
#180998 = DIRECTION ( 'NONE',  ( 1.000000000000000000, 0.000000000000000000, 0.000000000000000000 ) ) ;
#180999 = FACE_OUTER_BOUND ( 'NONE', #10349, .T. ) ;
#181000 = EDGE_LOOP ( 'NONE', ( #255291, #87630, #30264 ) ) ;
#181001 = LINE ( 'NONE', #234540, #42114 ) ;
#181002 = CIRCLE ( 'NONE', #139266, 0.09999999999999938105 ) ;
#181003 = ADVANCED_FACE ( 'NONE', ( #8890 ), #224969, .F. ) ;
#181004 = CIRCLE ( 'NONE', #68573, 0.1999999999999997335 ) ;
#181005 = FACE_BOUND ( 'NONE', #88877, .T. ) ;
#181006 = DIRECTION ( 'NONE',  ( 0.000000000000000000, 0.1350103645451876666, -0.9908441862701600211 ) ) ;
#181007 = ORIENTED_EDGE ( 'NONE', *, *, #81664, .T. ) ;
#181008 = DIRECTION ( 'NONE',  ( -0.000000000000000000, -6.982962677686266711E-15, 1.000000000000000000 ) ) ;
#181009 = DIRECTION ( 'NONE',  ( -0.000000000000000000, -1.000000000000000000, -8.609265936414532828E-15 ) ) ;
#181010 = ORIENTED_EDGE ( 'NONE', *, *, #223848, .F. ) ;
#181011 = DIRECTION ( 'NONE',  ( 0.000000000000000000, 0.2128009952263403282, -0.9770955615653358350 ) ) ;
#181012 = ADVANCED_FACE ( 'NONE', ( #68880 ), #145815, .T. ) ;
#181013 = ORIENTED_EDGE ( 'NONE', *, *, #248678, .T. ) ;
#181014 = EDGE_CURVE ( 'NONE', #57631, #7849, #95984, .T. ) ;
#181015 = ORIENTED_EDGE ( 'NONE', *, *, #123579, .F. ) ;
#181016 = DIRECTION ( 'NONE',  ( 0.000000000000000000, 0.000000000000000000, -1.000000000000000000 ) ) ;
#181017 = ORIENTED_EDGE ( 'NONE', *, *, #111469, .F. ) ;
#181019 = ORIENTED_EDGE ( 'NONE', *, *, #72754, .F. ) ;
#181018 = LINE ( 'NONE', #2347, #172198 ) ;
#181020 = EDGE_CURVE ( 'NONE', #258105, #22177, #71077, .T. ) ;
#181023 = VERTEX_POINT ( 'NONE', #188803 ) ;
#181022 = VERTEX_POINT ( 'NONE', #147097 ) ;
#181021 = DIRECTION ( 'NONE',  ( 1.000000000000000000, 0.000000000000000000, 0.000000000000000000 ) ) ;
#181024 = VECTOR ( 'NONE', #195371, 1000.000000000000000 ) ;
#181025 = DIRECTION ( 'NONE',  ( 0.000000000000000000, -6.982962677686266711E-15, 1.000000000000000000 ) ) ;
#181026 = CARTESIAN_POINT ( 'NONE',  ( -20.87600722750343252, 65.66887361445283489, -30.43298459182692994 ) ) ;
#181027 = AXIS2_PLACEMENT_3D ( 'NONE', #121342, #157910, #142141 ) ;
#181028 = CARTESIAN_POINT ( 'NONE',  ( 18.59999999999999787, -1.362429037182151470, -74.88888124792120493 ) ) ;
#181030 = DIRECTION ( 'NONE',  ( 0.000000000000000000, -0.3738317757009718689, 0.9274965247785342815 ) ) ;
#181029 = DIRECTION ( 'NONE',  ( 0.000000000000000000, 0.000000000000000000, 1.000000000000000000 ) ) ;
#181031 = CARTESIAN_POINT ( 'NONE',  ( 18.39999999999999503, 13.78091005366907140, -222.8171174488881832 ) ) ;
#181032 = AXIS2_PLACEMENT_3D ( 'NONE', #164896, #89198, #47491 ) ;
#181033 = EDGE_CURVE ( 'NONE', #110576, #101690, #133432, .T. ) ;
#181034 = CARTESIAN_POINT ( 'NONE',  ( -22.39999999999999858, 25.97741635855165754, -254.4468634167653249 ) ) ;
#181035 = CARTESIAN_POINT ( 'NONE',  ( 23.14999999999999503, 38.43293829866423295, -234.5626268121764895 ) ) ;
#181037 = CARTESIAN_POINT ( 'NONE',  ( 23.14999999999999503, 11.65000000001116298, -194.0851942293460013 ) ) ;
#181036 = CARTESIAN_POINT ( 'NONE',  ( -23.15000000000000213, 11.65000000001115588, -45.65000000000000568 ) ) ;
#181038 = ORIENTED_EDGE ( 'NONE', *, *, #53541, .F. ) ;
#181040 = ORIENTED_EDGE ( 'NONE', *, *, #241356, .T. ) ;
#181039 = AXIS2_PLACEMENT_3D ( 'NONE', #37289, #56795, #136333 ) ;
#181041 = EDGE_CURVE ( 'NONE', #4950, #76541, #79232, .T. ) ;
#181042 = DIRECTION ( 'NONE',  ( 1.000000000000000000, -2.952720810173289112E-16, -2.061873921506763405E-30 ) ) ;
#181043 = VECTOR ( 'NONE', #210592, 1000.000000000000000 ) ;
#181045 = VERTEX_POINT ( 'NONE', #88395 ) ;
#181044 = CARTESIAN_POINT ( 'NONE',  ( -23.15000000000000213, 11.75000000001115552, -55.25000000000004974 ) ) ;
#181046 = ORIENTED_EDGE ( 'NONE', *, *, #247643, .T. ) ;
#181047 = CARTESIAN_POINT ( 'NONE',  ( 23.15000000000000213, -6.438379425586758131, -212.1495692908769684 ) ) ;
#181048 = ORIENTED_EDGE ( 'NONE', *, *, #89382, .T. ) ;
#181049 = CARTESIAN_POINT ( 'NONE',  ( 22.39999999999999503, 76.10000000001222986, -148.1726782920690937 ) ) ;
#181050 = ADVANCED_FACE ( 'NONE', ( #130107 ), #49290, .T. ) ;
#181051 = CIRCLE ( 'NONE', #6229, 0.09999999999998902822 ) ;
#181052 = VECTOR ( 'NONE', #134366, 1000.000000000000000 ) ;
#181053 = ORIENTED_EDGE ( 'NONE', *, *, #180995, .F. ) ;
#181054 = CIRCLE ( 'NONE', #201696, 0.09999999999999939493 ) ;
#181055 = FACE_OUTER_BOUND ( 'NONE', #159147, .T. ) ;
#181056 = FACE_OUTER_BOUND ( 'NONE', #80236, .T. ) ;
#181058 = ORIENTED_EDGE ( 'NONE', *, *, #184387, .T. ) ;
#181057 = VERTEX_POINT ( 'NONE', #250066 ) ;
#181059 = ORIENTED_EDGE ( 'NONE', *, *, #5359, .T. ) ;
#181060 = CARTESIAN_POINT ( 'NONE',  ( 21.14999999999999503, 64.25000000001165290, -69.52310748452438816 ) ) ;
#181061 = ORIENTED_EDGE ( 'NONE', *, *, #224420, .T. ) ;
#181062 = ORIENTED_EDGE ( 'NONE', *, *, #70450, .T. ) ;
#181063 = DIRECTION ( 'NONE',  ( 0.000000000000000000, 0.000000000000000000, -1.000000000000000000 ) ) ;
#181065 = VERTEX_POINT ( 'NONE', #32333 ) ;
#181064 = CARTESIAN_POINT ( 'NONE',  ( 18.33996824403462611, -9.569639859420533412, -107.3190656375166725 ) ) ;
#181066 = ADVANCED_FACE ( 'NONE', ( #71451 ), #125059, .T. ) ;
#181067 = VECTOR ( 'NONE', #224462, 1000.000000000000114 ) ;
#181069 = CARTESIAN_POINT ( 'NONE',  ( -21.05000000000000071, 18.18127959618848166, -237.5711165786817389 ) ) ;
#181068 = DIRECTION ( 'NONE',  ( 0.000000000000000000, 6.982962677686267499E-15, -1.000000000000000000 ) ) ;
#181070 = DIRECTION ( 'NONE',  ( 0.000000000000000000, 0.2128009952263604232, -0.9770955615653316162 ) ) ;
#181071 = DIRECTION ( 'NONE',  ( 0.000000000000000000, 0.000000000000000000, -1.000000000000000000 ) ) ;
#181072 = DIRECTION ( 'NONE',  ( -1.000000000000000000, -2.952720810173289112E-16, 0.000000000000000000 ) ) ;
#181073 = ORIENTED_EDGE ( 'NONE', *, *, #174242, .F. ) ;
#181074 = ORIENTED_EDGE ( 'NONE', *, *, #17392, .F. ) ;
#181075 = CARTESIAN_POINT ( 'NONE',  ( -20.94999999999999929, 28.42524210734032053, -258.3567845160494585 ) ) ;
#181076 = TOROIDAL_SURFACE ( 'NONE', #118125, 0.6000000000000013101, 0.1000000000000000056 ) ;
#181077 = CARTESIAN_POINT ( 'NONE',  ( -20.94999999999999929, 77.83534155023598089, -57.96795619196132776 ) ) ;
#181078 = FACE_OUTER_BOUND ( 'NONE', #233364, .T. ) ;
#181079 = ORIENTED_EDGE ( 'NONE', *, *, #151316, .F. ) ;
#181080 = DIRECTION ( 'NONE',  ( 0.000000000000000000, 0.9651348961777157509, -0.2617529984165031243 ) ) ;
#181081 = CIRCLE ( 'NONE', #176798, 0.1000000000000028227 ) ;
#181082 = CIRCLE ( 'NONE', #68641, 0.1000000000000028644 ) ;
#181083 = DIRECTION ( 'NONE',  ( 0.000000000000000000, 0.000000000000000000, -1.000000000000000000 ) ) ;
#181084 = CARTESIAN_POINT ( 'NONE',  ( -23.25000000000000000, 74.08971962618080909, -190.8917396293254285 ) ) ;
#181085 = EDGE_LOOP ( 'NONE', ( #188631, #35267, #119173, #87792 ) ) ;
#181086 = ORIENTED_EDGE ( 'NONE', *, *, #104444, .T. ) ;
#181087 = DIRECTION ( 'NONE',  ( -1.000000000000000000, 0.000000000000000000, 0.000000000000000000 ) ) ;
#181088 = ADVANCED_FACE ( 'NONE', ( #191409 ), #74033, .F. ) ;
#181089 = CARTESIAN_POINT ( 'NONE',  ( -18.50000000000000000, 9.150000000000002132, -21.15000000000000213 ) ) ;
#181090 = ORIENTED_EDGE ( 'NONE', *, *, #199747, .T. ) ;
#181091 = CARTESIAN_POINT ( 'NONE',  ( 23.24999999999999645, 76.00000000001213607, -136.5231074845243313 ) ) ;
#181092 = ORIENTED_EDGE ( 'NONE', *, *, #815, .T. ) ;
#181093 = CARTESIAN_POINT ( 'NONE',  ( 23.04999999999999716, 8.822561741677553471, -121.3500000000000227 ) ) ;
#181094 = DIRECTION ( 'NONE',  ( -1.000000000000000000, 0.000000000000000000, 0.000000000000000000 ) ) ;
#181096 = CARTESIAN_POINT ( 'NONE',  ( -20.94403535211772294, 68.04082873524789932, -224.1991862745062178 ) ) ;
#181095 = CARTESIAN_POINT ( 'NONE',  ( -23.25000000000000000, -9.599999999988845900, -157.6060308773475924 ) ) ;
#181097 = CARTESIAN_POINT ( 'NONE',  ( 22.43288208788031568, 0.004899854896538679595, -55.35034815628097249 ) ) ;
#181098 = CARTESIAN_POINT ( 'NONE',  ( -22.39999999999999858, 64.25000000001237765, -170.1231074845244393 ) ) ;
#181099 = ORIENTED_EDGE ( 'NONE', *, *, #74557, .F. ) ;
#181100 = CARTESIAN_POINT ( 'NONE',  ( -18.47140463609788341, 85.67147468523253906, -62.85034702625018355 ) ) ;
#181101 = EDGE_CURVE ( 'NONE', #218845, #55374, #120979, .T. ) ;
#181102 = TOROIDAL_SURFACE ( 'NONE', #164533, 4.150000000000000355, 0.1000000000000000056 ) ;
#181104 = ORIENTED_EDGE ( 'NONE', *, *, #70228, .T. ) ;
#181103 = ORIENTED_EDGE ( 'NONE', *, *, #115016, .T. ) ;
#181105 = ORIENTED_EDGE ( 'NONE', *, *, #178039, .F. ) ;
#181106 = VERTEX_POINT ( 'NONE', #255140 ) ;
#181107 = LINE ( 'NONE', #186230, #41951 ) ;
#181108 = DIRECTION ( 'NONE',  ( 0.000000000000000000, 1.000000000000000000, 0.000000000000000000 ) ) ;
#181109 = VECTOR ( 'NONE', #273, 1000.000000000000000 ) ;
#181111 = FACE_OUTER_BOUND ( 'NONE', #246566, .T. ) ;
#181110 =( BOUNDED_SURFACE ( )  B_SPLINE_SURFACE ( 3, 2, ( 
 ( #134097, #10334, #252759 ),
 ( #234483, #75452, #15468 ),
 ( #190247, #152425, #93700 ),
 ( #135378, #211087, #74178 ),
 ( #35053, #230658, #154986 ),
 ( #55821, #70325, #151119 ),
 ( #214930, #14194, #113267 ),
 ( #115832, #32485, #173296 ),
 ( #153735, #149846, #131546 ),
 ( #231952, #229377, #53297 ) ),
 .UNSPECIFIED., .F., .F., .F. ) 
 B_SPLINE_SURFACE_WITH_KNOTS ( ( 4, 2, 2, 2, 4 ),
 ( 3, 3 ),
 ( 0.0001701955120502369480, 0.0002247052511886134046, 0.0002792149903269898611, 0.0003882344686037427200, 0.0006062734251572484377 ),
 ( 0.000000000000000000, 1.000000000000000000 ),
 .UNSPECIFIED. ) 
 GEOMETRIC_REPRESENTATION_ITEM ( )  RATIONAL_B_SPLINE_SURFACE ( (
 ( 1.000000000000000000, 0.2966190024560417804, 1.000000000000000000),
 ( 1.000000000000000000, 0.2964522492711155199, 1.000000000000000000),
 ( 1.000000000000000000, 0.3059923531884136128, 1.000000000000000000),
 ( 1.000000000000000000, 0.3355751146944749297, 1.000000000000000000),
 ( 1.000000000000000000, 0.3550672384963041162, 1.000000000000000000),
 ( 1.000000000000000000, 0.4157034672181008084, 1.000000000000000000),
 ( 1.000000000000000000, 0.4588031877652027912, 1.000000000000000000),
 ( 1.000000000000000000, 0.5771441759664686089, 1.000000000000000000),
 ( 1.000000000000000000, 0.6469377121768989936, 1.000000000000000000),
 ( 1.000000000000000000, 0.7071067811865475727, 1.000000000000000000) ) ) 
 REPRESENTATION_ITEM ( '' )  SURFACE ( )  );
#181112 = CARTESIAN_POINT ( 'NONE',  ( -20.85000000000000142, -1.835859311443635233, -45.00443916879852679 ) ) ;
#181113 = CARTESIAN_POINT ( 'NONE',  ( 0.9000000000000547562, 67.75000000001118394, -7.423107484524793520 ) ) ;
#181115 = CARTESIAN_POINT ( 'NONE',  ( 21.04999999999999716, 59.07346110239164716, -225.8107669182993789 ) ) ;
#181114 = CARTESIAN_POINT ( 'NONE',  ( 20.19326291201701196, 10.15606098790381751, -7.761861807602776331 ) ) ;
#181117 = ORIENTED_EDGE ( 'NONE', *, *, #174461, .F. ) ;
#181116 = DIRECTION ( 'NONE',  ( 4.336808689942128177E-15, 0.8660254037844330455, -0.5000000000000096589 ) ) ;
#181118 = FACE_OUTER_BOUND ( 'NONE', #231119, .T. ) ;
#181119 = ORIENTED_EDGE ( 'NONE', *, *, #76319, .T. ) ;
#181120 = CARTESIAN_POINT ( 'NONE',  ( 21.30740335185486245, 33.88803232685230427, -243.6079558105722356 ) ) ;
#181121 = ORIENTED_EDGE ( 'NONE', *, *, #184429, .F. ) ;
#181122 = ORIENTED_EDGE ( 'NONE', *, *, #219245, .T. ) ;
#181123 = DIRECTION ( 'NONE',  ( 1.000000000000000000, 0.000000000000000000, 0.000000000000000000 ) ) ;
#181124 = CARTESIAN_POINT ( 'NONE',  ( -21.04999999999999716, 76.01771943332158799, -209.9641921729950127 ) ) ;
#181125 = DIRECTION ( 'NONE',  ( 0.000000000000000000, -0.9915357197604971473, 0.1298341882519111479 ) ) ;
#181126 = AXIS2_PLACEMENT_3D ( 'NONE', #115207, #153097, #193480 ) ;
#181127 = AXIS2_PLACEMENT_3D ( 'NONE', #60338, #115193, #76059 ) ;
#181128 = CARTESIAN_POINT ( 'NONE',  ( -18.50000000000000000, 64.35000000001259934, -191.3731074845244393 ) ) ;
#181129 = ORIENTED_EDGE ( 'NONE', *, *, #239546, .F. ) ;
#181130 = EDGE_LOOP ( 'NONE', ( #77096, #142105, #208773, #113595, #110477 ) ) ;
#181131 = LINE ( 'NONE', #81974, #40692 ) ;
#181132 = ORIENTED_EDGE ( 'NONE', *, *, #17536, .F. ) ;
#181133 = LINE ( 'NONE', #178580, #181230 ) ;
#181134 = CARTESIAN_POINT ( 'NONE',  ( -16.94389599338512298, 9.991197989766199328, -46.10764480181025249 ) ) ;
#181135 = DIRECTION ( 'NONE',  ( -1.000000000000000000, 0.000000000000000000, 0.000000000000000000 ) ) ;
#181136 = DIRECTION ( 'NONE',  ( 1.000000000000000000, 2.952720810173289112E-16, -0.000000000000000000 ) ) ;
#181137 = DIRECTION ( 'NONE',  ( 1.000000000000000000, 0.000000000000000000, 0.000000000000000000 ) ) ;
#181138 = CARTESIAN_POINT ( 'NONE',  ( -21.05000000000000071, 76.00000000001173817, -73.62310748452429721 ) ) ;
#181139 = DIRECTION ( 'NONE',  ( -0.000000000000000000, 1.000000000000000000, 7.172728831056617961E-15 ) ) ;
#181141 = EDGE_CURVE ( 'NONE', #160519, #59315, #21024, .T. ) ;
#181140 = DIRECTION ( 'NONE',  ( 1.000000000000000000, 0.000000000000000000, 0.000000000000000000 ) ) ;
#181142 = CARTESIAN_POINT ( 'NONE',  ( -22.39999999999999858, 1.115600667400684642E-11, -27.25000000000000355 ) ) ;
#181143 = DIRECTION ( 'NONE',  ( 0.000000000000000000, 0.000000000000000000, -1.000000000000000000 ) ) ;
#181144 = AXIS2_PLACEMENT_3D ( 'NONE', #148276, #89571, #187415 ) ;
#181145 = DIRECTION ( 'NONE',  ( 0.000000000000000000, 0.2128009952263403282, -0.9770955615653358350 ) ) ;
#181146 = VECTOR ( 'NONE', #222926, 1000.000000000000000 ) ;
#181147 = CIRCLE ( 'NONE', #106076, 0.09999999999999967248 ) ;
#181148 = AXIS2_PLACEMENT_3D ( 'NONE', #187024, #13510, #153055 ) ;
#181149 = ORIENTED_EDGE ( 'NONE', *, *, #229601, .F. ) ;
#181150 = ADVANCED_FACE ( 'NONE', ( #213495 ), #252618, .F. ) ;
#181151 = CARTESIAN_POINT ( 'NONE',  ( 21.07928932188134397, 6.328516656404459262, -100.4011048543456468 ) ) ;
#181152 = ORIENTED_EDGE ( 'NONE', *, *, #66914, .T. ) ;
#181153 = DIRECTION ( 'NONE',  ( -0.000000000000000000, -0.8700118002898356018, 0.4930308989875170078 ) ) ;
#181154 = ADVANCED_FACE ( 'NONE', ( #94833 ), #83502, .F. ) ;
#181155 = FACE_OUTER_BOUND ( 'NONE', #217573, .T. ) ;
#181156 = EDGE_LOOP ( 'NONE', ( #181059, #75180, #136744, #129738 ) ) ;
#181157 = CARTESIAN_POINT ( 'NONE',  ( -20.00857864376270001, 66.75000000001260503, -191.1731074845244223 ) ) ;
#181158 = CARTESIAN_POINT ( 'NONE',  ( -18.59999999999999787, 1.162701749949165642, -175.5999999999999659 ) ) ;
#181159 = DIRECTION ( 'NONE',  ( 0.000000000000000000, 6.997203936713175802E-15, -1.000000000000000000 ) ) ;
#181160 = EDGE_CURVE ( 'NONE', #192209, #129105, #33510, .T. ) ;
#181161 = CYLINDRICAL_SURFACE ( 'NONE', #63981, 0.09999999999998898659 ) ;
#181162 = CIRCLE ( 'NONE', #101997, 0.1000000000000028644 ) ;
#181163 = CARTESIAN_POINT ( 'NONE',  ( 23.14999999999999503, 56.15782127605848473, -228.0502772851308748 ) ) ;
#181164 = DIRECTION ( 'NONE',  ( 0.000000000000000000, -0.4088369013363783999, 0.9126074666063545004 ) ) ;
#181165 = AXIS2_PLACEMENT_3D ( 'NONE', #3668, #61080, #182334 ) ;
#181166 = AXIS2_PLACEMENT_3D ( 'NONE', #120939, #21817, #221270 ) ;
#181167 = ORIENTED_EDGE ( 'NONE', *, *, #84670, .F. ) ;
#181168 = DIRECTION ( 'NONE',  ( 0.000000000000000000, 1.000000000000000000, 6.982962677686266711E-15 ) ) ;
#181170 = ORIENTED_EDGE ( 'NONE', *, *, #26916, .T. ) ;
#181169 = LINE ( 'NONE', #217679, #159484 ) ;
#181171 = DIRECTION ( 'NONE',  ( 0.000000000000000000, -0.8660254037844377084, -0.5000000000000016653 ) ) ;
#181172 = DIRECTION ( 'NONE',  ( 1.000000000000000000, 0.000000000000000000, 0.000000000000000000 ) ) ;
#181173 = ADVANCED_FACE ( 'NONE', ( #21418 ), #187608, .T. ) ;
#181174 = FILL_AREA_STYLE_COLOUR ( '', #204536 ) ;
#181175 =( BOUNDED_CURVE ( )  B_SPLINE_CURVE ( 3, ( #176563, #211831, #93144, #256022 ),
 .UNSPECIFIED., .F., .F. ) 
 B_SPLINE_CURVE_WITH_KNOTS ( ( 4, 4 ),
 ( 0.3000847527772381729, 0.5497968875596814797 ),
 .UNSPECIFIED. ) 
 CURVE ( )  GEOMETRIC_REPRESENTATION_ITEM ( )  RATIONAL_B_SPLINE_CURVE ( ( 1.000000000000000000, 0.9948104011409419911, 0.9948104011409419911, 1.000000000000000000 ) ) 
 REPRESENTATION_ITEM ( '' )  );
#181176 = ORIENTED_EDGE ( 'NONE', *, *, #155826, .F. ) ;
#181177 = CARTESIAN_POINT ( 'NONE',  ( -20.85000000000000142, 7.128833340094563376, -233.7327013124401276 ) ) ;
#181178 = CIRCLE ( 'NONE', #76914, 0.1000000000000028644 ) ;
#181179 = TOROIDAL_SURFACE ( 'NONE', #177082, 2.100000000000002309, 0.1000000000000000056 ) ;
#181180 = AXIS2_PLACEMENT_3D ( 'NONE', #84091, #86690, #223639 ) ;
#181181 = CIRCLE ( 'NONE', #218539, 7.791421356237338003 ) ;
#181183 = EDGE_CURVE ( 'NONE', #140297, #76466, #200233, .T. ) ;
#181182 = FACE_OUTER_BOUND ( 'NONE', #240727, .T. ) ;
#181184 = ORIENTED_EDGE ( 'NONE', *, *, #37348, .F. ) ;
#181185 = DIRECTION ( 'NONE',  ( 0.000000000000000000, 0.000000000000000000, -1.000000000000000000 ) ) ;
#181186 = DIRECTION ( 'NONE',  ( -1.000000000000000000, -2.952720810173289112E-16, 0.000000000000000000 ) ) ;
#181187 = CIRCLE ( 'NONE', #60529, 0.1000000000000000472 ) ;
#181188 = DIRECTION ( 'NONE',  ( -1.000000000000000000, -0.000000000000000000, 0.000000000000000000 ) ) ;
#181190 = VERTEX_POINT ( 'NONE', #154842 ) ;
#181189 = STYLED_ITEM ( 'NONE', ( #231555 ), #196328 ) ;
#181191 = EDGE_LOOP ( 'NONE', ( #53546, #212542, #10468, #120539 ) ) ;
#181192 = LINE ( 'NONE', #82033, #197182 ) ;
#181193 = VECTOR ( 'NONE', #137656, 1000.000000000000000 ) ;
#181194 = CARTESIAN_POINT ( 'NONE',  ( 23.14999999999999858, 7.128833340094563376, -233.7327013124401276 ) ) ;
#181195 = AXIS2_PLACEMENT_3D ( 'NONE', #100077, #179662, #80507 ) ;
#181196 = ADVANCED_FACE ( 'NONE', ( #76554 ), #113122, .F. ) ;
#181197 = FACE_OUTER_BOUND ( 'NONE', #79610, .T. ) ;
#181198 = DIRECTION ( 'NONE',  ( 0.000000000000000000, 0.000000000000000000, -1.000000000000000000 ) ) ;
#181199 = FACE_OUTER_BOUND ( 'NONE', #48412, .T. ) ;
#181200 = DIRECTION ( 'NONE',  ( -2.812466655313719426E-14, -0.1350103645451835865, -0.9908441862701605762 ) ) ;
#181201 = CARTESIAN_POINT ( 'NONE',  ( -14.00000000000000178, 66.15000000001155911, -52.77310748452439526 ) ) ;
#181202 = CARTESIAN_POINT ( 'NONE',  ( -20.54999999999999716, 52.99650480578122824, -234.2878581050858884 ) ) ;
#181203 = CARTESIAN_POINT ( 'NONE',  ( 23.14999999999999858, 87.75000000001173817, -81.27310748452423184 ) ) ;
#181204 = CARTESIAN_POINT ( 'NONE',  ( 22.47110162079220785, 0.02879741281384913879, -155.8500640633156422 ) ) ;
#181205 = CARTESIAN_POINT ( 'NONE',  ( 18.39999999999999858, 85.60000000001210196, -129.8229180933022633 ) ) ;
#181206 = VERTEX_POINT ( 'NONE', #14038 ) ;
#181207 = ORIENTED_EDGE ( 'NONE', *, *, #191076, .T. ) ;
#181208 = FACE_OUTER_BOUND ( 'NONE', #202927, .T. ) ;
#181210 = CARTESIAN_POINT ( 'NONE',  ( -20.64999999999999858, 68.63171270270233038, -223.0506438513196770 ) ) ;
#181209 = DIRECTION ( 'NONE',  ( 0.000000000000000000, 0.000000000000000000, 1.000000000000000000 ) ) ;
#181211 =( BOUNDED_SURFACE ( )  B_SPLINE_SURFACE ( 3, 2, ( 
 ( #247925, #112291, #8053 ),
 ( #246640, #191845, #69315 ),
 ( #30193, #172299, #210110 ),
 ( #28938, #13187, #31488 ),
 ( #87557, #251783, #73184 ),
 ( #152723, #232246, #53589 ) ),
 .UNSPECIFIED., .F., .F., .F. ) 
 B_SPLINE_SURFACE_WITH_KNOTS ( ( 4, 2, 4 ),
 ( 3, 3 ),
 ( 6.719893378900957922E-05, 0.0002757154632485724760, 0.0004842319927081353728 ),
 ( 0.000000000000000000, 1.000000000000000000 ),
 .UNSPECIFIED. ) 
 GEOMETRIC_REPRESENTATION_ITEM ( )  RATIONAL_B_SPLINE_SURFACE ( (
 ( 1.000000000000000000, 0.7250110520819756932, 1.000000000000000000),
 ( 1.000000000000000000, 0.7277932058358959067, 1.000000000000000000),
 ( 1.000000000000000000, 0.7278452872617939828, 1.000000000000000000),
 ( 1.000000000000000000, 0.7221445671548865075, 1.000000000000000000),
 ( 1.000000000000000000, 0.7163662143779842006, 1.000000000000000000),
 ( 1.000000000000000000, 0.7071067811865475727, 1.000000000000000000) ) ) 
 REPRESENTATION_ITEM ( '' )  SURFACE ( )  );
#181212 = EDGE_CURVE ( 'NONE', #138100, #167256, #100878, .T. ) ;
#181213 = DIRECTION ( 'NONE',  ( 0.000000000000000000, 0.000000000000000000, -1.000000000000000000 ) ) ;
#181214 = CARTESIAN_POINT ( 'NONE',  ( 21.14999999999999858, 64.35000000001214460, -136.4231074845243938 ) ) ;
#181215 = DIRECTION ( 'NONE',  ( -1.000000000000000000, -2.952720810173289112E-16, 0.000000000000000000 ) ) ;
#181216 = ORIENTED_EDGE ( 'NONE', *, *, #68303, .F. ) ;
#181217 = DIRECTION ( 'NONE',  ( 1.000000000000000000, 0.000000000000000000, 0.000000000000000000 ) ) ;
#181218 = ADVANCED_FACE ( 'NONE', ( #160918 ), #216808, .F. ) ;
#181219 = ORIENTED_EDGE ( 'NONE', *, *, #30633, .T. ) ;
#181220 = AXIS2_PLACEMENT_3D ( 'NONE', #170392, #92076, #88199 ) ;
#181221 = AXIS2_PLACEMENT_3D ( 'NONE', #128701, #163975, #243494 ) ;
#181222 = CARTESIAN_POINT ( 'NONE',  ( -16.91256925476569961, 51.71161613007730296, -231.8657639032808788 ) ) ;
#181223 = VERTEX_POINT ( 'NONE', #96105 ) ;
#181224 = EDGE_CURVE ( 'NONE', #73568, #2253, #129328, .T. ) ;
#181225 = CARTESIAN_POINT ( 'NONE',  ( -23.15000000000000213, 76.00000000001190870, -103.0231074845243029 ) ) ;
#181226 = VECTOR ( 'NONE', #21881, 1000.000000000000000 ) ;
#181227 = EDGE_CURVE ( 'NONE', #178773, #27724, #154328, .T. ) ;
#181228 = CARTESIAN_POINT ( 'NONE',  ( 18.52326479938716020, 85.64236444492679823, -29.30835007111852875 ) ) ;
#181229 = CIRCLE ( 'NONE', #214515, 7.800000000000001599 ) ;
#181230 = VECTOR ( 'NONE', #157755, 1000.000000000000000 ) ;
#181231 = ORIENTED_EDGE ( 'NONE', *, *, #6983, .F. ) ;
#181232 = FACE_OUTER_BOUND ( 'NONE', #232677, .T. ) ;
#181233 = EDGE_CURVE ( 'NONE', #60251, #166220, #58575, .T. ) ;
#181234 = ORIENTED_EDGE ( 'NONE', *, *, #158079, .F. ) ;
#181235 = LINE ( 'NONE', #196918, #124682 ) ;
#181237 = CIRCLE ( 'NONE', #14840, 0.09999999999999939493 ) ;
#181236 = DIRECTION ( 'NONE',  ( 0.7071067811865457964, 0.2890913453342137673, -0.6453109281988465007 ) ) ;
#181238 = FACE_OUTER_BOUND ( 'NONE', #81655, .T. ) ;
#181239 = EDGE_CURVE ( 'NONE', #17165, #187777, #66789, .T. ) ;
#181240 = DIRECTION ( 'NONE',  ( -0.000000000000000000, 1.000000000000000000, 0.000000000000000000 ) ) ;
#181241 = EDGE_CURVE ( 'NONE', #105777, #73858, #145173, .T. ) ;
#181242 = DIRECTION ( 'NONE',  ( -5.204170427930453469E-14, 1.000000000000000000, -0.000000000000000000 ) ) ;
#181243 = CARTESIAN_POINT ( 'NONE',  ( 18.59117750673696534, 65.66751761918692409, -130.9282609406112670 ) ) ;
#181244 = CYLINDRICAL_SURFACE ( 'NONE', #78156, 0.1000000000000038219 ) ;
#181246 = ORIENTED_EDGE ( 'NONE', *, *, #13200, .T. ) ;
#181245 = CARTESIAN_POINT ( 'NONE',  ( 20.22483756094572271, 66.49809532114170452, -128.3835683558091603 ) ) ;
#181248 = DIRECTION ( 'NONE',  ( 1.000000000000000000, 0.000000000000000000, 0.000000000000000000 ) ) ;
#181247 = DIRECTION ( 'NONE',  ( 0.000000000000000000, 0.2128009952263403282, -0.9770955615653358350 ) ) ;
#181249 = ORIENTED_EDGE ( 'NONE', *, *, #182375, .T. ) ;
#181251 = ORIENTED_EDGE ( 'NONE', *, *, #47354, .T. ) ;
#181250 = FACE_OUTER_BOUND ( 'NONE', #94072, .T. ) ;
#181252 = ORIENTED_EDGE ( 'NONE', *, *, #67045, .T. ) ;
#181253 = CARTESIAN_POINT ( 'NONE',  ( -18.50000000000000000, 66.65000000001180069, -81.87310748452438247 ) ) ;
#181254 = FACE_OUTER_BOUND ( 'NONE', #257741, .T. ) ;
#181255 = CARTESIAN_POINT ( 'NONE',  ( 19.88284271247461987, 11.69142135624847256, -158.7500000000000000 ) ) ;
#181256 = ADVANCED_FACE ( 'NONE', ( #27849 ), #4382, .T. ) ;
#181257 = VERTEX_POINT ( 'NONE', #107340 ) ;
#181258 = CARTESIAN_POINT ( 'NONE',  ( -23.15000000000000213, 10.78703865319379496, -235.6923017531418623 ) ) ;
#181259 = DIRECTION ( 'NONE',  ( -0.000000000000000000, 1.000000000000000000, 0.000000000000000000 ) ) ;
#181261 = DIRECTION ( 'NONE',  ( -1.000000000000000000, 0.000000000000000000, 0.000000000000000000 ) ) ;
#181260 = AXIS2_PLACEMENT_3D ( 'NONE', #76945, #114799, #136924 ) ;
#181262 = EDGE_CURVE ( 'NONE', #164498, #152420, #246845, .T. ) ;
#181263 = EDGE_CURVE ( 'NONE', #101660, #139720, #143896, .T. ) ;
#181264 = CARTESIAN_POINT ( 'NONE',  ( -16.89797118371713225, 9.976380722655967759, -154.9372933675581976 ) ) ;
#181265 = DIRECTION ( 'NONE',  ( 0.7071359030027766224, 0.000000000000000000, -0.7070776581709024011 ) ) ;
#181266 = CARTESIAN_POINT ( 'NONE',  ( -18.59999999999999787, 9.250000000011157297, -79.35000000000005116 ) ) ;
#181267 = ORIENTED_EDGE ( 'NONE', *, *, #70054, .T. ) ;
#181268 = ORIENTED_EDGE ( 'NONE', *, *, #138984, .T. ) ;
#181269 = CARTESIAN_POINT ( 'NONE',  ( 20.00000000000000355, 4.547418889303922462, 21.90000000000000213 ) ) ;
#181270 = AXIS2_PLACEMENT_3D ( 'NONE', #62063, #240688, #25507 ) ;
#181271 = EDGE_LOOP ( 'NONE', ( #178796, #79112, #86644, #187333 ) ) ;
#181272 = AXIS2_PLACEMENT_3D ( 'NONE', #163584, #181859, #241823 ) ;
#181273 = DIRECTION ( 'NONE',  ( 0.000000000000000000, -7.086529944415894657E-15, 1.000000000000000000 ) ) ;
#181274 = ORIENTED_EDGE ( 'NONE', *, *, #218512, .F. ) ;
#181275 = DIRECTION ( 'NONE',  ( 1.000000000000000000, 0.000000000000000000, 0.000000000000000000 ) ) ;
#181276 = EDGE_CURVE ( 'NONE', #14606, #92669, #91896, .T. ) ;
#181277 = CARTESIAN_POINT ( 'NONE',  ( -20.64999999999999858, 21.43869811404188752, -233.1734427395952025 ) ) ;
#181278 = CARTESIAN_POINT ( 'NONE',  ( -5.900000000000003020, -11.65000000000000036, 10.10000000000000142 ) ) ;
#181279 = EDGE_CURVE ( 'NONE', #171946, #58688, #83885, .T. ) ;
#181280 = CARTESIAN_POINT ( 'NONE',  ( -21.07928932188134041, 30.84304088367084162, -252.0482413927653340 ) ) ;
#181281 = CARTESIAN_POINT ( 'NONE',  ( 21.09793522318412684, 10.72462451022393282, -179.7392908709771007 ) ) ;
#181282 = ORIENTED_EDGE ( 'NONE', *, *, #1651, .T. ) ;
#181283 = DIRECTION ( 'NONE',  ( 0.000000000000000000, 0.000000000000000000, 1.000000000000000000 ) ) ;
#181284 = EDGE_CURVE ( 'NONE', #168864, #68442, #116851, .T. ) ;
#181285 = CARTESIAN_POINT ( 'NONE',  ( -18.50000000000000000, 10.29270135741298375, -105.9573618871519898 ) ) ;
#181286 = CARTESIAN_POINT ( 'NONE',  ( -21.14999999999999858, 64.25000000001232081, -163.2392418215462726 ) ) ;
#181287 = LINE ( 'NONE', #62608, #93339 ) ;
#181288 = ORIENTED_EDGE ( 'NONE', *, *, #1103, .F. ) ;
#181289 = CIRCLE ( 'NONE', #77199, 0.09999999999999939493 ) ;
#181291 = DIRECTION ( 'NONE',  ( -1.000000000000000000, -0.000000000000000000, 0.000000000000000000 ) ) ;
#181290 = CARTESIAN_POINT ( 'NONE',  ( -22.47071067811865319, 75.90090754530983475, -177.7431822290224090 ) ) ;
#181292 = ORIENTED_EDGE ( 'NONE', *, *, #143150, .T. ) ;
#181294 = EDGE_LOOP ( 'NONE', ( #31865, #190295, #95549 ) ) ;
#181293 = DIRECTION ( 'NONE',  ( 0.000000000000000000, 0.000000000000000000, -1.000000000000000000 ) ) ;
#181295 = ORIENTED_EDGE ( 'NONE', *, *, #116493, .F. ) ;
#181296 = CARTESIAN_POINT ( 'NONE',  ( -20.64999999999999858, 7.150000000011155876, -79.25000000000004263 ) ) ;
#181297 = DIRECTION ( 'NONE',  ( -0.000000000000000000, 0.2617529984165031243, 0.9651348961777157509 ) ) ;
#181298 = AXIS2_PLACEMENT_3D ( 'NONE', #102902, #182486, #162927 ) ;
#181299 = EDGE_LOOP ( 'NONE', ( #52137, #226914, #89615, #194047 ) ) ;
#181300 = CARTESIAN_POINT ( 'NONE',  ( -18.59999999999999787, 77.83534155023670564, -158.4679561919613491 ) ) ;
#181301 = CARTESIAN_POINT ( 'NONE',  ( -20.85000000000000142, -1.851617760468904805, -45.10318971960366241 ) ) ;
#181303 = CARTESIAN_POINT ( 'NONE',  ( -18.59999999999999787, 77.16270174995064224, -195.4231074845243370 ) ) ;
#181302 = CARTESIAN_POINT ( 'NONE',  ( 18.59999999999999432, -1.637172712970379918, -11.58215336547201701 ) ) ;
#181305 = EDGE_LOOP ( 'NONE', ( #95667, #222042, #164097, #179774 ) ) ;
#181304 = LINE ( 'NONE', #2634, #122566 ) ;
#181306 = ADVANCED_FACE ( 'NONE', ( #147769 ), #43534, .T. ) ;
#181307 = ORIENTED_EDGE ( 'NONE', *, *, #202985, .F. ) ;
#181308 = ADVANCED_FACE ( 'NONE', ( #85175 ), #244276, .T. ) ;
#181309 = CARTESIAN_POINT ( 'NONE',  ( 18.69999999999999929, 7.973296578895943121, -1.410778198689827123 ) ) ;
#181310 = AXIS2_PLACEMENT_3D ( 'NONE', #98232, #95695, #215641 ) ;
#181311 = AXIS2_PLACEMENT_3D ( 'NONE', #161605, #139424, #179874 ) ;
#181312 = CARTESIAN_POINT ( 'NONE',  ( -23.15000000000000213, 54.18213181965657554, -236.9344197582443883 ) ) ;
#181313 = VERTEX_POINT ( 'NONE', #166070 ) ;
#181314 = CYLINDRICAL_SURFACE ( 'NONE', #210198, 0.09999999999999939493 ) ;
#181315 = ORIENTED_EDGE ( 'NONE', *, *, #156571, .T. ) ;
#181316 = DIRECTION ( 'NONE',  ( 0.000000000000000000, 1.000000000000000000, 6.982962677686266711E-15 ) ) ;
#181317 = EDGE_CURVE ( 'NONE', #121092, #226829, #250134, .T. ) ;
#181318 = CARTESIAN_POINT ( 'NONE',  ( 22.45380639572251624, 75.99999985734478969, -114.7735403756311996 ) ) ;
#181319 = CARTESIAN_POINT ( 'NONE',  ( 21.53752568617663243, 6.786807874515133676, -33.40102553874074687 ) ) ;
#181320 = VERTEX_POINT ( 'NONE', #245585 ) ;
#181321 = FACE_OUTER_BOUND ( 'NONE', #37210, .T. ) ;
#181322 = EDGE_CURVE ( 'NONE', #41827, #134704, #123068, .T. ) ;
#181323 = EDGE_CURVE ( 'NONE', #71756, #60014, #201308, .T. ) ;
#181324 = AXIS2_PLACEMENT_3D ( 'NONE', #238742, #199641, #33203 ) ;
#181325 = LINE ( 'NONE', #2654, #223078 ) ;
#181326 = AXIS2_PLACEMENT_3D ( 'NONE', #171243, #250719, #132065 ) ;
#181327 = CIRCLE ( 'NONE', #135318, 0.1000000000000106498 ) ;
#181328 = ADVANCED_FACE ( 'NONE', ( #46078 ), #26545, .T. ) ;
#181329 = EDGE_LOOP ( 'NONE', ( #10928, #16491, #170188, #193416 ) ) ;
#181330 = ORIENTED_EDGE ( 'NONE', *, *, #100027, .T. ) ;
#181332 = EDGE_CURVE ( 'NONE', #155848, #2636, #126917, .T. ) ;
#181331 = EDGE_CURVE ( 'NONE', #77934, #212622, #25263, .T. ) ;
#181333 = ORIENTED_EDGE ( 'NONE', *, *, #133226, .F. ) ;
#181334 = MECHANICAL_DESIGN_GEOMETRIC_PRESENTATION_REPRESENTATION (  '', ( #152303 ), #168881 ) ;
#181335 = DIRECTION ( 'NONE',  ( -1.000000000000000000, -0.000000000000000000, 0.000000000000000000 ) ) ;
#181336 = VERTEX_POINT ( 'NONE', #8261 ) ;
#181338 = ORIENTED_EDGE ( 'NONE', *, *, #204532, .T. ) ;
#181337 = CARTESIAN_POINT ( 'NONE',  ( -23.15000000000000213, 68.56901367119438362, -214.3038979092079046 ) ) ;
#181339 = ORIENTED_EDGE ( 'NONE', *, *, #208897, .F. ) ;
#181342 = ORIENTED_EDGE ( 'NONE', *, *, #217354, .F. ) ;
#181341 = ORIENTED_EDGE ( 'NONE', *, *, #100935, .T. ) ;
#181340 = CARTESIAN_POINT ( 'NONE',  ( 18.46921299892754220, 78.23786519927757865, -231.6012438402944724 ) ) ;
#181343 = ORIENTED_EDGE ( 'NONE', *, *, #56331, .T. ) ;
#181344 = FACE_OUTER_BOUND ( 'NONE', #156834, .T. ) ;
#181345 = ADVANCED_FACE ( 'NONE', ( #167350 ), #98821, .T. ) ;
#181346 = ADVANCED_FACE ( 'NONE', ( #149066 ), #50370, .F. ) ;
#181347 = CIRCLE ( 'NONE', #247954, 4.041421356237306917 ) ;
#181348 = LINE ( 'NONE', #177515, #76257 ) ;
#181349 = CARTESIAN_POINT ( 'NONE',  ( -21.14999999999994174, 79.88763423575340994, -7.282924647898262549 ) ) ;
#181350 = VECTOR ( 'NONE', #918, 1000.000000000000000 ) ;
#181351 = ORIENTED_EDGE ( 'NONE', *, *, #117758, .T. ) ;
#181352 = EDGE_CURVE ( 'NONE', #256334, #61689, #75371, .T. ) ;
#181353 = DIRECTION ( 'NONE',  ( 0.000000000000000000, 0.000000000000000000, 1.000000000000000000 ) ) ;
#181355 = ORIENTED_EDGE ( 'NONE', *, *, #194309, .F. ) ;
#181354 = FACE_OUTER_BOUND ( 'NONE', #31777, .T. ) ;
#181357 = CARTESIAN_POINT ( 'NONE',  ( -20.95000000000000284, 11.65000000001115232, -59.98519422934605672 ) ) ;
#181356 = CIRCLE ( 'NONE', #68935, 0.9000000000000014655 ) ;
#181358 = EDGE_LOOP ( 'NONE', ( #227940, #100401, #41834, #14791 ) ) ;
#181359 = VERTEX_POINT ( 'NONE', #90340 ) ;
#181360 = EDGE_CURVE ( 'NONE', #178769, #164289, #117040, .T. ) ;
#181361 = AXIS2_PLACEMENT_3D ( 'NONE', #57730, #135980, #99420 ) ;
#181362 = CIRCLE ( 'NONE', #231416, 0.1000000000000028644 ) ;
#181363 = VECTOR ( 'NONE', #121711, 1000.000000000000000 ) ;
#181365 = EDGE_CURVE ( 'NONE', #18615, #31646, #122175, .T. ) ;
#181364 = CARTESIAN_POINT ( 'NONE',  ( 21.05000000000000071, 85.40000000001231228, -160.1291383618718385 ) ) ;
#181366 = DIRECTION ( 'NONE',  ( 0.000000000000000000, 4.336808689941893885E-15, 1.000000000000000000 ) ) ;
#181367 = ORIENTED_EDGE ( 'NONE', *, *, #155392, .T. ) ;
#181368 = ORIENTED_EDGE ( 'NONE', *, *, #175942, .F. ) ;
#181369 = FACE_OUTER_BOUND ( 'NONE', #212722, .T. ) ;
#181370 = FACE_OUTER_BOUND ( 'NONE', #108401, .T. ) ;
#181373 = ORIENTED_EDGE ( 'NONE', *, *, #217003, .F. ) ;
#181372 = ORIENTED_EDGE ( 'NONE', *, *, #12265, .T. ) ;
#181371 = CIRCLE ( 'NONE', #43790, 0.1000000000000028644 ) ;
#181374 = ORIENTED_EDGE ( 'NONE', *, *, #59944, .F. ) ;
#181375 = DIRECTION ( 'NONE',  ( 1.000000000000000000, 0.000000000000000000, -0.000000000000000000 ) ) ;
#181376 = ORIENTED_EDGE ( 'NONE', *, *, #172255, .F. ) ;
#181377 = AXIS2_PLACEMENT_3D ( 'NONE', #162099, #241614, #145069 ) ;
#181378 = VERTEX_POINT ( 'NONE', #210314 ) ;
#181379 = DIRECTION ( 'NONE',  ( 0.000000000000000000, 0.000000000000000000, 1.000000000000000000 ) ) ;
#181381 = VERTEX_POINT ( 'NONE', #250702 ) ;
#181380 = CARTESIAN_POINT ( 'NONE',  ( 21.05000000000000071, -4.914013037343259782, -233.1828366659746905 ) ) ;
#181382 = EDGE_CURVE ( 'NONE', #88661, #119088, #30397, .T. ) ;
#181383 = DIRECTION ( 'NONE',  ( 0.000000000000000000, 0.000000000000000000, -1.000000000000000000 ) ) ;
#181384 = AXIS2_PLACEMENT_3D ( 'NONE', #119632, #114482, #38808 ) ;
#181385 = CIRCLE ( 'NONE', #93874, 0.09999999999999749367 ) ;
#181387 = LINE ( 'NONE', #204759, #160833 ) ;
#181386 = LINE ( 'NONE', #36749, #207006 ) ;
#181388 = ORIENTED_EDGE ( 'NONE', *, *, #160028, .F. ) ;
#181390 = ORIENTED_EDGE ( 'NONE', *, *, #138799, .F. ) ;
#181389 = ORIENTED_EDGE ( 'NONE', *, *, #207387, .F. ) ;
#181391 = EDGE_CURVE ( 'NONE', #24478, #147651, #129514, .T. ) ;
#181392 = CARTESIAN_POINT ( 'NONE',  ( 18.59999999999999432, -1.299733671219632791, -124.0281295228694347 ) ) ;
#181393 = FILL_AREA_STYLE_COLOUR ( '', #33007 ) ;
#181394 = ORIENTED_EDGE ( 'NONE', *, *, #15598, .F. ) ;
#181395 = CARTESIAN_POINT ( 'NONE',  ( -18.44362607810621313, 85.49049615809671820, -95.96515361767714580 ) ) ;
#181396 = VERTEX_POINT ( 'NONE', #112501 ) ;
#181397 = ORIENTED_EDGE ( 'NONE', *, *, #136757, .T. ) ;
#181398 = CARTESIAN_POINT ( 'NONE',  ( 23.40000000000004476, 74.83745509109094485, -44.02310748452479316 ) ) ;
#181399 = EDGE_CURVE ( 'NONE', #10704, #74828, #200241, .T. ) ;
#181400 = ORIENTED_EDGE ( 'NONE', *, *, #94939, .T. ) ;
#181401 = DIRECTION ( 'NONE',  ( 0.000000000000000000, -1.000000000000000000, -6.982962677686265922E-15 ) ) ;
#181402 = CARTESIAN_POINT ( 'NONE',  ( 21.05000000000000071, 76.10000000001198828, -109.5001538663141787 ) ) ;
#181403 = VERTEX_POINT ( 'NONE', #9521 ) ;
#181404 = DIRECTION ( 'NONE',  ( 1.000000000000000000, -0.000000000000000000, 0.000000000000000000 ) ) ;
#181405 = DIRECTION ( 'NONE',  ( 1.000000000000000000, 0.000000000000000000, -0.000000000000000000 ) ) ;
#181407 = DIRECTION ( 'NONE',  ( -1.000000000000000000, -0.000000000000000000, -0.000000000000000000 ) ) ;
#181406 = CARTESIAN_POINT ( 'NONE',  ( -18.50000000000000000, 74.65925378207803931, -79.79596998994550461 ) ) ;
#181408 = DIRECTION ( 'NONE',  ( 0.000000000000000000, 0.9908441862701596881, 0.1350103645451904977 ) ) ;
#181409 = CARTESIAN_POINT ( 'NONE',  ( 19.90000000000000924, 4.513204987021263825, 22.10000000000000142 ) ) ;
#181410 = FACE_OUTER_BOUND ( 'NONE', #140292, .T. ) ;
#181411 = VECTOR ( 'NONE', #111390, 1000.000000000000000 ) ;
#181412 = FACE_OUTER_BOUND ( 'NONE', #240265, .T. ) ;
#181413 = FACE_OUTER_BOUND ( 'NONE', #243936, .T. ) ;
#181414 = VECTOR ( 'NONE', #247331, 1000.000000000000000 ) ;
#181415 = ORIENTED_EDGE ( 'NONE', *, *, #143286, .T. ) ;
#181416 = AXIS2_PLACEMENT_3D ( 'NONE', #164323, #200866, #183874 ) ;
#181418 = ORIENTED_EDGE ( 'NONE', *, *, #124434, .F. ) ;
#181417 = ORIENTED_EDGE ( 'NONE', *, *, #205291, .F. ) ;
#181419 = ORIENTED_EDGE ( 'NONE', *, *, #14079, .T. ) ;
#181420 = DIRECTION ( 'NONE',  ( 0.000000000000000000, -1.000000000000000000, 0.000000000000000000 ) ) ;
#181421 = CARTESIAN_POINT ( 'NONE',  ( -23.39999999999994529, 77.73640333653723644, -47.54092689884382850 ) ) ;
#181422 = CIRCLE ( 'NONE', #252296, 12.87499999999999822 ) ;
#181424 = CARTESIAN_POINT ( 'NONE',  ( -12.29659703204452015, 9.355888454502544249, -16.28864289677800059 ) ) ;
#181423 = CARTESIAN_POINT ( 'NONE',  ( -20.64999999999999858, 85.50000000001222134, -146.4170766071767389 ) ) ;
#181425 = CARTESIAN_POINT ( 'NONE',  ( 20.94999999999999574, 1.835341550235567887, -145.6551512925629766 ) ) ;
#181427 = ORIENTED_EDGE ( 'NONE', *, *, #231860, .F. ) ;
#181426 = AXIS2_PLACEMENT_3D ( 'NONE', #128517, #244599, #225021 ) ;
#181428 = DIRECTION ( 'NONE',  ( -1.000000000000000000, 3.265361837132813093E-16, 2.280189983783949500E-30 ) ) ;
#181429 = DIRECTION ( 'NONE',  ( 0.000000000000000000, 0.2617529984165033463, 0.9651348961777157509 ) ) ;
#181430 = AXIS2_PLACEMENT_3D ( 'NONE', #93740, #53331, #49483 ) ;
#181431 = CARTESIAN_POINT ( 'NONE',  ( 20.85000000000000142, 77.75000000001236344, -158.4041574459020865 ) ) ;
#181432 = LINE ( 'NONE', #185264, #183306 ) ;
#181433 = ORIENTED_EDGE ( 'NONE', *, *, #47424, .F. ) ;
#181434 = DIRECTION ( 'NONE',  ( 0.000000000000000000, 0.000000000000000000, 1.000000000000000000 ) ) ;
#181435 = ORIENTED_EDGE ( 'NONE', *, *, #34064, .F. ) ;
#181436 = CARTESIAN_POINT ( 'NONE',  ( 23.14999999999999503, 11.65000000000000746, -12.15000000000000036 ) ) ;
#181437 = CIRCLE ( 'NONE', #73121, 0.09999999999999739653 ) ;
#181438 = DIRECTION ( 'NONE',  ( 1.000000000000000000, 0.000000000000000000, 0.000000000000000000 ) ) ;
#181439 = CARTESIAN_POINT ( 'NONE',  ( 22.60000000000000142, 1.115600667400684642E-11, -167.4999999999999716 ) ) ;
#181440 = DIRECTION ( 'NONE',  ( 2.952720810173289112E-16, 1.000000000000000000, 6.982962677686266711E-15 ) ) ;
#181441 = FACE_OUTER_BOUND ( 'NONE', #5249, .T. ) ;
#181442 = VERTEX_POINT ( 'NONE', #150342 ) ;
#181443 = FACE_OUTER_BOUND ( 'NONE', #82658, .T. ) ;
#181444 = LINE ( 'NONE', #103150, #4924 ) ;
#181445 = CARTESIAN_POINT ( 'NONE',  ( -21.11833042828136087, 0.007100509070459421791, -60.55435530614461470 ) ) ;
#181447 = FACE_OUTER_BOUND ( 'NONE', #94996, .T. ) ;
#181446 = CARTESIAN_POINT ( 'NONE',  ( -21.05000000000000071, 70.10000000001149090, -46.24220724918073699 ) ) ;
#181449 = EDGE_CURVE ( 'NONE', #64683, #92040, #229869, .T. ) ;
#181448 = CARTESIAN_POINT ( 'NONE',  ( -18.43707690579160641, 85.68240343348881538, -163.3662641071115615 ) ) ;
#181450 = DIRECTION ( 'NONE',  ( 0.000000000000000000, 0.000000000000000000, -1.000000000000000000 ) ) ;
#181451 = LINE ( 'NONE', #2776, #239423 ) ;
#181452 = DIRECTION ( 'NONE',  ( 2.952720810173289112E-16, 1.000000000000000000, 6.982962677686266711E-15 ) ) ;
#181453 = VECTOR ( 'NONE', #146480, 1000.000000000000000 ) ;
#181456 = ORIENTED_EDGE ( 'NONE', *, *, #218641, .F. ) ;
#181455 = AXIS2_PLACEMENT_3D ( 'NONE', #246485, #226924, #127838 ) ;
#181454 = DIRECTION ( 'NONE',  ( 0.000000000000000000, 1.000000000000000000, 2.891205793294679805E-16 ) ) ;
#181457 = CIRCLE ( 'NONE', #169172, 0.09999999999999939493 ) ;
#181458 = ORIENTED_EDGE ( 'NONE', *, *, #157663, .T. ) ;
#181459 = ADVANCED_FACE ( 'NONE', ( #151644 ), #91641, .F. ) ;
#181460 = DIRECTION ( 'NONE',  ( 1.000000000000000000, 0.000000000000000000, 0.000000000000000000 ) ) ;
#181461 = EDGE_CURVE ( 'NONE', #87677, #248271, #225157, .T. ) ;
#181462 = LINE ( 'NONE', #120228, #29862 ) ;
#181463 = CARTESIAN_POINT ( 'NONE',  ( 21.05000000000000071, 8.876614585098254295, -41.88508047884467800 ) ) ;
#181464 = AXIS2_PLACEMENT_3D ( 'NONE', #229834, #51164, #151612 ) ;
#181465 = EDGE_CURVE ( 'NONE', #182323, #31369, #177628, .T. ) ;
#181466 = VERTEX_POINT ( 'NONE', #35549 ) ;
#181467 = DIRECTION ( 'NONE',  ( 0.000000000000000000, 1.000000000000000000, 0.000000000000000000 ) ) ;
#181468 = DIRECTION ( 'NONE',  ( 0.000000000000000000, -0.000000000000000000, 1.000000000000000000 ) ) ;
#181469 = CARTESIAN_POINT ( 'NONE',  ( -21.07016717457011978, 76.00000000001202238, -109.3440483226251985 ) ) ;
#181470 = EDGE_CURVE ( 'NONE', #174912, #136430, #96169, .T. ) ;
#181472 = ORIENTED_EDGE ( 'NONE', *, *, #79689, .T. ) ;
#181471 = ADVANCED_FACE ( 'NONE', ( #198436 ), #108660, .F. ) ;
#181473 = LINE ( 'NONE', #204850, #145472 ) ;
#181475 = VERTEX_POINT ( 'NONE', #159337 ) ;
#181474 = CARTESIAN_POINT ( 'NONE',  ( 22.60000000000000142, 7.128833340093095217, -233.7327013124392749 ) ) ;
#181477 = DIRECTION ( 'NONE',  ( 0.000000000000000000, -6.608470384673536824E-15, 1.000000000000000000 ) ) ;
#181476 = CARTESIAN_POINT ( 'NONE',  ( 23.04999999999999716, 8.822561741677553471, -146.6500000000000341 ) ) ;
#181478 = CARTESIAN_POINT ( 'NONE',  ( 20.13684514580103624, 66.50414460725968979, -161.8800757988351791 ) ) ;
#181479 = EDGE_CURVE ( 'NONE', #229370, #65743, #60203, .T. ) ;
#181480 = DIRECTION ( 'NONE',  ( 0.000000000000000000, -0.9651348961776677893, 0.2617529984166795387 ) ) ;
#181481 = EDGE_LOOP ( 'NONE', ( #5431, #66705, #163398, #219737 ) ) ;
#181482 = DIRECTION ( 'NONE',  ( 1.000000000000000000, 0.000000000000000000, 0.000000000000000000 ) ) ;
#181483 = DIRECTION ( 'NONE',  ( 0.000000000000000000, 0.8814952561688438326, -0.4721928772777330696 ) ) ;
#181484 = CARTESIAN_POINT ( 'NONE',  ( 20.27550659511089037, 66.78395627750268204, -48.67310748452439384 ) ) ;
#181485 = EDGE_CURVE ( 'NONE', #79879, #186539, #257080, .T. ) ;
#181486 = EDGE_LOOP ( 'NONE', ( #215777, #154425, #122429, #46576 ) ) ;
#181487 = CARTESIAN_POINT ( 'NONE',  ( 23.24999999999999645, 20.94763808724816556, -234.7254930126486556 ) ) ;
#181488 = CIRCLE ( 'NONE', #64928, 0.3999999999999975797 ) ;
#181490 = FILL_AREA_STYLE_COLOUR ( '', #159675 ) ;
#181489 = CIRCLE ( 'NONE', #89878, 0.09999999999998898659 ) ;
#181491 = ADVANCED_FACE ( 'NONE', ( #39402 ), #19827, .T. ) ;
#181492 = CARTESIAN_POINT ( 'NONE',  ( -23.25000000000000355, 5.650000000011139001, -146.6500000000000341 ) ) ;
#181493 = CARTESIAN_POINT ( 'NONE',  ( -22.47120815636973745, 0.02890382191504723905, -122.3500680112465204 ) ) ;
#181494 = ORIENTED_EDGE ( 'NONE', *, *, #27016, .F. ) ;
#181495 = ADVANCED_FACE ( 'NONE', ( #194622 ), #77198, .F. ) ;
#181496 = ORIENTED_EDGE ( 'NONE', *, *, #67663, .T. ) ;
#181497 = ADVANCED_FACE ( 'NONE', ( #175077 ), #62878, .F. ) ;
#181498 = DIRECTION ( 'NONE',  ( 0.000000000000000000, -0.8814952561688429444, 0.4721928772777349570 ) ) ;
#181499 = CARTESIAN_POINT ( 'NONE',  ( 18.59999999999999076, -1.249999999988843369, -175.4999999999999716 ) ) ;
#181500 = CARTESIAN_POINT ( 'NONE',  ( -20.94999999999999929, 1.115600667400684642E-11, -122.2000000000000313 ) ) ;
#181501 = DIRECTION ( 'NONE',  ( 0.000000000000000000, 1.000000000000000000, 0.000000000000000000 ) ) ;
#181504 = DIRECTION ( 'NONE',  ( 0.000000000000000000, 0.000000000000000000, -1.000000000000000000 ) ) ;
#181503 = CIRCLE ( 'NONE', #27404, 11.70000000000000284 ) ;
#181502 = DIRECTION ( 'NONE',  ( 1.000000000000000000, 0.000000000000000000, 0.000000000000000000 ) ) ;
#181505 = CARTESIAN_POINT ( 'NONE',  ( 18.42636655943168833, -9.496944315759476396, -174.1090805711555447 ) ) ;
#181506 = CIRCLE ( 'NONE', #31118, 12.87499999999999822 ) ;
#181507 = CARTESIAN_POINT ( 'NONE',  ( 20.85000000000000142, 67.23127455305835554, -235.8551265064784559 ) ) ;
#181508 = CARTESIAN_POINT ( 'NONE',  ( 18.46905048506370406, -9.473744257371240707, -107.1759862922554731 ) ) ;
#181510 = ORIENTED_EDGE ( 'NONE', *, *, #130128, .F. ) ;
#181509 = AXIS2_PLACEMENT_3D ( 'NONE', #53182, #36210, #234377 ) ;
#181511 = CARTESIAN_POINT ( 'NONE',  ( -20.64999999999999858, 67.23127455305835554, -235.8551265064784559 ) ) ;
#181512 = TOROIDAL_SURFACE ( 'NONE', #69082, 0.9750000000000019762, 0.1000000000000000056 ) ;
#181514 = ORIENTED_EDGE ( 'NONE', *, *, #81258, .T. ) ;
#181513 = PLANE ( 'NONE',  #232174 ) ;
#181515 = CARTESIAN_POINT ( 'NONE',  ( -21.05000000000000071, 64.35000000001208775, -129.7392418215462158 ) ) ;
#181516 = LINE ( 'NONE', #84924, #49182 ) ;
#181518 = LINE ( 'NONE', #2839, #115892 ) ;
#181517 = DIRECTION ( 'NONE',  ( 0.000000000000000000, 0.000000000000000000, -1.000000000000000000 ) ) ;
#181519 =( GEOMETRIC_REPRESENTATION_CONTEXT ( 3 ) GLOBAL_UNCERTAINTY_ASSIGNED_CONTEXT ( ( #941 ) ) GLOBAL_UNIT_ASSIGNED_CONTEXT ( ( #199056, #80350, #200335 ) ) REPRESENTATION_CONTEXT ( 'NONE', 'WORKASPACE' ) );
#181520 = ADVANCED_FACE ( 'NONE', ( #156776 ), #178915, .T. ) ;
#181521 = ORIENTED_EDGE ( 'NONE', *, *, #82959, .T. ) ;
#181523 = DIRECTION ( 'NONE',  ( 1.000000000000000000, -2.849773892568378313E-16, 7.728835255496647986E-17 ) ) ;
#181522 = CARTESIAN_POINT ( 'NONE',  ( -16.84981964351482731, 66.08268176591292331, -56.65350587050463815 ) ) ;
#181524 = CARTESIAN_POINT ( 'NONE',  ( -21.55000000000000426, 68.25000000001223555, -148.8731074845244109 ) ) ;
#181525 = DIRECTION ( 'NONE',  ( -1.000000000000000000, -1.875376730785737719E-16, -0.000000000000000000 ) ) ;
#181526 = FACE_OUTER_BOUND ( 'NONE', #87306, .T. ) ;
#181527 = CARTESIAN_POINT ( 'NONE',  ( -15.15564720441980207, 66.58929125296548079, -185.4538990786802799 ) ) ;
#181528 = ORIENTED_EDGE ( 'NONE', *, *, #130174, .F. ) ;
#181529 = EDGE_LOOP ( 'NONE', ( #120812, #137651, #191963, #113594 ) ) ;
#181530 = CARTESIAN_POINT ( 'NONE',  ( -18.59999999999999787, 64.35000000001276987, -215.2731074845244450 ) ) ;
#181531 = VERTEX_POINT ( 'NONE', #81037 ) ;
#181532 = PLANE ( 'NONE',  #138657 ) ;
#181533 = AXIS2_PLACEMENT_3D ( 'NONE', #195127, #131270, #16484 ) ;
#181534 = ORIENTED_EDGE ( 'NONE', *, *, #42060, .F. ) ;
#181535 = EDGE_CURVE ( 'NONE', #51816, #187259, #160630, .T. ) ;
#181536 = DIRECTION ( 'NONE',  ( 0.000000000000000000, 6.982962677686266711E-15, -1.000000000000000000 ) ) ;
#181537 = CIRCLE ( 'NONE', #2429, 0.1000000000000028644 ) ;
#181538 = CARTESIAN_POINT ( 'NONE',  ( -20.87155475150660777, 62.85241404162280077, -207.1112001314805582 ) ) ;
#181540 = ORIENTED_EDGE ( 'NONE', *, *, #9246, .F. ) ;
#181539 = AXIS2_PLACEMENT_3D ( 'NONE', #104531, #167144, #86258 ) ;
#181541 = EDGE_CURVE ( 'NONE', #114385, #119397, #58898, .T. ) ;
#181542 = AXIS2_PLACEMENT_3D ( 'NONE', #7744, #87250, #71582 ) ;
#181543 = CARTESIAN_POINT ( 'NONE',  ( -16.87683809663752399, 9.850000000011144508, -87.09763598180374800 ) ) ;
#181545 = CARTESIAN_POINT ( 'NONE',  ( -21.05000000000000071, 65.60141603934033583, -241.9453590735340924 ) ) ;
#181544 = CIRCLE ( 'NONE', #198274, 0.1000000000000013933 ) ;
#181546 = CARTESIAN_POINT ( 'NONE',  ( -18.69999999999999929, 1.149999999999999911, 16.60000000000000142 ) ) ;
#181547 = EDGE_CURVE ( 'NONE', #60723, #62069, #92087, .T. ) ;
#181548 = EDGE_CURVE ( 'NONE', #141640, #176854, #328, .T. ) ;
#181549 = CARTESIAN_POINT ( 'NONE',  ( 23.14999999999999858, 70.05000000001221849, -146.8288097895591875 ) ) ;
#181550 = CARTESIAN_POINT ( 'NONE',  ( 21.15000000000005542, 64.25000000001119815, -3.023107484524792277 ) ) ;
#181551 = CARTESIAN_POINT ( 'NONE',  ( 13.88302573338720869, 62.02991417940920371, -218.9025163457276904 ) ) ;
#181552 = ORIENTED_EDGE ( 'NONE', *, *, #152722, .F. ) ;
#181555 = ADVANCED_FACE ( 'NONE', ( #215434 ), #162095, .F. ) ;
#181554 = CARTESIAN_POINT ( 'NONE',  ( 20.73486653747088582, 62.65526179112259086, -225.0299194783148664 ) ) ;
#181553 = CARTESIAN_POINT ( 'NONE',  ( -23.49999999999994316, 76.00000000001119815, -36.02310748452479316 ) ) ;
#181556 = ORIENTED_EDGE ( 'NONE', *, *, #149800, .F. ) ;
#181558 = ORIENTED_EDGE ( 'NONE', *, *, #203792, .F. ) ;
#181557 = FACE_OUTER_BOUND ( 'NONE', #11379, .T. ) ;
#181559 = AXIS2_PLACEMENT_3D ( 'NONE', #113027, #29669, #153489 ) ;
#181560 = ORIENTED_EDGE ( 'NONE', *, *, #8297, .F. ) ;
#181561 = DIRECTION ( 'NONE',  ( 2.952720810173289112E-16, 0.4088369013363280513, -0.9126074666063769270 ) ) ;
#181562 = CARTESIAN_POINT ( 'NONE',  ( 23.14999999999999858, 76.00000000001186606, -90.14810748452431710 ) ) ;
#181563 = CARTESIAN_POINT ( 'NONE',  ( 21.13461538461538325, 60.21941965847795331, -221.1573116214326546 ) ) ;
#181564 = EDGE_CURVE ( 'NONE', #102375, #41172, #202297, .T. ) ;
#181565 = DIRECTION ( 'NONE',  ( -1.000000000000000000, -0.000000000000000000, -0.000000000000000000 ) ) ;
#181566 = EDGE_LOOP ( 'NONE', ( #245184, #232405, #39520 ) ) ;
#181567 = TOROIDAL_SURFACE ( 'NONE', #127374, 0.2000000000000000111, 0.1000000000000000056 ) ;
#181568 = FACE_OUTER_BOUND ( 'NONE', #118829, .T. ) ;
#181569 = CARTESIAN_POINT ( 'NONE',  ( -16.81453046979148880, 66.06089771857138260, -157.3113809609213831 ) ) ;
#181570 = VECTOR ( 'NONE', #164483, 1000.000000000000000 ) ;
#181571 = ORIENTED_EDGE ( 'NONE', *, *, #48838, .F. ) ;
#181572 = CARTESIAN_POINT ( 'NONE',  ( -20.94403535211772294, 10.30632246270531738, -39.00418367788957852 ) ) ;
#181573 = DIRECTION ( 'NONE',  ( 0.000000000000000000, 0.000000000000000000, 1.000000000000000000 ) ) ;
#181574 = ORIENTED_EDGE ( 'NONE', *, *, #96556, .T. ) ;
#181575 = DIRECTION ( 'NONE',  ( 0.000000000000000000, 0.000000000000000000, 1.000000000000000000 ) ) ;
#181576 = EDGE_CURVE ( 'NONE', #173680, #103428, #154484, .T. ) ;
#181577 = CARTESIAN_POINT ( 'NONE',  ( 21.15000000000005542, 67.85000000001119247, -3.123107484524795474 ) ) ;
#181578 = ORIENTED_EDGE ( 'NONE', *, *, #119169, .T. ) ;
#181579 = LINE ( 'NONE', #64186, #117061 ) ;
#181580 = ADVANCED_FACE ( 'NONE', ( #224413 ), #84870, .F. ) ;
#181581 = CARTESIAN_POINT ( 'NONE',  ( 21.05000000000000071, 63.62814136979439184, -224.4990371885399441 ) ) ;
#181582 = LINE ( 'NONE', #245399, #122325 ) ;
#181583 = EDGE_CURVE ( 'NONE', #184760, #56540, #193759, .T. ) ;
#181584 =( BOUNDED_CURVE ( )  B_SPLINE_CURVE ( 3, ( #85026, #145021, #104589, #82459 ),
 .UNSPECIFIED., .F., .F. ) 
 B_SPLINE_CURVE_WITH_KNOTS ( ( 4, 4 ),
 ( 1.570796326794892339, 3.141592653589784678 ),
 .UNSPECIFIED. ) 
 CURVE ( )  GEOMETRIC_REPRESENTATION_ITEM ( )  RATIONAL_B_SPLINE_CURVE ( ( 1.000000000000000000, 0.8047378541243659367, 0.8047378541243659367, 1.000000000000000000 ) ) 
 REPRESENTATION_ITEM ( '' )  );
#181585 = CARTESIAN_POINT ( 'NONE',  ( 18.59999999999998366, 68.97833521811131163, -32.18954208262707795 ) ) ;
#181586 = VECTOR ( 'NONE', #127722, 1000.000000000000000 ) ;
#181587 = TOROIDAL_SURFACE ( 'NONE', #31575, 11.70000000000000462, 0.1000000000000000056 ) ;
#181588 = AXIS2_PLACEMENT_3D ( 'NONE', #208357, #169249, #188765 ) ;
#181589 = CARTESIAN_POINT ( 'NONE',  ( -20.94999999999999929, -11.39257802169451672, -36.57394957983193251 ) ) ;
#181590 = CARTESIAN_POINT ( 'NONE',  ( -19.89999999999999858, 4.611773100472912112, 22.11686199900910665 ) ) ;
#181591 = EDGE_LOOP ( 'NONE', ( #36788, #64118, #200541, #52349 ) ) ;
#181593 = DIRECTION ( 'NONE',  ( -0.000000000000000000, -6.982962677686266711E-15, 1.000000000000000000 ) ) ;
#181592 = FACE_OUTER_BOUND ( 'NONE', #219195, .T. ) ;
#181594 = CIRCLE ( 'NONE', #10901, 0.09999999999999609201 ) ;
#181595 = ORIENTED_EDGE ( 'NONE', *, *, #40283, .F. ) ;
#181596 = CARTESIAN_POINT ( 'NONE',  ( -16.94878442675512531, 12.44667358478774055, -211.1966647789336093 ) ) ;
#181597 = CARTESIAN_POINT ( 'NONE',  ( 22.94999999999999929, 4.898587196589412829E-16, -4.000000000000000000 ) ) ;
#181599 = EDGE_LOOP ( 'NONE', ( #81277, #236837, #58124 ) ) ;
#181598 = CARTESIAN_POINT ( 'NONE',  ( -21.29999999999995808, 66.17117490947157421, -239.7639228359981303 ) ) ;
#181600 = CARTESIAN_POINT ( 'NONE',  ( -18.45140287520618472, 85.48607773954165623, -129.8825843578381694 ) ) ;
#181601 = CARTESIAN_POINT ( 'NONE',  ( 18.58685178364167712, 47.00654334275795776, -255.2230915614995865 ) ) ;
#181602 = DIRECTION ( 'NONE',  ( 1.000000000000000000, 0.000000000000000000, 0.000000000000000000 ) ) ;
#181603 = FACE_OUTER_BOUND ( 'NONE', #179803, .T. ) ;
#181604 = DIRECTION ( 'NONE',  ( -0.000000000000000000, 0.9770955615653313941, 0.2128009952263603954 ) ) ;
#181607 = ADVANCED_FACE ( 'NONE', ( #24965 ), #4087, .T. ) ;
#181606 = ORIENTED_EDGE ( 'NONE', *, *, #214235, .T. ) ;
#181605 = CARTESIAN_POINT ( 'NONE',  ( 23.04999999999999716, 67.17743825834619997, -190.8731074845244109 ) ) ;
#181608 = AXIS2_PLACEMENT_3D ( 'NONE', #150378, #52533, #116384 ) ;
#181609 = DIRECTION ( 'NONE',  ( 0.000000000000000000, -0.3042567129660269654, -0.9525900758537791946 ) ) ;
#181610 = EDGE_LOOP ( 'NONE', ( #1661, #79904, #7212, #228607 ) ) ;
#181611 = ORIENTED_EDGE ( 'NONE', *, *, #114243, .T. ) ;
#181612 = AXIS2_PLACEMENT_3D ( 'NONE', #46611, #145718, #70078 ) ;
#181613 = CARTESIAN_POINT ( 'NONE',  ( 23.14999999999999858, 4.775700934579428569, -11.84876810404597158 ) ) ;
#181614 = CARTESIAN_POINT ( 'NONE',  ( 19.94784844284926351, 34.43454196362160502, -235.0718703888029779 ) ) ;
#181615 = ORIENTED_EDGE ( 'NONE', *, *, #129836, .F. ) ;
#181616 = DIRECTION ( 'NONE',  ( 0.000000000000000000, 0.000000000000000000, -1.000000000000000000 ) ) ;
#181617 = ADVANCED_FACE ( 'NONE', ( #65343 ), #186601, .F. ) ;
#181618 = LINE ( 'NONE', #23843, #157349 ) ;
#181619 = EDGE_CURVE ( 'NONE', #155405, #29211, #71269, .T. ) ;
#181620 = EDGE_LOOP ( 'NONE', ( #229801, #172525, #80607, #38271, #225550 ) ) ;
#181621 = CIRCLE ( 'NONE', #73312, 0.1000000000000028644 ) ;
#181622 = AXIS2_PLACEMENT_3D ( 'NONE', #96073, #115660, #19121 ) ;
#181623 = CARTESIAN_POINT ( 'NONE',  ( -18.59999999999999787, 21.13195309841794867, -243.6318585593224100 ) ) ;
#181624 = AXIS2_PLACEMENT_3D ( 'NONE', #15625, #250351, #232093 ) ;
#181625 = PLANE ( 'NONE',  #255457 ) ;
#181626 = EDGE_CURVE ( 'NONE', #213687, #246745, #175325, .T. ) ;
#181627 = EDGE_LOOP ( 'NONE', ( #58174, #193022, #20421, #83957 ) ) ;
#181628 = ORIENTED_EDGE ( 'NONE', *, *, #66029, .T. ) ;
#181630 = EDGE_CURVE ( 'NONE', #34286, #12756, #101879, .T. ) ;
#181629 = CARTESIAN_POINT ( 'NONE',  ( -18.59999999999999787, 1.835341550235567887, -145.5551512925629822 ) ) ;
#181631 = VERTEX_POINT ( 'NONE', #181463 ) ;
#181632 = CARTESIAN_POINT ( 'NONE',  ( -20.94999999999999929, 6.846123162363745074, -70.73772626684986164 ) ) ;
#181633 = VERTEX_POINT ( 'NONE', #2787 ) ;
#181635 = ORIENTED_EDGE ( 'NONE', *, *, #198656, .T. ) ;
#181634 = DIRECTION ( 'NONE',  ( 0.000000000000000000, 0.000000000000000000, 1.000000000000000000 ) ) ;
#181636 = LINE ( 'NONE', #79911, #256716 ) ;
#181637 = ORIENTED_EDGE ( 'NONE', *, *, #71151, .F. ) ;
#181638 = LINE ( 'NONE', #102059, #209747 ) ;
#181639 = EDGE_LOOP ( 'NONE', ( #142245, #127852, #82529, #193426 ) ) ;
#181641 = ORIENTED_EDGE ( 'NONE', *, *, #252492, .F. ) ;
#181640 = VERTEX_POINT ( 'NONE', #143601 ) ;
#181642 = PLANE ( 'NONE',  #157196 ) ;
#181643 = AXIS2_PLACEMENT_3D ( 'NONE', #83579, #44505, #245271 ) ;
#181644 = AXIS2_PLACEMENT_3D ( 'NONE', #195869, #17229, #163156 ) ;
#181645 = ORIENTED_EDGE ( 'NONE', *, *, #185926, .T. ) ;
#181646 = EDGE_CURVE ( 'NONE', #127786, #222829, #250312, .T. ) ;
#181647 = EDGE_CURVE ( 'NONE', #10791, #40828, #25470, .T. ) ;
#181648 = VERTEX_POINT ( 'NONE', #170928 ) ;
#181649 = CYLINDRICAL_SURFACE ( 'NONE', #120354, 0.09999999999999939493 ) ;
#181650 = DIRECTION ( 'NONE',  ( -0.000000000000000000, -0.7397360091702755991, -0.6728971962616832059 ) ) ;
#181652 = ORIENTED_EDGE ( 'NONE', *, *, #68181, .F. ) ;
#181651 = DIRECTION ( 'NONE',  ( -1.000000000000000000, 0.000000000000000000, 0.000000000000000000 ) ) ;
#181653 = CARTESIAN_POINT ( 'NONE',  ( -22.57320508075687115, 64.25000000001165290, -69.52310748452440237 ) ) ;
#181654 = EDGE_LOOP ( 'NONE', ( #66828, #80122, #42526, #139911 ) ) ;
#181655 = LINE ( 'NONE', #18715, #82730 ) ;
#181656 = FACE_OUTER_BOUND ( 'NONE', #243262, .T. ) ;
#181657 = ORIENTED_EDGE ( 'NONE', *, *, #214552, .T. ) ;
#181659 = ADVANCED_FACE ( 'NONE', ( #49636 ), #212732, .F. ) ;
#181658 = CARTESIAN_POINT ( 'NONE',  ( -22.39999999999999858, 1.115600667400684642E-11, -100.5000000000000284 ) ) ;
#181660 = DIRECTION ( 'NONE',  ( 1.000000000000000000, 0.000000000000000000, 0.000000000000000000 ) ) ;
#181661 = ORIENTED_EDGE ( 'NONE', *, *, #32797, .F. ) ;
#181663 = ADVANCED_FACE ( 'NONE', ( #190462 ), #171256, .T. ) ;
#181662 = B_SPLINE_CURVE_WITH_KNOTS ( 'NONE', 3,
 ( #206118, #6623, #11798, #148725, #47019, #27523, #7929 ),
 .UNSPECIFIED., .F., .F.,
 ( 4, 3, 4 ),
 ( 0.000000000000000000, 4.520325912680429745E-05, 5.794988040901229230E-05 ),
 .UNSPECIFIED. ) ;
#181664 = PLANE ( 'NONE',  #105562 ) ;
#181665 = VERTEX_POINT ( 'NONE', #109599 ) ;
#181666 = VECTOR ( 'NONE', #215342, 1000.000000000000000 ) ;
#181668 = ORIENTED_EDGE ( 'NONE', *, *, #180997, .F. ) ;
#181667 = ORIENTED_EDGE ( 'NONE', *, *, #153553, .F. ) ;
#181669 = VERTEX_POINT ( 'NONE', #250401 ) ;
#181670 = FACE_OUTER_BOUND ( 'NONE', #3081, .T. ) ;
#181671 = ORIENTED_EDGE ( 'NONE', *, *, #112625, .F. ) ;
#181672 = DIRECTION ( 'NONE',  ( 0.000000000000000000, -0.9651348961777157509, 0.2617529984165032353 ) ) ;
#181673 = ORIENTED_EDGE ( 'NONE', *, *, #75031, .F. ) ;
#181674 = EDGE_CURVE ( 'NONE', #146445, #257922, #66965, .T. ) ;
#181675 = CYLINDRICAL_SURFACE ( 'NONE', #164780, 0.09999999999999939493 ) ;
#181676 = CARTESIAN_POINT ( 'NONE',  ( -18.59999999999999787, 68.97833521811131163, -32.18954208262707795 ) ) ;
#181677 = EDGE_LOOP ( 'NONE', ( #55048, #227588, #4747 ) ) ;
#181678 = ORIENTED_EDGE ( 'NONE', *, *, #151798, .T. ) ;
#181679 = AXIS2_PLACEMENT_3D ( 'NONE', #172242, #11865, #13134 ) ;
#181680 = ADVANCED_FACE ( 'NONE', ( #212581 ), #191755, .F. ) ;
#181681 = ORIENTED_EDGE ( 'NONE', *, *, #128039, .T. ) ;
#181682 = CIRCLE ( 'NONE', #40058, 4.049999999999998046 ) ;
#181683 = DIRECTION ( 'NONE',  ( -0.7071067811865463515, 0.2890913453342128236, -0.6453109281988462786 ) ) ;
#181684 = ORIENTED_EDGE ( 'NONE', *, *, #60826, .F. ) ;
#181685 = CARTESIAN_POINT ( 'NONE',  ( 21.05000000000000071, 36.65892442174472876, -249.5511627012454596 ) ) ;
#181686 = EDGE_CURVE ( 'NONE', #21708, #142373, #58754, .T. ) ;
#181687 = DIRECTION ( 'NONE',  ( -1.000000000000000000, -2.952720810173289112E-16, 0.000000000000000000 ) ) ;
#181688 = CARTESIAN_POINT ( 'NONE',  ( -21.05000000000000071, 11.60000000001115339, -127.0717967697245427 ) ) ;
#181689 = CARTESIAN_POINT ( 'NONE',  ( 21.04999999999999716, 65.37049252075472339, -162.3951280845285794 ) ) ;
#181690 = CARTESIAN_POINT ( 'NONE',  ( 21.14999999999999858, 64.35000000001195986, -102.9231074845243938 ) ) ;
#181691 = DIRECTION ( 'NONE',  ( 0.000000000000000000, 0.000000000000000000, -1.000000000000000000 ) ) ;
#181693 = CARTESIAN_POINT ( 'NONE',  ( 21.08376601933332495, 6.341947271286812793, -100.4362239890700437 ) ) ;
#181692 = DIRECTION ( 'NONE',  ( -1.000000000000000000, -0.000000000000000000, -0.000000000000000000 ) ) ;
#181694 = CARTESIAN_POINT ( 'NONE',  ( -23.15000000000000213, 11.65000000001115588, -121.7500000000000426 ) ) ;
#181695 = LINE ( 'NONE', #162145, #28004 ) ;
#181696 = FACE_OUTER_BOUND ( 'NONE', #132124, .T. ) ;
#181697 = DIRECTION ( 'NONE',  ( 0.000000000000000000, -1.000000000000000000, -6.982962677686265922E-15 ) ) ;
#181698 = AXIS2_PLACEMENT_3D ( 'NONE', #46117, #43563, #24018 ) ;
#181699 = EDGE_LOOP ( 'NONE', ( #156706, #31735, #71955, #157803 ) ) ;
#181700 = AXIS2_PLACEMENT_3D ( 'NONE', #20294, #82772, #60666 ) ;
#181702 = EDGE_LOOP ( 'NONE', ( #3007, #130593, #13498 ) ) ;
#181701 = CARTESIAN_POINT ( 'NONE',  ( 21.05000000000000071, 10.72371710471867701, -108.1649135690876449 ) ) ;
#181703 = VECTOR ( 'NONE', #117404, 1000.000000000000000 ) ;
#181704 = ORIENTED_EDGE ( 'NONE', *, *, #110202, .T. ) ;
#181705 = FACE_OUTER_BOUND ( 'NONE', #179050, .T. ) ;
#181706 = DIRECTION ( 'NONE',  ( 1.000000000000000000, 3.265361837132813093E-16, -0.000000000000000000 ) ) ;
#181707 = AXIS2_PLACEMENT_3D ( 'NONE', #118397, #141785, #182217 ) ;
#181708 = DIRECTION ( 'NONE',  ( 0.000000000000000000, 0.000000000000000000, 1.000000000000000000 ) ) ;
#181709 = ORIENTED_EDGE ( 'NONE', *, *, #254265, .F. ) ;
#181710 = CARTESIAN_POINT ( 'NONE',  ( -20.90000000000000213, 7.986648289447971116, -1.311673547813416718 ) ) ;
#181711 = FACE_OUTER_BOUND ( 'NONE', #19349, .T. ) ;
#181712 = ORIENTED_EDGE ( 'NONE', *, *, #199017, .T. ) ;
#181714 = CARTESIAN_POINT ( 'NONE',  ( -21.00448002041607864, 11.75000000001115552, -140.8483408623105220 ) ) ;
#181713 = VECTOR ( 'NONE', #60733, 1000.000000000000000 ) ;
#181715 = DIRECTION ( 'NONE',  ( 0.000000000000000000, -1.000000000000000000, -7.272083257015735086E-15 ) ) ;
#181716 = CIRCLE ( 'NONE', #115082, 3.999999999999996447 ) ;
#181717 = PLANE ( 'NONE',  #238728 ) ;
#181718 = CIRCLE ( 'NONE', #52525, 11.80000000000000426 ) ;
#181719 = CARTESIAN_POINT ( 'NONE',  ( -18.59999999999999787, -1.835859311432481045, -212.6044391687984785 ) ) ;
#181721 = ORIENTED_EDGE ( 'NONE', *, *, #90771, .T. ) ;
#181720 = DIRECTION ( 'NONE',  ( 0.000000000000000000, -0.03181660087583042251, 0.9994937237965568766 ) ) ;
#181723 = CARTESIAN_POINT ( 'NONE',  ( 18.59999999999999076, 51.96945017402672562, -231.5060697639786440 ) ) ;
#181722 = VECTOR ( 'NONE', #37828, 1000.000000000000000 ) ;
#181725 = ORIENTED_EDGE ( 'NONE', *, *, #155967, .T. ) ;
#181724 = CARTESIAN_POINT ( 'NONE',  ( 23.25000000000000000, -8.999999999988844479, -110.3939691226524786 ) ) ;
#181726 = CARTESIAN_POINT ( 'NONE',  ( -20.94999999999994600, 66.15000000001120384, -5.923107484524795296 ) ) ;
#181727 = DIRECTION ( 'NONE',  ( 1.000000000000000000, 0.000000000000000000, 0.000000000000000000 ) ) ;
#181728 = CARTESIAN_POINT ( 'NONE',  ( -23.25000000000000000, 71.75000000001180922, -81.87310748452433984 ) ) ;
#181729 = CARTESIAN_POINT ( 'NONE',  ( -14.11697426661281440, 9.457410944778571249, -182.5000839737900264 ) ) ;
#181731 = CARTESIAN_POINT ( 'NONE',  ( 23.14999999999999858, 45.21086124044690280, -238.4331873168094091 ) ) ;
#181730 = DIRECTION ( 'NONE',  ( 1.000000000000000000, 7.304098846218163263E-16, -4.217023435051627211E-16 ) ) ;
#181733 = ADVANCED_FACE ( 'NONE', ( #211286 ), #147454, .T. ) ;
#181732 = CARTESIAN_POINT ( 'NONE',  ( -16.92132318717937522, 66.03392997600667513, -190.9007008541723565 ) ) ;
#181734 = CYLINDRICAL_SURFACE ( 'NONE', #178391, 0.09999999999999939493 ) ;
#181735 = CIRCLE ( 'NONE', #173783, 0.1000000000000028644 ) ;
#181736 = CARTESIAN_POINT ( 'NONE',  ( -18.52643265882458579, 10.31973158070286978, -39.05053347133545572 ) ) ;
#181737 = DIRECTION ( 'NONE',  ( 1.000000000000000000, 0.000000000000000000, 0.000000000000000000 ) ) ;
#181738 = DIRECTION ( 'NONE',  ( -0.000000000000000000, -1.000000000000000000, -0.000000000000000000 ) ) ;
#181739 = VERTEX_POINT ( 'NONE', #228290 ) ;
#181740 = DIRECTION ( 'NONE',  ( 0.000000000000000000, -0.2617529984165031243, -0.9651348961777157509 ) ) ;
#181741 = EDGE_LOOP ( 'NONE', ( #75324, #198766, #22863, #205006 ) ) ;
#181742 = EDGE_LOOP ( 'NONE', ( #81586, #101146, #218906, #173679 ) ) ;
#181743 = CARTESIAN_POINT ( 'NONE',  ( -20.96428641294235717, 11.75000000000033928, -26.67489317794143133 ) ) ;
#181744 = EDGE_CURVE ( 'NONE', #144336, #39052, #50891, .T. ) ;
#181745 = DIRECTION ( 'NONE',  ( 0.000000000000000000, 0.8814952561688437216, -0.4721928772777334582 ) ) ;
#181746 = ORIENTED_EDGE ( 'NONE', *, *, #251038, .T. ) ;
#181747 = TOROIDAL_SURFACE ( 'NONE', #69335, 0.6000000000000009770, 0.1000000000000000056 ) ;
#181748 = EDGE_CURVE ( 'NONE', #99016, #64653, #158758, .T. ) ;
#181749 = TOROIDAL_SURFACE ( 'NONE', #202411, 0.2000000000000000111, 0.1000000000000000056 ) ;
#181750 = ORIENTED_EDGE ( 'NONE', *, *, #189256, .T. ) ;
#181751 = AXIS2_PLACEMENT_3D ( 'NONE', #146419, #83853, #23950 ) ;
#181752 = AXIS2_PLACEMENT_3D ( 'NONE', #156432, #160276, #217621 ) ;
#181753 = VERTEX_POINT ( 'NONE', #208730 ) ;
#181754 = DIRECTION ( 'NONE',  ( 0.000000000000000000, 0.9908441862701596881, 0.1350103645451904977 ) ) ;
#181755 = ORIENTED_EDGE ( 'NONE', *, *, #226797, .T. ) ;
#181756 = AXIS2_PLACEMENT_3D ( 'NONE', #99830, #41205, #227192 ) ;
#181757 = CARTESIAN_POINT ( 'NONE',  ( 23.14999999999999858, 7.187745831299792165, -211.5611048126997389 ) ) ;
#181758 = CARTESIAN_POINT ( 'NONE',  ( 20.85000000000000142, -1.149570369575693807, -41.31591248450196474 ) ) ;
#181759 = DIRECTION ( 'NONE',  ( -1.000000000000000000, -2.952720810173289112E-16, 0.000000000000000000 ) ) ;
#181760 = CARTESIAN_POINT ( 'NONE',  ( -16.87683809663752399, 29.49590395944699139, -234.5399335999045718 ) ) ;
#181761 = CYLINDRICAL_SURFACE ( 'NONE', #198356, 0.1000000000000066530 ) ;
#181762 = ADVANCED_FACE ( 'NONE', ( #67915 ), #31399, .T. ) ;
#181763 = FACE_OUTER_BOUND ( 'NONE', #126233, .T. ) ;
#181764 = EDGE_CURVE ( 'NONE', #217337, #181466, #82078, .T. ) ;
#181765 = DIRECTION ( 'NONE',  ( -0.000000000000000000, 0.1350103645451904977, 0.9908441862701597991 ) ) ;
#181767 = ORIENTED_EDGE ( 'NONE', *, *, #210634, .T. ) ;
#181766 = DIRECTION ( 'NONE',  ( -0.000000000000000000, 0.8814952561688430555, -0.4721928772777346239 ) ) ;
#181769 = CARTESIAN_POINT ( 'NONE',  ( 18.39999999999999858, 85.68240343348777799, -29.36626410711146562 ) ) ;
#181768 = CARTESIAN_POINT ( 'NONE',  ( -18.37013991200266005, 62.49123844501968961, -209.3989888458036148 ) ) ;
#181770 = FACE_BOUND ( 'NONE', #180692, .T. ) ;
#181771 = ORIENTED_EDGE ( 'NONE', *, *, #88223, .F. ) ;
#181773 = ADVANCED_FACE ( 'NONE', ( #13099 ), #10525, .T. ) ;
#181772 = DIRECTION ( 'NONE',  ( -1.000000000000000000, 1.836970198721029934E-16, 1.282749433769087757E-30 ) ) ;
#181774 = FACE_OUTER_BOUND ( 'NONE', #34353, .T. ) ;
#181776 = ORIENTED_EDGE ( 'NONE', *, *, #182060, .T. ) ;
#181775 = AXIS2_PLACEMENT_3D ( 'NONE', #22756, #83932, #142653 ) ;
#181777 = AXIS2_PLACEMENT_3D ( 'NONE', #35581, #233766, #198471 ) ;
#181778 = CARTESIAN_POINT ( 'NONE',  ( -20.94999999999999929, 7.021664781911246322, -104.3335654018973315 ) ) ;
#181779 = CARTESIAN_POINT ( 'NONE',  ( -20.64999999999999858, 78.08573236070779444, -228.9307947190811774 ) ) ;
#181780 = ORIENTED_EDGE ( 'NONE', *, *, #235997, .F. ) ;
#181781 = DIRECTION ( 'NONE',  ( 0.000000000000000000, 0.000000000000000000, -1.000000000000000000 ) ) ;
#181782 = DIRECTION ( 'NONE',  ( 0.000000000000000000, 6.938893903907222067E-15, -1.000000000000000000 ) ) ;
#181783 = ADVANCED_FACE ( 'NONE', ( #133046 ), #169636, .F. ) ;
#181784 = DIRECTION ( 'NONE',  ( 0.000000000000000000, 0.2617529984165030132, 0.9651348961777157509 ) ) ;
#181785 = CIRCLE ( 'NONE', #144330, 0.1000000000000024342 ) ;
#181786 = CARTESIAN_POINT ( 'NONE',  ( 18.59999999999999787, 77.36242903720497566, -61.63422623660309796 ) ) ;
#181787 = ORIENTED_EDGE ( 'NONE', *, *, #164870, .T. ) ;
#181788 = EDGE_CURVE ( 'NONE', #183348, #232311, #229571, .T. ) ;
#181789 = CARTESIAN_POINT ( 'NONE',  ( 21.09787244211741708, 67.22462929267454967, -90.78385410020683821 ) ) ;
#181790 = CARTESIAN_POINT ( 'NONE',  ( 18.59999999999998366, 1.115600667400684642E-11, -100.5000000000000426 ) ) ;
#181791 = DIRECTION ( 'NONE',  ( 0.000000000000000000, -0.8096735173027155286, 0.5868805631290315850 ) ) ;
#181792 = CIRCLE ( 'NONE', #69381, 11.89999999999998792 ) ;
#181793 = AXIS2_PLACEMENT_3D ( 'NONE', #144183, #201605, #243289 ) ;
#181794 = CARTESIAN_POINT ( 'NONE',  ( -18.59999999999999787, 36.65892442174935439, -249.5511627012433848 ) ) ;
#181795 = AXIS2_PLACEMENT_3D ( 'NONE', #51334, #72235, #168803 ) ;
#181796 = DIRECTION ( 'NONE',  ( 1.000000000000000000, -0.000000000000000000, 0.000000000000000000 ) ) ;
#181798 = VERTEX_POINT ( 'NONE', #173499 ) ;
#181797 = CARTESIAN_POINT ( 'NONE',  ( 23.25000000000000000, -11.64999999998883595, -55.25000000000004974 ) ) ;
#181799 = CARTESIAN_POINT ( 'NONE',  ( -21.05000000000000071, 6.258842723548718290, -33.46798630681211506 ) ) ;
#181800 = FACE_OUTER_BOUND ( 'NONE', #243389, .T. ) ;
#181801 = DIRECTION ( 'NONE',  ( 1.000000000000000000, -0.000000000000000000, -0.000000000000000000 ) ) ;
#181802 = CARTESIAN_POINT ( 'NONE',  ( 18.59999999999999787, 1.866714910068465239, -112.2526752462820525 ) ) ;
#181803 = DIRECTION ( 'NONE',  ( -1.000000000000000000, -0.000000000000000000, -0.000000000000000000 ) ) ;
#181805 = VERTEX_POINT ( 'NONE', #95188 ) ;
#181804 = DIRECTION ( 'NONE',  ( -1.000000000000000000, -0.000000000000000000, 0.000000000000000000 ) ) ;
#181806 = CYLINDRICAL_SURFACE ( 'NONE', #59052, 0.1000000000000028644 ) ;
#181807 = CARTESIAN_POINT ( 'NONE',  ( -21.64999999999999858, 7.350000000011155166, -88.15000000000004832 ) ) ;
#181808 = CARTESIAN_POINT ( 'NONE',  ( 20.93302460841143287, 67.49317130920637453, -195.4795610751097286 ) ) ;
#181809 = ORIENTED_EDGE ( 'NONE', *, *, #191807, .T. ) ;
#181810 = CARTESIAN_POINT ( 'NONE',  ( -14.22969084473440304, 66.54399267394295236, -151.5344739903776485 ) ) ;
#181811 = CARTESIAN_POINT ( 'NONE',  ( 23.24999999999999289, 64.35000000001228670, -157.8731074845244393 ) ) ;
#181812 = CARTESIAN_POINT ( 'NONE',  ( 18.49999999999999645, 1.728086936794461570, 13.11556499483223348 ) ) ;
#181813 = AXIS2_PLACEMENT_3D ( 'NONE', #124683, #187239, #110237 ) ;
#181814 = VECTOR ( 'NONE', #226645, 1000.000000000000000 ) ;
#181816 = CIRCLE ( 'NONE', #81814, 0.1000000000000079159 ) ;
#181815 = DIRECTION ( 'NONE',  ( 1.000000000000000000, 0.000000000000000000, 0.000000000000000000 ) ) ;
#181817 = ORIENTED_EDGE ( 'NONE', *, *, #123236, .T. ) ;
#181818 = DIRECTION ( 'NONE',  ( 0.000000000000000000, -1.000000000000000000, 0.000000000000000000 ) ) ;
#181819 = EDGE_LOOP ( 'NONE', ( #188000, #160256, #148107 ) ) ;
#181820 = ORIENTED_EDGE ( 'NONE', *, *, #6574, .T. ) ;
#181821 = EDGE_CURVE ( 'NONE', #25682, #95684, #25639, .T. ) ;
#181823 = DIRECTION ( 'NONE',  ( 0.000000000000000000, -1.000000000000000000, 0.000000000000000000 ) ) ;
#181822 = AXIS2_PLACEMENT_3D ( 'NONE', #108110, #51957, #225460 ) ;
#181825 = EDGE_CURVE ( 'NONE', #141325, #249646, #165595, .T. ) ;
#181824 = CARTESIAN_POINT ( 'NONE',  ( -20.54999999999999716, 2.500000000011156409, -180.7246219227620543 ) ) ;
#181826 = DIRECTION ( 'NONE',  ( 1.000000000000000000, 0.000000000000000000, 0.000000000000000000 ) ) ;
#181827 = FACE_OUTER_BOUND ( 'NONE', #249363, .T. ) ;
#181828 = ORIENTED_EDGE ( 'NONE', *, *, #96077, .F. ) ;
#181829 = EDGE_CURVE ( 'NONE', #173853, #216782, #83848, .T. ) ;
#181830 = ADVANCED_FACE ( 'NONE', ( #159040 ), #233438, .F. ) ;
#181831 = CARTESIAN_POINT ( 'NONE',  ( 20.95539060131842746, 10.62386215766680131, -175.1537338136561743 ) ) ;
#181832 = DIRECTION ( 'NONE',  ( 0.000000000000000000, 0.000000000000000000, -1.000000000000000000 ) ) ;
#181833 = EDGE_CURVE ( 'NONE', #239511, #166628, #112947, .T. ) ;
#181834 = CARTESIAN_POINT ( 'NONE',  ( -16.78055652883087134, 9.946776916125346091, -12.66079183759242888 ) ) ;
#181835 = LINE ( 'NONE', #154921, #49505 ) ;
#181836 = CARTESIAN_POINT ( 'NONE',  ( -16.87998658237741623, 9.949999999999983302, -20.63636043226203753 ) ) ;
#181837 = EDGE_CURVE ( 'NONE', #154355, #110815, #4757, .T. ) ;
#181840 = EDGE_CURVE ( 'NONE', #1463, #70494, #78173, .T. ) ;
#181839 = ADVANCED_FACE ( 'NONE', ( #40392 ), #158942, .F. ) ;
#181838 = CARTESIAN_POINT ( 'NONE',  ( -16.89268316805465986, 63.08557629953710943, -213.1216189793661329 ) ) ;
#181841 = ORIENTED_EDGE ( 'NONE', *, *, #230586, .T. ) ;
#181843 = VERTEX_POINT ( 'NONE', #54764 ) ;
#181842 = DIRECTION ( 'NONE',  ( -1.000000000000000000, 0.000000000000000000, -0.000000000000000000 ) ) ;
#181844 = ORIENTED_EDGE ( 'NONE', *, *, #111898, .T. ) ;
#181845 = DIRECTION ( 'NONE',  ( 0.000000000000000000, -6.982962677686266711E-15, 1.000000000000000000 ) ) ;
#181846 = ORIENTED_EDGE ( 'NONE', *, *, #166321, .F. ) ;
#181847 = DIRECTION ( 'NONE',  ( -1.000000000000000000, 0.000000000000000000, 0.000000000000000000 ) ) ;
#181848 = CARTESIAN_POINT ( 'NONE',  ( -21.04999999999999716, 6.344723404101477726, -100.4852821434760415 ) ) ;
#181849 = CARTESIAN_POINT ( 'NONE',  ( 18.59999999999999787, 1.115600667400684642E-11, -33.50000000000000000 ) ) ;
#181850 = ORIENTED_EDGE ( 'NONE', *, *, #209808, .F. ) ;
#181851 = DIRECTION ( 'NONE',  ( -5.603264701231742896E-32, 0.2128009952263605620, -0.9770955615653313941 ) ) ;
#181852 = DIRECTION ( 'NONE',  ( 0.000000000000000000, 1.000000000000000000, 0.000000000000000000 ) ) ;
#181853 = AXIS2_PLACEMENT_3D ( 'NONE', #248828, #41971, #234373 ) ;
#181854 = ORIENTED_EDGE ( 'NONE', *, *, #183702, .T. ) ;
#181855 = CARTESIAN_POINT ( 'NONE',  ( -14.11361717019516249, 9.457426452500060421, -152.5000418684000465 ) ) ;
#181856 = EDGE_CURVE ( 'NONE', #84452, #181843, #96350, .T. ) ;
#181858 = VERTEX_POINT ( 'NONE', #56028 ) ;
#181857 = DIRECTION ( 'NONE',  ( -0.000000000000000000, -0.000000000000000000, -1.000000000000000000 ) ) ;
#181859 = DIRECTION ( 'NONE',  ( 1.000000000000000000, 1.394253735153569469E-16, 2.602809386958778209E-16 ) ) ;
#181860 = AXIS2_PLACEMENT_3D ( 'NONE', #153323, #236659, #253645 ) ;
#181861 = EDGE_CURVE ( 'NONE', #143707, #121787, #125587, .T. ) ;
#181862 = EDGE_CURVE ( 'NONE', #188520, #111659, #157783, .T. ) ;
#181863 = AXIS2_PLACEMENT_3D ( 'NONE', #151881, #13627, #231400 ) ;
#181864 = ORIENTED_EDGE ( 'NONE', *, *, #201488, .F. ) ;
#181866 = CARTESIAN_POINT ( 'NONE',  ( 21.14999999999999503, -11.74999999998883560, -122.2500000000000284 ) ) ;
#181865 = AXIS2_PLACEMENT_3D ( 'NONE', #21135, #236298, #181482 ) ;
#181868 = EDGE_CURVE ( 'NONE', #225961, #61206, #104700, .T. ) ;
#181867 = CARTESIAN_POINT ( 'NONE',  ( 21.07888907270776002, 10.72506921352637654, -79.22119358683323753 ) ) ;
#181869 = DIRECTION ( 'NONE',  ( 0.000000000000000000, 0.8660254037844378194, 0.5000000000000016653 ) ) ;
#181870 = ORIENTED_EDGE ( 'NONE', *, *, #209439, .T. ) ;
#181871 = CARTESIAN_POINT ( 'NONE',  ( 23.14999999999999858, 28.08470566095357057, -239.2860081655328770 ) ) ;
#181872 = DIRECTION ( 'NONE',  ( 0.000000000000000000, -0.4999999999999689138, 0.8660254037844565822 ) ) ;
#181873 = CYLINDRICAL_SURFACE ( 'NONE', #151583, 0.1000000000000028644 ) ;
#181874 = EDGE_CURVE ( 'NONE', #68761, #104106, #246225, .T. ) ;
#181875 = ORIENTED_EDGE ( 'NONE', *, *, #238209, .T. ) ;
#181876 = CIRCLE ( 'NONE', #131805, 2.000000000000002665 ) ;
#181877 = CIRCLE ( 'NONE', #27789, 0.2000000000000057288 ) ;
#181878 = ORIENTED_EDGE ( 'NONE', *, *, #215424, .T. ) ;
#181879 = AXIS2_PLACEMENT_3D ( 'NONE', #108902, #50202, #151914 ) ;
#181880 = EDGE_LOOP ( 'NONE', ( #179221, #226574, #43990, #237606 ) ) ;
#181881 = AXIS2_PLACEMENT_3D ( 'NONE', #153714, #130224, #195372 ) ;
#181882 = CARTESIAN_POINT ( 'NONE',  ( 18.59999999999996945, 10.33248238082518711, -39.09484654391314962 ) ) ;
#181883 = CARTESIAN_POINT ( 'NONE',  ( 21.05000000000000071, 8.776282895303626930, -45.65000000000000568 ) ) ;
#181886 = ORIENTED_EDGE ( 'NONE', *, *, #54389, .F. ) ;
#181885 = CARTESIAN_POINT ( 'NONE',  ( 23.14999999999999858, 2.100000000011158274, -200.9999999999999432 ) ) ;
#181884 =( BOUNDED_SURFACE ( )  B_SPLINE_SURFACE ( 3, 2, ( 
 ( #224450, #242726, #126644 ),
 ( #45821, #141078, #185336 ),
 ( #64107, #143631, #2825 ),
 ( #122812, #220614, #160666 ),
 ( #27585, #202325, #62816 ),
 ( #125367, #165794, #244009 ) ),
 .UNSPECIFIED., .F., .F., .T. ) 
 B_SPLINE_SURFACE_WITH_KNOTS ( ( 4, 2, 4 ),
 ( 3, 3 ),
 ( 6.719893378901104289E-05, 0.0002757154632485492199, 0.0004842319927080873969 ),
 ( 0.000000000000000000, 1.000000000000000000 ),
 .UNSPECIFIED. ) 
 GEOMETRIC_REPRESENTATION_ITEM ( )  RATIONAL_B_SPLINE_SURFACE ( (
 ( 1.000000000000000000, 0.7250110520819756932, 1.000000000000000000),
 ( 1.000000000000000000, 0.7277932058358369538, 1.000000000000000000),
 ( 1.000000000000000000, 0.7278452872618610403, 1.000000000000000000),
 ( 1.000000000000000000, 0.7221445671548210044, 1.000000000000000000),
 ( 1.000000000000000000, 0.7163662143780332725, 1.000000000000000000),
 ( 1.000000000000000000, 0.7071067811865475727, 1.000000000000000000) ) ) 
 REPRESENTATION_ITEM ( '' )  SURFACE ( )  );
#181887 = DIRECTION ( 'NONE',  ( 0.000000000000000000, 0.5826443254699750218, 0.8127272543711313579 ) ) ;
#181889 = AXIS2_PLACEMENT_3D ( 'NONE', #257520, #159780, #219731 ) ;
#181888 = FACE_OUTER_BOUND ( 'NONE', #145130, .T. ) ;
#181890 = DIRECTION ( 'NONE',  ( 1.000000000000000000, 0.000000000000000000, -0.000000000000000000 ) ) ;
#181891 = AXIS2_PLACEMENT_3D ( 'NONE', #231414, #31942, #73641 ) ;
#181892 = DIRECTION ( 'NONE',  ( 2.694716079187272946E-16, -1.000000000000000000, 0.000000000000000000 ) ) ;
#181893 = CARTESIAN_POINT ( 'NONE',  ( -18.39999999999999858, 85.50000000001209344, -129.4910380878245633 ) ) ;
#181894 = LINE ( 'NONE', #4520, #88933 ) ;
#181896 = ORIENTED_EDGE ( 'NONE', *, *, #71226, .F. ) ;
#181895 = DIRECTION ( 'NONE',  ( 0.000000000000000000, 1.000000000000000000, 0.000000000000000000 ) ) ;
#181898 = ORIENTED_EDGE ( 'NONE', *, *, #78334, .F. ) ;
#181897 = LINE ( 'NONE', #26696, #240262 ) ;
#181899 = DIRECTION ( 'NONE',  ( 1.000000000000000000, 0.000000000000000000, 0.000000000000000000 ) ) ;
#181900 = ORIENTED_EDGE ( 'NONE', *, *, #176606, .T. ) ;
#181901 = ORIENTED_EDGE ( 'NONE', *, *, #28063, .T. ) ;
#181902 = DIRECTION ( 'NONE',  ( 0.000000000000000000, 6.982962677686266711E-15, -1.000000000000000000 ) ) ;
#181903 = CIRCLE ( 'NONE', #19603, 0.5000000000000004441 ) ;
#181904 = VECTOR ( 'NONE', #73776, 1000.000000000000000 ) ;
#181905 = FACE_OUTER_BOUND ( 'NONE', #230431, .T. ) ;
#181906 = CARTESIAN_POINT ( 'NONE',  ( -18.40000000000000213, 61.67221194087674263, -212.7442625272979058 ) ) ;
#181907 = DIRECTION ( 'NONE',  ( 0.000000000000000000, -0.9915357197604982575, 0.1298341882519033486 ) ) ;
#181908 = DIRECTION ( 'NONE',  ( 0.000000000000000000, 0.000000000000000000, 1.000000000000000000 ) ) ;
#181909 = ORIENTED_EDGE ( 'NONE', *, *, #222194, .T. ) ;
#181910 = CARTESIAN_POINT ( 'NONE',  ( -23.25000000000000000, 45.93315328338058379, -256.6017782078560003 ) ) ;
#181912 = ORIENTED_EDGE ( 'NONE', *, *, #158484, .T. ) ;
#181911 = ADVANCED_FACE ( 'NONE', ( #196840 ), #138141, .T. ) ;
#181913 = ORIENTED_EDGE ( 'NONE', *, *, #55272, .T. ) ;
#181914 = LINE ( 'NONE', #123220, #255884 ) ;
#181915 = AXIS2_PLACEMENT_3D ( 'NONE', #178860, #17195, #114989 ) ;
#181916 = ADVANCED_FACE ( 'NONE', ( #243684 ), #2488, .T. ) ;
#181917 = ORIENTED_EDGE ( 'NONE', *, *, #146481, .T. ) ;
#181918 = CARTESIAN_POINT ( 'NONE',  ( 21.00023020733501866, 76.00000000001243450, -176.4139767297927222 ) ) ;
#181919 = CARTESIAN_POINT ( 'NONE',  ( -16.97683809663753252, 61.10204373784839049, -220.4418724925039044 ) ) ;
#181920 = ADVANCED_FACE ( 'NONE', ( #140728 ), #79607, .T. ) ;
#181921 = EDGE_LOOP ( 'NONE', ( #42331, #131388, #76377, #259, #224315, #93379, #137385, #70744, #139234, #92163, #164333, #186725 ) ) ;
#181923 = ADVANCED_FACE ( 'NONE', ( #184998, #161607 ), #242390, .T. ) ;
#181922 = CARTESIAN_POINT ( 'NONE',  ( 23.24999999999999645, 10.93950603019935564, -232.9027774310573022 ) ) ;
#181924 = ORIENTED_EDGE ( 'NONE', *, *, #179227, .T. ) ;
#181925 = CARTESIAN_POINT ( 'NONE',  ( 21.14999999999999858, 69.45934304831143891, -203.4231074845244223 ) ) ;
#181926 = ORIENTED_EDGE ( 'NONE', *, *, #23463, .F. ) ;
#181927 = AXIS2_PLACEMENT_3D ( 'NONE', #241892, #63250, #125795 ) ;
#181928 = DIRECTION ( 'NONE',  ( 1.000000000000000000, 0.000000000000000000, -0.000000000000000000 ) ) ;
#181929 = AXIS2_PLACEMENT_3D ( 'NONE', #218479, #99806, #256274 ) ;
#181930 = LINE ( 'NONE', #44986, #59681 ) ;
#181931 = CIRCLE ( 'NONE', #148816, 0.1000000000000028644 ) ;
#181932 = EDGE_LOOP ( 'NONE', ( #219138, #127564, #97020, #85079, #148552 ) ) ;
#181933 = CYLINDRICAL_SURFACE ( 'NONE', #169498, 7.899999999999990585 ) ;
#181935 = EDGE_LOOP ( 'NONE', ( #31626, #138149, #105141, #214534 ) ) ;
#181934 = CARTESIAN_POINT ( 'NONE',  ( 20.94999999999999574, 72.02722222756958104, -225.1832529173024398 ) ) ;
#181936 = DIRECTION ( 'NONE',  ( 0.000000000000000000, -0.9770955615653321713, -0.2128009952263581472 ) ) ;
#181937 = EDGE_LOOP ( 'NONE', ( #202264, #3640, #239688, #125904 ) ) ;
#181938 = AXIS2_PLACEMENT_3D ( 'NONE', #252861, #110787, #109495 ) ;
#181939 = EDGE_CURVE ( 'NONE', #66990, #112216, #203272, .T. ) ;
#181940 = EDGE_CURVE ( 'NONE', #50036, #82237, #241140, .T. ) ;
#181941 = CARTESIAN_POINT ( 'NONE',  ( -16.89020380669786192, 66.05000000001261640, -190.7656963364138676 ) ) ;
#181942 = ORIENTED_EDGE ( 'NONE', *, *, #111090, .F. ) ;
#181943 = DIRECTION ( 'NONE',  ( -1.000000000000000000, 0.000000000000000000, 0.000000000000000000 ) ) ;
#181944 = CARTESIAN_POINT ( 'NONE',  ( 20.00000000000000355, 64.25000000001250555, -178.8731074845244393 ) ) ;
#181945 = VECTOR ( 'NONE', #23957, 1000.000000000000000 ) ;
#181946 = DIRECTION ( 'NONE',  ( -0.000000000000000000, -1.000000000000000000, 6.308085367188393199E-16 ) ) ;
#181947 = DIRECTION ( 'NONE',  ( -1.000000000000000000, -0.000000000000000000, 0.000000000000000000 ) ) ;
#181948 = AXIS2_PLACEMENT_3D ( 'NONE', #118535, #200617, #104052 ) ;
#181949 = CARTESIAN_POINT ( 'NONE',  ( -15.75000000000000355, 66.65000000001258229, -186.7731074845243882 ) ) ;
#181950 = DIRECTION ( 'NONE',  ( -2.489438768765008884E-17, -0.1686199900910312910, 0.9856811345164826488 ) ) ;
#181951 = AXIS2_PLACEMENT_3D ( 'NONE', #109319, #190174, #11540 ) ;
#181952 = VERTEX_POINT ( 'NONE', #220290 ) ;
#181953 = FACE_OUTER_BOUND ( 'NONE', #86063, .T. ) ;
#181955 = ADVANCED_FACE ( 'NONE', ( #65044 ), #179875, .F. ) ;
#181954 = CARTESIAN_POINT ( 'NONE',  ( 20.94999999999999574, -11.48912529307605901, -3.000000000000002665 ) ) ;
#181956 = CARTESIAN_POINT ( 'NONE',  ( 21.09096482362048164, 6.363544365415576110, -100.4605517212259969 ) ) ;
#181957 = CARTESIAN_POINT ( 'NONE',  ( -21.05000000000000071, 0.6656436123793491033, -212.6810495496487476 ) ) ;
#181958 = ADVANCED_BREP_SHAPE_REPRESENTATION ( '', ( #103691, #2425 ), #231953 ) ;
#181959 = ORIENTED_EDGE ( 'NONE', *, *, #101487, .T. ) ;
#181960 = EDGE_CURVE ( 'NONE', #121283, #138529, #183864, .T. ) ;
#181961 = CARTESIAN_POINT ( 'NONE',  ( -20.64999999999999858, 4.250000000011156409, -112.7500000000000284 ) ) ;
#181962 = ORIENTED_EDGE ( 'NONE', *, *, #183428, .T. ) ;
#181963 = CARTESIAN_POINT ( 'NONE',  ( -18.50000000000000000, 1.162701749949165642, -75.10000000000003695 ) ) ;
#181965 = ORIENTED_EDGE ( 'NONE', *, *, #131208, .T. ) ;
#181964 = CIRCLE ( 'NONE', #99114, 0.09999999999999939493 ) ;
#181966 = DIRECTION ( 'NONE',  ( -0.000000000000000000, 0.4791956752371484551, 0.8777080977375184556 ) ) ;
#181967 = VERTEX_POINT ( 'NONE', #25932 ) ;
#181969 = ORIENTED_EDGE ( 'NONE', *, *, #41052, .F. ) ;
#181968 = DIRECTION ( 'NONE',  ( 1.000000000000000000, 0.000000000000000000, 0.000000000000000000 ) ) ;
#181970 = FACE_OUTER_BOUND ( 'NONE', #52445, .T. ) ;
#181971 = ORIENTED_EDGE ( 'NONE', *, *, #107275, .T. ) ;
#181972 = EDGE_CURVE ( 'NONE', #34155, #135145, #224109, .T. ) ;
#181973 = DIRECTION ( 'NONE',  ( 1.000000000000000000, 0.000000000000000000, 0.000000000000000000 ) ) ;
#181974 = EDGE_CURVE ( 'NONE', #219191, #212760, #42212, .T. ) ;
#181975 = ORIENTED_EDGE ( 'NONE', *, *, #11425, .T. ) ;
#181976 = ORIENTED_EDGE ( 'NONE', *, *, #126436, .T. ) ;
#181977 = LINE ( 'NONE', #81552, #230874 ) ;
#181978 = CARTESIAN_POINT ( 'NONE',  ( -16.85718274719476995, 14.20298511439310296, -219.3341783597842038 ) ) ;
#181979 = CARTESIAN_POINT ( 'NONE',  ( -16.86757978335471719, 66.03434962097777827, -123.9251028313568526 ) ) ;
#181980 = EDGE_CURVE ( 'NONE', #80064, #174146, #117226, .T. ) ;
#181981 = VECTOR ( 'NONE', #144877, 1000.000000000000000 ) ;
#181982 = TOROIDAL_SURFACE ( 'NONE', #11287, 0.2000000000000000111, 0.1000000000000000056 ) ;
#181983 = AXIS2_PLACEMENT_3D ( 'NONE', #237717, #235149, #138573 ) ;
#181984 = VECTOR ( 'NONE', #170248, 1000.000000000000000 ) ;
#181985 = VERTEX_POINT ( 'NONE', #82004 ) ;
#181986 = ORIENTED_EDGE ( 'NONE', *, *, #24997, .F. ) ;
#181987 = DIRECTION ( 'NONE',  ( 1.000000000000000000, 0.000000000000000000, 0.000000000000000000 ) ) ;
#181988 =( BOUNDED_CURVE ( )  B_SPLINE_CURVE ( 3, ( #66370, #27281, #205870, #164196 ),
 .UNSPECIFIED., .F., .T. ) 
 B_SPLINE_CURVE_WITH_KNOTS ( ( 4, 4 ),
 ( 0.06456096931748397938, 3.077031684272309331 ),
 .UNSPECIFIED. ) 
 CURVE ( )  GEOMETRIC_REPRESENTATION_ITEM ( )  RATIONAL_B_SPLINE_CURVE ( ( 1.000000000000000000, 0.3763440860215099271, 0.3763440860215099271, 1.000000000000000000 ) ) 
 REPRESENTATION_ITEM ( '' )  );
#181989 = ADVANCED_FACE ( 'NONE', ( #162892, #221524 ), #42920, .F. ) ;
#181991 = ORIENTED_EDGE ( 'NONE', *, *, #43593, .T. ) ;
#181990 = LINE ( 'NONE', #4612, #130642 ) ;
#181992 = DIRECTION ( 'NONE',  ( 1.000000000000000000, 0.000000000000000000, 0.000000000000000000 ) ) ;
#181993 = DIRECTION ( 'NONE',  ( -0.7071067811865474617, 0.7071067811865474617, 4.937700262164531476E-15 ) ) ;
#181994 = CARTESIAN_POINT ( 'NONE',  ( -16.83794479845802172, 63.06835707360122711, -213.2820116777518535 ) ) ;
#181995 = EDGE_CURVE ( 'NONE', #231430, #130380, #144568, .T. ) ;
#181996 = AXIS2_PLACEMENT_3D ( 'NONE', #137202, #198460, #19847 ) ;
#181998 = FACE_OUTER_BOUND ( 'NONE', #27519, .T. ) ;
#181997 = DIRECTION ( 'NONE',  ( 1.000000000000000000, 0.000000000000000000, 0.000000000000000000 ) ) ;
#181999 = DIRECTION ( 'NONE',  ( -0.000000000000000000, -6.982962677686266711E-15, 1.000000000000000000 ) ) ;
#182000 = FACE_OUTER_BOUND ( 'NONE', #116705, .T. ) ;
#182001 = TOROIDAL_SURFACE ( 'NONE', #69590, 0.2000000000000000111, 0.1000000000000000056 ) ;
#182002 = VECTOR ( 'NONE', #253306, 1000.000000000000114 ) ;
#182003 = DIRECTION ( 'NONE',  ( 1.000000000000000000, 0.000000000000000000, -0.000000000000000000 ) ) ;
#182004 = ORIENTED_EDGE ( 'NONE', *, *, #203808, .T. ) ;
#182005 = CIRCLE ( 'NONE', #190405, 0.09999999999999939493 ) ;
#182006 = ORIENTED_EDGE ( 'NONE', *, *, #218988, .T. ) ;
#182007 = EDGE_CURVE ( 'NONE', #241874, #253941, #122465, .T. ) ;
#182008 = LINE ( 'NONE', #144132, #47957 ) ;
#182009 = EDGE_LOOP ( 'NONE', ( #58302, #204891, #199321, #169507 ) ) ;
#182010 = DIRECTION ( 'NONE',  ( 0.000000000000000000, 0.000000000000000000, -1.000000000000000000 ) ) ;
#182011 = ORIENTED_EDGE ( 'NONE', *, *, #52338, .T. ) ;
#182012 = CARTESIAN_POINT ( 'NONE',  ( 20.94788355080264353, 65.69792220476342948, -131.0335554128461979 ) ) ;
#182015 = ORIENTED_EDGE ( 'NONE', *, *, #134138, .T. ) ;
#182014 = VERTEX_POINT ( 'NONE', #61196 ) ;
#182013 = AXIS2_PLACEMENT_3D ( 'NONE', #171178, #188124, #14649 ) ;
#182016 = CARTESIAN_POINT ( 'NONE',  ( -22.39999999999999858, 1.148907358139439339E-11, -201.0000000000015064 ) ) ;
#182017 = ORIENTED_EDGE ( 'NONE', *, *, #117153, .F. ) ;
#182018 = ORIENTED_EDGE ( 'NONE', *, *, #40321, .T. ) ;
#182019 = DIRECTION ( 'NONE',  ( 0.000000000000000000, 0.000000000000000000, -1.000000000000000000 ) ) ;
#182020 = CARTESIAN_POINT ( 'NONE',  ( -21.07971444708686093, 75.91217656369416034, -109.3528995661508674 ) ) ;
#182022 = ORIENTED_EDGE ( 'NONE', *, *, #94939, .F. ) ;
#182021 = FACE_OUTER_BOUND ( 'NONE', #222487, .T. ) ;
#182023 = DIRECTION ( 'NONE',  ( -0.000000000000000000, -6.982962677686266711E-15, 1.000000000000000000 ) ) ;
#182024 = CARTESIAN_POINT ( 'NONE',  ( 20.93975676684922504, 65.68895814178239334, -97.50265578621379348 ) ) ;
#182026 = ORIENTED_EDGE ( 'NONE', *, *, #128742, .T. ) ;
#182025 = DIRECTION ( 'NONE',  ( -1.000000000000000000, 0.000000000000000000, -0.000000000000000000 ) ) ;
#182027 = CARTESIAN_POINT ( 'NONE',  ( 20.85000000000000142, 67.23127455305835554, -235.8551265064784559 ) ) ;
#182028 = ORIENTED_EDGE ( 'NONE', *, *, #42057, .T. ) ;
#182030 = FACE_OUTER_BOUND ( 'NONE', #204171, .T. ) ;
#182029 = TOROIDAL_SURFACE ( 'NONE', #236189, 0.2000000000000000111, 0.1000000000000000056 ) ;
#182032 = VERTEX_POINT ( 'NONE', #201993 ) ;
#182031 = FACE_OUTER_BOUND ( 'NONE', #100456, .T. ) ;
#182033 = FACE_OUTER_BOUND ( 'NONE', #147358, .T. ) ;
#182034 = DIRECTION ( 'NONE',  ( 0.000000000000000000, 0.9983803033886529121, 0.05689261644169053833 ) ) ;
#182035 = CARTESIAN_POINT ( 'NONE',  ( 20.96077737575326694, 11.62390063401587170, -60.14079195710662162 ) ) ;
#182036 = AXIS2_PLACEMENT_3D ( 'NONE', #126996, #149149, #203957 ) ;
#182037 = ORIENTED_EDGE ( 'NONE', *, *, #67234, .F. ) ;
#182039 = CARTESIAN_POINT ( 'NONE',  ( -22.50000000000000000, 64.35042919246758686, -170.1231074845244393 ) ) ;
#182038 = FACE_OUTER_BOUND ( 'NONE', #221680, .T. ) ;
#182040 = CARTESIAN_POINT ( 'NONE',  ( -15.39126916658602973, 66.61042836546539547, -85.20546677215520504 ) ) ;
#182041 = SPHERICAL_SURFACE ( 'NONE', #101717, 0.1000000000000000056 ) ;
#182042 = VECTOR ( 'NONE', #167811, 1000.000000000000000 ) ;
#182043 = CIRCLE ( 'NONE', #248675, 1.749999999999998002 ) ;
#182044 = DIRECTION ( 'NONE',  ( 1.000000000000000000, 0.000000000000000000, 0.000000000000000000 ) ) ;
#182045 = CYLINDRICAL_SURFACE ( 'NONE', #30357, 0.9000000000000014655 ) ;
#182046 = ORIENTED_EDGE ( 'NONE', *, *, #30080, .T. ) ;
#182047 = EDGE_LOOP ( 'NONE', ( #110594, #109783, #173963, #174368 ) ) ;
#182048 = VERTEX_POINT ( 'NONE', #41658 ) ;
#182049 = PRODUCT_DEFINITION_FORMATION_WITH_SPECIFIED_SOURCE ( 'ANY', '', #172353, .NOT_KNOWN. ) ;
#182050 = CARTESIAN_POINT ( 'NONE',  ( -21.05000000000000071, 36.73178316696986911, -249.7991537124309218 ) ) ;
#182051 = CIRCLE ( 'NONE', #7240, 0.1999999999999893807 ) ;
#182052 = VERTEX_POINT ( 'NONE', #22085 ) ;
#182053 = CARTESIAN_POINT ( 'NONE',  ( 21.05000000000000071, 68.17695920783671681, -227.9262201573640141 ) ) ;
#182054 = ORIENTED_EDGE ( 'NONE', *, *, #249728, .F. ) ;
#182056 = CARTESIAN_POINT ( 'NONE',  ( 22.39999999999999503, 76.00000000001273293, -211.3138870828977360 ) ) ;
#182055 = AXIS2_PLACEMENT_3D ( 'NONE', #36181, #72755, #231810 ) ;
#182057 = EDGE_CURVE ( 'NONE', #188351, #134102, #138048, .T. ) ;
#182058 = CARTESIAN_POINT ( 'NONE',  ( 16.87683809663749557, 63.08573235307424198, -213.1276215869287967 ) ) ;
#182059 = EDGE_CURVE ( 'NONE', #173016, #57651, #17280, .T. ) ;
#182060 = EDGE_CURVE ( 'NONE', #116777, #14829, #92269, .T. ) ;
#182061 = ORIENTED_EDGE ( 'NONE', *, *, #193925, .F. ) ;
#182062 = DIRECTION ( 'NONE',  ( -1.000000000000000000, 0.000000000000000000, 0.000000000000000000 ) ) ;
#182063 = AXIS2_PLACEMENT_3D ( 'NONE', #236005, #57352, #232183 ) ;
#182064 = EDGE_LOOP ( 'NONE', ( #2999, #150403, #243690, #1870 ) ) ;
#182065 = ORIENTED_EDGE ( 'NONE', *, *, #146174, .T. ) ;
#182066 = ORIENTED_EDGE ( 'NONE', *, *, #57442, .T. ) ;
#182068 = CARTESIAN_POINT ( 'NONE',  ( 21.05000000000000071, 85.40000000001198543, -112.9170766071766820 ) ) ;
#182067 = VECTOR ( 'NONE', #228569, 1000.000000000000000 ) ;
#182069 = CARTESIAN_POINT ( 'NONE',  ( 22.49999999999999645, 75.91119002362582080, -215.1728704025562706 ) ) ;
#182070 = DIRECTION ( 'NONE',  ( 0.000000000000000000, -0.9770955615653316162, -0.2128009952263604232 ) ) ;
#182071 = LINE ( 'NONE', #3407, #165565 ) ;
#182072 = CARTESIAN_POINT ( 'NONE',  ( -21.14999999999999858, 60.91865828504416669, -234.1430899377568551 ) ) ;
#182073 = CARTESIAN_POINT ( 'NONE',  ( 20.94999999999999574, -10.53375947859273865, -206.2621204135720632 ) ) ;
#182074 = ADVANCED_FACE ( 'NONE', ( #229271 ), #127595, .T. ) ;
#182076 = CARTESIAN_POINT ( 'NONE',  ( 18.49999999999999645, -1.835341550213255957, -145.5551512925629822 ) ) ;
#182075 = CARTESIAN_POINT ( 'NONE',  ( 20.85000000000000142, 11.75000000001115907, -194.2161343370218560 ) ) ;
#182077 = DIRECTION ( 'NONE',  ( 0.000000000000000000, -1.000000000000000000, 0.000000000000000000 ) ) ;
#182079 = ORIENTED_EDGE ( 'NONE', *, *, #244160, .F. ) ;
#182078 = DIRECTION ( 'NONE',  ( -1.000000000000000000, 0.000000000000000000, 0.000000000000000000 ) ) ;
#182080 = CARTESIAN_POINT ( 'NONE',  ( 21.08134388332232234, 69.66531941949399709, -103.0989264020313669 ) ) ;
#182081 = CIRCLE ( 'NONE', #94574, 7.900000000000007461 ) ;
#182082 = CARTESIAN_POINT ( 'NONE',  ( -23.25000000000000000, 87.65000000001192859, -106.1231074845242262 ) ) ;
#182083 = TOROIDAL_SURFACE ( 'NONE', #82082, 0.2000000000000000111, 0.1000000000000000056 ) ;
#182084 = EDGE_LOOP ( 'NONE', ( #240594, #139094, #7796, #83654 ) ) ;
#182085 = DIRECTION ( 'NONE',  ( 1.000000000000000000, 0.000000000000000000, 0.000000000000000000 ) ) ;
#182086 = DIRECTION ( 'NONE',  ( 1.000000000000000000, 0.000000000000000000, 0.000000000000000000 ) ) ;
#182087 = FACE_OUTER_BOUND ( 'NONE', #102124, .T. ) ;
#182088 = VERTEX_POINT ( 'NONE', #210985 ) ;
#182089 = CIRCLE ( 'NONE', #140373, 0.1999999999999908795 ) ;
#182090 = CARTESIAN_POINT ( 'NONE',  ( -23.25000000000000000, -6.688413578037177842, -212.5825622730469036 ) ) ;
#182091 = CARTESIAN_POINT ( 'NONE',  ( 18.69999999999999929, 5.488301202077013663, 16.39999999999999858 ) ) ;
#182093 = VERTEX_POINT ( 'NONE', #11511 ) ;
#182092 = AXIS2_PLACEMENT_3D ( 'NONE', #65015, #24646, #8903 ) ;
#182094 = ORIENTED_EDGE ( 'NONE', *, *, #87188, .T. ) ;
#182095 = DIRECTION ( 'NONE',  ( 0.000000000000000000, 0.000000000000000000, -1.000000000000000000 ) ) ;
#182097 = ORIENTED_EDGE ( 'NONE', *, *, #82486, .T. ) ;
#182096 = EDGE_CURVE ( 'NONE', #132176, #133329, #171890, .T. ) ;
#182098 = LINE ( 'NONE', #226321, #52854 ) ;
#182099 = EDGE_CURVE ( 'NONE', #179033, #143962, #192251, .T. ) ;
#182100 = CARTESIAN_POINT ( 'NONE',  ( -18.31572283045127847, -9.548437830874760834, -174.3506256510583796 ) ) ;
#182101 = CARTESIAN_POINT ( 'NONE',  ( -23.25000000000000000, -1.835859311432481045, -145.5044391687985694 ) ) ;
#182102 = FACE_OUTER_BOUND ( 'NONE', #141599, .T. ) ;
#182103 = ORIENTED_EDGE ( 'NONE', *, *, #133528, .T. ) ;
#182104 = FACE_OUTER_BOUND ( 'NONE', #33503, .T. ) ;
#182105 = AXIS2_PLACEMENT_3D ( 'NONE', #62741, #143547, #142264 ) ;
#182106 = DIRECTION ( 'NONE',  ( 1.000000000000000000, -0.000000000000000000, 0.000000000000000000 ) ) ;
#182107 = VECTOR ( 'NONE', #161851, 1000.000000000000114 ) ;
#182108 = EDGE_CURVE ( 'NONE', #107466, #256132, #167152, .T. ) ;
#182109 = CYLINDRICAL_SURFACE ( 'NONE', #170349, 7.900000000000007461 ) ;
#182110 = CARTESIAN_POINT ( 'NONE',  ( -23.15000000000000213, -8.999999999988846255, -143.8939691226524644 ) ) ;
#182111 = ORIENTED_EDGE ( 'NONE', *, *, #80246, .F. ) ;
#182112 = VECTOR ( 'NONE', #38630, 1000.000000000000000 ) ;
#182114 = ORIENTED_EDGE ( 'NONE', *, *, #245029, .T. ) ;
#182113 = DIRECTION ( 'NONE',  ( -1.836970198721029934E-16, 1.000000000000000000, 0.000000000000000000 ) ) ;
#182115 = FACE_OUTER_BOUND ( 'NONE', #189040, .T. ) ;
#182116 = DIRECTION ( 'NONE',  ( 1.000000000000000000, 0.000000000000000000, 0.000000000000000000 ) ) ;
#182117 = CARTESIAN_POINT ( 'NONE',  ( -21.14999999999999858, 11.65000000001115588, -167.5999999999999659 ) ) ;
#182118 = CARTESIAN_POINT ( 'NONE',  ( -23.25000000000000000, 67.85125148167622910, -227.9794913823769491 ) ) ;
#182119 = CARTESIAN_POINT ( 'NONE',  ( -16.97683809663752186, 9.849999999999985434, -12.65000000000000213 ) ) ;
#182121 = EDGE_LOOP ( 'NONE', ( #122476, #169845, #156550, #162673 ) ) ;
#182120 = AXIS2_PLACEMENT_3D ( 'NONE', #73591, #153140, #35745 ) ;
#182122 = EDGE_CURVE ( 'NONE', #96658, #115258, #58923, .T. ) ;
#182123 = FACE_OUTER_BOUND ( 'NONE', #145293, .T. ) ;
#182124 = CARTESIAN_POINT ( 'NONE',  ( -18.59999999999999787, 77.16412189325286874, -61.70825939895269840 ) ) ;
#182125 = AXIS2_PLACEMENT_3D ( 'NONE', #189125, #52165, #228262 ) ;
#182126 = CIRCLE ( 'NONE', #207263, 11.75000000000001066 ) ;
#182127 = DIRECTION ( 'NONE',  ( 1.000000000000000000, -0.000000000000000000, 0.000000000000000000 ) ) ;
#182128 = FACE_OUTER_BOUND ( 'NONE', #240700, .T. ) ;
#182129 = B_SPLINE_CURVE_WITH_KNOTS ( 'NONE', 3,
 ( #204160, #106333, #166373, #245876, #122084, #141634, #224997, #184611 ),
 .UNSPECIFIED., .F., .F.,
 ( 4, 2, 2, 4 ),
 ( 0.000000000000000000, 0.0002114466876442047964, 0.0003171700314663110300, 0.0004228933752884172907 ),
 .UNSPECIFIED. ) ;
#182130 = CARTESIAN_POINT ( 'NONE',  ( 20.85000000000000142, 1.115600667400684642E-11, -100.5000000000000426 ) ) ;
#182131 = VECTOR ( 'NONE', #162773, 1000.000000000000000 ) ;
#182132 = EDGE_LOOP ( 'NONE', ( #13355, #211143, #48739, #177798 ) ) ;
#182133 = ORIENTED_EDGE ( 'NONE', *, *, #244913, .T. ) ;
#182134 = DIRECTION ( 'NONE',  ( 2.715809747126117987E-16, 1.000000000000000000, 8.690591190803577558E-15 ) ) ;
#182135 = DIRECTION ( 'NONE',  ( 0.000000000000000000, 0.8814952561688437216, -0.4721928772777334582 ) ) ;
#182136 = ADVANCED_FACE ( 'NONE', ( #190147 ), #169330, .T. ) ;
#182137 = CARTESIAN_POINT ( 'NONE',  ( -20.64999999999999858, 66.36210077474692071, -222.8232602954134336 ) ) ;
#182138 = CARTESIAN_POINT ( 'NONE',  ( -20.65000000000000568, 7.250000000011138646, -143.2500000000000284 ) ) ;
#182139 = VERTEX_POINT ( 'NONE', #108034 ) ;
#182140 = LINE ( 'NONE', #67313, #101521 ) ;
#182141 = ADVANCED_FACE ( 'NONE', ( #31099 ), #128886, .F. ) ;
#182142 = ADVANCED_FACE ( 'NONE', ( #110589 ), #170628, .F. ) ;
#182143 = DIRECTION ( 'NONE',  ( -1.645090726704136556E-14, -0.1618390714546045217, 0.9868171638914230437 ) ) ;
#182144 = AXIS2_PLACEMENT_3D ( 'NONE', #240847, #73785, #232850 ) ;
#182145 = LINE ( 'NONE', #141715, #229627 ) ;
#182146 = CARTESIAN_POINT ( 'NONE',  ( 23.14999999999999858, 1.115600667400684642E-11, -100.5000000000000284 ) ) ;
#182147 = AXIS2_PLACEMENT_3D ( 'NONE', #50031, #129579, #209104 ) ;
#182148 = EDGE_CURVE ( 'NONE', #66925, #242911, #8929, .T. ) ;
#182149 = EDGE_CURVE ( 'NONE', #53335, #120408, #100612, .T. ) ;
#182150 = ORIENTED_EDGE ( 'NONE', *, *, #59423, .T. ) ;
#182151 = LINE ( 'NONE', #4756, #19410 ) ;
#182152 = VERTEX_POINT ( 'NONE', #230551 ) ;
#182153 = FACE_OUTER_BOUND ( 'NONE', #128253, .T. ) ;
#182154 = CARTESIAN_POINT ( 'NONE',  ( 21.05000000000000782, -0.01681986838567536488, 6.307425219565410579 ) ) ;
#182156 = EDGE_CURVE ( 'NONE', #239159, #134685, #147145, .T. ) ;
#182155 = CARTESIAN_POINT ( 'NONE',  ( -21.14999999999994174, 64.35000000001120668, -3.123107484524795474 ) ) ;
#182157 = CARTESIAN_POINT ( 'NONE',  ( 22.39999999999999503, 76.00000000001170974, -77.31388708289769340 ) ) ;
#182158 = FACE_OUTER_BOUND ( 'NONE', #210539, .T. ) ;
#182159 = CARTESIAN_POINT ( 'NONE',  ( -23.15000000000000213, 11.65000000001115588, -45.65000000000000568 ) ) ;
#182160 = DIRECTION ( 'NONE',  ( 0.000000000000000000, -0.9126074666063771490, -0.4088369013363276627 ) ) ;
#182161 = DIRECTION ( 'NONE',  ( 1.000000000000000000, 0.000000000000000000, 0.000000000000000000 ) ) ;
#182162 = CARTESIAN_POINT ( 'NONE',  ( 21.53699400384337181, -8.054621614985864327E-12, -93.71228820675614202 ) ) ;
#182163 = EDGE_CURVE ( 'NONE', #124908, #54825, #25829, .T. ) ;
#182164 = CARTESIAN_POINT ( 'NONE',  ( -23.25000000000000000, -1.164121893230052995, -175.4148480855716059 ) ) ;
#182165 = DIRECTION ( 'NONE',  ( 0.000000000000000000, -0.8700118002898357128, 0.4930308989875170633 ) ) ;
#182166 = DIRECTION ( 'NONE',  ( -0.000000000000000000, 6.982962677686266711E-15, -1.000000000000000000 ) ) ;
#182167 = VECTOR ( 'NONE', #152631, 1000.000000000000000 ) ;
#182168 = CIRCLE ( 'NONE', #69749, 11.65000000000000746 ) ;
#182169 = EDGE_CURVE ( 'NONE', #132345, #41773, #9075, .T. ) ;
#182170 = EDGE_CURVE ( 'NONE', #86585, #206520, #204871, .T. ) ;
#182171 = CARTESIAN_POINT ( 'NONE',  ( -21.14999999999999858, 36.65892442174472876, -249.5511627012454596 ) ) ;
#182172 = DIRECTION ( 'NONE',  ( -0.000000000000000000, -0.8700118002898321601, 0.4930308989875230030 ) ) ;
#182173 = EDGE_LOOP ( 'NONE', ( #191330, #229035, #219495, #67737, #33125 ) ) ;
#182174 = CARTESIAN_POINT ( 'NONE',  ( -20.94999999999999929, 6.977140961446278489, -233.9419795020459389 ) ) ;
#182176 = EDGE_CURVE ( 'NONE', #172898, #105425, #96536, .T. ) ;
#182175 = DIRECTION ( 'NONE',  ( 0.000000000000000000, -0.4088369013363280513, 0.9126074666063769270 ) ) ;
#182177 = ORIENTED_EDGE ( 'NONE', *, *, #239164, .T. ) ;
#182178 = CARTESIAN_POINT ( 'NONE',  ( -18.59999999999999787, 77.68707439010360360, -115.8376804510659497 ) ) ;
#182179 = CARTESIAN_POINT ( 'NONE',  ( 20.94999999999999929, 1.115600667400684642E-11, -134.0000000000000284 ) ) ;
#182180 = EDGE_CURVE ( 'NONE', #184724, #126269, #10226, .T. ) ;
#182181 = EDGE_CURVE ( 'NONE', #152824, #165380, #238195, .T. ) ;
#182182 = B_SPLINE_CURVE_WITH_KNOTS ( 'NONE', 3,
 ( #11184, #90704, #177969, #97089, #81382, #257428, #22761, #77539, #120572, #241773, #181808, #42300, #82668, #99670, #176690, #200092, #57983, #61867, #218340 ),
 .UNSPECIFIED., .F., .F.,
 ( 4, 3, 3, 3, 3, 3, 4 ),
 ( 1.387778780781445676E-17, 2.646747978908967593E-05, 5.271166642128211505E-05, 9.008788829882676842E-05, 0.0001426648776560830647, 0.0001897378458659620612, 0.0001917382627806005289 ),
 .UNSPECIFIED. ) ;
#182183 = CARTESIAN_POINT ( 'NONE',  ( -20.64999999999999858, 71.65000000001155911, -57.17310748452435121 ) ) ;
#182184 = ORIENTED_EDGE ( 'NONE', *, *, #193973, .T. ) ;
#182185 = VECTOR ( 'NONE', #147577, 1000.000000000000000 ) ;
#182186 = CARTESIAN_POINT ( 'NONE',  ( 23.15000000000000213, -11.39257802169451139, -164.4260504201680817 ) ) ;
#182187 = DIRECTION ( 'NONE',  ( 2.557131231893036985E-16, -0.9525900758537791946, 0.3042567129660269099 ) ) ;
#182188 = ADVANCED_FACE ( 'NONE', ( #16645 ), #118305, .F. ) ;
#182189 = VECTOR ( 'NONE', #237007, 1000.000000000000000 ) ;
#182190 = VERTEX_POINT ( 'NONE', #257745 ) ;
#182191 = CIRCLE ( 'NONE', #223852, 0.1000000000000052097 ) ;
#182192 = ORIENTED_EDGE ( 'NONE', *, *, #138001, .T. ) ;
#182193 = CARTESIAN_POINT ( 'NONE',  ( 20.94999999999999574, 74.16465844978819177, -191.9679561919613775 ) ) ;
#182194 = ORIENTED_EDGE ( 'NONE', *, *, #192322, .F. ) ;
#182195 = EDGE_CURVE ( 'NONE', #162811, #163992, #158737, .T. ) ;
#182196 = DIRECTION ( 'NONE',  ( 1.000000000000000000, 0.000000000000000000, 0.000000000000000000 ) ) ;
#182197 = CARTESIAN_POINT ( 'NONE',  ( -18.59999999999999787, 9.105964803472822666, -245.3658845043482586 ) ) ;
#182198 = CARTESIAN_POINT ( 'NONE',  ( -21.05000000000000071, 1.115600667400684642E-11, -67.00000000000000000 ) ) ;
#182199 = FACE_OUTER_BOUND ( 'NONE', #25764, .T. ) ;
#182200 = CARTESIAN_POINT ( 'NONE',  ( -16.97683809663752186, 66.05000000001230376, -156.6207434663279230 ) ) ;
#182201 = CARTESIAN_POINT ( 'NONE',  ( -20.94999999999999929, 87.48912529308822172, -139.4231074845242802 ) ) ;
#182202 = CYLINDRICAL_SURFACE ( 'NONE', #51138, 4.049999999999998046 ) ;
#182203 = CARTESIAN_POINT ( 'NONE',  ( -23.15000000000000213, 74.08971962618075224, -182.6544753397233194 ) ) ;
#182205 = EDGE_LOOP ( 'NONE', ( #129308, #200093, #106478, #88259 ) ) ;
#182204 = DIRECTION ( 'NONE',  ( 0.000000000000000000, -1.000000000000000000, 0.000000000000000000 ) ) ;
#182206 = EDGE_LOOP ( 'NONE', ( #150251, #185352, #187114, #207324 ) ) ;
#182208 = DIRECTION ( 'NONE',  ( 1.000000000000000000, 3.265361837132813093E-16, -0.000000000000000000 ) ) ;
#182207 = FACE_OUTER_BOUND ( 'NONE', #184802, .T. ) ;
#182210 = EDGE_LOOP ( 'NONE', ( #196259, #145589, #41359, #87969 ) ) ;
#182209 = CARTESIAN_POINT ( 'NONE',  ( -16.87683809663752754, 61.18214872564366402, -220.4678436623806022 ) ) ;
#182211 = AXIS2_PLACEMENT_3D ( 'NONE', #15939, #80994, #199708 ) ;
#182212 = VERTEX_POINT ( 'NONE', #17897 ) ;
#182213 = CARTESIAN_POINT ( 'NONE',  ( 23.14999999999999503, 64.35000000001249987, -176.9379132551783869 ) ) ;
#182215 = CARTESIAN_POINT ( 'NONE',  ( -23.25000000000000000, 1.115600667400684642E-11, -67.00000000000000000 ) ) ;
#182214 = CIRCLE ( 'NONE', #165656, 12.87500000000000000 ) ;
#182216 = CARTESIAN_POINT ( 'NONE',  ( 18.59999999999999076, 11.65000000001115943, -21.75000000000000355 ) ) ;
#182217 = DIRECTION ( 'NONE',  ( 0.000000000000000000, 0.000000000000000000, -1.000000000000000000 ) ) ;
#182219 = DIRECTION ( 'NONE',  ( 1.000000000000000000, 5.603460673774838784E-17, 1.046060675573451523E-16 ) ) ;
#182218 = AXIS2_PLACEMENT_3D ( 'NONE', #232519, #95544, #74747 ) ;
#182220 = DIRECTION ( 'NONE',  ( 0.000000000000000000, 1.000000000000000000, 0.000000000000000000 ) ) ;
#182221 = CARTESIAN_POINT ( 'NONE',  ( 22.39999999999999858, 68.20922040163929978, -203.6231074845244109 ) ) ;
#182223 = ORIENTED_EDGE ( 'NONE', *, *, #41412, .F. ) ;
#182222 = EDGE_CURVE ( 'NONE', #242995, #248066, #229828, .T. ) ;
#182224 = ORIENTED_EDGE ( 'NONE', *, *, #146740, .F. ) ;
#182225 = CARTESIAN_POINT ( 'NONE',  ( 16.87683809663750267, 60.93935776605891164, -221.0417277355860790 ) ) ;
#182226 = AXIS2_PLACEMENT_3D ( 'NONE', #92091, #256228, #157235 ) ;
#182227 = AXIS2_PLACEMENT_3D ( 'NONE', #46665, #205748, #104064 ) ;
#182228 = EDGE_CURVE ( 'NONE', #154602, #243191, #113128, .T. ) ;
#182229 = EDGE_LOOP ( 'NONE', ( #235415, #151572, #220687, #7612 ) ) ;
#182230 = CARTESIAN_POINT ( 'NONE',  ( 21.05000000000000071, -0.09999993529482767429, -27.02192177890524150 ) ) ;
#182231 = VERTEX_POINT ( 'NONE', #153625 ) ;
#182233 = DIRECTION ( 'NONE',  ( 1.000000000000000000, 0.000000000000000000, 0.000000000000000000 ) ) ;
#182232 = AXIS2_PLACEMENT_3D ( 'NONE', #199188, #102613, #201742 ) ;
#182234 = VECTOR ( 'NONE', #244214, 1000.000000000000000 ) ;
#182235 = CARTESIAN_POINT ( 'NONE',  ( -12.30589683808040391, 48.53345590596380532, -233.9787581418636364 ) ) ;
#182236 = CIRCLE ( 'NONE', #257007, 0.1000000000000028644 ) ;
#182237 = CARTESIAN_POINT ( 'NONE',  ( 18.52928932304157073, 65.72071067696991520, -44.84685405172078987 ) ) ;
#182238 = LINE ( 'NONE', #192196, #212256 ) ;
#182239 = ORIENTED_EDGE ( 'NONE', *, *, #247175, .F. ) ;
#182240 = APPLICATION_CONTEXT ( 'automotive_design' ) ;
#182241 = ORIENTED_EDGE ( 'NONE', *, *, #188461, .T. ) ;
#182242 = CARTESIAN_POINT ( 'NONE',  ( -23.25000000000000000, 71.65000000001155911, -57.37310748452435405 ) ) ;
#182243 = DIRECTION ( 'NONE',  ( 0.000000000000000000, -0.9651348961777155289, 0.2617529984165036794 ) ) ;
#182244 = CARTESIAN_POINT ( 'NONE',  ( -1.820710678118658388, 85.92928932189354896, -145.3731074845242972 ) ) ;
#182245 = EDGE_CURVE ( 'NONE', #121144, #21187, #246408, .T. ) ;
#182246 = ORIENTED_EDGE ( 'NONE', *, *, #166621, .T. ) ;
#182247 = CARTESIAN_POINT ( 'NONE',  ( 21.05000000000000071, 87.75000000001143974, -39.12310748452424747 ) ) ;
#182248 = VECTOR ( 'NONE', #96175, 1000.000000000000000 ) ;
#182249 = ORIENTED_EDGE ( 'NONE', *, *, #92443, .T. ) ;
#182252 = VERTEX_POINT ( 'NONE', #174474 ) ;
#182251 = CARTESIAN_POINT ( 'NONE',  ( 18.52351027002947959, -9.642162904684026259, -107.2150469505098300 ) ) ;
#182250 = DIRECTION ( 'NONE',  ( 0.000000000000000000, 0.5000683049008606273, 0.8659859643398268858 ) ) ;
#182253 = DIRECTION ( 'NONE',  ( -1.000000000000000000, -0.000000000000000000, -0.000000000000000000 ) ) ;
#182254 = VECTOR ( 'NONE', #64572, 1000.000000000000000 ) ;
#182255 = ORIENTED_EDGE ( 'NONE', *, *, #118951, .F. ) ;
#182256 = AXIS2_PLACEMENT_3D ( 'NONE', #14302, #130356, #149956 ) ;
#182257 = CARTESIAN_POINT ( 'NONE',  ( 18.59999999999999787, 16.53615870702968138, -240.8540256063542984 ) ) ;
#182258 = VERTEX_POINT ( 'NONE', #238231 ) ;
#182260 = AXIS2_PLACEMENT_3D ( 'NONE', #117817, #241621, #20029 ) ;
#182259 = DIRECTION ( 'NONE',  ( 0.000000000000000000, 0.9126074666063781482, 0.4088369013363256643 ) ) ;
#182261 = CIRCLE ( 'NONE', #107228, 0.09999999999998898659 ) ;
#182262 = CARTESIAN_POINT ( 'NONE',  ( 20.94999999999999929, 70.15000000001221281, -146.6556047088023149 ) ) ;
#182263 = TOROIDAL_SURFACE ( 'NONE', #19777, 0.6000000000000015321, 0.1000000000000000056 ) ;
#182264 = CARTESIAN_POINT ( 'NONE',  ( -20.94999999999999929, 1.115600667400684642E-11, -130.0000000000000284 ) ) ;
#182265 = CARTESIAN_POINT ( 'NONE',  ( -20.65000000000000568, 70.35000000001190301, -93.77310748452434552 ) ) ;
#182266 = PLANE ( 'NONE',  #143569 ) ;
#182267 = B_SPLINE_CURVE_WITH_KNOTS ( 'NONE', 3,
 ( #36083, #16523, #217249, #175595, #255044, #236823, #23915, #235540, #56878, #77740 ),
 .UNSPECIFIED., .F., .F.,
 ( 4, 2, 2, 2, 4 ),
 ( 0.000000000000000000, 0.0001584437871625799649, 0.0002376656807438381125, 0.0002772766275344300930, 0.0003168875743250220735 ),
 .UNSPECIFIED. ) ;
#182268 = ORIENTED_EDGE ( 'NONE', *, *, #254731, .F. ) ;
#182269 = LINE ( 'NONE', #222646, #44208 ) ;
#182270 = CARTESIAN_POINT ( 'NONE',  ( -20.85000000000000142, 65.66751761918690988, -130.9282609406112670 ) ) ;
#182271 = CARTESIAN_POINT ( 'NONE',  ( -18.43634282235125710, -9.679787199916876972, -140.6606518854538592 ) ) ;
#182272 = AXIS2_PLACEMENT_3D ( 'NONE', #101490, #162816, #227567 ) ;
#182273 = EDGE_LOOP ( 'NONE', ( #202336, #74280, #183869, #250991 ) ) ;
#182274 = DIRECTION ( 'NONE',  ( -1.000000000000000000, -0.000000000000000000, -0.000000000000000000 ) ) ;
#182276 = ORIENTED_EDGE ( 'NONE', *, *, #248339, .F. ) ;
#182275 = CIRCLE ( 'NONE', #69861, 0.09999999999999739653 ) ;
#182278 = AXIS2_PLACEMENT_3D ( 'NONE', #13718, #210638, #150669 ) ;
#182277 = DIRECTION ( 'NONE',  ( 0.000000000000000000, -7.487053152578134969E-15, 1.000000000000000000 ) ) ;
#182279 = FACE_OUTER_BOUND ( 'NONE', #111563, .T. ) ;
#182280 = DIRECTION ( 'NONE',  ( 1.000000000000000000, 0.000000000000000000, 0.000000000000000000 ) ) ;
#182281 = B_SPLINE_CURVE_WITH_KNOTS ( 'NONE', 3,
 ( #41402, #21824, #98742, #928, #140467, #160069, #137892, #120949, #80461, #222559 ),
 .UNSPECIFIED., .F., .F.,
 ( 4, 3, 3, 4 ),
 ( 7.632826238681696029E-06, 4.756916949875625587E-05, 9.484459048152062838E-05, 0.0001435500935100044199 ),
 .UNSPECIFIED. ) ;
#182283 = ORIENTED_EDGE ( 'NONE', *, *, #40866, .T. ) ;
#182282 = FACE_OUTER_BOUND ( 'NONE', #178877, .T. ) ;
#182284 = EDGE_CURVE ( 'NONE', #126005, #170174, #104888, .T. ) ;
#182285 = FACE_OUTER_BOUND ( 'NONE', #72847, .T. ) ;
#182286 = AXIS2_PLACEMENT_3D ( 'NONE', #32638, #172150, #116000 ) ;
#182287 = CARTESIAN_POINT ( 'NONE',  ( -21.05000000000000071, 1.750000000011155743, -145.6695115579016715 ) ) ;
#182288 = EDGE_CURVE ( 'NONE', #166875, #51521, #115730, .T. ) ;
#182289 = AXIS2_PLACEMENT_3D ( 'NONE', #40964, #72711, #131367 ) ;
#182290 = ORIENTED_EDGE ( 'NONE', *, *, #206634, .T. ) ;
#182291 = FACE_OUTER_BOUND ( 'NONE', #131920, .T. ) ;
#182292 = CYLINDRICAL_SURFACE ( 'NONE', #31773, 0.09999999999999939493 ) ;
#182293 = AXIS2_PLACEMENT_3D ( 'NONE', #217047, #57975, #60551 ) ;
#182294 = VERTEX_POINT ( 'NONE', #132744 ) ;
#182295 = EDGE_LOOP ( 'NONE', ( #101337, #235589, #58771, #195777 ) ) ;
#182296 = CIRCLE ( 'NONE', #165553, 0.09999999999999939493 ) ;
#182297 = ADVANCED_FACE ( 'NONE', ( #177018 ), #212280, .F. ) ;
#182298 = DIRECTION ( 'NONE',  ( 1.000000000000000000, 0.000000000000000000, 0.000000000000000000 ) ) ;
#182299 = ORIENTED_EDGE ( 'NONE', *, *, #123749, .T. ) ;
#182301 = ORIENTED_EDGE ( 'NONE', *, *, #96319, .F. ) ;
#182300 = DIRECTION ( 'NONE',  ( 0.000000000000000000, 0.8700118002898356018, -0.4930308989875170078 ) ) ;
#182302 = EDGE_CURVE ( 'NONE', #32767, #71370, #109007, .T. ) ;
#182303 = AXIS2_PLACEMENT_3D ( 'NONE', #188693, #88282, #53029 ) ;
#182304 = EDGE_CURVE ( 'NONE', #48144, #8827, #125767, .T. ) ;
#182307 = ORIENTED_EDGE ( 'NONE', *, *, #205814, .T. ) ;
#182306 = ORIENTED_EDGE ( 'NONE', *, *, #96204, .T. ) ;
#182305 = DIRECTION ( 'NONE',  ( 1.000000000000000000, 0.000000000000000000, 0.000000000000000000 ) ) ;
#182308 = DIRECTION ( 'NONE',  ( -0.000000000000000000, 1.000000000000000000, 6.982962677686266711E-15 ) ) ;
#182309 = CIRCLE ( 'NONE', #153117, 0.1000000000000013933 ) ;
#182310 = CARTESIAN_POINT ( 'NONE',  ( -20.54999999999999716, 73.60000000001259934, -190.2984855617622770 ) ) ;
#182311 = AXIS2_PLACEMENT_3D ( 'NONE', #236576, #99616, #218287 ) ;
#182312 = CARTESIAN_POINT ( 'NONE',  ( 18.52928932188133970, 65.72071067813016043, -48.17310748452439384 ) ) ;
#182313 = EDGE_CURVE ( 'NONE', #172639, #82065, #154848, .T. ) ;
#182314 = AXIS2_PLACEMENT_3D ( 'NONE', #16408, #197580, #1937 ) ;
#182316 = CARTESIAN_POINT ( 'NONE',  ( -21.05000000000000071, 74.16465844978715438, -57.86795619196135476 ) ) ;
#182315 = CARTESIAN_POINT ( 'NONE',  ( 20.93975676684922504, 46.39397692848788068, -243.0687461883537424 ) ) ;
#182317 = CARTESIAN_POINT ( 'NONE',  ( 21.14999999999999503, 64.25000000001215028, -136.5231074845243597 ) ) ;
#182318 = CIRCLE ( 'NONE', #244830, 11.79999999999999893 ) ;
#182319 = LINE ( 'NONE', #218842, #247099 ) ;
#182321 = DIRECTION ( 'NONE',  ( 0.000000000000000000, 0.4088369013363281068, -0.9126074666063770380 ) ) ;
#182320 = CARTESIAN_POINT ( 'NONE',  ( -15.55912972643741199, 8.490870273573719373, -46.04999999999999716 ) ) ;
#182322 = ORIENTED_EDGE ( 'NONE', *, *, #211342, .F. ) ;
#182323 = VERTEX_POINT ( 'NONE', #114446 ) ;
#182324 = CARTESIAN_POINT ( 'NONE',  ( 15.74999999999999645, 62.10905854918434699, -217.1108499610991203 ) ) ;
#182326 = ORIENTED_EDGE ( 'NONE', *, *, #148057, .T. ) ;
#182325 = DIRECTION ( 'NONE',  ( 0.000000000000000000, 0.2558827019434435912, -0.9667078373770033872 ) ) ;
#182327 = VERTEX_POINT ( 'NONE', #135271 ) ;
#182328 = EDGE_CURVE ( 'NONE', #173723, #114955, #214818, .T. ) ;
#182329 = CARTESIAN_POINT ( 'NONE',  ( -21.53752568617671059, 6.786807874503945293, 0.09897446126636783026 ) ) ;
#182330 = ORIENTED_EDGE ( 'NONE', *, *, #129349, .F. ) ;
#182331 = CARTESIAN_POINT ( 'NONE',  ( -5.900000000000002132, -11.65000000000000036, 13.90000000000000213 ) ) ;
#182332 = AXIS2_PLACEMENT_3D ( 'NONE', #240539, #202687, #43626 ) ;
#182333 = ORIENTED_EDGE ( 'NONE', *, *, #165090, .F. ) ;
#182334 = DIRECTION ( 'NONE',  ( 0.000000000000000000, -0.000000000000000000, 1.000000000000000000 ) ) ;
#182335 = FACE_OUTER_BOUND ( 'NONE', #122525, .T. ) ;
#182336 = TOROIDAL_SURFACE ( 'NONE', #40718, 11.65000000000000036, 0.1000000000000000056 ) ;
#182338 = ORIENTED_EDGE ( 'NONE', *, *, #32495, .T. ) ;
#182337 = ORIENTED_EDGE ( 'NONE', *, *, #35548, .F. ) ;
#182339 = VERTEX_POINT ( 'NONE', #36214 ) ;
#182340 = CARTESIAN_POINT ( 'NONE',  ( -20.94999999999999929, 87.29603075034764004, -166.9752083248604038 ) ) ;
#182341 = VERTEX_POINT ( 'NONE', #236958 ) ;
#182342 = ORIENTED_EDGE ( 'NONE', *, *, #149288, .T. ) ;
#182343 = CARTESIAN_POINT ( 'NONE',  ( 21.05000000000000071, 84.73084112150752389, -146.1211822035086527 ) ) ;
#182345 = ORIENTED_EDGE ( 'NONE', *, *, #159185, .F. ) ;
#182344 = CARTESIAN_POINT ( 'NONE',  ( 18.59999996954842771, -9.523204137847672612, -107.3830417119164906 ) ) ;
#182347 = CARTESIAN_POINT ( 'NONE',  ( -16.89268316805466341, 60.93619025550653134, -221.0468289635910537 ) ) ;
#182346 = CARTESIAN_POINT ( 'NONE',  ( 21.00000000000000000, 66.25000000001151079, -48.27310748452438816 ) ) ;
#182348 = CARTESIAN_POINT ( 'NONE',  ( 20.99999999999999645, 9.750000000011137757, -87.85000000000003695 ) ) ;
#182349 = CARTESIAN_POINT ( 'NONE',  ( -18.40000000000000213, 8.822561741677553471, -109.7500000000000426 ) ) ;
#182350 = DIRECTION ( 'NONE',  ( 0.000000000000000000, 1.000000000000000000, 6.982962677686266711E-15 ) ) ;
#182351 = VERTEX_POINT ( 'NONE', #38765 ) ;
#182352 = ORIENTED_EDGE ( 'NONE', *, *, #19173, .F. ) ;
#182353 = CARTESIAN_POINT ( 'NONE',  ( -16.87786941232800686, 66.04184528586726799, -149.1459216847304390 ) ) ;
#182354 = DIRECTION ( 'NONE',  ( 1.000000000000000000, 0.000000000000000000, 0.000000000000000000 ) ) ;
#182355 = VERTEX_POINT ( 'NONE', #19194 ) ;
#182356 = AXIS2_PLACEMENT_3D ( 'NONE', #4739, #25621, #165128 ) ;
#182357 = AXIS2_PLACEMENT_3D ( 'NONE', #124693, #243338, #145519 ) ;
#182358 = CARTESIAN_POINT ( 'NONE',  ( 21.40925344232283223, 0.09895018863080314031, -26.84148114060954526 ) ) ;
#182359 = AXIS2_PLACEMENT_3D ( 'NONE', #24331, #3447, #146801 ) ;
#182360 = EDGE_CURVE ( 'NONE', #148974, #57410, #14077, .T. ) ;
#182361 = CARTESIAN_POINT ( 'NONE',  ( -13.39999999999994529, 67.75000000001118394, -21.02310748452479316 ) ) ;
#182362 = CARTESIAN_POINT ( 'NONE',  ( 21.04999999999999716, 18.80863553818519307, -227.8685860884963290 ) ) ;
#182363 = ORIENTED_EDGE ( 'NONE', *, *, #25419, .T. ) ;
#182364 = ORIENTED_EDGE ( 'NONE', *, *, #162538, .T. ) ;
#182365 = CARTESIAN_POINT ( 'NONE',  ( -20.94999999999999929, 17.12338108143915250, -224.6426509580150537 ) ) ;
#182366 = CARTESIAN_POINT ( 'NONE',  ( -23.15000000000000213, 87.65000000001144542, -39.12310748452424747 ) ) ;
#182367 = ORIENTED_EDGE ( 'NONE', *, *, #14856, .T. ) ;
#182368 = DIRECTION ( 'NONE',  ( -1.000000000000000000, 2.952720810173289112E-16, 2.061873921506763405E-30 ) ) ;
#182369 = ORIENTED_EDGE ( 'NONE', *, *, #36878, .T. ) ;
#182370 = DIRECTION ( 'NONE',  ( 1.000000000000000000, 7.304098846218135653E-16, 0.000000000000000000 ) ) ;
#182372 = ADVANCED_FACE ( 'NONE', ( #233141 ), #54463, .T. ) ;
#182371 = DIRECTION ( 'NONE',  ( 0.000000000000000000, 2.891205793294679805E-16, -1.000000000000000000 ) ) ;
#182373 = CARTESIAN_POINT ( 'NONE',  ( -21.05000000000000071, 1.115600667400684642E-11, -134.0000000000000000 ) ) ;
#182374 = DIRECTION ( 'NONE',  ( 0.000000000000000000, -1.000000000000000000, -6.982962677686266711E-15 ) ) ;
#182375 = EDGE_CURVE ( 'NONE', #202321, #18724, #119601, .T. ) ;
#182376 = VECTOR ( 'NONE', #212398, 1000.000000000000114 ) ;
#182377 = EDGE_CURVE ( 'NONE', #206683, #116233, #82978, .T. ) ;
#182378 = ORIENTED_EDGE ( 'NONE', *, *, #56608, .T. ) ;
#182379 = CIRCLE ( 'NONE', #174031, 0.1000000000000050293 ) ;
#182380 = CARTESIAN_POINT ( 'NONE',  ( -20.94999999999999929, -11.64999999998884483, -69.90000000000004832 ) ) ;
#182382 = ORIENTED_EDGE ( 'NONE', *, *, #103792, .T. ) ;
#182381 = ORIENTED_EDGE ( 'NONE', *, *, #65959, .T. ) ;
#182383 = CIRCLE ( 'NONE', #103239, 0.1999999999999985401 ) ;
#182384 = VERTEX_POINT ( 'NONE', #243366 ) ;
#182385 = ORIENTED_EDGE ( 'NONE', *, *, #19451, .F. ) ;
#182386 = DIRECTION ( 'NONE',  ( -3.265361837132814079E-16, 0.4721928772777359007, 0.8814952561688425003 ) ) ;
#182387 = CARTESIAN_POINT ( 'NONE',  ( -22.59999999999999787, 55.96169194136206215, -232.9023299069559130 ) ) ;
#182388 = LINE ( 'NONE', #205781, #150729 ) ;
#182389 = CARTESIAN_POINT ( 'NONE',  ( -18.59999999999999787, 1.162701749938009677, -8.099999999999999645 ) ) ;
#182390 = DIRECTION ( 'NONE',  ( 0.000000000000000000, -0.9770955615653321713, -0.2128009952263575366 ) ) ;
#182391 = EDGE_CURVE ( 'NONE', #158643, #74054, #25619, .T. ) ;
#182392 = CARTESIAN_POINT ( 'NONE',  ( 21.05000000000000071, 58.97943978561187350, -225.6753515332448217 ) ) ;
#182394 = ORIENTED_EDGE ( 'NONE', *, *, #177185, .T. ) ;
#182393 = DIRECTION ( 'NONE',  ( -0.000000000000000000, 0.1298341882519668811, 0.9915357197604899309 ) ) ;
#182395 = CARTESIAN_POINT ( 'NONE',  ( -21.07954640115348610, 6.329287696035510891, -167.4339922928603528 ) ) ;
#182396 = ORIENTED_EDGE ( 'NONE', *, *, #109769, .T. ) ;
#182397 = ADVANCED_FACE ( 'NONE', ( #80407 ), #222500, .T. ) ;
#182398 = DIRECTION ( 'NONE',  ( -1.836970198721029934E-16, -1.000000000000000000, -6.982962677686266711E-15 ) ) ;
#182399 = VERTEX_POINT ( 'NONE', #161293 ) ;
#182400 = ORIENTED_EDGE ( 'NONE', *, *, #188301, .T. ) ;
#182401 = CARTESIAN_POINT ( 'NONE',  ( -20.64999999999999858, 7.150000000000000355, -12.25000000000000000 ) ) ;
#182402 = CARTESIAN_POINT ( 'NONE',  ( 21.05000000000000071, 6.257814610476124528, 0.09779029130879343668 ) ) ;
#182403 = DIRECTION ( 'NONE',  ( 0.000000000000000000, 0.000000000000000000, -1.000000000000000000 ) ) ;
#182404 = PRODUCT_DEFINITION ( 'UNKNOWN', '', #177954, #178363 ) ;
#182405 = CIRCLE ( 'NONE', #20076, 0.09999999999999971412 ) ;
#182406 = AXIS2_PLACEMENT_3D ( 'NONE', #39598, #119105, #181651 ) ;
#182407 = VECTOR ( 'NONE', #58319, 1000.000000000000000 ) ;
#182408 = DIRECTION ( 'NONE',  ( 0.000000000000000000, -1.000000000000000000, 0.000000000000000000 ) ) ;
#182409 = VERTEX_POINT ( 'NONE', #160014 ) ;
#182410 = ORIENTED_EDGE ( 'NONE', *, *, #128756, .F. ) ;
#182411 = ADVANCED_FACE ( 'NONE', ( #182128 ), #240815, .F. ) ;
#182412 = FACE_OUTER_BOUND ( 'NONE', #147975, .T. ) ;
#182414 = ORIENTED_EDGE ( 'NONE', *, *, #180695, .F. ) ;
#182413 = ADVANCED_FACE ( 'NONE', ( #163844 ), #21555, .T. ) ;
#182415 = SPHERICAL_SURFACE ( 'NONE', #31405, 0.1000000000000000056 ) ;
#182416 = CARTESIAN_POINT ( 'NONE',  ( -16.92925196614875460, 9.972331796421277872, -46.11674484771679516 ) ) ;
#182417 = ADVANCED_FACE ( 'NONE', ( #880 ), #84240, .F. ) ;
#182419 = DIRECTION ( 'NONE',  ( -1.000000000000000000, 1.387778780781454006E-13, 0.000000000000000000 ) ) ;
#182418 = CIRCLE ( 'NONE', #132312, 11.65000000000000036 ) ;
#182420 = CARTESIAN_POINT ( 'NONE',  ( 20.12500000000000000, 66.25000000001253397, -182.2731074845244450 ) ) ;
#182421 = CARTESIAN_POINT ( 'NONE',  ( -20.64999999999999858, 76.00000000001213607, -136.5231074845243313 ) ) ;
#182422 = CARTESIAN_POINT ( 'NONE',  ( 22.47071067811865319, 0.09909245471376171288, -59.27992525550200043 ) ) ;
#182423 = DIRECTION ( 'NONE',  ( 0.000000000000000000, -0.008583690987162452199, -0.9999631594459053030 ) ) ;
#182424 = DIRECTION ( 'NONE',  ( 1.000000000000000000, 0.000000000000000000, 0.000000000000000000 ) ) ;
#182425 = DIRECTION ( 'NONE',  ( 0.000000000000000000, 0.1568667991644863147, 0.9876197685951252359 ) ) ;
#182426 = CARTESIAN_POINT ( 'NONE',  ( 18.49999999999997868, 65.62657994473291012, -178.7573193598993555 ) ) ;
#182427 = CARTESIAN_POINT ( 'NONE',  ( -22.59999985501179154, 11.74986979301414003, -133.9344013302004726 ) ) ;
#182428 = CIRCLE ( 'NONE', #16021, 1.899999999999999023 ) ;
#182429 = FACE_OUTER_BOUND ( 'NONE', #126792, .T. ) ;
#182430 = VECTOR ( 'NONE', #240419, 1000.000000000000000 ) ;
#182431 = CIRCLE ( 'NONE', #232318, 0.09999999999999986677 ) ;
#182432 = VERTEX_POINT ( 'NONE', #23071 ) ;
#182433 = AXIS2_PLACEMENT_3D ( 'NONE', #167095, #181502, #204882 ) ;
#182434 = CARTESIAN_POINT ( 'NONE',  ( -16.88853107394619357, 30.20933174956215694, -234.8076571479847985 ) ) ;
#182435 = EDGE_LOOP ( 'NONE', ( #32919, #4755, #94672, #5460 ) ) ;
#182436 = CARTESIAN_POINT ( 'NONE',  ( 20.73486653747088937, 68.25000000001227818, -157.3731074845244109 ) ) ;
#182437 = DIRECTION ( 'NONE',  ( 0.000000000000000000, 0.000000000000000000, -1.000000000000000000 ) ) ;
#182438 = CARTESIAN_POINT ( 'NONE',  ( 21.00000000000000000, 9.750000000011153745, -155.2500000000000284 ) ) ;
#182439 = ORIENTED_EDGE ( 'NONE', *, *, #171239, .T. ) ;
#182440 = EDGE_CURVE ( 'NONE', #50587, #230108, #239532, .T. ) ;
#182441 = DIRECTION ( 'NONE',  ( 1.000000000000000000, 0.000000000000000000, 0.000000000000000000 ) ) ;
#182442 = CARTESIAN_POINT ( 'NONE',  ( -22.47071067811865319, 75.90090754530910999, -77.24318222902238062 ) ) ;
#182443 = CARTESIAN_POINT ( 'NONE',  ( -18.40000000000000213, 11.75000000001113953, -46.15000000000000568 ) ) ;
#182444 = CARTESIAN_POINT ( 'NONE',  ( 22.47071067811865319, 1.148907358139439339E-11, -201.0000000000015064 ) ) ;
#182445 = CIRCLE ( 'NONE', #211465, 7.900000000000003908 ) ;
#182446 = SPHERICAL_SURFACE ( 'NONE', #197256, 0.1000000000000000056 ) ;
#182447 = PLANE ( 'NONE',  #132090 ) ;
#182448 = AXIS2_PLACEMENT_3D ( 'NONE', #70114, #229169, #49232 ) ;
#182449 = VECTOR ( 'NONE', #122671, 1000.000000000000000 ) ;
#182450 = ORIENTED_EDGE ( 'NONE', *, *, #145357, .T. ) ;
#182451 = CARTESIAN_POINT ( 'NONE',  ( 22.16821283564876666, 68.44102665923138318, -136.5231074845243313 ) ) ;
#182454 = VERTEX_POINT ( 'NONE', #184674 ) ;
#182453 = DIRECTION ( 'NONE',  ( 0.000000000000000000, 0.8814952561688476074, -0.4721928772777262417 ) ) ;
#182452 = AXIS2_PLACEMENT_3D ( 'NONE', #229396, #126426, #108157 ) ;
#182455 = DIRECTION ( 'NONE',  ( -1.000000000000000000, -1.394253735153569469E-16, -2.602809386958778209E-16 ) ) ;
#182456 = ADVANCED_FACE ( 'NONE', ( #6030 ), #124718, .F. ) ;
#182457 = FACE_OUTER_BOUND ( 'NONE', #71692, .T. ) ;
#182458 = AXIS2_PLACEMENT_3D ( 'NONE', #81515, #78952, #101057 ) ;
#182459 = DIRECTION ( 'NONE',  ( 0.000000000000000000, 0.000000000000000000, -1.000000000000000000 ) ) ;
#182460 = VERTEX_POINT ( 'NONE', #141698 ) ;
#182461 = DIRECTION ( 'NONE',  ( 0.000000000000000000, 0.000000000000000000, 1.000000000000000000 ) ) ;
#182462 = ADVANCED_FACE ( 'NONE', ( #140411 ), #178872, .F. ) ;
#182463 = CONTEXT_DEPENDENT_SHAPE_REPRESENTATION ( #210775, #124738 ) ;
#182464 = FACE_OUTER_BOUND ( 'NONE', #59825, .T. ) ;
#182465 = VERTEX_POINT ( 'NONE', #102541 ) ;
#182467 = ADVANCED_FACE ( 'NONE', ( #101241 ), #233927, .T. ) ;
#182466 = CARTESIAN_POINT ( 'NONE',  ( 11.60000000000000142, -11.75000000000000000, 12.30000000000000426 ) ) ;
#182468 = FACE_OUTER_BOUND ( 'NONE', #104027, .T. ) ;
#182469 = VECTOR ( 'NONE', #107920, 1000.000000000000000 ) ;
#182470 = AXIS2_PLACEMENT_3D ( 'NONE', #137208, #158108, #120260 ) ;
#182471 = EDGE_CURVE ( 'NONE', #30937, #248593, #88138, .T. ) ;
#182472 = EDGE_CURVE ( 'NONE', #27072, #134711, #68598, .T. ) ;
#182473 = DIRECTION ( 'NONE',  ( 0.000000000000000000, -6.982962677686266711E-15, 1.000000000000000000 ) ) ;
#182474 = ORIENTED_EDGE ( 'NONE', *, *, #38418, .F. ) ;
#182475 = ORIENTED_EDGE ( 'NONE', *, *, #23809, .T. ) ;
#182476 = CARTESIAN_POINT ( 'NONE',  ( 20.85000000000000142, -1.164121893230052995, -141.9148480855716343 ) ) ;
#182477 = DIRECTION ( 'NONE',  ( 0.000000000000000000, 0.8660254037844352659, -0.5000000000000058842 ) ) ;
#182478 = CARTESIAN_POINT ( 'NONE',  ( -20.94999999999999929, 38.25685495413521409, -235.9601135138701693 ) ) ;
#182479 = CARTESIAN_POINT ( 'NONE',  ( -18.40000000000000213, 64.52683809664910086, -56.97310748452440521 ) ) ;
#182480 = LINE ( 'NONE', #161641, #205590 ) ;
#182481 = VECTOR ( 'NONE', #167964, 1000.000000000000000 ) ;
#182483 = CARTESIAN_POINT ( 'NONE',  ( -23.25000000000000000, 70.76519756549812712, -215.1840646563997836 ) ) ;
#182482 = CARTESIAN_POINT ( 'NONE',  ( 20.95052659398289308, 65.52017563223198238, -95.44786872865877569 ) ) ;
#182484 = LINE ( 'NONE', #110296, #27765 ) ;
#182485 = AXIS2_PLACEMENT_3D ( 'NONE', #13142, #110946, #108385 ) ;
#182486 = DIRECTION ( 'NONE',  ( 0.000000000000000000, -1.000000000000000000, -6.982962677686265922E-15 ) ) ;
#182487 = DIRECTION ( 'NONE',  ( 0.000000000000000000, 0.9651348961777157509, -0.2617529984165031243 ) ) ;
#182488 = DIRECTION ( 'NONE',  ( -0.000000000000000000, -0.4721928772777346239, -0.8814952561688430555 ) ) ;
#182489 = ORIENTED_EDGE ( 'NONE', *, *, #16035, .T. ) ;
#182490 = EDGE_CURVE ( 'NONE', #110926, #82512, #660, .T. ) ;
#182491 = VERTEX_POINT ( 'NONE', #46445 ) ;
#182492 = CARTESIAN_POINT ( 'NONE',  ( -23.25000000000000000, 6.982009704867601307, -137.6961521182563217 ) ) ;
#182493 = EDGE_CURVE ( 'NONE', #47603, #172479, #127043, .T. ) ;
#182494 = CARTESIAN_POINT ( 'NONE',  ( 23.40000000000005187, 76.00000000001119815, -36.02310748452479316 ) ) ;
#182496 = CARTESIAN_POINT ( 'NONE',  ( 21.09706851349341861, 67.22415748653919820, -191.2875412681247838 ) ) ;
#182495 = DIRECTION ( 'NONE',  ( 1.000000000000000000, -7.125593699324843413E-30, 1.020425574104004196E-15 ) ) ;
#182497 = VECTOR ( 'NONE', #182688, 1000.000000000000000 ) ;
#182498 = DIRECTION ( 'NONE',  ( 0.000000000000000000, -0.1495327102803586661, -0.9887567792719350601 ) ) ;
#182500 = EDGE_CURVE ( 'NONE', #178818, #97821, #54849, .T. ) ;
#182499 = DIRECTION ( 'NONE',  ( 1.000000000000000000, 0.000000000000000000, 0.000000000000000000 ) ) ;
#182501 = DIRECTION ( 'NONE',  ( 2.952720810173288126E-16, -0.4721928772777345684, -0.8814952561688429444 ) ) ;
#182502 = ORIENTED_EDGE ( 'NONE', *, *, #227856, .T. ) ;
#182503 = CIRCLE ( 'NONE', #228282, 0.5000000000000004441 ) ;
#182504 = CARTESIAN_POINT ( 'NONE',  ( -23.25000000000000000, 2.000000000011154189, -54.37537807723790451 ) ) ;
#182505 = ORIENTED_EDGE ( 'NONE', *, *, #162166, .T. ) ;
#182506 = VECTOR ( 'NONE', #50258, 1000.000000000000000 ) ;
#182507 = VECTOR ( 'NONE', #40701, 1000.000000000000000 ) ;
#182508 = EDGE_CURVE ( 'NONE', #172354, #57307, #188725, .T. ) ;
#182509 = FACE_OUTER_BOUND ( 'NONE', #170876, .T. ) ;
#182510 = AXIS2_PLACEMENT_3D ( 'NONE', #162340, #31833, #9666 ) ;
#182511 = ORIENTED_EDGE ( 'NONE', *, *, #109785, .F. ) ;
#182512 = CARTESIAN_POINT ( 'NONE',  ( 18.69999999999999929, -1.467286812112899463, 32.89999999999999858 ) ) ;
#182513 = EDGE_CURVE ( 'NONE', #229956, #246051, #205518, .T. ) ;
#182514 = TOROIDAL_SURFACE ( 'NONE', #215787, 0.4000000000000009104, 0.1000000000000000056 ) ;
#182515 = CARTESIAN_POINT ( 'NONE',  ( 18.49362639424906263, 85.44260436789944890, -29.25866655101286185 ) ) ;
#182516 = EDGE_CURVE ( 'NONE', #173891, #151159, #63216, .T. ) ;
#182517 = ORIENTED_EDGE ( 'NONE', *, *, #57423, .F. ) ;
#182518 = DIRECTION ( 'NONE',  ( 0.000000000000000000, -0.9915357197604892647, 0.1298341882519715440 ) ) ;
#182519 = ORIENTED_EDGE ( 'NONE', *, *, #243537, .T. ) ;
#182520 = CARTESIAN_POINT ( 'NONE',  ( 18.49999999999999645, 79.11538813396778380, -196.3722783875038544 ) ) ;
#182521 = EDGE_CURVE ( 'NONE', #162878, #79207, #202994, .T. ) ;
#182522 = CARTESIAN_POINT ( 'NONE',  ( -21.53752568617669994, 69.21319212550778843, -69.62208194579494602 ) ) ;
#182524 = CARTESIAN_POINT ( 'NONE',  ( 21.72449340488910607, 10.28395627750227703, -76.25000000000004263 ) ) ;
#182523 = AXIS2_PLACEMENT_3D ( 'NONE', #204614, #88502, #145925 ) ;
#182525 = CARTESIAN_POINT ( 'NONE',  ( -21.04999999999994387, 67.85000000001119247, -3.123107484524795474 ) ) ;
#182527 = CARTESIAN_POINT ( 'NONE',  ( -20.94999999999999929, 44.18518595211054389, -258.7688298343402380 ) ) ;
#182526 = DIRECTION ( 'NONE',  ( -3.265361837132813093E-16, 1.000000000000000000, 0.000000000000000000 ) ) ;
#182528 = DIRECTION ( 'NONE',  ( -0.8049926720990042694, -0.5932847527679310229, 0.000000000000000000 ) ) ;
#182530 = VERTEX_POINT ( 'NONE', #12490 ) ;
#182529 = CARTESIAN_POINT ( 'NONE',  ( 21.14999999999999858, 65.28660755661270798, -191.2731074845244166 ) ) ;
#182532 = CARTESIAN_POINT ( 'NONE',  ( 18.59999999999999787, 77.83534155023646406, -124.8679561919613121 ) ) ;
#182531 = CARTESIAN_POINT ( 'NONE',  ( -16.88328101497759448, 9.950352834230013599, -188.3511795149292425 ) ) ;
#182533 = ORIENTED_EDGE ( 'NONE', *, *, #62307, .T. ) ;
#182535 = EDGE_LOOP ( 'NONE', ( #152068, #211211, #86229, #54173 ) ) ;
#182534 = CARTESIAN_POINT ( 'NONE',  ( -21.05000000000000071, 77.16270174995010223, -128.5231074845242745 ) ) ;
#182536 = ORIENTED_EDGE ( 'NONE', *, *, #78547, .T. ) ;
#182537 = CARTESIAN_POINT ( 'NONE',  ( 18.39999999999999858, 85.51932773110404185, -62.55013110796492271 ) ) ;
#182538 = DIRECTION ( 'NONE',  ( 0.000000000000000000, 0.000000000000000000, -1.000000000000000000 ) ) ;
#182539 = DIRECTION ( 'NONE',  ( 0.000000000000000000, -6.467318590049456648E-15, 1.000000000000000000 ) ) ;
#182540 = ORIENTED_EDGE ( 'NONE', *, *, #161059, .F. ) ;
#182541 = FACE_OUTER_BOUND ( 'NONE', #38553, .T. ) ;
#182542 = CARTESIAN_POINT ( 'NONE',  ( 13.99999999999999822, 9.850000000011137402, -117.2500000000000284 ) ) ;
#182543 = PLANE ( 'NONE',  #231415 ) ;
#182544 = DIRECTION ( 'NONE',  ( 0.000000000000000000, 0.9167729611565434977, -0.3994087351226345284 ) ) ;
#182545 = DIRECTION ( 'NONE',  ( -1.000000000000000000, 2.952720810173289112E-16, 2.061873921506763405E-30 ) ) ;
#182546 = DIRECTION ( 'NONE',  ( -1.000000000000000000, 0.000000000000000000, 0.000000000000000000 ) ) ;
#182547 = TOROIDAL_SURFACE ( 'NONE', #70127, 4.041421356237312246, 0.1000000000000000056 ) ;
#182548 = ORIENTED_EDGE ( 'NONE', *, *, #146375, .F. ) ;
#182549 = VERTEX_POINT ( 'NONE', #91996 ) ;
#182550 = AXIS2_PLACEMENT_3D ( 'NONE', #127148, #28077, #150569 ) ;
#182551 = DIRECTION ( 'NONE',  ( 0.000000000000000000, 0.4721928772776973204, 0.8814952561688629284 ) ) ;
#182552 = CIRCLE ( 'NONE', #219944, 0.1000000000000033362 ) ;
#182553 = EDGE_CURVE ( 'NONE', #136295, #87098, #242290, .T. ) ;
#182554 = ORIENTED_EDGE ( 'NONE', *, *, #229381, .F. ) ;
#182555 = DIRECTION ( 'NONE',  ( 1.000000000000000000, -2.952720810173289112E-16, -2.061873921506763405E-30 ) ) ;
#182556 = ORIENTED_EDGE ( 'NONE', *, *, #129460, .F. ) ;
#182557 = CARTESIAN_POINT ( 'NONE',  ( -20.64999999999999858, 85.00000000001188027, -93.12913836187181005 ) ) ;
#182558 = DIRECTION ( 'NONE',  ( -2.252264143451593919E-15, 0.08413937888703756918, -0.9964539953858901900 ) ) ;
#182559 = CARTESIAN_POINT ( 'NONE',  ( -22.39999999999999503, 68.20922040163854660, -103.0231074845243597 ) ) ;
#182560 = CARTESIAN_POINT ( 'NONE',  ( -21.08376601933334271, 30.84514200246639604, -252.0857823083072446 ) ) ;
#182561 = CARTESIAN_POINT ( 'NONE',  ( 21.06089410995830491, 10.72529553213474429, -179.7023807310431494 ) ) ;
#182562 = ORIENTED_EDGE ( 'NONE', *, *, #201271, .T. ) ;
#182563 = CARTESIAN_POINT ( 'NONE',  ( 18.49999999999999645, 77.36242903720516040, -95.13422623660308375 ) ) ;
#182564 = AXIS2_PLACEMENT_3D ( 'NONE', #75971, #135921, #34304 ) ;
#182566 = AXIS2_PLACEMENT_3D ( 'NONE', #79534, #100375, #219051 ) ;
#182565 = CARTESIAN_POINT ( 'NONE',  ( -16.86379686415369150, 66.02478224075939295, -182.5897175954341662 ) ) ;
#182567 = FACE_OUTER_BOUND ( 'NONE', #241159, .T. ) ;
#182569 = EDGE_CURVE ( 'NONE', #100977, #164049, #42029, .T. ) ;
#182568 = CARTESIAN_POINT ( 'NONE',  ( 20.94999999999999574, 8.926614585098251453, -75.47168301922316402 ) ) ;
#182570 = ORIENTED_EDGE ( 'NONE', *, *, #242937, .T. ) ;
#182572 = DIRECTION ( 'NONE',  ( -1.000000000000000000, -2.952720810173289112E-16, 0.000000000000000000 ) ) ;
#182571 = CARTESIAN_POINT ( 'NONE',  ( -20.94999999999999929, 77.83534155023627932, -91.46795619196130644 ) ) ;
#182573 = ORIENTED_EDGE ( 'NONE', *, *, #246052, .F. ) ;
#182576 = ORIENTED_EDGE ( 'NONE', *, *, #190660, .F. ) ;
#182575 = DIRECTION ( 'NONE',  ( 0.000000000000000000, -1.000000000000000000, -6.982962677686265922E-15 ) ) ;
#182574 = DIRECTION ( 'NONE',  ( -1.000000000000000000, 0.000000000000000000, 0.000000000000000000 ) ) ;
#182577 = ORIENTED_EDGE ( 'NONE', *, *, #64847, .T. ) ;
#182578 = AXIS2_PLACEMENT_3D ( 'NONE', #143191, #6244, #165341 ) ;
#182579 = CYLINDRICAL_SURFACE ( 'NONE', #14455, 0.09999999999999939493 ) ;
#182580 = CARTESIAN_POINT ( 'NONE',  ( -20.94999999999999929, 67.23127455305835554, -235.8551265064784559 ) ) ;
#182581 = FACE_OUTER_BOUND ( 'NONE', #145431, .T. ) ;
#182582 = ORIENTED_EDGE ( 'NONE', *, *, #131058, .T. ) ;
#182583 = DIRECTION ( 'NONE',  ( 0.000000000000000000, -6.982962677686266711E-15, 1.000000000000000000 ) ) ;
#182584 = LINE ( 'NONE', #84704, #82080 ) ;
#182586 = FACE_OUTER_BOUND ( 'NONE', #102297, .T. ) ;
#182585 = CARTESIAN_POINT ( 'NONE',  ( 18.59999999999999076, 53.42432843990430058, -234.7536552047824330 ) ) ;
#182588 = ORIENTED_EDGE ( 'NONE', *, *, #177464, .T. ) ;
#182587 = DIRECTION ( 'NONE',  ( 1.000000000000000000, 0.000000000000000000, 0.000000000000000000 ) ) ;
#182589 = ORIENTED_EDGE ( 'NONE', *, *, #171082, .T. ) ;
#182590 = CIRCLE ( 'NONE', #241018, 0.1999999999999996503 ) ;
#182591 = CARTESIAN_POINT ( 'NONE',  ( 19.94784844284961167, 64.28691006698288390, -78.32090876722591588 ) ) ;
#182592 = CARTESIAN_POINT ( 'NONE',  ( 21.05000000000000071, 76.10000000001214460, -136.5231074845242745 ) ) ;
#182593 = AXIS2_PLACEMENT_3D ( 'NONE', #37999, #138326, #117509 ) ;
#182594 = AXIS2_PLACEMENT_3D ( 'NONE', #6381, #242416, #125063 ) ;
#182595 = CYLINDRICAL_SURFACE ( 'NONE', #5059, 11.75000000000001066 ) ;
#182596 = VERTEX_POINT ( 'NONE', #9891 ) ;
#182597 = FACE_OUTER_BOUND ( 'NONE', #29208, .T. ) ;
#182598 = ORIENTED_EDGE ( 'NONE', *, *, #38334, .T. ) ;
#182599 = CARTESIAN_POINT ( 'NONE',  ( 20.94999999999999929, 11.65000000001115943, -60.21613433702191287 ) ) ;
#182600 = PLANE ( 'NONE',  #157694 ) ;
#182601 = AXIS2_PLACEMENT_3D ( 'NONE', #147513, #8017, #48401 ) ;
#182602 = ORIENTED_EDGE ( 'NONE', *, *, #124374, .T. ) ;
#182603 = CARTESIAN_POINT ( 'NONE',  ( 18.39999999999999503, 64.52683809665005299, -182.6731074845244507 ) ) ;
#182604 = ADVANCED_FACE ( 'NONE', ( #26925 ), #171062, .F. ) ;
#182605 = AXIS2_PLACEMENT_3D ( 'NONE', #114266, #174295, #37315 ) ;
#182606 = AXIS2_PLACEMENT_3D ( 'NONE', #225951, #30376, #8238 ) ;
#182607 = CARTESIAN_POINT ( 'NONE',  ( 23.24999999999999289, 5.950000000011163692, -157.1942976949652007 ) ) ;
#182608 = AXIS2_PLACEMENT_3D ( 'NONE', #112626, #190907, #150478 ) ;
#182609 = ORIENTED_EDGE ( 'NONE', *, *, #146143, .F. ) ;
#182610 = VERTEX_POINT ( 'NONE', #7330 ) ;
#182611 = CIRCLE ( 'NONE', #174457, 0.1000000000000028644 ) ;
#182612 = ORIENTED_EDGE ( 'NONE', *, *, #64746, .F. ) ;
#182613 = EDGE_CURVE ( 'NONE', #159456, #77841, #83661, .T. ) ;
#182614 = DIRECTION ( 'NONE',  ( -0.000000000000000000, 1.000000000000000000, -0.000000000000000000 ) ) ;
#182615 = VERTEX_POINT ( 'NONE', #166441 ) ;
#182617 = VERTEX_POINT ( 'NONE', #88119 ) ;
#182616 = LINE ( 'NONE', #120092, #26232 ) ;
#182618 = EDGE_CURVE ( 'NONE', #155020, #53624, #247216, .T. ) ;
#182619 = ORIENTED_EDGE ( 'NONE', *, *, #139267, .T. ) ;
#182622 = VERTEX_POINT ( 'NONE', #174159 ) ;
#182621 = VERTEX_POINT ( 'NONE', #29501 ) ;
#182620 = CARTESIAN_POINT ( 'NONE',  ( 18.43565242384933711, 78.24390740893980478, -231.6169762517608888 ) ) ;
#182625 = ADVANCED_FACE ( 'NONE', ( #194980 ), #237650, .T. ) ;
#182624 = ORIENTED_EDGE ( 'NONE', *, *, #170001, .F. ) ;
#182623 = AXIS2_PLACEMENT_3D ( 'NONE', #1274, #185060, #204613 ) ;
#182626 = DIRECTION ( 'NONE',  ( 0.000000000000000000, -0.8636236514130390951, 0.5041370733441546959 ) ) ;
#182627 = DIRECTION ( 'NONE',  ( -1.000000000000000000, 0.000000000000000000, 0.000000000000000000 ) ) ;
#182628 = AXIS2_PLACEMENT_3D ( 'NONE', #151594, #31650, #111156 ) ;
#182629 = CYLINDRICAL_SURFACE ( 'NONE', #196863, 0.09999999999999939493 ) ;
#182630 = AXIS2_PLACEMENT_3D ( 'NONE', #5383, #87501, #126648 ) ;
#182631 = AXIS2_PLACEMENT_3D ( 'NONE', #67854, #7909, #168293 ) ;
#182632 = EDGE_LOOP ( 'NONE', ( #92472, #203289, #115075 ) ) ;
#182633 = AXIS2_PLACEMENT_3D ( 'NONE', #209498, #251175, #72580 ) ;
#182634 = DIRECTION ( 'NONE',  ( 0.000000000000000000, 0.000000000000000000, -1.000000000000000000 ) ) ;
#182635 =( BOUNDED_SURFACE ( )  B_SPLINE_SURFACE ( 3, 2, ( 
 ( #245362, #240234, #66718 ),
 ( #161989, #84954, #146234 ),
 ( #144946, #225764, #224495 ),
 ( #160716, #163261, #103245 ),
 ( #61581, #201085, #42034 ),
 ( #164543, #141128, #241502 ) ),
 .UNSPECIFIED., .F., .F., .F. ) 
 B_SPLINE_SURFACE_WITH_KNOTS ( ( 4, 2, 4 ),
 ( 3, 3 ),
 ( -1.776356839400250465E-15, 0.7853981633974468357, 1.570796326794895448 ),
 ( 0.000000000000000000, 1.000000000000000000 ),
 .UNSPECIFIED. ) 
 GEOMETRIC_REPRESENTATION_ITEM ( )  RATIONAL_B_SPLINE_SURFACE ( (
 ( 1.000000000000000000, 0.5000000000000260902, 1.000000000000000000),
 ( 1.000000000000000000, 0.4993418825329626332, 1.000000000000000000),
 ( 1.000000000000000000, 0.5278258667064184007, 1.000000000000000000),
 ( 1.000000000000000000, 0.6092287576689454642, 1.000000000000000000),
 ( 1.000000000000000000, 0.6611148371783867050, 1.000000000000000000),
 ( 1.000000000000000000, 0.7071067811865597852, 1.000000000000000000) ) ) 
 REPRESENTATION_ITEM ( '' )  SURFACE ( )  );
#182636 = ORIENTED_EDGE ( 'NONE', *, *, #103815, .F. ) ;
#182637 = CARTESIAN_POINT ( 'NONE',  ( -20.64999999999999858, 2.000000000011154189, -80.22462192276213955 ) ) ;
#182639 = ORIENTED_EDGE ( 'NONE', *, *, #154555, .T. ) ;
#182638 = LINE ( 'NONE', #86049, #164740 ) ;
#182640 = AXIS2_PLACEMENT_3D ( 'NONE', #167587, #111440, #189696 ) ;
#182641 = EDGE_CURVE ( 'NONE', #72979, #5184, #166947, .T. ) ;
#182642 = ORIENTED_EDGE ( 'NONE', *, *, #207983, .T. ) ;
#182643 = ORIENTED_EDGE ( 'NONE', *, *, #201297, .T. ) ;
#182644 = ORIENTED_EDGE ( 'NONE', *, *, #238339, .F. ) ;
#182645 = CARTESIAN_POINT ( 'NONE',  ( -21.55000000000000071, 68.85000000001180354, -81.77310748452435973 ) ) ;
#182646 = DIRECTION ( 'NONE',  ( -6.938893903907222856E-15, 0.9770955615653316162, 0.2128009952263604232 ) ) ;
#182647 = PRESENTATION_LAYER_ASSIGNMENT (  '', '', ( #253361 ) ) ;
#182648 = AXIS2_PLACEMENT_3D ( 'NONE', #78507, #95514, #75960 ) ;
#182650 = ORIENTED_EDGE ( 'NONE', *, *, #143636, .T. ) ;
#182649 = EDGE_LOOP ( 'NONE', ( #193186, #155573, #85548, #67484, #199966, #122952, #124867, #182855, #125471, #97196, #92061, #100490, #66983, #36147 ) ) ;
#182651 = ORIENTED_EDGE ( 'NONE', *, *, #131821, .T. ) ;
#182652 = DIRECTION ( 'NONE',  ( 1.000000000000000000, 0.000000000000000000, 0.000000000000000000 ) ) ;
#182653 = ORIENTED_EDGE ( 'NONE', *, *, #174242, .T. ) ;
#182654 = ORIENTED_EDGE ( 'NONE', *, *, #3102, .T. ) ;
#182655 = CARTESIAN_POINT ( 'NONE',  ( -16.97683809663752186, 9.850000000011140955, -113.1500000000000341 ) ) ;
#182657 = ORIENTED_EDGE ( 'NONE', *, *, #62876, .T. ) ;
#182656 = CARTESIAN_POINT ( 'NONE',  ( -21.55000000000000426, 7.708578643773852157, -188.7499999999999716 ) ) ;
#182658 = DIRECTION ( 'NONE',  ( 0.000000000000000000, 0.1332476588733589318, -0.9910827722268050755 ) ) ;
#182660 = CARTESIAN_POINT ( 'NONE',  ( 18.40000000000000213, -9.519327731081279609, -107.4729763765593731 ) ) ;
#182659 = CARTESIAN_POINT ( 'NONE',  ( -16.93658623642890859, 22.95883090495301104, -230.8902928517333919 ) ) ;
#182661 = EDGE_CURVE ( 'NONE', #230787, #250736, #38449, .T. ) ;
#182662 = EDGE_LOOP ( 'NONE', ( #238274, #92056, #150056, #9298 ) ) ;
#182663 = CIRCLE ( 'NONE', #91062, 0.09999999999998898659 ) ;
#182664 = VECTOR ( 'NONE', #70360, 1000.000000000000000 ) ;
#182666 = VERTEX_POINT ( 'NONE', #236639 ) ;
#182665 = VERTEX_POINT ( 'NONE', #217063 ) ;
#182667 = CARTESIAN_POINT ( 'NONE',  ( 20.94999999999999929, 74.16465844978787914, -158.4679561919613775 ) ) ;
#182668 = SURFACE_SIDE_STYLE ('',( #223051 ) ) ;
#182669 = AXIS2_PLACEMENT_3D ( 'NONE', #30147, #11873, #109647 ) ;
#182670 = EDGE_LOOP ( 'NONE', ( #158338, #98274, #64491, #182028 ) ) ;
#182671 = TOROIDAL_SURFACE ( 'NONE', #140975, 0.2000000000000000111, 0.1000000000000000056 ) ;
#182672 = EDGE_CURVE ( 'NONE', #159251, #55121, #112853, .T. ) ;
#182673 = DIRECTION ( 'NONE',  ( 0.000000000000000000, 0.000000000000000000, -1.000000000000000000 ) ) ;
#182674 = ORIENTED_EDGE ( 'NONE', *, *, #126415, .F. ) ;
#182675 = ORIENTED_EDGE ( 'NONE', *, *, #199048, .F. ) ;
#182676 = DIRECTION ( 'NONE',  ( 1.000000000000000000, 0.000000000000000000, 0.000000000000000000 ) ) ;
#182677 = ORIENTED_EDGE ( 'NONE', *, *, #163463, .T. ) ;
#182678 = FACE_OUTER_BOUND ( 'NONE', #156340, .T. ) ;
#182679 = DIRECTION ( 'NONE',  ( 0.000000000000000000, -0.4721928772776973204, -0.8814952561688629284 ) ) ;
#182680 = VERTEX_POINT ( 'NONE', #73752 ) ;
#182681 = CIRCLE ( 'NONE', #169670, 0.2000000000000057288 ) ;
#182682 = FACE_OUTER_BOUND ( 'NONE', #183772, .T. ) ;
#182684 = EDGE_CURVE ( 'NONE', #4251, #185125, #214508, .T. ) ;
#182683 = CARTESIAN_POINT ( 'NONE',  ( 18.59999999999999432, 85.48068669529105534, -129.5819923157664562 ) ) ;
#182686 = CARTESIAN_POINT ( 'NONE',  ( -16.89155683852579060, 9.950000000011137047, -120.7226281504603378 ) ) ;
#182685 = DIRECTION ( 'NONE',  ( 0.000000000000000000, 0.000000000000000000, -1.000000000000000000 ) ) ;
#182687 = DIRECTION ( 'NONE',  ( 0.000000000000000000, 0.000000000000000000, 1.000000000000000000 ) ) ;
#182688 = DIRECTION ( 'NONE',  ( -1.000000000000000000, -0.000000000000000000, -0.000000000000000000 ) ) ;
#182689 = VECTOR ( 'NONE', #76901, 1000.000000000000000 ) ;
#182690 = DIRECTION ( 'NONE',  ( 0.000000000000000000, 0.000000000000000000, 1.000000000000000000 ) ) ;
#182691 = CARTESIAN_POINT ( 'NONE',  ( 23.15000000000000213, -11.74999999999999112, -12.15000000000000036 ) ) ;
#182693 = DIRECTION ( 'NONE',  ( 1.000000000000000000, -0.000000000000000000, -0.000000000000000000 ) ) ;
#182692 = VECTOR ( 'NONE', #57316, 1000.000000000000000 ) ;
#182694 = EDGE_CURVE ( 'NONE', #56926, #21183, #172875, .T. ) ;
#182695 = ORIENTED_EDGE ( 'NONE', *, *, #17564, .F. ) ;
#182697 = ORIENTED_EDGE ( 'NONE', *, *, #120871, .T. ) ;
#182696 = ORIENTED_EDGE ( 'NONE', *, *, #28142, .F. ) ;
#182698 = EDGE_LOOP ( 'NONE', ( #111989, #171855, #189181 ) ) ;
#182699 = DIRECTION ( 'NONE',  ( 0.000000000000000000, 0.4721928772777351790, 0.8814952561688427224 ) ) ;
#182700 = EDGE_CURVE ( 'NONE', #110943, #159030, #115410, .T. ) ;
#182701 = LINE ( 'NONE', #165712, #82731 ) ;
#182702 =( BOUNDED_CURVE ( )  B_SPLINE_CURVE ( 3, ( #103156, #26225, #125317, #185287 ),
 .UNSPECIFIED., .F., .F. ) 
 B_SPLINE_CURVE_WITH_KNOTS ( ( 4, 4 ),
 ( 4.712388980384689674, 6.231880751915386263 ),
 .UNSPECIFIED. ) 
 CURVE ( )  GEOMETRIC_REPRESENTATION_ITEM ( )  RATIONAL_B_SPLINE_CURVE ( ( 1.000000000000000000, 0.8166740347213228279, 0.8166740347213228279, 1.000000000000000000 ) ) 
 REPRESENTATION_ITEM ( '' )  );
#182704 = CARTESIAN_POINT ( 'NONE',  ( -12.93407622233967658, 9.417789466952205757, -15.35738454397687214 ) ) ;
#182703 = CARTESIAN_POINT ( 'NONE',  ( -21.05000000000000071, 1.115600667400684642E-11, -200.9999999999999432 ) ) ;
#182705 = CARTESIAN_POINT ( 'NONE',  ( -21.14250536705909411, 76.00000000001219291, -143.0412796614050706 ) ) ;
#182706 = ORIENTED_EDGE ( 'NONE', *, *, #179540, .T. ) ;
#182707 = AXIS2_PLACEMENT_3D ( 'NONE', #144311, #67376, #205581 ) ;
#182708 = ADVANCED_FACE ( 'NONE', ( #231529 ), #33358, .F. ) ;
#182709 = CARTESIAN_POINT ( 'NONE',  ( -20.94788355080264353, 10.30207779525983014, -105.9895520716782897 ) ) ;
#182710 = EDGE_CURVE ( 'NONE', #12190, #100578, #125221, .T. ) ;
#182711 = DIRECTION ( 'NONE',  ( -1.020425574104004196E-15, 6.982962677686266711E-15, -1.000000000000000000 ) ) ;
#182712 = DIRECTION ( 'NONE',  ( 1.000000000000000000, -0.000000000000000000, -0.000000000000000000 ) ) ;
#182713 = CARTESIAN_POINT ( 'NONE',  ( -16.90128866880176517, 9.953795777214113016, -87.86267618338868601 ) ) ;
#182714 = ORIENTED_EDGE ( 'NONE', *, *, #15413, .F. ) ;
#182715 = DIRECTION ( 'NONE',  ( 0.000000000000000000, 0.8660254037844378194, 0.5000000000000016653 ) ) ;
#182716 = ADVANCED_FACE ( 'NONE', ( #154580 ), #134948, .T. ) ;
#182717 = DIRECTION ( 'NONE',  ( -3.890533409366484652E-14, 0.1298341882520054891, 0.9915357197604850459 ) ) ;
#182718 = VERTEX_POINT ( 'NONE', #232824 ) ;
#182719 = CARTESIAN_POINT ( 'NONE',  ( -21.76363531954647357, 0.9937110212123942965, -230.3339729431867511 ) ) ;
#182720 = DIRECTION ( 'NONE',  ( 0.000000000000000000, 0.000000000000000000, 1.000000000000000000 ) ) ;
#182721 = EDGE_CURVE ( 'NONE', #49571, #183971, #4397, .T. ) ;
#182722 = CARTESIAN_POINT ( 'NONE',  ( 21.05000000000000071, -11.64999999999999147, -2.900000000000003464 ) ) ;
#182723 = CARTESIAN_POINT ( 'NONE',  ( 23.24999999999999289, 69.45000000001252261, -182.1731074845243938 ) ) ;
#182724 = EDGE_CURVE ( 'NONE', #16861, #241304, #213219, .T. ) ;
#182725 = CARTESIAN_POINT ( 'NONE',  ( 23.25000000000000000, -8.596261682242991142, -9.450127517150276546 ) ) ;
#182726 = ORIENTED_EDGE ( 'NONE', *, *, #121609, .T. ) ;
#182727 = LINE ( 'NONE', #62763, #244408 ) ;
#182728 = DIRECTION ( 'NONE',  ( 0.000000000000000000, 1.000000000000000000, 0.000000000000000000 ) ) ;
#182729 = CARTESIAN_POINT ( 'NONE',  ( 20.94999999999999929, 11.84624361595474795, -206.1763227999733203 ) ) ;
#182730 = CARTESIAN_POINT ( 'NONE',  ( 18.49999999999999645, 70.47363787294415260, -228.3418745167492432 ) ) ;
#182731 = CARTESIAN_POINT ( 'NONE',  ( -16.89268316805466341, 12.41449167011727361, -211.2369018264743090 ) ) ;
#182732 = DIRECTION ( 'NONE',  ( -0.000000000000000000, 6.982962677686266711E-15, -1.000000000000000000 ) ) ;
#182733 = CIRCLE ( 'NONE', #70314, 0.1000000000000028644 ) ;
#182734 = TOROIDAL_SURFACE ( 'NONE', #132647, 0.2000000000000000111, 0.1000000000000000056 ) ;
#182735 = CARTESIAN_POINT ( 'NONE',  ( -23.15000000000000213, 76.00000000001190870, -103.0231074845243029 ) ) ;
#182736 = LINE ( 'NONE', #163171, #110896 ) ;
#182737 = VECTOR ( 'NONE', #254567, 1000.000000000000000 ) ;
#182739 = EDGE_LOOP ( 'NONE', ( #225293, #128367, #173704, #120971 ) ) ;
#182738 = PLANE ( 'NONE',  #27892 ) ;
#182740 =( BOUNDED_CURVE ( )  B_SPLINE_CURVE ( 3, ( #151381, #253017, #230918, #190512 ),
 .UNSPECIFIED., .F., .F. ) 
 B_SPLINE_CURVE_WITH_KNOTS ( ( 4, 4 ),
 ( 1.570796326794895448, 3.141592653589791784 ),
 .UNSPECIFIED. ) 
 CURVE ( )  GEOMETRIC_REPRESENTATION_ITEM ( )  RATIONAL_B_SPLINE_CURVE ( ( 1.000000000000000000, 0.8047378541243650485, 0.8047378541243650485, 1.000000000000000000 ) ) 
 REPRESENTATION_ITEM ( '' )  );
#182741 = VERTEX_POINT ( 'NONE', #55406 ) ;
#182742 = AXIS2_PLACEMENT_3D ( 'NONE', #227603, #48968, #196187 ) ;
#182743 = ADVANCED_FACE ( 'NONE', ( #95831 ), #175423, .F. ) ;
#182744 = EDGE_CURVE ( 'NONE', #129055, #206460, #208621, .T. ) ;
#182745 = AXIS2_PLACEMENT_3D ( 'NONE', #120424, #62976, #199943 ) ;
#182746 = EDGE_CURVE ( 'NONE', #153892, #145261, #158550, .T. ) ;
#182748 = VECTOR ( 'NONE', #217451, 1000.000000000000000 ) ;
#182747 = CARTESIAN_POINT ( 'NONE',  ( -18.51024323315077424, 65.68895814178191017, -30.50265578621381124 ) ) ;
#182749 = CARTESIAN_POINT ( 'NONE',  ( 15.52844286134407881, 9.375669526436929857, -149.8677900093859705 ) ) ;
#182750 = ORIENTED_EDGE ( 'NONE', *, *, #255314, .T. ) ;
#182751 = CIRCLE ( 'NONE', #195235, 0.1000000000000002554 ) ;
#182752 = CARTESIAN_POINT ( 'NONE',  ( 18.59999999999999076, 43.08613539620618837, -254.3146655184800409 ) ) ;
#182753 = CARTESIAN_POINT ( 'NONE',  ( -21.14999999999999858, 64.25000000001215028, -136.4231074845243938 ) ) ;
#182754 = CARTESIAN_POINT ( 'NONE',  ( -20.94999999999999574, 11.62071067811865177, -26.63158334765902424 ) ) ;
#182755 = ORIENTED_EDGE ( 'NONE', *, *, #180068, .T. ) ;
#182756 = DIRECTION ( 'NONE',  ( -1.000000000000000000, -0.000000000000000000, -0.000000000000000000 ) ) ;
#182758 = ORIENTED_EDGE ( 'NONE', *, *, #36050, .F. ) ;
#182757 = CARTESIAN_POINT ( 'NONE',  ( -23.25000000000000000, 11.75000000001115552, -45.65000000000000568 ) ) ;
#182760 = CARTESIAN_POINT ( 'NONE',  ( 21.13614978966381841, -3.602007608198911206E-16, 6.499104701833793740 ) ) ;
#182759 = DIRECTION ( 'NONE',  ( 0.000000000000000000, 0.9126074666063771490, 0.4088369013363276627 ) ) ;
#182761 = CARTESIAN_POINT ( 'NONE',  ( 20.94999999999999929, 68.03191114188443578, -213.8010436651919122 ) ) ;
#182762 = EDGE_LOOP ( 'NONE', ( #34038, #167652, #71076, #201886 ) ) ;
#182763 = EDGE_CURVE ( 'NONE', #233645, #52039, #157136, .T. ) ;
#182764 = DIRECTION ( 'NONE',  ( 0.000000000000000000, 0.000000000000000000, 1.000000000000000000 ) ) ;
#182765 = DIRECTION ( 'NONE',  ( 0.000000000000000000, 0.7106264324241465813, -0.7035695228903323661 ) ) ;
#182766 = EDGE_LOOP ( 'NONE', ( #226877, #13052, #7477, #63856, #88991, #113682 ) ) ;
#182768 = EDGE_CURVE ( 'NONE', #60900, #214033, #581, .T. ) ;
#182767 = CARTESIAN_POINT ( 'NONE',  ( -21.44999999999999929, 21.48591740176965814, -233.0852932139783036 ) ) ;
#182769 = VECTOR ( 'NONE', #128763, 1000.000000000000000 ) ;
#182770 = AXIS2_PLACEMENT_3D ( 'NONE', #21200, #100665, #180249 ) ;
#182771 = CARTESIAN_POINT ( 'NONE',  ( 23.25000000000000000, 12.29073439453116201, -249.8274140313476437 ) ) ;
#182772 = CARTESIAN_POINT ( 'NONE',  ( 21.00000000000000000, 9.750000000011153745, -54.75000000000000000 ) ) ;
#182773 = EDGE_CURVE ( 'NONE', #160725, #235880, #78837, .T. ) ;
#182774 = CARTESIAN_POINT ( 'NONE',  ( -5.900000000000002132, -11.34999999999999964, 14.00000000000000178 ) ) ;
#182775 = ORIENTED_EDGE ( 'NONE', *, *, #243850, .F. ) ;
#182776 = CIRCLE ( 'NONE', #186874, 12.77500000000000924 ) ;
#182777 = ORIENTED_EDGE ( 'NONE', *, *, #230660, .T. ) ;
#182778 = EDGE_CURVE ( 'NONE', #257895, #201510, #220918, .T. ) ;
#182779 = CARTESIAN_POINT ( 'NONE',  ( 21.11344571971299544, 65.38212097649356735, -124.2770865921250447 ) ) ;
#182780 = B_SPLINE_CURVE_WITH_KNOTS ( 'NONE', 3,
 ( #248549, #30818, #234118, #69941, #134997, #214554, #129876, #119323, #256186, #121902, #138838, #176739, #220970 ),
 .UNSPECIFIED., .F., .F.,
 ( 4, 3, 3, 3, 4 ),
 ( 1.084999851846394431E-16, 1.946463881814305957E-05, 3.922356109944007726E-05, 4.215060953238855979E-05, 4.415117091092329025E-05 ),
 .UNSPECIFIED. ) ;
#182781 = DIRECTION ( 'NONE',  ( 0.000000000000000000, 0.8814952561688430555, -0.4721928772777344574 ) ) ;
#182782 = CARTESIAN_POINT ( 'NONE',  ( -20.94999999999999929, 16.53615870702968138, -240.8540256063542984 ) ) ;
#182783 = SPHERICAL_SURFACE ( 'NONE', #203567, 0.1000000000000000056 ) ;
#182784 = LINE ( 'NONE', #21157, #20299 ) ;
#182785 = EDGE_CURVE ( 'NONE', #206438, #80321, #33687, .T. ) ;
#182787 = DIRECTION ( 'NONE',  ( 0.000000000000000000, 0.000000000000000000, -1.000000000000000000 ) ) ;
#182786 = CARTESIAN_POINT ( 'NONE',  ( -20.54999999999999716, 76.00000000001243450, -168.0231074845243597 ) ) ;
#182788 = AXIS2_PLACEMENT_3D ( 'NONE', #140221, #101062, #103660 ) ;
#182790 = CARTESIAN_POINT ( 'NONE',  ( -21.14999999999999858, -11.74999999998884448, -136.9000000000000341 ) ) ;
#182789 = VECTOR ( 'NONE', #196822, 1000.000000000000000 ) ;
#182791 = DIRECTION ( 'NONE',  ( 0.000000000000000000, -1.000000000000000000, 0.000000000000000000 ) ) ;
#182792 = CARTESIAN_POINT ( 'NONE',  ( 23.24999999999999645, 5.599999999999996980, 11.75000000000000000 ) ) ;
#182793 = VECTOR ( 'NONE', #144685, 1000.000000000000000 ) ;
#182794 = ORIENTED_EDGE ( 'NONE', *, *, #131123, .T. ) ;
#182795 = CARTESIAN_POINT ( 'NONE',  ( 23.14999999999999503, 64.25000000001276135, -215.2731074845244450 ) ) ;
#182796 = ADVANCED_FACE ( 'NONE', ( #63130 ), #239216, .T. ) ;
#182798 = ORIENTED_EDGE ( 'NONE', *, *, #29158, .F. ) ;
#182797 = DIRECTION ( 'NONE',  ( 1.186688945009009831E-16, 1.000000000000000000, 6.982962677686266711E-15 ) ) ;
#182799 = DIRECTION ( 'NONE',  ( 0.000000000000000000, -6.853228547068871147E-15, 1.000000000000000000 ) ) ;
#182802 = EDGE_CURVE ( 'NONE', #45647, #255801, #154467, .T. ) ;
#182801 = EDGE_CURVE ( 'NONE', #203994, #70783, #44875, .T. ) ;
#182800 = AXIS2_PLACEMENT_3D ( 'NONE', #84596, #202032, #123780 ) ;
#182803 = DIRECTION ( 'NONE',  ( 0.000000000000000000, 4.163336342344217877E-13, -1.000000000000000000 ) ) ;
#182805 = FACE_OUTER_BOUND ( 'NONE', #201525, .T. ) ;
#182804 = DIRECTION ( 'NONE',  ( -1.000000000000000000, 9.012599976028471648E-15, 6.882867235861662930E-14 ) ) ;
#182806 = ORIENTED_EDGE ( 'NONE', *, *, #2605, .F. ) ;
#182808 = CARTESIAN_POINT ( 'NONE',  ( -23.25000000000000000, 2.000000000011154189, -121.3753780772379258 ) ) ;
#182807 = CARTESIAN_POINT ( 'NONE',  ( -16.87401514999235275, 66.05000000001157900, -56.80312547705646153 ) ) ;
#182810 = EDGE_CURVE ( 'NONE', #87157, #257284, #98372, .T. ) ;
#182809 = DIRECTION ( 'NONE',  ( -1.000000000000000000, -0.000000000000000000, -0.000000000000000000 ) ) ;
#182811 = CARTESIAN_POINT ( 'NONE',  ( -21.05000000000000071, 66.97496366775517629, -235.8217698210967512 ) ) ;
#182812 = DIRECTION ( 'NONE',  ( 0.000000000000000000, 8.770518838402102073E-15, -1.000000000000000000 ) ) ;
#182813 = CARTESIAN_POINT ( 'NONE',  ( 21.14999999999999858, 8.980461154494404852, -187.0187154576991304 ) ) ;
#182814 = ORIENTED_EDGE ( 'NONE', *, *, #240088, .F. ) ;
#182815 = AXIS2_PLACEMENT_3D ( 'NONE', #248115, #210293, #29123 ) ;
#182816 = CIRCLE ( 'NONE', #41157, 11.65000000000000391 ) ;
#182817 = ORIENTED_EDGE ( 'NONE', *, *, #180755, .F. ) ;
#182818 = CARTESIAN_POINT ( 'NONE',  ( 21.97500000000000497, 22.61918030723622408, -230.9697045991730988 ) ) ;
#182819 = CIRCLE ( 'NONE', #70396, 2.000000000000001776 ) ;
#182820 = ORIENTED_EDGE ( 'NONE', *, *, #214699, .T. ) ;
#182821 = CARTESIAN_POINT ( 'NONE',  ( 18.49999999999999645, 46.45388641681647357, -243.1520440498138385 ) ) ;
#182822 = EDGE_CURVE ( 'NONE', #97363, #214650, #141956, .T. ) ;
#182823 = ADVANCED_FACE ( 'NONE', ( #41044 ), #120578, .T. ) ;
#182824 = ORIENTED_EDGE ( 'NONE', *, *, #84100, .T. ) ;
#182825 = AXIS2_PLACEMENT_3D ( 'NONE', #138390, #158036, #18476 ) ;
#182826 = CARTESIAN_POINT ( 'NONE',  ( -23.25000000000000000, 2.319530388122572617, -217.8268657444419887 ) ) ;
#182827 = CONICAL_SURFACE ( 'NONE', #257749, 4.049999999999998046, 0.7853981633974604915 ) ;
#182829 = AXIS2_PLACEMENT_3D ( 'NONE', #237211, #42853, #179813 ) ;
#182828 = DIRECTION ( 'NONE',  ( 1.000000000000000000, -0.000000000000000000, -0.000000000000000000 ) ) ;
#182830 = AXIS2_PLACEMENT_3D ( 'NONE', #163106, #242613, #243899 ) ;
#182831 = ADVANCED_FACE ( 'NONE', ( #21476 ), #146050, .T. ) ;
#182832 = CARTESIAN_POINT ( 'NONE',  ( 20.09999999999999787, 9.749999999999982236, -9.250000000000001776 ) ) ;
#182833 = VERTEX_POINT ( 'NONE', #59248 ) ;
#182834 = ADVANCED_FACE ( 'NONE', ( #102233 ), #142661, .T. ) ;
#182835 = CARTESIAN_POINT ( 'NONE',  ( -24.30000000000000071, -12.80000000000000249, -347.0000000000001137 ) ) ;
#182836 = DIRECTION ( 'NONE',  ( -1.000000000000000000, -0.000000000000000000, 0.000000000000000000 ) ) ;
#182837 = EDGE_CURVE ( 'NONE', #81993, #248248, #183111, .T. ) ;
#182838 = DIRECTION ( 'NONE',  ( 0.000000000000000000, 0.9856811345164832039, 0.1686199900910280158 ) ) ;
#182839 = CARTESIAN_POINT ( 'NONE',  ( 21.14999999999999858, 6.550000000011156231, -112.6500000000000341 ) ) ;
#182840 = FACE_OUTER_BOUND ( 'NONE', #241711, .T. ) ;
#182841 = CARTESIAN_POINT ( 'NONE',  ( 21.05000000000005400, 82.84256550613280012, -26.34830530078816935 ) ) ;
#182842 = DIRECTION ( 'NONE',  ( 1.000000000000000000, -1.207181226542539700E-16, 2.694675058168174199E-16 ) ) ;
#182843 = ORIENTED_EDGE ( 'NONE', *, *, #229768, .F. ) ;
#182845 = CARTESIAN_POINT ( 'NONE',  ( -22.46246831459151494, 75.97808783307333158, -215.1729720457343262 ) ) ;
#182844 = CARTESIAN_POINT ( 'NONE',  ( -20.54999999999999716, 54.14029358995846053, -238.9803212882090691 ) ) ;
#182846 = AXIS2_PLACEMENT_3D ( 'NONE', #22115, #161632, #23411 ) ;
#182847 = VERTEX_POINT ( 'NONE', #141394 ) ;
#182849 = VERTEX_POINT ( 'NONE', #64440 ) ;
#182848 = DIRECTION ( 'NONE',  ( 1.000000000000000000, 0.000000000000000000, -0.000000000000000000 ) ) ;
#182850 = ORIENTED_EDGE ( 'NONE', *, *, #164799, .T. ) ;
#182851 = CARTESIAN_POINT ( 'NONE',  ( 18.58685178364169133, -9.406733083804247997, -7.124420469087726637 ) ) ;
#182852 = CARTESIAN_POINT ( 'NONE',  ( -20.64999999999999858, 4.350000000011156054, -179.8499999999999943 ) ) ;
#182853 = DIRECTION ( 'NONE',  ( 0.000000000000000000, 0.000000000000000000, -1.000000000000000000 ) ) ;
#182854 = CARTESIAN_POINT ( 'NONE',  ( -21.05000000000000071, 1.115653327213047955E-11, -62.70000000000008811 ) ) ;
#182855 = ORIENTED_EDGE ( 'NONE', *, *, #10574, .T. ) ;
#182856 = EDGE_CURVE ( 'NONE', #116798, #82199, #133578, .T. ) ;
#182857 = DIRECTION ( 'NONE',  ( 0.000000000000000000, -0.9501938099239353175, 0.3116596277708039708 ) ) ;
#182858 = SPHERICAL_SURFACE ( 'NONE', #218723, 0.1000000000000000056 ) ;
#182859 = AXIS2_PLACEMENT_3D ( 'NONE', #117312, #74371, #14389 ) ;
#182860 = ORIENTED_EDGE ( 'NONE', *, *, #92532, .F. ) ;
#182861 = CIRCLE ( 'NONE', #236791, 0.09999999999999939493 ) ;
#182862 = CARTESIAN_POINT ( 'NONE',  ( -23.25000000000000000, 2.600000000000000089, -20.27537807723789953 ) ) ;
#182863 = EDGE_CURVE ( 'NONE', #113079, #77452, #200222, .T. ) ;
#182864 = AXIS2_PLACEMENT_3D ( 'NONE', #253985, #37531, #177054 ) ;
#182865 = CARTESIAN_POINT ( 'NONE',  ( 18.59999999999999076, 10.20857864377385127, -121.8500000000000369 ) ) ;
#182866 = ORIENTED_EDGE ( 'NONE', *, *, #112718, .F. ) ;
#182867 = DIRECTION ( 'NONE',  ( 0.000000000000000000, -1.000000000000000000, 0.000000000000000000 ) ) ;
#182868 = VECTOR ( 'NONE', #81304, 1000.000000000000227 ) ;
#182869 = DIRECTION ( 'NONE',  ( 0.000000000000000000, 0.000000000000000000, -1.000000000000000000 ) ) ;
#182870 = VERTEX_POINT ( 'NONE', #163534 ) ;
#182871 = CARTESIAN_POINT ( 'NONE',  ( -16.94107738177415712, 10.01423928514777728, -180.0499999999999545 ) ) ;
#182872 = EDGE_CURVE ( 'NONE', #254638, #143544, #43590, .T. ) ;
#182873 = CARTESIAN_POINT ( 'NONE',  ( 21.05000000000000426, 6.413826288824131971, -134.0857409370334778 ) ) ;
#182874 = FACE_OUTER_BOUND ( 'NONE', #109705, .T. ) ;
#182875 = CARTESIAN_POINT ( 'NONE',  ( 23.14999999999999503, 42.98415524044398950, -233.9519173640447889 ) ) ;
#182876 = CIRCLE ( 'NONE', #203522, 0.1000000000000124678 ) ;
#182877 = AXIS2_PLACEMENT_3D ( 'NONE', #215614, #232646, #115241 ) ;
#182879 = EDGE_CURVE ( 'NONE', #89267, #215885, #19171, .T. ) ;
#182878 = DIRECTION ( 'NONE',  ( 0.000000000000000000, 0.9999631594459056361, -0.008583690987128059571 ) ) ;
#182881 = CARTESIAN_POINT ( 'NONE',  ( -20.64999999999999858, 7.250000000011155521, -45.85000000000000142 ) ) ;
#182880 = AXIS2_PLACEMENT_3D ( 'NONE', #85015, #148889, #190592 ) ;
#182882 = VERTEX_POINT ( 'NONE', #47420 ) ;
#182883 = DIRECTION ( 'NONE',  ( 0.000000000000000000, -0.9651348961777157509, 0.2617529984165031243 ) ) ;
#182884 = ORIENTED_EDGE ( 'NONE', *, *, #138548, .T. ) ;
#182885 = CARTESIAN_POINT ( 'NONE',  ( -23.15000000000000213, 23.45160524131172508, -253.2535058871250726 ) ) ;
#182886 = DIRECTION ( 'NONE',  ( 0.000000000000000000, 0.000000000000000000, -1.000000000000000000 ) ) ;
#182888 = EDGE_LOOP ( 'NONE', ( #200166, #235101, #132609, #2483 ) ) ;
#182887 = CARTESIAN_POINT ( 'NONE',  ( 21.12400247839510925, 10.72148804404153921, -146.2500000000000568 ) ) ;
#182890 = EDGE_LOOP ( 'NONE', ( #230521, #41139, #13121, #177392 ) ) ;
#182889 = CARTESIAN_POINT ( 'NONE',  ( 21.05000005001279817, 67.12872030824136971, -57.34515989627826826 ) ) ;
#182891 = LINE ( 'NONE', #5484, #77046 ) ;
#182892 = CARTESIAN_POINT ( 'NONE',  ( -20.65000000000000568, 7.250000000011138646, -113.1500000000000341 ) ) ;
#182894 = VERTEX_POINT ( 'NONE', #74421 ) ;
#182893 = DIRECTION ( 'NONE',  ( 0.000000000000000000, -0.7397360091702744889, 0.6728971962616842051 ) ) ;
#182895 = DIRECTION ( 'NONE',  ( 0.000000000000000000, 0.000000000000000000, 1.000000000000000000 ) ) ;
#182896 = ORIENTED_EDGE ( 'NONE', *, *, #210598, .F. ) ;
#182897 = EDGE_LOOP ( 'NONE', ( #86357, #105238, #225743, #13423 ) ) ;
#182898 = CARTESIAN_POINT ( 'NONE',  ( -18.48408745364670480, 85.66432225867477257, -62.84002895119587606 ) ) ;
#182899 = FACE_OUTER_BOUND ( 'NONE', #172385, .T. ) ;
#182900 = ORIENTED_EDGE ( 'NONE', *, *, #15160, .F. ) ;
#182901 = CARTESIAN_POINT ( 'NONE',  ( -23.15000000000000213, 64.35000000001249987, -177.0379132551783812 ) ) ;
#182902 = ADVANCED_FACE ( 'NONE', ( #188237 ), #145241, .F. ) ;
#182903 = CARTESIAN_POINT ( 'NONE',  ( -16.87036670365549895, 9.989418819312803066, -180.0204398826979286 ) ) ;
#182904 = AXIS2_PLACEMENT_3D ( 'NONE', #222548, #86884, #166479 ) ;
#182905 = AXIS2_PLACEMENT_3D ( 'NONE', #105967, #70753, #150275 ) ;
#182906 = VERTEX_POINT ( 'NONE', #14437 ) ;
#182907 = AXIS2_PLACEMENT_3D ( 'NONE', #123451, #247232, #68617 ) ;
#182908 = TOROIDAL_SURFACE ( 'NONE', #153730, 0.6000000000000004219, 0.1000000000000000056 ) ;
#182909 = CARTESIAN_POINT ( 'NONE',  ( -16.88853107394619357, 66.04912151666452758, -48.67017113763215974 ) ) ;
#182910 = LINE ( 'NONE', #142471, #93010 ) ;
#182911 = ORIENTED_EDGE ( 'NONE', *, *, #32652, .F. ) ;
#182912 = AXIS2_PLACEMENT_3D ( 'NONE', #155509, #182756, #161916 ) ;
#182913 = EDGE_LOOP ( 'NONE', ( #186750, #219634, #137850, #70672 ) ) ;
#182914 = DIRECTION ( 'NONE',  ( 2.952720810173289112E-16, 1.000000000000000000, 7.086529944415894657E-15 ) ) ;
#182915 = ORIENTED_EDGE ( 'NONE', *, *, #110834, .F. ) ;
#182916 = ADVANCED_FACE ( 'NONE', ( #7023 ), #29562, .F. ) ;
#182917 = FACE_OUTER_BOUND ( 'NONE', #83287, .T. ) ;
#182918 = VERTEX_POINT ( 'NONE', #166143 ) ;
#182920 = ORIENTED_EDGE ( 'NONE', *, *, #240506, .F. ) ;
#182919 = CARTESIAN_POINT ( 'NONE',  ( 21.00000000000000000, 9.750000000011153745, -112.8500000000000369 ) ) ;
#182922 = EDGE_CURVE ( 'NONE', #169290, #54640, #254371, .T. ) ;
#182921 = CARTESIAN_POINT ( 'NONE',  ( -18.59999999999999787, 1.115600667400684642E-11, -167.4999999999999716 ) ) ;
#182923 = EDGE_LOOP ( 'NONE', ( #199816, #170408, #120118, #82142 ) ) ;
#182924 = CARTESIAN_POINT ( 'NONE',  ( -22.39999999999999503, 1.115541036281197940E-11, -92.70922040162662370 ) ) ;
#182925 = CIRCLE ( 'NONE', #211967, 0.1000000000000108025 ) ;
#182926 = CIRCLE ( 'NONE', #70520, 0.2000000000000005107 ) ;
#182927 = ORIENTED_EDGE ( 'NONE', *, *, #103325, .T. ) ;
#182929 = EDGE_LOOP ( 'NONE', ( #152481, #29857, #36176, #118384 ) ) ;
#182928 = ORIENTED_EDGE ( 'NONE', *, *, #151531, .T. ) ;
#182931 = CARTESIAN_POINT ( 'NONE',  ( 21.05000000000000071, 69.74218538953601865, -136.6208977758331287 ) ) ;
#182930 = CIRCLE ( 'NONE', #224596, 0.09999999999999939493 ) ;
#182932 = CARTESIAN_POINT ( 'NONE',  ( -20.64999999999999858, 7.150000000011155876, -146.3500000000000227 ) ) ;
#182934 = ADVANCED_FACE ( 'NONE', ( #212620 ), #245644, .F. ) ;
#182933 = EDGE_LOOP ( 'NONE', ( #80166, #42551, #72944, #220827 ) ) ;
#182935 = AXIS2_PLACEMENT_3D ( 'NONE', #13361, #18496, #77169 ) ;
#182936 = ADVANCED_FACE ( 'NONE', ( #172245 ), #147838, .T. ) ;
#182937 = EDGE_CURVE ( 'NONE', #41742, #139213, #206512, .T. ) ;
#182938 = VERTEX_POINT ( 'NONE', #128269 ) ;
#182939 = DIRECTION ( 'NONE',  ( -0.000000000000000000, 1.000000000000000000, 2.891205793294679805E-16 ) ) ;
#182940 = DIRECTION ( 'NONE',  ( -1.000000000000000000, -7.304098846218135653E-16, 4.607487905232624742E-31 ) ) ;
#182942 = VERTEX_POINT ( 'NONE', #53533 ) ;
#182941 = CARTESIAN_POINT ( 'NONE',  ( -21.14999999999999858, -11.74999999998884448, -67.00000000000004263 ) ) ;
#182943 = DIRECTION ( 'NONE',  ( 0.000000000000000000, -0.3896596508880098009, -0.9209589331071361684 ) ) ;
#182944 = ORIENTED_EDGE ( 'NONE', *, *, #184122, .F. ) ;
#182945 = EDGE_CURVE ( 'NONE', #52103, #207394, #175478, .T. ) ;
#182946 = CARTESIAN_POINT ( 'NONE',  ( -17.29158576265543346, 65.63525233399359138, -47.44034923973222106 ) ) ;
#182947 = CARTESIAN_POINT ( 'NONE',  ( -23.25000000000000355, 58.31215475832291162, -223.8520309854405923 ) ) ;
#182948 = ORIENTED_EDGE ( 'NONE', *, *, #77344, .F. ) ;
#182949 = PLANE ( 'NONE',  #86230 ) ;
#182950 = CARTESIAN_POINT ( 'NONE',  ( -18.34374000495059676, 11.47316190337362940, -57.75000000000000711 ) ) ;
#182951 = EDGE_CURVE ( 'NONE', #79720, #147882, #26614, .T. ) ;
#182952 = ORIENTED_EDGE ( 'NONE', *, *, #214430, .T. ) ;
#182953 = CARTESIAN_POINT ( 'NONE',  ( -16.94445028196808778, 66.00793639031412852, -90.41577730610593733 ) ) ;
#182954 = ORIENTED_EDGE ( 'NONE', *, *, #2918, .T. ) ;
#182955 = AXIS2_PLACEMENT_3D ( 'NONE', #13165, #90104, #10598 ) ;
#182957 = ORIENTED_EDGE ( 'NONE', *, *, #179314, .T. ) ;
#182956 = ORIENTED_EDGE ( 'NONE', *, *, #77556, .F. ) ;
#182958 = ORIENTED_EDGE ( 'NONE', *, *, #173006, .T. ) ;
#182959 = DIRECTION ( 'NONE',  ( 1.000000000000000000, -0.000000000000000000, -0.000000000000000000 ) ) ;
#182960 = EDGE_LOOP ( 'NONE', ( #2021, #233264, #248340, #15546 ) ) ;
#182961 = CARTESIAN_POINT ( 'NONE',  ( -18.79999999999999716, 1.149999999999999911, -15.00000000000000000 ) ) ;
#182962 = VECTOR ( 'NONE', #149327, 1000.000000000000000 ) ;
#182963 = ORIENTED_EDGE ( 'NONE', *, *, #176025, .F. ) ;
#182964 = CARTESIAN_POINT ( 'NONE',  ( -16.91256925476570672, 66.01426884188333588, -48.55546499551912376 ) ) ;
#182965 = CARTESIAN_POINT ( 'NONE',  ( 23.24999999999999289, 53.24180694658302571, -234.8354225850497130 ) ) ;
#182966 = EDGE_CURVE ( 'NONE', #149012, #170938, #233743, .T. ) ;
#182967 = ORIENTED_EDGE ( 'NONE', *, *, #2804, .T. ) ;
#182968 = ORIENTED_EDGE ( 'NONE', *, *, #251364, .T. ) ;
#182969 = CIRCLE ( 'NONE', #82958, 3.900000000000000799 ) ;
#182971 = ORIENTED_EDGE ( 'NONE', *, *, #44807, .T. ) ;
#182970 = AXIS2_PLACEMENT_3D ( 'NONE', #111547, #151987, #231505 ) ;
#182972 = AXIS2_PLACEMENT_3D ( 'NONE', #189552, #153020, #253356 ) ;
#182973 = ADVANCED_FACE ( 'NONE', ( #107406 ), #87823, .T. ) ;
#182974 = CARTESIAN_POINT ( 'NONE',  ( 21.05000000000000071, 69.74115287693359733, -203.5548658375798823 ) ) ;
#182975 = ORIENTED_EDGE ( 'NONE', *, *, #41412, .T. ) ;
#182976 = FACE_OUTER_BOUND ( 'NONE', #194568, .T. ) ;
#182977 = CARTESIAN_POINT ( 'NONE',  ( -13.40000000000000213, -11.65000000000000036, 15.00000000000000355 ) ) ;
#182978 = CARTESIAN_POINT ( 'NONE',  ( -16.77732147262506146, 14.15218621894316087, -219.2427314506515756 ) ) ;
#182979 = DIRECTION ( 'NONE',  ( 1.000000000000000000, 0.000000000000000000, 0.000000000000000000 ) ) ;
#182980 = CIRCLE ( 'NONE', #216089, 0.09999999999999939493 ) ;
#182981 = CARTESIAN_POINT ( 'NONE',  ( 21.05000000000000071, 65.57661458509943486, -162.5310555606543232 ) ) ;
#182982 = DIRECTION ( 'NONE',  ( 0.000000000000000000, 0.000000000000000000, -1.000000000000000000 ) ) ;
#182984 = CYLINDRICAL_SURFACE ( 'NONE', #128639, 0.09999999999998898659 ) ;
#182983 = CARTESIAN_POINT ( 'NONE',  ( -23.49999999999994316, 64.25000000001119815, -3.123107484524795474 ) ) ;
#182985 = CARTESIAN_POINT ( 'NONE',  ( 20.94999999999999929, 43.16354019706792400, -239.5695141926698284 ) ) ;
#182986 = CARTESIAN_POINT ( 'NONE',  ( 19.93974701750897438, 4.631764625248131928, 22.00000000173902137 ) ) ;
#182987 = DIRECTION ( 'NONE',  ( 0.000000000000000000, -0.2438576117979363023, 0.9698110461157920525 ) ) ;
#182988 = EDGE_LOOP ( 'NONE', ( #235248, #120143, #191139 ) ) ;
#182989 = EDGE_CURVE ( 'NONE', #222451, #105736, #207834, .T. ) ;
#182990 = CIRCLE ( 'NONE', #58046, 4.000000000000010658 ) ;
#182991 = AXIS2_PLACEMENT_3D ( 'NONE', #54499, #237001, #197857 ) ;
#182992 = AXIS2_PLACEMENT_3D ( 'NONE', #172788, #64971, #46684 ) ;
#182993 = CIRCLE ( 'NONE', #232885, 11.90000000000000568 ) ;
#182995 = ORIENTED_EDGE ( 'NONE', *, *, #35846, .F. ) ;
#182994 = DIRECTION ( 'NONE',  ( 1.186688945009010077E-16, 0.4088369013363281068, -0.9126074666063770380 ) ) ;
#182996 = ORIENTED_EDGE ( 'NONE', *, *, #56964, .T. ) ;
#182997 = AXIS2_PLACEMENT_3D ( 'NONE', #149659, #50508, #210891 ) ;
#182998 = CARTESIAN_POINT ( 'NONE',  ( 23.15000000000000213, -9.499999999988844479, -90.60603087734760663 ) ) ;
#182999 = ADVANCED_FACE ( 'NONE', ( #253010 ), #117208, .T. ) ;
#183000 = CARTESIAN_POINT ( 'NONE',  ( -17.01473183483380680, 9.950000000011138823, -54.25000000000000000 ) ) ;
#183001 = CARTESIAN_POINT ( 'NONE',  ( 23.24999999999999289, 45.29262862071417572, -238.6157088101306556 ) ) ;
#183002 = ORIENTED_EDGE ( 'NONE', *, *, #52299, .T. ) ;
#183003 = EDGE_CURVE ( 'NONE', #61667, #173551, #153161, .T. ) ;
#183004 = SURFACE_STYLE_FILL_AREA ( #160876 ) ;
#183005 = ADVANCED_FACE ( 'NONE', ( #34012 ), #237313, .F. ) ;
#183006 = CYLINDRICAL_SURFACE ( 'NONE', #87341, 0.09999999999999939493 ) ;
#183007 = PRODUCT_DEFINITION_SHAPE ( 'NONE', 'NONE',  #258125 ) ;
#183008 = DIRECTION ( 'NONE',  ( -1.000000000000000000, 2.952720810173289112E-16, 2.061873921506763405E-30 ) ) ;
#183009 = AXIS2_PLACEMENT_3D ( 'NONE', #146527, #184381, #46160 ) ;
#183010 = EDGE_LOOP ( 'NONE', ( #223413, #110645, #57838, #227931 ) ) ;
#183011 = DIRECTION ( 'NONE',  ( 0.000000000000000000, -0.9770955615653316162, -0.2128009952263604232 ) ) ;
#183012 = CARTESIAN_POINT ( 'NONE',  ( 18.59999999999999076, 62.49201502323811752, -208.8221019049098857 ) ) ;
#183013 = EDGE_CURVE ( 'NONE', #60388, #48459, #75684, .T. ) ;
#183014 = LINE ( 'NONE', #160887, #99498 ) ;
#183016 = VERTEX_POINT ( 'NONE', #78221 ) ;
#183015 = CARTESIAN_POINT ( 'NONE',  ( 23.14999999999999858, 70.40000000001253966, -182.4283735034374843 ) ) ;
#183017 = CARTESIAN_POINT ( 'NONE',  ( 21.05000000000000071, 10.72371710471867701, -79.15000000000004832 ) ) ;
#183019 = ORIENTED_EDGE ( 'NONE', *, *, #178311, .T. ) ;
#183018 = DIRECTION ( 'NONE',  ( 0.000000000000000000, 0.000000000000000000, -1.000000000000000000 ) ) ;
#183020 = FACE_OUTER_BOUND ( 'NONE', #70926, .T. ) ;
#183021 = CARTESIAN_POINT ( 'NONE',  ( -23.15000000000000213, 86.43238724539048690, -209.5644480942280836 ) ) ;
#183022 = ORIENTED_EDGE ( 'NONE', *, *, #26073, .F. ) ;
#183023 = CARTESIAN_POINT ( 'NONE',  ( -16.93339986808596720, 65.99489607144637660, -157.4571138127115830 ) ) ;
#183024 = AXIS2_PLACEMENT_3D ( 'NONE', #169438, #112005, #191555 ) ;
#183025 = CARTESIAN_POINT ( 'NONE',  ( -21.64999999999999858, 9.350000000011133849, -76.25000000000004263 ) ) ;
#183027 = DIRECTION ( 'NONE',  ( 0.000000000000000000, -0.2818822000685679008, 0.9594490217226259166 ) ) ;
#183026 = CYLINDRICAL_SURFACE ( 'NONE', #228209, 0.09999999999999939493 ) ;
#183028 = CARTESIAN_POINT ( 'NONE',  ( 21.05000000000000071, 36.65892442174935439, -249.5511627012433848 ) ) ;
#183029 = CARTESIAN_POINT ( 'NONE',  ( 20.95224633520496127, 40.77109002121920156, -237.9561148901888430 ) ) ;
#183030 = CARTESIAN_POINT ( 'NONE',  ( -18.50596464788227635, 10.30632246270531560, -39.00418367788958562 ) ) ;
#183031 = CARTESIAN_POINT ( 'NONE',  ( 23.14999999999999858, 5.500000000011153745, -79.40526601891313874 ) ) ;
#183032 = CARTESIAN_POINT ( 'NONE',  ( 21.05000000000000071, 1.115600667400684642E-11, -100.5000000000000426 ) ) ;
#183034 = EDGE_LOOP ( 'NONE', ( #239503, #5832, #38053 ) ) ;
#183033 = AXIS2_PLACEMENT_3D ( 'NONE', #36819, #39386, #116335 ) ;
#183035 = CARTESIAN_POINT ( 'NONE',  ( 23.14999999999998437, 76.00000000001216449, -140.5731074845242858 ) ) ;
#183036 = ORIENTED_EDGE ( 'NONE', *, *, #234562, .T. ) ;
#183037 = ORIENTED_EDGE ( 'NONE', *, *, #107575, .T. ) ;
#183038 = DIRECTION ( 'NONE',  ( 0.000000000000000000, -1.000000000000000000, 0.000000000000000000 ) ) ;
#183039 = CARTESIAN_POINT ( 'NONE',  ( -23.25000000000000000, 7.021664781911246322, -137.8335654018973457 ) ) ;
#183040 = EDGE_CURVE ( 'NONE', #249694, #246415, #236015, .T. ) ;
#183041 = ORIENTED_EDGE ( 'NONE', *, *, #221498, .T. ) ;
#183042 = ADVANCED_FACE ( 'NONE', ( #95226 ), #150526, .T. ) ;
#183043 = AXIS2_PLACEMENT_3D ( 'NONE', #152328, #147157, #10235 ) ;
#183044 = ORIENTED_EDGE ( 'NONE', *, *, #25519, .T. ) ;
#183045 = CIRCLE ( 'NONE', #12194, 0.09999999999998898659 ) ;
#183046 = ADVANCED_FACE ( 'NONE', ( #136919 ), #196887, .T. ) ;
#183047 = ORIENTED_EDGE ( 'NONE', *, *, #4953, .T. ) ;
#183048 = DIRECTION ( 'NONE',  ( 0.000000000000000000, -0.1350103645451876666, -0.9908441862701600211 ) ) ;
#183049 = AXIS2_PLACEMENT_3D ( 'NONE', #196134, #254770, #76169 ) ;
#183050 = ORIENTED_EDGE ( 'NONE', *, *, #37475, .T. ) ;
#183051 = CARTESIAN_POINT ( 'NONE',  ( -23.15000000000000213, 4.150000000000001243, 11.75000000000000000 ) ) ;
#183052 = CARTESIAN_POINT ( 'NONE',  ( 20.04142135623730070, 21.17283678855157802, -243.7231193059830332 ) ) ;
#183053 = CARTESIAN_POINT ( 'NONE',  ( 21.05000000000000071, 75.90220970870321082, -109.2809220950004345 ) ) ;
#183054 = DIRECTION ( 'NONE',  ( 1.000000000000000000, 0.000000000000000000, 0.000000000000000000 ) ) ;
#183055 = CARTESIAN_POINT ( 'NONE',  ( -20.94999999999999929, 87.29603075034721371, -106.0710066441880883 ) ) ;
#183056 = CARTESIAN_POINT ( 'NONE',  ( -23.15000000000000213, 56.06656052939784729, -228.0911609752645290 ) ) ;
#183057 = DIRECTION ( 'NONE',  ( 0.000000000000000000, -0.4856429311786307212, -0.8741572761215384846 ) ) ;
#183059 = ORIENTED_EDGE ( 'NONE', *, *, #70897, .T. ) ;
#183058 = CARTESIAN_POINT ( 'NONE',  ( 23.24999999999999645, 79.76402609510435582, -204.5439441783492498 ) ) ;
#183061 = DIRECTION ( 'NONE',  ( -0.000000000000000000, 0.8660254037844411501, 0.4999999999999956701 ) ) ;
#183060 = CARTESIAN_POINT ( 'NONE',  ( 20.95265033839679347, 65.48774916754445030, -61.95734372849443616 ) ) ;
#183062 = DIRECTION ( 'NONE',  ( 1.000000000000000000, 0.000000000000000000, 0.000000000000000000 ) ) ;
#183063 = EDGE_LOOP ( 'NONE', ( #209545, #60716, #88029, #126672 ) ) ;
#183064 = CARTESIAN_POINT ( 'NONE',  ( -21.05000000000000071, 67.70174932746996888, -211.7710791003628401 ) ) ;
#183065 = DIRECTION ( 'NONE',  ( 0.000000000000000000, 0.4930308989875575865, 0.8700118002898125091 ) ) ;
#183066 = EDGE_LOOP ( 'NONE', ( #186206, #203153, #1532, #105648 ) ) ;
#183068 = CARTESIAN_POINT ( 'NONE',  ( -16.93211319090181632, 66.00001321885453365, -115.6006019852513020 ) ) ;
#183067 = CARTESIAN_POINT ( 'NONE',  ( -0.8999999999999425127, 64.35000000001120668, -7.423107484524793520 ) ) ;
#183069 = VECTOR ( 'NONE', #156245, 1000.000000000000000 ) ;
#183070 = ADVANCED_FACE ( 'NONE', ( #217720 ), #76940, .F. ) ;
#183071 = B_SPLINE_CURVE_WITH_KNOTS ( 'NONE', 3,
 ( #204491, #25887, #141957, #105364, #104096, #6290, #122410, #84507, #143238, #45434 ),
 .UNSPECIFIED., .F., .F.,
 ( 4, 3, 3, 4 ),
 ( 0.000000000000000000, 0.0002000000000002908468, 0.001000000000045115191, 0.001967863649472108723 ),
 .UNSPECIFIED. ) ;
#183072 = DIRECTION ( 'NONE',  ( 1.000000000000000000, 0.000000000000000000, 0.000000000000000000 ) ) ;
#183073 = ORIENTED_EDGE ( 'NONE', *, *, #13164, .T. ) ;
#183074 = CARTESIAN_POINT ( 'NONE',  ( -20.94999999999999929, 77.16412189325305349, -95.30825939895268561 ) ) ;
#183075 = CYLINDRICAL_SURFACE ( 'NONE', #186777, 0.1000000000000028644 ) ;
#183076 = LINE ( 'NONE', #22732, #228142 ) ;
#183077 = EDGE_CURVE ( 'NONE', #4930, #83940, #216448, .T. ) ;
#183078 = CARTESIAN_POINT ( 'NONE',  ( -22.39999999999999503, 1.114087072463500573E-11, -122.2495671075414094 ) ) ;
#183079 = ORIENTED_EDGE ( 'NONE', *, *, #49650, .F. ) ;
#183080 = VERTEX_POINT ( 'NONE', #96487 ) ;
#183081 = EDGE_CURVE ( 'NONE', #236987, #198367, #121348, .T. ) ;
#183082 = CARTESIAN_POINT ( 'NONE',  ( 21.11345278033283890, 67.11787792664061669, -90.77708531376950418 ) ) ;
#183083 = CARTESIAN_POINT ( 'NONE',  ( 20.97239005616516394, 67.12515615866247742, -191.2729546823712496 ) ) ;
#183084 = CIRCLE ( 'NONE', #170658, 1.900000000000005906 ) ;
#183085 = CARTESIAN_POINT ( 'NONE',  ( -20.64999999999999858, 7.250000000011155521, -45.75000000000000000 ) ) ;
#183086 = VECTOR ( 'NONE', #114684, 1000.000000000000000 ) ;
#183087 = ADVANCED_FACE ( 'NONE', ( #99051 ), #234738, .T. ) ;
#183088 = AXIS2_PLACEMENT_3D ( 'NONE', #90421, #154314, #228681 ) ;
#183089 = AXIS2_PLACEMENT_3D ( 'NONE', #98957, #116007, #153887 ) ;
#183090 = CARTESIAN_POINT ( 'NONE',  ( -23.15000000000000213, 85.00000000001159606, -60.12913836187181715 ) ) ;
#183091 = EDGE_CURVE ( 'NONE', #251642, #207654, #6692, .T. ) ;
#183093 = ORIENTED_EDGE ( 'NONE', *, *, #38371, .F. ) ;
#183092 = PLANE ( 'NONE',  #229641 ) ;
#183094 = CIRCLE ( 'NONE', #145648, 12.87499999999999467 ) ;
#183095 = DIRECTION ( 'NONE',  ( -1.000000000000000000, 0.000000000000000000, 0.000000000000000000 ) ) ;
#183096 = ADVANCED_FACE ( 'NONE', ( #219014 ), #179583, .F. ) ;
#183097 = DIRECTION ( 'NONE',  ( -2.252264143451594314E-15, -0.1298341882520124002, -0.9915357197604841577 ) ) ;
#183098 = CARTESIAN_POINT ( 'NONE',  ( -18.50000000000000000, 64.25000000001195133, -102.9231074845243938 ) ) ;
#183099 = CARTESIAN_POINT ( 'NONE',  ( 21.04999999999999716, 6.304455821958825368, -167.5210354765400780 ) ) ;
#183100 = DIRECTION ( 'NONE',  ( 0.000000000000000000, 0.000000000000000000, -1.000000000000000000 ) ) ;
#183102 = ORIENTED_EDGE ( 'NONE', *, *, #99644, .T. ) ;
#183101 = DIRECTION ( 'NONE',  ( 0.000000000000000000, 1.000000000000000000, -0.000000000000000000 ) ) ;
#183103 = LINE ( 'NONE', #123125, #25773 ) ;
#183104 = CARTESIAN_POINT ( 'NONE',  ( -18.52643265882458579, 65.68026841930954163, -164.4725740131889893 ) ) ;
#183105 = CARTESIAN_POINT ( 'NONE',  ( 21.05000000000000071, -11.29603075032412640, -164.4521008403361577 ) ) ;
#183106 = CARTESIAN_POINT ( 'NONE',  ( 20.94999999999999929, 85.00000000001251976, -179.9170766071767389 ) ) ;
#183107 = ORIENTED_EDGE ( 'NONE', *, *, #187811, .T. ) ;
#183108 = CARTESIAN_POINT ( 'NONE',  ( -15.06720934482786411, 66.58230930894919197, -151.8815067877598608 ) ) ;
#183109 = CARTESIAN_POINT ( 'NONE',  ( -16.89155683852747103, 66.05000000001469118, -116.3004793340649741 ) ) ;
#183110 = AXIS2_PLACEMENT_3D ( 'NONE', #74048, #12784, #171873 ) ;
#183111 = LINE ( 'NONE', #181812, #246012 ) ;
#183112 = CIRCLE ( 'NONE', #41656, 0.09999999999999939493 ) ;
#183113 = FACE_OUTER_BOUND ( 'NONE', #255224, .T. ) ;
#183114 = VERTEX_POINT ( 'NONE', #199486 ) ;
#183115 = CARTESIAN_POINT ( 'NONE',  ( -16.82542659449980604, 9.934499891438555608, -87.75536439997381422 ) ) ;
#183117 = ADVANCED_FACE ( 'NONE', ( #45525, #101603, #27284 ), #225421, .T. ) ;
#183116 = CIRCLE ( 'NONE', #149807, 0.09999999999999939493 ) ;
#183118 = EDGE_CURVE ( 'NONE', #158092, #40817, #250296, .T. ) ;
#183119 = VERTEX_POINT ( 'NONE', #186329 ) ;
#183120 = FACE_OUTER_BOUND ( 'NONE', #8234, .T. ) ;
#183121 = CARTESIAN_POINT ( 'NONE',  ( -21.07928932188134041, 33.98134083355423485, -243.8161431329846778 ) ) ;
#183122 = EDGE_CURVE ( 'NONE', #30882, #2981, #187949, .T. ) ;
#183123 = CARTESIAN_POINT ( 'NONE',  ( -20.94999999999999929, 69.56804783242856161, -248.4091712263733882 ) ) ;
#183124 = CARTESIAN_POINT ( 'NONE',  ( 18.39999999999999503, 70.35000000001254250, -179.2731074845243882 ) ) ;
#183125 = ORIENTED_EDGE ( 'NONE', *, *, #129431, .F. ) ;
#183126 = LINE ( 'NONE', #48728, #104483 ) ;
#183127 = EDGE_CURVE ( 'NONE', #14167, #77508, #165485, .T. ) ;
#183128 = CARTESIAN_POINT ( 'NONE',  ( 21.13461538461538680, 12.99955419111918786, -210.8083363671015604 ) ) ;
#183129 = EDGE_CURVE ( 'NONE', #104276, #210147, #183671, .T. ) ;
#183130 = CYLINDRICAL_SURFACE ( 'NONE', #170351, 0.1000000000000055844 ) ;
#183132 = CARTESIAN_POINT ( 'NONE',  ( -16.85697194749130645, 9.908543714123666746, -20.56499573238607326 ) ) ;
#183131 = CIRCLE ( 'NONE', #153953, 0.1999999999999987899 ) ;
#183133 = DIRECTION ( 'NONE',  ( 0.000000000000000000, 0.2128009952263605620, -0.9770955615653313941 ) ) ;
#183134 = VERTEX_POINT ( 'NONE', #7697 ) ;
#183136 = ORIENTED_EDGE ( 'NONE', *, *, #1734, .T. ) ;
#183135 = CARTESIAN_POINT ( 'NONE',  ( -16.87036670365549895, 65.91505003675658259, -90.47310748452439100 ) ) ;
#183137 = ORIENTED_EDGE ( 'NONE', *, *, #101046, .F. ) ;
#183138 = CARTESIAN_POINT ( 'NONE',  ( 18.49999999999998934, 65.75000000001196554, -111.8731074845243683 ) ) ;
#183139 = ORIENTED_EDGE ( 'NONE', *, *, #72860, .T. ) ;
#183140 = CARTESIAN_POINT ( 'NONE',  ( 21.05000000000000071, 61.00573819068043235, -234.0630943441842646 ) ) ;
#183141 = CARTESIAN_POINT ( 'NONE',  ( -23.25000000000000000, 4.349999999999999645, -21.14999999999999858 ) ) ;
#183142 = DIRECTION ( 'NONE',  ( -1.000000000000000000, 0.000000000000000000, 0.000000000000000000 ) ) ;
#183143 = CIRCLE ( 'NONE', #66427, 0.1000000000000028644 ) ;
#183144 = ORIENTED_EDGE ( 'NONE', *, *, #214919, .T. ) ;
#183145 = EDGE_CURVE ( 'NONE', #228089, #50473, #102903, .T. ) ;
#183146 = DIRECTION ( 'NONE',  ( -2.952720810173288126E-16, 0.9770955615653313941, 0.2128009952263603677 ) ) ;
#183147 = DIRECTION ( 'NONE',  ( 1.000000000000000000, 0.000000000000000000, 0.000000000000000000 ) ) ;
#183148 = ORIENTED_EDGE ( 'NONE', *, *, #231921, .T. ) ;
#183149 = CARTESIAN_POINT ( 'NONE',  ( 23.24999999999999645, 71.22429906543254674, -114.8718755885703047 ) ) ;
#183151 = ORIENTED_EDGE ( 'NONE', *, *, #29356, .F. ) ;
#183150 = DIRECTION ( 'NONE',  ( -0.000000000000000000, -6.982962677686266711E-15, 1.000000000000000000 ) ) ;
#183152 = DIRECTION ( 'NONE',  ( 0.000000000000000000, -0.000000000000000000, -1.000000000000000000 ) ) ;
#183153 = DIRECTION ( 'NONE',  ( 1.000000000000000000, -0.000000000000000000, 0.000000000000000000 ) ) ;
#183154 = EDGE_CURVE ( 'NONE', #213696, #94420, #221235, .T. ) ;
#183155 = AXIS2_PLACEMENT_3D ( 'NONE', #47101, #126662, #206202 ) ;
#183156 = CIRCLE ( 'NONE', #216454, 0.09999999999999939493 ) ;
#183157 = VERTEX_POINT ( 'NONE', #221566 ) ;
#183158 = DIRECTION ( 'NONE',  ( -1.000000000000000000, -0.000000000000000000, -0.000000000000000000 ) ) ;
#183159 = DIRECTION ( 'NONE',  ( 0.000000000000000000, 0.3738317757009942399, -0.9274965247785252886 ) ) ;
#183160 = CARTESIAN_POINT ( 'NONE',  ( -18.59999999999999787, 11.65000000001115232, -107.5148057706540357 ) ) ;
#183161 = VERTEX_POINT ( 'NONE', #220323 ) ;
#183162 = CARTESIAN_POINT ( 'NONE',  ( -20.94999999999999929, 18.51199663233067483, -231.2535697180530292 ) ) ;
#183163 = AXIS2_PLACEMENT_3D ( 'NONE', #23033, #102503, #162536 ) ;
#183164 = EDGE_CURVE ( 'NONE', #246198, #198338, #96332, .T. ) ;
#183165 = DIRECTION ( 'NONE',  ( 0.000000000000000000, -0.1350103645451876944, 0.9908441862701601321 ) ) ;
#183166 = AXIS2_PLACEMENT_3D ( 'NONE', #258042, #119893, #199424 ) ;
#183167 = CIRCLE ( 'NONE', #54145, 0.1000000000000024342 ) ;
#183168 = ORIENTED_EDGE ( 'NONE', *, *, #76886, .T. ) ;
#183169 = B_SPLINE_CURVE_WITH_KNOTS ( 'NONE', 3,
 ( #232444, #72075, #14685, #133324, #55040, #152916, #94178 ),
 .UNSPECIFIED., .F., .F.,
 ( 4, 3, 4 ),
 ( 0.000000000000000000, 0.0007844235214594269838, 0.001767853679404345069 ),
 .UNSPECIFIED. ) ;
#183170 = CIRCLE ( 'NONE', #70763, 0.09999999999999939493 ) ;
#183171 = VECTOR ( 'NONE', #98410, 1000.000000000000000 ) ;
#183172 = CIRCLE ( 'NONE', #212220, 0.09999999999999609201 ) ;
#183173 = EDGE_LOOP ( 'NONE', ( #109425, #3661, #251816, #210208 ) ) ;
#183174 = AXIS2_PLACEMENT_3D ( 'NONE', #77453, #177884, #13659 ) ;
#183175 = AXIS2_PLACEMENT_3D ( 'NONE', #212367, #130227, #31187 ) ;
#183176 = ORIENTED_EDGE ( 'NONE', *, *, #123320, .T. ) ;
#183177 = CARTESIAN_POINT ( 'NONE',  ( -18.50000000000000000, 11.65000000001115232, -122.2500000000000284 ) ) ;
#183178 = CIRCLE ( 'NONE', #20694, 11.90000000000000746 ) ;
#183179 = DIRECTION ( 'NONE',  ( 0.000000000000000000, 0.000000000000000000, 1.000000000000000000 ) ) ;
#183181 = ORIENTED_EDGE ( 'NONE', *, *, #143541, .T. ) ;
#183180 = DIRECTION ( 'NONE',  ( 0.000000000000000000, -0.008583690987135041833, 0.9999631594459055250 ) ) ;
#183182 = CARTESIAN_POINT ( 'NONE',  ( -20.64999999999999858, 76.00000000001142553, -36.02310748452432421 ) ) ;
#183183 = DIRECTION ( 'NONE',  ( 1.000000000000000000, 0.000000000000000000, 0.000000000000000000 ) ) ;
#183184 = DIRECTION ( 'NONE',  ( -0.000000000000000000, 0.000000000000000000, -1.000000000000000000 ) ) ;
#183185 = DIRECTION ( 'NONE',  ( -1.000000000000000000, 1.836970198721029934E-16, 1.282749433769087582E-30 ) ) ;
#183186 = CARTESIAN_POINT ( 'NONE',  ( -20.94999999999999929, 64.35000000001251408, -176.8069731475025321 ) ) ;
#183187 = DIRECTION ( 'NONE',  ( 0.000000000000000000, -1.000000000000000000, 0.000000000000000000 ) ) ;
#183189 = ORIENTED_EDGE ( 'NONE', *, *, #79671, .T. ) ;
#183188 = CARTESIAN_POINT ( 'NONE',  ( -18.59999996769639097, -9.363273769819080883, -107.6814939154659783 ) ) ;
#183191 = VERTEX_POINT ( 'NONE', #144604 ) ;
#183190 = DIRECTION ( 'NONE',  ( -1.000000000000000000, -2.952720810173289112E-16, 0.000000000000000000 ) ) ;
#183192 = CARTESIAN_POINT ( 'NONE',  ( 18.54999999999999716, 66.05000000001206217, -123.8731074845244251 ) ) ;
#183193 = ORIENTED_EDGE ( 'NONE', *, *, #57608, .F. ) ;
#183194 = DIRECTION ( 'NONE',  ( 0.000000000000000000, 6.982962677686267499E-15, -1.000000000000000000 ) ) ;
#183195 = DIRECTION ( 'NONE',  ( 0.000000000000000000, 0.000000000000000000, -1.000000000000000000 ) ) ;
#183196 = DIRECTION ( 'NONE',  ( -1.000000000000000000, 2.952720810173289112E-16, 2.061873921506763405E-30 ) ) ;
#183197 = DIRECTION ( 'NONE',  ( 0.000000000000000000, 0.000000000000000000, 1.000000000000000000 ) ) ;
#183198 = EDGE_LOOP ( 'NONE', ( #175229, #15145, #163208, #10557, #104088 ) ) ;
#183199 = VECTOR ( 'NONE', #154992, 1000.000000000000000 ) ;
#183200 = CARTESIAN_POINT ( 'NONE',  ( 21.04999999999999716, 10.48937277454169781, -207.4747812581268249 ) ) ;
#183201 = ORIENTED_EDGE ( 'NONE', *, *, #111284, .T. ) ;
#183202 = EDGE_CURVE ( 'NONE', #221407, #144142, #237821, .T. ) ;
#183203 = CARTESIAN_POINT ( 'NONE',  ( -23.25000000000000000, -11.65000000000000036, -30.39999999999999858 ) ) ;
#183204 = CIRCLE ( 'NONE', #75079, 0.09999999999998898659 ) ;
#183205 = ORIENTED_EDGE ( 'NONE', *, *, #94238, .F. ) ;
#183206 = VECTOR ( 'NONE', #58587, 1000.000000000000227 ) ;
#183207 = LINE ( 'NONE', #144049, #1927 ) ;
#183208 = CARTESIAN_POINT ( 'NONE',  ( -16.90137573187934805, 60.97558894184935241, -220.9081362493511449 ) ) ;
#183209 = ORIENTED_EDGE ( 'NONE', *, *, #71037, .T. ) ;
#183210 = CARTESIAN_POINT ( 'NONE',  ( -20.64999999999999858, 54.73010456436290383, -239.3295147855486107 ) ) ;
#183211 = EDGE_LOOP ( 'NONE', ( #111066, #24181, #170507, #191821 ) ) ;
#183212 = DIRECTION ( 'NONE',  ( 4.239556034732056743E-17, 0.1298341882519953860, 0.9915357197604862671 ) ) ;
#183213 = ORIENTED_EDGE ( 'NONE', *, *, #177987, .T. ) ;
#183215 = ADVANCED_FACE ( 'NONE', ( #164200 ), #126340, .F. ) ;
#183214 = CIRCLE ( 'NONE', #241488, 0.1999999999999921840 ) ;
#183217 = EDGE_CURVE ( 'NONE', #256296, #47933, #254542, .T. ) ;
#183216 = CARTESIAN_POINT ( 'NONE',  ( -21.64999999999999858, 23.11343627288707481, -230.8941331732335129 ) ) ;
#183218 = AXIS2_PLACEMENT_3D ( 'NONE', #2365, #178485, #238431 ) ;
#183219 = CARTESIAN_POINT ( 'NONE',  ( 15.39793903038208533, 9.389686005666813884, -183.1728435063512848 ) ) ;
#183220 = ORIENTED_EDGE ( 'NONE', *, *, #56923, .F. ) ;
#183221 = DIRECTION ( 'NONE',  ( 0.000000000000000000, -7.056502275159890832E-15, 1.000000000000000000 ) ) ;
#183223 = EDGE_LOOP ( 'NONE', ( #21625, #250338, #3597, #56251 ) ) ;
#183222 = CARTESIAN_POINT ( 'NONE',  ( -21.12642695952773764, 6.375659922046319927, -100.4010967168106703 ) ) ;
#183224 = CARTESIAN_POINT ( 'NONE',  ( 21.13461538461538680, 67.11458296203814200, -191.1731074845244223 ) ) ;
#183225 = AXIS2_PLACEMENT_3D ( 'NONE', #48607, #207706, #89010 ) ;
#183226 = VERTEX_POINT ( 'NONE', #104194 ) ;
#183227 = EDGE_CURVE ( 'NONE', #212847, #20798, #183756, .T. ) ;
#183228 = ADVANCED_FACE ( 'NONE', ( #84601 ), #137849, .T. ) ;
#183229 = ORIENTED_EDGE ( 'NONE', *, *, #122043, .T. ) ;
#183230 = CARTESIAN_POINT ( 'NONE',  ( -23.15000000000000213, 4.350000000011156054, -121.6500000000000341 ) ) ;
#183231 = DIRECTION ( 'NONE',  ( 0.000000000000000000, 0.000000000000000000, 1.000000000000000000 ) ) ;
#183232 = FACE_OUTER_BOUND ( 'NONE', #235836, .T. ) ;
#183233 = EDGE_CURVE ( 'NONE', #236853, #128410, #65808, .T. ) ;
#183234 = DIRECTION ( 'NONE',  ( 1.000000000000000000, 0.000000000000000000, 0.000000000000000000 ) ) ;
#183235 = FACE_OUTER_BOUND ( 'NONE', #124563, .T. ) ;
#183236 = ORIENTED_EDGE ( 'NONE', *, *, #169896, .F. ) ;
#183237 = CARTESIAN_POINT ( 'NONE',  ( -18.59999999999999787, 77.26178616857734482, -161.9366085209788650 ) ) ;
#183238 = LINE ( 'NONE', #4575, #140204 ) ;
#183239 = DIRECTION ( 'NONE',  ( 0.000000000000000000, -0.2617529984165031243, -0.9651348961777157509 ) ) ;
#183240 = EDGE_CURVE ( 'NONE', #127487, #16805, #25445, .T. ) ;
#183241 = CARTESIAN_POINT ( 'NONE',  ( -18.59999999999999787, 1.340746217933695750, 10.27286250542118040 ) ) ;
#183242 = VERTEX_POINT ( 'NONE', #128921 ) ;
#183243 = CARTESIAN_POINT ( 'NONE',  ( -21.05000000000000426, 75.98514436511810288, -109.3674665265678385 ) ) ;
#183244 = EDGE_LOOP ( 'NONE', ( #168018, #251165, #119652, #244929 ) ) ;
#183245 = CARTESIAN_POINT ( 'NONE',  ( 20.94999999999999929, 76.00000000001190870, -103.0231074845243029 ) ) ;
#183246 = ORIENTED_EDGE ( 'NONE', *, *, #122007, .F. ) ;
#183247 = EDGE_CURVE ( 'NONE', #108747, #4968, #148482, .T. ) ;
#183248 = CARTESIAN_POINT ( 'NONE',  ( 22.39999999999999503, 7.790779598384535376, -100.4000000000000341 ) ) ;
#183249 = CARTESIAN_POINT ( 'NONE',  ( -18.41431012584568805, 64.51252797080434220, -179.2498714714227503 ) ) ;
#183250 = ORIENTED_EDGE ( 'NONE', *, *, #183127, .F. ) ;
#183252 = ORIENTED_EDGE ( 'NONE', *, *, #25384, .F. ) ;
#183251 = CARTESIAN_POINT ( 'NONE',  ( -23.15000000000000213, 85.60000000001159037, -59.62913836187181005 ) ) ;
#183253 = CARTESIAN_POINT ( 'NONE',  ( 23.14999999999999503, 42.98415524044398950, -233.9519173640447889 ) ) ;
#183254 = ORIENTED_EDGE ( 'NONE', *, *, #228993, .F. ) ;
#183255 = CARTESIAN_POINT ( 'NONE',  ( -20.94999999999999929, 77.83534155023599510, -57.96795619196132776 ) ) ;
#183256 = FACE_OUTER_BOUND ( 'NONE', #172257, .T. ) ;
#183258 = EDGE_CURVE ( 'NONE', #112749, #5367, #239944, .T. ) ;
#183257 = ORIENTED_EDGE ( 'NONE', *, *, #134131, .T. ) ;
#183259 = ORIENTED_EDGE ( 'NONE', *, *, #252443, .T. ) ;
#183260 = AXIS2_PLACEMENT_3D ( 'NONE', #132145, #13494, #112591 ) ;
#183262 = CIRCLE ( 'NONE', #195757, 0.09999999999999990841 ) ;
#183261 = CARTESIAN_POINT ( 'NONE',  ( -18.59999999999999787, 77.83585931145526615, -58.01866831572577610 ) ) ;
#183263 = CIRCLE ( 'NONE', #58331, 0.1000000000000002554 ) ;
#183265 = CYLINDRICAL_SURFACE ( 'NONE', #103166, 0.1000000000000075273 ) ;
#183264 = AXIS2_PLACEMENT_3D ( 'NONE', #4695, #219912, #225024 ) ;
#183266 = ORIENTED_EDGE ( 'NONE', *, *, #69166, .T. ) ;
#183267 = VERTEX_POINT ( 'NONE', #130181 ) ;
#183268 = VECTOR ( 'NONE', #83301, 1000.000000000000000 ) ;
#183270 = VERTEX_POINT ( 'NONE', #190182 ) ;
#183269 = DIRECTION ( 'NONE',  ( -1.000000000000000000, 0.000000000000000000, 3.469446951953635015E-14 ) ) ;
#183271 = CARTESIAN_POINT ( 'NONE',  ( -33.72168855820452649, 11.47316190337362940, -158.2500000000000284 ) ) ;
#183272 = AXIS2_PLACEMENT_3D ( 'NONE', #162555, #182106, #46423 ) ;
#183273 = DIRECTION ( 'NONE',  ( 1.000000000000000000, 0.000000000000000000, -0.000000000000000000 ) ) ;
#183274 = LINE ( 'NONE', #43759, #177725 ) ;
#183275 = CIRCLE ( 'NONE', #216595, 0.1000000000000028644 ) ;
#183277 = DIRECTION ( 'NONE',  ( 0.000000000000000000, 0.2128009952263485993, -0.9770955615653341697 ) ) ;
#183276 = CARTESIAN_POINT ( 'NONE',  ( -16.93909480342659890, 66.00692163521031830, -90.42276046785205779 ) ) ;
#183278 = CARTESIAN_POINT ( 'NONE',  ( 20.95595012432476523, 10.60417921308733469, -108.0957693302181895 ) ) ;
#183279 = DIRECTION ( 'NONE',  ( 0.000000000000000000, -0.2128009952263603677, 0.9770955615653313941 ) ) ;
#183280 = DIRECTION ( 'NONE',  ( 0.000000000000000000, 0.8814952561688430555, -0.4721928772777346239 ) ) ;
#183281 = CARTESIAN_POINT ( 'NONE',  ( -23.25000000000000000, 2.600000000011156054, -46.72462192276210402 ) ) ;
#183282 = VERTEX_POINT ( 'NONE', #11549 ) ;
#183283 = EDGE_CURVE ( 'NONE', #89895, #171481, #49382, .T. ) ;
#183284 = ADVANCED_FACE ( 'NONE', ( #208473 ), #79588, .F. ) ;
#183285 = ORIENTED_EDGE ( 'NONE', *, *, #85878, .F. ) ;
#183286 = DIRECTION ( 'NONE',  ( 1.000000000000000000, 0.000000000000000000, 0.000000000000000000 ) ) ;
#183287 = ORIENTED_EDGE ( 'NONE', *, *, #5826, .F. ) ;
#183288 = EDGE_CURVE ( 'NONE', #177211, #235019, #146231, .T. ) ;
#183289 = EDGE_CURVE ( 'NONE', #163426, #105990, #29756, .T. ) ;
#183290 = DIRECTION ( 'NONE',  ( 0.000000000000000000, 0.000000000000000000, -1.000000000000000000 ) ) ;
#183291 = ORIENTED_EDGE ( 'NONE', *, *, #27775, .F. ) ;
#183292 = EDGE_CURVE ( 'NONE', #71259, #206012, #33866, .T. ) ;
#183293 = DIRECTION ( 'NONE',  ( 1.000000000000000000, 0.000000000000000000, 0.000000000000000000 ) ) ;
#183294 = AXIS2_PLACEMENT_3D ( 'NONE', #86909, #166502, #226418 ) ;
#183295 = ADVANCED_FACE ( 'NONE', ( #147188 ), #151055, .T. ) ;
#183296 = ORIENTED_EDGE ( 'NONE', *, *, #117001, .F. ) ;
#183297 = CARTESIAN_POINT ( 'NONE',  ( -21.14999999999999858, 87.75000000001193712, -103.0231074845242318 ) ) ;
#183298 = ORIENTED_EDGE ( 'NONE', *, *, #202908, .F. ) ;
#183299 = EDGE_CURVE ( 'NONE', #242093, #39515, #246205, .T. ) ;
#183300 = ORIENTED_EDGE ( 'NONE', *, *, #150187, .F. ) ;
#183301 = DIRECTION ( 'NONE',  ( -1.000000000000000000, 0.000000000000000000, 0.000000000000000000 ) ) ;
#183302 = DIRECTION ( 'NONE',  ( 0.000000000000000000, -1.000000000000000000, 0.000000000000000000 ) ) ;
#183304 = EDGE_LOOP ( 'NONE', ( #193262, #163006 ) ) ;
#183303 = DIRECTION ( 'NONE',  ( 0.000000000000000000, -0.1298341882520079038, -0.9915357197604846018 ) ) ;
#183305 = ADVANCED_FACE ( 'NONE', ( #70258 ), #191488, .T. ) ;
#183306 = VECTOR ( 'NONE', #5306, 1000.000000000000000 ) ;
#183307 = CARTESIAN_POINT ( 'NONE',  ( 20.87600722750343252, 65.66887361445333227, -97.43298459182690863 ) ) ;
#183309 = ORIENTED_EDGE ( 'NONE', *, *, #96776, .T. ) ;
#183308 = FACE_OUTER_BOUND ( 'NONE', #121607, .T. ) ;
#183310 = LINE ( 'NONE', #2081, #233383 ) ;
#183311 = ORIENTED_EDGE ( 'NONE', *, *, #216556, .T. ) ;
#183312 = DIRECTION ( 'NONE',  ( -0.000000000000000000, 1.000000000000000000, 0.000000000000000000 ) ) ;
#183314 = ORIENTED_EDGE ( 'NONE', *, *, #169214, .F. ) ;
#183313 = DIRECTION ( 'NONE',  ( 0.000000000000000000, 1.000000000000000000, 0.000000000000000000 ) ) ;
#183315 = DIRECTION ( 'NONE',  ( -0.000000000000000000, -0.000000000000000000, -1.000000000000000000 ) ) ;
#183317 = EDGE_CURVE ( 'NONE', #94180, #172403, #254703, .T. ) ;
#183316 = CARTESIAN_POINT ( 'NONE',  ( -21.14999999999999858, 64.25000000001165290, -69.42310748452440805 ) ) ;
#183318 = CARTESIAN_POINT ( 'NONE',  ( -16.97048326478264713, 9.950000000011137047, -113.6411068801271966 ) ) ;
#183319 = EDGE_LOOP ( 'NONE', ( #167183, #12595, #186665, #130676 ) ) ;
#183321 = CARTESIAN_POINT ( 'NONE',  ( 23.14999999999999858, 72.00000000001190870, -103.0231074845243313 ) ) ;
#183320 = CARTESIAN_POINT ( 'NONE',  ( -23.15000000000000213, 11.65000000000000036, -12.14999999999999858 ) ) ;
#183322 = CARTESIAN_POINT ( 'NONE',  ( -18.39999999999999858, -9.499999999988849808, -73.60018939122203108 ) ) ;
#183323 = EDGE_CURVE ( 'NONE', #36199, #222722, #213050, .T. ) ;
#183324 = EDGE_CURVE ( 'NONE', #204466, #39339, #146398, .T. ) ;
#183325 = TOROIDAL_SURFACE ( 'NONE', #229114, 0.4000000000000012990, 0.1000000000000000056 ) ;
#183326 = DIRECTION ( 'NONE',  ( -0.000000000000000000, -0.000000000000000000, 1.000000000000000000 ) ) ;
#183327 = LINE ( 'NONE', #248433, #59959 ) ;
#183328 = CYLINDRICAL_SURFACE ( 'NONE', #246806, 0.1000000000000028644 ) ;
#183329 = TOROIDAL_SURFACE ( 'NONE', #33336, 0.9750000000000019762, 0.1000000000000000056 ) ;
#183330 = ORIENTED_EDGE ( 'NONE', *, *, #220280, .F. ) ;
#183331 = EDGE_LOOP ( 'NONE', ( #182177, #64140, #210241, #221166 ) ) ;
#183332 = ORIENTED_EDGE ( 'NONE', *, *, #46958, .F. ) ;
#183333 = EDGE_CURVE ( 'NONE', #84692, #33602, #34041, .T. ) ;
#183334 = CARTESIAN_POINT ( 'NONE',  ( -21.65000000000000213, 68.29142135624952914, -148.7731074845244166 ) ) ;
#183335 = ORIENTED_EDGE ( 'NONE', *, *, #39002, .T. ) ;
#183337 = DIRECTION ( 'NONE',  ( 1.000000000000000000, -7.510212038922846022E-17, 1.676432719286211941E-16 ) ) ;
#183336 = VECTOR ( 'NONE', #124375, 1000.000000000000227 ) ;
#183338 = ORIENTED_EDGE ( 'NONE', *, *, #225967, .F. ) ;
#183339 = DIRECTION ( 'NONE',  ( -0.000000000000000000, 0.9770955615653313941, 0.2128009952263603677 ) ) ;
#183340 = FILL_AREA_STYLE ('',( #103763 ) ) ;
#183341 = EDGE_CURVE ( 'NONE', #26422, #151535, #196518, .T. ) ;
#183342 = ADVANCED_FACE ( 'NONE', ( #5915 ), #64621, .F. ) ;
#183343 = CIRCLE ( 'NONE', #208284, 0.1000000000000018374 ) ;
#183344 = AXIS2_PLACEMENT_3D ( 'NONE', #225454, #8997, #88505 ) ;
#183345 = ORIENTED_EDGE ( 'NONE', *, *, #213656, .T. ) ;
#183346 = FACE_OUTER_BOUND ( 'NONE', #101175, .T. ) ;
#183348 = VERTEX_POINT ( 'NONE', #244539 ) ;
#183347 = CIRCLE ( 'NONE', #249979, 2.000000000000001776 ) ;
#183349 = VERTEX_POINT ( 'NONE', #65916 ) ;
#183350 = AXIS2_PLACEMENT_3D ( 'NONE', #47172, #58068, #201132 ) ;
#183351 = CIRCLE ( 'NONE', #220760, 1.749999999999999778 ) ;
#183352 = ORIENTED_EDGE ( 'NONE', *, *, #160692, .F. ) ;
#183353 = VECTOR ( 'NONE', #86436, 1000.000000000000000 ) ;
#183354 = AXIS2_PLACEMENT_3D ( 'NONE', #217957, #39382, #139711 ) ;
#183355 = DIRECTION ( 'NONE',  ( -1.000000000000000000, 3.448943450116721596E-16, 6.438528483529608630E-16 ) ) ;
#183356 = CARTESIAN_POINT ( 'NONE',  ( -16.87683809663752399, 66.05000000001207638, -123.8731074845243683 ) ) ;
#183357 = CARTESIAN_POINT ( 'NONE',  ( 17.74533788810829904, 10.81849979148194763, -157.1863773250524616 ) ) ;
#183358 = CARTESIAN_POINT ( 'NONE',  ( 15.66039659514495064, 26.81162386565848621, -233.6570620184931215 ) ) ;
#183359 = FACE_OUTER_BOUND ( 'NONE', #256278, .T. ) ;
#183360 = FACE_OUTER_BOUND ( 'NONE', #118670, .T. ) ;
#183362 = DIRECTION ( 'NONE',  ( 0.000000000000000000, -0.8814952561688430555, 0.4721928772777346239 ) ) ;
#183361 = DIRECTION ( 'NONE',  ( -1.000000000000000000, 0.000000000000000000, 0.000000000000000000 ) ) ;
#183363 = CARTESIAN_POINT ( 'NONE',  ( -21.05000000000000071, 76.00000000001142553, -36.02310748452432421 ) ) ;
#183365 = ORIENTED_EDGE ( 'NONE', *, *, #66843, .F. ) ;
#183364 = DIRECTION ( 'NONE',  ( 1.000000000000000000, -0.000000000000000000, -0.000000000000000000 ) ) ;
#183367 = CARTESIAN_POINT ( 'NONE',  ( 21.08884785362045378, 69.64280663258671211, -103.0728905795912027 ) ) ;
#183366 = DIRECTION ( 'NONE',  ( -1.000000000000000000, 0.000000000000000000, -0.000000000000000000 ) ) ;
#183368 = DIRECTION ( 'NONE',  ( -5.603264701231743991E-32, 1.897661533703520143E-16, -1.000000000000000000 ) ) ;
#183369 = VERTEX_POINT ( 'NONE', #26819 ) ;
#183370 = CARTESIAN_POINT ( 'NONE',  ( -21.14999999999999858, 57.66663670110953888, -226.2321832927624712 ) ) ;
#183371 = CARTESIAN_POINT ( 'NONE',  ( 21.56666275994540172, 76.00000000001271871, -210.4804758914176830 ) ) ;
#183372 = DIRECTION ( 'NONE',  ( 0.000000000000000000, 0.03181660087583048496, -0.9994937237965570986 ) ) ;
#183373 = ORIENTED_EDGE ( 'NONE', *, *, #229993, .F. ) ;
#183374 = AXIS2_PLACEMENT_3D ( 'NONE', #159542, #9128, #6545 ) ;
#183375 = DIRECTION ( 'NONE',  ( -0.000000000000000000, 6.982962677686266711E-15, -1.000000000000000000 ) ) ;
#183376 = CARTESIAN_POINT ( 'NONE',  ( -18.40000000000000213, 64.52683809665012404, -190.8731074845244393 ) ) ;
#183377 = EDGE_LOOP ( 'NONE', ( #61706, #170193, #51607, #226434, #99712 ) ) ;
#183378 = ORIENTED_EDGE ( 'NONE', *, *, #221293, .F. ) ;
#183379 = DIRECTION ( 'NONE',  ( 1.000000000000000000, 8.153259210133937167E-16, 2.158126701439427224E-16 ) ) ;
#183380 = VERTEX_POINT ( 'NONE', #42490 ) ;
#183381 = CARTESIAN_POINT ( 'NONE',  ( -23.25000000000000000, 77.85161776048073534, -91.41991776492061206 ) ) ;
#183382 = DIRECTION ( 'NONE',  ( 0.000000000000000000, -0.1350103645451876666, -0.9908441862701600211 ) ) ;
#183383 = DIRECTION ( 'NONE',  ( -1.020425574104004196E-15, -1.210927747993693964E-31, -1.000000000000000000 ) ) ;
#183384 = CARTESIAN_POINT ( 'NONE',  ( -23.49999999999994316, 79.88763423575340994, -7.282924647898262549 ) ) ;
#183385 = VERTEX_POINT ( 'NONE', #183297 ) ;
#183386 = AXIS2_PLACEMENT_3D ( 'NONE', #138585, #1662, #181616 ) ;
#183387 = DIRECTION ( 'NONE',  ( 0.000000000000000000, -0.9126074666063660468, -0.4088369013363524762 ) ) ;
#183388 = ADVANCED_FACE ( 'NONE', ( #122039 ), #138029, .T. ) ;
#183389 = CARTESIAN_POINT ( 'NONE',  ( 15.48841904831874849, 67.43841904833101353, -149.1731074845244223 ) ) ;
#183390 = VECTOR ( 'NONE', #223962, 1000.000000000000000 ) ;
#183391 = CARTESIAN_POINT ( 'NONE',  ( 23.14999999999999858, 70.60134440767089359, -223.4290147181903023 ) ) ;
#183392 = DIRECTION ( 'NONE',  ( 1.000000000000000000, 0.000000000000000000, 0.000000000000000000 ) ) ;
#183393 = EDGE_CURVE ( 'NONE', #233085, #66177, #223684, .T. ) ;
#183394 = AXIS2_PLACEMENT_3D ( 'NONE', #206648, #227480, #243192 ) ;
#183395 = ORIENTED_EDGE ( 'NONE', *, *, #157061, .T. ) ;
#183396 = ADVANCED_FACE ( 'NONE', ( #63329, #205407, #3347 ), #226239, .F. ) ;
#183398 = ORIENTED_EDGE ( 'NONE', *, *, #91630, .T. ) ;
#183397 = PLANE ( 'NONE',  #96160 ) ;
#183399 = ADVANCED_FACE ( 'NONE', ( #67198 ), #24241, .T. ) ;
#183400 = CARTESIAN_POINT ( 'NONE',  ( -23.25000000000000000, 1.115600667400684642E-11, -33.50000000000000000 ) ) ;
#183401 = CARTESIAN_POINT ( 'NONE',  ( 18.46947024752512334, 78.23781598975503471, -231.6011157545027856 ) ) ;
#183402 = DIRECTION ( 'NONE',  ( -3.469446951953604722E-14, -0.9999176327611370985, -0.01283462868040260302 ) ) ;
#183403 = FACE_OUTER_BOUND ( 'NONE', #103377, .T. ) ;
#183404 = DIRECTION ( 'NONE',  ( 1.000000000000000000, 0.000000000000000000, 0.000000000000000000 ) ) ;
#183405 = CYLINDRICAL_SURFACE ( 'NONE', #94715, 0.09999999999999939493 ) ;
#183406 = ORIENTED_EDGE ( 'NONE', *, *, #180932, .T. ) ;
#183407 = CARTESIAN_POINT ( 'NONE',  ( -16.92778301347321346, 63.05711598624363745, -213.0385060362119702 ) ) ;
#183408 = AXIS2_PLACEMENT_3D ( 'NONE', #223355, #176887, #58172 ) ;
#183409 = CARTESIAN_POINT ( 'NONE',  ( -16.79184697841823848, 9.948761661669548673, -146.6541422706025628 ) ) ;
#183410 = CARTESIAN_POINT ( 'NONE',  ( -21.05000000000000071, 77.83534155023627932, -91.46795619196132066 ) ) ;
#183412 = AXIS2_PLACEMENT_3D ( 'NONE', #235930, #76856, #97683 ) ;
#183411 = CARTESIAN_POINT ( 'NONE',  ( -20.94999999999999929, 7.021664781911246322, -204.8335654018972605 ) ) ;
#183413 = FACE_OUTER_BOUND ( 'NONE', #125077, .T. ) ;
#183414 = CIRCLE ( 'NONE', #158487, 0.09999999999999864553 ) ;
#183415 = EDGE_CURVE ( 'NONE', #76541, #28264, #144143, .T. ) ;
#183416 = VERTEX_POINT ( 'NONE', #45064 ) ;
#183417 = VERTEX_POINT ( 'NONE', #84133 ) ;
#183418 = DIRECTION ( 'NONE',  ( 0.000000000000000000, 7.116814260417668513E-15, -1.000000000000000000 ) ) ;
#183419 = CARTESIAN_POINT ( 'NONE',  ( 20.94999999999999929, 77.83585931145600512, -158.5186683157258187 ) ) ;
#183420 = CARTESIAN_POINT ( 'NONE',  ( -21.04999999999999716, -9.599999999988844124, -174.5320693966996259 ) ) ;
#183421 = CARTESIAN_POINT ( 'NONE',  ( 11.60000000000006182, 66.35000000001119247, -18.42310748452479530 ) ) ;
#183422 =( BOUNDED_CURVE ( )  B_SPLINE_CURVE ( 3, ( #225299, #184913, #64957, #165356 ),
 .UNSPECIFIED., .F., .F. ) 
 B_SPLINE_CURVE_WITH_KNOTS ( ( 4, 4 ),
 ( 5.731445031868799056, 5.983100554402346560 ),
 .UNSPECIFIED. ) 
 CURVE ( )  GEOMETRIC_REPRESENTATION_ITEM ( )  RATIONAL_B_SPLINE_CURVE ( ( 1.000000000000000000, 0.9947294176030465618, 0.9947294176030465618, 1.000000000000000000 ) ) 
 REPRESENTATION_ITEM ( '' )  );
#183423 = ORIENTED_EDGE ( 'NONE', *, *, #60038, .T. ) ;
#183424 = LINE ( 'NONE', #247226, #118320 ) ;
#183425 = B_SPLINE_CURVE_WITH_KNOTS ( 'NONE', 3,
 ( #163240, #184068, #118979, #5401, #79812, #84932, #23750, #2848, #164525, #40750, #244035, #64129, #121570, #143655, #1568, #81103, #223186, #120289, #202352, #219337, #181527, #21182, #39466, #238918, #82371, #240210, #65404, #198497, #19882, #160695 ),
 .UNSPECIFIED., .F., .F.,
 ( 4, 2, 2, 2, 2, 2, 2, 2, 2, 2, 2, 2, 2, 2, 4 ),
 ( 0.000000000000000000, 0.0003422764154113552447, 0.0006845528308227104893, 0.001026829246234065842, 0.001369105661645420979, 0.002053658492468075740, 0.002738211323290730068, 0.003080487738702054629, 0.003422764154113380058, 0.003765040569524704620, 0.004107316984936030049, 0.004449593400347354177, 0.004791869815758679173, 0.005134146231170004168, 0.005476422646581329164 ),
 .UNSPECIFIED. ) ;
#183426 = DIRECTION ( 'NONE',  ( 1.000000000000000000, 5.945622153099073960E-16, -5.981866248895712861E-16 ) ) ;
#183427 = DIRECTION ( 'NONE',  ( 1.000000000000000000, 0.000000000000000000, 0.000000000000000000 ) ) ;
#183428 = EDGE_CURVE ( 'NONE', #191176, #163267, #204675, .T. ) ;
#183429 = AXIS2_PLACEMENT_3D ( 'NONE', #238124, #240709, #241984 ) ;
#183430 = AXIS2_PLACEMENT_3D ( 'NONE', #20951, #154063, #19646 ) ;
#183431 = CARTESIAN_POINT ( 'NONE',  ( -16.89268316805466341, 9.951721813242185632, -12.64424752145445296 ) ) ;
#183432 = EDGE_CURVE ( 'NONE', #104106, #52101, #187168, .T. ) ;
#183433 = EDGE_LOOP ( 'NONE', ( #46934, #214804, #145671, #138235 ) ) ;
#183434 = DIRECTION ( 'NONE',  ( 0.000000000000000000, -0.1686199900910312910, 0.9856811345164826488 ) ) ;
#183435 = ORIENTED_EDGE ( 'NONE', *, *, #3449, .F. ) ;
#183436 = CARTESIAN_POINT ( 'NONE',  ( 21.05000000000000071, 1.115600667400684642E-11, -33.50000000000000000 ) ) ;
#183437 = CYLINDRICAL_SURFACE ( 'NONE', #245617, 0.09999999999999609201 ) ;
#183438 = CARTESIAN_POINT ( 'NONE',  ( -21.04999999999958149, 10.11179281909484828, -228.1329080630113140 ) ) ;
#183439 = EDGE_CURVE ( 'NONE', #158005, #74064, #104991, .T. ) ;
#183440 = DIRECTION ( 'NONE',  ( -2.827886303505248766E-16, 0.8660254037844411501, 0.4999999999999956146 ) ) ;
#183441 = LINE ( 'NONE', #144273, #165399 ) ;
#183442 = CARTESIAN_POINT ( 'NONE',  ( -18.40000000000000213, 64.51332499825382172, -45.27310748452440947 ) ) ;
#183443 = CARTESIAN_POINT ( 'NONE',  ( -18.46093223321774701, -9.480682968274523503, -7.084550513926728854 ) ) ;
#183444 = CARTESIAN_POINT ( 'NONE',  ( -18.47140463609786920, -9.671474685209730637, -107.1727604582741407 ) ) ;
#183445 = ADVANCED_FACE ( 'NONE', ( #247103 ), #196482, .F. ) ;
#183446 = DIRECTION ( 'NONE',  ( 0.000000000000000000, 0.000000000000000000, 1.000000000000000000 ) ) ;
#183447 = VECTOR ( 'NONE', #9963, 1000.000000000000000 ) ;
#183448 = DIRECTION ( 'NONE',  ( 0.000000000000000000, 0.000000000000000000, -1.000000000000000000 ) ) ;
#183449 = AXIS2_PLACEMENT_3D ( 'NONE', #60177, #141023, #219253 ) ;
#183450 = DIRECTION ( 'NONE',  ( 1.000000000000000000, 0.000000000000000000, 0.000000000000000000 ) ) ;
#183451 = CARTESIAN_POINT ( 'NONE',  ( 18.42636655943171320, -9.496944315770630141, -40.10908057115552339 ) ) ;
#183452 = AXIS2_PLACEMENT_3D ( 'NONE', #35853, #134901, #192344 ) ;
#183453 = EDGE_CURVE ( 'NONE', #74763, #243465, #63194, .T. ) ;
#183454 = CYLINDRICAL_SURFACE ( 'NONE', #33039, 0.5000000000000004441 ) ;
#183455 = CIRCLE ( 'NONE', #79376, 0.09999999999999766020 ) ;
#183456 = ORIENTED_EDGE ( 'NONE', *, *, #106259, .T. ) ;
#183457 = CARTESIAN_POINT ( 'NONE',  ( 18.46905048506370406, 85.47374425739451453, -129.8471211922688724 ) ) ;
#183458 = CARTESIAN_POINT ( 'NONE',  ( -20.54999999999999716, 1.925233644870972816, -79.73024353312617052 ) ) ;
#183459 = ADVANCED_FACE ( 'NONE', ( #53682 ), #91531, .F. ) ;
#183460 = VERTEX_POINT ( 'NONE', #155388 ) ;
#183461 = DIRECTION ( 'NONE',  ( 0.000000000000000000, 1.000000000000000000, -6.308085367188393199E-16 ) ) ;
#183462 = CARTESIAN_POINT ( 'NONE',  ( 21.05995757104869881, 67.22461075529101038, -157.8282023615332150 ) ) ;
#183463 = AXIS2_PLACEMENT_3D ( 'NONE', #182767, #161928, #43248 ) ;
#183464 = CARTESIAN_POINT ( 'NONE',  ( -21.05000000000000071, 69.60000000001187459, -93.09268285446279378 ) ) ;
#183465 = EDGE_CURVE ( 'NONE', #145746, #114547, #112386, .T. ) ;
#183466 = ORIENTED_EDGE ( 'NONE', *, *, #126646, .T. ) ;
#183467 = FACE_OUTER_BOUND ( 'NONE', #105329, .T. ) ;
#183468 = CARTESIAN_POINT ( 'NONE',  ( 23.14999999999999503, 11.65000000001116298, -146.1500000000000341 ) ) ;
#183469 = ORIENTED_EDGE ( 'NONE', *, *, #186282, .F. ) ;
#183470 = ORIENTED_EDGE ( 'NONE', *, *, #71525, .T. ) ;
#183471 = CARTESIAN_POINT ( 'NONE',  ( 20.90000000000000213, 11.59795743183152972, -1.899104650876408451 ) ) ;
#183472 = ORIENTED_EDGE ( 'NONE', *, *, #213954, .F. ) ;
#183473 = DIRECTION ( 'NONE',  ( -1.000000000000000000, 0.000000000000000000, 0.000000000000000000 ) ) ;
#183474 = VECTOR ( 'NONE', #119282, 1000.000000000000114 ) ;
#183475 = CARTESIAN_POINT ( 'NONE',  ( 22.59999954896768770, -0.008828232233014684030, -21.74949132593200574 ) ) ;
#183476 = CARTESIAN_POINT ( 'NONE',  ( 20.94999999999999929, 5.000000000011153745, -188.5947339810868755 ) ) ;
#183478 = CYLINDRICAL_SURFACE ( 'NONE', #86806, 0.09999999999999530098 ) ;
#183477 = PRODUCT_DEFINITION_CONTEXT ( 'detailed design', #247326, 'design' ) ;
#183479 = DIRECTION ( 'NONE',  ( 0.000000000000000000, 0.000000000000000000, -1.000000000000000000 ) ) ;
#183480 = LINE ( 'NONE', #84309, #164282 ) ;
#183481 = DIRECTION ( 'NONE',  ( 1.000000000000000000, 0.000000000000000000, 0.000000000000000000 ) ) ;
#183482 = AXIS2_PLACEMENT_3D ( 'NONE', #169003, #223781, #248497 ) ;
#183483 = DIRECTION ( 'NONE',  ( 0.000000000000000000, 0.000000000000000000, -1.000000000000000000 ) ) ;
#183485 = ORIENTED_EDGE ( 'NONE', *, *, #169830, .F. ) ;
#183484 = CARTESIAN_POINT ( 'NONE',  ( -18.52186455168988388, -9.481018481431377154, -40.52501647791446970 ) ) ;
#183486 = ORIENTED_EDGE ( 'NONE', *, *, #179161, .F. ) ;
#183488 = DIRECTION ( 'NONE',  ( 0.000000000000000000, 0.000000000000000000, 1.000000000000000000 ) ) ;
#183487 = CARTESIAN_POINT ( 'NONE',  ( 20.85000000000000142, 68.97833521811203639, -132.6895420826271277 ) ) ;
#183490 = VERTEX_POINT ( 'NONE', #71975 ) ;
#183489 = CARTESIAN_POINT ( 'NONE',  ( -16.77308656112213825, 60.93940833456625938, -221.0415412795326233 ) ) ;
#183491 = AXIS2_PLACEMENT_3D ( 'NONE', #5783, #82738, #163609 ) ;
#183492 = ORIENTED_EDGE ( 'NONE', *, *, #4276, .F. ) ;
#183493 = DIRECTION ( 'NONE',  ( 0.000000000000000000, 0.000000000000000000, -1.000000000000000000 ) ) ;
#183494 = CARTESIAN_POINT ( 'NONE',  ( 20.77766267348356166, 10.44904239062959839, -175.0927089158778074 ) ) ;
#183495 = DIRECTION ( 'NONE',  ( 1.000000000000000000, 0.000000000000000000, 0.000000000000000000 ) ) ;
#183496 = AXIS2_PLACEMENT_3D ( 'NONE', #22702, #222126, #86469 ) ;
#183497 = DIRECTION ( 'NONE',  ( 0.000000000000000000, 0.000000000000000000, 1.000000000000000000 ) ) ;
#183498 = CARTESIAN_POINT ( 'NONE',  ( -20.85000000000000142, 11.75000000001115197, -93.71613433702194129 ) ) ;
#183499 = DIRECTION ( 'NONE',  ( 0.000000000000000000, 0.000000000000000000, 1.000000000000000000 ) ) ;
#183500 = ORIENTED_EDGE ( 'NONE', *, *, #28609, .T. ) ;
#183501 = ORIENTED_EDGE ( 'NONE', *, *, #243629, .F. ) ;
#183502 = CARTESIAN_POINT ( 'NONE',  ( 20.94999999999999929, 76.00000000001190870, -103.0231074845243029 ) ) ;
#183503 = AXIS2_PLACEMENT_3D ( 'NONE', #186016, #200450, #102591 ) ;
#183504 = VERTEX_POINT ( 'NONE', #151529 ) ;
#183505 = CARTESIAN_POINT ( 'NONE',  ( 22.59080734064468743, 64.25000000001237765, -170.0538571926215070 ) ) ;
#183507 = ORIENTED_EDGE ( 'NONE', *, *, #117599, .T. ) ;
#183506 = CIRCLE ( 'NONE', #200075, 0.2000000000000057288 ) ;
#183508 = CARTESIAN_POINT ( 'NONE',  ( -16.77683809663752257, 9.945835743215303282, -154.8360509808958057 ) ) ;
#183509 = AXIS2_PLACEMENT_3D ( 'NONE', #72210, #172630, #93037 ) ;
#183510 = AXIS2_PLACEMENT_3D ( 'NONE', #28859, #110909, #208745 ) ;
#183511 = CARTESIAN_POINT ( 'NONE',  ( -22.39999999999999858, 76.00000000001170974, -77.31388708289772183 ) ) ;
#183512 = EDGE_CURVE ( 'NONE', #203844, #41248, #54828, .T. ) ;
#183513 = DIRECTION ( 'NONE',  ( 0.000000000000000000, 0.000000000000000000, -1.000000000000000000 ) ) ;
#183514 = CYLINDRICAL_SURFACE ( 'NONE', #220611, 4.049999999999998046 ) ;
#183515 = ORIENTED_EDGE ( 'NONE', *, *, #65728, .T. ) ;
#183516 = AXIS2_PLACEMENT_3D ( 'NONE', #188197, #186937, #89080 ) ;
#183518 = AXIS2_PLACEMENT_3D ( 'NONE', #237032, #242153, #23140 ) ;
#183517 = FACE_OUTER_BOUND ( 'NONE', #242414, .T. ) ;
#183519 = ORIENTED_EDGE ( 'NONE', *, *, #113065, .F. ) ;
#183520 = ADVANCED_FACE ( 'NONE', ( #171115 ), #17422, .T. ) ;
#183521 = CARTESIAN_POINT ( 'NONE',  ( 22.42196299218230493, 0.002441673998456600492, -122.3503882973505483 ) ) ;
#183522 = EDGE_CURVE ( 'NONE', #47428, #102195, #237985, .T. ) ;
#183523 = DIRECTION ( 'NONE',  ( -1.073024830501117725E-15, 0.2617529984165031243, 0.9651348961777157509 ) ) ;
#183524 = CARTESIAN_POINT ( 'NONE',  ( -21.29999999999995808, 76.00000000001192291, -98.97310748452431994 ) ) ;
#183525 = PLANE ( 'NONE',  #115728 ) ;
#183526 = ORIENTED_EDGE ( 'NONE', *, *, #69283, .T. ) ;
#183527 = CARTESIAN_POINT ( 'NONE',  ( -21.05000000000000071, 1.851028230152016674, -112.1539132694225316 ) ) ;
#183528 = ORIENTED_EDGE ( 'NONE', *, *, #5749, .T. ) ;
#183531 = VERTEX_POINT ( 'NONE', #231062 ) ;
#183530 = CARTESIAN_POINT ( 'NONE',  ( -23.15000000000000213, 87.65000000001144542, -39.12310748452424747 ) ) ;
#183529 = CARTESIAN_POINT ( 'NONE',  ( -18.59999999999999787, 11.65000000001115232, -74.01480577065404987 ) ) ;
#183532 = AXIS2_PLACEMENT_3D ( 'NONE', #104146, #183715, #5034 ) ;
#183533 = DIRECTION ( 'NONE',  ( 0.000000000000000000, 1.000000000000000000, 0.000000000000000000 ) ) ;
#183534 = CIRCLE ( 'NONE', #117078, 0.1000000000000024342 ) ;
#183536 = EDGE_LOOP ( 'NONE', ( #42143, #77004, #66188, #95245 ) ) ;
#183535 = CONICAL_SURFACE ( 'NONE', #83542, 4.299999999999956302, 0.7853981633974466137 ) ;
#183537 = AXIS2_PLACEMENT_3D ( 'NONE', #186249, #242355, #46713 ) ;
#183538 = CIRCLE ( 'NONE', #100303, 0.1000000000000028644 ) ;
#183539 = DIRECTION ( 'NONE',  ( 0.000000000000000000, 0.000000000000000000, -1.000000000000000000 ) ) ;
#183540 = ORIENTED_EDGE ( 'NONE', *, *, #61729, .F. ) ;
#183541 = FACE_OUTER_BOUND ( 'NONE', #224250, .T. ) ;
#183542 = ADVANCED_FACE ( 'NONE', ( #129369 ), #113653, .F. ) ;
#183543 = CARTESIAN_POINT ( 'NONE',  ( -20.94999999999999929, 5.850000000011160495, -123.8675027757221017 ) ) ;
#183544 = CARTESIAN_POINT ( 'NONE',  ( 20.94999999999999929, -11.48912529306489994, -130.9000000000000341 ) ) ;
#183545 = CARTESIAN_POINT ( 'NONE',  ( -18.52139480978222608, 8.843916517143410871, -245.4074197334283838 ) ) ;
#183546 = DIRECTION ( 'NONE',  ( -1.000000000000000000, -9.012599976027990443E-15, -6.882867235861669241E-14 ) ) ;
#183547 = CIRCLE ( 'NONE', #125292, 0.1000000000000014488 ) ;
#183548 = ORIENTED_EDGE ( 'NONE', *, *, #92950, .F. ) ;
#183549 = DIRECTION ( 'NONE',  ( 0.000000000000000000, 0.000000000000000000, -1.000000000000000000 ) ) ;
#183550 = CARTESIAN_POINT ( 'NONE',  ( 21.05000000000000071, 5.400000000011154988, -88.09473398108696074 ) ) ;
#183551 = CARTESIAN_POINT ( 'NONE',  ( -13.88555196119804869, 66.54256847116334939, -155.0231905466248179 ) ) ;
#183552 = ORIENTED_EDGE ( 'NONE', *, *, #177271, .T. ) ;
#183553 = CARTESIAN_POINT ( 'NONE',  ( 5.900000000000059863, 64.25000000001119815, -26.12310748452479103 ) ) ;
#183554 = VERTEX_POINT ( 'NONE', #249333 ) ;
#183555 = DIRECTION ( 'NONE',  ( -0.000000000000000000, -0.000000000000000000, -1.000000000000000000 ) ) ;
#183556 = EDGE_CURVE ( 'NONE', #2313, #224490, #14585, .T. ) ;
#183557 = LINE ( 'NONE', #188680, #39241 ) ;
#183558 = CARTESIAN_POINT ( 'NONE',  ( 20.95000000000002416, 36.22724532936084074, -235.9903003947922002 ) ) ;
#183559 = ADVANCED_FACE ( 'NONE', ( #70711 ), #31588, .F. ) ;
#183561 = ORIENTED_EDGE ( 'NONE', *, *, #122929, .F. ) ;
#183560 = CARTESIAN_POINT ( 'NONE',  ( -16.89935556175728593, 44.58236401100771928, -235.0987338397486326 ) ) ;
#183562 = DIRECTION ( 'NONE',  ( 0.000000000000000000, 0.9770955615653312831, 0.2128009952263621163 ) ) ;
#183563 = VECTOR ( 'NONE', #9080, 1000.000000000000000 ) ;
#183564 = FACE_OUTER_BOUND ( 'NONE', #77125, .T. ) ;
#183565 = FACE_OUTER_BOUND ( 'NONE', #152710, .T. ) ;
#183567 = ADVANCED_FACE ( 'NONE', ( #212772 ), #15875, .F. ) ;
#183566 = ORIENTED_EDGE ( 'NONE', *, *, #116570, .T. ) ;
#183568 = DIRECTION ( 'NONE',  ( 1.000000000000000000, 0.000000000000000000, 0.000000000000000000 ) ) ;
#183569 = CARTESIAN_POINT ( 'NONE',  ( -21.05000000000000071, 74.83729825007462466, -195.6231074845243540 ) ) ;
#183570 = VERTEX_POINT ( 'NONE', #111088 ) ;
#183571 = CARTESIAN_POINT ( 'NONE',  ( -23.15000000000000213, 1.115625160336667635E-11, -202.9999999999999716 ) ) ;
#183572 = AXIS2_PLACEMENT_3D ( 'NONE', #150535, #151838, #213060 ) ;
#183573 = ORIENTED_EDGE ( 'NONE', *, *, #195927, .T. ) ;
#183575 = DIRECTION ( 'NONE',  ( 1.000000000000000000, 0.000000000000000000, 0.000000000000000000 ) ) ;
#183574 = AXIS2_PLACEMENT_3D ( 'NONE', #72724, #136491, #53124 ) ;
#183577 = EDGE_LOOP ( 'NONE', ( #230131, #103054, #67105, #113896 ) ) ;
#183576 = CARTESIAN_POINT ( 'NONE',  ( -23.15000000000000213, 11.65000000001115588, -155.2500000000000284 ) ) ;
#183580 = EDGE_LOOP ( 'NONE', ( #80556, #110887, #5634, #245503 ) ) ;
#183579 = EDGE_LOOP ( 'NONE', ( #89745, #252844 ) ) ;
#183578 = DIRECTION ( 'NONE',  ( 1.000000000000000000, 0.000000000000000000, 0.000000000000000000 ) ) ;
#183581 = AXIS2_PLACEMENT_3D ( 'NONE', #206381, #246772, #29062 ) ;
#183582 = DIRECTION ( 'NONE',  ( -1.000000000000000000, -0.000000000000000000, -0.000000000000000000 ) ) ;
#183583 = PLANE ( 'NONE',  #189719 ) ;
#183584 = CARTESIAN_POINT ( 'NONE',  ( 21.05000000000000071, 76.00000000001165290, -69.52310748452431710 ) ) ;
#183586 = LINE ( 'NONE', #6212, #66993 ) ;
#183585 = CARTESIAN_POINT ( 'NONE',  ( 22.43288208788031568, 0.004899854896538679595, -88.85034815628095828 ) ) ;
#183587 = DIRECTION ( 'NONE',  ( 1.000000000000000000, -0.000000000000000000, -0.000000000000000000 ) ) ;
#183588 = AXIS2_PLACEMENT_3D ( 'NONE', #130104, #28491, #225339 ) ;
#183589 = DIRECTION ( 'NONE',  ( 0.000000000000000000, 6.982962677686266711E-15, -1.000000000000000000 ) ) ;
#183590 = AXIS2_PLACEMENT_3D ( 'NONE', #212209, #233062, #75277 ) ;
#183591 = CARTESIAN_POINT ( 'NONE',  ( 20.94999999999999574, 8.926614585098251453, -108.9716830192231498 ) ) ;
#183592 = CARTESIAN_POINT ( 'NONE',  ( -18.39999999999999858, -0.8254770802754705095, -242.3223161824233500 ) ) ;
#183593 = ORIENTED_EDGE ( 'NONE', *, *, #96245, .T. ) ;
#183594 = VERTEX_POINT ( 'NONE', #34160 ) ;
#183595 = EDGE_CURVE ( 'NONE', #236709, #249163, #134481, .T. ) ;
#183596 = EDGE_CURVE ( 'NONE', #214564, #145730, #154828, .T. ) ;
#183598 = ORIENTED_EDGE ( 'NONE', *, *, #135640, .F. ) ;
#183597 = CARTESIAN_POINT ( 'NONE',  ( -18.50000000000000000, 9.250000000011157297, -54.75000000000000000 ) ) ;
#183599 = ORIENTED_EDGE ( 'NONE', *, *, #232618, .T. ) ;
#183600 = CARTESIAN_POINT ( 'NONE',  ( 20.94999999999999574, -1.261786168553869603, -108.5864989635455089 ) ) ;
#183601 = VERTEX_POINT ( 'NONE', #234901 ) ;
#183602 = DIRECTION ( 'NONE',  ( -1.000000000000000000, -0.000000000000000000, -0.000000000000000000 ) ) ;
#183603 = EDGE_CURVE ( 'NONE', #45697, #20936, #42368, .T. ) ;
#183604 = EDGE_CURVE ( 'NONE', #90327, #56940, #172398, .T. ) ;
#183605 = ORIENTED_EDGE ( 'NONE', *, *, #114615, .T. ) ;
#183606 = CIRCLE ( 'NONE', #75309, 0.5000000000000004441 ) ;
#183607 = FACE_OUTER_BOUND ( 'NONE', #45404, .T. ) ;
#183608 = LINE ( 'NONE', #67498, #182131 ) ;
#183609 = EDGE_CURVE ( 'NONE', #234753, #257268, #188121, .T. ) ;
#183611 = ORIENTED_EDGE ( 'NONE', *, *, #70321, .F. ) ;
#183610 = ORIENTED_EDGE ( 'NONE', *, *, #219705, .F. ) ;
#183612 = VERTEX_POINT ( 'NONE', #219160 ) ;
#183615 = EDGE_CURVE ( 'NONE', #197543, #118259, #96512, .T. ) ;
#183614 = EDGE_CURVE ( 'NONE', #212703, #160183, #108996, .T. ) ;
#183613 = FACE_OUTER_BOUND ( 'NONE', #234924, .T. ) ;
#183616 = VERTEX_POINT ( 'NONE', #18406 ) ;
#183617 = ORIENTED_EDGE ( 'NONE', *, *, #230628, .T. ) ;
#183618 = CARTESIAN_POINT ( 'NONE',  ( -20.94999999999999929, 1.835341550235569663, -112.0551512925630249 ) ) ;
#183619 = CARTESIAN_POINT ( 'NONE',  ( 13.40000000000000036, -8.250000000000003553, 17.60000000000000497 ) ) ;
#183621 = ORIENTED_EDGE ( 'NONE', *, *, #39573, .T. ) ;
#183620 = DIRECTION ( 'NONE',  ( 0.000000000000000000, 0.000000000000000000, -1.000000000000000000 ) ) ;
#183622 = ADVANCED_FACE ( 'NONE', ( #118806 ), #121403, .T. ) ;
#183623 = DIRECTION ( 'NONE',  ( 1.000000000000000000, 0.000000000000000000, 0.000000000000000000 ) ) ;
#183624 = CARTESIAN_POINT ( 'NONE',  ( -22.39999999999999858, 0.1000000000111554016, -92.70922040162662370 ) ) ;
#183626 = EDGE_LOOP ( 'NONE', ( #147102, #10584, #64436, #158988 ) ) ;
#183625 = LINE ( 'NONE', #138055, #27869 ) ;
#183627 = ORIENTED_EDGE ( 'NONE', *, *, #17538, .F. ) ;
#183628 = DIRECTION ( 'NONE',  ( 0.000000000000000000, -0.2617529984165031243, -0.9651348961777157509 ) ) ;
#183629 = EDGE_LOOP ( 'NONE', ( #34235, #21536, #105797, #240163 ) ) ;
#183631 = CONICAL_SURFACE ( 'NONE', #200380, 6.250000000000005329, 0.7853981633974431720 ) ;
#183630 = CARTESIAN_POINT ( 'NONE',  ( 21.05000000000000071, 67.23127455305835554, -235.8551265064784559 ) ) ;
#183633 = ADVANCED_FACE ( 'NONE', ( #238741 ), #60088, .F. ) ;
#183632 = DIRECTION ( 'NONE',  ( 0.000000000000000000, -0.8814952561688429444, 0.4721928772777345684 ) ) ;
#183634 = AXIS2_PLACEMENT_3D ( 'NONE', #204819, #127877, #70501 ) ;
#183635 = AXIS2_PLACEMENT_3D ( 'NONE', #87838, #67018, #124435 ) ;
#183636 = AXIS2_PLACEMENT_3D ( 'NONE', #81050, #122791, #78488 ) ;
#183637 = ORIENTED_EDGE ( 'NONE', *, *, #180779, .F. ) ;
#183638 = CARTESIAN_POINT ( 'NONE',  ( 21.04999999999999716, 10.62872031401550466, -45.64999999999999858 ) ) ;
#183639 = EDGE_CURVE ( 'NONE', #130380, #170720, #250471, .T. ) ;
#183640 = EDGE_CURVE ( 'NONE', #56614, #241870, #161798, .T. ) ;
#183641 = DIRECTION ( 'NONE',  ( 0.7070776581708964059, -0.1850949428989398515, -0.6824815363281259151 ) ) ;
#183642 = CIRCLE ( 'NONE', #104493, 11.75000000000000000 ) ;
#183643 = CARTESIAN_POINT ( 'NONE',  ( 18.59999999999999076, 11.75000000001115907, -55.25000000000004974 ) ) ;
#183644 = VERTEX_POINT ( 'NONE', #2681 ) ;
#183645 = ORIENTED_EDGE ( 'NONE', *, *, #230443, .T. ) ;
#183646 = EDGE_CURVE ( 'NONE', #38095, #22582, #200895, .T. ) ;
#183647 = CARTESIAN_POINT ( 'NONE',  ( 22.39999999999999858, 7.790779598373383408, 0.09999999999999939493 ) ) ;
#183648 = FACE_OUTER_BOUND ( 'NONE', #112442, .T. ) ;
#183649 = ORIENTED_EDGE ( 'NONE', *, *, #210155, .F. ) ;
#183650 = CARTESIAN_POINT ( 'NONE',  ( 22.50000000000000000, -1.560176095955058129, -193.3663837337745122 ) ) ;
#183651 = ORIENTED_EDGE ( 'NONE', *, *, #92395, .T. ) ;
#183652 = DIRECTION ( 'NONE',  ( 1.000000000000000000, 0.000000000000000000, 0.000000000000000000 ) ) ;
#183653 = CARTESIAN_POINT ( 'NONE',  ( -18.50000000000000000, 76.00000000001126921, -203.5231074845248997 ) ) ;
#183655 = CARTESIAN_POINT ( 'NONE',  ( 20.94999999999999574, -11.64999999998883595, -103.6000000000000369 ) ) ;
#183654 = CARTESIAN_POINT ( 'NONE',  ( -15.75000000000000355, 66.65000000001155911, -52.77310748452439526 ) ) ;
#183656 = ADVANCED_FACE ( 'NONE', ( #140935 ), #77092, .T. ) ;
#183657 = CARTESIAN_POINT ( 'NONE',  ( 22.44352723754029810, 0.009277095054436620969, -55.35027865465133345 ) ) ;
#183658 = DIRECTION ( 'NONE',  ( 0.000000000000000000, 0.000000000000000000, 1.000000000000000000 ) ) ;
#183659 = EDGE_CURVE ( 'NONE', #217291, #79953, #184019, .T. ) ;
#183660 = ORIENTED_EDGE ( 'NONE', *, *, #17173, .T. ) ;
#183661 = CARTESIAN_POINT ( 'NONE',  ( 18.48413544395662100, -9.664304033616598844, -207.6831049930382562 ) ) ;
#183663 = ORIENTED_EDGE ( 'NONE', *, *, #7291, .F. ) ;
#183662 = ORIENTED_EDGE ( 'NONE', *, *, #244913, .F. ) ;
#183664 = ORIENTED_EDGE ( 'NONE', *, *, #1258, .T. ) ;
#183665 = ORIENTED_EDGE ( 'NONE', *, *, #29121, .F. ) ;
#183666 = CYLINDRICAL_SURFACE ( 'NONE', #33599, 0.09999999999999990841 ) ;
#183667 = CARTESIAN_POINT ( 'NONE',  ( -18.50000000000000000, 74.16465844978819177, -191.9679561919613775 ) ) ;
#183668 = CARTESIAN_POINT ( 'NONE',  ( -21.14999999999999858, -0.09999999998884338825, -122.3504291924552092 ) ) ;
#183669 = DIRECTION ( 'NONE',  ( 0.000000000000000000, -0.1350103645451904977, 0.9908441862701596881 ) ) ;
#183670 = EDGE_CURVE ( 'NONE', #154226, #169429, #237458, .T. ) ;
#183671 = CIRCLE ( 'NONE', #104517, 11.80000000000000426 ) ;
#183673 = CARTESIAN_POINT ( 'NONE',  ( -22.00411653889214136, 0.09903810579743195508, -160.2465571323594986 ) ) ;
#183672 = DIRECTION ( 'NONE',  ( 0.000000000000000000, 0.000000000000000000, 1.000000000000000000 ) ) ;
#183675 = ORIENTED_EDGE ( 'NONE', *, *, #185181, .T. ) ;
#183674 = CARTESIAN_POINT ( 'NONE',  ( 21.05000000000000071, 70.50000000001151079, -48.42837350343745584 ) ) ;
#183676 = CARTESIAN_POINT ( 'NONE',  ( -21.05000000000000071, 6.478078221105875834, -167.5999999353044529 ) ) ;
#183677 = EDGE_LOOP ( 'NONE', ( #150471, #194909, #195200, #12441, #219977, #175538, #99330, #222026, #71595, #18300, #92194, #180282, #48644, #244151 ) ) ;
#183678 = CARTESIAN_POINT ( 'NONE',  ( 21.05000000000005400, 86.36484105039212977, -51.23044614117323903 ) ) ;
#183679 = ORIENTED_EDGE ( 'NONE', *, *, #152429, .F. ) ;
#183680 = VERTEX_POINT ( 'NONE', #99205 ) ;
#183681 = DIRECTION ( 'NONE',  ( -0.000000000000000000, -0.000000000000000000, 1.000000000000000000 ) ) ;
#183682 = CIRCLE ( 'NONE', #8887, 0.2000000000000027867 ) ;
#183683 = DIRECTION ( 'NONE',  ( -1.000000000000000000, -0.000000000000000000, 0.000000000000000000 ) ) ;
#183684 = CARTESIAN_POINT ( 'NONE',  ( 18.59999999999999076, 6.550000000000000711, -21.25000000000000000 ) ) ;
#183685 = DIRECTION ( 'NONE',  ( 0.000000000000000000, 0.000000000000000000, 1.000000000000000000 ) ) ;
#183686 = AXIS2_PLACEMENT_3D ( 'NONE', #256579, #40183, #77984 ) ;
#183687 = CARTESIAN_POINT ( 'NONE',  ( 18.59999999999999076, 1.115600667400684642E-11, -134.0000000000000284 ) ) ;
#183688 = AXIS2_PLACEMENT_3D ( 'NONE', #176344, #193329, #159347 ) ;
#183689 = VERTEX_POINT ( 'NONE', #160516 ) ;
#183690 = ORIENTED_EDGE ( 'NONE', *, *, #16409, .F. ) ;
#183691 = DIRECTION ( 'NONE',  ( 0.000000000000000000, -0.000000000000000000, 1.000000000000000000 ) ) ;
#183692 = EDGE_LOOP ( 'NONE', ( #249491, #44580, #161043 ) ) ;
#183693 = CARTESIAN_POINT ( 'NONE',  ( -20.85000000000000497, 11.75000000001115019, -127.0808527540413166 ) ) ;
#183694 = DIRECTION ( 'NONE',  ( -1.000000000000000000, -3.190570557967288949E-16, -6.948722487160392945E-17 ) ) ;
#183695 = DIRECTION ( 'NONE',  ( -6.938893903907220489E-15, 0.4721928772777343464, 0.8814952561688431665 ) ) ;
#183696 = DIRECTION ( 'NONE',  ( -0.000000000000000000, -0.1350103645451904977, 0.9908441862701596881 ) ) ;
#183697 = LINE ( 'NONE', #67589, #178000 ) ;
#183698 = CARTESIAN_POINT ( 'NONE',  ( 21.07928932188134397, 1.115600667400684642E-11, -67.00000000000004263 ) ) ;
#183699 = DIRECTION ( 'NONE',  ( 0.000000000000000000, 0.000000000000000000, -1.000000000000000000 ) ) ;
#183700 = FACE_OUTER_BOUND ( 'NONE', #229661, .T. ) ;
#183701 = FACE_OUTER_BOUND ( 'NONE', #4221, .T. ) ;
#183702 = EDGE_CURVE ( 'NONE', #137777, #211036, #82197, .T. ) ;
#183703 = DIRECTION ( 'NONE',  ( 0.000000000000000000, 0.000000000000000000, 1.000000000000000000 ) ) ;
#183704 = AXIS2_PLACEMENT_3D ( 'NONE', #235398, #195023, #252386 ) ;
#183705 = CARTESIAN_POINT ( 'NONE',  ( 19.75857864376268935, 64.25000000001196554, -111.6731074845243796 ) ) ;
#183706 = ADVANCED_FACE ( 'NONE', ( #58792 ), #41850, .T. ) ;
#183707 = ORIENTED_EDGE ( 'NONE', *, *, #69166, .F. ) ;
#183708 = AXIS2_PLACEMENT_3D ( 'NONE', #221536, #19531, #258076 ) ;
#183709 = ADVANCED_FACE ( 'NONE', ( #19707 ), #56229, .F. ) ;
#183710 = DIRECTION ( 'NONE',  ( 0.000000000000000000, 0.000000000000000000, 1.000000000000000000 ) ) ;
#183711 = EDGE_CURVE ( 'NONE', #16494, #55133, #5103, .T. ) ;
#183712 = ORIENTED_EDGE ( 'NONE', *, *, #124742, .F. ) ;
#183713 = TOROIDAL_SURFACE ( 'NONE', #71291, 3.899999999999999467, 0.1000000000000000056 ) ;
#183714 = AXIS2_PLACEMENT_3D ( 'NONE', #21539, #38526, #18944 ) ;
#183715 = DIRECTION ( 'NONE',  ( 1.000000000000000000, 0.000000000000000000, 0.000000000000000000 ) ) ;
#183716 = DIRECTION ( 'NONE',  ( -1.000000000000000000, -0.000000000000000000, -0.000000000000000000 ) ) ;
#183717 = CARTESIAN_POINT ( 'NONE',  ( 21.09787244211714352, 61.96551932823614095, -221.7456163672507898 ) ) ;
#183718 = ORIENTED_EDGE ( 'NONE', *, *, #6057, .T. ) ;
#183719 = DIRECTION ( 'NONE',  ( -1.000000000000000000, 0.000000000000000000, 0.000000000000000000 ) ) ;
#183720 = DIRECTION ( 'NONE',  ( 1.000000000000000000, -0.000000000000000000, -0.000000000000000000 ) ) ;
#183721 = CARTESIAN_POINT ( 'NONE',  ( 23.14999999999999858, 36.65892442174935439, -249.5511627012433848 ) ) ;
#183722 = DIRECTION ( 'NONE',  ( 1.000000000000000000, 0.000000000000000000, 0.000000000000000000 ) ) ;
#183723 = CARTESIAN_POINT ( 'NONE',  ( -22.50000000000000000, 1.115600667400684642E-11, -134.0000000000000000 ) ) ;
#183724 = AXIS2_PLACEMENT_3D ( 'NONE', #39219, #198257, #75762 ) ;
#183725 = VECTOR ( 'NONE', #58278, 1000.000000000000000 ) ;
#183726 = CIRCLE ( 'NONE', #88004, 0.1000000000000028644 ) ;
#183727 = ORIENTED_EDGE ( 'NONE', *, *, #238765, .F. ) ;
#183728 = CARTESIAN_POINT ( 'NONE',  ( -23.39999999999994529, 76.00000000001119815, -36.02310748452479316 ) ) ;
#183730 = EDGE_LOOP ( 'NONE', ( #28970, #101766, #32948, #10388 ) ) ;
#183729 = CARTESIAN_POINT ( 'NONE',  ( 22.49231231312462853, 11.64998490368843953, -167.4389471123986084 ) ) ;
#183731 = CARTESIAN_POINT ( 'NONE',  ( -23.25000000000000000, 87.75000000001246292, -170.0231074845242745 ) ) ;
#183732 = CARTESIAN_POINT ( 'NONE',  ( -20.54999999999999716, 54.18213181965657554, -236.9344197582443883 ) ) ;
#183733 = DIRECTION ( 'NONE',  ( 0.000000000000000000, -0.9999176327611369874, 0.01283462868041987913 ) ) ;
#183734 = VERTEX_POINT ( 'NONE', #156672 ) ;
#183735 = LINE ( 'NONE', #160341, #230358 ) ;
#183736 = DIRECTION ( 'NONE',  ( -0.000000000000000000, -0.000000000000000000, 1.000000000000000000 ) ) ;
#183737 = ORIENTED_EDGE ( 'NONE', *, *, #125305, .F. ) ;
#183738 = LINE ( 'NONE', #238569, #92526 ) ;
#183739 = EDGE_CURVE ( 'NONE', #20227, #30979, #105047, .T. ) ;
#183740 = LINE ( 'NONE', #5062, #53821 ) ;
#183741 = EDGE_LOOP ( 'NONE', ( #158252, #98751, #159537, #141060 ) ) ;
#183742 = VERTEX_POINT ( 'NONE', #203474 ) ;
#183743 = CARTESIAN_POINT ( 'NONE',  ( 21.05000000000000071, 10.68429367439822997, -74.52667393863758605 ) ) ;
#183744 = DIRECTION ( 'NONE',  ( 1.000000000000000000, 0.000000000000000000, 0.000000000000000000 ) ) ;
#183745 = DIRECTION ( 'NONE',  ( 1.000000000000000000, 0.000000000000000000, 0.000000000000000000 ) ) ;
#183746 = EDGE_CURVE ( 'NONE', #248393, #433, #118470, .T. ) ;
#183747 = CIRCLE ( 'NONE', #179480, 0.09999999999999939493 ) ;
#183748 = LINE ( 'NONE', #22122, #3154 ) ;
#183749 = FACE_OUTER_BOUND ( 'NONE', #21678, .T. ) ;
#183750 = FACE_OUTER_BOUND ( 'NONE', #188041, .T. ) ;
#183751 = CARTESIAN_POINT ( 'NONE',  ( 20.05000000000002913, 21.70314669089255233, -233.3151006027785002 ) ) ;
#183752 = EDGE_CURVE ( 'NONE', #156184, #82535, #45674, .T. ) ;
#183754 = LINE ( 'NONE', #203317, #103654 ) ;
#183753 = CARTESIAN_POINT ( 'NONE',  ( 21.05000000000000071, -1.448466219907752039, -194.7514528548905730 ) ) ;
#183755 = DIRECTION ( 'NONE',  ( -1.000000000000000000, -0.000000000000000000, -0.000000000000000000 ) ) ;
#183756 = LINE ( 'NONE', #25973, #54650 ) ;
#183757 = DIRECTION ( 'NONE',  ( 1.000000000000000000, -0.000000000000000000, -0.000000000000000000 ) ) ;
#183758 = EDGE_LOOP ( 'NONE', ( #226138, #168827, #63620, #86141 ) ) ;
#183759 = ORIENTED_EDGE ( 'NONE', *, *, #76039, .F. ) ;
#183760 = DIRECTION ( 'NONE',  ( 1.000000000000000000, 0.000000000000000000, 0.000000000000000000 ) ) ;
#183761 = CARTESIAN_POINT ( 'NONE',  ( 21.14999999999999503, -11.74999999998883560, -170.3999999999999773 ) ) ;
#183763 = CARTESIAN_POINT ( 'NONE',  ( -15.73854595235691534, 12.75065881068273832, -215.6014281960218852 ) ) ;
#183762 = CARTESIAN_POINT ( 'NONE',  ( -21.05000000000000426, 69.66772772607630770, -102.9855714212386744 ) ) ;
#183764 = EDGE_CURVE ( 'NONE', #14083, #98899, #108222, .T. ) ;
#183765 = CIRCLE ( 'NONE', #117123, 0.09999999999999789613 ) ;
#183766 = CARTESIAN_POINT ( 'NONE',  ( 20.94999999999999929, 5.400000000011154988, -157.6060308773475640 ) ) ;
#183767 = CARTESIAN_POINT ( 'NONE',  ( -23.15000000000000213, -11.64999999998884483, -97.50000000000004263 ) ) ;
#183768 = CARTESIAN_POINT ( 'NONE',  ( -22.47071067811865319, 68.27992525551407255, -136.6221999392269595 ) ) ;
#183769 = EDGE_CURVE ( 'NONE', #180654, #143742, #7847, .T. ) ;
#183770 = ADVANCED_FACE ( 'NONE', ( #187770 ), #104865, .T. ) ;
#183771 = DIRECTION ( 'NONE',  ( 0.000000000000000000, -0.9126074666063622720, -0.4088369013363611360 ) ) ;
#183772 = EDGE_LOOP ( 'NONE', ( #180121, #88804, #158521, #151710 ) ) ;
#183773 = CARTESIAN_POINT ( 'NONE',  ( -22.47071067811865319, 76.00000000001165290, -69.52310748452431710 ) ) ;
#183774 = EDGE_CURVE ( 'NONE', #117379, #226840, #130014, .T. ) ;
#183775 = ORIENTED_EDGE ( 'NONE', *, *, #86680, .T. ) ;
#183776 = CARTESIAN_POINT ( 'NONE',  ( -18.52328366898032286, -9.642321089030096104, -73.71481933757003446 ) ) ;
#183777 = AXIS2_PLACEMENT_3D ( 'NONE', #45780, #223127, #121501 ) ;
#183778 = AXIS2_PLACEMENT_3D ( 'NONE', #114344, #150900, #93484 ) ;
#183779 = CARTESIAN_POINT ( 'NONE',  ( 19.99999999999998934, 64.25000000001220712, -145.1731074845244507 ) ) ;
#183780 = ORIENTED_EDGE ( 'NONE', *, *, #99000, .T. ) ;
#183781 = CARTESIAN_POINT ( 'NONE',  ( -20.94999999999999929, 2.859758780633683273, -208.6670499591424459 ) ) ;
#183782 = EDGE_CURVE ( 'NONE', #144953, #131204, #87349, .T. ) ;
#183783 = ORIENTED_EDGE ( 'NONE', *, *, #154920, .T. ) ;
#183784 = CARTESIAN_POINT ( 'NONE',  ( -18.58671080940899500, 85.40693285883894248, -162.8989530196195972 ) ) ;
#183785 = DIRECTION ( 'NONE',  ( -0.7071067811865708874, 0.3338907855511046296, 0.6233112732207185536 ) ) ;
#183786 = CARTESIAN_POINT ( 'NONE',  ( -18.35235881385853318, 64.52658099229870459, -60.27310748452440947 ) ) ;
#183787 = CARTESIAN_POINT ( 'NONE',  ( -20.54999999999999716, 1.115600667400684642E-11, -167.5000000000000284 ) ) ;
#183788 = CARTESIAN_POINT ( 'NONE',  ( -14.00000000000000178, 9.850000000011133849, -50.25000000000000711 ) ) ;
#183789 = CARTESIAN_POINT ( 'NONE',  ( -16.81744102076748959, 66.05000000001255955, -182.6731074845244223 ) ) ;
#183790 = LINE ( 'NONE', #224187, #234317 ) ;
#183791 = LINE ( 'NONE', #168126, #240473 ) ;
#183793 = VERTEX_POINT ( 'NONE', #243866 ) ;
#183792 = CARTESIAN_POINT ( 'NONE',  ( 20.97438252431638972, 67.07457649393607824, -128.0507367955135578 ) ) ;
#183794 = CARTESIAN_POINT ( 'NONE',  ( -21.59142135623730852, 7.850000000011158718, -179.8499999999999943 ) ) ;
#183795 = ORIENTED_EDGE ( 'NONE', *, *, #50725, .F. ) ;
#183797 = ORIENTED_EDGE ( 'NONE', *, *, #79432, .T. ) ;
#183796 = FACE_OUTER_BOUND ( 'NONE', #47691, .T. ) ;
#183798 = VERTEX_POINT ( 'NONE', #127791 ) ;
#183799 = CARTESIAN_POINT ( 'NONE',  ( 23.24999999999997513, 11.75000000001116263, -59.98519422934606382 ) ) ;
#183800 = CARTESIAN_POINT ( 'NONE',  ( -18.59999999999999787, 11.64999999999999680, -21.35000000000000142 ) ) ;
#183801 = ORIENTED_EDGE ( 'NONE', *, *, #190788, .F. ) ;
#183802 = CARTESIAN_POINT ( 'NONE',  ( -20.00857864376270001, 9.150000000011157653, -54.75000000000000000 ) ) ;
#183803 = DIRECTION ( 'NONE',  ( -1.000000000000000000, -0.000000000000000000, -0.000000000000000000 ) ) ;
#183804 = LINE ( 'NONE', #101663, #218925 ) ;
#183805 = DIRECTION ( 'NONE',  ( 1.000000000000000000, -7.304098846218134667E-16, -5.100424963727255829E-30 ) ) ;
#183806 = DIRECTION ( 'NONE',  ( 0.000000000000000000, -6.308085367188367561E-15, 1.000000000000000000 ) ) ;
#183807 = AXIS2_PLACEMENT_3D ( 'NONE', #111859, #113135, #132710 ) ;
#183808 = VECTOR ( 'NONE', #51608, 1000.000000000000000 ) ;
#183809 = CYLINDRICAL_SURFACE ( 'NONE', #60178, 11.75000000000000000 ) ;
#183810 = VERTEX_POINT ( 'NONE', #86048 ) ;
#183811 = ORIENTED_EDGE ( 'NONE', *, *, #114358, .T. ) ;
#183812 = CARTESIAN_POINT ( 'NONE',  ( 20.00000000000000711, 4.527376849368447864, 21.95857864376269220 ) ) ;
#183813 = EDGE_CURVE ( 'NONE', #200838, #220497, #105956, .T. ) ;
#183814 = VERTEX_POINT ( 'NONE', #66530 ) ;
#183815 = DIRECTION ( 'NONE',  ( 0.000000000000000000, 0.1335171055202867274, 0.9910465087640866200 ) ) ;
#183816 = EDGE_LOOP ( 'NONE', ( #90915, #117366, #73393, #115779 ) ) ;
#183817 = CARTESIAN_POINT ( 'NONE',  ( -18.39999999999999858, 77.27075167199318173, -241.8768735168259241 ) ) ;
#183818 = CARTESIAN_POINT ( 'NONE',  ( -16.93388492042259230, 9.988541822527057690, -180.0994548768137804 ) ) ;
#183819 = CARTESIAN_POINT ( 'NONE',  ( -21.46681500593007996, 69.14248884062476463, -103.0231074845243597 ) ) ;
#183820 = EDGE_CURVE ( 'NONE', #244409, #115244, #96684, .T. ) ;
#183821 = CARTESIAN_POINT ( 'NONE',  ( -21.08078803292166725, 30.84699535066559761, -252.0680663746180414 ) ) ;
#183822 = CARTESIAN_POINT ( 'NONE',  ( 21.11344571971254069, 10.61787902352924817, -179.7460208924021856 ) ) ;
#183823 = ORIENTED_EDGE ( 'NONE', *, *, #34716, .F. ) ;
#183824 = AXIS2_PLACEMENT_3D ( 'NONE', #252674, #255196, #136573 ) ;
#183825 = DIRECTION ( 'NONE',  ( 0.000000000000000000, 0.000000000000000000, -1.000000000000000000 ) ) ;
#183826 = EDGE_CURVE ( 'NONE', #17324, #136972, #30112, .T. ) ;
#183827 = ADVANCED_FACE ( 'NONE', ( #242579 ), #186478, .T. ) ;
#183828 = FACE_OUTER_BOUND ( 'NONE', #101230, .T. ) ;
#183829 = DIRECTION ( 'NONE',  ( 0.000000000000000000, -0.4791956752371546169, -0.8777080977375152360 ) ) ;
#183830 = DIRECTION ( 'NONE',  ( 0.000000000000000000, 1.000000000000000000, 0.000000000000000000 ) ) ;
#183831 = ORIENTED_EDGE ( 'NONE', *, *, #152814, .T. ) ;
#183833 = LINE ( 'NONE', #48166, #181586 ) ;
#183832 = CARTESIAN_POINT ( 'NONE',  ( 21.08621493067296626, 61.08863989881826484, -234.2474152884988996 ) ) ;
#183834 = VERTEX_POINT ( 'NONE', #63958 ) ;
#183837 = ORIENTED_EDGE ( 'NONE', *, *, #128526, .T. ) ;
#183836 = DIRECTION ( 'NONE',  ( 0.000000000000000000, 0.000000000000000000, -1.000000000000000000 ) ) ;
#183835 = DIRECTION ( 'NONE',  ( -1.000000000000000000, 0.000000000000000000, -0.000000000000000000 ) ) ;
#183838 = VERTEX_POINT ( 'NONE', #147339 ) ;
#183839 = CARTESIAN_POINT ( 'NONE',  ( -16.87242674293850087, 9.950000000011138823, -113.1489097536276773 ) ) ;
#183840 = CARTESIAN_POINT ( 'NONE',  ( 15.74999999999999645, 66.15000000001155911, -52.77310748452440237 ) ) ;
#183841 = CYLINDRICAL_SURFACE ( 'NONE', #129263, 0.09999999999999939493 ) ;
#183842 = ORIENTED_EDGE ( 'NONE', *, *, #105583, .T. ) ;
#183843 = FACE_OUTER_BOUND ( 'NONE', #93123, .T. ) ;
#183844 = EDGE_CURVE ( 'NONE', #232247, #115618, #9123, .T. ) ;
#183845 = AXIS2_PLACEMENT_3D ( 'NONE', #100482, #180059, #256966 ) ;
#183846 = DIRECTION ( 'NONE',  ( 1.000000000000000000, 0.000000000000000000, 0.000000000000000000 ) ) ;
#183847 = ADVANCED_FACE ( 'NONE', ( #131627 ), #112087, .T. ) ;
#183849 = DIRECTION ( 'NONE',  ( -1.000000000000000000, 0.000000000000000000, 0.000000000000000000 ) ) ;
#183848 = FACE_OUTER_BOUND ( 'NONE', #167668, .T. ) ;
#183851 = EDGE_LOOP ( 'NONE', ( #189409, #62618, #119375 ) ) ;
#183850 = DIRECTION ( 'NONE',  ( 0.000000000000000000, 0.2128009952263600346, -0.9770955615653315052 ) ) ;
#183852 = AXIS2_PLACEMENT_3D ( 'NONE', #57296, #173478, #232124 ) ;
#183853 = ORIENTED_EDGE ( 'NONE', *, *, #216567, .F. ) ;
#183854 = CIRCLE ( 'NONE', #54659, 7.900000000000000355 ) ;
#183855 = CARTESIAN_POINT ( 'NONE',  ( 21.05000000000000071, 36.65892442174472876, -249.5511627012454596 ) ) ;
#183856 = CARTESIAN_POINT ( 'NONE',  ( 22.39999999999999503, -2.598867842139048090, -189.5410128746472083 ) ) ;
#183857 = CARTESIAN_POINT ( 'NONE',  ( -20.64999999999999858, 4.350000000011156054, -112.7500000000000284 ) ) ;
#183859 = ORIENTED_EDGE ( 'NONE', *, *, #193369, .T. ) ;
#183858 = TOROIDAL_SURFACE ( 'NONE', #34057, 0.2000000000000000111, 0.1000000000000000056 ) ;
#183860 = CARTESIAN_POINT ( 'NONE',  ( -23.15000000000000213, 4.350000000011156054, -179.7499999999999716 ) ) ;
#183861 = VERTEX_POINT ( 'NONE', #70414 ) ;
#183862 = EDGE_CURVE ( 'NONE', #66328, #83116, #225684, .T. ) ;
#183863 = DIRECTION ( 'NONE',  ( -0.000000000000000000, 1.000000000000000000, 0.000000000000000000 ) ) ;
#183864 = CIRCLE ( 'NONE', #71458, 11.89999999999999325 ) ;
#183866 = EDGE_CURVE ( 'NONE', #61549, #154428, #163366, .T. ) ;
#183865 = DIRECTION ( 'NONE',  ( 1.000000000000000000, 0.000000000000000000, 0.000000000000000000 ) ) ;
#183867 = DIRECTION ( 'NONE',  ( 0.000000000000000000, 0.000000000000000000, -1.000000000000000000 ) ) ;
#183868 = ADVANCED_FACE ( 'NONE', ( #251572 ), #252851, .T. ) ;
#183869 = ORIENTED_EDGE ( 'NONE', *, *, #46107, .T. ) ;
#183870 = DIRECTION ( 'NONE',  ( 1.000000000000000000, 2.952720810173289112E-16, -0.000000000000000000 ) ) ;
#183871 = AXIS2_PLACEMENT_3D ( 'NONE', #233972, #59154, #252246 ) ;
#183872 = ADVANCED_FACE ( 'NONE', ( #31290 ), #67490, .T. ) ;
#183873 = TOROIDAL_SURFACE ( 'NONE', #221263, 3.899999999999999467, 0.1000000000000000056 ) ;
#183874 = DIRECTION ( 'NONE',  ( 0.000000000000000000, 0.000000000000000000, 1.000000000000000000 ) ) ;
#183875 = CIRCLE ( 'NONE', #196332, 0.5000000000000004441 ) ;
#183876 = ORIENTED_EDGE ( 'NONE', *, *, #6684, .F. ) ;
#183877 = VERTEX_POINT ( 'NONE', #50783 ) ;
#183878 = CIRCLE ( 'NONE', #96373, 0.09999999999999939493 ) ;
#183879 = EDGE_LOOP ( 'NONE', ( #211518, #182367, #249723, #122094 ) ) ;
#183880 = CARTESIAN_POINT ( 'NONE',  ( -20.54999999999999716, -8.999999999988844479, -191.1060308773475356 ) ) ;
#183881 = VERTEX_POINT ( 'NONE', #130333 ) ;
#183883 = ORIENTED_EDGE ( 'NONE', *, *, #192488, .T. ) ;
#183882 = DIRECTION ( 'NONE',  ( 0.000000000000000000, 0.000000000000000000, -1.000000000000000000 ) ) ;
#183884 = ORIENTED_EDGE ( 'NONE', *, *, #64704, .T. ) ;
#183888 = ADVANCED_FACE ( 'NONE', ( #114634 ), #192898, .T. ) ;
#183887 = ORIENTED_EDGE ( 'NONE', *, *, #25218, .F. ) ;
#183886 = VERTEX_POINT ( 'NONE', #213731 ) ;
#183885 = CARTESIAN_POINT ( 'NONE',  ( 23.14999999999999858, 76.00000000001190870, -103.0231074845243029 ) ) ;
#183889 = DIRECTION ( 'NONE',  ( -1.000000000000000000, 0.000000000000000000, 0.000000000000000000 ) ) ;
#183890 = ORIENTED_EDGE ( 'NONE', *, *, #24924, .T. ) ;
#183891 = DIRECTION ( 'NONE',  ( 1.000000000000000000, -7.304098846218134667E-16, -5.100424963727255829E-30 ) ) ;
#183892 = AXIS2_PLACEMENT_3D ( 'NONE', #125100, #245031, #45550 ) ;
#183893 = AXIS2_PLACEMENT_3D ( 'NONE', #27571, #187900, #87485 ) ;
#183894 = LINE ( 'NONE', #5224, #238775 ) ;
#183895 = AXIS2_PLACEMENT_3D ( 'NONE', #23103, #160051, #141735 ) ;
#183897 = CARTESIAN_POINT ( 'NONE',  ( -18.41817142474038249, 86.89613756584731163, -199.6357039480042488 ) ) ;
#183896 = AXIS2_PLACEMENT_3D ( 'NONE', #191719, #254206, #33948 ) ;
#183898 = ORIENTED_EDGE ( 'NONE', *, *, #91308, .F. ) ;
#183899 = ADVANCED_FACE ( 'NONE', ( #209900 ), #11702, .T. ) ;
#183900 = LINE ( 'NONE', #186474, #253935 ) ;
#183902 = ORIENTED_EDGE ( 'NONE', *, *, #154948, .F. ) ;
#183901 = DIRECTION ( 'NONE',  ( 1.000000000000000000, 0.000000000000000000, 0.000000000000000000 ) ) ;
#183903 = DIRECTION ( 'NONE',  ( -1.000000000000000000, -0.000000000000000000, 0.000000000000000000 ) ) ;
#183905 = ORIENTED_EDGE ( 'NONE', *, *, #248794, .F. ) ;
#183904 = CARTESIAN_POINT ( 'NONE',  ( -21.05000000000000071, 7.939498413483247141, -209.7295111514051200 ) ) ;
#183906 = ORIENTED_EDGE ( 'NONE', *, *, #235590, .F. ) ;
#183907 = ADVANCED_FACE ( 'NONE', ( #232036 ), #53378, .T. ) ;
#183908 = EDGE_LOOP ( 'NONE', ( #211194, #192123, #46693, #146991 ) ) ;
#183909 = ORIENTED_EDGE ( 'NONE', *, *, #257151, .T. ) ;
#183910 = CARTESIAN_POINT ( 'NONE',  ( 18.54999999999999716, 66.05000000001223270, -149.1731074845243654 ) ) ;
#183911 = CARTESIAN_POINT ( 'NONE',  ( -33.72168855820451938, 9.950000000011156587, -79.65000000000000568 ) ) ;
#183912 = VECTOR ( 'NONE', #160591, 1000.000000000000000 ) ;
#183913 = B_SPLINE_CURVE_WITH_KNOTS ( 'NONE', 3,
 ( #36466, #96386, #254180, #114688, #153871, #35195, #95125, #232090, #115987, #73035, #233384, #16890, #136808, #174716, #195538, #13049 ),
 .UNSPECIFIED., .F., .F.,
 ( 4, 3, 3, 3, 3, 4 ),
 ( 0.000000000000000000, 3.357088238233600668E-05, 6.714213034886770139E-05, 0.0001007408646120938085, 0.0001343627955914254344, 0.0001573956632896058639 ),
 .UNSPECIFIED. ) ;
#183914 = EDGE_CURVE ( 'NONE', #26458, #208846, #250293, .T. ) ;
#183916 = ORIENTED_EDGE ( 'NONE', *, *, #205891, .F. ) ;
#183915 = ORIENTED_EDGE ( 'NONE', *, *, #76498, .T. ) ;
#183917 = ORIENTED_EDGE ( 'NONE', *, *, #257764, .T. ) ;
#183919 = EDGE_CURVE ( 'NONE', #9029, #241512, #230748, .T. ) ;
#183918 = DIRECTION ( 'NONE',  ( 0.000000000000000000, 6.982962677686266711E-15, -1.000000000000000000 ) ) ;
#183920 = VERTEX_POINT ( 'NONE', #233324 ) ;
#183921 = ORIENTED_EDGE ( 'NONE', *, *, #20064, .F. ) ;
#183922 = FACE_OUTER_BOUND ( 'NONE', #164816, .T. ) ;
#183924 = ORIENTED_EDGE ( 'NONE', *, *, #102042, .T. ) ;
#183923 = DIRECTION ( 'NONE',  ( 0.000000000000000000, 0.9126074666063660468, 0.4088369013363524762 ) ) ;
#183925 = DIRECTION ( 'NONE',  ( 1.000000000000000000, -0.000000000000000000, -0.000000000000000000 ) ) ;
#183927 = CYLINDRICAL_SURFACE ( 'NONE', #23475, 0.1000000000000024342 ) ;
#183926 = DIRECTION ( 'NONE',  ( 0.000000000000000000, 0.000000000000000000, -1.000000000000000000 ) ) ;
#183928 = AXIS2_PLACEMENT_3D ( 'NONE', #202805, #141543, #64574 ) ;
#183929 = ORIENTED_EDGE ( 'NONE', *, *, #61571, .F. ) ;
#183931 = EDGE_LOOP ( 'NONE', ( #70188, #201472 ) ) ;
#183930 = ORIENTED_EDGE ( 'NONE', *, *, #22304, .T. ) ;
#183932 = CARTESIAN_POINT ( 'NONE',  ( -23.25000000000000355, 53.37686160793744961, -235.8706811220569932 ) ) ;
#183934 = EDGE_CURVE ( 'NONE', #187756, #103678, #14277, .T. ) ;
#183933 = DIRECTION ( 'NONE',  ( 0.000000000000000000, 0.8814952561688437216, -0.4721928772777331806 ) ) ;
#183935 = ORIENTED_EDGE ( 'NONE', *, *, #85126, .F. ) ;
#183936 = EDGE_CURVE ( 'NONE', #126, #75809, #200774, .T. ) ;
#183937 = AXIS2_PLACEMENT_3D ( 'NONE', #180475, #86471, #26547 ) ;
#183938 = DIRECTION ( 'NONE',  ( 0.000000000000000000, -0.8700118002898321601, 0.4930308989875230030 ) ) ;
#183939 = ORIENTED_EDGE ( 'NONE', *, *, #127158, .T. ) ;
#183940 = ORIENTED_EDGE ( 'NONE', *, *, #20721, .T. ) ;
#183941 = EDGE_CURVE ( 'NONE', #235080, #70430, #71802, .T. ) ;
#183942 = DIRECTION ( 'NONE',  ( 0.000000000000000000, 0.000000000000000000, -1.000000000000000000 ) ) ;
#183943 = ORIENTED_EDGE ( 'NONE', *, *, #7888, .T. ) ;
#183944 = FACE_OUTER_BOUND ( 'NONE', #133891, .T. ) ;
#183945 = DIRECTION ( 'NONE',  ( -1.000000000000000000, -0.000000000000000000, -0.000000000000000000 ) ) ;
#183946 = ORIENTED_EDGE ( 'NONE', *, *, #165471, .T. ) ;
#183947 = CARTESIAN_POINT ( 'NONE',  ( 20.85000000000000142, 77.83585931145498193, -24.51866831572578320 ) ) ;
#183948 = CARTESIAN_POINT ( 'NONE',  ( 18.59999999999999076, 55.04793976901536467, -229.8170162380219494 ) ) ;
#183950 = CYLINDRICAL_SURFACE ( 'NONE', #103859, 0.09999999999999939493 ) ;
#183949 = DIRECTION ( 'NONE',  ( 0.000000000000000000, 0.1350103645451807555, 0.9908441862701609093 ) ) ;
#183951 = DIRECTION ( 'NONE',  ( 1.000000000000000000, 0.000000000000000000, 0.000000000000000000 ) ) ;
#183952 = CARTESIAN_POINT ( 'NONE',  ( -21.14999999999999858, 87.75000000001212186, -133.6231074845242119 ) ) ;
#183954 = EDGE_CURVE ( 'NONE', #43709, #113685, #75875, .T. ) ;
#183953 = DIRECTION ( 'NONE',  ( -1.000000000000000000, 0.000000000000000000, 0.000000000000000000 ) ) ;
#183955 = DIRECTION ( 'NONE',  ( 0.000000000000000000, -6.938893903907234689E-15, 1.000000000000000000 ) ) ;
#183956 = EDGE_CURVE ( 'NONE', #251409, #17057, #221592, .T. ) ;
#183957 = CIRCLE ( 'NONE', #21479, 11.64999999999999325 ) ;
#183958 = ORIENTED_EDGE ( 'NONE', *, *, #235000, .T. ) ;
#183959 = CIRCLE ( 'NONE', #175590, 0.09999999999999939493 ) ;
#183960 = AXIS2_PLACEMENT_3D ( 'NONE', #193706, #186337, #35929 ) ;
#183962 = VERTEX_POINT ( 'NONE', #249030 ) ;
#183961 = ORIENTED_EDGE ( 'NONE', *, *, #160624, .T. ) ;
#183963 = EDGE_LOOP ( 'NONE', ( #85903, #35033, #186705, #184734 ) ) ;
#183964 = FACE_OUTER_BOUND ( 'NONE', #18339, .T. ) ;
#183965 = DIRECTION ( 'NONE',  ( -4.701977403289178058E-30, 0.2128009952263773819, -0.9770955615653279525 ) ) ;
#183966 = ADVANCED_FACE ( 'NONE', ( #158920 ), #159105, .F. ) ;
#183968 = CARTESIAN_POINT ( 'NONE',  ( -23.15000000000000213, -11.39257802170566691, -30.42605042016806394 ) ) ;
#183967 = DIRECTION ( 'NONE',  ( -0.8049926720990042694, -0.5932847527679310229, 0.000000000000000000 ) ) ;
#183969 = EDGE_CURVE ( 'NONE', #243144, #96731, #232159, .T. ) ;
#183970 = CARTESIAN_POINT ( 'NONE',  ( -21.14999999999999858, 76.00000000001219291, -143.0637644362255401 ) ) ;
#183971 = VERTEX_POINT ( 'NONE', #218851 ) ;
#183972 = DIRECTION ( 'NONE',  ( 0.000000000000000000, 1.000000000000000000, 0.000000000000000000 ) ) ;
#183973 = FACE_OUTER_BOUND ( 'NONE', #52321, .T. ) ;
#183975 = AXIS2_PLACEMENT_3D ( 'NONE', #12830, #33701, #113188 ) ;
#183974 = CARTESIAN_POINT ( 'NONE',  ( -16.94225986326250677, 66.05000000001189164, -90.07638810891651815 ) ) ;
#183976 = CARTESIAN_POINT ( 'NONE',  ( -16.91776028072577631, 9.963400393640901243, -87.87502401470217706 ) ) ;
#183977 = EDGE_LOOP ( 'NONE', ( #253063, #235630, #214134, #148445 ) ) ;
#183978 = DIRECTION ( 'NONE',  ( -1.000000000000000000, 0.000000000000000000, 0.000000000000000000 ) ) ;
#183979 = CARTESIAN_POINT ( 'NONE',  ( -5.899999999999938183, 64.75000000001119815, -25.92310748452479174 ) ) ;
#183980 = ORIENTED_EDGE ( 'NONE', *, *, #186908, .F. ) ;
#183981 = CARTESIAN_POINT ( 'NONE',  ( -22.94999999999999929, 1.800000000000000044, -11.61130914238355771 ) ) ;
#183982 = DIRECTION ( 'NONE',  ( 1.000000000000000000, 0.000000000000000000, 0.000000000000000000 ) ) ;
#183984 = CARTESIAN_POINT ( 'NONE',  ( 20.85000000000000142, -1.835859311443637010, -45.00443916879852679 ) ) ;
#183983 = B_SPLINE_CURVE_WITH_KNOTS ( 'NONE', 3,
 ( #96935, #40886, #22591, #215625, #37028, #425 ),
 .UNSPECIFIED., .F., .F.,
 ( 4, 2, 4 ),
 ( 0.000000000000000000, 0.0002113392456166052918, 0.0004226784912332105836 ),
 .UNSPECIFIED. ) ;
#183985 = CARTESIAN_POINT ( 'NONE',  ( 19.90000000000000924, 11.61130914238355771, 21.90000000000000213 ) ) ;
#183986 = FACE_OUTER_BOUND ( 'NONE', #6506, .T. ) ;
#183987 = CARTESIAN_POINT ( 'NONE',  ( -18.37013991200266005, 11.49974761621197494, -24.29302301051712121 ) ) ;
#183988 = ORIENTED_EDGE ( 'NONE', *, *, #35283, .F. ) ;
#183989 = DIRECTION ( 'NONE',  ( 1.000000000000000000, 0.000000000000000000, 0.000000000000000000 ) ) ;
#183990 = DIRECTION ( 'NONE',  ( 0.7071067811865474617, 0.7071067811865474617, 0.000000000000000000 ) ) ;
#183991 = CARTESIAN_POINT ( 'NONE',  ( -21.05000000000000071, 1.115526128501326264E-11, -60.45934304829882677 ) ) ;
#183994 = DIRECTION ( 'NONE',  ( 2.952720810173289112E-16, 1.000000000000000000, 6.982962677686266711E-15 ) ) ;
#183993 = AXIS2_PLACEMENT_3D ( 'NONE', #48458, #5459, #246655 ) ;
#183992 = FACE_OUTER_BOUND ( 'NONE', #39780, .T. ) ;
#183996 = DIRECTION ( 'NONE',  ( -0.000000000000000000, 1.000000000000000000, 6.982962677686266711E-15 ) ) ;
#183995 = CIRCLE ( 'NONE', #71588, 0.1000000000000028644 ) ;
#183997 = AXIS2_PLACEMENT_3D ( 'NONE', #243055, #25323, #20173 ) ;
#183998 = DIRECTION ( 'NONE',  ( 0.000000000000000000, 0.000000000000000000, -1.000000000000000000 ) ) ;
#183999 = FACE_OUTER_BOUND ( 'NONE', #140698, .T. ) ;
#184000 = DIRECTION ( 'NONE',  ( 0.000000000000000000, 1.000000000000000000, 6.352154140967427193E-15 ) ) ;
#184002 = VERTEX_POINT ( 'NONE', #135465 ) ;
#184001 = LINE ( 'NONE', #69219, #119447 ) ;
#184003 = EDGE_CURVE ( 'NONE', #7325, #195498, #178488, .T. ) ;
#184004 = AXIS2_PLACEMENT_3D ( 'NONE', #222522, #64749, #223813 ) ;
#184005 = DIRECTION ( 'NONE',  ( -0.000000000000000000, -0.8814952561688430555, 0.4721928772777346239 ) ) ;
#184006 = CARTESIAN_POINT ( 'NONE',  ( 18.49999999999999645, 77.16270174995064224, -195.4231074845243370 ) ) ;
#184007 = EDGE_CURVE ( 'NONE', #52602, #180036, #138205, .T. ) ;
#184008 = CARTESIAN_POINT ( 'NONE',  ( 12.60053434924910398, 9.389534562357857439, -149.6748093043899814 ) ) ;
#184009 = VERTEX_POINT ( 'NONE', #156364 ) ;
#184010 = FACE_OUTER_BOUND ( 'NONE', #126526, .T. ) ;
#184011 = CARTESIAN_POINT ( 'NONE',  ( 21.03670563405601968, 65.37517631068334367, -57.19756059831524908 ) ) ;
#184012 = DIRECTION ( 'NONE',  ( -1.000000000000000000, -0.000000000000000000, 0.000000000000000000 ) ) ;
#184013 = ORIENTED_EDGE ( 'NONE', *, *, #163929, .F. ) ;
#184014 = DIRECTION ( 'NONE',  ( -1.000000000000000000, 0.000000000000000000, 0.000000000000000000 ) ) ;
#184016 = VERTEX_POINT ( 'NONE', #36409 ) ;
#184015 = CARTESIAN_POINT ( 'NONE',  ( -16.27683809663750480, 9.350000000011133849, -188.4499999999999886 ) ) ;
#184018 = FACE_OUTER_BOUND ( 'NONE', #31441, .T. ) ;
#184017 = CARTESIAN_POINT ( 'NONE',  ( -20.07928932188135107, 22.36925365942468957, -231.4362706255523108 ) ) ;
#184019 = CIRCLE ( 'NONE', #183845, 0.09999999999999939493 ) ;
#184020 = CARTESIAN_POINT ( 'NONE',  ( -23.39999999999994529, 74.16448838626247664, -47.52760213295649550 ) ) ;
#184021 = ORIENTED_EDGE ( 'NONE', *, *, #153056, .T. ) ;
#184022 = DIRECTION ( 'NONE',  ( -1.652117596168391700E-15, 0.9651348961777157509, -0.2617529984165031243 ) ) ;
#184023 = VECTOR ( 'NONE', #241115, 1000.000000000000000 ) ;
#184024 = CARTESIAN_POINT ( 'NONE',  ( 0.000000000000000000, 0.000000000000000000, 0.000000000000000000 ) ) ;
#184025 = CARTESIAN_POINT ( 'NONE',  ( 21.05000000000000071, 36.65892442174935439, -249.5511627012433848 ) ) ;
#184026 = CARTESIAN_POINT ( 'NONE',  ( 20.95429402530550433, 67.12380584890989610, -128.0000207865865320 ) ) ;
#184028 = VECTOR ( 'NONE', #116791, 1000.000000000000000 ) ;
#184027 = DIRECTION ( 'NONE',  ( 1.000000000000000000, 0.000000000000000000, 0.000000000000000000 ) ) ;
#184029 = ORIENTED_EDGE ( 'NONE', *, *, #90839, .T. ) ;
#184030 = AXIS2_PLACEMENT_3D ( 'NONE', #171388, #151805, #128375 ) ;
#184031 = CARTESIAN_POINT ( 'NONE',  ( 19.75857864376268935, 64.35000000001251408, -178.6731074845244507 ) ) ;
#184032 = B_SPLINE_CURVE_WITH_KNOTS ( 'NONE', 3,
 ( #139709, #237549, #138414, #39380, #118901, #79727, #60180, #40674, #74663, #122758 ),
 .UNSPECIFIED., .F., .F.,
 ( 4, 2, 2, 2, 4 ),
 ( 0.000000000000000000, 0.0001584437871625145604, 0.0002376656807437778308, 0.0002772766275344028795, 0.0003168875743250278740 ),
 .UNSPECIFIED. ) ;
#184033 = CARTESIAN_POINT ( 'NONE',  ( 23.04999999999999716, 67.17743825834557470, -112.2731074845243597 ) ) ;
#184034 = CIRCLE ( 'NONE', #34230, 0.5000000000000004441 ) ;
#184035 = CYLINDRICAL_SURFACE ( 'NONE', #70128, 0.09999999999999939493 ) ;
#184036 = CARTESIAN_POINT ( 'NONE',  ( -20.64999999999999858, 68.75000000001158185, -57.27310748452437394 ) ) ;
#184037 = ORIENTED_EDGE ( 'NONE', *, *, #95848, .F. ) ;
#184038 = EDGE_LOOP ( 'NONE', ( #221371, #92054, #30953, #144672, #72620 ) ) ;
#184040 = VECTOR ( 'NONE', #224052, 1000.000000000000000 ) ;
#184039 = CARTESIAN_POINT ( 'NONE',  ( 22.50046968638157452, 75.95483015287189232, -81.27315263899684794 ) ) ;
#184042 = AXIS2_PLACEMENT_3D ( 'NONE', #254819, #71129, #171524 ) ;
#184041 = DIRECTION ( 'NONE',  ( 1.000000000000000000, 0.000000000000000000, 0.000000000000000000 ) ) ;
#184043 = DIRECTION ( 'NONE',  ( 0.000000000000000000, 0.000000000000000000, 1.000000000000000000 ) ) ;
#184044 = DIRECTION ( 'NONE',  ( 0.000000000000000000, -1.000000000000000000, -6.982962677686265922E-15 ) ) ;
#184045 = LINE ( 'NONE', #100623, #16046 ) ;
#184046 = EDGE_CURVE ( 'NONE', #131237, #224599, #25803, .T. ) ;
#184047 = LINE ( 'NONE', #104484, #11747 ) ;
#184048 = VECTOR ( 'NONE', #218745, 1000.000000000000000 ) ;
#184049 = DIRECTION ( 'NONE',  ( 0.000000000000000000, 0.000000000000000000, -1.000000000000000000 ) ) ;
#184050 = CARTESIAN_POINT ( 'NONE',  ( -18.59999999999999787, 1.162701749949165642, -75.10000000000003695 ) ) ;
#184052 = CARTESIAN_POINT ( 'NONE',  ( -18.50000000000000711, 47.12013762176896847, -255.1881735838713610 ) ) ;
#184051 = CIRCLE ( 'NONE', #146438, 0.09999999999999459321 ) ;
#184053 = DIRECTION ( 'NONE',  ( 0.000000000000000000, 0.8814952561688428334, -0.4721928772777349570 ) ) ;
#184055 = ORIENTED_EDGE ( 'NONE', *, *, #29132, .F. ) ;
#184054 = CARTESIAN_POINT ( 'NONE',  ( 15.69410316191958010, 62.70378344720913333, -216.8024073824997799 ) ) ;
#184056 = CARTESIAN_POINT ( 'NONE',  ( 20.95378194480896639, 65.46508800846984855, -195.9580533363765937 ) ) ;
#184057 = DIRECTION ( 'NONE',  ( 0.000000000000000000, 0.000000000000000000, -1.000000000000000000 ) ) ;
#184059 = LINE ( 'NONE', #79802, #140836 ) ;
#184058 = DIRECTION ( 'NONE',  ( -2.602085213965226419E-14, -0.000000000000000000, -1.000000000000000000 ) ) ;
#184060 = VECTOR ( 'NONE', #33671, 1000.000000000000000 ) ;
#184061 = EDGE_CURVE ( 'NONE', #252315, #66860, #115927, .T. ) ;
#184062 = VERTEX_POINT ( 'NONE', #61070 ) ;
#184063 = CARTESIAN_POINT ( 'NONE',  ( -16.84793658983426923, 66.05000000001159322, -56.78946080671413199 ) ) ;
#184064 = DIRECTION ( 'NONE',  ( 0.000000000000000000, 0.2617529984165031243, 0.9651348961777157509 ) ) ;
#184065 = CARTESIAN_POINT ( 'NONE',  ( 23.24999999999999289, 11.65000000000000746, 0.000000000000000000 ) ) ;
#184066 = DIRECTION ( 'NONE',  ( 0.000000000000000000, 0.000000000000000000, -1.000000000000000000 ) ) ;
#184068 = CARTESIAN_POINT ( 'NONE',  ( -12.25000000000000178, 66.65000000001258229, -186.6573643172504831 ) ) ;
#184067 = CIRCLE ( 'NONE', #209013, 0.1000000000000106498 ) ;
#184069 = EDGE_CURVE ( 'NONE', #124845, #71933, #37692, .T. ) ;
#184070 = ORIENTED_EDGE ( 'NONE', *, *, #34408, .F. ) ;
#184071 = ORIENTED_EDGE ( 'NONE', *, *, #14498, .T. ) ;
#184072 = CARTESIAN_POINT ( 'NONE',  ( -20.00857864376270001, 9.250000000011157297, -155.1500000000000057 ) ) ;
#184073 = EDGE_CURVE ( 'NONE', #68947, #83472, #100766, .T. ) ;
#184074 = ORIENTED_EDGE ( 'NONE', *, *, #58026, .F. ) ;
#184076 = FACE_OUTER_BOUND ( 'NONE', #154806, .T. ) ;
#184075 = AXIS2_PLACEMENT_3D ( 'NONE', #4496, #103586, #124475 ) ;
#184077 = CIRCLE ( 'NONE', #250703, 0.1000000000000128147 ) ;
#184078 = ORIENTED_EDGE ( 'NONE', *, *, #164017, .T. ) ;
#184079 = AXIS2_PLACEMENT_3D ( 'NONE', #100976, #161013, #4483 ) ;
#184080 = CARTESIAN_POINT ( 'NONE',  ( -21.07928932188134041, 67.23127455305841238, -235.8551265064783991 ) ) ;
#184081 = AXIS2_PLACEMENT_3D ( 'NONE', #106683, #224071, #107993 ) ;
#184082 = DIRECTION ( 'NONE',  ( -1.000000000000000000, -0.000000000000000000, -0.000000000000000000 ) ) ;
#184083 = CARTESIAN_POINT ( 'NONE',  ( -21.02374657821572868, 62.99095723451760165, -207.1734234075708230 ) ) ;
#184084 = ORIENTED_EDGE ( 'NONE', *, *, #134458, .T. ) ;
#184085 = EDGE_CURVE ( 'NONE', #67538, #176131, #198010, .T. ) ;
#184086 = CYLINDRICAL_SURFACE ( 'NONE', #174622, 0.09999999999999939493 ) ;
#184087 = CARTESIAN_POINT ( 'NONE',  ( -21.04999999999939320, 65.54489249088371139, -242.1291417229003287 ) ) ;
#184088 = FACE_OUTER_BOUND ( 'NONE', #83897, .T. ) ;
#184089 = DIRECTION ( 'NONE',  ( 0.000000000000000000, 0.000000000000000000, 1.000000000000000000 ) ) ;
#184090 = FACE_OUTER_BOUND ( 'NONE', #146007, .T. ) ;
#184091 = DIRECTION ( 'NONE',  ( -1.000000000000000000, 0.000000000000000000, -0.000000000000000000 ) ) ;
#184092 = ORIENTED_EDGE ( 'NONE', *, *, #246555, .T. ) ;
#184093 = CIRCLE ( 'NONE', #59151, 0.09999999999999939493 ) ;
#184095 = DIRECTION ( 'NONE',  ( 0.000000000000000000, 1.000000000000000000, 0.000000000000000000 ) ) ;
#184094 = CARTESIAN_POINT ( 'NONE',  ( -16.92989143108098204, 66.05000000001209060, -123.6406236097677152 ) ) ;
#184096 = ORIENTED_EDGE ( 'NONE', *, *, #19921, .T. ) ;
#184098 = EDGE_LOOP ( 'NONE', ( #174628, #125724, #223279, #126803, #198661, #108891 ) ) ;
#184097 = DIRECTION ( 'NONE',  ( 0.000000000000000000, 0.000000000000000000, -1.000000000000000000 ) ) ;
#184099 = ORIENTED_EDGE ( 'NONE', *, *, #67939, .F. ) ;
#184100 = CYLINDRICAL_SURFACE ( 'NONE', #169905, 0.09999999999999939493 ) ;
#184101 = DIRECTION ( 'NONE',  ( 0.000000000000000000, -0.000000000000000000, 1.000000000000000000 ) ) ;
#184102 = CARTESIAN_POINT ( 'NONE',  ( -20.64999999999999858, 62.08591502004791352, -248.5699171172615820 ) ) ;
#184103 = DIRECTION ( 'NONE',  ( -1.000000000000000000, -0.000000000000000000, -0.000000000000000000 ) ) ;
#184104 = ORIENTED_EDGE ( 'NONE', *, *, #61952, .T. ) ;
#184105 = DIRECTION ( 'NONE',  ( 1.000000000000000000, 0.000000000000000000, 0.000000000000000000 ) ) ;
#184106 = CARTESIAN_POINT ( 'NONE',  ( 21.05000000000000071, 11.65000000001116298, -100.5000000000000284 ) ) ;
#184107 = VERTEX_POINT ( 'NONE', #59765 ) ;
#184108 = CARTESIAN_POINT ( 'NONE',  ( -20.93302460841142931, 10.31565961586829872, -39.03641941191782649 ) ) ;
#184109 = DIRECTION ( 'NONE',  ( 0.000000000000000000, -1.000000000000000000, -8.609265936414504429E-15 ) ) ;
#184110 = EDGE_LOOP ( 'NONE', ( #218570, #57204, #104684, #32207 ) ) ;
#184111 = DIRECTION ( 'NONE',  ( 0.000000000000000000, 0.000000000000000000, -1.000000000000000000 ) ) ;
#184112 = ADVANCED_FACE ( 'NONE', ( #199318 ), #254873, .F. ) ;
#184113 = VERTEX_POINT ( 'NONE', #19393 ) ;
#184114 = DIRECTION ( 'NONE',  ( 4.408576920032447355E-17, -0.1350103645451876666, 0.9908441862701600211 ) ) ;
#184115 = ORIENTED_EDGE ( 'NONE', *, *, #54576, .T. ) ;
#184116 = DIRECTION ( 'NONE',  ( 1.186688945009010077E-16, 1.000000000000000000, 6.982962677686266711E-15 ) ) ;
#184117 = CARTESIAN_POINT ( 'NONE',  ( -21.56666275994539816, 1.115600667400684642E-11, -127.0426315931066910 ) ) ;
#184119 = CARTESIAN_POINT ( 'NONE',  ( -1.739115166359751801E-14, 64.35000000001187459, -90.77310748452438816 ) ) ;
#184118 =( REPRESENTATION_RELATIONSHIP ('NONE','NONE', #36900, #108449 ) REPRESENTATION_RELATIONSHIP_WITH_TRANSFORMATION ( #89748 )SHAPE_REPRESENTATION_RELATIONSHIP( ) );
#184120 = EDGE_CURVE ( 'NONE', #125280, #27505, #153763, .T. ) ;
#184121 = CARTESIAN_POINT ( 'NONE',  ( 18.49999999999999645, 77.63717271298195044, -57.94095411905229298 ) ) ;
#184122 = EDGE_CURVE ( 'NONE', #116070, #164389, #175920, .T. ) ;
#184123 = EDGE_CURVE ( 'NONE', #149328, #100941, #234081, .T. ) ;
#184124 = CIRCLE ( 'NONE', #71730, 11.80000000000000426 ) ;
#184125 = CARTESIAN_POINT ( 'NONE',  ( 20.12500000000000000, 66.25000000001179501, -81.77310748452437394 ) ) ;
#184126 = CARTESIAN_POINT ( 'NONE',  ( 21.05000000000000071, 69.65000000001158753, -59.67928539484124428 ) ) ;
#184127 = DIRECTION ( 'NONE',  ( -1.000000000000000000, 0.000000000000000000, -0.000000000000000000 ) ) ;
#184129 = ORIENTED_EDGE ( 'NONE', *, *, #116277, .F. ) ;
#184128 = AXIS2_PLACEMENT_3D ( 'NONE', #215524, #36935, #116443 ) ;
#184130 = CARTESIAN_POINT ( 'NONE',  ( 23.14999999999999858, 7.128833340094563376, -233.7327013124401276 ) ) ;
#184131 = VERTEX_POINT ( 'NONE', #255369 ) ;
#184132 = FACE_OUTER_BOUND ( 'NONE', #30901, .T. ) ;
#184133 = DIRECTION ( 'NONE',  ( 0.000000000000000000, 0.000000000000000000, -1.000000000000000000 ) ) ;
#184137 = EDGE_CURVE ( 'NONE', #25096, #226829, #196731, .T. ) ;
#184136 = ORIENTED_EDGE ( 'NONE', *, *, #13854, .T. ) ;
#184135 = DIRECTION ( 'NONE',  ( 0.000000000000000000, -6.688090509790120484E-15, 1.000000000000000000 ) ) ;
#184134 =( BOUNDED_SURFACE ( )  B_SPLINE_SURFACE ( 3, 2, ( 
 ( #256139, #3151, #197508 ),
 ( #18876, #580, #97092 ),
 ( #98370, #158430, #121849 ),
 ( #138785, #201369, #177973 ),
 ( #22764, #80098, #82671 ),
 ( #219640, #102230, #77543 ) ),
 .UNSPECIFIED., .F., .F., .F. ) 
 B_SPLINE_SURFACE_WITH_KNOTS ( ( 4, 2, 4 ),
 ( 3, 3 ),
 ( 0.0001300404313046550988, 0.0003183318589266453426, 0.0005066232865486356134 ),
 ( 0.000000000000000000, 1.000000000000000000 ),
 .UNSPECIFIED. ) 
 GEOMETRIC_REPRESENTATION_ITEM ( )  RATIONAL_B_SPLINE_SURFACE ( (
 ( 1.000000000000000000, 0.7071067811865719976, 1.000000000000000000),
 ( 1.000000000000000000, 0.7625113560537848389, 1.000000000000000000),
 ( 1.000000000000000000, 0.8126073484691938020, 1.000000000000000000),
 ( 1.000000000000000000, 0.8923049332728831828, 1.000000000000000000),
 ( 1.000000000000000000, 0.9231914937772871532, 1.000000000000000000),
 ( 1.000000000000000000, 0.9238795325112716395, 1.000000000000000000) ) ) 
 REPRESENTATION_ITEM ( '' )  SURFACE ( )  );
#184139 = ORIENTED_EDGE ( 'NONE', *, *, #15148, .T. ) ;
#184138 = DIRECTION ( 'NONE',  ( 0.000000000000000000, -0.4088369013363280513, 0.9126074666063769270 ) ) ;
#184140 = EDGE_CURVE ( 'NONE', #157401, #235855, #97605, .T. ) ;
#184141 = LINE ( 'NONE', #83725, #256050 ) ;
#184142 = CARTESIAN_POINT ( 'NONE',  ( -20.01715728752537871, 5.586869315528661062, 16.41686199900910736 ) ) ;
#184143 = CARTESIAN_POINT ( 'NONE',  ( 20.99999999999999645, 41.11438369982452912, -236.8714985644722617 ) ) ;
#184144 = EDGE_CURVE ( 'NONE', #208027, #143163, #157658, .T. ) ;
#184145 = DIRECTION ( 'NONE',  ( -1.000000000000000000, -0.000000000000000000, -0.000000000000000000 ) ) ;
#184147 = EDGE_LOOP ( 'NONE', ( #104376, #36271 ) ) ;
#184146 = CARTESIAN_POINT ( 'NONE',  ( -17.01825945287481545, 9.950000000011138823, -188.2499999999999716 ) ) ;
#184148 = AXIS2_PLACEMENT_3D ( 'NONE', #223983, #7514, #124904 ) ;
#184149 = VECTOR ( 'NONE', #143443, 1000.000000000000000 ) ;
#184151 = EDGE_CURVE ( 'NONE', #32139, #191879, #250998, .T. ) ;
#184150 = DIRECTION ( 'NONE',  ( 0.000000000000000000, 0.000000000000000000, -1.000000000000000000 ) ) ;
#184152 = ORIENTED_EDGE ( 'NONE', *, *, #179929, .F. ) ;
#184153 = ORIENTED_EDGE ( 'NONE', *, *, #244399, .T. ) ;
#184154 = ADVANCED_FACE ( 'NONE', ( #106270 ), #30636, .F. ) ;
#184155 = EDGE_CURVE ( 'NONE', #167941, #248236, #146674, .T. ) ;
#184156 = DIRECTION ( 'NONE',  ( 0.000000000000000000, 6.982962677686266711E-15, -1.000000000000000000 ) ) ;
#184157 = ADVANCED_FACE ( 'NONE', ( #125843 ), #163544, .T. ) ;
#184158 = ORIENTED_EDGE ( 'NONE', *, *, #244079, .T. ) ;
#184159 = AXIS2_PLACEMENT_3D ( 'NONE', #255598, #215245, #195707 ) ;
#184160 = VECTOR ( 'NONE', #214228, 1000.000000000000000 ) ;
#184161 = CYLINDRICAL_SURFACE ( 'NONE', #7677, 0.09999999999999939493 ) ;
#184162 = VECTOR ( 'NONE', #172573, 1000.000000000000000 ) ;
#184163 = EDGE_LOOP ( 'NONE', ( #46628, #204763, #122728, #131874 ) ) ;
#184164 = CARTESIAN_POINT ( 'NONE',  ( -21.05000000000000071, 87.65000000001214175, -136.5231074845242176 ) ) ;
#184165 = LINE ( 'NONE', #190298, #251204 ) ;
#184166 = ORIENTED_EDGE ( 'NONE', *, *, #184085, .F. ) ;
#184167 = ORIENTED_EDGE ( 'NONE', *, *, #133631, .T. ) ;
#184168 = CARTESIAN_POINT ( 'NONE',  ( -18.49372193242239959, -9.442484523346879044, -73.76478126003453895 ) ) ;
#184169 = EDGE_CURVE ( 'NONE', #162626, #250243, #159286, .T. ) ;
#184170 = ORIENTED_EDGE ( 'NONE', *, *, #162199, .T. ) ;
#184171 = EDGE_CURVE ( 'NONE', #244003, #88477, #92612, .T. ) ;
#184172 = CARTESIAN_POINT ( 'NONE',  ( 16.87683809663750267, 9.950000000011138823, -180.1499999999999773 ) ) ;
#184173 = ORIENTED_EDGE ( 'NONE', *, *, #16454, .T. ) ;
#184174 = ORIENTED_EDGE ( 'NONE', *, *, #70239, .F. ) ;
#184175 = AXIS2_PLACEMENT_3D ( 'NONE', #251443, #35009, #37548 ) ;
#184176 = CARTESIAN_POINT ( 'NONE',  ( -21.03922262424656253, 11.62390063401577933, -73.85920804289372654 ) ) ;
#184177 = ORIENTED_EDGE ( 'NONE', *, *, #221528, .F. ) ;
#184178 = CARTESIAN_POINT ( 'NONE',  ( 22.49999999999999645, 0.1008583691098678403, -88.75043287651062940 ) ) ;
#184179 = VERTEX_POINT ( 'NONE', #26789 ) ;
#184182 = ADVANCED_FACE ( 'NONE', ( #5891 ), #46812, .T. ) ;
#184181 = EDGE_LOOP ( 'NONE', ( #219040, #113426 ) ) ;
#184180 = VERTEX_POINT ( 'NONE', #206681 ) ;
#184183 = DIRECTION ( 'NONE',  ( 0.000000000000000000, 0.8814952561688476074, -0.4721928772777262417 ) ) ;
#184184 = CARTESIAN_POINT ( 'NONE',  ( -16.94165728009538086, 14.20474050515682940, -219.2871285009821634 ) ) ;
#184185 = EDGE_LOOP ( 'NONE', ( #156065, #111541, #158969, #162169 ) ) ;
#184186 = AXIS2_PLACEMENT_3D ( 'NONE', #53714, #212804, #253192 ) ;
#184187 = EDGE_LOOP ( 'NONE', ( #5287, #123454, #86361, #221984 ) ) ;
#184188 = SPHERICAL_SURFACE ( 'NONE', #257607, 0.1000000000000000056 ) ;
#184190 = CARTESIAN_POINT ( 'NONE',  ( -20.94999999999999929, 87.48912529308798014, -106.1231074845242262 ) ) ;
#184189 = VECTOR ( 'NONE', #109484, 1000.000000000000000 ) ;
#184192 = ORIENTED_EDGE ( 'NONE', *, *, #254176, .T. ) ;
#184191 = CARTESIAN_POINT ( 'NONE',  ( 20.94999999999999929, 76.00000000001213607, -136.5231074845243313 ) ) ;
#184193 = DIRECTION ( 'NONE',  ( 0.7071067811865474617, 0.7071067811865474617, -0.000000000000000000 ) ) ;
#184194 = ORIENTED_EDGE ( 'NONE', *, *, #211385, .T. ) ;
#184195 = DIRECTION ( 'NONE',  ( 0.000000000000000000, 0.7106264324241465813, -0.7035695228903324772 ) ) ;
#184196 = CARTESIAN_POINT ( 'NONE',  ( -20.94999999999999929, 64.21185867012613357, -224.4479740254296303 ) ) ;
#184197 = CIRCLE ( 'NONE', #50907, 0.09999999999998898659 ) ;
#184199 = ORIENTED_EDGE ( 'NONE', *, *, #188763, .F. ) ;
#184198 = EDGE_CURVE ( 'NONE', #73105, #138276, #28074, .T. ) ;
#184200 = CARTESIAN_POINT ( 'NONE',  ( -22.50000000000000000, 64.35042919246686210, -69.62310748452439668 ) ) ;
#184201 = CARTESIAN_POINT ( 'NONE',  ( -23.15000000000000213, 4.350000000011156054, -146.3500000000000227 ) ) ;
#184202 = CIRCLE ( 'NONE', #71811, 0.09999999999999949207 ) ;
#184203 = AXIS2_PLACEMENT_3D ( 'NONE', #215162, #234730, #198163 ) ;
#184204 = EDGE_CURVE ( 'NONE', #17857, #126912, #246731, .T. ) ;
#184206 = EDGE_LOOP ( 'NONE', ( #253433, #244817 ) ) ;
#184205 = CIRCLE ( 'NONE', #55014, 0.09999999999998898659 ) ;
#184207 = CYLINDRICAL_SURFACE ( 'NONE', #222080, 0.09999999999999939493 ) ;
#184208 = EDGE_LOOP ( 'NONE', ( #114317, #93695, #249545, #69006 ) ) ;
#184209 = CIRCLE ( 'NONE', #255067, 12.87499999999999822 ) ;
#184210 = AXIS2_PLACEMENT_3D ( 'NONE', #194111, #134098, #231955 ) ;
#184211 = EDGE_CURVE ( 'NONE', #90311, #26818, #250413, .T. ) ;
#184213 = ORIENTED_EDGE ( 'NONE', *, *, #150697, .F. ) ;
#184212 = ORIENTED_EDGE ( 'NONE', *, *, #231279, .T. ) ;
#184214 = EDGE_LOOP ( 'NONE', ( #91002, #236742, #93045, #52334, #2717, #24795, #82644 ) ) ;
#184216 = EDGE_CURVE ( 'NONE', #114885, #30145, #67677, .T. ) ;
#184215 = CARTESIAN_POINT ( 'NONE',  ( -21.05000000000000426, -0.02103547652895631712, -127.6955441780524012 ) ) ;
#184217 = EDGE_LOOP ( 'NONE', ( #68520, #58269, #243637, #92420 ) ) ;
#184218 = DIRECTION ( 'NONE',  ( 0.000000000000000000, -0.9126074666064812879, -0.4088369013360954596 ) ) ;
#184219 = ORIENTED_EDGE ( 'NONE', *, *, #212162, .F. ) ;
#184220 = CARTESIAN_POINT ( 'NONE',  ( -20.00857864376270001, 9.150000000011157653, -146.3500000000000227 ) ) ;
#184221 = ADVANCED_FACE ( 'NONE', ( #187140 ), #168883, .T. ) ;
#184222 = CIRCLE ( 'NONE', #84214, 0.1000000000000011990 ) ;
#184223 = CARTESIAN_POINT ( 'NONE',  ( 23.24999999999999645, 8.822561741677553471, -121.3500000000000227 ) ) ;
#184225 = ORIENTED_EDGE ( 'NONE', *, *, #111455, .T. ) ;
#184224 = VECTOR ( 'NONE', #190473, 1000.000000000000000 ) ;
#184226 = ORIENTED_EDGE ( 'NONE', *, *, #113244, .F. ) ;
#184227 = CIRCLE ( 'NONE', #109207, 0.09999999999998898659 ) ;
#184228 = VECTOR ( 'NONE', #256700, 1000.000000000000000 ) ;
#184229 = AXIS2_PLACEMENT_3D ( 'NONE', #31741, #250742, #173835 ) ;
#184230 = ORIENTED_EDGE ( 'NONE', *, *, #161914, .T. ) ;
#184231 = EDGE_CURVE ( 'NONE', #201531, #19748, #71045, .T. ) ;
#184232 = EDGE_CURVE ( 'NONE', #19933, #188240, #21899, .T. ) ;
#184233 = CIRCLE ( 'NONE', #130249, 0.6000000000000033085 ) ;
#184235 =( BOUNDED_SURFACE ( )  B_SPLINE_SURFACE ( 3, 2, ( 
 ( #199320, #20695, #100175 ),
 ( #194197, #16839, #54651 ),
 ( #213733, #15565, #95068 ),
 ( #62373, #85737, #225262 ) ),
 .UNSPECIFIED., .F., .F., .F. ) 
 B_SPLINE_SURFACE_WITH_KNOTS ( ( 4, 4 ),
 ( 3, 3 ),
 ( 0.04058434257139475337, 0.04256401539001600232 ),
 ( 0.000000000000000000, 1.000000000000000000 ),
 .UNSPECIFIED. ) 
 GEOMETRIC_REPRESENTATION_ITEM ( )  RATIONAL_B_SPLINE_SURFACE ( (
 ( 1.000000000000000000, 0.7103081912008297749, 1.000000000000000000),
 ( 1.000000000000000000, 0.7104998333555460066, 1.000000000000000000),
 ( 1.000000000000000000, 0.7107238315755025626, 1.000000000000000000),
 ( 1.000000000000000000, 0.7110073749539292942, 1.000000000000000000) ) ) 
 REPRESENTATION_ITEM ( '' )  SURFACE ( )  );
#184234 = VECTOR ( 'NONE', #191126, 1000.000000000000000 ) ;
#184236 = CARTESIAN_POINT ( 'NONE',  ( 23.14999999999999503, 6.650000000011155876, -45.65000000000000568 ) ) ;
#184237 = ORIENTED_EDGE ( 'NONE', *, *, #197533, .T. ) ;
#184238 = EDGE_CURVE ( 'NONE', #221150, #173825, #100944, .T. ) ;
#184239 = DIRECTION ( 'NONE',  ( 0.000000000000000000, -1.000000000000000000, -8.609265936414504429E-15 ) ) ;
#184240 = AXIS2_PLACEMENT_3D ( 'NONE', #38659, #196434, #178191 ) ;
#184242 = ORIENTED_EDGE ( 'NONE', *, *, #152780, .F. ) ;
#184241 = DIRECTION ( 'NONE',  ( 0.000000000000000000, 0.000000000000000000, 1.000000000000000000 ) ) ;
#184243 = PLANE ( 'NONE',  #34563 ) ;
#184244 = DIRECTION ( 'NONE',  ( 1.000000000000000000, 0.000000000000000000, 0.000000000000000000 ) ) ;
#184245 = CARTESIAN_POINT ( 'NONE',  ( -20.85000000000000142, 68.97833521811159585, -65.68954208262705663 ) ) ;
#184247 = DIRECTION ( 'NONE',  ( -1.000000000000000000, 0.000000000000000000, 0.000000000000000000 ) ) ;
#184246 = DIRECTION ( 'NONE',  ( 1.296989514748957922E-15, -0.9887567792719341719, 0.1495327102803664099 ) ) ;
#184248 = FACE_OUTER_BOUND ( 'NONE', #84778, .T. ) ;
#184249 = DIRECTION ( 'NONE',  ( 1.000000000000000000, 0.000000000000000000, 0.000000000000000000 ) ) ;
#184250 = DIRECTION ( 'NONE',  ( 0.000000000000000000, 0.000000000000000000, -1.000000000000000000 ) ) ;
#184251 = EDGE_CURVE ( 'NONE', #151819, #159539, #59291, .T. ) ;
#184252 = CIRCLE ( 'NONE', #254922, 11.75000000000001066 ) ;
#184254 = ORIENTED_EDGE ( 'NONE', *, *, #147346, .T. ) ;
#184253 = CIRCLE ( 'NONE', #109233, 0.09999999999999609201 ) ;
#184255 = TOROIDAL_SURFACE ( 'NONE', #150948, 11.70000000000000462, 0.1000000000000000056 ) ;
#184256 = EDGE_CURVE ( 'NONE', #183881, #100350, #63575, .T. ) ;
#184258 = ORIENTED_EDGE ( 'NONE', *, *, #123670, .F. ) ;
#184257 = DIRECTION ( 'NONE',  ( -1.000000000000000000, 7.492892343619937423E-30, -1.073024830501117725E-15 ) ) ;
#184259 = ORIENTED_EDGE ( 'NONE', *, *, #74480, .F. ) ;
#184260 = DIRECTION ( 'NONE',  ( 0.000000000000000000, -1.734723475976757554E-14, -1.000000000000000000 ) ) ;
#184261 = EDGE_CURVE ( 'NONE', #188649, #239049, #17770, .T. ) ;
#184262 = SPHERICAL_SURFACE ( 'NONE', #127916, 0.1000000000000000056 ) ;
#184263 = DIRECTION ( 'NONE',  ( 0.000000000000000000, 0.1618390714546044939, 0.9868171638914228216 ) ) ;
#184264 = EDGE_CURVE ( 'NONE', #163442, #89935, #210537, .T. ) ;
#184265 = ORIENTED_EDGE ( 'NONE', *, *, #252667, .F. ) ;
#184266 =( NAMED_UNIT ( * ) SI_UNIT ( $, .STERADIAN. ) SOLID_ANGLE_UNIT ( ) );
#184267 = DIRECTION ( 'NONE',  ( 0.7071067811865463515, -0.7071067811865487940, -5.696443396193425170E-15 ) ) ;
#184268 = DIRECTION ( 'NONE',  ( 1.073024830501117725E-15, -6.982962677686266711E-15, 1.000000000000000000 ) ) ;
#184269 = CIRCLE ( 'NONE', #101020, 0.1000000000000026007 ) ;
#184270 = EDGE_LOOP ( 'NONE', ( #120180, #222772, #29817, #135813, #174966, #207018, #104554, #30245, #18851 ) ) ;
#184271 = DIRECTION ( 'NONE',  ( 1.000000000000000000, 0.000000000000000000, 0.000000000000000000 ) ) ;
#184272 = DIRECTION ( 'NONE',  ( -0.000000000000000000, 1.000000000000000000, 0.000000000000000000 ) ) ;
#184273 = DIRECTION ( 'NONE',  ( 0.000000000000000000, 0.8814952561688476074, -0.4721928772777262417 ) ) ;
#184274 = CIRCLE ( 'NONE', #213501, 0.09999999999999939493 ) ;
#184275 = EDGE_CURVE ( 'NONE', #235864, #86355, #113472, .T. ) ;
#184277 = ORIENTED_EDGE ( 'NONE', *, *, #8450, .F. ) ;
#184276 = CARTESIAN_POINT ( 'NONE',  ( -20.86777300164945004, 67.49225400653517681, -195.4205142095401868 ) ) ;
#184278 = LINE ( 'NONE', #125591, #190143 ) ;
#184279 = DIRECTION ( 'NONE',  ( 0.000000000000000000, -3.339342691255721203E-13, 1.000000000000000000 ) ) ;
#184280 = CARTESIAN_POINT ( 'NONE',  ( -20.07928932188135107, 9.220710678129810489, -146.3500000000000227 ) ) ;
#184281 = DIRECTION ( 'NONE',  ( 1.000000000000000000, 0.000000000000000000, 0.000000000000000000 ) ) ;
#184282 = ORIENTED_EDGE ( 'NONE', *, *, #233697, .T. ) ;
#184283 = CARTESIAN_POINT ( 'NONE',  ( -23.15000000000000213, 76.00000000001165290, -69.52310748452431710 ) ) ;
#184284 = CARTESIAN_POINT ( 'NONE',  ( -20.64999999999999858, 9.712035112405693837, -211.5243229699422614 ) ) ;
#184286 = CYLINDRICAL_SURFACE ( 'NONE', #20298, 0.1000000000000054040 ) ;
#184285 = LINE ( 'NONE', #121774, #24204 ) ;
#184287 = FACE_OUTER_BOUND ( 'NONE', #130750, .T. ) ;
#184288 = PLANE ( 'NONE',  #199220 ) ;
#184289 = DIRECTION ( 'NONE',  ( 0.000000000000000000, -0.2605042016806740079, 0.9654727137038698892 ) ) ;
#184290 = FACE_OUTER_BOUND ( 'NONE', #97127, .T. ) ;
#184291 = DIRECTION ( 'NONE',  ( -0.000000000000000000, -1.000000000000000000, -6.982962677686266711E-15 ) ) ;
#184292 = ORIENTED_EDGE ( 'NONE', *, *, #165921, .T. ) ;
#184294 = AXIS2_PLACEMENT_3D ( 'NONE', #177979, #78841, #75047 ) ;
#184293 = FACE_OUTER_BOUND ( 'NONE', #18844, .T. ) ;
#184295 = VERTEX_POINT ( 'NONE', #116571 ) ;
#184296 = ORIENTED_EDGE ( 'NONE', *, *, #205097, .F. ) ;
#184297 = EDGE_CURVE ( 'NONE', #97495, #218378, #250827, .T. ) ;
#184298 = CARTESIAN_POINT ( 'NONE',  ( -20.85000000000000142, 77.16412189325305349, -95.10825939895268277 ) ) ;
#184299 = DIRECTION ( 'NONE',  ( -1.000000000000000000, -0.000000000000000000, -0.000000000000000000 ) ) ;
#184300 = ORIENTED_EDGE ( 'NONE', *, *, #140285, .F. ) ;
#184301 = ORIENTED_EDGE ( 'NONE', *, *, #57206, .F. ) ;
#184302 = AXIS2_PLACEMENT_3D ( 'NONE', #173184, #251377, #235657 ) ;
#184303 = ADVANCED_FACE ( 'NONE', ( #72322 ), #192270, .F. ) ;
#184304 = ORIENTED_EDGE ( 'NONE', *, *, #3981, .F. ) ;
#184305 = DIRECTION ( 'NONE',  ( 0.000000000000000000, -0.4930308989874653269, -0.8700118002898649117 ) ) ;
#184306 = ORIENTED_EDGE ( 'NONE', *, *, #17466, .F. ) ;
#184307 = AXIS2_PLACEMENT_3D ( 'NONE', #224198, #105507, #245057 ) ;
#184308 = FACE_OUTER_BOUND ( 'NONE', #28670, .T. ) ;
#184309 = FACE_OUTER_BOUND ( 'NONE', #45334, .T. ) ;
#184310 = CARTESIAN_POINT ( 'NONE',  ( -18.50000000000000000, -1.866714910046153308, -78.75267524628205251 ) ) ;
#184311 = CYLINDRICAL_SURFACE ( 'NONE', #136481, 0.1000000000000024342 ) ;
#184312 = TOROIDAL_SURFACE ( 'NONE', #217617, 11.65000000000000036, 0.1000000000000000056 ) ;
#184313 = DIRECTION ( 'NONE',  ( -0.000000000000000000, -0.8700118002898321601, 0.4930308989875230030 ) ) ;
#184314 = CARTESIAN_POINT ( 'NONE',  ( -18.50000000000000000, 11.75000000001115552, -179.6499999999999773 ) ) ;
#184316 = ORIENTED_EDGE ( 'NONE', *, *, #19670, .F. ) ;
#184315 = CARTESIAN_POINT ( 'NONE',  ( -20.94999999999999929, 1.116121084443477685E-11, -136.9000000000000057 ) ) ;
#184318 = DIRECTION ( 'NONE',  ( -1.000000000000000000, -1.794895427898103559E-16, -3.909090864890002444E-17 ) ) ;
#184317 = FACE_OUTER_BOUND ( 'NONE', #86301, .T. ) ;
#184319 = FACE_BOUND ( 'NONE', #43474, .T. ) ;
#184320 = ORIENTED_EDGE ( 'NONE', *, *, #180284, .T. ) ;
#184321 = DIRECTION ( 'NONE',  ( 1.000000000000000000, 0.000000000000000000, 0.000000000000000000 ) ) ;
#184322 = DIRECTION ( 'NONE',  ( -0.000000000000000000, 0.000000000000000000, 1.000000000000000000 ) ) ;
#184323 = ORIENTED_EDGE ( 'NONE', *, *, #166001, .F. ) ;
#184324 = AXIS2_PLACEMENT_3D ( 'NONE', #190380, #166014, #151247 ) ;
#184327 = CARTESIAN_POINT ( 'NONE',  ( -21.09610168723073187, 6.378955715235940183, -33.46641049310851201 ) ) ;
#184326 = AXIS2_PLACEMENT_3D ( 'NONE', #46895, #106876, #129030 ) ;
#184325 = DIRECTION ( 'NONE',  ( 0.000000000000000000, -6.789366196018718420E-15, 1.000000000000000000 ) ) ;
#184328 = DIRECTION ( 'NONE',  ( 0.000000000000000000, 2.891205793294679805E-16, -1.000000000000000000 ) ) ;
#184329 = EDGE_LOOP ( 'NONE', ( #88922, #127807, #62251, #45314 ) ) ;
#184330 = CARTESIAN_POINT ( 'NONE',  ( 21.05000000000000071, 6.540656951712400691, -67.00000000000004263 ) ) ;
#184331 = DIRECTION ( 'NONE',  ( 1.000000000000000000, 0.000000000000000000, 0.000000000000000000 ) ) ;
#184332 = VECTOR ( 'NONE', #53607, 1000.000000000000000 ) ;
#184333 = DIRECTION ( 'NONE',  ( -1.000000000000000000, -0.000000000000000000, -0.000000000000000000 ) ) ;
#184334 = CARTESIAN_POINT ( 'NONE',  ( -23.15000000000000213, 11.75000000000000000, -12.15000000000000036 ) ) ;
#184335 = VERTEX_POINT ( 'NONE', #74904 ) ;
#184336 = VERTEX_POINT ( 'NONE', #151873 ) ;
#184337 = CIRCLE ( 'NONE', #155175, 3.999999999999996447 ) ;
#184338 = AXIS2_PLACEMENT_3D ( 'NONE', #214608, #15144, #193776 ) ;
#184340 = ADVANCED_FACE ( 'NONE', ( #254746, #157001 ), #13621, .T. ) ;
#184339 = VECTOR ( 'NONE', #6720, 1000.000000000000000 ) ;
#184341 = CIRCLE ( 'NONE', #255217, 11.90000000000000391 ) ;
#184342 = CARTESIAN_POINT ( 'NONE',  ( 21.05000000000000071, 67.22371710471938400, -90.87310748452436826 ) ) ;
#184343 = CARTESIAN_POINT ( 'NONE',  ( 21.05000000000000071, 10.42338541492406279, -40.99205192387010044 ) ) ;
#184344 = CARTESIAN_POINT ( 'NONE',  ( 21.05000000000000071, 69.74218538953624602, -170.1208977758331855 ) ) ;
#184345 = DIRECTION ( 'NONE',  ( 1.000000000000000000, 0.000000000000000000, 0.000000000000000000 ) ) ;
#184346 = DIRECTION ( 'NONE',  ( -1.000000000000000000, -1.394253735153569469E-16, -2.602809386958778209E-16 ) ) ;
#184347 = LINE ( 'NONE', #30441, #88652 ) ;
#184348 = ORIENTED_EDGE ( 'NONE', *, *, #54643, .T. ) ;
#184349 = CARTESIAN_POINT ( 'NONE',  ( -20.92356734117541706, 65.68026841930900162, -97.47257401318893244 ) ) ;
#184351 = ORIENTED_EDGE ( 'NONE', *, *, #134141, .T. ) ;
#184350 = DIRECTION ( 'NONE',  ( -1.000000000000000000, 0.000000000000000000, 0.000000000000000000 ) ) ;
#184352 = DIRECTION ( 'NONE',  ( -0.000000000000000000, -1.000000000000000000, -6.982962677686266711E-15 ) ) ;
#184353 = CARTESIAN_POINT ( 'NONE',  ( -6.099999999999939249, 64.35000000001120668, -51.02310748452479316 ) ) ;
#184354 = CARTESIAN_POINT ( 'NONE',  ( -21.08884785362073089, 75.95021690494498046, -75.88030085194994001 ) ) ;
#184355 = CARTESIAN_POINT ( 'NONE',  ( 20.04142135623730070, 11.65000000000000391, -21.35000000000000142 ) ) ;
#184356 = EDGE_CURVE ( 'NONE', #118795, #165206, #242644, .T. ) ;
#184357 = DIRECTION ( 'NONE',  ( -0.000000000000000000, -0.2605042016806452532, -0.9654727137038777718 ) ) ;
#184359 = ORIENTED_EDGE ( 'NONE', *, *, #97713, .F. ) ;
#184358 = DIRECTION ( 'NONE',  ( 0.000000000000000000, -6.982962677686266711E-15, 1.000000000000000000 ) ) ;
#184360 = CYLINDRICAL_SURFACE ( 'NONE', #63178, 0.09999999999999939493 ) ;
#184361 = CARTESIAN_POINT ( 'NONE',  ( 21.14261333020286671, 10.71569264926606202, -179.7500000000001990 ) ) ;
#184362 = DIRECTION ( 'NONE',  ( -1.000000000000000000, 0.000000000000000000, 0.000000000000000000 ) ) ;
#184363 = DIRECTION ( 'NONE',  ( 0.000000000000000000, 1.224646799142185182E-16, 1.000000000000000000 ) ) ;
#184364 = EDGE_CURVE ( 'NONE', #203380, #239517, #124462, .T. ) ;
#184365 = VERTEX_POINT ( 'NONE', #136096 ) ;
#184366 = DIRECTION ( 'NONE',  ( 0.000000000000000000, 1.000000000000000000, 0.000000000000000000 ) ) ;
#184367 = CARTESIAN_POINT ( 'NONE',  ( -16.87683809663752044, 66.05000000001201954, -116.4254715027206828 ) ) ;
#184368 = CARTESIAN_POINT ( 'NONE',  ( 22.59080734064467677, 11.75000000001115552, -100.4692502919029664 ) ) ;
#184369 = AXIS2_PLACEMENT_3D ( 'NONE', #193874, #230425, #131319 ) ;
#184370 = CARTESIAN_POINT ( 'NONE',  ( 22.57320508075687115, 11.75000000001115552, -167.4999999999999716 ) ) ;
#184371 = EDGE_CURVE ( 'NONE', #54998, #57631, #115278, .T. ) ;
#184372 = EDGE_LOOP ( 'NONE', ( #117575, #179063, #231465 ) ) ;
#184373 = CIRCLE ( 'NONE', #5288, 0.1000000000000033362 ) ;
#184374 = CARTESIAN_POINT ( 'NONE',  ( -20.54999999999999716, 73.50000000001186606, -89.79848556176223440 ) ) ;
#184375 = EDGE_LOOP ( 'NONE', ( #208279, #189404, #146349, #80865 ) ) ;
#184376 = EDGE_CURVE ( 'NONE', #116906, #242879, #117749, .T. ) ;
#184377 = DIRECTION ( 'NONE',  ( 0.000000000000000000, -1.000000000000000000, 0.000000000000000000 ) ) ;
#184378 = CYLINDRICAL_SURFACE ( 'NONE', #108396, 0.09999999999999939493 ) ;
#184379 = B_SPLINE_CURVE_WITH_KNOTS ( 'NONE', 3,
 ( #223608, #141520, #202782, #119406, #238052, #24168, #44999, #103659, #124547, #257563, #59384, #221052, #200223, #121969, #3279, #41175 ),
 .UNSPECIFIED., .F., .F.,
 ( 4, 3, 3, 3, 3, 4 ),
 ( 0.000000000000000000, 2.209833635978175731E-05, 5.595056164117426028E-05, 8.979992002653444747E-05, 0.0001236482757198794019, 0.0001574984039362407678 ),
 .UNSPECIFIED. ) ;
#184380 = CIRCLE ( 'NONE', #71972, 0.09999999999998898659 ) ;
#184381 = DIRECTION ( 'NONE',  ( -1.000000000000000000, -7.304098846218134667E-16, 0.000000000000000000 ) ) ;
#184382 = CARTESIAN_POINT ( 'NONE',  ( -21.05000000000000071, -0.09999999998884338825, -122.3500000000000085 ) ) ;
#184383 = VERTEX_POINT ( 'NONE', #56558 ) ;
#184384 = EDGE_CURVE ( 'NONE', #56204, #46280, #37062, .T. ) ;
#184385 = AXIS2_PLACEMENT_3D ( 'NONE', #192362, #52834, #151979 ) ;
#184387 = EDGE_CURVE ( 'NONE', #116858, #72339, #155207, .T. ) ;
#184386 = AXIS2_PLACEMENT_3D ( 'NONE', #23204, #203094, #222638 ) ;
#184388 = CARTESIAN_POINT ( 'NONE',  ( -21.14999999999994174, 64.35000000001120668, -3.123107484524795474 ) ) ;
#184389 = AXIS2_PLACEMENT_3D ( 'NONE', #240052, #140960, #3994 ) ;
#184390 = DIRECTION ( 'NONE',  ( 0.000000000000000000, 1.000000000000000000, 7.272083257015735086E-15 ) ) ;
#184391 = FACE_BOUND ( 'NONE', #14276, .T. ) ;
#184392 = LINE ( 'NONE', #83964, #182189 ) ;
#184393 = ORIENTED_EDGE ( 'NONE', *, *, #131112, .T. ) ;
#184395 = ORIENTED_EDGE ( 'NONE', *, *, #114790, .T. ) ;
#184394 = SPHERICAL_SURFACE ( 'NONE', #94405, 0.1000000000000000056 ) ;
#184396 = VECTOR ( 'NONE', #75144, 1000.000000000000000 ) ;
#184397 = ORIENTED_EDGE ( 'NONE', *, *, #144784, .T. ) ;
#184398 = CARTESIAN_POINT ( 'NONE',  ( -23.15000000000000213, 76.00000000001142553, -36.02310748452432421 ) ) ;
#184399 = ORIENTED_EDGE ( 'NONE', *, *, #79285, .F. ) ;
#184400 = CARTESIAN_POINT ( 'NONE',  ( 23.15000000000000213, -9.000000000000000000, -23.60603087734755690 ) ) ;
#184401 = CARTESIAN_POINT ( 'NONE',  ( 18.50000000000000000, -9.499999999988842703, -141.0320693966996828 ) ) ;
#184402 = CARTESIAN_POINT ( 'NONE',  ( -21.05000000000000071, 11.65000000001115232, -40.28386566297815108 ) ) ;
#184403 = ORIENTED_EDGE ( 'NONE', *, *, #122451, .F. ) ;
#184404 = DIRECTION ( 'NONE',  ( 1.000000000000000000, -2.283407518332345398E-16, 1.048447799332034305E-15 ) ) ;
#184405 = CYLINDRICAL_SURFACE ( 'NONE', #134558, 0.1000000000000033362 ) ;
#184407 = DIRECTION ( 'NONE',  ( -0.000000000000000000, 1.000000000000000000, -0.000000000000000000 ) ) ;
#184406 = AXIS2_PLACEMENT_3D ( 'NONE', #64380, #104747, #239162 ) ;
#184408 = ORIENTED_EDGE ( 'NONE', *, *, #21277, .F. ) ;
#184409 = EDGE_CURVE ( 'NONE', #89644, #223762, #151076, .T. ) ;
#184410 = CARTESIAN_POINT ( 'NONE',  ( 22.57320508075688892, 11.75000000001115552, -100.5000000000000284 ) ) ;
#184411 = AXIS2_PLACEMENT_3D ( 'NONE', #32703, #252977, #112215 ) ;
#184413 = ORIENTED_EDGE ( 'NONE', *, *, #19507, .F. ) ;
#184412 = DIRECTION ( 'NONE',  ( 0.000000000000000000, -6.982962677686266711E-15, 1.000000000000000000 ) ) ;
#184414 = CARTESIAN_POINT ( 'NONE',  ( 0.000000000000000000, -8.350000000000004974, 32.89999999999999858 ) ) ;
#184415 = LINE ( 'NONE', #223528, #31445 ) ;
#184416 = VECTOR ( 'NONE', #149576, 1000.000000000000000 ) ;
#184417 = AXIS2_PLACEMENT_3D ( 'NONE', #211144, #174643, #192877 ) ;
#184418 = ORIENTED_EDGE ( 'NONE', *, *, #160551, .F. ) ;
#184419 = AXIS2_PLACEMENT_3D ( 'NONE', #183105, #202646, #163528 ) ;
#184420 = AXIS2_PLACEMENT_3D ( 'NONE', #232294, #191891, #131885 ) ;
#184421 = FACE_OUTER_BOUND ( 'NONE', #236156, .T. ) ;
#184423 = EDGE_CURVE ( 'NONE', #212994, #58091, #88498, .T. ) ;
#184422 = FACE_OUTER_BOUND ( 'NONE', #52161, .T. ) ;
#184424 = VECTOR ( 'NONE', #107366, 1000.000000000000000 ) ;
#184425 = CARTESIAN_POINT ( 'NONE',  ( 21.04999999999999716, 39.15970426261371529, -236.7233909955383240 ) ) ;
#184426 = ORIENTED_EDGE ( 'NONE', *, *, #239629, .T. ) ;
#184427 = DIRECTION ( 'NONE',  ( 1.000000000000000000, 1.394253735153569469E-16, 2.602809386958778209E-16 ) ) ;
#184428 = DIRECTION ( 'NONE',  ( 0.000000000000000000, 0.000000000000000000, 1.000000000000000000 ) ) ;
#184429 = EDGE_CURVE ( 'NONE', #101132, #197749, #234258, .T. ) ;
#184430 = ORIENTED_EDGE ( 'NONE', *, *, #245032, .F. ) ;
#184431 = ADVANCED_FACE ( 'NONE', ( #141268 ), #38329, .F. ) ;
#184432 = AXIS2_PLACEMENT_3D ( 'NONE', #69056, #208565, #45628 ) ;
#184433 = EDGE_CURVE ( 'NONE', #55301, #212340, #251906, .T. ) ;
#184434 = AXIS2_PLACEMENT_3D ( 'NONE', #239704, #75514, #256632 ) ;
#184435 = VERTEX_POINT ( 'NONE', #177847 ) ;
#184436 = DIRECTION ( 'NONE',  ( 1.000000000000000000, 0.000000000000000000, 0.000000000000000000 ) ) ;
#184437 = ORIENTED_EDGE ( 'NONE', *, *, #98087, .T. ) ;
#184438 = CARTESIAN_POINT ( 'NONE',  ( 18.55121869061587958, 10.32747123226657848, -39.07740328502492844 ) ) ;
#184439 = CARTESIAN_POINT ( 'NONE',  ( 5.999999999999995559, -11.75000000000000000, 10.10000000000000142 ) ) ;
#184442 = EDGE_CURVE ( 'NONE', #201917, #374, #255049, .T. ) ;
#184441 = VERTEX_POINT ( 'NONE', #40916 ) ;
#184440 = CARTESIAN_POINT ( 'NONE',  ( -16.79139129368503802, 9.944944162472834748, -146.6702446328258134 ) ) ;
#184443 = CARTESIAN_POINT ( 'NONE',  ( -21.00000000000000000, 0.000000000000000000, 0.000000000000000000 ) ) ;
#184444 = DIRECTION ( 'NONE',  ( 0.000000000000000000, -0.1568667991644355497, 0.9876197685951332295 ) ) ;
#184445 = FACE_OUTER_BOUND ( 'NONE', #176467, .T. ) ;
#184446 = LINE ( 'NONE', #146584, #67171 ) ;
#184447 = DIRECTION ( 'NONE',  ( 0.000000000000000000, 0.000000000000000000, -1.000000000000000000 ) ) ;
#184448 = EDGE_CURVE ( 'NONE', #145757, #230164, #184380, .T. ) ;
#184449 = CARTESIAN_POINT ( 'NONE',  ( -23.15000000000000213, 1.115600667400684642E-11, -71.05000000000003979 ) ) ;
#184450 = EDGE_CURVE ( 'NONE', #111084, #214648, #217682, .T. ) ;
#184451 = CYLINDRICAL_SURFACE ( 'NONE', #136352, 0.09999999999999976963 ) ;
#184453 = ORIENTED_EDGE ( 'NONE', *, *, #138338, .F. ) ;
#184452 = CARTESIAN_POINT ( 'NONE',  ( -1.739115166359751801E-14, 11.64999999999998970, -24.85000000000000142 ) ) ;
#184454 = FACE_OUTER_BOUND ( 'NONE', #254986, .T. ) ;
#184455 = ORIENTED_EDGE ( 'NONE', *, *, #52488, .F. ) ;
#184456 = DIRECTION ( 'NONE',  ( -1.000000000000000000, 0.000000000000000000, 0.000000000000000000 ) ) ;
#184457 = AXIS2_PLACEMENT_3D ( 'NONE', #79719, #118890, #181434 ) ;
#184459 = ADVANCED_FACE ( 'NONE', ( #42180 ), #119146, .T. ) ;
#184458 = DIRECTION ( 'NONE',  ( 0.000000000000000000, 0.9910827722268049644, -0.1332476588733589040 ) ) ;
#184460 = AXIS2_PLACEMENT_3D ( 'NONE', #38487, #138824, #21508 ) ;
#184461 = CARTESIAN_POINT ( 'NONE',  ( 23.24999999999999289, 6.650000000011155876, -45.85000000000000142 ) ) ;
#184462 = CARTESIAN_POINT ( 'NONE',  ( 20.41140022480505323, 65.58956915761099538, -195.9081061808921902 ) ) ;
#184463 = EDGE_LOOP ( 'NONE', ( #225839, #239305, #127820, #135775 ) ) ;
#184464 = CARTESIAN_POINT ( 'NONE',  ( 23.24999999999999645, 67.23127455305835554, -235.8551265064784559 ) ) ;
#184465 = CARTESIAN_POINT ( 'NONE',  ( 18.69999999999999929, -10.64999999999999325, 33.00000000000000000 ) ) ;
#184466 = VERTEX_POINT ( 'NONE', #160850 ) ;
#184467 = FACE_OUTER_BOUND ( 'NONE', #156047, .T. ) ;
#184468 = VECTOR ( 'NONE', #6722, 1000.000000000000000 ) ;
#184469 = LINE ( 'NONE', #241881, #176426 ) ;
#184470 = ORIENTED_EDGE ( 'NONE', *, *, #173760, .F. ) ;
#184471 = CARTESIAN_POINT ( 'NONE',  ( 18.39999999999999503, 5.650000000011139001, -188.3499999999999659 ) ) ;
#184472 = ADVANCED_FACE ( 'NONE', ( #240375 ), #171766, .T. ) ;
#184473 = EDGE_LOOP ( 'NONE', ( #78186, #186936, #15864, #103021 ) ) ;
#184474 = EDGE_CURVE ( 'NONE', #177788, #172262, #121725, .T. ) ;
#184475 = CYLINDRICAL_SURFACE ( 'NONE', #133956, 0.1000000000000046685 ) ;
#184476 = EDGE_LOOP ( 'NONE', ( #227785, #68007, #60068, #163541 ) ) ;
#184477 = CARTESIAN_POINT ( 'NONE',  ( 20.73486653747088937, 68.25000000001155342, -56.87310748452437537 ) ) ;
#184478 = CARTESIAN_POINT ( 'NONE',  ( 13.43443725621852813, 9.446557523083688679, -182.5899419543458464 ) ) ;
#184479 = ORIENTED_EDGE ( 'NONE', *, *, #167346, .F. ) ;
#184480 = EDGE_CURVE ( 'NONE', #195387, #107897, #199971, .T. ) ;
#184482 = LINE ( 'NONE', #120698, #40504 ) ;
#184481 = AXIS2_PLACEMENT_3D ( 'NONE', #170303, #204236, #6027 ) ;
#184484 = ORIENTED_EDGE ( 'NONE', *, *, #167461, .F. ) ;
#184483 = CARTESIAN_POINT ( 'NONE',  ( -20.94999999999999929, 1.115600667400684642E-11, -63.00000000000000000 ) ) ;
#184485 = CARTESIAN_POINT ( 'NONE',  ( -22.50000000000094147, 75.89914163091414423, -215.2726746080137730 ) ) ;
#184486 = ORIENTED_EDGE ( 'NONE', *, *, #231641, .F. ) ;
#184487 = CIRCLE ( 'NONE', #246847, 0.1000000000000075273 ) ;
#184488 = CIRCLE ( 'NONE', #72097, 0.09999999999999939493 ) ;
#184489 = ORIENTED_EDGE ( 'NONE', *, *, #115460, .T. ) ;
#184490 = CARTESIAN_POINT ( 'NONE',  ( 23.14999999999998437, 1.115600667400684642E-11, -134.0000000000000000 ) ) ;
#184491 = DIRECTION ( 'NONE',  ( 0.000000000000000000, 0.000000000000000000, 1.000000000000000000 ) ) ;
#184492 = DIRECTION ( 'NONE',  ( -1.000000000000000000, -0.000000000000000000, -0.000000000000000000 ) ) ;
#184493 = CARTESIAN_POINT ( 'NONE',  ( 23.14999999999998437, 1.115600667400684642E-11, -67.00000000000004263 ) ) ;
#184494 = CARTESIAN_POINT ( 'NONE',  ( -13.77178122865955068, 66.54397173950466993, -188.5119094494586705 ) ) ;
#184495 = CARTESIAN_POINT ( 'NONE',  ( 22.20000000000000284, 10.21702379168713115, -11.24211197275198160 ) ) ;
#184496 = AXIS2_PLACEMENT_3D ( 'NONE', #110812, #25205, #103410 ) ;
#184497 = VERTEX_POINT ( 'NONE', #197378 ) ;
#184498 = AXIS2_PLACEMENT_3D ( 'NONE', #3290, #162407, #106242 ) ;
#184499 = CARTESIAN_POINT ( 'NONE',  ( 23.15000000000000213, -11.64999999998883595, -197.8999999999999773 ) ) ;
#184500 = LINE ( 'NONE', #85374, #65212 ) ;
#184501 = DIRECTION ( 'NONE',  ( 3.265361837132813093E-16, -1.000000000000000000, -0.000000000000000000 ) ) ;
#184502 = VECTOR ( 'NONE', #605, 1000.000000000000000 ) ;
#184503 = CARTESIAN_POINT ( 'NONE',  ( -20.07928932188135107, 9.220710678129810489, -121.7500000000000426 ) ) ;
#184504 = EDGE_CURVE ( 'NONE', #129641, #120222, #138660, .T. ) ;
#184505 = ORIENTED_EDGE ( 'NONE', *, *, #103714, .T. ) ;
#184506 = CARTESIAN_POINT ( 'NONE',  ( 20.91682497891423154, 68.08564185115264422, -224.1612363371343122 ) ) ;
#184507 = EDGE_LOOP ( 'NONE', ( #196492, #39821, #20189, #30428, #152207, #219208, #154715, #144817, #216029, #253557, #121399, #135224, #37049, #164032 ) ) ;
#184508 = FACE_OUTER_BOUND ( 'NONE', #105803, .T. ) ;
#184509 = ORIENTED_EDGE ( 'NONE', *, *, #187956, .F. ) ;
#184510 = CARTESIAN_POINT ( 'NONE',  ( -22.01447462590972748, 68.73619979878276354, -203.6221444845839699 ) ) ;
#184511 = FACE_OUTER_BOUND ( 'NONE', #117280, .T. ) ;
#184513 = ORIENTED_EDGE ( 'NONE', *, *, #144629, .T. ) ;
#184512 = CIRCLE ( 'NONE', #109502, 0.09999999999999939493 ) ;
#184516 = ORIENTED_EDGE ( 'NONE', *, *, #8192, .T. ) ;
#184515 = ADVANCED_FACE ( 'NONE', ( #218205 ), #23917, .F. ) ;
#184514 = DIRECTION ( 'NONE',  ( -0.000000000000000000, 6.982962677686266711E-15, -1.000000000000000000 ) ) ;
#184517 = CARTESIAN_POINT ( 'NONE',  ( -18.59999999999999787, -1.835341550213255957, -78.65515129256301918 ) ) ;
#184518 = ORIENTED_EDGE ( 'NONE', *, *, #125197, .T. ) ;
#184519 = CARTESIAN_POINT ( 'NONE',  ( -22.39999999999999858, 1.115600667400684642E-11, -21.85042919245520210 ) ) ;
#184520 = AXIS2_PLACEMENT_3D ( 'NONE', #237620, #137224, #198481 ) ;
#184521 = EDGE_CURVE ( 'NONE', #142859, #62686, #217862, .T. ) ;
#184522 = CIRCLE ( 'NONE', #68019, 11.64999999999999325 ) ;
#184523 = CIRCLE ( 'NONE', #238709, 0.5999999999999894307 ) ;
#184524 = DIRECTION ( 'NONE',  ( -1.000000000000000000, 7.304098846218134667E-16, 4.217023435051625732E-16 ) ) ;
#184525 = VECTOR ( 'NONE', #115399, 1000.000000000000000 ) ;
#184526 = EDGE_LOOP ( 'NONE', ( #149970, #247135, #210452 ) ) ;
#184527 = LINE ( 'NONE', #205368, #43599 ) ;
#184528 = ADVANCED_FACE ( 'NONE', ( #79977 ), #159557, .F. ) ;
#184529 = FACE_OUTER_BOUND ( 'NONE', #221723, .T. ) ;
#184530 = ORIENTED_EDGE ( 'NONE', *, *, #162558, .T. ) ;
#184531 = EDGE_CURVE ( 'NONE', #167845, #205806, #202525, .T. ) ;
#184534 = EDGE_CURVE ( 'NONE', #227113, #225538, #159454, .T. ) ;
#184533 = ADVANCED_FACE ( 'NONE', ( #25194 ), #246921, .F. ) ;
#184532 = CARTESIAN_POINT ( 'NONE',  ( 18.49999999999999289, 6.450000000011156587, -88.15000000000004832 ) ) ;
#184536 = ORIENTED_EDGE ( 'NONE', *, *, #235601, .T. ) ;
#184535 = CARTESIAN_POINT ( 'NONE',  ( -23.25000000000000000, -11.48912529306489994, -97.40000000000004832 ) ) ;
#184537 = CYLINDRICAL_SURFACE ( 'NONE', #253799, 0.1000000000000028644 ) ;
#184538 = DIRECTION ( 'NONE',  ( -0.000000000000000000, 0.000000000000000000, -1.000000000000000000 ) ) ;
#184539 = CARTESIAN_POINT ( 'NONE',  ( -20.15000000000000568, 9.291421356248463326, -79.35000000000005116 ) ) ;
#184540 = AXIS2_PLACEMENT_3D ( 'NONE', #247905, #187946, #109668 ) ;
#184542 = CARTESIAN_POINT ( 'NONE',  ( 22.50000000000000000, 36.65892442174472876, -249.5511627012454596 ) ) ;
#184541 = CARTESIAN_POINT ( 'NONE',  ( -16.93772744219066340, 66.00645889125951271, -90.42504551255468925 ) ) ;
#184543 = CARTESIAN_POINT ( 'NONE',  ( 21.05000000000000071, 39.23476235320398331, -236.9756760510740321 ) ) ;
#184544 = FACE_OUTER_BOUND ( 'NONE', #219102, .T. ) ;
#184545 = AXIS2_PLACEMENT_3D ( 'NONE', #96855, #21379, #160885 ) ;
#184546 = CARTESIAN_POINT ( 'NONE',  ( 18.69999999999999929, -8.350000000000004974, 10.52591260281975138 ) ) ;
#184547 = CARTESIAN_POINT ( 'NONE',  ( -23.49999999999994316, 77.16254490893143725, -43.82310748452479743 ) ) ;
#184548 = EDGE_CURVE ( 'NONE', #199384, #38969, #56947, .T. ) ;
#184549 = EDGE_CURVE ( 'NONE', #232784, #209275, #130402, .T. ) ;
#184550 = VERTEX_POINT ( 'NONE', #189388 ) ;
#184551 = CIRCLE ( 'NONE', #80468, 0.1000000000000028644 ) ;
#184552 = ORIENTED_EDGE ( 'NONE', *, *, #234624, .F. ) ;
#184553 = ADVANCED_FACE ( 'NONE', ( #169870 ), #5579, .F. ) ;
#184555 = CARTESIAN_POINT ( 'NONE',  ( -21.05000000000000071, 1.115600667400684642E-11, -100.5000000000000284 ) ) ;
#184554 = CIRCLE ( 'NONE', #67863, 0.1000000000000028644 ) ;
#184556 = VERTEX_POINT ( 'NONE', #29065 ) ;
#184557 = CARTESIAN_POINT ( 'NONE',  ( 18.59999999999999432, 85.48068669529062902, -62.58199231576638510 ) ) ;
#184558 = CIRCLE ( 'NONE', #126311, 0.1000000000000028644 ) ;
#184559 = ADVANCED_FACE ( 'NONE', ( #90261 ), #184243, .T. ) ;
#184560 = EDGE_LOOP ( 'NONE', ( #151720, #84351, #220722, #211870 ) ) ;
#184561 = AXIS2_PLACEMENT_3D ( 'NONE', #9712, #46265, #107529 ) ;
#184563 = VECTOR ( 'NONE', #197377, 1000.000000000000000 ) ;
#184562 =( LENGTH_UNIT ( ) NAMED_UNIT ( * ) SI_UNIT ( .MILLI., .METRE. ) );
#184564 = CARTESIAN_POINT ( 'NONE',  ( 20.94403535211772294, 65.69367753730678317, -131.0189238066348594 ) ) ;
#184565 = AXIS2_PLACEMENT_3D ( 'NONE', #183618, #4937, #199337 ) ;
#184566 = EDGE_CURVE ( 'NONE', #89986, #110564, #17962, .T. ) ;
#184567 = PRODUCT_DEFINITION_SHAPE ( 'NONE', 'NONE',  #32578 ) ;
#184568 = VERTEX_POINT ( 'NONE', #167284 ) ;
#184569 = DIRECTION ( 'NONE',  ( 0.000000000000000000, 0.2128009952263607285, -0.9770955615653316162 ) ) ;
#184570 = ORIENTED_EDGE ( 'NONE', *, *, #163722, .T. ) ;
#184571 = ORIENTED_EDGE ( 'NONE', *, *, #189300, .T. ) ;
#184572 = VECTOR ( 'NONE', #250861, 1000.000000000000000 ) ;
#184573 = CARTESIAN_POINT ( 'NONE',  ( 20.94999999999997442, 77.26327546522863088, -28.12124281777790813 ) ) ;
#184574 = CYLINDRICAL_SURFACE ( 'NONE', #46292, 0.09999999999999939493 ) ;
#184576 = VERTEX_POINT ( 'NONE', #145105 ) ;
#184575 = CARTESIAN_POINT ( 'NONE',  ( 20.73486653747088582, 68.75000000001178080, -82.17310748452436542 ) ) ;
#184577 = EDGE_CURVE ( 'NONE', #110088, #61112, #180298, .T. ) ;
#184578 = DIRECTION ( 'NONE',  ( 1.000000000000000000, 7.304098846218134667E-16, 0.000000000000000000 ) ) ;
#184580 = ORIENTED_EDGE ( 'NONE', *, *, #181980, .T. ) ;
#184579 = CARTESIAN_POINT ( 'NONE',  ( -18.59999999999999787, 1.835341550235567887, -145.5551512925629822 ) ) ;
#184581 = CARTESIAN_POINT ( 'NONE',  ( 21.05000000000000071, -11.64999999998883595, -131.1000000000000227 ) ) ;
#184582 = DIRECTION ( 'NONE',  ( 0.000000000000000000, 0.000000000000000000, 1.000000000000000000 ) ) ;
#184583 = VECTOR ( 'NONE', #104451, 1000.000000000000000 ) ;
#184585 = VERTEX_POINT ( 'NONE', #65577 ) ;
#184584 = DIRECTION ( 'NONE',  ( 0.000000000000000000, 0.000000000000000000, 1.000000000000000000 ) ) ;
#184586 = AXIS2_PLACEMENT_3D ( 'NONE', #238013, #99768, #142754 ) ;
#184587 = CARTESIAN_POINT ( 'NONE',  ( 18.59117750673696534, 10.33248238083634796, -173.0948465439131496 ) ) ;
#184588 = CARTESIAN_POINT ( 'NONE',  ( -15.69373346032658745, 26.71301589465422666, -233.6087318245599533 ) ) ;
#184590 = EDGE_CURVE ( 'NONE', #81650, #24606, #224644, .T. ) ;
#184589 = EDGE_LOOP ( 'NONE', ( #154462, #246628, #105899, #196292 ) ) ;
#184591 = AXIS2_PLACEMENT_3D ( 'NONE', #89913, #52064, #228164 ) ;
#184593 = CARTESIAN_POINT ( 'NONE',  ( -21.07946286933445279, 69.67096268100499401, -203.5997913277808493 ) ) ;
#184592 = LINE ( 'NONE', #240728, #219806 ) ;
#184594 = CARTESIAN_POINT ( 'NONE',  ( 18.49999999999999289, 10.23906162413259402, -91.75439743459725150 ) ) ;
#184595 = DIRECTION ( 'NONE',  ( 0.000000000000000000, 1.000000000000000000, 0.000000000000000000 ) ) ;
#184596 = DIRECTION ( 'NONE',  ( 0.000000000000000000, 0.000000000000000000, 1.000000000000000000 ) ) ;
#184597 = CYLINDRICAL_SURFACE ( 'NONE', #217571, 12.87499999999999822 ) ;
#184599 = EDGE_LOOP ( 'NONE', ( #113728, #2118, #9435, #33397 ) ) ;
#184598 = CIRCLE ( 'NONE', #55384, 3.999999999999989786 ) ;
#184600 = ORIENTED_EDGE ( 'NONE', *, *, #17203, .T. ) ;
#184601 = VECTOR ( 'NONE', #174512, 1000.000000000000000 ) ;
#184603 = ORIENTED_EDGE ( 'NONE', *, *, #224314, .T. ) ;
#184602 = AXIS2_PLACEMENT_3D ( 'NONE', #230691, #250240, #256252 ) ;
#184604 = CARTESIAN_POINT ( 'NONE',  ( -15.55912972643740488, 67.50912972644894694, -48.67310748452438673 ) ) ;
#184605 = STYLED_ITEM ( 'NONE', ( #6679 ), #26097 ) ;
#184606 = ORIENTED_EDGE ( 'NONE', *, *, #114180, .T. ) ;
#184607 = DIRECTION ( 'NONE',  ( 0.000000000000000000, 0.1350103645451807555, 0.9908441862701609093 ) ) ;
#184608 = EDGE_LOOP ( 'NONE', ( #121122, #159803, #215845, #152158 ) ) ;
#184609 = EDGE_CURVE ( 'NONE', #66896, #186169, #101117, .T. ) ;
#184610 = CARTESIAN_POINT ( 'NONE',  ( -23.25000000000000000, 7.128833340094563376, -233.7327013124401276 ) ) ;
#184611 = CARTESIAN_POINT ( 'NONE',  ( 18.39999999999999858, -9.519327731081283162, -40.47297637655933755 ) ) ;
#184612 = ORIENTED_EDGE ( 'NONE', *, *, #103425, .F. ) ;
#184613 = CARTESIAN_POINT ( 'NONE',  ( 15.57250062127603663, 9.370689921613768902, -151.5264651266610940 ) ) ;
#184614 = FILL_AREA_STYLE ('',( #201610 ) ) ;
#184615 = TOROIDAL_SURFACE ( 'NONE', #80536, 11.89999999999999858, 0.1000000000000000056 ) ;
#184616 = CIRCLE ( 'NONE', #68106, 11.64999999999999680 ) ;
#184617 = ORIENTED_EDGE ( 'NONE', *, *, #173945, .F. ) ;
#184618 = TOROIDAL_SURFACE ( 'NONE', #251245, 0.4000000000000012990, 0.1000000000000000056 ) ;
#184620 = VERTEX_POINT ( 'NONE', #44746 ) ;
#184619 = CIRCLE ( 'NONE', #101369, 0.1999999999999987899 ) ;
#184621 = ORIENTED_EDGE ( 'NONE', *, *, #23856, .T. ) ;
#184622 = DIRECTION ( 'NONE',  ( 0.000000000000000000, 0.000000000000000000, 1.000000000000000000 ) ) ;
#184623 = CARTESIAN_POINT ( 'NONE',  ( -23.15000000000000213, 70.10000000001220144, -146.7422072491807796 ) ) ;
#184624 = DIRECTION ( 'NONE',  ( 1.000000000000000000, 0.000000000000000000, 0.000000000000000000 ) ) ;
#184625 = CARTESIAN_POINT ( 'NONE',  ( 14.22916352759893499, 27.90214353194706121, -234.1315669640962085 ) ) ;
#184626 = CARTESIAN_POINT ( 'NONE',  ( -21.08479644141223375, 61.09212952597296464, -234.2508065485932889 ) ) ;
#184627 = DIRECTION ( 'NONE',  ( 0.000000000000000000, 0.000000000000000000, -1.000000000000000000 ) ) ;
#184629 = DIRECTION ( 'NONE',  ( 0.000000000000000000, -7.116814260417668513E-15, 1.000000000000000000 ) ) ;
#184628 = DIRECTION ( 'NONE',  ( -0.000000000000000000, -0.7397890806274287634, -0.6728388485992942147 ) ) ;
#184630 = CARTESIAN_POINT ( 'NONE',  ( -20.85000000000000497, 11.75000000001115019, -160.5808527540413024 ) ) ;
#184632 = ORIENTED_EDGE ( 'NONE', *, *, #172920, .T. ) ;
#184631 = CARTESIAN_POINT ( 'NONE',  ( -20.85000000000000142, 87.75000000001143974, -38.92310748452424463 ) ) ;
#184634 = LINE ( 'NONE', #145503, #54247 ) ;
#184633 = CARTESIAN_POINT ( 'NONE',  ( -20.94999999999999929, 11.75000000001115197, -40.51480577065400013 ) ) ;
#184635 = CARTESIAN_POINT ( 'NONE',  ( 18.49999999999998934, 63.53162788017662166, -224.4728618886983043 ) ) ;
#184636 = EDGE_LOOP ( 'NONE', ( #62446, #255795, #12330, #173469 ) ) ;
#184637 = CARTESIAN_POINT ( 'NONE',  ( 20.95520789717937404, 10.57693059939611224, -74.58023297387489947 ) ) ;
#184638 = DIRECTION ( 'NONE',  ( -0.000000000000000000, 1.000000000000000000, -0.000000000000000000 ) ) ;
#184639 = EDGE_LOOP ( 'NONE', ( #18175, #74024, #65273, #37097 ) ) ;
#184640 = DIRECTION ( 'NONE',  ( 0.000000000000000000, 0.000000000000000000, -1.000000000000000000 ) ) ;
#184641 = PLANE ( 'NONE',  #209195 ) ;
#184642 = ORIENTED_EDGE ( 'NONE', *, *, #170635, .F. ) ;
#184643 = ORIENTED_EDGE ( 'NONE', *, *, #91212, .F. ) ;
#184644 = CIRCLE ( 'NONE', #197112, 4.041421356237310469 ) ;
#184645 = CARTESIAN_POINT ( 'NONE',  ( -23.15000000000000213, 71.65000000001187175, -90.67310748452433700 ) ) ;
#184646 = ORIENTED_EDGE ( 'NONE', *, *, #128372, .T. ) ;
#184647 = CARTESIAN_POINT ( 'NONE',  ( -18.43634282235125710, -9.679787199916876972, -174.1606518854538592 ) ) ;
#184648 = CARTESIAN_POINT ( 'NONE',  ( -18.59999999999999787, 85.48068669529084218, -96.08199231576638510 ) ) ;
#184649 = DIRECTION ( 'NONE',  ( 0.000000000000000000, 0.1332476588733589318, 0.9910827722268049644 ) ) ;
#184650 = ORIENTED_EDGE ( 'NONE', *, *, #72688, .T. ) ;
#184651 = DIRECTION ( 'NONE',  ( 0.000000000000000000, -7.304098846218139203E-15, 1.000000000000000000 ) ) ;
#184653 = ADVANCED_FACE ( 'NONE', ( #245515 ), #168590, .F. ) ;
#184652 = CARTESIAN_POINT ( 'NONE',  ( -23.15000000000000213, 74.00000000001254818, -183.2477294072864709 ) ) ;
#184654 = CARTESIAN_POINT ( 'NONE',  ( 18.49999999999999289, 10.20857864377384416, -192.1499999999999488 ) ) ;
#184655 = CARTESIAN_POINT ( 'NONE',  ( 21.05000000000000071, 8.876614585098254295, -41.88508047884467800 ) ) ;
#184656 = AXIS2_PLACEMENT_3D ( 'NONE', #126760, #184156, #167208 ) ;
#184658 = ORIENTED_EDGE ( 'NONE', *, *, #187807, .F. ) ;
#184657 = AXIS2_PLACEMENT_3D ( 'NONE', #73153, #76961, #56094 ) ;
#184659 = CARTESIAN_POINT ( 'NONE',  ( 21.05000000000000071, 70.15000000001252545, -180.1556047088023149 ) ) ;
#184660 = CIRCLE ( 'NONE', #164013, 0.09999999999998898659 ) ;
#184662 = VERTEX_POINT ( 'NONE', #148994 ) ;
#184661 = CARTESIAN_POINT ( 'NONE',  ( -20.94999999999999929, 0.000000000000000000, -33.50000000000000000 ) ) ;
#184663 = CARTESIAN_POINT ( 'NONE',  ( -21.14999999999999858, 1.115600667400684642E-11, -93.95934304829879125 ) ) ;
#184664 = CARTESIAN_POINT ( 'NONE',  ( 18.59999994388910238, 78.14805800158373472, -231.3753211930361999 ) ) ;
#184665 = ADVANCED_FACE ( 'NONE', ( #66869 ), #146379, .T. ) ;
#184666 = CARTESIAN_POINT ( 'NONE',  ( 20.94999999999999929, -8.663551401857999323, -124.4758988819327215 ) ) ;
#184667 = CARTESIAN_POINT ( 'NONE',  ( -23.15000000000000213, 64.25000000001146816, -43.03791325517834565 ) ) ;
#184668 = CARTESIAN_POINT ( 'NONE',  ( 21.93642651522410603, 10.58866904893262095, -227.2738390313130878 ) ) ;
#184669 = DIRECTION ( 'NONE',  ( 0.000000000000000000, -1.000000000000000000, 0.000000000000000000 ) ) ;
#184670 = ADVANCED_FACE ( 'NONE', ( #227219 ), #163727, .T. ) ;
#184671 = EDGE_LOOP ( 'NONE', ( #41735, #3594, #126819, #22238 ) ) ;
#184672 = CYLINDRICAL_SURFACE ( 'NONE', #51190, 0.1000000000000070832 ) ;
#184673 = DIRECTION ( 'NONE',  ( -0.000000000000000000, 0.000000000000000000, -1.000000000000000000 ) ) ;
#184674 = CARTESIAN_POINT ( 'NONE',  ( -21.05000000000000071, 87.65000000001165859, -69.52310748452424605 ) ) ;
#184675 = CARTESIAN_POINT ( 'NONE',  ( -21.05000000000000071, 62.99095723518624368, -207.1734234082435080 ) ) ;
#184677 = CARTESIAN_POINT ( 'NONE',  ( -20.54999999999999716, 70.60814576644823148, -215.7631455941064189 ) ) ;
#184676 = CIRCLE ( 'NONE', #180414, 0.1000000000000028644 ) ;
#184679 = ORIENTED_EDGE ( 'NONE', *, *, #28217, .F. ) ;
#184678 = AXIS2_PLACEMENT_3D ( 'NONE', #240132, #237559, #61489 ) ;
#184680 = VERTEX_POINT ( 'NONE', #207678 ) ;
#184681 = CARTESIAN_POINT ( 'NONE',  ( -20.64999999999999858, 68.75000000001158185, -57.17310748452437252 ) ) ;
#184682 = ADVANCED_FACE ( 'NONE', ( #208945 ), #30326, .F. ) ;
#184683 = CARTESIAN_POINT ( 'NONE',  ( 22.00411653889210228, 0.09903810579702632122, -126.7465571323596123 ) ) ;
#184684 = CARTESIAN_POINT ( 'NONE',  ( 20.99749315643146730, 17.11694853957538598, -224.3781540366317131 ) ) ;
#184685 = EDGE_CURVE ( 'NONE', #131341, #190027, #1208, .T. ) ;
#184686 = CARTESIAN_POINT ( 'NONE',  ( -18.39999999999999858, 85.50000000001209344, -129.5238218066853904 ) ) ;
#184687 = EDGE_CURVE ( 'NONE', #34062, #31046, #151276, .T. ) ;
#184688 = CARTESIAN_POINT ( 'NONE',  ( 21.05000000000005400, 74.94272479589878344, -3.123107484524795474 ) ) ;
#184689 = AXIS2_PLACEMENT_3D ( 'NONE', #233050, #54385, #133917 ) ;
#184690 = CIRCLE ( 'NONE', #226166, 0.1000000000000045158 ) ;
#184691 = LINE ( 'NONE', #8638, #9218 ) ;
#184692 = VECTOR ( 'NONE', #235105, 1000.000000000000000 ) ;
#184693 = EDGE_CURVE ( 'NONE', #231948, #182351, #5479, .T. ) ;
#184694 = CARTESIAN_POINT ( 'NONE',  ( 20.94999999999999929, -11.64999999998883595, -164.6000000000000227 ) ) ;
#184695 = EDGE_CURVE ( 'NONE', #178001, #53093, #109546, .T. ) ;
#184696 = EDGE_LOOP ( 'NONE', ( #90597, #109937, #108473, #250570 ) ) ;
#184697 = DIRECTION ( 'NONE',  ( 0.000000000000000000, -6.769652589177772835E-15, 1.000000000000000000 ) ) ;
#184698 = CIRCLE ( 'NONE', #138876, 7.900000000000003908 ) ;
#184699 = ORIENTED_EDGE ( 'NONE', *, *, #254633, .T. ) ;
#184700 = CARTESIAN_POINT ( 'NONE',  ( -16.87683809663752399, 52.34166666667851331, -86.27310748452447342 ) ) ;
#184701 = DIRECTION ( 'NONE',  ( 1.000000000000000000, 0.000000000000000000, 0.000000000000000000 ) ) ;
#184702 = FACE_OUTER_BOUND ( 'NONE', #12360, .T. ) ;
#184703 = CARTESIAN_POINT ( 'NONE',  ( -16.87331047859651179, 9.950000000011142376, -46.15000000000000568 ) ) ;
#184705 = CIRCLE ( 'NONE', #89027, 12.87499999999999822 ) ;
#184704 = FACE_OUTER_BOUND ( 'NONE', #232672, .T. ) ;
#184706 = FACE_BOUND ( 'NONE', #203959, .T. ) ;
#184707 = AXIS2_PLACEMENT_3D ( 'NONE', #121360, #219115, #120067 ) ;
#184708 = AXIS2_PLACEMENT_3D ( 'NONE', #223843, #63492, #100035 ) ;
#184709 = CARTESIAN_POINT ( 'NONE',  ( 22.10000000000000142, -11.65000000000000036, 11.99999999999999645 ) ) ;
#184710 = EDGE_CURVE ( 'NONE', #50987, #76744, #184554, .T. ) ;
#184711 = CIRCLE ( 'NONE', #34926, 3.899999999999987033 ) ;
#184712 = DIRECTION ( 'NONE',  ( 0.000000000000000000, 0.000000000000000000, 1.000000000000000000 ) ) ;
#184713 = DIRECTION ( 'NONE',  ( 1.000000000000000000, -0.000000000000000000, -0.000000000000000000 ) ) ;
#184714 = DIRECTION ( 'NONE',  ( 1.000000000000000000, -0.000000000000000000, -0.000000000000000000 ) ) ;
#184715 = CARTESIAN_POINT ( 'NONE',  ( -18.50000000000000000, 77.16412189325330928, -128.6082593989527254 ) ) ;
#184716 = ORIENTED_EDGE ( 'NONE', *, *, #234358, .T. ) ;
#184717 = FACE_OUTER_BOUND ( 'NONE', #204130, .T. ) ;
#184718 = CARTESIAN_POINT ( 'NONE',  ( 21.05000000000000071, 76.00000000001213607, -136.5231074845243313 ) ) ;
#184719 = EDGE_LOOP ( 'NONE', ( #3952, #158181, #24611, #63976 ) ) ;
#184720 = CARTESIAN_POINT ( 'NONE',  ( -16.94275863006528482, 51.64076883226000092, -231.8933771982521250 ) ) ;
#184721 = DIRECTION ( 'NONE',  ( -0.000000000000000000, 0.2128009952263603677, -0.9770955615653313941 ) ) ;
#184722 = LINE ( 'NONE', #66068, #30624 ) ;
#184723 = AXIS2_PLACEMENT_3D ( 'NONE', #188578, #208168, #6084 ) ;
#184724 = VERTEX_POINT ( 'NONE', #190699 ) ;
#184725 = CARTESIAN_POINT ( 'NONE',  ( 20.94999999999999574, 1.115600667400684642E-11, -33.50000000000000000 ) ) ;
#184726 = CARTESIAN_POINT ( 'NONE',  ( 18.60000000000000142, 47.07326788871598922, -255.0992659944397190 ) ) ;
#184727 = AXIS2_PLACEMENT_3D ( 'NONE', #5309, #230835, #15649 ) ;
#184729 = ORIENTED_EDGE ( 'NONE', *, *, #166225, .F. ) ;
#184728 = AXIS2_PLACEMENT_3D ( 'NONE', #92375, #216168, #194076 ) ;
#184730 = EDGE_CURVE ( 'NONE', #165926, #254695, #257842, .T. ) ;
#184732 = CARTESIAN_POINT ( 'NONE',  ( -21.05000000000000071, 76.10000000001198828, -109.5637644362255543 ) ) ;
#184731 = AXIS2_PLACEMENT_3D ( 'NONE', #249255, #94007, #173617 ) ;
#184733 = TOROIDAL_SURFACE ( 'NONE', #151464, 11.89999999999999858, 0.1000000000000000056 ) ;
#184734 = ORIENTED_EDGE ( 'NONE', *, *, #160945, .F. ) ;
#184735 = LINE ( 'NONE', #163910, #200010 ) ;
#184736 = EDGE_CURVE ( 'NONE', #127766, #117549, #171958, .T. ) ;
#184738 = EDGE_CURVE ( 'NONE', #174426, #106998, #92793, .T. ) ;
#184737 = LINE ( 'NONE', #23134, #112397 ) ;
#184739 = CARTESIAN_POINT ( 'NONE',  ( 20.94999999999999574, 4.436385504674529301, -245.3241086753762659 ) ) ;
#184741 = VECTOR ( 'NONE', #117027, 1000.000000000000000 ) ;
#184740 = CARTESIAN_POINT ( 'NONE',  ( 21.05000000000000071, 1.115600667400684642E-11, -167.4999999999999716 ) ) ;
#184742 = CARTESIAN_POINT ( 'NONE',  ( 21.05000000000000071, 81.86853375790846599, -214.9828603846715964 ) ) ;
#184743 = CARTESIAN_POINT ( 'NONE',  ( -20.85000000000000142, -1.164121893230052995, -175.4148480855716059 ) ) ;
#184744 = FACE_OUTER_BOUND ( 'NONE', #25057, .T. ) ;
#184745 = CIRCLE ( 'NONE', #93168, 0.09999999999999609201 ) ;
#184746 = EDGE_CURVE ( 'NONE', #96338, #74028, #213597, .T. ) ;
#184747 = DIRECTION ( 'NONE',  ( 1.000000000000000000, -0.000000000000000000, 0.000000000000000000 ) ) ;
#184748 = CARTESIAN_POINT ( 'NONE',  ( -20.94999999999999929, 77.16270174995034381, -162.1231074845243540 ) ) ;
#184749 = EDGE_CURVE ( 'NONE', #74900, #70387, #167849, .T. ) ;
#184750 = AXIS2_PLACEMENT_3D ( 'NONE', #19382, #40252, #237144 ) ;
#184752 = VERTEX_POINT ( 'NONE', #111131 ) ;
#184751 = DIRECTION ( 'NONE',  ( -0.4999999999999799050, -6.047423072554995242E-15, 0.8660254037844502539 ) ) ;
#184753 = ORIENTED_EDGE ( 'NONE', *, *, #96704, .T. ) ;
#184755 = CARTESIAN_POINT ( 'NONE',  ( -20.94999999999999929, 64.30000000001196270, -109.7781056340430013 ) ) ;
#184754 = CARTESIAN_POINT ( 'NONE',  ( 20.94999999999999574, -1.835341550213255957, -78.55515129256302487 ) ) ;
#184756 = AXIS2_PLACEMENT_3D ( 'NONE', #197085, #18464, #52432 ) ;
#184758 = EDGE_LOOP ( 'NONE', ( #20671, #116226, #26567, #156297 ) ) ;
#184757 = DIRECTION ( 'NONE',  ( -1.000000000000000000, -0.000000000000000000, -0.000000000000000000 ) ) ;
#184759 = ADVANCED_FACE ( 'NONE', ( #152865 ), #255244, .T. ) ;
#184760 = VERTEX_POINT ( 'NONE', #31627 ) ;
#184761 = FACE_OUTER_BOUND ( 'NONE', #179325, .T. ) ;
#184762 = EDGE_CURVE ( 'NONE', #178346, #214744, #232386, .T. ) ;
#184763 = DIRECTION ( 'NONE',  ( 0.000000000000000000, -0.9770955615653551529, -0.2128009952262517601 ) ) ;
#184764 = AXIS2_PLACEMENT_3D ( 'NONE', #124864, #84392, #145690 ) ;
#184766 = EDGE_CURVE ( 'NONE', #213112, #71518, #142840, .T. ) ;
#184765 = FACE_OUTER_BOUND ( 'NONE', #215941, .T. ) ;
#184767 = CARTESIAN_POINT ( 'NONE',  ( -20.86777300164945004, 10.33200063080771969, -173.0931674956643178 ) ) ;
#184768 = CARTESIAN_POINT ( 'NONE',  ( -18.55121869061588669, 67.49249915771264341, -195.4369143829851510 ) ) ;
#184769 = AXIS2_PLACEMENT_3D ( 'NONE', #93898, #74383, #153934 ) ;
#184770 = CARTESIAN_POINT ( 'NONE',  ( 18.59999999999999432, 14.81796439977981272, -236.5325475414793743 ) ) ;
#184771 = DIRECTION ( 'NONE',  ( 0.000000000000000000, 0.4721928772778128947, 0.8814952561688012000 ) ) ;
#184772 = VECTOR ( 'NONE', #235843, 1000.000000000000000 ) ;
#184773 = EDGE_LOOP ( 'NONE', ( #229095, #250839, #104345, #57503, #43433, #165526, #15441, #4662 ) ) ;
#184774 = ORIENTED_EDGE ( 'NONE', *, *, #220678, .F. ) ;
#184775 = DIRECTION ( 'NONE',  ( 0.000000000000000000, 0.8814952561688476074, -0.4721928772777262417 ) ) ;
#184776 = VERTEX_POINT ( 'NONE', #75855 ) ;
#184777 = LINE ( 'NONE', #180941, #5259 ) ;
#184778 = ORIENTED_EDGE ( 'NONE', *, *, #168478, .T. ) ;
#184780 = AXIS2_PLACEMENT_3D ( 'NONE', #63302, #43753, #87983 ) ;
#184779 = DIRECTION ( 'NONE',  ( 0.000000000000000000, -1.000000000000000000, 0.000000000000000000 ) ) ;
#184781 = AXIS2_PLACEMENT_3D ( 'NONE', #187083, #155674, #35723 ) ;
#184782 = EDGE_CURVE ( 'NONE', #100799, #22210, #63770, .T. ) ;
#184783 = AXIS2_PLACEMENT_3D ( 'NONE', #230238, #30784, #111583 ) ;
#184784 = CARTESIAN_POINT ( 'NONE',  ( 21.14999999999999858, 59.19392724319016708, -220.9828015967491126 ) ) ;
#184785 = DIRECTION ( 'NONE',  ( 0.000000000000000000, -0.4088369013363280513, 0.9126074666063772600 ) ) ;
#184786 = ADVANCED_FACE ( 'NONE', ( #155436 ), #42932, .T. ) ;
#184787 = CARTESIAN_POINT ( 'NONE',  ( -21.08198257630413508, 75.92735667622814333, -209.8597042185394059 ) ) ;
#184788 = ORIENTED_EDGE ( 'NONE', *, *, #138201, .F. ) ;
#184789 = EDGE_CURVE ( 'NONE', #193723, #173680, #209507, .T. ) ;
#184790 = CARTESIAN_POINT ( 'NONE',  ( 23.25000000000000000, 85.60000000001204512, -114.7731074845242460 ) ) ;
#184791 = VERTEX_POINT ( 'NONE', #216645 ) ;
#184792 = FACE_OUTER_BOUND ( 'NONE', #101938, .T. ) ;
#184793 = FACE_OUTER_BOUND ( 'NONE', #152100, .T. ) ;
#184794 = CARTESIAN_POINT ( 'NONE',  ( -21.05000000000000071, 4.436385504674529301, -245.3241086753762659 ) ) ;
#184795 = DIRECTION ( 'NONE',  ( 1.000000000000000000, 0.000000000000000000, 0.000000000000000000 ) ) ;
#184796 = ORIENTED_EDGE ( 'NONE', *, *, #63365, .F. ) ;
#184797 = CARTESIAN_POINT ( 'NONE',  ( -21.00219873199078435, 64.39461131213531075, -96.11046005622981170 ) ) ;
#184798 = AXIS2_PLACEMENT_3D ( 'NONE', #128070, #90197, #108498 ) ;
#184799 = EDGE_LOOP ( 'NONE', ( #135089, #33526, #31120, #222626, #112960 ) ) ;
#184802 = EDGE_LOOP ( 'NONE', ( #111491, #151486, #9617, #17136 ) ) ;
#184801 = DIRECTION ( 'NONE',  ( 1.000000000000000000, 0.000000000000000000, 0.000000000000000000 ) ) ;
#184800 = DIRECTION ( 'NONE',  ( -1.000000000000000000, 0.000000000000000000, 0.000000000000000000 ) ) ;
#184803 = VECTOR ( 'NONE', #31539, 1000.000000000000000 ) ;
#184804 = VECTOR ( 'NONE', #206626, 1000.000000000000000 ) ;
#184805 = AXIS2_PLACEMENT_3D ( 'NONE', #77418, #98246, #56559 ) ;
#184806 = ORIENTED_EDGE ( 'NONE', *, *, #146181, .F. ) ;
#184807 = CARTESIAN_POINT ( 'NONE',  ( 18.59999999999999432, 1.162701749949165642, -142.1000000000000227 ) ) ;
#184808 = ORIENTED_EDGE ( 'NONE', *, *, #46420, .F. ) ;
#184809 = CYLINDRICAL_SURFACE ( 'NONE', #34810, 2.000000000000012879 ) ;
#184810 = CARTESIAN_POINT ( 'NONE',  ( -23.15000000000000213, 64.25000000001249134, -177.0379132551784096 ) ) ;
#184811 = DIRECTION ( 'NONE',  ( 1.000000000000000000, 0.000000000000000000, 0.000000000000000000 ) ) ;
#184812 = PLANE ( 'NONE',  #14425 ) ;
#184813 = CARTESIAN_POINT ( 'NONE',  ( -16.88219499860498374, 9.950206425427586154, -12.64930969010730699 ) ) ;
#184814 = ORIENTED_EDGE ( 'NONE', *, *, #88734, .F. ) ;
#184815 = DIRECTION ( 'NONE',  ( 1.073024830501117725E-15, -0.2128009952263604232, 0.9770955615653316162 ) ) ;
#184816 = DIRECTION ( 'NONE',  ( 0.000000000000000000, 0.000000000000000000, 1.000000000000000000 ) ) ;
#184817 = CYLINDRICAL_SURFACE ( 'NONE', #188513, 0.09999999999999939493 ) ;
#184818 = VERTEX_POINT ( 'NONE', #237505 ) ;
#184819 = DIRECTION ( 'NONE',  ( -1.000000000000000000, -0.000000000000000000, -0.000000000000000000 ) ) ;
#184820 = ORIENTED_EDGE ( 'NONE', *, *, #253354, .F. ) ;
#184821 = DIRECTION ( 'NONE',  ( 2.694716079187273439E-16, 1.000000000000000000, 6.467318590049456648E-15 ) ) ;
#184822 = VECTOR ( 'NONE', #224201, 1000.000000000000000 ) ;
#184823 = CARTESIAN_POINT ( 'NONE',  ( -20.54999999999999716, -4.161311414658873886, -226.0656773515597706 ) ) ;
#184824 = CARTESIAN_POINT ( 'NONE',  ( 20.85000000000000142, 36.22724532936083364, -235.9903003947922002 ) ) ;
#184826 = ORIENTED_EDGE ( 'NONE', *, *, #172759, .T. ) ;
#184825 = CARTESIAN_POINT ( 'NONE',  ( 20.95512820512820440, 10.62384868372303615, -141.6649135690876165 ) ) ;
#184827 = CARTESIAN_POINT ( 'NONE',  ( 20.12499999999999645, 11.68002377302066463, -206.5006728669541189 ) ) ;
#184828 = CARTESIAN_POINT ( 'NONE',  ( -15.39126916658602973, 62.83289218956783628, -216.2009511582250809 ) ) ;
#184829 = EDGE_CURVE ( 'NONE', #53002, #177501, #242828, .T. ) ;
#184830 = CARTESIAN_POINT ( 'NONE',  ( 20.99999999999999645, 22.88362888408687468, -231.1113624623564249 ) ) ;
#184831 = VERTEX_POINT ( 'NONE', #140981 ) ;
#184832 = DIRECTION ( 'NONE',  ( 0.000000000000000000, -6.308085367188393199E-16, -1.000000000000000000 ) ) ;
#184834 = EDGE_CURVE ( 'NONE', #164528, #146084, #101302, .T. ) ;
#184833 = CARTESIAN_POINT ( 'NONE',  ( -23.15000000000000213, 70.79044367282321559, -234.2606625912667937 ) ) ;
#184835 = ORIENTED_EDGE ( 'NONE', *, *, #220977, .F. ) ;
#184837 = CARTESIAN_POINT ( 'NONE',  ( 22.50014994444007144, 64.25028026812033488, -170.1061876412437641 ) ) ;
#184836 = CIRCLE ( 'NONE', #189139, 0.09999999999999939493 ) ;
#184838 = CIRCLE ( 'NONE', #205681, 11.89999999999999325 ) ;
#184839 = EDGE_LOOP ( 'NONE', ( #178500, #34526, #202675, #191927, #181053 ) ) ;
#184840 = CIRCLE ( 'NONE', #72443, 0.1000000000000124678 ) ;
#184841 = ADVANCED_FACE ( 'NONE', ( #97955 ), #137117, .F. ) ;
#184842 = DIRECTION ( 'NONE',  ( 1.000000000000000000, -0.000000000000000000, -0.000000000000000000 ) ) ;
#184845 = ADVANCED_FACE ( 'NONE', ( #39323 ), #38040, .F. ) ;
#184844 = ORIENTED_EDGE ( 'NONE', *, *, #19629, .T. ) ;
#184843 = DIRECTION ( 'NONE',  ( 2.557131231893036985E-16, -0.8660254037844383745, 0.5000000000000003331 ) ) ;
#184848 = EDGE_LOOP ( 'NONE', ( #115874, #132701, #210074, #97250, #163673, #109017 ) ) ;
#184847 = VERTEX_POINT ( 'NONE', #178846 ) ;
#184846 = LINE ( 'NONE', #203131, #176101 ) ;
#184849 = DIRECTION ( 'NONE',  ( 0.000000000000000000, -0.1290532225515392817, -0.9916376685811520986 ) ) ;
#184850 = CARTESIAN_POINT ( 'NONE',  ( -23.25000000000000000, 76.00000000001192291, -105.1231074845242972 ) ) ;
#184851 = DIRECTION ( 'NONE',  ( 0.000000000000000000, 0.000000000000000000, -1.000000000000000000 ) ) ;
#184852 = VECTOR ( 'NONE', #236686, 1000.000000000000000 ) ;
#184854 = DIRECTION ( 'NONE',  ( 1.000000000000000000, 0.000000000000000000, 0.000000000000000000 ) ) ;
#184853 = DIRECTION ( 'NONE',  ( -1.186688945009010077E-16, -1.000000000000000000, -6.982962677686266711E-15 ) ) ;
#184855 = CARTESIAN_POINT ( 'NONE',  ( -16.94445028196808778, 9.992063609708889516, -146.6073301784184935 ) ) ;
#184856 = DIRECTION ( 'NONE',  ( 1.000000000000000000, 0.000000000000000000, 0.000000000000000000 ) ) ;
#184857 = VECTOR ( 'NONE', #53173, 1000.000000000000000 ) ;
#184858 = CARTESIAN_POINT ( 'NONE',  ( -22.48660254037843487, 11.65000000001115588, -33.45000000000002416 ) ) ;
#184859 = ADVANCED_FACE ( 'NONE', ( #255730 ), #155577, .F. ) ;
#184860 = LINE ( 'NONE', #62363, #118258 ) ;
#184861 = EDGE_CURVE ( 'NONE', #165453, #49989, #63955, .T. ) ;
#184862 = TOROIDAL_SURFACE ( 'NONE', #251505, 4.149999999999999467, 0.1000000000000000056 ) ;
#184863 = ORIENTED_EDGE ( 'NONE', *, *, #120220, .F. ) ;
#184864 = EDGE_LOOP ( 'NONE', ( #124111, #215202, #178508, #25462, #42813 ) ) ;
#184865 = CIRCLE ( 'NONE', #18281, 0.1000000000000028644 ) ;
#184866 = SPHERICAL_SURFACE ( 'NONE', #45, 0.1000000000000000056 ) ;
#184868 = EDGE_LOOP ( 'NONE', ( #63938, #144580, #77804, #43819 ) ) ;
#184867 = DIRECTION ( 'NONE',  ( 1.000000000000000000, -0.000000000000000000, -0.000000000000000000 ) ) ;
#184869 = EDGE_LOOP ( 'NONE', ( #15315, #128825, #153857 ) ) ;
#184870 = DIRECTION ( 'NONE',  ( 0.000000000000000000, -6.982962677686266711E-15, 1.000000000000000000 ) ) ;
#184871 = ORIENTED_EDGE ( 'NONE', *, *, #134714, .F. ) ;
#184872 = DIRECTION ( 'NONE',  ( -0.000000000000000000, -0.9770955615653313941, -0.2128009952263603677 ) ) ;
#184873 = AXIS2_PLACEMENT_3D ( 'NONE', #167631, #7233, #68516 ) ;
#184874 = AXIS2_PLACEMENT_3D ( 'NONE', #41533, #218844, #140598 ) ;
#184875 = ADVANCED_FACE ( 'NONE', ( #198368 ), #158007, .T. ) ;
#184876 = ORIENTED_EDGE ( 'NONE', *, *, #29642, .T. ) ;
#184877 = CIRCLE ( 'NONE', #26698, 0.1000000000000028644 ) ;
#184878 = CARTESIAN_POINT ( 'NONE',  ( -16.94445028196808778, 9.992063609708889516, -180.1073301784184366 ) ) ;
#184879 = DIRECTION ( 'NONE',  ( 0.000000000000000000, 0.8660254037844383745, -0.5000000000000003331 ) ) ;
#184880 = EDGE_CURVE ( 'NONE', #63952, #175143, #22330, .T. ) ;
#184881 = AXIS2_PLACEMENT_3D ( 'NONE', #228747, #12272, #30552 ) ;
#184883 = EDGE_LOOP ( 'NONE', ( #194577, #125664, #193924, #91636, #152345 ) ) ;
#184882 = EDGE_LOOP ( 'NONE', ( #126862, #228690, #1702, #228552 ) ) ;
#184884 = EDGE_LOOP ( 'NONE', ( #208131, #123956, #158057, #66059 ) ) ;
#184885 = CARTESIAN_POINT ( 'NONE',  ( -22.39999999999999858, 7.790779598384560245, -66.90000000000004832 ) ) ;
#184886 = EDGE_LOOP ( 'NONE', ( #185192, #231014, #157594, #108657, #187170, #72790, #82602, #193865, #51806, #53698, #28668, #157400, #188366, #185729 ) ) ;
#184887 = EDGE_LOOP ( 'NONE', ( #33643, #150286, #43150, #150477 ) ) ;
#184889 = DIRECTION ( 'NONE',  ( 1.000000000000000000, 0.000000000000000000, 0.000000000000000000 ) ) ;
#184888 = AXIS2_PLACEMENT_3D ( 'NONE', #80891, #221682, #41812 ) ;
#184890 = CARTESIAN_POINT ( 'NONE',  ( -23.25000000000000000, 54.18213181965657554, -236.9344197582443883 ) ) ;
#184892 = ORIENTED_EDGE ( 'NONE', *, *, #32491, .T. ) ;
#184891 = DIRECTION ( 'NONE',  ( 1.000000000000000000, -0.000000000000000000, -0.000000000000000000 ) ) ;
#184893 = CARTESIAN_POINT ( 'NONE',  ( -18.59999999999999787, -26.43935341558978891, -185.6415086075074328 ) ) ;
#184894 = EDGE_CURVE ( 'NONE', #208477, #118994, #163908, .T. ) ;
#184895 = CARTESIAN_POINT ( 'NONE',  ( 19.58285714285715073, 9.015001489659738354, -108.9206528160817555 ) ) ;
#184897 = EDGE_LOOP ( 'NONE', ( #253087, #22027, #156191, #216707 ) ) ;
#184896 = DIRECTION ( 'NONE',  ( 0.000000000000000000, 6.982962677686266711E-15, -1.000000000000000000 ) ) ;
#184898 = CARTESIAN_POINT ( 'NONE',  ( -21.05000000000000071, 1.835341550235569663, -45.05515129256298223 ) ) ;
#184899 = EDGE_LOOP ( 'NONE', ( #201837, #198334, #171739 ) ) ;
#184900 = AXIS2_PLACEMENT_3D ( 'NONE', #43063, #242535, #62630 ) ;
#184901 = CYLINDRICAL_SURFACE ( 'NONE', #199340, 2.600000000000001421 ) ;
#184902 = CIRCLE ( 'NONE', #168390, 0.09999999999999939493 ) ;
#184903 = ADVANCED_FACE ( 'NONE', ( #159265 ), #201316, .F. ) ;
#184904 = ORIENTED_EDGE ( 'NONE', *, *, #172092, .F. ) ;
#184905 = VECTOR ( 'NONE', #242108, 1000.000000000000000 ) ;
#184906 = CARTESIAN_POINT ( 'NONE',  ( 20.94999999999999574, 1.115600667400684642E-11, -167.4999999999999716 ) ) ;
#184907 = CYLINDRICAL_SURFACE ( 'NONE', #99557, 0.09999999999999939493 ) ;
#184909 = EDGE_CURVE ( 'NONE', #99703, #72316, #68050, .T. ) ;
#184908 = ORIENTED_EDGE ( 'NONE', *, *, #207833, .T. ) ;
#184911 = CARTESIAN_POINT ( 'NONE',  ( -21.05000000000000071, 76.00000000001234923, -167.1231074845243825 ) ) ;
#184910 = CARTESIAN_POINT ( 'NONE',  ( 20.94999999999999929, 68.48451787451661232, -224.2224406095231757 ) ) ;
#184912 = DIRECTION ( 'NONE',  ( 0.000000000000000000, 0.5000000000000004441, 0.8660254037844384856 ) ) ;
#184913 = CARTESIAN_POINT ( 'NONE',  ( -17.71734398241074260, 21.30575908404109953, -229.0269313818040189 ) ) ;
#184914 = ORIENTED_EDGE ( 'NONE', *, *, #253996, .T. ) ;
#184915 = ORIENTED_EDGE ( 'NONE', *, *, #4237, .T. ) ;
#184916 = CARTESIAN_POINT ( 'NONE',  ( -20.54999999999999716, 67.23127455305835554, -235.8551265064784559 ) ) ;
#184917 = DIRECTION ( 'NONE',  ( 0.000000000000000000, 6.467318590049456648E-15, -1.000000000000000000 ) ) ;
#184918 = EDGE_LOOP ( 'NONE', ( #65678, #197797, #52800, #184643 ) ) ;
#184919 = FACE_OUTER_BOUND ( 'NONE', #123264, .T. ) ;
#184920 = EDGE_LOOP ( 'NONE', ( #45838, #75158, #161695, #213047, #118924, #130978 ) ) ;
#184921 = EDGE_CURVE ( 'NONE', #101735, #117327, #105614, .T. ) ;
#184922 = DIRECTION ( 'NONE',  ( -1.000000000000000000, 0.000000000000000000, 0.000000000000000000 ) ) ;
#184923 = ORIENTED_EDGE ( 'NONE', *, *, #211467, .F. ) ;
#184925 = EDGE_CURVE ( 'NONE', #208289, #64347, #213799, .T. ) ;
#184924 = CARTESIAN_POINT ( 'NONE',  ( 18.59999999999999076, 43.16354019706792400, -239.5695141926698284 ) ) ;
#184926 = VECTOR ( 'NONE', #57407, 1000.000000000000114 ) ;
#184927 = AXIS2_PLACEMENT_3D ( 'NONE', #230998, #57457, #32817 ) ;
#184928 = ORIENTED_EDGE ( 'NONE', *, *, #220982, .F. ) ;
#184929 = CARTESIAN_POINT ( 'NONE',  ( 18.59999999999999787, -1.835859311432481045, -179.0044391687985410 ) ) ;
#184930 = CIRCLE ( 'NONE', #147523, 7.720710678118663850 ) ;
#184931 = VERTEX_POINT ( 'NONE', #120159 ) ;
#184932 = VERTEX_POINT ( 'NONE', #156712 ) ;
#184933 = EDGE_LOOP ( 'NONE', ( #140909, #20916, #150439, #207411 ) ) ;
#184934 = CIRCLE ( 'NONE', #139106, 7.800000000000001599 ) ;
#184935 = FACE_OUTER_BOUND ( 'NONE', #197146, .T. ) ;
#184936 = DIRECTION ( 'NONE',  ( 0.000000000000000000, 0.000000000000000000, 1.000000000000000000 ) ) ;
#184937 = VECTOR ( 'NONE', #78106, 1000.000000000000000 ) ;
#184938 = PLANE ( 'NONE',  #221435 ) ;
#184939 = LINE ( 'NONE', #67558, #28020 ) ;
#184940 = CARTESIAN_POINT ( 'NONE',  ( -6.000000000000002665, -11.65000000000000036, 14.00000000000000178 ) ) ;
#184941 =( BOUNDED_SURFACE ( )  B_SPLINE_SURFACE ( 3, 2, ( 
 ( #171241, #172529, #249460 ),
 ( #69540, #211608, #229884 ),
 ( #49948, #134604, #33016 ),
 ( #133354, #210329, #129502 ) ),
 .UNSPECIFIED., .F., .F., .F. ) 
 B_SPLINE_SURFACE_WITH_KNOTS ( ( 4, 4 ),
 ( 3, 3 ),
 ( 3.658908243880901523, 4.712388980384689674 ),
 ( 0.000000000000000000, 1.000000000000000000 ),
 .UNSPECIFIED. ) 
 GEOMETRIC_REPRESENTATION_ITEM ( )  RATIONAL_B_SPLINE_SURFACE ( (
 ( 1.000000000000000000, 0.8984936768950576580, 1.000000000000000000),
 ( 1.000000000000000000, 0.8646876308615482065, 1.000000000000000000),
 ( 1.000000000000000000, 0.7953136715913182719, 1.000000000000000000),
 ( 1.000000000000000000, 0.7071067811865414665, 1.000000000000000000) ) ) 
 REPRESENTATION_ITEM ( '' )  SURFACE ( )  );
#184943 = CARTESIAN_POINT ( 'NONE',  ( 21.05000000000000071, 59.03303942657512238, -225.8023344323644324 ) ) ;
#184942 = DIRECTION ( 'NONE',  ( 0.000000000000000000, -0.4721928772777332917, -0.8814952561688437216 ) ) ;
#184945 = ORIENTED_EDGE ( 'NONE', *, *, #91763, .T. ) ;
#184944 = DIRECTION ( 'NONE',  ( 0.000000000000000000, 0.000000000000000000, 1.000000000000000000 ) ) ;
#184946 = ORIENTED_EDGE ( 'NONE', *, *, #215719, .F. ) ;
#184947 = AXIS2_PLACEMENT_3D ( 'NONE', #234083, #189838, #114137 ) ;
#184948 = DIRECTION ( 'NONE',  ( 0.000000000000000000, 0.000000000000000000, -1.000000000000000000 ) ) ;
#184949 = ORIENTED_EDGE ( 'NONE', *, *, #67932, .F. ) ;
#184950 = ORIENTED_EDGE ( 'NONE', *, *, #11377, .T. ) ;
#184951 = CARTESIAN_POINT ( 'NONE',  ( -23.15000000000000213, 71.65000000001199965, -115.2731074845243171 ) ) ;
#184952 = AXIS2_PLACEMENT_3D ( 'NONE', #56901, #132635, #212181 ) ;
#184953 = DIRECTION ( 'NONE',  ( 0.000000000000000000, -6.982962677686266711E-15, 1.000000000000000000 ) ) ;
#184954 = DIRECTION ( 'NONE',  ( -0.000000000000000000, -0.000000000000000000, -1.000000000000000000 ) ) ;
#184955 = CIRCLE ( 'NONE', #176588, 0.09999999999999939493 ) ;
#184956 = FACE_OUTER_BOUND ( 'NONE', #2968, .T. ) ;
#184957 = AXIS2_PLACEMENT_3D ( 'NONE', #196455, #157375, #60788 ) ;
#184958 = CIRCLE ( 'NONE', #184764, 0.3999999999999948597 ) ;
#184959 = DIRECTION ( 'NONE',  ( 0.000000000000000000, 0.8814952561688476074, -0.4721928772777262417 ) ) ;
#184960 = ORIENTED_EDGE ( 'NONE', *, *, #128540, .T. ) ;
#184961 = ORIENTED_EDGE ( 'NONE', *, *, #132700, .T. ) ;
#184962 =( BOUNDED_CURVE ( )  B_SPLINE_CURVE ( 3, ( #208142, #2526, #164197, #242427 ),
 .UNSPECIFIED., .F., .F. ) 
 B_SPLINE_CURVE_WITH_KNOTS ( ( 4, 4 ),
 ( 3.192897208853993529, 4.712388980384689674 ),
 .UNSPECIFIED. ) 
 CURVE ( )  GEOMETRIC_REPRESENTATION_ITEM ( )  RATIONAL_B_SPLINE_CURVE ( ( 1.000000000000000000, 0.8166740347213228279, 0.8166740347213228279, 1.000000000000000000 ) ) 
 REPRESENTATION_ITEM ( '' )  );
#184963 = CARTESIAN_POINT ( 'NONE',  ( 23.24999999999999645, 67.34812900481119868, -214.0300458246130972 ) ) ;
#184964 = ORIENTED_EDGE ( 'NONE', *, *, #156955, .F. ) ;
#184965 = CARTESIAN_POINT ( 'NONE',  ( -21.65000000000000213, 68.29142135624930177, -115.3731074845243540 ) ) ;
#184966 = CARTESIAN_POINT ( 'NONE',  ( -17.11825945287482753, 65.95000000001232365, -157.3731074845244393 ) ) ;
#184967 = DIRECTION ( 'NONE',  ( 0.000000000000000000, 0.000000000000000000, -1.000000000000000000 ) ) ;
#184969 = CIRCLE ( 'NONE', #205811, 0.09999999999999939493 ) ;
#184968 = CARTESIAN_POINT ( 'NONE',  ( 21.40925344232283223, -1.320255649883980809, -194.4729340772759372 ) ) ;
#184970 = FACE_OUTER_BOUND ( 'NONE', #163093, .T. ) ;
#184971 = LINE ( 'NONE', #205813, #42556 ) ;
#184972 = ORIENTED_EDGE ( 'NONE', *, *, #24403, .F. ) ;
#184973 = DIRECTION ( 'NONE',  ( 0.000000000000000000, 6.982962677686266711E-15, -1.000000000000000000 ) ) ;
#184974 = CARTESIAN_POINT ( 'NONE',  ( 21.05000000000000071, -1.736257131586239844, -78.56865232901753870 ) ) ;
#184975 = CARTESIAN_POINT ( 'NONE',  ( -20.94999999999999929, -11.64999999998884483, -64.10000000000000853 ) ) ;
#184976 = FACE_OUTER_BOUND ( 'NONE', #191425, .T. ) ;
#184977 = AXIS2_PLACEMENT_3D ( 'NONE', #25498, #102418, #204111 ) ;
#184979 = EDGE_CURVE ( 'NONE', #172995, #28201, #55529, .T. ) ;
#184978 = CARTESIAN_POINT ( 'NONE',  ( -18.58671080940900211, 85.40693285883851615, -95.89895301961956875 ) ) ;
#184980 = CARTESIAN_POINT ( 'NONE',  ( -18.50000000000000000, 9.150000000011157653, -146.3500000000000227 ) ) ;
#184981 = CIRCLE ( 'NONE', #255658, 0.09999999999999854838 ) ;
#184982 =( BOUNDED_CURVE ( )  B_SPLINE_CURVE ( 3, ( #252551, #115624, #32263, #92198 ),
 .UNSPECIFIED., .F., .F. ) 
 B_SPLINE_CURVE_WITH_KNOTS ( ( 4, 4 ),
 ( 0.000000000000000000, 1.570796326794908992 ),
 .UNSPECIFIED. ) 
 CURVE ( )  GEOMETRIC_REPRESENTATION_ITEM ( )  RATIONAL_B_SPLINE_CURVE ( ( 1.000000000000000000, 0.8047378541243619399, 0.8047378541243619399, 1.000000000000000000 ) ) 
 REPRESENTATION_ITEM ( '' )  );
#184983 = AXIS2_PLACEMENT_3D ( 'NONE', #234579, #216293, #156366 ) ;
#184984 = ORIENTED_EDGE ( 'NONE', *, *, #135086, .T. ) ;
#184985 = AXIS2_PLACEMENT_3D ( 'NONE', #245651, #5724, #42313 ) ;
#184986 = CARTESIAN_POINT ( 'NONE',  ( -17.01764560440407692, 66.05000000001231797, -157.2731074853133180 ) ) ;
#184987 = ADVANCED_FACE ( 'NONE', ( #240074 ), #184733, .T. ) ;
#184988 = EDGE_LOOP ( 'NONE', ( #246223, #240015, #53647, #237398 ) ) ;
#184989 = CARTESIAN_POINT ( 'NONE',  ( -23.15000000000000213, 62.08148826970418099, -247.6553521922769221 ) ) ;
#184990 = DIRECTION ( 'NONE',  ( 0.000000000000000000, 0.000000000000000000, -1.000000000000000000 ) ) ;
#184992 = EDGE_CURVE ( 'NONE', #155242, #176792, #202228, .T. ) ;
#184991 = CARTESIAN_POINT ( 'NONE',  ( 21.14999999999999858, 61.95748721176698837, -221.7323031544521825 ) ) ;
#184993 = ADVANCED_FACE ( 'NONE', ( #143525 ), #18889, .T. ) ;
#184994 = EDGE_LOOP ( 'NONE', ( #92534, #29192, #31992, #111419 ) ) ;
#184995 = FACE_OUTER_BOUND ( 'NONE', #245815, .T. ) ;
#184996 = CARTESIAN_POINT ( 'NONE',  ( 23.14999999999999503, 6.550000000011156231, -121.7500000000000426 ) ) ;
#184997 = FACE_OUTER_BOUND ( 'NONE', #238084, .T. ) ;
#184998 = FACE_BOUND ( 'NONE', #226081, .T. ) ;
#184999 = CIRCLE ( 'NONE', #147401, 7.800000000000001599 ) ;
#185001 = CARTESIAN_POINT ( 'NONE',  ( -18.59999999999999787, 7.070967871809997973, -70.74656422186831151 ) ) ;
#185000 = AXIS2_PLACEMENT_3D ( 'NONE', #43453, #64300, #143819 ) ;
#185002 = CARTESIAN_POINT ( 'NONE',  ( 22.40736611211992368, 76.00000000001246292, -181.6726782920691505 ) ) ;
#185003 = ORIENTED_EDGE ( 'NONE', *, *, #139679, .T. ) ;
#185004 = VERTEX_POINT ( 'NONE', #203512 ) ;
#185005 = CARTESIAN_POINT ( 'NONE',  ( 23.14999999999998437, 4.959819536546799335E-16, 4.049999999999998934 ) ) ;
#185007 = EDGE_LOOP ( 'NONE', ( #185649, #207033, #200412, #209666 ) ) ;
#185006 = DIRECTION ( 'NONE',  ( -0.000000000000000000, 0.9126074666063770380, 0.4088369013363281068 ) ) ;
#185008 = CARTESIAN_POINT ( 'NONE',  ( 20.94999999999999574, 77.26178616857765746, -195.4366085209788935 ) ) ;
#185009 = EDGE_CURVE ( 'NONE', #219222, #5557, #238738, .T. ) ;
#185010 = DIRECTION ( 'NONE',  ( 1.000000000000000000, 0.000000000000000000, 0.000000000000000000 ) ) ;
#185011 = ORIENTED_EDGE ( 'NONE', *, *, #135493, .F. ) ;
#185012 = LINE ( 'NONE', #248844, #201327 ) ;
#185013 = DIRECTION ( 'NONE',  ( -0.7071067811865474617, -0.7071067811865474617, -2.044391222244499837E-16 ) ) ;
#185014 = ORIENTED_EDGE ( 'NONE', *, *, #84864, .T. ) ;
#185015 = CARTESIAN_POINT ( 'NONE',  ( 23.14999999999999503, 11.65000000001116298, -45.65000000000000568 ) ) ;
#185016 = AXIS2_PLACEMENT_3D ( 'NONE', #19283, #91777, #9667 ) ;
#185017 = DIRECTION ( 'NONE',  ( 0.000000000000000000, 0.000000000000000000, -1.000000000000000000 ) ) ;
#185018 = ADVANCED_FACE ( 'NONE', ( #69157 ), #187818, .T. ) ;
#185019 = ORIENTED_EDGE ( 'NONE', *, *, #247258, .F. ) ;
#185020 = VERTEX_POINT ( 'NONE', #24897 ) ;
#185021 = CARTESIAN_POINT ( 'NONE',  ( 20.94999999999999929, 85.00000000001222134, -146.4170766071767389 ) ) ;
#185022 = FACE_OUTER_BOUND ( 'NONE', #149622, .T. ) ;
#185023 = DIRECTION ( 'NONE',  ( -1.000000000000000000, 0.000000000000000000, 0.000000000000000000 ) ) ;
#185024 = CYLINDRICAL_SURFACE ( 'NONE', #65237, 4.049999999999995381 ) ;
#185025 = DIRECTION ( 'NONE',  ( 0.000000000000000000, 0.2128009952263620885, -0.9770955615653311721 ) ) ;
#185026 = DIRECTION ( 'NONE',  ( -1.000000000000000000, -0.000000000000000000, -0.000000000000000000 ) ) ;
#185027 = ADVANCED_FACE ( 'NONE', ( #183944 ), #228218, .F. ) ;
#185029 = CARTESIAN_POINT ( 'NONE',  ( -18.39999999999999858, -9.499999999988849808, -74.03206939669971121 ) ) ;
#185028 = CARTESIAN_POINT ( 'NONE',  ( 22.47071067811865319, 7.720074744498043984, 0.09909245470260480415 ) ) ;
#185030 = CARTESIAN_POINT ( 'NONE',  ( 23.24999999999999289, 11.50215294792677767, -198.5972978622482970 ) ) ;
#185031 = CARTESIAN_POINT ( 'NONE',  ( -18.59999999999999787, 18.18127959618848166, -237.5711165786817389 ) ) ;
#185033 = DIRECTION ( 'NONE',  ( 0.000000000000000000, 0.9947597004326491632, -0.1022405907413782566 ) ) ;
#185032 = AXIS2_PLACEMENT_3D ( 'NONE', #139263, #153777, #137986 ) ;
#185034 = VERTEX_POINT ( 'NONE', #84805 ) ;
#185035 = AXIS2_PLACEMENT_3D ( 'NONE', #88173, #109042, #6089 ) ;
#185036 = ORIENTED_EDGE ( 'NONE', *, *, #241026, .T. ) ;
#185037 = DIRECTION ( 'NONE',  ( 2.659396599871503635E-15, 0.4701782451859590206, 0.8825714802517993229 ) ) ;
#185040 = CARTESIAN_POINT ( 'NONE',  ( -23.15000000000000213, 11.65000000001115588, -121.8500000000000369 ) ) ;
#185039 = DIRECTION ( 'NONE',  ( -1.020425574104004196E-15, -6.982962677686266711E-15, 1.000000000000000000 ) ) ;
#185038 = AXIS2_PLACEMENT_3D ( 'NONE', #122422, #62448, #201959 ) ;
#185041 = AXIS2_PLACEMENT_3D ( 'NONE', #27163, #187506, #107944 ) ;
#185042 = CARTESIAN_POINT ( 'NONE',  ( 20.95576188350343116, 39.26765041487632857, -236.7575746322726502 ) ) ;
#185043 = DIRECTION ( 'NONE',  ( -0.000000000000000000, -1.000000000000000000, -8.609265936414532828E-15 ) ) ;
#185044 = DIRECTION ( 'NONE',  ( -1.000000000000000000, 0.000000000000000000, -0.000000000000000000 ) ) ;
#185045 = ORIENTED_EDGE ( 'NONE', *, *, #145146, .F. ) ;
#185046 = EDGE_LOOP ( 'NONE', ( #154294, #231865, #161660, #15286 ) ) ;
#185047 = EDGE_CURVE ( 'NONE', #63983, #83974, #13883, .T. ) ;
#185048 = CARTESIAN_POINT ( 'NONE',  ( -12.48127053791144903, 9.376580978043939751, -17.62694624701194002 ) ) ;
#185049 = ORIENTED_EDGE ( 'NONE', *, *, #186038, .F. ) ;
#185051 = DIRECTION ( 'NONE',  ( -0.000000000000000000, 0.000000000000000000, -1.000000000000000000 ) ) ;
#185050 = CIRCLE ( 'NONE', #68537, 12.87499999999999822 ) ;
#185052 = EDGE_CURVE ( 'NONE', #79373, #226022, #97214, .T. ) ;
#185053 = ADVANCED_FACE ( 'NONE', ( #88667 ), #59632, .T. ) ;
#185054 = VERTEX_POINT ( 'NONE', #186524 ) ;
#185055 = CARTESIAN_POINT ( 'NONE',  ( -18.50016250449483479, 18.35558276679128298, -236.8903279188150748 ) ) ;
#185056 = VERTEX_POINT ( 'NONE', #7896 ) ;
#185057 = ADVANCED_FACE ( 'NONE', ( #182678 ), #247090, .T. ) ;
#185059 = EDGE_CURVE ( 'NONE', #141855, #71313, #59831, .T. ) ;
#185058 = DIRECTION ( 'NONE',  ( -1.000000000000000000, -0.000000000000000000, 0.000000000000000000 ) ) ;
#185060 = DIRECTION ( 'NONE',  ( 1.000000000000000000, 0.000000000000000000, 0.000000000000000000 ) ) ;
#185061 = LINE ( 'NONE', #6422, #86612 ) ;
#185062 = CIRCLE ( 'NONE', #218361, 0.2000000000000005107 ) ;
#185064 = CARTESIAN_POINT ( 'NONE',  ( 18.49351773456749370, -9.443025695134306119, -141.1853255260278104 ) ) ;
#185063 = AXIS2_PLACEMENT_3D ( 'NONE', #29256, #108746, #89174 ) ;
#185065 = CARTESIAN_POINT ( 'NONE',  ( -21.14999999999994174, 77.83551161375991967, -47.62760213295649692 ) ) ;
#185067 = AXIS2_PLACEMENT_3D ( 'NONE', #78895, #60624, #77608 ) ;
#185066 = CARTESIAN_POINT ( 'NONE',  ( -23.15000000000000213, 1.115600667400684642E-11, -167.5000000000000284 ) ) ;
#185068 = ADVANCED_FACE ( 'NONE', ( #127834 ), #1389, .T. ) ;
#185069 = CARTESIAN_POINT ( 'NONE',  ( -22.59999999999999787, 64.25043287652255231, -103.1239658536231047 ) ) ;
#185070 = DIRECTION ( 'NONE',  ( -1.000000000000000000, 0.000000000000000000, 0.000000000000000000 ) ) ;
#185072 = VERTEX_POINT ( 'NONE', #83523 ) ;
#185071 = CARTESIAN_POINT ( 'NONE',  ( 18.49362639424899157, -0.6580137145852484881, -242.3516021320601794 ) ) ;
#185074 = CARTESIAN_POINT ( 'NONE',  ( -20.64999999999999858, -9.399999999988850163, -143.8939691226524644 ) ) ;
#185073 = CARTESIAN_POINT ( 'NONE',  ( 22.39999999999999503, 31.98723526783714277, -238.8784020251475511 ) ) ;
#185075 = CIRCLE ( 'NONE', #189365, 0.09999999999999939493 ) ;
#185076 = ORIENTED_EDGE ( 'NONE', *, *, #217061, .F. ) ;
#185078 = VERTEX_POINT ( 'NONE', #35187 ) ;
#185077 = DIRECTION ( 'NONE',  ( 1.000000000000000000, 0.000000000000000000, 0.000000000000000000 ) ) ;
#185079 = ADVANCED_FACE ( 'NONE', ( #249076 ), #70459, .F. ) ;
#185080 = ORIENTED_EDGE ( 'NONE', *, *, #69602, .T. ) ;
#185081 = CARTESIAN_POINT ( 'NONE',  ( 23.14999999999999503, 69.35000000001222986, -148.8731074845244109 ) ) ;
#185083 = EDGE_CURVE ( 'NONE', #77835, #34405, #55964, .T. ) ;
#185082 = ADVANCED_FACE ( 'NONE', ( #230799 ), #169567, .F. ) ;
#185084 = CARTESIAN_POINT ( 'NONE',  ( -22.37643362114956957, 29.65906341269005608, -252.5784446511937347 ) ) ;
#185085 = VECTOR ( 'NONE', #78954, 1000.000000000000227 ) ;
#185086 = CARTESIAN_POINT ( 'NONE',  ( 20.94999999999999929, 1.115600667400684642E-11, -33.50000000000000000 ) ) ;
#185087 = DIRECTION ( 'NONE',  ( 1.000000000000000000, 0.000000000000000000, 0.000000000000000000 ) ) ;
#185088 = DIRECTION ( 'NONE',  ( -1.000000000000000000, 0.000000000000000000, 0.000000000000000000 ) ) ;
#185089 = VECTOR ( 'NONE', #24489, 1000.000000000000114 ) ;
#185090 = ORIENTED_EDGE ( 'NONE', *, *, #114198, .T. ) ;
#185091 = AXIS2_PLACEMENT_3D ( 'NONE', #140835, #41758, #28641 ) ;
#185092 = FACE_OUTER_BOUND ( 'NONE', #73661, .T. ) ;
#185093 = TOROIDAL_SURFACE ( 'NONE', #159582, 11.65000000000000036, 0.1000000000000000056 ) ;
#185094 = EDGE_CURVE ( 'NONE', #18698, #201752, #53422, .T. ) ;
#185095 = DIRECTION ( 'NONE',  ( 0.000000000000000000, -6.982962677686266711E-15, 1.000000000000000000 ) ) ;
#185096 = VERTEX_POINT ( 'NONE', #172131 ) ;
#185097 = ORIENTED_EDGE ( 'NONE', *, *, #226465, .T. ) ;
#185098 = DIRECTION ( 'NONE',  ( -0.000000000000000000, 1.000000000000000000, 8.717686153663073805E-15 ) ) ;
#185099 = ADVANCED_FACE ( 'NONE', ( #232081 ), #188855, .F. ) ;
#185100 = EDGE_CURVE ( 'NONE', #57467, #46518, #113840, .T. ) ;
#185101 = EDGE_LOOP ( 'NONE', ( #87671, #42235 ) ) ;
#185102 = SPHERICAL_SURFACE ( 'NONE', #154976, 0.1000000000000000056 ) ;
#185103 = ORIENTED_EDGE ( 'NONE', *, *, #186549, .T. ) ;
#185104 = EDGE_CURVE ( 'NONE', #73834, #207677, #192942, .T. ) ;
#185105 = DIRECTION ( 'NONE',  ( 0.000000000000000000, 0.000000000000000000, -1.000000000000000000 ) ) ;
#185106 = FACE_OUTER_BOUND ( 'NONE', #103948, .T. ) ;
#185107 = DIRECTION ( 'NONE',  ( 1.000000000000000000, 0.000000000000000000, 0.000000000000000000 ) ) ;
#185108 = DIRECTION ( 'NONE',  ( 0.000000000000000000, 0.000000000000000000, 1.000000000000000000 ) ) ;
#185109 = ORIENTED_EDGE ( 'NONE', *, *, #189710, .T. ) ;
#185110 = EDGE_CURVE ( 'NONE', #248008, #146487, #91276, .T. ) ;
#185111 = CARTESIAN_POINT ( 'NONE',  ( -20.94999999999999929, 43.52285900727589762, -245.0935880436369985 ) ) ;
#185112 = TOROIDAL_SURFACE ( 'NONE', #239279, 4.149999999999999467, 0.1000000000000000056 ) ;
#185113 = AXIS2_PLACEMENT_3D ( 'NONE', #84697, #228117, #49467 ) ;
#185114 = CARTESIAN_POINT ( 'NONE',  ( -17.04761207306817994, 51.58760699400681915, -231.8766993777581717 ) ) ;
#185115 = CARTESIAN_POINT ( 'NONE',  ( 20.94999999999999929, 44.05869416168422958, -258.6139110589941197 ) ) ;
#185116 = CARTESIAN_POINT ( 'NONE',  ( 20.94999999999999929, 65.27628289530511552, -195.8581939154368285 ) ) ;
#185117 = AXIS2_PLACEMENT_3D ( 'NONE', #141180, #142452, #61640 ) ;
#185118 = EDGE_LOOP ( 'NONE', ( #255264, #244068, #197978, #123276, #34939, #15954, #55130, #214734 ) ) ;
#185120 = DIRECTION ( 'NONE',  ( 1.000000000000000000, -0.000000000000000000, -0.000000000000000000 ) ) ;
#185119 = CARTESIAN_POINT ( 'NONE',  ( -21.93340585971863632, 7.324147022866478451, -134.0000000000000000 ) ) ;
#185121 = VERTEX_POINT ( 'NONE', #10453 ) ;
#185124 = VERTEX_POINT ( 'NONE', #135507 ) ;
#185123 =( NAMED_UNIT ( * ) SI_UNIT ( $, .STERADIAN. ) SOLID_ANGLE_UNIT ( ) );
#185122 =( NAMED_UNIT ( * ) SI_UNIT ( $, .STERADIAN. ) SOLID_ANGLE_UNIT ( ) );
#185125 = VERTEX_POINT ( 'NONE', #229501 ) ;
#185126 = CARTESIAN_POINT ( 'NONE',  ( 21.05000000000000071, 10.39655183198268418, -207.4949966697317620 ) ) ;
#185127 = AXIS2_PLACEMENT_3D ( 'NONE', #162369, #77652, #120684 ) ;
#185128 = DIRECTION ( 'NONE',  ( -1.000000000000000000, -0.000000000000000000, -0.000000000000000000 ) ) ;
#185129 = VECTOR ( 'NONE', #255109, 1000.000000000000000 ) ;
#185130 = EDGE_LOOP ( 'NONE', ( #204039, #251259, #148959, #51296 ) ) ;
#185131 = DIRECTION ( 'NONE',  ( 0.000000000000000000, -6.789366196018718420E-15, 1.000000000000000000 ) ) ;
#185132 = LINE ( 'NONE', #6483, #11204 ) ;
#185133 = AXIS2_PLACEMENT_3D ( 'NONE', #250780, #209092, #115132 ) ;
#185134 = CARTESIAN_POINT ( 'NONE',  ( -23.25000000000000000, 80.80934863333322937, -192.8037999715871535 ) ) ;
#185136 = ORIENTED_EDGE ( 'NONE', *, *, #17479, .F. ) ;
#185135 = CARTESIAN_POINT ( 'NONE',  ( 20.96077737575326694, 11.62390063401587348, -93.64079195710665715 ) ) ;
#185137 = CIRCLE ( 'NONE', #218418, 0.3999999999999973022 ) ;
#185138 = CIRCLE ( 'NONE', #172711, 0.1000000000000002692 ) ;
#185139 = CIRCLE ( 'NONE', #164305, 0.1000000000000002554 ) ;
#185140 = EDGE_LOOP ( 'NONE', ( #40609, #203387, #15930, #120537 ) ) ;
#185141 = CARTESIAN_POINT ( 'NONE',  ( 19.81427058490526605, 64.33143601963001856, -78.27310748452438816 ) ) ;
#185142 = DIRECTION ( 'NONE',  ( -0.000000000000000000, 1.000000000000000000, -0.000000000000000000 ) ) ;
#185143 = DIRECTION ( 'NONE',  ( -1.000000000000000000, 0.000000000000000000, 0.000000000000000000 ) ) ;
#185144 = ORIENTED_EDGE ( 'NONE', *, *, #165108, .T. ) ;
#185145 = CARTESIAN_POINT ( 'NONE',  ( -16.80469485234341320, 9.942151663152191787, -188.3099668439311074 ) ) ;
#185146 = EDGE_LOOP ( 'NONE', ( #176351, #101758, #185641, #143893 ) ) ;
#185147 = CARTESIAN_POINT ( 'NONE',  ( 21.05000000000000071, 18.71397270169369875, -229.9382605683272232 ) ) ;
#185148 = CARTESIAN_POINT ( 'NONE',  ( -22.50000000000000000, 64.35023708198045256, -170.1119174609113713 ) ) ;
#185149 = DIRECTION ( 'NONE',  ( 1.000000000000000000, 0.000000000000000000, 0.000000000000000000 ) ) ;
#185150 = AXIS2_PLACEMENT_3D ( 'NONE', #57677, #18578, #194675 ) ;
#185151 = ORIENTED_EDGE ( 'NONE', *, *, #72898, .F. ) ;
#185152 = CYLINDRICAL_SURFACE ( 'NONE', #145951, 0.1000000000000052097 ) ;
#185153 = AXIS2_PLACEMENT_3D ( 'NONE', #74916, #153183, #253509 ) ;
#185154 = EDGE_CURVE ( 'NONE', #228990, #114385, #108740, .T. ) ;
#185155 = ORIENTED_EDGE ( 'NONE', *, *, #105400, .F. ) ;
#185156 = ADVANCED_FACE ( 'NONE', ( #109528 ), #113400, .T. ) ;
#185157 = AXIS2_PLACEMENT_3D ( 'NONE', #140626, #162782, #183620 ) ;
#185158 = B_SPLINE_CURVE_WITH_KNOTS ( 'NONE', 3,
 ( #1174, #59859, #62463, #83269, #141981, #173792, #42897, #238519, #253258, #39063 ),
 .UNSPECIFIED., .F., .F.,
 ( 4, 3, 3, 4 ),
 ( 0.000000000000000000, 0.0002000000000002785953, 0.001000000000045107602, 0.001967863649472123035 ),
 .UNSPECIFIED. ) ;
#185159 = AXIS2_PLACEMENT_3D ( 'NONE', #97285, #56883, #174352 ) ;
#185160 = VERTEX_POINT ( 'NONE', #153862 ) ;
#185161 = AXIS2_PLACEMENT_3D ( 'NONE', #42025, #26303, #40763 ) ;
#185162 = ORIENTED_EDGE ( 'NONE', *, *, #201940, .T. ) ;
#185163 = ORIENTED_EDGE ( 'NONE', *, *, #67965, .F. ) ;
#185164 = EDGE_CURVE ( 'NONE', #185550, #6865, #76398, .T. ) ;
#185165 = DIRECTION ( 'NONE',  ( 0.7071067811865474617, -0.7071067811865474617, -4.937700262164531476E-15 ) ) ;
#185166 = ORIENTED_EDGE ( 'NONE', *, *, #196277, .T. ) ;
#185169 = EDGE_CURVE ( 'NONE', #153341, #70373, #222135, .T. ) ;
#185168 = VERTEX_POINT ( 'NONE', #89966 ) ;
#185167 = DIRECTION ( 'NONE',  ( 1.000000000000000000, -0.000000000000000000, 0.000000000000000000 ) ) ;
#185170 = EDGE_LOOP ( 'NONE', ( #57696, #68476, #164432, #160133 ) ) ;
#185172 = VERTEX_POINT ( 'NONE', #114681 ) ;
#185171 = EDGE_LOOP ( 'NONE', ( #240090, #9052, #222813, #146939, #191721 ) ) ;
#185173 = DIRECTION ( 'NONE',  ( -0.000000000000000000, -0.03181660087583042251, 0.9994937237965568766 ) ) ;
#185174 = ORIENTED_EDGE ( 'NONE', *, *, #147890, .T. ) ;
#185175 = DIRECTION ( 'NONE',  ( 4.026293107431335996E-15, 0.8700118002898393765, -0.4930308989875104575 ) ) ;
#185176 = DIRECTION ( 'NONE',  ( 0.000000000000000000, 0.000000000000000000, 1.000000000000000000 ) ) ;
#185177 = AXIS2_PLACEMENT_3D ( 'NONE', #245216, #233041, #225607 ) ;
#185178 = DIRECTION ( 'NONE',  ( 1.000000000000000000, 0.000000000000000000, 0.000000000000000000 ) ) ;
#185179 = ADVANCED_FACE ( 'NONE', ( #194247 ), #174707, .T. ) ;
#185180 = CARTESIAN_POINT ( 'NONE',  ( -18.33682934331556780, 86.98715295972735362, -199.3478004332870341 ) ) ;
#185181 = EDGE_CURVE ( 'NONE', #4003, #68241, #179804, .T. ) ;
#185182 = ORIENTED_EDGE ( 'NONE', *, *, #102572, .F. ) ;
#185183 = ORIENTED_EDGE ( 'NONE', *, *, #38217, .F. ) ;
#185184 = DIRECTION ( 'NONE',  ( 0.000000000000000000, -0.8454177738465993297, -0.5341055959866553016 ) ) ;
#185185 = AXIS2_PLACEMENT_3D ( 'NONE', #225722, #207490, #125374 ) ;
#185187 = ORIENTED_EDGE ( 'NONE', *, *, #174713, .T. ) ;
#185186 = CARTESIAN_POINT ( 'NONE',  ( -16.93294127766158752, 65.99671989705768738, -182.5932002186951877 ) ) ;
#185189 = EDGE_LOOP ( 'NONE', ( #194710, #257526, #61444, #81128 ) ) ;
#185188 = CARTESIAN_POINT ( 'NONE',  ( 20.94999999999999929, 70.10000000001220144, -146.7422072491807796 ) ) ;
#185190 = EDGE_LOOP ( 'NONE', ( #72030, #162381, #233600, #165201, #75164 ) ) ;
#185191 = DIRECTION ( 'NONE',  ( -1.000000000000000000, 0.000000000000000000, 0.000000000000000000 ) ) ;
#185192 = ORIENTED_EDGE ( 'NONE', *, *, #62469, .F. ) ;
#185193 = EDGE_CURVE ( 'NONE', #182870, #46719, #20733, .T. ) ;
#185194 = ORIENTED_EDGE ( 'NONE', *, *, #38386, .T. ) ;
#185195 = CARTESIAN_POINT ( 'NONE',  ( 21.05000000000000071, 6.350000000011161383, -110.3438220896831581 ) ) ;
#185196 = CARTESIAN_POINT ( 'NONE',  ( -20.54999999999999716, 0.000000000000000000, 0.000000000000000000 ) ) ;
#185197 = EDGE_CURVE ( 'NONE', #60065, #114887, #64144, .T. ) ;
#185200 = ORIENTED_EDGE ( 'NONE', *, *, #189705, .F. ) ;
#185199 = ORIENTED_EDGE ( 'NONE', *, *, #250888, .F. ) ;
#185198 = VECTOR ( 'NONE', #162365, 1000.000000000000000 ) ;
#185201 = AXIS2_PLACEMENT_3D ( 'NONE', #215566, #78615, #1642 ) ;
#185202 = VERTEX_POINT ( 'NONE', #177255 ) ;
#185203 = CARTESIAN_POINT ( 'NONE',  ( -22.50875500270926821, 64.25313161950418817, -247.2214436174568277 ) ) ;
#185204 = ORIENTED_EDGE ( 'NONE', *, *, #197697, .T. ) ;
#185205 = ORIENTED_EDGE ( 'NONE', *, *, #123407, .F. ) ;
#185206 = DIRECTION ( 'NONE',  ( -1.000000000000000000, 1.335000415235278971E-16, -2.979993593738921214E-16 ) ) ;
#185208 = ORIENTED_EDGE ( 'NONE', *, *, #92779, .T. ) ;
#185207 = FACE_OUTER_BOUND ( 'NONE', #55165, .T. ) ;
#185209 = DIRECTION ( 'NONE',  ( -1.000000000000000000, -0.000000000000000000, -0.000000000000000000 ) ) ;
#185210 = LINE ( 'NONE', #62701, #153070 ) ;
#185211 = ADVANCED_FACE ( 'NONE', ( #115979 ), #136799, .F. ) ;
#185212 = FACE_OUTER_BOUND ( 'NONE', #112110, .T. ) ;
#185213 = DIRECTION ( 'NONE',  ( 1.000000000000000000, -0.000000000000000000, -0.000000000000000000 ) ) ;
#185214 = ORIENTED_EDGE ( 'NONE', *, *, #162028, .F. ) ;
#185215 = EDGE_CURVE ( 'NONE', #47350, #36387, #218224, .T. ) ;
#185216 = VERTEX_POINT ( 'NONE', #237202 ) ;
#185217 = CARTESIAN_POINT ( 'NONE',  ( -20.64999999999999858, 85.50000000001232081, -160.1291383618718385 ) ) ;
#185218 = DIRECTION ( 'NONE',  ( 0.000000000000000000, 0.000000000000000000, -1.000000000000000000 ) ) ;
#185219 = AXIS2_PLACEMENT_3D ( 'NONE', #19028, #13908, #97240 ) ;
#185221 = EDGE_CURVE ( 'NONE', #207337, #64464, #239768, .T. ) ;
#185220 = ORIENTED_EDGE ( 'NONE', *, *, #190234, .F. ) ;
#185222 = VECTOR ( 'NONE', #91450, 1000.000000000000000 ) ;
#185223 = AXIS2_PLACEMENT_3D ( 'NONE', #132370, #210624, #35857 ) ;
#185224 = AXIS2_PLACEMENT_3D ( 'NONE', #189579, #34376, #10944 ) ;
#185225 = EDGE_CURVE ( 'NONE', #166958, #8900, #117254, .T. ) ;
#185226 = DIRECTION ( 'NONE',  ( -1.000000000000000000, -0.000000000000000000, -0.000000000000000000 ) ) ;
#185227 = ORIENTED_EDGE ( 'NONE', *, *, #242240, .T. ) ;
#185228 = ORIENTED_EDGE ( 'NONE', *, *, #224044, .F. ) ;
#185229 = STYLED_ITEM ( 'NONE', ( #112745 ), #1633 ) ;
#185230 = CARTESIAN_POINT ( 'NONE',  ( -21.00448002041592233, 64.25000000001263345, -196.6747666222132125 ) ) ;
#185231 = EDGE_LOOP ( 'NONE', ( #147684, #22371, #144179, #93661 ) ) ;
#185232 = CARTESIAN_POINT ( 'NONE',  ( -20.94999999999999929, -1.162701749926853712, -175.5999999999999659 ) ) ;
#185233 = VERTEX_POINT ( 'NONE', #218897 ) ;
#185234 = ADVANCED_FACE ( 'NONE', ( #81926 ), #1122, .F. ) ;
#185235 = CARTESIAN_POINT ( 'NONE',  ( 19.90621891164687440, 64.25000000001220712, -145.1946622066474220 ) ) ;
#185237 = DIRECTION ( 'NONE',  ( 1.000000000000000000, 0.000000000000000000, 0.000000000000000000 ) ) ;
#185236 = CARTESIAN_POINT ( 'NONE',  ( -23.25000000000000000, 69.20602499728043711, -247.8456586332460176 ) ) ;
#185238 = DIRECTION ( 'NONE',  ( 0.000000000000000000, -0.8814952561688430555, 0.4721928772777346239 ) ) ;
#185239 = LINE ( 'NONE', #220524, #57742 ) ;
#185240 = DIRECTION ( 'NONE',  ( -0.7071067811865127117, -0.7071067811865821007, 0.000000000000000000 ) ) ;
#185242 = EDGE_CURVE ( 'NONE', #115342, #238407, #68233, .T. ) ;
#185241 = DIRECTION ( 'NONE',  ( -1.000000000000000000, 1.836970198721029934E-16, 1.282749433769087757E-30 ) ) ;
#185243 = AXIS2_PLACEMENT_3D ( 'NONE', #71399, #214731, #16553 ) ;
#185244 = ORIENTED_EDGE ( 'NONE', *, *, #227193, .T. ) ;
#185245 = CIRCLE ( 'NONE', #235292, 0.1000000000000124678 ) ;
#185246 = AXIS2_PLACEMENT_3D ( 'NONE', #48874, #128419, #207976 ) ;
#185248 = ORIENTED_EDGE ( 'NONE', *, *, #186894, .F. ) ;
#185247 = ORIENTED_EDGE ( 'NONE', *, *, #115299, .F. ) ;
#185249 = ORIENTED_EDGE ( 'NONE', *, *, #100541, .F. ) ;
#185250 = VECTOR ( 'NONE', #239896, 1000.000000000000114 ) ;
#185252 = EDGE_CURVE ( 'NONE', #111790, #176023, #130766, .T. ) ;
#185251 = CYLINDRICAL_SURFACE ( 'NONE', #236260, 0.09999999999999939493 ) ;
#185253 = PLANE ( 'NONE',  #78653 ) ;
#185255 = DIRECTION ( 'NONE',  ( 0.000000000000000000, -0.000000000000000000, 1.000000000000000000 ) ) ;
#185254 = DIRECTION ( 'NONE',  ( 1.000000000000000000, 0.000000000000000000, 0.000000000000000000 ) ) ;
#185256 = CARTESIAN_POINT ( 'NONE',  ( -23.25000000000000355, 5.650000000011139001, -79.65000000000004832 ) ) ;
#185257 = EDGE_LOOP ( 'NONE', ( #160387, #106551, #253066 ) ) ;
#185258 = CIRCLE ( 'NONE', #135155, 0.09999999999998898659 ) ;
#185259 = CARTESIAN_POINT ( 'NONE',  ( -18.50000000000000000, 11.65000000001115232, -55.25000000000004974 ) ) ;
#185260 = AXIS2_PLACEMENT_3D ( 'NONE', #132807, #169394, #212346 ) ;
#185262 = VECTOR ( 'NONE', #211734, 1000.000000000000000 ) ;
#185261 = LINE ( 'NONE', #6614, #62786 ) ;
#185263 = CARTESIAN_POINT ( 'NONE',  ( 20.94999999999999574, 79.13126459505528487, -235.8705213229730191 ) ) ;
#185264 = CARTESIAN_POINT ( 'NONE',  ( -23.15000000000000213, 85.50000000001261924, -193.6291383618718385 ) ) ;
#185266 = ORIENTED_EDGE ( 'NONE', *, *, #160343, .F. ) ;
#185265 = TOROIDAL_SURFACE ( 'NONE', #51372, 0.2000000000000000111, 0.1000000000000000056 ) ;
#185267 = DIRECTION ( 'NONE',  ( 0.7071067811865214825, -0.7071067811865735520, 0.000000000000000000 ) ) ;
#185268 = AXIS2_PLACEMENT_3D ( 'NONE', #165257, #106543, #186108 ) ;
#185269 = SPHERICAL_SURFACE ( 'NONE', #213113, 0.1000000000000000056 ) ;
#185270 = ORIENTED_EDGE ( 'NONE', *, *, #98565, .F. ) ;
#185271 = ORIENTED_EDGE ( 'NONE', *, *, #245235, .F. ) ;
#185272 = CARTESIAN_POINT ( 'NONE',  ( -23.15000000000000213, 71.65000000001222702, -148.7731074845243882 ) ) ;
#185273 = VECTOR ( 'NONE', #152034, 1000.000000000000000 ) ;
#185274 = CARTESIAN_POINT ( 'NONE',  ( -21.95218792049438861, 0.8274991115115355456, -230.2449076364474081 ) ) ;
#185275 = DIRECTION ( 'NONE',  ( 1.000000000000000000, -0.000000000000000000, -0.000000000000000000 ) ) ;
#185276 = CARTESIAN_POINT ( 'NONE',  ( -20.54999999999999716, 7.249999999999999112, -12.25000000000000000 ) ) ;
#185277 = FACE_OUTER_BOUND ( 'NONE', #129379, .T. ) ;
#185278 = AXIS2_PLACEMENT_3D ( 'NONE', #98503, #178114, #2002 ) ;
#185279 = CARTESIAN_POINT ( 'NONE',  ( -21.04999999999999716, 6.440770893661913910, -0.01759718700864921007 ) ) ;
#185281 = ORIENTED_EDGE ( 'NONE', *, *, #166756, .F. ) ;
#185280 = VECTOR ( 'NONE', #158827, 1000.000000000000000 ) ;
#185282 = DIRECTION ( 'NONE',  ( 1.000000000000000000, 0.000000000000000000, 0.000000000000000000 ) ) ;
#185283 = DIRECTION ( 'NONE',  ( 0.000000000000000000, 0.000000000000000000, -1.000000000000000000 ) ) ;
#185284 = FACE_OUTER_BOUND ( 'NONE', #107331, .T. ) ;
#185286 = DIRECTION ( 'NONE',  ( 0.000000000000000000, 0.000000000000000000, -1.000000000000000000 ) ) ;
#185285 = DIRECTION ( 'NONE',  ( 0.000000000000000000, -0.1455152366551721865, -0.9893560106964475187 ) ) ;
#185287 = CARTESIAN_POINT ( 'NONE',  ( 20.95512820512820440, 65.37615131630076348, -195.8581939154368285 ) ) ;
#185288 = FACE_OUTER_BOUND ( 'NONE', #222748, .T. ) ;
#185289 = FACE_OUTER_BOUND ( 'NONE', #85333, .T. ) ;
#185290 = DIRECTION ( 'NONE',  ( 0.000000000000000000, 0.000000000000000000, 1.000000000000000000 ) ) ;
#185292 = ORIENTED_EDGE ( 'NONE', *, *, #152011, .F. ) ;
#185291 = DIRECTION ( 'NONE',  ( 0.7071067811865474617, 0.7071067811865474617, 0.000000000000000000 ) ) ;
#185293 = EDGE_CURVE ( 'NONE', #11972, #69129, #60029, .T. ) ;
#185294 = DIRECTION ( 'NONE',  ( 0.000000000000000000, 0.9654727137038715545, 0.2605042016806676242 ) ) ;
#185295 = AXIS2_PLACEMENT_3D ( 'NONE', #42686, #244720, #954 ) ;
#185296 = EDGE_CURVE ( 'NONE', #210038, #70242, #105801, .T. ) ;
#185297 = EDGE_CURVE ( 'NONE', #159714, #40953, #147336, .T. ) ;
#185298 = AXIS2_PLACEMENT_3D ( 'NONE', #216223, #167844, #226479 ) ;
#185299 = CARTESIAN_POINT ( 'NONE',  ( 23.24999999999999645, 7.128833340094563376, -233.7327013124401276 ) ) ;
#185300 = DIRECTION ( 'NONE',  ( 0.000000000000000000, 0.000000000000000000, -1.000000000000000000 ) ) ;
#185301 = ORIENTED_EDGE ( 'NONE', *, *, #249878, .F. ) ;
#185302 = LINE ( 'NONE', #151336, #76433 ) ;
#185303 = CARTESIAN_POINT ( 'NONE',  ( 23.15000000000000213, -9.599999999988842347, -124.1060308773475924 ) ) ;
#185304 = CARTESIAN_POINT ( 'NONE',  ( 20.94999999999999929, 65.27628289530453287, -124.3731074845243825 ) ) ;
#185305 = CIRCLE ( 'NONE', #14637, 3.999999999999999112 ) ;
#185306 = AXIS2_PLACEMENT_3D ( 'NONE', #69205, #167030, #148728 ) ;
#185307 = ORIENTED_EDGE ( 'NONE', *, *, #178627, .F. ) ;
#185308 = DIRECTION ( 'NONE',  ( -1.000000000000000000, -0.000000000000000000, -0.000000000000000000 ) ) ;
#185310 = VERTEX_POINT ( 'NONE', #140653 ) ;
#185309 = DIRECTION ( 'NONE',  ( 0.000000000000000000, 0.9371753822965315228, -0.3488585713686133682 ) ) ;
#185312 = CARTESIAN_POINT ( 'NONE',  ( -18.59999999999999787, 67.49222854868494892, -195.4187676019683693 ) ) ;
#185311 = CARTESIAN_POINT ( 'NONE',  ( 23.14999999999998437, -4.049999999988842525, -100.5000000000000284 ) ) ;
#185313 = ADVANCED_FACE ( 'NONE', ( #62415 ), #41587, .T. ) ;
#185314 = CARTESIAN_POINT ( 'NONE',  ( 18.59999999999999076, 68.87972903831409610, -65.86354444268503983 ) ) ;
#185315 = ORIENTED_EDGE ( 'NONE', *, *, #201347, .F. ) ;
#185316 = DIRECTION ( 'NONE',  ( 0.000000000000000000, 0.000000000000000000, -1.000000000000000000 ) ) ;
#185317 = AXIS2_PLACEMENT_3D ( 'NONE', #14668, #248104, #250666 ) ;
#185318 = DIRECTION ( 'NONE',  ( 1.000000000000000000, 0.000000000000000000, 0.000000000000000000 ) ) ;
#185319 = CYLINDRICAL_SURFACE ( 'NONE', #175352, 0.1000000000000055705 ) ;
#185320 = DIRECTION ( 'NONE',  ( 0.000000000000000000, 0.000000000000000000, -1.000000000000000000 ) ) ;
#185321 = VECTOR ( 'NONE', #140011, 1000.000000000000000 ) ;
#185322 = ORIENTED_EDGE ( 'NONE', *, *, #188023, .T. ) ;
#185323 = DIRECTION ( 'NONE',  ( 0.000000000000000000, 0.000000000000000000, -1.000000000000000000 ) ) ;
#185324 = CARTESIAN_POINT ( 'NONE',  ( 18.59999999999999787, -1.249999999988843369, -108.3004807544151191 ) ) ;
#185325 = CIRCLE ( 'NONE', #135422, 0.1000000000000012546 ) ;
#185326 = CARTESIAN_POINT ( 'NONE',  ( 20.04142135623730070, 51.38014393322265505, -230.1906178717505611 ) ) ;
#185327 = CARTESIAN_POINT ( 'NONE',  ( -18.59999999999999787, -0.6576273345615599730, -242.5323337003318898 ) ) ;
#185328 = ADVANCED_FACE ( 'NONE', ( #178534 ), #195530, .F. ) ;
#185329 = ORIENTED_EDGE ( 'NONE', *, *, #74848, .T. ) ;
#185330 = EDGE_CURVE ( 'NONE', #49587, #61696, #226415, .T. ) ;
#185331 = VECTOR ( 'NONE', #96492, 1000.000000000000000 ) ;
#185332 = VERTEX_POINT ( 'NONE', #96377 ) ;
#185333 = CARTESIAN_POINT ( 'NONE',  ( 22.39999999999999503, 76.10000000001245724, -181.6726782920691505 ) ) ;
#185334 = CARTESIAN_POINT ( 'NONE',  ( 20.94999999999999929, 1.115600667400684642E-11, -134.0000000000000000 ) ) ;
#185335 = DIRECTION ( 'NONE',  ( 0.000000000000000000, -1.000000000000000000, -6.982962677686266711E-15 ) ) ;
#185336 = CARTESIAN_POINT ( 'NONE',  ( 20.95595624212399954, 10.62389120310529833, -141.6296329141270007 ) ) ;
#185337 = DIRECTION ( 'NONE',  ( 0.000000000000000000, 0.000000000000000000, 1.000000000000000000 ) ) ;
#185338 = EDGE_CURVE ( 'NONE', #201436, #46286, #4969, .T. ) ;
#185340 = DIRECTION ( 'NONE',  ( 0.000000000000000000, -0.9651348961777028723, 0.2617529984165503087 ) ) ;
#185339 = CARTESIAN_POINT ( 'NONE',  ( -20.94999999999999929, 77.84915357198842401, -158.4171408647273154 ) ) ;
#185341 = CARTESIAN_POINT ( 'NONE',  ( -23.25000000000000355, 70.35000000001264198, -194.2731074845243882 ) ) ;
#185342 = CARTESIAN_POINT ( 'NONE',  ( 21.05000000000000071, 77.83534155023627932, -91.46795619196130644 ) ) ;
#185343 = CARTESIAN_POINT ( 'NONE',  ( -21.59142135623730852, 7.850000000011158718, -54.65000000000000568 ) ) ;
#185344 = CIRCLE ( 'NONE', #10386, 7.791421356237310469 ) ;
#185346 = ORIENTED_EDGE ( 'NONE', *, *, #131304, .F. ) ;
#185345 = CARTESIAN_POINT ( 'NONE',  ( 18.49999999999998934, 11.65000000001115943, -125.2500000000000284 ) ) ;
#185347 = CIRCLE ( 'NONE', #152045, 3.900000000000000799 ) ;
#185348 = DIRECTION ( 'NONE',  ( -0.000000000000000000, 1.000000000000000000, 6.982962677686266711E-15 ) ) ;
#185349 = FACE_OUTER_BOUND ( 'NONE', #221727, .T. ) ;
#185351 = CARTESIAN_POINT ( 'NONE',  ( 21.30000000000002558, 1.115600667400684642E-11, -33.50000000000000000 ) ) ;
#185350 = CARTESIAN_POINT ( 'NONE',  ( -20.65000000000000568, 7.488999128699433072, -208.8358083214519070 ) ) ;
#185352 = ORIENTED_EDGE ( 'NONE', *, *, #191972, .T. ) ;
#185353 = DIRECTION ( 'NONE',  ( 0.000000000000000000, -0.4930308989874653269, -0.8700118002898649117 ) ) ;
#185354 = CARTESIAN_POINT ( 'NONE',  ( -21.05000000000000071, 77.85102823015347440, -191.8691942151018566 ) ) ;
#185355 = CARTESIAN_POINT ( 'NONE',  ( 20.95512820512820440, 18.90192396791319851, -227.9871466877642661 ) ) ;
#185356 = CARTESIAN_POINT ( 'NONE',  ( 22.50000000000000000, 11.64957080755595520, -133.9000000000000057 ) ) ;
#185357 = DIRECTION ( 'NONE',  ( 1.000000000000000000, 0.000000000000000000, 0.000000000000000000 ) ) ;
#185358 = ORIENTED_EDGE ( 'NONE', *, *, #182472, .F. ) ;
#185359 = ORIENTED_EDGE ( 'NONE', *, *, #101734, .T. ) ;
#185360 = EDGE_CURVE ( 'NONE', #96681, #138858, #126491, .T. ) ;
#185361 = CYLINDRICAL_SURFACE ( 'NONE', #34531, 0.1000000000000028644 ) ;
#185362 = ORIENTED_EDGE ( 'NONE', *, *, #168658, .F. ) ;
#185363 = DIRECTION ( 'NONE',  ( 0.000000000000000000, -0.2128009952263604787, 0.9770955615653313941 ) ) ;
#185364 = AXIS2_PLACEMENT_3D ( 'NONE', #63342, #204138, #243264 ) ;
#185365 = EDGE_LOOP ( 'NONE', ( #115022, #1465, #231609, #207826 ) ) ;
#185366 = CARTESIAN_POINT ( 'NONE',  ( -22.39999999999999858, 12.67709964810648238, -223.3751320524553705 ) ) ;
#185367 = CARTESIAN_POINT ( 'NONE',  ( 18.59999999999999076, 77.85161776048053639, -57.91991776492063337 ) ) ;
#185368 = ADVANCED_FACE ( 'NONE', ( #204471 ), #27169, .T. ) ;
#185369 = AXIS2_PLACEMENT_3D ( 'NONE', #217719, #5077, #101602 ) ;
#185370 = CARTESIAN_POINT ( 'NONE',  ( -20.85000000000000142, 62.88396779178383156, -206.9948552354529454 ) ) ;
#185371 = ORIENTED_EDGE ( 'NONE', *, *, #184736, .T. ) ;
#185372 = ADVANCED_FACE ( 'NONE', ( #225305 ), #244888, .F. ) ;
#185374 = ADVANCED_FACE ( 'NONE', ( #184919 ), #1582, .T. ) ;
#185373 = FACE_OUTER_BOUND ( 'NONE', #174988, .T. ) ;
#185375 = CARTESIAN_POINT ( 'NONE',  ( -21.05000000000000071, 65.48742650828276624, -241.9089677661029043 ) ) ;
#185376 = LINE ( 'NONE', #47120, #219825 ) ;
#185377 = CARTESIAN_POINT ( 'NONE',  ( -20.64999999999999858, 1.115600667400684642E-11, -167.5000000000000284 ) ) ;
#185378 = PLANE ( 'NONE',  #226635 ) ;
#185379 = CARTESIAN_POINT ( 'NONE',  ( -20.54999999999999716, 68.75000000001199396, -115.2731074845243455 ) ) ;
#185380 = CARTESIAN_POINT ( 'NONE',  ( 20.04142135623730070, 64.35000000001254250, -182.1731074845244507 ) ) ;
#185381 = ORIENTED_EDGE ( 'NONE', *, *, #227096, .T. ) ;
#185383 = PLANE ( 'NONE',  #120162 ) ;
#185382 = CARTESIAN_POINT ( 'NONE',  ( -16.84421487269769813, 66.05000000001207638, -123.8536053620794348 ) ) ;
#185384 = ORIENTED_EDGE ( 'NONE', *, *, #35563, .T. ) ;
#185386 = ORIENTED_EDGE ( 'NONE', *, *, #100054, .F. ) ;
#185385 = FACE_OUTER_BOUND ( 'NONE', #234101, .T. ) ;
#185387 = EDGE_CURVE ( 'NONE', #12386, #219655, #213991, .T. ) ;
#185388 = VECTOR ( 'NONE', #76435, 1000.000000000000000 ) ;
#185389 = ORIENTED_EDGE ( 'NONE', *, *, #233955, .T. ) ;
#185390 = AXIS2_PLACEMENT_3D ( 'NONE', #85860, #123745, #27242 ) ;
#185391 = DIRECTION ( 'NONE',  ( -0.7071067811865685560, -0.2890913453344204909, 0.6453109281987288171 ) ) ;
#185392 = ADVANCED_FACE ( 'NONE', ( #205760 ), #25863, .F. ) ;
#185393 = DIRECTION ( 'NONE',  ( 0.000000000000000000, -0.000000000000000000, 1.000000000000000000 ) ) ;
#185394 = CARTESIAN_POINT ( 'NONE',  ( 18.49999999999999289, 65.71984138295462685, -78.29853541332350630 ) ) ;
#185395 = DIRECTION ( 'NONE',  ( 0.000000000000000000, 1.000000000000000000, 0.000000000000000000 ) ) ;
#185396 = ORIENTED_EDGE ( 'NONE', *, *, #55748, .T. ) ;
#185397 = DIRECTION ( 'NONE',  ( 0.000000000000000000, 0.000000000000000000, -1.000000000000000000 ) ) ;
#185399 = EDGE_CURVE ( 'NONE', #9216, #31326, #101510, .T. ) ;
#185398 = SPHERICAL_SURFACE ( 'NONE', #156237, 0.1000000000000000056 ) ;
#185400 = ORIENTED_EDGE ( 'NONE', *, *, #196005, .F. ) ;
#185401 = CARTESIAN_POINT ( 'NONE',  ( -16.93935632781549572, 9.984730499736244269, -154.8896607487103267 ) ) ;
#185402 = EDGE_CURVE ( 'NONE', #153506, #214929, #134834, .T. ) ;
#185404 = CIRCLE ( 'NONE', #135494, 0.2000000000000057288 ) ;
#185403 = DIRECTION ( 'NONE',  ( -0.000000000000000000, 1.000000000000000000, 6.982962677686267499E-15 ) ) ;
#185405 = VERTEX_POINT ( 'NONE', #183650 ) ;
#185407 = CARTESIAN_POINT ( 'NONE',  ( -20.64999999999999858, 73.50000000001180922, -82.74772940728642823 ) ) ;
#185406 = VECTOR ( 'NONE', #118726, 1000.000000000000000 ) ;
#185408 = ADVANCED_FACE ( 'NONE', ( #102785 ), #143212, .T. ) ;
#185409 = EDGE_CURVE ( 'NONE', #34727, #122206, #144486, .T. ) ;
#185410 = AXIS2_PLACEMENT_3D ( 'NONE', #52818, #71136, #50246 ) ;
#185411 = CIRCLE ( 'NONE', #106267, 0.1000000000000124678 ) ;
#185412 = EDGE_LOOP ( 'NONE', ( #233658, #142061, #206221 ) ) ;
#185413 = ORIENTED_EDGE ( 'NONE', *, *, #220919, .T. ) ;
#185414 = CARTESIAN_POINT ( 'NONE',  ( 18.39999999999997371, 13.44928205424795564, -207.5377222505711075 ) ) ;
#185415 =( GEOMETRIC_REPRESENTATION_CONTEXT ( 3 ) GLOBAL_UNCERTAINTY_ASSIGNED_CONTEXT ( ( #209444 ) ) GLOBAL_UNIT_ASSIGNED_CONTEXT ( ( #178879, #225318, #139689 ) ) REPRESENTATION_CONTEXT ( 'NONE', 'WORKASPACE' ) );
#185416 = ADVANCED_FACE ( 'NONE', ( #165364 ), #45409, .F. ) ;
#185417 = CARTESIAN_POINT ( 'NONE',  ( 20.96428641294179585, 64.25000000001175238, -76.34821430658304564 ) ) ;
#185418 = DIRECTION ( 'NONE',  ( 0.000000000000000000, 0.000000000000000000, 1.000000000000000000 ) ) ;
#185419 = CARTESIAN_POINT ( 'NONE',  ( -21.07094088545304089, 6.154362662572049558, -199.5584335273501324 ) ) ;
#185420 = EDGE_CURVE ( 'NONE', #224923, #127762, #89063, .T. ) ;
#185421 = EDGE_CURVE ( 'NONE', #24871, #138064, #51616, .T. ) ;
#185422 = ADVANCED_FACE ( 'NONE', ( #226597 ), #143233, .T. ) ;
#185423 = CARTESIAN_POINT ( 'NONE',  ( 18.49999999999999289, 6.450000000011156587, -122.2500000000000284 ) ) ;
#185424 = CARTESIAN_POINT ( 'NONE',  ( 20.89192007715127986, 10.32898536001801304, -72.58266832227644727 ) ) ;
#185425 = CIRCLE ( 'NONE', #135517, 12.87499999999999822 ) ;
#185426 = ORIENTED_EDGE ( 'NONE', *, *, #240704, .F. ) ;
#185428 = CARTESIAN_POINT ( 'NONE',  ( -22.39999999999999858, 11.50215294792677057, -198.5972978622482970 ) ) ;
#185427 = CARTESIAN_POINT ( 'NONE',  ( -21.04999999999999716, 69.70076908992010090, -170.1215449845247463 ) ) ;
#185429 = TOROIDAL_SURFACE ( 'NONE', #210383, 12.97499999999999609, 0.1000000000000000056 ) ;
#185430 = AXIS2_PLACEMENT_3D ( 'NONE', #115454, #170353, #153355 ) ;
#185431 = LINE ( 'NONE', #245414, #230482 ) ;
#185432 = DIRECTION ( 'NONE',  ( -1.000000000000000000, 0.000000000000000000, -0.000000000000000000 ) ) ;
#185433 = CARTESIAN_POINT ( 'NONE',  ( 18.79999999999999716, -1.885425182446133885, -11.49641995933507843 ) ) ;
#185435 = EDGE_LOOP ( 'NONE', ( #238045, #136433, #10291 ) ) ;
#185434 = DIRECTION ( 'NONE',  ( -1.836970198721029934E-16, -0.9651348961777157509, 0.2617529984165031243 ) ) ;
#185437 = EDGE_LOOP ( 'NONE', ( #236414, #107435, #175029, #209822 ) ) ;
#185436 = DIRECTION ( 'NONE',  ( 1.000000000000000000, 0.000000000000000000, 0.000000000000000000 ) ) ;
#185438 = EDGE_CURVE ( 'NONE', #203994, #230665, #155747, .T. ) ;
#185439 = CARTESIAN_POINT ( 'NONE',  ( 18.46921299892754931, 46.92271302580608960, -255.3731210386297050 ) ) ;
#185440 = FACE_OUTER_BOUND ( 'NONE', #60997, .T. ) ;
#185441 = EDGE_CURVE ( 'NONE', #209575, #234902, #43300, .T. ) ;
#185442 = TOROIDAL_SURFACE ( 'NONE', #118811, 0.2000000000000000111, 0.1000000000000000056 ) ;
#185443 = DIRECTION ( 'NONE',  ( 0.000000000000000000, 0.8814952561688430555, -0.4721928772777346239 ) ) ;
#185444 = VECTOR ( 'NONE', #3533, 1000.000000000000000 ) ;
#185445 = VECTOR ( 'NONE', #141256, 1000.000000000000000 ) ;
#185447 = EDGE_LOOP ( 'NONE', ( #119022, #116894, #208628, #44367 ) ) ;
#185446 = CARTESIAN_POINT ( 'NONE',  ( 21.04999999999999716, 67.12872031401664685, -157.8731074845244109 ) ) ;
#185448 = CARTESIAN_POINT ( 'NONE',  ( 18.49999999999999645, -1.135018845899022466, -175.2169768834323520 ) ) ;
#185449 = AXIS2_PLACEMENT_3D ( 'NONE', #59085, #133526, #115248 ) ;
#185450 = CARTESIAN_POINT ( 'NONE',  ( -20.94999999999999929, 68.22930980752001062, -227.7331931781284879 ) ) ;
#185451 = ORIENTED_EDGE ( 'NONE', *, *, #74646, .T. ) ;
#185452 = CARTESIAN_POINT ( 'NONE',  ( 20.94999999999999929, 1.148907358139439339E-11, -201.0000000000015064 ) ) ;
#185453 = EDGE_LOOP ( 'NONE', ( #160866, #161998, #5836 ) ) ;
#185454 = AXIS2_PLACEMENT_3D ( 'NONE', #151694, #31747, #173845 ) ;
#185455 = CARTESIAN_POINT ( 'NONE',  ( -20.54999999999999716, 4.350000000011156054, -121.7500000000000426 ) ) ;
#185456 = DIRECTION ( 'NONE',  ( 1.000000000000000000, 8.674042436075324885E-17, 1.619280515896126624E-16 ) ) ;
#185457 = CIRCLE ( 'NONE', #222855, 0.6000000000000015321 ) ;
#185459 = ORIENTED_EDGE ( 'NONE', *, *, #3402, .F. ) ;
#185458 = VECTOR ( 'NONE', #193767, 1000.000000000000000 ) ;
#185460 = DIRECTION ( 'NONE',  ( 0.000000000000000000, -0.9876197685951263461, 0.1568667991644794590 ) ) ;
#185461 = CARTESIAN_POINT ( 'NONE',  ( 18.59999999999999076, 6.550000000011156231, -121.6500000000000341 ) ) ;
#185462 = EDGE_CURVE ( 'NONE', #148383, #255010, #118315, .T. ) ;
#185463 = VERTEX_POINT ( 'NONE', #14000 ) ;
#185465 = EDGE_CURVE ( 'NONE', #233652, #209763, #30835, .T. ) ;
#185464 = CARTESIAN_POINT ( 'NONE',  ( -18.39999999999999858, -9.600000000000003197, -40.20018939122204671 ) ) ;
#185466 = ORIENTED_EDGE ( 'NONE', *, *, #127761, .F. ) ;
#185467 = ORIENTED_EDGE ( 'NONE', *, *, #162, .T. ) ;
#185468 = CARTESIAN_POINT ( 'NONE',  ( -21.05000000000000071, 61.00523048461932518, -234.0629566809490143 ) ) ;
#185469 = ORIENTED_EDGE ( 'NONE', *, *, #25218, .T. ) ;
#185470 = CARTESIAN_POINT ( 'NONE',  ( -18.59999999999999787, 0.5876173420563349792, -209.1618981382189588 ) ) ;
#185471 = VERTEX_POINT ( 'NONE', #29735 ) ;
#185473 = ORIENTED_EDGE ( 'NONE', *, *, #134283, .T. ) ;
#185472 = CARTESIAN_POINT ( 'NONE',  ( -21.45000000000000284, 7.708578643773852157, -88.25000000000005684 ) ) ;
#185474 = CARTESIAN_POINT ( 'NONE',  ( 21.05000000000000071, 76.00000000001126921, -203.5231074845248997 ) ) ;
#185475 = VERTEX_POINT ( 'NONE', #174397 ) ;
#185476 = AXIS2_PLACEMENT_3D ( 'NONE', #171050, #71910, #111022 ) ;
#185477 = DIRECTION ( 'NONE',  ( 1.000000000000000000, -2.952720810173289112E-16, -2.061873921506763405E-30 ) ) ;
#185478 = VERTEX_POINT ( 'NONE', #170552 ) ;
#185480 = B_SPLINE_CURVE_WITH_KNOTS ( 'NONE', 3,
 ( #97052, #210961, #51855, #152291, #18840, #196198 ),
 .UNSPECIFIED., .F., .F.,
 ( 4, 2, 4 ),
 ( 0.000000000000000000, 0.0001569047307838624338, 0.0003138094615677248676 ),
 .UNSPECIFIED. ) ;
#185479 = AXIS2_PLACEMENT_3D ( 'NONE', #224889, #106221, #181936 ) ;
#185482 = VERTEX_POINT ( 'NONE', #93516 ) ;
#185481 = ORIENTED_EDGE ( 'NONE', *, *, #195131, .F. ) ;
#185483 = CARTESIAN_POINT ( 'NONE',  ( -20.64999999999999858, 6.724511449164477739, -231.8762197454659884 ) ) ;
#185484 = EDGE_CURVE ( 'NONE', #134466, #25818, #209897, .T. ) ;
#185485 = AXIS2_PLACEMENT_3D ( 'NONE', #153746, #217488, #98807 ) ;
#185486 = FACE_OUTER_BOUND ( 'NONE', #211963, .T. ) ;
#185487 = ORIENTED_EDGE ( 'NONE', *, *, #1875, .F. ) ;
#185488 = VECTOR ( 'NONE', #207308, 1000.000000000000000 ) ;
#185489 = CIRCLE ( 'NONE', #206342, 0.09999999999999895084 ) ;
#185490 = ORIENTED_EDGE ( 'NONE', *, *, #208587, .T. ) ;
#185491 = CARTESIAN_POINT ( 'NONE',  ( -21.13435531349799135, 69.50627893642020183, -203.5231074845243882 ) ) ;
#185492 = CARTESIAN_POINT ( 'NONE',  ( 18.59999999999999076, 11.65000000001115943, -58.25000000000000000 ) ) ;
#185494 = ORIENTED_EDGE ( 'NONE', *, *, #40277, .T. ) ;
#185493 = CARTESIAN_POINT ( 'NONE',  ( -18.59999999999999787, -1.736705739456431807, -212.5174225876236846 ) ) ;
#185495 = DIRECTION ( 'NONE',  ( -1.000000000000000000, 0.000000000000000000, 0.000000000000000000 ) ) ;
#185496 = ORIENTED_EDGE ( 'NONE', *, *, #6762, .T. ) ;
#185498 = CIRCLE ( 'NONE', #31413, 0.09999999999999939493 ) ;
#185497 = CARTESIAN_POINT ( 'NONE',  ( 21.87500000000000355, 66.25000000001223555, -148.8731074845244393 ) ) ;
#185499 = DIRECTION ( 'NONE',  ( 1.000000000000000000, 0.000000000000000000, 0.000000000000000000 ) ) ;
#185500 = VECTOR ( 'NONE', #145805, 1000.000000000000000 ) ;
#185501 = ORIENTED_EDGE ( 'NONE', *, *, #137624, .F. ) ;
#185502 = DIRECTION ( 'NONE',  ( 0.000000000000000000, 0.000000000000000000, 1.000000000000000000 ) ) ;
#185503 = CARTESIAN_POINT ( 'NONE',  ( 22.50000000000000000, 0.1000000000111554016, -126.2092204016266379 ) ) ;
#185504 = CIRCLE ( 'NONE', #227187, 0.1000000000000054040 ) ;
#185505 = ORIENTED_EDGE ( 'NONE', *, *, #69969, .F. ) ;
#185506 = CARTESIAN_POINT ( 'NONE',  ( 19.75857864376269291, 54.53338637621133955, -228.6684279704127789 ) ) ;
#185507 = ORIENTED_EDGE ( 'NONE', *, *, #221868, .F. ) ;
#185509 = ORIENTED_EDGE ( 'NONE', *, *, #160975, .T. ) ;
#185508 = EDGE_LOOP ( 'NONE', ( #106066, #143496, #8852, #108532 ) ) ;
#185510 = EDGE_LOOP ( 'NONE', ( #235182, #181971, #189248, #194178, #65449 ) ) ;
#185511 = CARTESIAN_POINT ( 'NONE',  ( -21.05000000000000071, -0.09999999998884338825, -127.4593430482987912 ) ) ;
#185512 = ORIENTED_EDGE ( 'NONE', *, *, #127365, .F. ) ;
#185513 = B_SPLINE_CURVE_WITH_KNOTS ( 'NONE', 3,
 ( #69514, #206431, #26528, #244255, #47336, #189448, #8245, #246832 ),
 .UNSPECIFIED., .F., .F.,
 ( 4, 2, 2, 4 ),
 ( 0.000000000000000000, 0.0002114466876442005951, 0.0003171700314663121684, 0.0004228933752884237417 ),
 .UNSPECIFIED. ) ;
#185514 = CARTESIAN_POINT ( 'NONE',  ( -20.64999999999999858, 75.50266930301991408, -205.3568637872625686 ) ) ;
#185515 = AXIS2_PLACEMENT_3D ( 'NONE', #74248, #192883, #175905 ) ;
#185516 = ORIENTED_EDGE ( 'NONE', *, *, #219395, .T. ) ;
#185517 = LINE ( 'NONE', #66853, #27447 ) ;
#185518 = DIRECTION ( 'NONE',  ( -1.000000000000000000, 0.000000000000000000, 0.000000000000000000 ) ) ;
#185519 = EDGE_CURVE ( 'NONE', #100496, #15616, #54394, .T. ) ;
#185520 = B_SPLINE_CURVE_WITH_KNOTS ( 'NONE', 3,
 ( #68345, #203984, #25378, #5763, #206562, #27960 ),
 .UNSPECIFIED., .F., .F.,
 ( 4, 2, 4 ),
 ( 0.000000000000000000, 0.0001895189928937332253, 0.0003790379857874664506 ),
 .UNSPECIFIED. ) ;
#185521 = ORIENTED_EDGE ( 'NONE', *, *, #225077, .F. ) ;
#185522 = EDGE_CURVE ( 'NONE', #57917, #234078, #139111, .T. ) ;
#185523 = ORIENTED_EDGE ( 'NONE', *, *, #106508, .F. ) ;
#185524 = EDGE_LOOP ( 'NONE', ( #102852, #229384, #33237, #156125, #71737 ) ) ;
#185525 = CIRCLE ( 'NONE', #210472, 0.09999999999999939493 ) ;
#185526 = VECTOR ( 'NONE', #219685, 1000.000000000000000 ) ;
#185527 = EDGE_CURVE ( 'NONE', #11913, #186847, #133926, .T. ) ;
#185528 = DIRECTION ( 'NONE',  ( -3.469446951953612296E-14, -0.9908441862701596881, -0.1350103645451904977 ) ) ;
#185529 = EDGE_LOOP ( 'NONE', ( #191103, #165649, #60000, #59900 ) ) ;
#185530 = FACE_OUTER_BOUND ( 'NONE', #207666, .T. ) ;
#185533 = EDGE_CURVE ( 'NONE', #223778, #217337, #126859, .T. ) ;
#185532 = ORIENTED_EDGE ( 'NONE', *, *, #64920, .F. ) ;
#185531 = CARTESIAN_POINT ( 'NONE',  ( 23.14999999999999503, 64.35000000001178933, -81.77310748452438816 ) ) ;
#185534 = DIRECTION ( 'NONE',  ( 0.000000000000000000, 0.000000000000000000, -1.000000000000000000 ) ) ;
#185535 = CARTESIAN_POINT ( 'NONE',  ( -20.94999999999999574, 11.63687328911503371, -127.1782407866755307 ) ) ;
#185536 = CARTESIAN_POINT ( 'NONE',  ( 19.90000000000000568, 1.350000000000000089, 16.60000000000000142 ) ) ;
#185537 = CARTESIAN_POINT ( 'NONE',  ( 21.05000000000000426, -0.01681986837451403261, -127.6925747804346116 ) ) ;
#185538 = LINE ( 'NONE', #66873, #197954 ) ;
#185540 = CARTESIAN_POINT ( 'NONE',  ( 21.00000000000000000, 66.25000000001158185, -57.17310748452438673 ) ) ;
#185539 = DIRECTION ( 'NONE',  ( 0.000000000000000000, -1.000000000000000000, -6.982962677686266711E-15 ) ) ;
#185541 = DIRECTION ( 'NONE',  ( 0.000000000000000000, -1.000000000000000000, 0.000000000000000000 ) ) ;
#185542 = CARTESIAN_POINT ( 'NONE',  ( 19.99016485861948667, 4.635725510443823971, 21.97684634237453594 ) ) ;
#185543 = EDGE_CURVE ( 'NONE', #90831, #117062, #142416, .T. ) ;
#185544 = DIRECTION ( 'NONE',  ( 1.000000000000000000, 0.000000000000000000, 0.000000000000000000 ) ) ;
#185545 = LINE ( 'NONE', #130372, #113781 ) ;
#185546 = ORIENTED_EDGE ( 'NONE', *, *, #230080, .T. ) ;
#185547 = VECTOR ( 'NONE', #170345, 1000.000000000000000 ) ;
#185549 = ORIENTED_EDGE ( 'NONE', *, *, #164755, .F. ) ;
#185548 = DIRECTION ( 'NONE',  ( -1.000000000000000000, -0.000000000000000000, -0.000000000000000000 ) ) ;
#185550 = VERTEX_POINT ( 'NONE', #128812 ) ;
#185552 = EDGE_CURVE ( 'NONE', #61933, #230047, #68844, .T. ) ;
#185551 = CARTESIAN_POINT ( 'NONE',  ( -20.85000000000000142, -11.74999999998884448, -198.0999999999999659 ) ) ;
#185553 = DIRECTION ( 'NONE',  ( 0.000000000000000000, 1.000000000000000000, 0.000000000000000000 ) ) ;
#185554 = DIRECTION ( 'NONE',  ( -0.000000000000000000, 0.9770955615653313941, 0.2128009952263603954 ) ) ;
#185555 = ORIENTED_EDGE ( 'NONE', *, *, #100550, .F. ) ;
#185556 =( LENGTH_UNIT ( ) NAMED_UNIT ( * ) SI_UNIT ( .MILLI., .METRE. ) );
#185557 = LINE ( 'NONE', #6914, #108403 ) ;
#185558 = CARTESIAN_POINT ( 'NONE',  ( -23.25000000000000000, -11.74999999998884448, -55.25000000000004974 ) ) ;
#185559 = ORIENTED_EDGE ( 'NONE', *, *, #235601, .F. ) ;
#185561 = DIRECTION ( 'NONE',  ( 1.000000000000000000, 0.000000000000000000, -0.000000000000000000 ) ) ;
#185560 = MECHANICAL_DESIGN_GEOMETRIC_PRESENTATION_REPRESENTATION (  '', ( #202141 ), #60459 ) ;
#185562 = CIRCLE ( 'NONE', #102137, 0.2000000000000057288 ) ;
#185563 = LINE ( 'NONE', #199393, #254734 ) ;
#185564 = CARTESIAN_POINT ( 'NONE',  ( 20.95512820512820085, 65.37615131629971188, -61.85819391543678591 ) ) ;
#185565 = CARTESIAN_POINT ( 'NONE',  ( 21.05000000000000071, 40.68212387350988735, -238.0221676322813096 ) ) ;
#185567 = ORIENTED_EDGE ( 'NONE', *, *, #217231, .T. ) ;
#185566 = DIRECTION ( 'NONE',  ( -1.000000000000000000, -2.952720810173289112E-16, 0.000000000000000000 ) ) ;
#185568 = CARTESIAN_POINT ( 'NONE',  ( 22.60000000000000142, 76.00000000001195133, -103.0231074845243171 ) ) ;
#185569 = CARTESIAN_POINT ( 'NONE',  ( -18.41809261886928084, 85.68240331476862082, -96.36626393443329164 ) ) ;
#185570 = CARTESIAN_POINT ( 'NONE',  ( -22.50000000000000000, 11.64957080755595520, -167.3999999999999773 ) ) ;
#185571 = CARTESIAN_POINT ( 'NONE',  ( 18.41789779300679086, 85.50000000001189449, -95.99103781816336323 ) ) ;
#185572 = ORIENTED_EDGE ( 'NONE', *, *, #103790, .T. ) ;
#185573 = CARTESIAN_POINT ( 'NONE',  ( 23.14999999999999858, 5.950000000000003730, -23.19429769496518645 ) ) ;
#185574 = DIRECTION ( 'NONE',  ( 0.000000000000000000, -0.9770955615653315052, -0.2128009952263607008 ) ) ;
#185576 = DIRECTION ( 'NONE',  ( 0.000000000000000000, 0.000000000000000000, 1.000000000000000000 ) ) ;
#185575 = FACE_OUTER_BOUND ( 'NONE', #189074, .T. ) ;
#185577 = DIRECTION ( 'NONE',  ( 0.000000000000000000, 0.000000000000000000, -1.000000000000000000 ) ) ;
#185578 = CARTESIAN_POINT ( 'NONE',  ( -16.89155683852559875, 9.950000000011137047, -53.72262815045999673 ) ) ;
#185579 = AXIS2_PLACEMENT_3D ( 'NONE', #103059, #144753, #245167 ) ;
#185580 =( LENGTH_UNIT ( ) NAMED_UNIT ( * ) SI_UNIT ( .MILLI., .METRE. ) );
#185581 = FACE_OUTER_BOUND ( 'NONE', #25559, .T. ) ;
#185582 = CARTESIAN_POINT ( 'NONE',  ( -20.64999999999999858, 76.00000000001172396, -71.52310748452431710 ) ) ;
#185583 = AXIS2_PLACEMENT_3D ( 'NONE', #152101, #72557, #93375 ) ;
#185584 = CARTESIAN_POINT ( 'NONE',  ( -16.77732147262506146, 9.945966932629787038, -87.83649124327591551 ) ) ;
#185585 = VECTOR ( 'NONE', #220880, 1000.000000000000000 ) ;
#185586 = ORIENTED_EDGE ( 'NONE', *, *, #191024, .F. ) ;
#185587 = CIRCLE ( 'NONE', #235453, 3.999999999999996447 ) ;
#185588 = ADVANCED_FACE ( 'NONE', ( #113091 ), #148367, .F. ) ;
#185589 = DIRECTION ( 'NONE',  ( -0.7071067811865127117, -0.7071067811865821007, 0.000000000000000000 ) ) ;
#185590 = ORIENTED_EDGE ( 'NONE', *, *, #32495, .F. ) ;
#185592 = ORIENTED_EDGE ( 'NONE', *, *, #173156, .F. ) ;
#185591 = STYLED_ITEM ( 'NONE', ( #62115 ), #51500 ) ;
#185593 = DIRECTION ( 'NONE',  ( 0.000000000000000000, 0.000000000000000000, -1.000000000000000000 ) ) ;
#185594 = CARTESIAN_POINT ( 'NONE',  ( 20.94999999999999574, 43.10494791715829166, -239.6505508802563327 ) ) ;
#185595 = ORIENTED_EDGE ( 'NONE', *, *, #33114, .T. ) ;
#185596 = EDGE_CURVE ( 'NONE', #16273, #170246, #71416, .T. ) ;
#185597 = EDGE_LOOP ( 'NONE', ( #179732, #197949, #141287, #201181 ) ) ;
#185598 = EDGE_CURVE ( 'NONE', #95600, #246752, #227900, .T. ) ;
#185599 = ADVANCED_FACE ( 'NONE', ( #188767 ), #70141, .F. ) ;
#185600 = ORIENTED_EDGE ( 'NONE', *, *, #220458, .T. ) ;
#185601 = CARTESIAN_POINT ( 'NONE',  ( 20.94999999999999574, 87.41227409416181615, -133.5231074845242176 ) ) ;
#185602 = AXIS2_PLACEMENT_3D ( 'NONE', #217207, #76423, #256281 ) ;
#185603 = ORIENTED_EDGE ( 'NONE', *, *, #230053, .F. ) ;
#185604 = STYLED_ITEM ( 'NONE', ( #99865 ), #132346 ) ;
#185605 = DIRECTION ( 'NONE',  ( 1.000000000000000000, 0.000000000000000000, 0.000000000000000000 ) ) ;
#185606 = DIRECTION ( 'NONE',  ( 1.301042606982683734E-14, 0.8660254037844367092, -0.5000000000000037748 ) ) ;
#185607 = DIRECTION ( 'NONE',  ( 0.000000000000000000, -0.9999631594459056361, -0.008583690987124413183 ) ) ;
#185608 = VECTOR ( 'NONE', #19303, 1000.000000000000000 ) ;
#185609 = DIRECTION ( 'NONE',  ( 0.000000000000000000, 0.9126074666063660468, 0.4088369013363524762 ) ) ;
#185610 = DIRECTION ( 'NONE',  ( 0.000000000000000000, -1.000000000000000000, -6.352154140967427193E-15 ) ) ;
#185611 = CARTESIAN_POINT ( 'NONE',  ( -23.25000000000000000, 43.08613539620618837, -254.3146655184800409 ) ) ;
#185612 = CARTESIAN_POINT ( 'NONE',  ( -21.04999999999994387, 57.01194402951015405, -45.05752083424646059 ) ) ;
#185615 = ORIENTED_EDGE ( 'NONE', *, *, #55122, .T. ) ;
#185614 = CARTESIAN_POINT ( 'NONE',  ( 21.05000005000965757, 44.14570381864804460, -236.4763722595682509 ) ) ;
#185613 = AXIS2_PLACEMENT_3D ( 'NONE', #125424, #147545, #227068 ) ;
#185617 = CARTESIAN_POINT ( 'NONE',  ( 20.95512828230152280, 8.876151312336450161, -79.20243026550316756 ) ) ;
#185616 = CARTESIAN_POINT ( 'NONE',  ( 21.05000000000000071, 6.350000000011161383, -76.84382208968317229 ) ) ;
#185618 = EDGE_CURVE ( 'NONE', #231873, #177651, #39407, .T. ) ;
#185619 = CARTESIAN_POINT ( 'NONE',  ( -21.07016717457011268, 76.00000000001170974, -75.84404832262522689 ) ) ;
#185620 = ORIENTED_EDGE ( 'NONE', *, *, #39212, .F. ) ;
#185621 = CARTESIAN_POINT ( 'NONE',  ( 20.73486653747088582, 7.250000000011182166, -176.7499999999999716 ) ) ;
#185622 = AXIS2_PLACEMENT_3D ( 'NONE', #242485, #80832, #160424 ) ;
#185623 = CARTESIAN_POINT ( 'NONE',  ( -21.05000000000000071, -0.09999999998884338825, -88.85042919245522341 ) ) ;
#185625 = EDGE_CURVE ( 'NONE', #34477, #102301, #6041, .T. ) ;
#185624 = DIRECTION ( 'NONE',  ( 2.827886303505249259E-16, -0.8660254037844411501, -0.4999999999999956701 ) ) ;
#185627 = VERTEX_POINT ( 'NONE', #150935 ) ;
#185626 = CIRCLE ( 'NONE', #64801, 0.1000000000000028644 ) ;
#185628 = LINE ( 'NONE', #205167, #158244 ) ;
#185629 = FACE_OUTER_BOUND ( 'NONE', #131167, .T. ) ;
#185630 = ORIENTED_EDGE ( 'NONE', *, *, #26813, .F. ) ;
#185631 = AXIS2_PLACEMENT_3D ( 'NONE', #151534, #188069, #210210 ) ;
#185632 = DIRECTION ( 'NONE',  ( 1.000000000000000000, 0.000000000000000000, -0.000000000000000000 ) ) ;
#185633 = VECTOR ( 'NONE', #43271, 1000.000000000000000 ) ;
#185634 = ADVANCED_FACE ( 'NONE', ( #90952 ), #131362, .T. ) ;
#185635 = DIRECTION ( 'NONE',  ( 1.000000000000000000, 0.000000000000000000, 0.000000000000000000 ) ) ;
#185636 = EDGE_CURVE ( 'NONE', #226146, #162071, #218582, .T. ) ;
#185637 = VERTEX_POINT ( 'NONE', #159939 ) ;
#185638 = EDGE_CURVE ( 'NONE', #83997, #72480, #59494, .T. ) ;
#185639 = AXIS2_PLACEMENT_3D ( 'NONE', #27294, #185044, #205886 ) ;
#185640 = CIRCLE ( 'NONE', #35811, 0.5000000000000004441 ) ;
#185641 = ORIENTED_EDGE ( 'NONE', *, *, #233033, .F. ) ;
#185642 = DIRECTION ( 'NONE',  ( 0.000000000000000000, 0.000000000000000000, -1.000000000000000000 ) ) ;
#185643 = DIRECTION ( 'NONE',  ( 2.952720810173289605E-16, -0.9770955615653313941, -0.2128009952263610893 ) ) ;
#185645 = B_SPLINE_CURVE_WITH_KNOTS ( 'NONE', 3,
 ( #190155, #251393, #51890, #11521, #111907, #87172, #208446, #227988, #109301, #229279 ),
 .UNSPECIFIED., .F., .F.,
 ( 4, 3, 3, 4 ),
 ( 0.000000000000000000, 4.874959354401955399E-05, 9.785140065120999852E-05, 0.0001360444631936036581 ),
 .UNSPECIFIED. ) ;
#185644 = DIRECTION ( 'NONE',  ( 0.000000000000000000, 0.2617529984165031243, 0.9651348961777157509 ) ) ;
#185646 = DIRECTION ( 'NONE',  ( 1.000000000000000000, 0.000000000000000000, 0.000000000000000000 ) ) ;
#185647 = CARTESIAN_POINT ( 'NONE',  ( 21.09813707148777340, 6.385062105747654648, -167.4686485004704650 ) ) ;
#185648 = DIRECTION ( 'NONE',  ( 0.000000000000000000, 0.000000000000000000, -1.000000000000000000 ) ) ;
#185649 = ORIENTED_EDGE ( 'NONE', *, *, #189016, .T. ) ;
#185650 = LINE ( 'NONE', #69571, #157724 ) ;
#185652 = EDGE_LOOP ( 'NONE', ( #200634, #113786, #140574, #95691 ) ) ;
#185651 = CYLINDRICAL_SURFACE ( 'NONE', #79595, 0.5000000000000014433 ) ;
#185653 = CARTESIAN_POINT ( 'NONE',  ( -21.05000000000000071, 6.344723404101344499, -33.48528214347599885 ) ) ;
#185654 = CARTESIAN_POINT ( 'NONE',  ( 19.75857864376268935, 54.48300931968434213, -228.8005724072070564 ) ) ;
#185655 = DIRECTION ( 'NONE',  ( 1.000000000000000000, 0.000000000000000000, 0.000000000000000000 ) ) ;
#185656 = B_SPLINE_CURVE_WITH_KNOTS ( 'NONE', 3,
 ( #10021, #28340, #170433, #205636, #68716, #50403, #49139, #187390, #51682, #227779, #248630, #208241, #129946, #29616, #110396, #66144, #70020, #30903, #165246 ),
 .UNSPECIFIED., .F., .F.,
 ( 4, 3, 3, 3, 3, 3, 4 ),
 ( -2.000416914664862515E-06, 0.000000000000000000, 4.714008503747113684E-05, 9.979203887778935727E-05, 0.0001372215519229636642, 0.0001635031576221091139, 0.0001900083748504286928 ),
 .UNSPECIFIED. ) ;
#185657 = FACE_OUTER_BOUND ( 'NONE', #36593, .T. ) ;
#185659 = EDGE_LOOP ( 'NONE', ( #36787, #66547, #177133, #90784 ) ) ;
#185658 = DIRECTION ( 'NONE',  ( 0.000000000000000000, 0.000000000000000000, -1.000000000000000000 ) ) ;
#185660 = FACE_OUTER_BOUND ( 'NONE', #201075, .T. ) ;
#185661 = CARTESIAN_POINT ( 'NONE',  ( 21.06490991615909181, 10.72489134759826790, -179.7037113535330946 ) ) ;
#185662 = CARTESIAN_POINT ( 'NONE',  ( 21.14999999999999503, 26.06832281015329755, -254.4051978787608732 ) ) ;
#185663 = DIRECTION ( 'NONE',  ( 0.000000000000000000, -1.000000000000000000, -7.272083257015735086E-15 ) ) ;
#185664 = VERTEX_POINT ( 'NONE', #17823 ) ;
#185665 = CARTESIAN_POINT ( 'NONE',  ( 18.59999999999999787, -7.567701079425742883, -210.0537230116848377 ) ) ;
#185666 = CIRCLE ( 'NONE', #19053, 0.1000000000000106498 ) ;
#185667 = CARTESIAN_POINT ( 'NONE',  ( -16.82542659449974565, 66.06550010858458677, -115.7677430845504318 ) ) ;
#185669 = CIRCLE ( 'NONE', #44004, 0.1000000000000024342 ) ;
#185668 = DIRECTION ( 'NONE',  ( 1.000000000000000000, -0.000000000000000000, -0.000000000000000000 ) ) ;
#185670 = EDGE_CURVE ( 'NONE', #147060, #95393, #14462, .T. ) ;
#185671 = VECTOR ( 'NONE', #93823, 1000.000000000000000 ) ;
#185672 = VECTOR ( 'NONE', #46552, 1000.000000000000000 ) ;
#185673 = DIRECTION ( 'NONE',  ( 0.000000000000000000, -0.9770955615653357240, -0.2128009952263410220 ) ) ;
#185674 = ORIENTED_EDGE ( 'NONE', *, *, #188389, .T. ) ;
#185675 = DIRECTION ( 'NONE',  ( 0.000000000000000000, -1.265107689135680095E-16, 1.000000000000000000 ) ) ;
#185676 = ORIENTED_EDGE ( 'NONE', *, *, #92597, .T. ) ;
#185677 = CIRCLE ( 'NONE', #256515, 0.09999999999999939493 ) ;
#185678 = CARTESIAN_POINT ( 'NONE',  ( 21.30740335185486245, 60.87731878144036557, -234.2343867990592798 ) ) ;
#185679 = CARTESIAN_POINT ( 'NONE',  ( 23.24999999999999289, 64.35000000001197407, -115.1731074845243796 ) ) ;
#185680 = ADVANCED_FACE ( 'NONE', ( #178222 ), #41285, .F. ) ;
#185681 =( BOUNDED_SURFACE ( )  B_SPLINE_SURFACE ( 3, 2, ( 
 ( #153330, #207188, #34648 ),
 ( #134980, #28592, #88480 ),
 ( #18905, #140124, #121884 ),
 ( #179300, #116725, #20210 ) ),
 .UNSPECIFIED., .F., .F., .F. ) 
 B_SPLINE_SURFACE_WITH_KNOTS ( ( 4, 4 ),
 ( 3, 3 ),
 ( 3.658908243880901523, 4.712388980384689674 ),
 ( 0.000000000000000000, 1.000000000000000000 ),
 .UNSPECIFIED. ) 
 GEOMETRIC_REPRESENTATION_ITEM ( )  RATIONAL_B_SPLINE_SURFACE ( (
 ( 1.000000000000000000, 0.8984936768950646524, 1.000000000000000000),
 ( 1.000000000000000000, 0.8646876308615526474, 1.000000000000000000),
 ( 1.000000000000000000, 0.7953136715913150523, 1.000000000000000000),
 ( 1.000000000000000000, 0.7071067811865475727, 1.000000000000000000) ) ) 
 REPRESENTATION_ITEM ( '' )  SURFACE ( )  );
#185682 = CARTESIAN_POINT ( 'NONE',  ( 20.04142135623730070, 11.65000000001115943, -188.8499999999999659 ) ) ;
#185683 = CARTESIAN_POINT ( 'NONE',  ( -23.15000000000000213, 4.350000000011156054, -88.15000000000004832 ) ) ;
#185684 = VERTEX_POINT ( 'NONE', #200328 ) ;
#185685 = AXIS2_PLACEMENT_3D ( 'NONE', #236902, #252607, #58254 ) ;
#185686 = ADVANCED_FACE ( 'NONE', ( #101174 ), #201687, .F. ) ;
#185687 = DIRECTION ( 'NONE',  ( 1.000000000000000000, 0.000000000000000000, 0.000000000000000000 ) ) ;
#185688 = CARTESIAN_POINT ( 'NONE',  ( 20.95512840106821528, 12.97721512785410702, -210.6622227115684325 ) ) ;
#185689 = EDGE_CURVE ( 'NONE', #109487, #1729, #197573, .T. ) ;
#185690 = CARTESIAN_POINT ( 'NONE',  ( -22.39999999999999858, 1.115600667400684642E-11, -126.2092204016266379 ) ) ;
#185691 = CARTESIAN_POINT ( 'NONE',  ( -21.14999999999999858, 1.115600667400684642E-11, -134.0000000000000000 ) ) ;
#185692 = DIRECTION ( 'NONE',  ( 0.000000000000000000, 0.000000000000000000, -1.000000000000000000 ) ) ;
#185693 = VERTEX_POINT ( 'NONE', #58226 ) ;
#185695 = EDGE_LOOP ( 'NONE', ( #163538, #31690, #57673, #57435 ) ) ;
#185694 = CARTESIAN_POINT ( 'NONE',  ( 20.89192007715127986, 10.32898536001801304, -106.0826683222764899 ) ) ;
#185696 = EDGE_CURVE ( 'NONE', #31610, #156407, #36137, .T. ) ;
#185697 = VERTEX_POINT ( 'NONE', #216021 ) ;
#185698 = CARTESIAN_POINT ( 'NONE',  ( -23.15000000000000213, 1.115600667400684642E-11, -69.10000000000000853 ) ) ;
#185699 = ADVANCED_FACE ( 'NONE', ( #158663 ), #143429, .T. ) ;
#185700 = EDGE_LOOP ( 'NONE', ( #61211, #225240, #39570, #141810 ) ) ;
#185701 = CARTESIAN_POINT ( 'NONE',  ( -20.64999999999999858, 0.000000000000000000, -33.50000000000000000 ) ) ;
#185702 = DIRECTION ( 'NONE',  ( 1.000000000000000000, 0.000000000000000000, 0.000000000000000000 ) ) ;
#185703 = DIRECTION ( 'NONE',  ( 1.000000000000000000, 0.000000000000000000, 0.000000000000000000 ) ) ;
#185705 = ORIENTED_EDGE ( 'NONE', *, *, #16448, .T. ) ;
#185704 = AXIS2_PLACEMENT_3D ( 'NONE', #85717, #149612, #47905 ) ;
#185706 = DIRECTION ( 'NONE',  ( -1.000000000000000000, 1.836970198721029934E-16, 1.282749433769087582E-30 ) ) ;
#185707 = DIRECTION ( 'NONE',  ( -1.000000000000000000, 0.000000000000000000, 0.000000000000000000 ) ) ;
#185708 = CARTESIAN_POINT ( 'NONE',  ( 20.21567752745019320, 10.19811410124265905, -41.38262034765165964 ) ) ;
#185709 = EDGE_LOOP ( 'NONE', ( #75806, #160270, #38874 ) ) ;
#185710 = CARTESIAN_POINT ( 'NONE',  ( 21.00000000000000000, 52.06567329910104291, -231.9654557484363409 ) ) ;
#185712 = EDGE_LOOP ( 'NONE', ( #124274, #67389, #160701, #195056 ) ) ;
#185711 = FACE_OUTER_BOUND ( 'NONE', #74514, .T. ) ;
#185713 = DIRECTION ( 'NONE',  ( 0.000000000000000000, -0.7397360091702647189, -0.6728971962616949742 ) ) ;
#185714 = CARTESIAN_POINT ( 'NONE',  ( 20.04142135623730070, 15.92646454033040015, -219.3818586450342423 ) ) ;
#185715 = CIRCLE ( 'NONE', #39993, 7.791421356237310469 ) ;
#185716 = AXIS2_PLACEMENT_3D ( 'NONE', #6268, #242322, #182370 ) ;
#185717 = EDGE_CURVE ( 'NONE', #24355, #138354, #64316, .T. ) ;
#185718 = AXIS2_PLACEMENT_3D ( 'NONE', #236385, #60306, #120340 ) ;
#185719 = CIRCLE ( 'NONE', #48344, 0.09999999999999892308 ) ;
#185720 = EDGE_CURVE ( 'NONE', #90093, #140287, #239459, .T. ) ;
#185721 = ORIENTED_EDGE ( 'NONE', *, *, #211331, .F. ) ;
#185722 = DIRECTION ( 'NONE',  ( -1.020425574104003999E-15, 0.2128009952263603677, -0.9770955615653313941 ) ) ;
#185723 = FACE_OUTER_BOUND ( 'NONE', #201148, .T. ) ;
#185724 = CARTESIAN_POINT ( 'NONE',  ( 20.94999999999999574, 1.250000000011155299, -175.4999999999999716 ) ) ;
#185725 = ORIENTED_EDGE ( 'NONE', *, *, #246642, .F. ) ;
#185726 = DIRECTION ( 'NONE',  ( -0.000000000000000000, 1.000000000000000000, 6.982962677686266711E-15 ) ) ;
#185727 = EDGE_CURVE ( 'NONE', #146391, #28556, #77792, .T. ) ;
#185728 = DIRECTION ( 'NONE',  ( 1.000000000000000000, 0.000000000000000000, 0.000000000000000000 ) ) ;
#185729 = ORIENTED_EDGE ( 'NONE', *, *, #50157, .T. ) ;
#185730 = ADVANCED_FACE ( 'NONE', ( #115657 ), #243378, .F. ) ;
#185731 = CIRCLE ( 'NONE', #48350, 0.1000000000000013933 ) ;
#185732 = ADVANCED_FACE ( 'NONE', ( #235588 ), #130952, .T. ) ;
#185733 = ORIENTED_EDGE ( 'NONE', *, *, #187873, .F. ) ;
#185734 = CARTESIAN_POINT ( 'NONE',  ( 21.95218792049437795, 68.79849243876603282, -203.6221359243243114 ) ) ;
#185735 = ADVANCED_FACE ( 'NONE', ( #806 ), #157386, .F. ) ;
#185736 = VERTEX_POINT ( 'NONE', #80344 ) ;
#185737 = DIRECTION ( 'NONE',  ( 1.000000000000000000, 0.000000000000000000, 0.000000000000000000 ) ) ;
#185738 = PLANE ( 'NONE',  #221016 ) ;
#185740 = EDGE_LOOP ( 'NONE', ( #131450, #80762, #58283, #225633 ) ) ;
#185739 = DIRECTION ( 'NONE',  ( -1.000000000000000000, 0.000000000000000000, -0.000000000000000000 ) ) ;
#185741 = DIRECTION ( 'NONE',  ( -0.000000000000000000, 0.000000000000000000, 1.000000000000000000 ) ) ;
#185742 = CARTESIAN_POINT ( 'NONE',  ( 20.94999999999999929, 71.00000000001151079, -48.42837350343745584 ) ) ;
#185743 = FACE_OUTER_BOUND ( 'NONE', #124324, .T. ) ;
#185744 = EDGE_CURVE ( 'NONE', #139626, #118915, #19119, .T. ) ;
#185745 = CARTESIAN_POINT ( 'NONE',  ( -21.07928932188134041, 0.09889514566555068775, -27.17148334360670958 ) ) ;
#185746 = CARTESIAN_POINT ( 'NONE',  ( 21.05000000000000071, 1.115600667400684642E-11, -134.0000000000000000 ) ) ;
#185747 = DIRECTION ( 'NONE',  ( 3.616040088954497272E-32, -1.224646799147352961E-16, 1.000000000000000000 ) ) ;
#185749 = ORIENTED_EDGE ( 'NONE', *, *, #81222, .T. ) ;
#185748 = DIRECTION ( 'NONE',  ( 2.694716079187272946E-16, -1.000000000000000000, 0.000000000000000000 ) ) ;
#185750 = DIRECTION ( 'NONE',  ( -1.000000000000000000, 0.000000000000000000, 0.000000000000000000 ) ) ;
#185751 = EDGE_LOOP ( 'NONE', ( #97302, #188165, #237542, #152717 ) ) ;
#185752 = DIRECTION ( 'NONE',  ( 0.7071067811865127117, 0.7071067811865821007, 0.000000000000000000 ) ) ;
#185753 = AXIS2_PLACEMENT_3D ( 'NONE', #235223, #136088, #185518 ) ;
#185754 = CARTESIAN_POINT ( 'NONE',  ( 18.59999999999999076, 77.85161776048127535, -158.4199177649206831 ) ) ;
#185755 = FACE_OUTER_BOUND ( 'NONE', #195994, .T. ) ;
#185756 = CARTESIAN_POINT ( 'NONE',  ( 20.74897398619119215, 65.40430697834617035, -195.8437960282675192 ) ) ;
#185757 = ORIENTED_EDGE ( 'NONE', *, *, #144866, .T. ) ;
#185758 = DIRECTION ( 'NONE',  ( -2.940209281316621016E-16, -1.000000000000000000, -4.704334850106593625E-15 ) ) ;
#185759 = CARTESIAN_POINT ( 'NONE',  ( -20.90000000000000213, 11.49641995933507843, 1.885425182446133885 ) ) ;
#185760 = AXIS2_PLACEMENT_3D ( 'NONE', #11239, #229009, #12541 ) ;
#185761 = AXIS2_PLACEMENT_3D ( 'NONE', #58082, #174252, #137623 ) ;
#185762 = VERTEX_POINT ( 'NONE', #182053 ) ;
#185763 = VECTOR ( 'NONE', #195291, 1000.000000000000000 ) ;
#185764 = CIRCLE ( 'NONE', #123226, 0.09999999999999939493 ) ;
#185765 = LINE ( 'NONE', #166236, #97785 ) ;
#185766 =( BOUNDED_CURVE ( )  B_SPLINE_CURVE ( 3, ( #43055, #238678, #82143, #22218 ),
 .UNSPECIFIED., .F., .F. ) 
 B_SPLINE_CURVE_WITH_KNOTS ( ( 4, 4 ),
 ( 3.141592653589793116, 4.712388980384689674 ),
 .UNSPECIFIED. ) 
 CURVE ( )  GEOMETRIC_REPRESENTATION_ITEM ( )  RATIONAL_B_SPLINE_CURVE ( ( 1.000000000000000000, 0.8047378541243649375, 0.8047378541243649375, 1.000000000000000000 ) ) 
 REPRESENTATION_ITEM ( '' )  );
#185767 = LINE ( 'NONE', #24145, #130420 ) ;
#185768 =( GEOMETRIC_REPRESENTATION_CONTEXT ( 3 ) GLOBAL_UNCERTAINTY_ASSIGNED_CONTEXT ( ( #196607 ) ) GLOBAL_UNIT_ASSIGNED_CONTEXT ( ( #185899, #12427, #129775 ) ) REPRESENTATION_CONTEXT ( 'NONE', 'WORKASPACE' ) );
#185769 = ORIENTED_EDGE ( 'NONE', *, *, #123615, .F. ) ;
#185770 = EDGE_CURVE ( 'NONE', #255048, #211247, #189230, .T. ) ;
#185771 = CARTESIAN_POINT ( 'NONE',  ( -21.07954640115336176, 6.329287696035376776, -66.93399229286031016 ) ) ;
#185772 = VERTEX_POINT ( 'NONE', #28135 ) ;
#185773 = CARTESIAN_POINT ( 'NONE',  ( -14.56556274378147720, 9.446557523083688679, -48.58994195434590324 ) ) ;
#185774 = EDGE_LOOP ( 'NONE', ( #199910, #25546, #238081, #127022 ) ) ;
#185775 = CARTESIAN_POINT ( 'NONE',  ( -23.15000000000000213, 85.00000000001197975, -112.9170766071766820 ) ) ;
#185776 = CARTESIAN_POINT ( 'NONE',  ( 20.85000000000000142, 77.83585931145526615, -58.01866831572577610 ) ) ;
#185777 = VERTEX_POINT ( 'NONE', #166370 ) ;
#185778 = ORIENTED_EDGE ( 'NONE', *, *, #147521, .T. ) ;
#185779 = CARTESIAN_POINT ( 'NONE',  ( 18.59999999999998366, 1.115600667400684642E-11, -67.00000000000000000 ) ) ;
#185781 = VERTEX_POINT ( 'NONE', #205446 ) ;
#185780 = CARTESIAN_POINT ( 'NONE',  ( 15.06592377766032520, 9.417789466963363054, -48.85738454397687036 ) ) ;
#185782 = EDGE_CURVE ( 'NONE', #19886, #237795, #105982, .T. ) ;
#185783 = CARTESIAN_POINT ( 'NONE',  ( -18.59999999999999787, 43.24695311518262031, -245.0026972281755491 ) ) ;
#185785 = ORIENTED_EDGE ( 'NONE', *, *, #2437, .T. ) ;
#185784 = AXIS2_PLACEMENT_3D ( 'NONE', #27616, #228355, #207519 ) ;
#185786 = AXIS2_PLACEMENT_3D ( 'NONE', #180950, #140516, #200507 ) ;
#185787 = EDGE_LOOP ( 'NONE', ( #148724, #112912, #248394, #70234 ) ) ;
#185788 = VECTOR ( 'NONE', #1287, 1000.000000000000000 ) ;
#185789 = CARTESIAN_POINT ( 'NONE',  ( -20.54999999999999716, 85.00000000001232081, -160.1291383618718385 ) ) ;
#185790 = CYLINDRICAL_SURFACE ( 'NONE', #238564, 0.1000000000000028644 ) ;
#185791 = DIRECTION ( 'NONE',  ( 0.000000000000000000, 0.8814952561688439436, -0.4721928772777332362 ) ) ;
#185792 = VECTOR ( 'NONE', #152410, 1000.000000000000114 ) ;
#185793 = CARTESIAN_POINT ( 'NONE',  ( -18.69999999999999929, -10.63400887967554986, 6.002871413764276909 ) ) ;
#185794 = DIRECTION ( 'NONE',  ( -1.000000000000000000, 0.000000000000000000, 0.000000000000000000 ) ) ;
#185795 = DIRECTION ( 'NONE',  ( -1.000000000000000000, -0.000000000000000000, -0.000000000000000000 ) ) ;
#185796 = EDGE_LOOP ( 'NONE', ( #156954, #182363, #254712, #223511 ) ) ;
#185797 = DIRECTION ( 'NONE',  ( -1.000000000000000000, -0.000000000000000000, -0.000000000000000000 ) ) ;
#185798 = LINE ( 'NONE', #21603, #11053 ) ;
#185799 = CARTESIAN_POINT ( 'NONE',  ( 20.94999999999999574, 67.07338541492499928, -128.0514244653012383 ) ) ;
#185800 = ORIENTED_EDGE ( 'NONE', *, *, #31943, .F. ) ;
#185801 = ORIENTED_EDGE ( 'NONE', *, *, #122873, .T. ) ;
#185802 = CARTESIAN_POINT ( 'NONE',  ( 12.84233041328155878, 9.410538608540022665, -115.9326879971408886 ) ) ;
#185803 = ORIENTED_EDGE ( 'NONE', *, *, #202271, .T. ) ;
#185804 = TOROIDAL_SURFACE ( 'NONE', #56777, 3.899999999999999467, 0.1000000000000000056 ) ;
#185805 = CIRCLE ( 'NONE', #73419, 0.09999999999999939493 ) ;
#185806 = DIRECTION ( 'NONE',  ( -0.7070776581708965169, -0.7071359030027827286, -0.000000000000000000 ) ) ;
#185807 = DIRECTION ( 'NONE',  ( 2.715809747126116508E-16, -1.000000000000000000, 0.000000000000000000 ) ) ;
#185808 = ORIENTED_EDGE ( 'NONE', *, *, #154330, .T. ) ;
#185809 = VERTEX_POINT ( 'NONE', #81621 ) ;
#185811 = VERTEX_POINT ( 'NONE', #226279 ) ;
#185810 = CYLINDRICAL_SURFACE ( 'NONE', #36534, 7.900000000000003908 ) ;
#185812 = CARTESIAN_POINT ( 'NONE',  ( 20.94999999999999929, -9.000000000000000000, -23.60603087734755690 ) ) ;
#185813 = EDGE_LOOP ( 'NONE', ( #40644, #213527, #87011 ) ) ;
#185814 = CIRCLE ( 'NONE', #6759, 0.1000000000000013933 ) ;
#185815 = CARTESIAN_POINT ( 'NONE',  ( -23.15000000000000213, 71.75000000001253397, -182.2731074845243882 ) ) ;
#185816 = EDGE_CURVE ( 'NONE', #236713, #12394, #62107, .T. ) ;
#185817 = DIRECTION ( 'NONE',  ( 0.000000000000000000, -6.853228547068871147E-15, 1.000000000000000000 ) ) ;
#185818 = VERTEX_POINT ( 'NONE', #47646 ) ;
#185819 = DIRECTION ( 'NONE',  ( 1.000000000000000000, 0.000000000000000000, 0.000000000000000000 ) ) ;
#185820 = EDGE_CURVE ( 'NONE', #16905, #212172, #193324, .T. ) ;
#185821 = AXIS2_PLACEMENT_3D ( 'NONE', #186801, #8155, #88947 ) ;
#185822 = DIRECTION ( 'NONE',  ( 0.000000000000000000, 0.2128009952263485993, -0.9770955615653341697 ) ) ;
#185823 = ORIENTED_EDGE ( 'NONE', *, *, #107424, .F. ) ;
#185824 = CARTESIAN_POINT ( 'NONE',  ( -21.05000000000000071, 74.25000000001259082, -191.8535959266227451 ) ) ;
#185825 = EDGE_CURVE ( 'NONE', #161777, #204733, #204157, .T. ) ;
#185826 = ADVANCED_FACE ( 'NONE', ( #26853 ), #89244, .T. ) ;
#185827 = CARTESIAN_POINT ( 'NONE',  ( -21.04999999999994387, 83.80000000001119531, -51.02310748452479316 ) ) ;
#185829 = ORIENTED_EDGE ( 'NONE', *, *, #78483, .F. ) ;
#185828 = CARTESIAN_POINT ( 'NONE',  ( -16.83199030136658081, 9.930648033124626295, -46.27240102265748334 ) ) ;
#185830 = CIRCLE ( 'NONE', #227351, 12.87499999999999822 ) ;
#185831 = CYLINDRICAL_SURFACE ( 'NONE', #203383, 0.1000000000000028644 ) ;
#185832 = CARTESIAN_POINT ( 'NONE',  ( -22.46246831459151494, 75.97808783307230840, -81.17297204573428360 ) ) ;
#185833 = AXIS2_PLACEMENT_3D ( 'NONE', #187405, #110415, #53003 ) ;
#185834 = CARTESIAN_POINT ( 'NONE',  ( 18.59999999999999787, 77.85102823015347440, -191.8691942151018566 ) ) ;
#185836 = CARTESIAN_POINT ( 'NONE',  ( 21.05000000000000071, 7.128833340093095217, -233.7327013124392749 ) ) ;
#185835 = CYLINDRICAL_SURFACE ( 'NONE', #73555, 0.09999999999999939493 ) ;
#185838 = AXIS2_PLACEMENT_3D ( 'NONE', #193920, #93513, #73996 ) ;
#185837 = DIRECTION ( 'NONE',  ( 0.000000000000000000, 0.000000000000000000, -1.000000000000000000 ) ) ;
#185839 = CIRCLE ( 'NONE', #139857, 11.89999999999999325 ) ;
#185840 = DIRECTION ( 'NONE',  ( 0.000000000000000000, -0.1350103645451807555, -0.9908441862701610203 ) ) ;
#185841 = EDGE_CURVE ( 'NONE', #157652, #149628, #102470, .T. ) ;
#185842 = CARTESIAN_POINT ( 'NONE',  ( 23.30000000000000426, 3.332938107839120701, -347.0000000000001137 ) ) ;
#185843 = LINE ( 'NONE', #64602, #50856 ) ;
#185844 = ORIENTED_EDGE ( 'NONE', *, *, #158321, .F. ) ;
#185845 = ORIENTED_EDGE ( 'NONE', *, *, #135082, .T. ) ;
#185846 = CARTESIAN_POINT ( 'NONE',  ( 20.95576188350343116, 65.39101945504869207, -128.9118737617700674 ) ) ;
#185847 = ORIENTED_EDGE ( 'NONE', *, *, #98597, .F. ) ;
#185848 = EDGE_CURVE ( 'NONE', #9918, #76960, #124645, .T. ) ;
#185849 = CIRCLE ( 'NONE', #256726, 0.1999999999999987899 ) ;
#185850 = CARTESIAN_POINT ( 'NONE',  ( -20.99780126800916591, 64.39461131213562339, -143.4357549128189362 ) ) ;
#185851 = AXIS2_PLACEMENT_3D ( 'NONE', #77535, #137518, #217052 ) ;
#185852 = VERTEX_POINT ( 'NONE', #103760 ) ;
#185853 = VECTOR ( 'NONE', #101911, 1000.000000000000000 ) ;
#185854 = CARTESIAN_POINT ( 'NONE',  ( -21.05000000000000782, 69.66772772607673403, -169.9855714212388023 ) ) ;
#185855 = DIRECTION ( 'NONE',  ( 0.000000000000000000, -7.272083257015735086E-15, 1.000000000000000000 ) ) ;
#185856 = ORIENTED_EDGE ( 'NONE', *, *, #206547, .F. ) ;
#185857 = CARTESIAN_POINT ( 'NONE',  ( 24.30000000000000071, 3.175288713399624818, -347.0000000000001137 ) ) ;
#185858 = ORIENTED_EDGE ( 'NONE', *, *, #125912, .T. ) ;
#185859 = ORIENTED_EDGE ( 'NONE', *, *, #127914, .T. ) ;
#185860 = DIRECTION ( 'NONE',  ( 5.603264701231745086E-32, -1.897661533703520636E-16, 1.000000000000000000 ) ) ;
#185861 = CARTESIAN_POINT ( 'NONE',  ( 20.85000000000000142, 78.48087866980282001, -232.8271061603568910 ) ) ;
#185863 = ORIENTED_EDGE ( 'NONE', *, *, #168478, .F. ) ;
#185862 = DIRECTION ( 'NONE',  ( -1.000000000000000000, 0.000000000000000000, 0.000000000000000000 ) ) ;
#185864 = CARTESIAN_POINT ( 'NONE',  ( 20.91682497891422798, 65.67736539654943329, -97.46251168765718376 ) ) ;
#185866 = VERTEX_POINT ( 'NONE', #202887 ) ;
#185865 = DIRECTION ( 'NONE',  ( -1.000000000000000000, 2.849773892568378313E-16, -7.728835255496647986E-17 ) ) ;
#185867 = FACE_BOUND ( 'NONE', #225943, .T. ) ;
#185868 = CARTESIAN_POINT ( 'NONE',  ( -18.59999999999999787, 11.65000000001115232, -146.1500000000000341 ) ) ;
#185871 = ADVANCED_FACE ( 'NONE', ( #4669 ), #65951, .F. ) ;
#185870 = ORIENTED_EDGE ( 'NONE', *, *, #167281, .F. ) ;
#185869 = DIRECTION ( 'NONE',  ( 0.000000000000000000, 0.9651348961777160840, -0.2617529984165018475 ) ) ;
#185872 = CARTESIAN_POINT ( 'NONE',  ( 18.59999999999996945, 10.33248238083634440, -173.0948465439131496 ) ) ;
#185873 = CARTESIAN_POINT ( 'NONE',  ( -21.51976009735018991, 33.83367400564330296, -243.2446267297141844 ) ) ;
#185874 = CARTESIAN_POINT ( 'NONE',  ( -16.92989143108098560, 9.950000000011138823, -113.3824838747567298 ) ) ;
#185876 = LINE ( 'NONE', #244562, #174848 ) ;
#185875 = DIRECTION ( 'NONE',  ( 0.000000000000000000, 0.9651348961777379554, -0.2617529984164210233 ) ) ;
#185877 = DIRECTION ( 'NONE',  ( -1.000000000000000000, -0.000000000000000000, -0.000000000000000000 ) ) ;
#185878 = DIRECTION ( 'NONE',  ( 3.469446951953635015E-14, -0.2617529984165031243, -0.9651348961777157509 ) ) ;
#185879 = VECTOR ( 'NONE', #78779, 1000.000000000000000 ) ;
#185880 = CIRCLE ( 'NONE', #219197, 0.09999999999999724387 ) ;
#185881 = LINE ( 'NONE', #128484, #109855 ) ;
#185882 = CIRCLE ( 'NONE', #19296, 0.1999999999999997335 ) ;
#185884 = DIRECTION ( 'NONE',  ( 0.000000000000000000, -1.000000000000000000, 0.000000000000000000 ) ) ;
#185883 = AXIS2_PLACEMENT_3D ( 'NONE', #120825, #239469, #216031 ) ;
#185885 = EDGE_LOOP ( 'NONE', ( #76717, #37227, #92524, #23190 ) ) ;
#185886 = ORIENTED_EDGE ( 'NONE', *, *, #4562, .T. ) ;
#185887 = ORIENTED_EDGE ( 'NONE', *, *, #86162, .T. ) ;
#185888 = EDGE_CURVE ( 'NONE', #237217, #35141, #3387, .T. ) ;
#185889 = SPHERICAL_SURFACE ( 'NONE', #142986, 0.1000000000000000056 ) ;
#185890 = ORIENTED_EDGE ( 'NONE', *, *, #119424, .T. ) ;
#185891 = CARTESIAN_POINT ( 'NONE',  ( 23.04999999999999716, 8.822561741677553471, -191.7499999999999716 ) ) ;
#185892 = ORIENTED_EDGE ( 'NONE', *, *, #97123, .F. ) ;
#185893 = CARTESIAN_POINT ( 'NONE',  ( -18.39999999999999858, -7.817436562502981801, -209.8389866834999111 ) ) ;
#185894 = CARTESIAN_POINT ( 'NONE',  ( -16.91256925476569251, 14.21894878281401375, -219.3624168839846789 ) ) ;
#185895 = ADVANCED_FACE ( 'NONE', ( #82908 ), #42525, .F. ) ;
#185896 = ORIENTED_EDGE ( 'NONE', *, *, #157892, .F. ) ;
#185897 = VECTOR ( 'NONE', #12451, 1000.000000000000000 ) ;
#185898 = CARTESIAN_POINT ( 'NONE',  ( 13.43663047529819998, 9.446645344706400493, -152.4108064561002607 ) ) ;
#185899 =( LENGTH_UNIT ( ) NAMED_UNIT ( * ) SI_UNIT ( .MILLI., .METRE. ) );
#185900 = EDGE_CURVE ( 'NONE', #118795, #198340, #5950, .T. ) ;
#185901 = CIRCLE ( 'NONE', #148505, 0.5000000000000004441 ) ;
#185902 = VECTOR ( 'NONE', #249268, 1000.000000000000000 ) ;
#185903 = ORIENTED_EDGE ( 'NONE', *, *, #138964, .T. ) ;
#185904 = ORIENTED_EDGE ( 'NONE', *, *, #48804, .F. ) ;
#185905 = ORIENTED_EDGE ( 'NONE', *, *, #134772, .F. ) ;
#185906 = CARTESIAN_POINT ( 'NONE',  ( 23.14999999999999858, 76.00000000001142553, -36.02310748452432421 ) ) ;
#185907 = FACE_OUTER_BOUND ( 'NONE', #122645, .T. ) ;
#185908 = VECTOR ( 'NONE', #221297, 1000.000000000000000 ) ;
#185909 = CYLINDRICAL_SURFACE ( 'NONE', #175877, 0.1000000000000002554 ) ;
#185910 = CYLINDRICAL_SURFACE ( 'NONE', #144686, 11.80000000000000426 ) ;
#185911 = CARTESIAN_POINT ( 'NONE',  ( -20.64999999999999858, 54.34471204062663219, -239.4366250215122420 ) ) ;
#185912 = FACE_OUTER_BOUND ( 'NONE', #159215, .T. ) ;
#185913 = ADVANCED_FACE ( 'NONE', ( #161209 ), #63363, .F. ) ;
#185915 = LINE ( 'NONE', #67251, #78499 ) ;
#185914 = PLANE ( 'NONE',  #74864 ) ;
#185916 = DIRECTION ( 'NONE',  ( 0.000000000000000000, 0.000000000000000000, -1.000000000000000000 ) ) ;
#185918 = ORIENTED_EDGE ( 'NONE', *, *, #177417, .F. ) ;
#185917 = CARTESIAN_POINT ( 'NONE',  ( -20.91682497891423154, 10.32263460347359185, -139.5605957968672328 ) ) ;
#185920 = FACE_OUTER_BOUND ( 'NONE', #238698, .T. ) ;
#185919 = CARTESIAN_POINT ( 'NONE',  ( -18.40000000000000213, 64.66825945288661615, -82.17310748452439384 ) ) ;
#185921 = CARTESIAN_POINT ( 'NONE',  ( -18.50000000000000355, -9.399999999988809307, -141.2972597596633193 ) ) ;
#185922 = ORIENTED_EDGE ( 'NONE', *, *, #234516, .T. ) ;
#185923 = CARTESIAN_POINT ( 'NONE',  ( 20.85000000000000142, 11.75000000001115907, -160.7161343370219129 ) ) ;
#185924 = DIRECTION ( 'NONE',  ( 0.000000000000000000, -1.000000000000000000, 0.000000000000000000 ) ) ;
#185926 = EDGE_CURVE ( 'NONE', #246673, #18925, #46366, .T. ) ;
#185925 = CARTESIAN_POINT ( 'NONE',  ( 20.00000000000000355, 64.25000000001148237, -44.87310748452439668 ) ) ;
#185928 = EDGE_CURVE ( 'NONE', #161687, #43295, #43823, .T. ) ;
#185927 = EDGE_LOOP ( 'NONE', ( #28487, #56861, #55109, #104163 ) ) ;
#185929 = DIRECTION ( 'NONE',  ( 0.7071067811865388020, -0.7071067811865561215, 0.000000000000000000 ) ) ;
#185930 = FACE_OUTER_BOUND ( 'NONE', #189594, .T. ) ;
#185931 = DIRECTION ( 'NONE',  ( 0.000000000000000000, -0.4999999999999836242, 0.8660254037844480335 ) ) ;
#185932 = VERTEX_POINT ( 'NONE', #123364 ) ;
#185933 = ORIENTED_EDGE ( 'NONE', *, *, #123483, .T. ) ;
#185934 = EDGE_CURVE ( 'NONE', #102195, #206017, #76782, .T. ) ;
#185935 = DIRECTION ( 'NONE',  ( -1.000000000000000000, -0.000000000000000000, -0.000000000000000000 ) ) ;
#185936 = ORIENTED_EDGE ( 'NONE', *, *, #4097, .F. ) ;
#185937 = FACE_OUTER_BOUND ( 'NONE', #56529, .T. ) ;
#185938 = CARTESIAN_POINT ( 'NONE',  ( 20.94999999999997442, -1.263275465206102233, -108.4018646667464481 ) ) ;
#185939 = DIRECTION ( 'NONE',  ( 0.000000000000000000, -1.000000000000000000, -6.982962677686265922E-15 ) ) ;
#185941 = ADVANCED_FACE ( 'NONE', ( #77173, #230154 ), #250982, .F. ) ;
#185940 = DIRECTION ( 'NONE',  ( 0.7071067811865460184, 0.6824534298470606997, -0.1850873201761399356 ) ) ;
#185942 = ORIENTED_EDGE ( 'NONE', *, *, #49680, .F. ) ;
#185943 = EDGE_CURVE ( 'NONE', #120605, #238407, #135015, .T. ) ;
#185944 = AXIS2_PLACEMENT_3D ( 'NONE', #111524, #191084, #214457 ) ;
#185945 = B_SPLINE_CURVE_WITH_KNOTS ( 'NONE', 3,
 ( #203080, #179689, #122273, #243491, #182251, #61002, #83097, #102675 ),
 .UNSPECIFIED., .F., .F.,
 ( 4, 2, 2, 4 ),
 ( 0.000000000000000000, 0.0002181133598169135998, 0.0003271700397253561425, 0.0004362267196337987936 ),
 .UNSPECIFIED. ) ;
#185946 = CARTESIAN_POINT ( 'NONE',  ( 20.85000000000000142, 70.08587962373171365, -198.1273832143211848 ) ) ;
#185947 = DIRECTION ( 'NONE',  ( 1.000000000000000000, -0.000000000000000000, 0.000000000000000000 ) ) ;
#185948 = CIRCLE ( 'NONE', #44313, 4.299999999999956302 ) ;
#185949 = CARTESIAN_POINT ( 'NONE',  ( 21.14999999999999503, 0.000000000000000000, 6.249999999999998224 ) ) ;
#185950 = CARTESIAN_POINT ( 'NONE',  ( 23.24999999999999645, 36.65892442174472876, -249.5511627012454596 ) ) ;
#185951 = AXIS2_PLACEMENT_3D ( 'NONE', #71176, #76276, #32058 ) ;
#185952 = AXIS2_PLACEMENT_3D ( 'NONE', #173050, #213396, #215960 ) ;
#185953 = VERTEX_POINT ( 'NONE', #151932 ) ;
#185954 = LINE ( 'NONE', #86829, #117719 ) ;
#185955 = MECHANICAL_DESIGN_GEOMETRIC_PRESENTATION_REPRESENTATION (  '', ( #10981 ), #106834 ) ;
#185957 = EDGE_LOOP ( 'NONE', ( #181121, #197320, #204347, #35951, #137 ) ) ;
#185956 = DIRECTION ( 'NONE',  ( -7.304098846218132695E-16, 0.4721928772777346794, 0.8814952561688431665 ) ) ;
#185958 = EDGE_CURVE ( 'NONE', #211698, #143787, #110097, .T. ) ;
#185959 = DIRECTION ( 'NONE',  ( -1.000000000000000000, 0.000000000000000000, 0.000000000000000000 ) ) ;
#185960 = CARTESIAN_POINT ( 'NONE',  ( 18.42595409746851587, 78.23215996841915398, -231.5864510857097684 ) ) ;
#185961 = EDGE_CURVE ( 'NONE', #211199, #183348, #197769, .T. ) ;
#185962 = DIRECTION ( 'NONE',  ( -4.408576920032448588E-17, -0.3896596508880098009, -0.9209589331071360574 ) ) ;
#185963 = CARTESIAN_POINT ( 'NONE',  ( -21.65000000000000213, 7.250000000011138646, -154.8500000000000227 ) ) ;
#185964 = CARTESIAN_POINT ( 'NONE',  ( 23.14999999999999858, 0.000000000000000000, -33.50000000000000000 ) ) ;
#185965 = EDGE_LOOP ( 'NONE', ( #7717, #31526, #58794, #104367, #143955, #148285, #229410, #114234, #90435 ) ) ;
#185966 = SPHERICAL_SURFACE ( 'NONE', #38766, 0.1000000000000000056 ) ;
#185967 = CARTESIAN_POINT ( 'NONE',  ( -23.49999999999994316, 77.25000000001119815, -43.92310748452479885 ) ) ;
#185968 = DIRECTION ( 'NONE',  ( 0.000000000000000000, -6.982962677686266711E-15, 1.000000000000000000 ) ) ;
#185969 = ADVANCED_FACE ( 'NONE', ( #236253 ), #68525, .F. ) ;
#185970 = FACE_OUTER_BOUND ( 'NONE', #146690, .T. ) ;
#185971 = CIRCLE ( 'NONE', #11190, 0.1000000000000024342 ) ;
#185972 = FACE_OUTER_BOUND ( 'NONE', #191545, .T. ) ;
#185973 = AXIS2_PLACEMENT_3D ( 'NONE', #230030, #9692, #89226 ) ;
#185974 = ORIENTED_EDGE ( 'NONE', *, *, #202522, .T. ) ;
#185975 = ORIENTED_EDGE ( 'NONE', *, *, #42046, .F. ) ;
#185976 = CARTESIAN_POINT ( 'NONE',  ( 20.94999999999999574, 4.296375042184049420, -245.1619261326362391 ) ) ;
#185977 = CIRCLE ( 'NONE', #106858, 0.1000000000000072220 ) ;
#185978 = DIRECTION ( 'NONE',  ( 0.000000000000000000, -1.000000000000000000, -7.109473446599835262E-15 ) ) ;
#185979 = CARTESIAN_POINT ( 'NONE',  ( 23.14999999999999858, 5.950000000011160139, -90.19429769496522908 ) ) ;
#185980 = DIRECTION ( 'NONE',  ( -1.000000000000000000, 0.000000000000000000, 0.000000000000000000 ) ) ;
#185981 = AXIS2_PLACEMENT_3D ( 'NONE', #231619, #235437, #52955 ) ;
#185982 = AXIS2_PLACEMENT_3D ( 'NONE', #211852, #33239, #174040 ) ;
#185983 = DIRECTION ( 'NONE',  ( 0.000000000000000000, -1.000000000000000000, -6.982962677686265922E-15 ) ) ;
#185984 = EDGE_CURVE ( 'NONE', #188047, #37415, #132334, .T. ) ;
#185985 = DIRECTION ( 'NONE',  ( 0.000000000000000000, 0.000000000000000000, -1.000000000000000000 ) ) ;
#185986 = B_SPLINE_CURVE_WITH_KNOTS ( 'NONE', 3,
 ( #209896, #31286, #35136, #110774, #190335, #170811 ),
 .UNSPECIFIED., .F., .F.,
 ( 4, 2, 4 ),
 ( 0.000000000000000000, 0.0001496588209255837190, 0.0002993176418511674379 ),
 .UNSPECIFIED. ) ;
#185987 = FACE_OUTER_BOUND ( 'NONE', #137261, .T. ) ;
#185988 = EDGE_CURVE ( 'NONE', #198538, #83517, #137154, .T. ) ;
#185989 = AXIS2_PLACEMENT_3D ( 'NONE', #82543, #202528, #145106 ) ;
#185990 = CIRCLE ( 'NONE', #48613, 0.1000000000000028644 ) ;
#185991 = ORIENTED_EDGE ( 'NONE', *, *, #10294, .T. ) ;
#185993 = CARTESIAN_POINT ( 'NONE',  ( 22.50000000000000000, 75.90000000001276703, -215.2731074845243597 ) ) ;
#185992 = CIRCLE ( 'NONE', #102760, 0.09999999999999939493 ) ;
#185994 = EDGE_CURVE ( 'NONE', #120640, #213598, #17228, .T. ) ;
#185995 = ORIENTED_EDGE ( 'NONE', *, *, #210239, .F. ) ;
#185996 = CARTESIAN_POINT ( 'NONE',  ( 23.24999999999999289, -4.149999999988843058, -134.0000000000000000 ) ) ;
#185997 = DIRECTION ( 'NONE',  ( 0.000000000000000000, 7.026728003956683390E-15, -1.000000000000000000 ) ) ;
#185998 = FACE_OUTER_BOUND ( 'NONE', #188011, .T. ) ;
#185999 = CARTESIAN_POINT ( 'NONE',  ( -16.78055652883087134, 9.946776916136505164, -46.16079183759243421 ) ) ;
#186001 = EDGE_CURVE ( 'NONE', #235587, #86393, #10360, .T. ) ;
#186000 = DIRECTION ( 'NONE',  ( 1.000000000000000000, 0.000000000000000000, 0.000000000000000000 ) ) ;
#186002 = DIRECTION ( 'NONE',  ( 1.000000000000000000, 0.000000000000000000, 0.000000000000000000 ) ) ;
#186003 = DIRECTION ( 'NONE',  ( 1.000000000000000000, 0.000000000000000000, 0.000000000000000000 ) ) ;
#186004 = DIRECTION ( 'NONE',  ( -0.000000000000000000, 0.4721928772777346239, 0.8814952561688430555 ) ) ;
#186005 = DIRECTION ( 'NONE',  ( 0.000000000000000000, -1.000000000000000000, 0.000000000000000000 ) ) ;
#186006 = EDGE_CURVE ( 'NONE', #184576, #210749, #81044, .T. ) ;
#186007 = CYLINDRICAL_SURFACE ( 'NONE', #69054, 0.09999999999999939493 ) ;
#186008 = CARTESIAN_POINT ( 'NONE',  ( 18.49999999999999645, -9.419078080849526913, -40.32992535020828484 ) ) ;
#186009 = DIRECTION ( 'NONE',  ( 2.952720810173289112E-16, -1.000000000000000000, 0.000000000000000000 ) ) ;
#186010 = CARTESIAN_POINT ( 'NONE',  ( 20.95429402530550433, 8.876194151113340425, -176.0230866979378561 ) ) ;
#186011 = ADVANCED_FACE ( 'NONE', ( #50217 ), #52786, .T. ) ;
#186013 = EDGE_CURVE ( 'NONE', #14295, #103755, #43655, .T. ) ;
#186012 = EDGE_CURVE ( 'NONE', #91096, #245418, #131135, .T. ) ;
#186014 = ORIENTED_EDGE ( 'NONE', *, *, #243296, .F. ) ;
#186015 = CARTESIAN_POINT ( 'NONE',  ( 18.50000000000000000, 85.40000000001208491, -129.6410656363516125 ) ) ;
#186016 = CARTESIAN_POINT ( 'NONE',  ( -21.65000000000000213, 68.25000000001205080, -124.1731074845243512 ) ) ;
#186017 = ORIENTED_EDGE ( 'NONE', *, *, #127702, .F. ) ;
#186018 = DIRECTION ( 'NONE',  ( 0.000000000000000000, 0.000000000000000000, 1.000000000000000000 ) ) ;
#186019 = CARTESIAN_POINT ( 'NONE',  ( -23.25000000000000000, 21.13195309841794867, -243.6318585593224100 ) ) ;
#186020 = AXIS2_PLACEMENT_3D ( 'NONE', #84361, #163966, #25734 ) ;
#186021 = AXIS2_PLACEMENT_3D ( 'NONE', #136363, #94698, #135098 ) ;
#186022 = CARTESIAN_POINT ( 'NONE',  ( -23.25000000000000000, 10.74948822439028895, -222.3968794097801549 ) ) ;
#186023 = EDGE_LOOP ( 'NONE', ( #73453, #113240, #196330, #69476 ) ) ;
#186025 = VECTOR ( 'NONE', #241690, 1000.000000000000000 ) ;
#186024 = CARTESIAN_POINT ( 'NONE',  ( 21.05000000000000071, 64.40000000001145963, -42.95131071479990936 ) ) ;
#186026 = CARTESIAN_POINT ( 'NONE',  ( 21.05000000000000071, 70.10000000001177511, -79.74220724918072278 ) ) ;
#186027 = AXIS2_PLACEMENT_3D ( 'NONE', #141214, #42131, #38267 ) ;
#186028 = ORIENTED_EDGE ( 'NONE', *, *, #92662, .T. ) ;
#186029 = EDGE_CURVE ( 'NONE', #207656, #158228, #111496, .T. ) ;
#186030 = EDGE_CURVE ( 'NONE', #179663, #140297, #251942, .T. ) ;
#186031 = VECTOR ( 'NONE', #165652, 1000.000000000000000 ) ;
#186032 = DIRECTION ( 'NONE',  ( 1.000000000000000000, -0.000000000000000000, -0.000000000000000000 ) ) ;
#186033 = ADVANCED_FACE ( 'NONE', ( #51487 ), #71103, .T. ) ;
#186034 = ORIENTED_EDGE ( 'NONE', *, *, #72632, .T. ) ;
#186035 = CARTESIAN_POINT ( 'NONE',  ( -20.85000000000000142, 11.75000000001115552, -200.9999999999999432 ) ) ;
#186037 = VECTOR ( 'NONE', #100851, 1000.000000000000000 ) ;
#186036 = CARTESIAN_POINT ( 'NONE',  ( 21.05000000000000071, 0.09779029130922507751, 6.257814610481526429 ) ) ;
#186038 = EDGE_CURVE ( 'NONE', #26287, #168738, #160391, .T. ) ;
#186039 = CARTESIAN_POINT ( 'NONE',  ( 20.94999999999999929, 5.500000000011153745, -54.59473398108690390 ) ) ;
#186041 = CARTESIAN_POINT ( 'NONE',  ( -21.05000000000000071, -3.187805682001703556, -228.3198038177705484 ) ) ;
#186040 = UNCERTAINTY_MEASURE_WITH_UNIT (LENGTH_MEASURE( 1.000000000000000082E-05 ), #58860, 'distance_accuracy_value', 'NONE');
#186042 = DIRECTION ( 'NONE',  ( 0.000000000000000000, 0.9667078373770113808, 0.2558827019434133376 ) ) ;
#186043 = AXIS2_PLACEMENT_3D ( 'NONE', #132109, #252047, #52552 ) ;
#186044 = DIRECTION ( 'NONE',  ( 1.000000000000000000, 0.000000000000000000, 0.000000000000000000 ) ) ;
#186045 = ADVANCED_FACE ( 'NONE', ( #62758 ), #121478, .T. ) ;
#186046 = DIRECTION ( 'NONE',  ( 0.000000000000000000, 0.2617529984164915779, 0.9651348961777189706 ) ) ;
#186047 = VECTOR ( 'NONE', #238580, 1000.000000000000000 ) ;
#186048 = CARTESIAN_POINT ( 'NONE',  ( -21.05000000000000071, 76.00000000001190870, -103.0231074845243029 ) ) ;
#186049 = LINE ( 'NONE', #204306, #241331 ) ;
#186051 = EDGE_LOOP ( 'NONE', ( #149143, #146500, #30151, #149442 ) ) ;
#186050 = DIRECTION ( 'NONE',  ( 1.000000000000000000, 0.000000000000000000, 0.000000000000000000 ) ) ;
#186052 = ORIENTED_EDGE ( 'NONE', *, *, #214473, .T. ) ;
#186053 = CARTESIAN_POINT ( 'NONE',  ( -15.06720934482788188, 9.417690691074263043, -85.14160069676464104 ) ) ;
#186055 = ORIENTED_EDGE ( 'NONE', *, *, #204351, .F. ) ;
#186054 = FACE_OUTER_BOUND ( 'NONE', #192492, .T. ) ;
#186056 = ORIENTED_EDGE ( 'NONE', *, *, #140940, .T. ) ;
#186057 = CARTESIAN_POINT ( 'NONE',  ( -20.64999999999999858, 53.03738849591485405, -234.3791188517465400 ) ) ;
#186058 = CARTESIAN_POINT ( 'NONE',  ( -23.15000000000000213, 76.00000000001267608, -203.5231074845243597 ) ) ;
#186059 = DIRECTION ( 'NONE',  ( 1.000000000000000000, 0.000000000000000000, -0.000000000000000000 ) ) ;
#186061 = CARTESIAN_POINT ( 'NONE',  ( 20.94999999999999574, 4.136903274969363942, -245.4596299165286268 ) ) ;
#186060 = VECTOR ( 'NONE', #225909, 1000.000000000000000 ) ;
#186062 = EDGE_CURVE ( 'NONE', #128197, #114211, #138409, .T. ) ;
#186063 = EDGE_CURVE ( 'NONE', #25677, #45011, #22368, .T. ) ;
#186064 = CARTESIAN_POINT ( 'NONE',  ( -20.85000000000000142, 64.35000000001141984, -36.02310748452440237 ) ) ;
#186065 = DIRECTION ( 'NONE',  ( -0.000000000000000000, 0.000000000000000000, -1.000000000000000000 ) ) ;
#186066 = CARTESIAN_POINT ( 'NONE',  ( -18.59999999999999787, 61.95000000001162022, -64.00941241376342816 ) ) ;
#186067 = EDGE_CURVE ( 'NONE', #96287, #92780, #240119, .T. ) ;
#186068 = ORIENTED_EDGE ( 'NONE', *, *, #168070, .F. ) ;
#186069 = EDGE_LOOP ( 'NONE', ( #219233, #166774, #55887, #141456 ) ) ;
#186070 = CARTESIAN_POINT ( 'NONE',  ( 20.94999999999999929, -11.39257802169451317, -63.92605042016806749 ) ) ;
#186071 = AXIS2_PLACEMENT_3D ( 'NONE', #55059, #13404, #31704 ) ;
#186072 = TOROIDAL_SURFACE ( 'NONE', #131906, 0.2000000000000000111, 0.1000000000000000056 ) ;
#186073 = ORIENTED_EDGE ( 'NONE', *, *, #101046, .T. ) ;
#186074 = AXIS2_PLACEMENT_3D ( 'NONE', #78907, #159768, #236708 ) ;
#186076 = LINE ( 'NONE', #86937, #59408 ) ;
#186075 = CIRCLE ( 'NONE', #252698, 0.1000000000000024342 ) ;
#186077 = ORIENTED_EDGE ( 'NONE', *, *, #134902, .T. ) ;
#186078 = DIRECTION ( 'NONE',  ( 0.000000000000000000, -7.086529944415894657E-15, 1.000000000000000000 ) ) ;
#186079 = CARTESIAN_POINT ( 'NONE',  ( -21.05000000000000071, 48.05114133249968944, -246.4758750954581785 ) ) ;
#186080 = EDGE_CURVE ( 'NONE', #45216, #74886, #214343, .T. ) ;
#186081 = DIRECTION ( 'NONE',  ( 1.000000000000000000, 0.000000000000000000, 0.000000000000000000 ) ) ;
#186082 = CARTESIAN_POINT ( 'NONE',  ( -16.89318236219976654, 22.97427065100864851, -230.9312879128452494 ) ) ;
#186083 = ORIENTED_EDGE ( 'NONE', *, *, #236007, .T. ) ;
#186084 = DIRECTION ( 'NONE',  ( -1.000000000000000000, -0.000000000000000000, -0.000000000000000000 ) ) ;
#186085 = ORIENTED_EDGE ( 'NONE', *, *, #120594, .T. ) ;
#186086 = PLANE ( 'NONE',  #171625 ) ;
#186087 = DIRECTION ( 'NONE',  ( 0.000000000000000000, 0.000000000000000000, -1.000000000000000000 ) ) ;
#186088 = CARTESIAN_POINT ( 'NONE',  ( 6.099999999999998757, -11.65000000000000036, 10.10000000000000142 ) ) ;
#186089 = AXIS2_PLACEMENT_3D ( 'NONE', #246873, #224736, #164784 ) ;
#186090 = DIRECTION ( 'NONE',  ( 0.000000000000000000, 0.7035695228903320331, 0.7106264324241468033 ) ) ;
#186091 = EDGE_LOOP ( 'NONE', ( #158639, #72587, #200502 ) ) ;
#186092 = AXIS2_PLACEMENT_3D ( 'NONE', #117296, #192988, #14371 ) ;
#186094 = CARTESIAN_POINT ( 'NONE',  ( -21.05000000000000071, 64.36312671090743720, -96.20134827119950671 ) ) ;
#186093 = CIRCLE ( 'NONE', #252714, 0.09999999999999939493 ) ;
#186095 = ORIENTED_EDGE ( 'NONE', *, *, #90844, .F. ) ;
#186098 = ORIENTED_EDGE ( 'NONE', *, *, #219772, .T. ) ;
#186097 = DIRECTION ( 'NONE',  ( 0.000000000000000000, -6.467318590049456648E-15, 1.000000000000000000 ) ) ;
#186096 = DIRECTION ( 'NONE',  ( 1.000000000000000000, -0.000000000000000000, -0.000000000000000000 ) ) ;
#186099 = EDGE_CURVE ( 'NONE', #148396, #178251, #47733, .T. ) ;
#186100 = DIRECTION ( 'NONE',  ( -0.000000000000000000, 0.000000000000000000, -1.000000000000000000 ) ) ;
#186101 = ORIENTED_EDGE ( 'NONE', *, *, #53994, .T. ) ;
#186102 = CARTESIAN_POINT ( 'NONE',  ( -21.64999999999999858, 7.350000000011155166, -146.2500000000000284 ) ) ;
#186103 = ORIENTED_EDGE ( 'NONE', *, *, #245809, .F. ) ;
#186104 = B_SPLINE_CURVE_WITH_KNOTS ( 'NONE', 3,
 ( #124007, #144823, #43179, #202251, #224369, #143548, #45736, #147408, #106984, #2744 ),
 .UNSPECIFIED., .F., .F.,
 ( 4, 3, 3, 4 ),
 ( 7.632826238683052976E-06, 4.756916949876723342E-05, 9.484459048151396053E-05, 0.0001435500935099974268 ),
 .UNSPECIFIED. ) ;
#186105 = DIRECTION ( 'NONE',  ( 0.000000000000000000, 0.000000000000000000, 1.000000000000000000 ) ) ;
#186106 = FACE_OUTER_BOUND ( 'NONE', #151642, .T. ) ;
#186107 = CARTESIAN_POINT ( 'NONE',  ( -22.59999999999999787, 76.00000000001267608, -203.5231074845243597 ) ) ;
#186108 = DIRECTION ( 'NONE',  ( 0.000000000000000000, 0.000000000000000000, -1.000000000000000000 ) ) ;
#186109 = VERTEX_POINT ( 'NONE', #219249 ) ;
#186110 = CARTESIAN_POINT ( 'NONE',  ( 13.40000000000000036, -11.75000000000000000, 12.30000000000000426 ) ) ;
#186111 = DIRECTION ( 'NONE',  ( 0.000000000000000000, -0.2128009952263604232, 0.9770955615653316162 ) ) ;
#186112 = CARTESIAN_POINT ( 'NONE',  ( 21.09813707148777340, 6.385062105747658201, -33.46864850047048634 ) ) ;
#186113 = ORIENTED_EDGE ( 'NONE', *, *, #30699, .F. ) ;
#186114 = CARTESIAN_POINT ( 'NONE',  ( -20.94999999999999929, 76.00000000001165290, -69.52310748452431710 ) ) ;
#186115 = EDGE_LOOP ( 'NONE', ( #30591, #91856, #102051, #196201, #64213, #201093, #257511, #169471, #93794, #124255, #62714, #243604, #255236, #13918, #97870, #20902, #185705, #35789, #108116, #167686, #145955, #198459, #22261, #168831, #100348, #161856, #174494 ) ) ;
#186116 = LINE ( 'NONE', #146968, #231241 ) ;
#186117 = CARTESIAN_POINT ( 'NONE',  ( 23.24999999999999289, 6.450000000011156587, -122.2500000000000284 ) ) ;
#186118 = CARTESIAN_POINT ( 'NONE',  ( 21.05000000000000071, 76.00000000001237765, -170.0231074845243597 ) ) ;
#186120 = ORIENTED_EDGE ( 'NONE', *, *, #96629, .T. ) ;
#186119 = DIRECTION ( 'NONE',  ( 1.000000000000000000, 0.000000000000000000, 0.000000000000000000 ) ) ;
#186121 = CARTESIAN_POINT ( 'NONE',  ( 18.69999999999998153, 7.900000000000000355, -1.212568896937008089 ) ) ;
#186122 = AXIS2_PLACEMENT_3D ( 'NONE', #252647, #192700, #210977 ) ;
#186123 = CARTESIAN_POINT ( 'NONE',  ( -20.94999999999999929, 1.250000000011155299, -108.5000000000000426 ) ) ;
#186124 = EDGE_CURVE ( 'NONE', #71912, #246315, #56100, .T. ) ;
#186125 = CARTESIAN_POINT ( 'NONE',  ( -21.05000000000000071, 2.838478681111047841, -208.5693404029859437 ) ) ;
#186126 = ORIENTED_EDGE ( 'NONE', *, *, #143062, .F. ) ;
#186127 = CIRCLE ( 'NONE', #198591, 0.1000000000000028644 ) ;
#186128 = LINE ( 'NONE', #167878, #97539 ) ;
#186129 = DIRECTION ( 'NONE',  ( 0.000000000000000000, -0.9126074666063660468, -0.4088369013363524762 ) ) ;
#186130 = EDGE_LOOP ( 'NONE', ( #46168, #137081, #72741, #8818 ) ) ;
#186131 = CARTESIAN_POINT ( 'NONE',  ( 18.59999999999999432, 77.73625713160946304, -124.9544551555067926 ) ) ;
#186132 = VECTOR ( 'NONE', #224338, 1000.000000000000000 ) ;
#186133 = AXIS2_PLACEMENT_3D ( 'NONE', #158308, #239096, #201236 ) ;
#186134 = VERTEX_POINT ( 'NONE', #2762 ) ;
#186135 = DIRECTION ( 'NONE',  ( 0.7071067811865463515, 0.7071067811865487940, 4.937700262164540154E-15 ) ) ;
#186138 = ORIENTED_EDGE ( 'NONE', *, *, #253664, .T. ) ;
#186137 = CARTESIAN_POINT ( 'NONE',  ( -22.19999999999999929, -11.65000000000000036, 28.70000000000000284 ) ) ;
#186136 = AXIS2_PLACEMENT_3D ( 'NONE', #131949, #103071, #182652 ) ;
#186139 = ADVANCED_FACE ( 'NONE', ( #142285 ), #127039, .T. ) ;
#186140 = AXIS2_PLACEMENT_3D ( 'NONE', #44186, #68888, #224076 ) ;
#186141 = ADVANCED_FACE ( 'NONE', ( #39373 ), #161882, .F. ) ;
#186144 = ORIENTED_EDGE ( 'NONE', *, *, #256705, .T. ) ;
#186143 = ORIENTED_EDGE ( 'NONE', *, *, #251716, .T. ) ;
#186142 = CARTESIAN_POINT ( 'NONE',  ( 22.48660254037844197, 55.97436536266718576, -232.8539608197349935 ) ) ;
#186145 = DIRECTION ( 'NONE',  ( 0.000000000000000000, 0.9651348961777157509, -0.2617529984165031243 ) ) ;
#186146 = DIRECTION ( 'NONE',  ( -0.000000000000000000, 6.982962677686266711E-15, -1.000000000000000000 ) ) ;
#186147 = CARTESIAN_POINT ( 'NONE',  ( 22.39999999999999503, 1.115600667400684642E-11, -92.75000000000002842 ) ) ;
#186149 = CARTESIAN_POINT ( 'NONE',  ( -12.25000000000000000, 66.65000000001154490, -52.65736431725047595 ) ) ;
#186148 = LINE ( 'NONE', #53048, #31687 ) ;
#186150 = CARTESIAN_POINT ( 'NONE',  ( 18.49999999999998934, 65.75000000001176659, -78.37310748452438247 ) ) ;
#186151 = CARTESIAN_POINT ( 'NONE',  ( -21.45000000000000284, 7.708578643773852157, -179.8499999999999943 ) ) ;
#186153 = EDGE_CURVE ( 'NONE', #97301, #8175, #226816, .T. ) ;
#186152 = AXIS2_PLACEMENT_3D ( 'NONE', #174808, #39121, #75674 ) ;
#186154 = LINE ( 'NONE', #225251, #180694 ) ;
#186155 = DIRECTION ( 'NONE',  ( 1.000000000000000000, 1.186688945009009831E-16, 0.000000000000000000 ) ) ;
#186156 = LINE ( 'NONE', #204418, #176530 ) ;
#186157 = CIRCLE ( 'NONE', #215371, 0.8750000000000007772 ) ;
#186158 = ORIENTED_EDGE ( 'NONE', *, *, #4658, .F. ) ;
#186159 = ORIENTED_EDGE ( 'NONE', *, *, #231563, .F. ) ;
#186160 = EDGE_CURVE ( 'NONE', #209135, #187669, #61476, .T. ) ;
#186162 = DIRECTION ( 'NONE',  ( 1.000000000000000000, 0.000000000000000000, 0.000000000000000000 ) ) ;
#186161 = VECTOR ( 'NONE', #19799, 1000.000000000000000 ) ;
#186165 = ORIENTED_EDGE ( 'NONE', *, *, #4664, .F. ) ;
#186164 = EDGE_CURVE ( 'NONE', #110735, #180828, #152018, .T. ) ;
#186163 = LINE ( 'NONE', #208309, #57830 ) ;
#186166 = AXIS2_PLACEMENT_3D ( 'NONE', #55166, #73517, #96860 ) ;
#186167 = ORIENTED_EDGE ( 'NONE', *, *, #481, .F. ) ;
#186168 = FACE_OUTER_BOUND ( 'NONE', #239332, .T. ) ;
#186169 = VERTEX_POINT ( 'NONE', #41932 ) ;
#186170 = AXIS2_PLACEMENT_3D ( 'NONE', #99151, #111355, #110060 ) ;
#186171 = EDGE_CURVE ( 'NONE', #82116, #42365, #110283, .T. ) ;
#186172 = CIRCLE ( 'NONE', #98641, 12.87499999999999112 ) ;
#186173 = VERTEX_POINT ( 'NONE', #103145 ) ;
#186174 = EDGE_CURVE ( 'NONE', #13269, #124911, #247669, .T. ) ;
#186175 = DIRECTION ( 'NONE',  ( -1.000000000000000000, -0.000000000000000000, 0.000000000000000000 ) ) ;
#186176 = DIRECTION ( 'NONE',  ( 0.000000000000000000, -0.8814952561688476074, 0.4721928772777262417 ) ) ;
#186179 = ORIENTED_EDGE ( 'NONE', *, *, #191429, .F. ) ;
#186178 = ORIENTED_EDGE ( 'NONE', *, *, #99450, .F. ) ;
#186177 = AXIS2_PLACEMENT_3D ( 'NONE', #79692, #53725, #133270 ) ;
#186180 = ORIENTED_EDGE ( 'NONE', *, *, #152939, .T. ) ;
#186181 = CARTESIAN_POINT ( 'NONE',  ( -23.15000000000000213, 11.75000000001116263, -79.15000000000004832 ) ) ;
#186182 = AXIS2_PLACEMENT_3D ( 'NONE', #97381, #102514, #118275 ) ;
#186183 = ORIENTED_EDGE ( 'NONE', *, *, #565, .T. ) ;
#186184 = ORIENTED_EDGE ( 'NONE', *, *, #253079, .T. ) ;
#186185 = CARTESIAN_POINT ( 'NONE',  ( -16.88593481969334675, 14.15994726773271850, -219.2567827423596043 ) ) ;
#186186 = CARTESIAN_POINT ( 'NONE',  ( 21.05000000000000071, 84.73084112150709757, -79.12118220350858167 ) ) ;
#186188 = VERTEX_POINT ( 'NONE', #182722 ) ;
#186187 = DIRECTION ( 'NONE',  ( 1.000000000000000000, 0.000000000000000000, -0.000000000000000000 ) ) ;
#186189 = DIRECTION ( 'NONE',  ( 0.000000000000000000, 0.8814952561688430555, -0.4721928772777346239 ) ) ;
#186190 = DIRECTION ( 'NONE',  ( 1.073024830501117725E-15, -0.000000000000000000, -1.000000000000000000 ) ) ;
#186192 = EDGE_LOOP ( 'NONE', ( #141909, #197253, #107047, #40617 ) ) ;
#186191 = CARTESIAN_POINT ( 'NONE',  ( -18.59999999999999787, 64.25000000001190870, -103.0231074845243882 ) ) ;
#186193 = CARTESIAN_POINT ( 'NONE',  ( 21.14999999999999503, -0.09999999998884338825, -88.85042919245522341 ) ) ;
#186194 = ORIENTED_EDGE ( 'NONE', *, *, #41597, .T. ) ;
#186195 = CARTESIAN_POINT ( 'NONE',  ( -21.07928932188134041, 69.67148334361326079, -103.1220026301789972 ) ) ;
#186197 = EDGE_CURVE ( 'NONE', #38363, #45147, #118691, .T. ) ;
#186196 = ORIENTED_EDGE ( 'NONE', *, *, #164266, .F. ) ;
#186198 = DIRECTION ( 'NONE',  ( 1.000000000000000000, 0.000000000000000000, 0.000000000000000000 ) ) ;
#186199 = FACE_OUTER_BOUND ( 'NONE', #147607, .T. ) ;
#186200 = CIRCLE ( 'NONE', #119579, 3.999999999999999112 ) ;
#186201 = EDGE_LOOP ( 'NONE', ( #34843, #256343, #237134, #131021 ) ) ;
#186203 = DIRECTION ( 'NONE',  ( 0.000000000000000000, -1.000000000000000000, 0.000000000000000000 ) ) ;
#186202 = CARTESIAN_POINT ( 'NONE',  ( 20.95512820512820440, 10.62384868372303259, -45.65000000000000568 ) ) ;
#186204 = DIRECTION ( 'NONE',  ( -0.000000000000000000, 0.000000000000000000, 1.000000000000000000 ) ) ;
#186205 = LINE ( 'NONE', #183643, #234932 ) ;
#186206 = ORIENTED_EDGE ( 'NONE', *, *, #159450, .F. ) ;
#186207 = VERTEX_POINT ( 'NONE', #4061 ) ;
#186208 = AXIS2_PLACEMENT_3D ( 'NONE', #132603, #175586, #130003 ) ;
#186209 = EDGE_CURVE ( 'NONE', #245711, #101037, #135214, .T. ) ;
#186210 = LINE ( 'NONE', #247455, #67819 ) ;
#186211 = DIRECTION ( 'NONE',  ( 0.000000000000000000, 0.000000000000000000, -1.000000000000000000 ) ) ;
#186212 = VERTEX_POINT ( 'NONE', #180150 ) ;
#186213 = CARTESIAN_POINT ( 'NONE',  ( 18.59999999999999076, 6.650000000011155876, -155.1500000000000057 ) ) ;
#186214 = ORIENTED_EDGE ( 'NONE', *, *, #177181, .T. ) ;
#186215 = FACE_OUTER_BOUND ( 'NONE', #12486, .T. ) ;
#186216 = ORIENTED_EDGE ( 'NONE', *, *, #133059, .F. ) ;
#186217 = CIRCLE ( 'NONE', #27841, 0.1999999999999987899 ) ;
#186218 = LINE ( 'NONE', #105347, #149174 ) ;
#186219 = TOROIDAL_SURFACE ( 'NONE', #7122, 0.2000000000000000111, 0.1000000000000000056 ) ;
#186220 = DIRECTION ( 'NONE',  ( 0.000000000000000000, -0.2617529984165152257, -0.9651348961777124202 ) ) ;
#186221 = VECTOR ( 'NONE', #143574, 1000.000000000000000 ) ;
#186222 = AXIS2_PLACEMENT_3D ( 'NONE', #88380, #205782, #83242 ) ;
#186223 = VERTEX_POINT ( 'NONE', #223103 ) ;
#186224 = CARTESIAN_POINT ( 'NONE',  ( 18.39999999999999858, -9.499999999988844479, -207.6001893912220169 ) ) ;
#186225 = AXIS2_PLACEMENT_3D ( 'NONE', #13963, #93475, #11391 ) ;
#186226 = EDGE_CURVE ( 'NONE', #134102, #241641, #255978, .T. ) ;
#186227 = VERTEX_POINT ( 'NONE', #26213 ) ;
#186228 = ORIENTED_EDGE ( 'NONE', *, *, #248453, .F. ) ;
#186229 = ORIENTED_EDGE ( 'NONE', *, *, #245579, .T. ) ;
#186230 = CARTESIAN_POINT ( 'NONE',  ( -18.40000000000000213, 5.649999999999983480, -20.85000000000000142 ) ) ;
#186231 = CYLINDRICAL_SURFACE ( 'NONE', #219679, 0.1000000000000124678 ) ;
#186232 = LINE ( 'NONE', #246201, #17450 ) ;
#186233 = DIRECTION ( 'NONE',  ( -1.000000000000000000, -0.000000000000000000, 0.000000000000000000 ) ) ;
#186234 = CARTESIAN_POINT ( 'NONE',  ( 21.05000000000000071, 5.400000000011154988, -188.5947339810868755 ) ) ;
#186235 = ADVANCED_FACE ( 'NONE', ( #125306 ), #204817, .T. ) ;
#186237 = CARTESIAN_POINT ( 'NONE',  ( 21.05000000000000071, 10.72371710471867701, -74.66491356908764487 ) ) ;
#186236 = CARTESIAN_POINT ( 'NONE',  ( -21.05000000000000071, 1.115600667400684642E-11, -67.00000000000000000 ) ) ;
#186239 = ORIENTED_EDGE ( 'NONE', *, *, #223430, .T. ) ;
#186238 = CARTESIAN_POINT ( 'NONE',  ( -21.05000000000000782, 61.17395774131533415, -234.2804044302905311 ) ) ;
#186240 = CARTESIAN_POINT ( 'NONE',  ( -21.04999999999998295, 6.440770893673168018, -167.5175971870085050 ) ) ;
#186241 = ORIENTED_EDGE ( 'NONE', *, *, #204943, .T. ) ;
#186242 = DIRECTION ( 'NONE',  ( 1.000000000000000000, 0.000000000000000000, 0.000000000000000000 ) ) ;
#186243 = CIRCLE ( 'NONE', #144521, 0.1000000000000002554 ) ;
#186244 = ORIENTED_EDGE ( 'NONE', *, *, #180316, .T. ) ;
#186245 = VERTEX_POINT ( 'NONE', #105701 ) ;
#186246 = DIRECTION ( 'NONE',  ( 0.000000000000000000, 0.000000000000000000, -1.000000000000000000 ) ) ;
#186247 = AXIS2_PLACEMENT_3D ( 'NONE', #134026, #94898, #131472 ) ;
#186248 = CARTESIAN_POINT ( 'NONE',  ( -20.94999999999999929, 7.219003623157315808, -233.4904674204326227 ) ) ;
#186250 = ADVANCED_FACE ( 'NONE', ( #146137 ), #44492, .F. ) ;
#186249 = CARTESIAN_POINT ( 'NONE',  ( -23.24999999999999645, -0.8467571797981052750, -242.2246066262668194 ) ) ;
#186251 = ADVANCED_FACE ( 'NONE', ( #108311 ), #206122, .T. ) ;
#186252 = CARTESIAN_POINT ( 'NONE',  ( -18.59999999999999787, 1.162701749949165642, -41.50000000000000000 ) ) ;
#186253 = EDGE_CURVE ( 'NONE', #243532, #101690, #139141, .T. ) ;
#186254 = AXIS2_PLACEMENT_3D ( 'NONE', #184398, #85274, #244368 ) ;
#186255 = LINE ( 'NONE', #29773, #121741 ) ;
#186256 = ORIENTED_EDGE ( 'NONE', *, *, #126410, .F. ) ;
#186257 = ORIENTED_EDGE ( 'NONE', *, *, #170730, .T. ) ;
#186258 = ADVANCED_FACE ( 'NONE', ( #48325 ), #9199, .T. ) ;
#186259 = DIRECTION ( 'NONE',  ( -1.000000000000000000, 0.000000000000000000, 0.000000000000000000 ) ) ;
#186260 = ORIENTED_EDGE ( 'NONE', *, *, #112633, .F. ) ;
#186261 = CARTESIAN_POINT ( 'NONE',  ( -20.54999999999999716, 7.150000000011155876, -146.3500000000000227 ) ) ;
#186262 = CARTESIAN_POINT ( 'NONE',  ( -18.40000000000000213, 64.52683809664949877, -112.3490535513323323 ) ) ;
#186263 = CARTESIAN_POINT ( 'NONE',  ( 21.05000000000000071, -11.48912529306490349, -103.6000000000000369 ) ) ;
#186264 = DIRECTION ( 'NONE',  ( 0.000000000000000000, 0.9908441862701596881, 0.1350103645451904977 ) ) ;
#186265 = DIRECTION ( 'NONE',  ( 1.000000000000000000, -0.000000000000000000, -0.000000000000000000 ) ) ;
#186266 = DIRECTION ( 'NONE',  ( -1.713057248573685501E-14, 0.9875102702516477260, 0.1575546449569727447 ) ) ;
#186267 = ORIENTED_EDGE ( 'NONE', *, *, #240118, .T. ) ;
#186268 = PLANE ( 'NONE',  #196019 ) ;
#186269 = CARTESIAN_POINT ( 'NONE',  ( 23.24999999999997513, 11.65000000001116298, -59.98519422934606382 ) ) ;
#186270 = DIRECTION ( 'NONE',  ( -1.000000000000000000, -0.000000000000000000, -0.000000000000000000 ) ) ;
#186271 = DIRECTION ( 'NONE',  ( 1.000000000000000000, -0.000000000000000000, -0.000000000000000000 ) ) ;
#186272 = FACE_OUTER_BOUND ( 'NONE', #63226, .T. ) ;
#186273 = AXIS2_PLACEMENT_3D ( 'NONE', #224114, #246263, #127597 ) ;
#186275 = AXIS2_PLACEMENT_3D ( 'NONE', #106693, #66309, #225358 ) ;
#186274 = CARTESIAN_POINT ( 'NONE',  ( 18.45139536634709287, 77.16971529390174567, -241.7973093201318022 ) ) ;
#186276 = AXIS2_PLACEMENT_3D ( 'NONE', #236423, #198576, #213009 ) ;
#186277 = AXIS2_PLACEMENT_3D ( 'NONE', #40375, #162875, #239830 ) ;
#186278 = EDGE_CURVE ( 'NONE', #30941, #119976, #210262, .T. ) ;
#186279 = VERTEX_POINT ( 'NONE', #164438 ) ;
#186280 = CARTESIAN_POINT ( 'NONE',  ( -18.50000000000000000, 70.65875701002036635, -112.8297576910123752 ) ) ;
#186281 = EDGE_LOOP ( 'NONE', ( #203499, #44811, #45439, #136541 ) ) ;
#186282 = EDGE_CURVE ( 'NONE', #203548, #9287, #6222, .T. ) ;
#186283 = EDGE_CURVE ( 'NONE', #183380, #225002, #72917, .T. ) ;
#186284 = CARTESIAN_POINT ( 'NONE',  ( 0.000000000000000000, -10.64999999999999325, 32.89999999999999858 ) ) ;
#186285 = DIRECTION ( 'NONE',  ( 1.000000000000000000, -0.000000000000000000, -0.000000000000000000 ) ) ;
#186286 = DIRECTION ( 'NONE',  ( 1.000000000000000000, 0.000000000000000000, 0.000000000000000000 ) ) ;
#186287 = CARTESIAN_POINT ( 'NONE',  ( 20.53930447208010790, 67.02285131248730465, -161.5806003429519535 ) ) ;
#186288 = ORIENTED_EDGE ( 'NONE', *, *, #209262, .F. ) ;
#186289 = CARTESIAN_POINT ( 'NONE',  ( -20.94999999999999929, -11.39257802169451317, -197.9260504201680249 ) ) ;
#186290 = DIRECTION ( 'NONE',  ( 0.000000000000000000, 0.000000000000000000, 1.000000000000000000 ) ) ;
#186291 = AXIS2_PLACEMENT_3D ( 'NONE', #160446, #20934, #236096 ) ;
#186292 = CARTESIAN_POINT ( 'NONE',  ( -18.40000000000000213, 11.33174054713633261, -87.85000000000003695 ) ) ;
#186293 = DIRECTION ( 'NONE',  ( 1.000000000000000000, -0.000000000000000000, -0.000000000000000000 ) ) ;
#186294 = VECTOR ( 'NONE', #165486, 1000.000000000000000 ) ;
#186295 = DIRECTION ( 'NONE',  ( -1.284434275755705296E-16, 0.7071067811865471286, -0.7071067811865479058 ) ) ;
#186296 = LINE ( 'NONE', #108038, #15600 ) ;
#186297 = TOROIDAL_SURFACE ( 'NONE', #36472, 0.6000000000000015321, 0.1000000000000000056 ) ;
#186298 = VERTEX_POINT ( 'NONE', #87442 ) ;
#186299 = ORIENTED_EDGE ( 'NONE', *, *, #230612, .T. ) ;
#186300 = CARTESIAN_POINT ( 'NONE',  ( -18.79999999999999716, 4.611773100472912112, 22.11686199900910665 ) ) ;
#186301 = CARTESIAN_POINT ( 'NONE',  ( -23.25000000000000000, -11.74999999998884448, -130.9000000000000341 ) ) ;
#186302 = DIRECTION ( 'NONE',  ( 0.000000000000000000, 0.000000000000000000, 1.000000000000000000 ) ) ;
#186303 = CARTESIAN_POINT ( 'NONE',  ( 20.94999999999999929, 87.29603075034701476, -72.57100664418810254 ) ) ;
#186304 = CARTESIAN_POINT ( 'NONE',  ( -22.39999999999999503, 68.20922040163897293, -170.0231074845244166 ) ) ;
#186305 = ORIENTED_EDGE ( 'NONE', *, *, #217838, .F. ) ;
#186306 = DIRECTION ( 'NONE',  ( 0.000000000000000000, -0.8660254037844468122, -0.4999999999999859557 ) ) ;
#186307 = EDGE_CURVE ( 'NONE', #15545, #134939, #106168, .T. ) ;
#186308 = CARTESIAN_POINT ( 'NONE',  ( -23.15000000000000213, 79.08634564045905790, -228.8189404293001132 ) ) ;
#186309 = EDGE_LOOP ( 'NONE', ( #241939, #38305, #36767, #116549 ) ) ;
#186310 = FACE_OUTER_BOUND ( 'NONE', #257244, .T. ) ;
#186311 = VECTOR ( 'NONE', #34217, 1000.000000000000000 ) ;
#186312 = ORIENTED_EDGE ( 'NONE', *, *, #172087, .F. ) ;
#186313 = ORIENTED_EDGE ( 'NONE', *, *, #210950, .F. ) ;
#186314 = DIRECTION ( 'NONE',  ( 0.7071067811865456854, 0.7071067811865493491, 4.937700262164544098E-15 ) ) ;
#186315 = DIRECTION ( 'NONE',  ( -0.7071067811865487940, 0.7071067811865463515, 0.000000000000000000 ) ) ;
#186316 = AXIS2_PLACEMENT_3D ( 'NONE', #102534, #21770, #3462 ) ;
#186317 = CARTESIAN_POINT ( 'NONE',  ( -1.739115166359751801E-14, 11.65000000001114699, -188.8499999999999659 ) ) ;
#186318 = CARTESIAN_POINT ( 'NONE',  ( 21.14999999999999858, 11.65000000001116298, -179.7499999999999716 ) ) ;
#186319 = CARTESIAN_POINT ( 'NONE',  ( 21.05000000000000071, 69.35000000001187459, -93.17928539484123007 ) ) ;
#186320 = EDGE_CURVE ( 'NONE', #135040, #249019, #139500, .T. ) ;
#186321 = CARTESIAN_POINT ( 'NONE',  ( -20.64999999999999858, 4.350000000011156054, -188.6499999999999488 ) ) ;
#186322 = CARTESIAN_POINT ( 'NONE',  ( -16.94445028196808778, 9.992063609697733995, -12.60733017841845438 ) ) ;
#186325 = LINE ( 'NONE', #106763, #49523 ) ;
#186324 = AXIS2_PLACEMENT_3D ( 'NONE', #148837, #25053, #8041 ) ;
#186323 = CARTESIAN_POINT ( 'NONE',  ( 20.95575313997065336, 65.38544669673706267, -95.40181678257957287 ) ) ;
#186326 = DIRECTION ( 'NONE',  ( -1.000000000000000000, -9.012599976027990443E-15, -6.882867235861669241E-14 ) ) ;
#186327 = EDGE_CURVE ( 'NONE', #109487, #102722, #226995, .T. ) ;
#186328 = DIRECTION ( 'NONE',  ( 0.7071359030027766224, -0.7070776581709024011, 0.000000000000000000 ) ) ;
#186329 = CARTESIAN_POINT ( 'NONE',  ( -20.94999999999999929, -11.64999999998884483, -131.1000000000000227 ) ) ;
#186330 = LINE ( 'NONE', #164202, #86467 ) ;
#186331 = AXIS2_PLACEMENT_3D ( 'NONE', #49108, #46530, #7410 ) ;
#186332 = ORIENTED_EDGE ( 'NONE', *, *, #92641, .T. ) ;
#186333 = VECTOR ( 'NONE', #11422, 1000.000000000000000 ) ;
#186334 = VERTEX_POINT ( 'NONE', #7932 ) ;
#186335 = LINE ( 'NONE', #207186, #56618 ) ;
#186336 = DIRECTION ( 'NONE',  ( 2.840903330521631775E-16, -0.8700118002898321601, 0.4930308989875230585 ) ) ;
#186338 = CARTESIAN_POINT ( 'NONE',  ( -15.39126916658603150, 12.96612044530440500, -216.4114274690425361 ) ) ;
#186337 = DIRECTION ( 'NONE',  ( -1.000000000000000000, 2.952720810173289112E-16, 2.061873921506763405E-30 ) ) ;
#186339 = PRODUCT_DEFINITION_FORMATION_WITH_SPECIFIED_SOURCE ( 'ANY', '', #188868, .NOT_KNOWN. ) ;
#186340 = EDGE_CURVE ( 'NONE', #220534, #219647, #131313, .T. ) ;
#186342 = ADVANCED_FACE ( 'NONE', ( #107003 ), #186574, .F. ) ;
#186341 = VECTOR ( 'NONE', #57216, 1000.000000000000000 ) ;
#186343 = CARTESIAN_POINT ( 'NONE',  ( 20.94999999999999574, 39.29335463311362275, -236.8946393634874994 ) ) ;
#186344 = DIRECTION ( 'NONE',  ( -1.000000000000000000, 0.000000000000000000, 0.000000000000000000 ) ) ;
#186345 = VECTOR ( 'NONE', #89372, 1000.000000000000000 ) ;
#186346 = CARTESIAN_POINT ( 'NONE',  ( -20.85000000000000142, 76.00000000001190870, -103.0231074845243029 ) ) ;
#186347 = ORIENTED_EDGE ( 'NONE', *, *, #122702, .T. ) ;
#186348 = ORIENTED_EDGE ( 'NONE', *, *, #23417, .T. ) ;
#186349 = CARTESIAN_POINT ( 'NONE',  ( -15.75000000000000355, 9.349999999999983658, -16.75000000000000355 ) ) ;
#186350 = EDGE_LOOP ( 'NONE', ( #49423, #215967, #118484, #10984 ) ) ;
#186351 = CYLINDRICAL_SURFACE ( 'NONE', #72440, 0.1999999999999987899 ) ;
#186352 = CIRCLE ( 'NONE', #115593, 0.1000000000000000472 ) ;
#186353 = ADVANCED_FACE ( 'NONE', ( #211258 ), #232120, .F. ) ;
#186355 = ADVANCED_FACE ( 'NONE', ( #194290 ), #27308, .T. ) ;
#186354 = AXIS2_PLACEMENT_3D ( 'NONE', #102385, #181968, #3299 ) ;
#186356 = CARTESIAN_POINT ( 'NONE',  ( -21.59142135623730852, 29.56732162031123323, -236.8470621936657210 ) ) ;
#186357 = VECTOR ( 'NONE', #75173, 1000.000000000000000 ) ;
#186359 = ORIENTED_EDGE ( 'NONE', *, *, #225314, .F. ) ;
#186358 = CIRCLE ( 'NONE', #73949, 0.1000000000000124678 ) ;
#186360 = FACE_OUTER_BOUND ( 'NONE', #208601, .T. ) ;
#186361 = ORIENTED_EDGE ( 'NONE', *, *, #241662, .T. ) ;
#186362 = AXIS2_PLACEMENT_3D ( 'NONE', #29626, #50413, #146953 ) ;
#186363 = CARTESIAN_POINT ( 'NONE',  ( -21.14999999999994174, 74.16448838626247664, -47.52760213295649550 ) ) ;
#186364 = DIRECTION ( 'NONE',  ( 1.000000000000000000, 0.000000000000000000, 0.000000000000000000 ) ) ;
#186365 = DIRECTION ( 'NONE',  ( 0.7071067811865474617, 0.7071067811865474617, 0.000000000000000000 ) ) ;
#186366 = DIRECTION ( 'NONE',  ( -1.000000000000000000, -2.952720810173289112E-16, 0.000000000000000000 ) ) ;
#186367 = EDGE_CURVE ( 'NONE', #109875, #70645, #127225, .T. ) ;
#186368 = CARTESIAN_POINT ( 'NONE',  ( -21.14999999999999858, 12.62988036037870998, -223.4632815780722410 ) ) ;
#186369 = CARTESIAN_POINT ( 'NONE',  ( -21.44999999999999929, 68.65000000001253966, -182.3731074845244109 ) ) ;
#186370 = DIRECTION ( 'NONE',  ( -0.7070776581709311559, 0.000000000000000000, 0.7071359030027479786 ) ) ;
#186373 = VERTEX_POINT ( 'NONE', #250380 ) ;
#186372 = ADVANCED_FACE ( 'NONE', ( #74351 ), #75622, .F. ) ;
#186371 = CARTESIAN_POINT ( 'NONE',  ( 18.47135592147653327, -0.7030496522306831642, -242.2786693462419123 ) ) ;
#186375 = CARTESIAN_POINT ( 'NONE',  ( -20.64999999999999858, 4.350000000011156054, -54.65000000000000568 ) ) ;
#186374 = DIRECTION ( 'NONE',  ( 1.000000000000000000, -1.772924042024179204E-16, 4.808324575169891715E-17 ) ) ;
#186376 = ORIENTED_EDGE ( 'NONE', *, *, #129794, .F. ) ;
#186378 = ORIENTED_EDGE ( 'NONE', *, *, #220465, .T. ) ;
#186377 = DIRECTION ( 'NONE',  ( 0.000000000000000000, 1.000000000000000000, 0.000000000000000000 ) ) ;
#186379 = VECTOR ( 'NONE', #247773, 1000.000000000000000 ) ;
#186380 = ORIENTED_EDGE ( 'NONE', *, *, #184140, .F. ) ;
#186381 = DIRECTION ( 'NONE',  ( -0.000000000000000000, -6.982962677686266711E-15, 1.000000000000000000 ) ) ;
#186382 = VECTOR ( 'NONE', #203622, 1000.000000000000000 ) ;
#186383 = CIRCLE ( 'NONE', #190669, 0.1000000000000072220 ) ;
#186384 = DIRECTION ( 'NONE',  ( -1.000000000000000000, -0.000000000000000000, -0.000000000000000000 ) ) ;
#186385 = DIRECTION ( 'NONE',  ( 0.000000000000000000, 6.982962677686266711E-15, -1.000000000000000000 ) ) ;
#186386 = CARTESIAN_POINT ( 'NONE',  ( -18.50000000000000000, 64.35000000001264198, -196.5083017138704236 ) ) ;
#186387 = DIRECTION ( 'NONE',  ( -1.000000000000000000, -0.000000000000000000, -0.000000000000000000 ) ) ;
#186388 = EDGE_CURVE ( 'NONE', #101205, #156063, #164649, .T. ) ;
#186389 = FACE_OUTER_BOUND ( 'NONE', #58537, .T. ) ;
#186390 = CARTESIAN_POINT ( 'NONE',  ( 18.39999999999999503, 70.35000000001230092, -157.3731074845244109 ) ) ;
#186391 = DIRECTION ( 'NONE',  ( 0.000000000000000000, -0.9915357197604882655, 0.1298341882519793711 ) ) ;
#186392 = CIRCLE ( 'NONE', #194772, 0.4999999999999972800 ) ;
#186393 = AXIS2_PLACEMENT_3D ( 'NONE', #118862, #74625, #18460 ) ;
#186394 = FACE_OUTER_BOUND ( 'NONE', #200154, .T. ) ;
#186395 = ADVANCED_FACE ( 'NONE', ( #13078 ), #73072, .T. ) ;
#186396 = EDGE_LOOP ( 'NONE', ( #100557, #60225, #106825 ) ) ;
#186397 = EDGE_LOOP ( 'NONE', ( #180346, #142405, #48130, #225788 ) ) ;
#186398 = CARTESIAN_POINT ( 'NONE',  ( -16.92132318717937522, 9.966070024017081863, -180.1224066303520317 ) ) ;
#186399 = AXIS2_PLACEMENT_3D ( 'NONE', #240488, #98358, #138775 ) ;
#186400 = EDGE_LOOP ( 'NONE', ( #237109, #226473, #90976, #5723 ) ) ;
#186401 = VERTEX_POINT ( 'NONE', #52166 ) ;
#186402 = FACE_OUTER_BOUND ( 'NONE', #143642, .T. ) ;
#186403 = CIRCLE ( 'NONE', #111553, 0.1000000000000028644 ) ;
#186404 = CARTESIAN_POINT ( 'NONE',  ( 19.80993210785512204, 11.74999999999953104, -24.76711774888639184 ) ) ;
#186405 = CARTESIAN_POINT ( 'NONE',  ( -21.53752568617673191, 69.21319212550804423, -103.1220819457949318 ) ) ;
#186406 = EDGE_CURVE ( 'NONE', #110700, #27581, #14828, .T. ) ;
#186407 = CYLINDRICAL_SURFACE ( 'NONE', #6533, 0.1000000000000098310 ) ;
#186408 = DIRECTION ( 'NONE',  ( -1.000000000000000000, 0.000000000000000000, 0.000000000000000000 ) ) ;
#186409 = EDGE_LOOP ( 'NONE', ( #50744, #240073, #81739, #118129 ) ) ;
#186410 = CONICAL_SURFACE ( 'NONE', #74003, 4.000000000000000000, 0.7853981633974489451 ) ;
#186411 = PLANE ( 'NONE',  #132723 ) ;
#186412 = TOROIDAL_SURFACE ( 'NONE', #190523, 11.70000000000000462, 0.1000000000000000056 ) ;
#186413 = AXIS2_PLACEMENT_3D ( 'NONE', #116644, #138731, #97033 ) ;
#186414 = CARTESIAN_POINT ( 'NONE',  ( 23.15000000000000213, -8.999999999988842703, -57.10603087734755690 ) ) ;
#186415 = CIRCLE ( 'NONE', #107283, 0.1000000000000012546 ) ;
#186416 = CARTESIAN_POINT ( 'NONE',  ( -21.11101077989000174, 0.01528526892543598421, -27.07631526527388033 ) ) ;
#186417 = DIRECTION ( 'NONE',  ( -1.652117596168391700E-15, -1.000000000000000000, 0.000000000000000000 ) ) ;
#186418 = ORIENTED_EDGE ( 'NONE', *, *, #192038, .T. ) ;
#186420 = LINE ( 'NONE', #241258, #6778 ) ;
#186419 = SPHERICAL_SURFACE ( 'NONE', #54088, 0.1000000000000000056 ) ;
#186421 = EDGE_LOOP ( 'NONE', ( #13804, #82696, #92256, #182643, #37283 ) ) ;
#186423 = ORIENTED_EDGE ( 'NONE', *, *, #43221, .T. ) ;
#186422 = CARTESIAN_POINT ( 'NONE',  ( 21.14999999999999858, 26.02743912001966464, -254.3139371321002216 ) ) ;
#186424 = AXIS2_PLACEMENT_3D ( 'NONE', #89620, #50480, #32254 ) ;
#186425 = ORIENTED_EDGE ( 'NONE', *, *, #67605, .F. ) ;
#186426 = CARTESIAN_POINT ( 'NONE',  ( 22.50000000000000000, 7.790779598384538929, -33.39999999999999858 ) ) ;
#186427 = CARTESIAN_POINT ( 'NONE',  ( -23.15000000000000213, 11.75000000000000000, -30.39999999999999858 ) ) ;
#186428 = LINE ( 'NONE', #225507, #216735 ) ;
#186429 = ORIENTED_EDGE ( 'NONE', *, *, #54381, .T. ) ;
#186430 = CARTESIAN_POINT ( 'NONE',  ( 20.27550659511088682, 9.216043722520002035, -109.7500000000000426 ) ) ;
#186431 = DIRECTION ( 'NONE',  ( -1.000000000000000000, 0.000000000000000000, 0.000000000000000000 ) ) ;
#186433 = DIRECTION ( 'NONE',  ( 0.000000000000000000, 0.000000000000000000, -1.000000000000000000 ) ) ;
#186432 = CARTESIAN_POINT ( 'NONE',  ( -22.49999999999999645, 11.74956712348939014, 0.1008583690987081283 ) ) ;
#186435 = ORIENTED_EDGE ( 'NONE', *, *, #250201, .F. ) ;
#186434 = CARTESIAN_POINT ( 'NONE',  ( 20.99551997958378635, 11.75000000001123901, -93.65165913769003225 ) ) ;
#186436 = TOROIDAL_SURFACE ( 'NONE', #11655, 1.900000000000002576, 0.1000000000000000056 ) ;
#186437 = VERTEX_POINT ( 'NONE', #135553 ) ;
#186438 = CARTESIAN_POINT ( 'NONE',  ( 18.49999999999999645, -1.835859311432484375, -179.0044391687985410 ) ) ;
#186439 = CIRCLE ( 'NONE', #78073, 7.900000000000000355 ) ;
#186440 = CARTESIAN_POINT ( 'NONE',  ( -18.40000000000000213, 11.48667500176882861, -158.2500000000000284 ) ) ;
#186441 = ORIENTED_EDGE ( 'NONE', *, *, #183609, .F. ) ;
#186442 = CARTESIAN_POINT ( 'NONE',  ( -18.79999999999999716, -1.467286812112899463, 28.00000000000000000 ) ) ;
#186443 = FACE_OUTER_BOUND ( 'NONE', #111060, .T. ) ;
#186444 = CYLINDRICAL_SURFACE ( 'NONE', #118406, 0.1000000000000013933 ) ;
#186445 = ORIENTED_EDGE ( 'NONE', *, *, #17389, .T. ) ;
#186446 = DIRECTION ( 'NONE',  ( 0.000000000000000000, 0.1350103645451807832, 0.9908441862701610203 ) ) ;
#186447 = EDGE_CURVE ( 'NONE', #150252, #51689, #210447, .T. ) ;
#186448 = VERTEX_POINT ( 'NONE', #92576 ) ;
#186449 = CIRCLE ( 'NONE', #144725, 0.2000000000000057288 ) ;
#186450 = FACE_OUTER_BOUND ( 'NONE', #187602, .T. ) ;
#186451 = LINE ( 'NONE', #26098, #252114 ) ;
#186452 = CIRCLE ( 'NONE', #7366, 0.2000000000000111688 ) ;
#186453 = ORIENTED_EDGE ( 'NONE', *, *, #192819, .T. ) ;
#186454 = ORIENTED_EDGE ( 'NONE', *, *, #96936, .T. ) ;
#186455 = CYLINDRICAL_SURFACE ( 'NONE', #241464, 0.5000000000000004441 ) ;
#186456 = ORIENTED_EDGE ( 'NONE', *, *, #199516, .F. ) ;
#186458 = ORIENTED_EDGE ( 'NONE', *, *, #206393, .T. ) ;
#186457 = CARTESIAN_POINT ( 'NONE',  ( -22.50875500270928598, -0.1008579137641491541, -155.7504328726020617 ) ) ;
#186459 = EDGE_LOOP ( 'NONE', ( #251838, #184259, #241023, #228840 ) ) ;
#186460 = EDGE_CURVE ( 'NONE', #158102, #193505, #185489, .T. ) ;
#186462 = ORIENTED_EDGE ( 'NONE', *, *, #182472, .T. ) ;
#186461 = ORIENTED_EDGE ( 'NONE', *, *, #204459, .F. ) ;
#186463 = CIRCLE ( 'NONE', #82374, 11.65000000000000036 ) ;
#186464 = CARTESIAN_POINT ( 'NONE',  ( -18.31572283045302285, -9.548437830874318522, -107.3506256510583086 ) ) ;
#186465 = ORIENTED_EDGE ( 'NONE', *, *, #199235, .F. ) ;
#186466 = CARTESIAN_POINT ( 'NONE',  ( -18.59999999999999787, 1.115600667400684642E-11, -134.0000000000000284 ) ) ;
#186467 = DIRECTION ( 'NONE',  ( 0.000000000000000000, 1.000000000000000000, -0.000000000000000000 ) ) ;
#186468 = CARTESIAN_POINT ( 'NONE',  ( -23.25000000000000000, -11.75000000000000000, -3.100000000000001865 ) ) ;
#186469 = CIRCLE ( 'NONE', #144936, 0.5000000000000004441 ) ;
#186470 = CARTESIAN_POINT ( 'NONE',  ( 20.94999999999999929, 76.00000000001213607, -136.5231074845242745 ) ) ;
#186471 = VERTEX_POINT ( 'NONE', #116023 ) ;
#186472 = ORIENTED_EDGE ( 'NONE', *, *, #16551, .T. ) ;
#186473 = EDGE_CURVE ( 'NONE', #51370, #219226, #114580, .T. ) ;
#186474 = CARTESIAN_POINT ( 'NONE',  ( -18.40000000000000213, 64.25000000001207923, -123.8731074845243683 ) ) ;
#186477 = VERTEX_POINT ( 'NONE', #152601 ) ;
#186476 = ADVANCED_FACE ( 'NONE', ( #16919 ), #2122, .F. ) ;
#186475 = CARTESIAN_POINT ( 'NONE',  ( 18.49999999999999289, 63.61019970229973808, -209.1253633388161006 ) ) ;
#186478 = CYLINDRICAL_SURFACE ( 'NONE', #84183, 0.09999999999999939493 ) ;
#186480 = VERTEX_POINT ( 'NONE', #130428 ) ;
#186479 = CARTESIAN_POINT ( 'NONE',  ( 23.15000000000000213, -12.41227409414968363, -30.39999999999999503 ) ) ;
#186481 =( BOUNDED_SURFACE ( )  B_SPLINE_SURFACE ( 3, 2, ( 
 ( #109915, #167365, #227301 ),
 ( #229881, #189475, #224724 ),
 ( #246858, #245595, #206461 ),
 ( #66947, #149076, #46090 ),
 ( #186927, #126929, #209031 ),
 ( #147783, #111214, #106048 ) ),
 .UNSPECIFIED., .F., .F., .F. ) 
 B_SPLINE_SURFACE_WITH_KNOTS ( ( 4, 2, 4 ),
 ( 3, 3 ),
 ( -1.776356839400250465E-15, 0.7853981633974468357, 1.570796326794895448 ),
 ( 0.000000000000000000, 1.000000000000000000 ),
 .UNSPECIFIED. ) 
 GEOMETRIC_REPRESENTATION_ITEM ( )  RATIONAL_B_SPLINE_SURFACE ( (
 ( 1.000000000000000000, 0.5000000000000101030, 1.000000000000000000),
 ( 1.000000000000000000, 0.4993418825328820865, 1.000000000000000000),
 ( 1.000000000000000000, 0.5278258667065299781, 1.000000000000000000),
 ( 1.000000000000000000, 0.6092287576688560913, 1.000000000000000000),
 ( 1.000000000000000000, 0.6611148371784629774, 1.000000000000000000),
 ( 1.000000000000000000, 0.7071067811865658914, 1.000000000000000000) ) ) 
 REPRESENTATION_ITEM ( '' )  SURFACE ( )  );
#186482 = VERTEX_POINT ( 'NONE', #113438 ) ;
#186483 = CARTESIAN_POINT ( 'NONE',  ( -20.65000000000000568, 68.75000000001188027, -90.37310748452435405 ) ) ;
#186484 = ADVANCED_FACE ( 'NONE', ( #53469 ), #93870, .F. ) ;
#186485 = ORIENTED_EDGE ( 'NONE', *, *, #14510, .T. ) ;
#186486 = ORIENTED_EDGE ( 'NONE', *, *, #166810, .T. ) ;
#186487 = ADVANCED_FACE ( 'NONE', ( #254213 ), #234671, .T. ) ;
#186488 = DIRECTION ( 'NONE',  ( 0.000000000000000000, -0.09425075112713271475, -0.9955484899852801162 ) ) ;
#186489 = CARTESIAN_POINT ( 'NONE',  ( -21.11833042828112994, 0.007100509070636552671, -161.0543553061450837 ) ) ;
#186490 = CIRCLE ( 'NONE', #11528, 0.1000000000000066530 ) ;
#186492 = ORIENTED_EDGE ( 'NONE', *, *, #142487, .T. ) ;
#186491 = VERTEX_POINT ( 'NONE', #209984 ) ;
#186493 = EDGE_LOOP ( 'NONE', ( #134036, #97622, #145896, #225391 ) ) ;
#186494 = CARTESIAN_POINT ( 'NONE',  ( 23.14999999999999858, 78.00000000001190870, -103.0231074845242887 ) ) ;
#186496 = ORIENTED_EDGE ( 'NONE', *, *, #220025, .T. ) ;
#186495 = ADVANCED_FACE ( 'NONE', ( #121180 ), #223741, .T. ) ;
#186497 =( BOUNDED_SURFACE ( )  B_SPLINE_SURFACE ( 3, 2, ( 
 ( #147416, #7922, #11788 ),
 ( #249104, #71750, #150010 ),
 ( #165718, #229532, #146125 ),
 ( #108298, #129142, #148715 ),
 ( #87427, #67874, #131706 ),
 ( #50854, #126573, #211244 ) ),
 .UNSPECIFIED., .F., .F., .F. ) 
 B_SPLINE_SURFACE_WITH_KNOTS ( ( 4, 2, 4 ),
 ( 3, 3 ),
 ( 0.0001792624049599548033, 0.0003686986002124708565, 0.0005581347954649869096 ),
 ( 0.000000000000000000, 1.000000000000000000 ),
 .UNSPECIFIED. ) 
 GEOMETRIC_REPRESENTATION_ITEM ( )  RATIONAL_B_SPLINE_SURFACE ( (
 ( 1.000000000000000000, 0.9238795325112848511, 1.000000000000000000),
 ( 1.000000000000000000, 0.9229318695238726278, 1.000000000000000000),
 ( 1.000000000000000000, 0.8926288119230381124, 1.000000000000000000),
 ( 1.000000000000000000, 0.8123777807271690410, 1.000000000000000000),
 ( 1.000000000000000000, 0.7629087100931283283, 1.000000000000000000),
 ( 1.000000000000000000, 0.7071067811865475727, 1.000000000000000000) ) ) 
 REPRESENTATION_ITEM ( '' )  SURFACE ( )  );
#186498 = ORIENTED_EDGE ( 'NONE', *, *, #133771, .F. ) ;
#186499 = CARTESIAN_POINT ( 'NONE',  ( -20.94999999999999929, -11.48912529306490349, -36.39999999999999858 ) ) ;
#186501 = ORIENTED_EDGE ( 'NONE', *, *, #160495, .T. ) ;
#186500 = CARTESIAN_POINT ( 'NONE',  ( -22.94999999999999929, 0.000000000000000000, 0.000000000000000000 ) ) ;
#186502 = CARTESIAN_POINT ( 'NONE',  ( -23.15000000000000213, 75.45031870333662027, -205.5498907664980948 ) ) ;
#186503 = AXIS2_PLACEMENT_3D ( 'NONE', #206506, #145234, #65711 ) ;
#186504 = DIRECTION ( 'NONE',  ( -1.000000000000000000, 0.000000000000000000, 0.000000000000000000 ) ) ;
#186505 = DIRECTION ( 'NONE',  ( 0.000000000000000000, 0.000000000000000000, 1.000000000000000000 ) ) ;
#186506 = CYLINDRICAL_SURFACE ( 'NONE', #177708, 11.80000000000000426 ) ;
#186507 = ORIENTED_EDGE ( 'NONE', *, *, #248664, .F. ) ;
#186509 = EDGE_CURVE ( 'NONE', #7014, #204625, #139675, .T. ) ;
#186508 = ORIENTED_EDGE ( 'NONE', *, *, #26948, .F. ) ;
#186510 = AXIS2_PLACEMENT_3D ( 'NONE', #48122, #182528, #85937 ) ;
#186511 = LINE ( 'NONE', #183932, #94351 ) ;
#186512 =( NAMED_UNIT ( * ) SI_UNIT ( $, .STERADIAN. ) SOLID_ANGLE_UNIT ( ) );
#186513 = ORIENTED_EDGE ( 'NONE', *, *, #190363, .T. ) ;
#186514 = AXIS2_PLACEMENT_3D ( 'NONE', #56601, #215694, #39676 ) ;
#186515 =( BOUNDED_SURFACE ( )  B_SPLINE_SURFACE ( 3, 2, ( 
 ( #224985, #86763, #72379 ),
 ( #253550, #94479, #191051 ),
 ( #231451, #153217, #71094 ),
 ( #131044, #52779, #111488 ),
 ( #235273, #93197, #12411 ),
 ( #33274, #132327, #155780 ) ),
 .UNSPECIFIED., .F., .F., .F. ) 
 B_SPLINE_SURFACE_WITH_KNOTS ( ( 4, 2, 4 ),
 ( 3, 3 ),
 ( 0.0001300404313046743976, 0.0003183318589266739113, 0.0005066232865486734521 ),
 ( 0.000000000000000000, 1.000000000000000000 ),
 .UNSPECIFIED. ) 
 GEOMETRIC_REPRESENTATION_ITEM ( )  RATIONAL_B_SPLINE_SURFACE ( (
 ( 1.000000000000000000, 0.7071067811866340591, 1.000000000000000000),
 ( 1.000000000000000000, 0.7625113560533209878, 1.000000000000000000),
 ( 1.000000000000000000, 0.8126073484696791915, 1.000000000000000000),
 ( 1.000000000000000000, 0.8923049332723984595, 1.000000000000000000),
 ( 1.000000000000000000, 0.9231914937775878016, 1.000000000000000000),
 ( 1.000000000000000000, 0.9238795325112881818, 1.000000000000000000) ) ) 
 REPRESENTATION_ITEM ( '' )  SURFACE ( )  );
#186516 = DIRECTION ( 'NONE',  ( 0.000000000000000000, 0.4088369013363287729, -0.9126074666063767049 ) ) ;
#186517 = AXIS2_PLACEMENT_3D ( 'NONE', #136114, #38347, #154465 ) ;
#186518 = ORIENTED_EDGE ( 'NONE', *, *, #54710, .F. ) ;
#186519 = VERTEX_POINT ( 'NONE', #119884 ) ;
#186520 = DIRECTION ( 'NONE',  ( 0.000000000000000000, -1.000000000000000000, 0.000000000000000000 ) ) ;
#186521 = CIRCLE ( 'NONE', #231746, 0.1000000000000028644 ) ;
#186522 = DIRECTION ( 'NONE',  ( 0.000000000000000000, 0.000000000000000000, -1.000000000000000000 ) ) ;
#186523 = ORIENTED_EDGE ( 'NONE', *, *, #16135, .T. ) ;
#186524 = CARTESIAN_POINT ( 'NONE',  ( -20.64999999999999858, 0.000000000000000000, -20.62500000000000355 ) ) ;
#186525 = FACE_OUTER_BOUND ( 'NONE', #213053, .T. ) ;
#186526 = ORIENTED_EDGE ( 'NONE', *, *, #58441, .T. ) ;
#186527 = FACE_OUTER_BOUND ( 'NONE', #243149, .T. ) ;
#186528 = LINE ( 'NONE', #166994, #236864 ) ;
#186530 = LINE ( 'NONE', #26175, #58072 ) ;
#186529 = DIRECTION ( 'NONE',  ( 0.000000000000000000, -0.4088369013363280513, 0.9126074666063769270 ) ) ;
#186531 = CARTESIAN_POINT ( 'NONE',  ( -21.05000000000000071, 1.162701749949165642, -75.10000000000003695 ) ) ;
#186532 = CARTESIAN_POINT ( 'NONE',  ( -20.64999999999999858, 65.86663596189677605, -213.5709895136416776 ) ) ;
#186533 = FACE_OUTER_BOUND ( 'NONE', #211181, .T. ) ;
#186534 = LINE ( 'NONE', #11766, #224300 ) ;
#186535 = VERTEX_POINT ( 'NONE', #156457 ) ;
#186536 = VECTOR ( 'NONE', #22604, 1000.000000000000000 ) ;
#186537 = EDGE_CURVE ( 'NONE', #188655, #156311, #97977, .T. ) ;
#186540 = EDGE_LOOP ( 'NONE', ( #212998, #65853, #166646, #136840 ) ) ;
#186539 = VERTEX_POINT ( 'NONE', #41629 ) ;
#186538 = AXIS2_PLACEMENT_3D ( 'NONE', #161504, #241034, #165340 ) ;
#186541 = ORIENTED_EDGE ( 'NONE', *, *, #135206, .F. ) ;
#186543 = ADVANCED_FACE ( 'NONE', ( #101540 ), #160298, .T. ) ;
#186542 = CIRCLE ( 'NONE', #140735, 0.09999999999998898659 ) ;
#186544 = CIRCLE ( 'NONE', #24229, 0.1000000000000024342 ) ;
#186545 = CARTESIAN_POINT ( 'NONE',  ( 16.27683809663749770, 66.65000000001263913, -194.2731074845244166 ) ) ;
#186546 = CARTESIAN_POINT ( 'NONE',  ( 23.14999999999999503, 69.55000000001157900, -57.17310748452436542 ) ) ;
#186547 = AXIS2_PLACEMENT_3D ( 'NONE', #195111, #171704, #135088 ) ;
#186548 = EDGE_CURVE ( 'NONE', #46294, #125917, #220258, .T. ) ;
#186549 = EDGE_CURVE ( 'NONE', #120661, #50342, #118596, .T. ) ;
#186551 = CARTESIAN_POINT ( 'NONE',  ( -23.25000000000000000, 77.73670573947921980, -58.00568489690056850 ) ) ;
#186550 = DIRECTION ( 'NONE',  ( 1.000000000000000000, -0.000000000000000000, -0.000000000000000000 ) ) ;
#186552 = CARTESIAN_POINT ( 'NONE',  ( 21.05000000000000071, 84.73084112150739600, -126.9250327655398962 ) ) ;
#186553 = ORIENTED_EDGE ( 'NONE', *, *, #90244, .F. ) ;
#186554 = CARTESIAN_POINT ( 'NONE',  ( -20.94999999999999929, 87.41227409416181615, -133.5231074845242176 ) ) ;
#186555 = CARTESIAN_POINT ( 'NONE',  ( 18.39999999999999858, -9.499999999988842703, -174.4146583429696875 ) ) ;
#186556 = LINE ( 'NONE', #147417, #214074 ) ;
#186557 = EDGE_CURVE ( 'NONE', #171125, #171525, #181133, .T. ) ;
#186558 = CARTESIAN_POINT ( 'NONE',  ( -21.05000000000002203, 1.363275264940673859, -230.6442496871288483 ) ) ;
#186559 = ORIENTED_EDGE ( 'NONE', *, *, #196340, .F. ) ;
#186560 = EDGE_CURVE ( 'NONE', #61043, #89516, #77152, .T. ) ;
#186561 = CIRCLE ( 'NONE', #128292, 2.100000000000002309 ) ;
#186564 = ADVANCED_FACE ( 'NONE', ( #59855 ), #139397, .T. ) ;
#186563 = ADVANCED_FACE ( 'NONE', ( #159016 ), #238517, .T. ) ;
#186562 = CIRCLE ( 'NONE', #11598, 2.000000000000002665 ) ;
#186565 = CIRCLE ( 'NONE', #40831, 0.09999999999999935330 ) ;
#186566 = CARTESIAN_POINT ( 'NONE',  ( -15.55912972643741199, 67.50912972645004118, -190.9731074845244336 ) ) ;
#186567 = CARTESIAN_POINT ( 'NONE',  ( 21.05000000000000071, 76.00000000001141132, -34.12310748452431852 ) ) ;
#186568 = ORIENTED_EDGE ( 'NONE', *, *, #188393, .T. ) ;
#186569 = ORIENTED_EDGE ( 'NONE', *, *, #162388, .T. ) ;
#186570 = CARTESIAN_POINT ( 'NONE',  ( -16.88005004766534967, 9.950100503332199864, -54.35033611194875647 ) ) ;
#186571 = DIRECTION ( 'NONE',  ( -1.000000000000000000, 0.000000000000000000, 0.000000000000000000 ) ) ;
#186572 = EDGE_CURVE ( 'NONE', #214994, #44904, #218946, .T. ) ;
#186573 = CARTESIAN_POINT ( 'NONE',  ( -21.55000000000000426, 68.25000000001223555, -148.7731074845244166 ) ) ;
#186574 = CYLINDRICAL_SURFACE ( 'NONE', #56294, 0.1000000000000024342 ) ;
#186575 = CARTESIAN_POINT ( 'NONE',  ( -21.05000000000000071, 1.162701749938009677, -8.000000000000000000 ) ) ;
#186576 = CARTESIAN_POINT ( 'NONE',  ( 20.94999999999999929, 1.115600667400684642E-11, -100.5000000000000426 ) ) ;
#186577 = ORIENTED_EDGE ( 'NONE', *, *, #219615, .F. ) ;
#186578 = DIRECTION ( 'NONE',  ( 1.000000000000000000, 0.000000000000000000, -0.000000000000000000 ) ) ;
#186579 = CARTESIAN_POINT ( 'NONE',  ( 21.05000000000000071, 12.04125963260215393, -206.0806513715932624 ) ) ;
#186580 = EDGE_CURVE ( 'NONE', #235714, #59070, #76868, .T. ) ;
#186582 = CARTESIAN_POINT ( 'NONE',  ( -21.03922262424684675, 11.62390063401601381, -174.3592080428932434 ) ) ;
#186581 = DIRECTION ( 'NONE',  ( 0.000000000000000000, -0.9893560106964500722, 0.1455152366551550613 ) ) ;
#186583 = DIRECTION ( 'NONE',  ( 0.000000000000000000, 0.000000000000000000, -1.000000000000000000 ) ) ;
#186584 = CARTESIAN_POINT ( 'NONE',  ( -23.49999999999994316, 84.00000000001119815, -34.86056257560453986 ) ) ;
#186585 = DIRECTION ( 'NONE',  ( 0.000000000000000000, -1.000000000000000000, 0.000000000000000000 ) ) ;
#186587 = DIRECTION ( 'NONE',  ( -1.000000000000000000, -0.000000000000000000, -0.000000000000000000 ) ) ;
#186586 = VECTOR ( 'NONE', #96791, 1000.000000000000000 ) ;
#186588 = ADVANCED_FACE ( 'NONE', ( #1170 ), #182415, .F. ) ;
#186589 = ADVANCED_FACE ( 'NONE', ( #216382 ), #62460, .F. ) ;
#186591 = ORIENTED_EDGE ( 'NONE', *, *, #197841, .T. ) ;
#186590 = CARTESIAN_POINT ( 'NONE',  ( 20.94999999999999929, 77.16270174995034381, -162.1231074845243540 ) ) ;
#186592 = AXIS2_PLACEMENT_3D ( 'NONE', #253207, #88985, #131982 ) ;
#186593 = ADVANCED_FACE ( 'NONE', ( #7613 ), #81224, .F. ) ;
#186594 = EDGE_CURVE ( 'NONE', #178174, #94242, #89609, .T. ) ;
#186595 = EDGE_CURVE ( 'NONE', #110369, #193988, #122955, .T. ) ;
#186596 = CIRCLE ( 'NONE', #119974, 0.1000000000000028644 ) ;
#186597 = FACE_OUTER_BOUND ( 'NONE', #31640, .T. ) ;
#186598 = CIRCLE ( 'NONE', #190707, 0.09999999999999681366 ) ;
#186599 = CARTESIAN_POINT ( 'NONE',  ( -21.05000000000000071, 72.05339752741123505, -225.0867394276846483 ) ) ;
#186600 = AXIS2_PLACEMENT_3D ( 'NONE', #13531, #130893, #228737 ) ;
#186601 = CYLINDRICAL_SURFACE ( 'NONE', #158570, 0.5000000000000004441 ) ;
#186602 = EDGE_LOOP ( 'NONE', ( #66101, #30611, #62917, #141064 ) ) ;
#186603 = AXIS2_PLACEMENT_3D ( 'NONE', #115613, #193881, #218541 ) ;
#186604 = CARTESIAN_POINT ( 'NONE',  ( 21.13736287352038445, 67.95335762362832099, -160.7731074845244166 ) ) ;
#186605 = CYLINDRICAL_SURFACE ( 'NONE', #95365, 0.09999999999999939493 ) ;
#186606 = PLANE ( 'NONE',  #27888 ) ;
#186607 = ORIENTED_EDGE ( 'NONE', *, *, #174502, .T. ) ;
#186608 = CARTESIAN_POINT ( 'NONE',  ( -16.91049119928364419, 66.05000000001160743, -56.90482787771522766 ) ) ;
#186610 = ORIENTED_EDGE ( 'NONE', *, *, #18954, .F. ) ;
#186609 = DIRECTION ( 'NONE',  ( 0.000000000000000000, -1.000000000000000000, 0.000000000000000000 ) ) ;
#186612 = LINE ( 'NONE', #6663, #21341 ) ;
#186611 = DIRECTION ( 'NONE',  ( 0.7071067811865127117, 0.7071067811865821007, 0.000000000000000000 ) ) ;
#186613 = DIRECTION ( 'NONE',  ( -0.000000000000000000, 1.000000000000000000, 6.982962677686266711E-15 ) ) ;
#186614 = ORIENTED_EDGE ( 'NONE', *, *, #217935, .F. ) ;
#186615 = CARTESIAN_POINT ( 'NONE',  ( -16.97683810757273193, 66.05000000001261640, -190.2595307720632150 ) ) ;
#186616 = AXIS2_PLACEMENT_3D ( 'NONE', #26002, #105492, #15432 ) ;
#186617 = DIRECTION ( 'NONE',  ( 0.000000000000000000, 0.000000000000000000, 1.000000000000000000 ) ) ;
#186618 = CARTESIAN_POINT ( 'NONE',  ( -20.89192007715127986, 65.67101464000481315, -63.94043916224794089 ) ) ;
#186619 = LINE ( 'NONE', #228308, #248182 ) ;
#186620 = CARTESIAN_POINT ( 'NONE',  ( 20.94999999999999929, 6.550000000011156231, -177.5170271704400022 ) ) ;
#186621 = ORIENTED_EDGE ( 'NONE', *, *, #220377, .F. ) ;
#186622 = DIRECTION ( 'NONE',  ( 1.000000000000000000, -0.000000000000000000, 0.000000000000000000 ) ) ;
#186623 = DIRECTION ( 'NONE',  ( 1.000000000000000000, -0.000000000000000000, -0.000000000000000000 ) ) ;
#186624 = AXIS2_PLACEMENT_3D ( 'NONE', #89816, #169414, #173276 ) ;
#186625 = DIRECTION ( 'NONE',  ( 0.000000000000000000, -7.026728003956695223E-15, 1.000000000000000000 ) ) ;
#186626 = ORIENTED_EDGE ( 'NONE', *, *, #22388, .T. ) ;
#186627 = EDGE_LOOP ( 'NONE', ( #154932, #171895, #254003, #38653 ) ) ;
#186628 = FACE_OUTER_BOUND ( 'NONE', #216906, .T. ) ;
#186629 = CARTESIAN_POINT ( 'NONE',  ( -21.65000000000000213, 7.708578643773852157, -79.25000000000004263 ) ) ;
#186630 = FACE_OUTER_BOUND ( 'NONE', #203279, .T. ) ;
#186631 = EDGE_CURVE ( 'NONE', #88161, #132227, #156304, .T. ) ;
#186632 = CARTESIAN_POINT ( 'NONE',  ( -21.05000000000000071, -11.41227409413852989, -170.4999999999999716 ) ) ;
#186633 = DIRECTION ( 'NONE',  ( 0.000000000000000000, 0.4721928772777820860, 0.8814952561688176313 ) ) ;
#186634 = CARTESIAN_POINT ( 'NONE',  ( 21.14999999999999503, -11.64999999998883595, -88.75000000000004263 ) ) ;
#186635 = VECTOR ( 'NONE', #137232, 1000.000000000000000 ) ;
#186636 = AXIS2_PLACEMENT_3D ( 'NONE', #151675, #33028, #192071 ) ;
#186638 = FACE_OUTER_BOUND ( 'NONE', #145645, .T. ) ;
#186637 = AXIS2_PLACEMENT_3D ( 'NONE', #142827, #222358, #244514 ) ;
#186639 = EDGE_CURVE ( 'NONE', #229490, #61591, #143265, .T. ) ;
#186640 = CARTESIAN_POINT ( 'NONE',  ( -17.27223548802017561, 65.65460260866892384, -114.3895013053276557 ) ) ;
#186641 = CIRCLE ( 'NONE', #153351, 0.09999999999999939493 ) ;
#186642 = DIRECTION ( 'NONE',  ( 0.000000000000000000, 0.9770955615653313941, 0.2128009952263603677 ) ) ;
#186643 = DIRECTION ( 'NONE',  ( -0.000000000000000000, 0.000000000000000000, 1.000000000000000000 ) ) ;
#186645 = EDGE_LOOP ( 'NONE', ( #88018, #38654, #141750, #130938, #38642 ) ) ;
#186644 = CARTESIAN_POINT ( 'NONE',  ( 15.39170923737819408, 62.83279349218705079, -216.2014764372738114 ) ) ;
#186646 = CARTESIAN_POINT ( 'NONE',  ( 21.11101077988997332, 69.57631526528633970, -170.0383927534386999 ) ) ;
#186647 = DIRECTION ( 'NONE',  ( -1.000000000000000000, 0.000000000000000000, 0.000000000000000000 ) ) ;
#186649 = CARTESIAN_POINT ( 'NONE',  ( -21.05000000000000071, 77.36087058720467269, -195.4501095574333931 ) ) ;
#186648 = DIRECTION ( 'NONE',  ( 0.000000000000000000, 6.982962677686266711E-15, -1.000000000000000000 ) ) ;
#186650 = EDGE_CURVE ( 'NONE', #234836, #184062, #222890, .T. ) ;
#186651 = EDGE_CURVE ( 'NONE', #60888, #188088, #222789, .T. ) ;
#186652 = VERTEX_POINT ( 'NONE', #106691 ) ;
#186653 = DIRECTION ( 'NONE',  ( 0.000000000000000000, 0.2466408114429753939, 0.9691069652678959701 ) ) ;
#186654 = FACE_OUTER_BOUND ( 'NONE', #208633, .T. ) ;
#186655 = DIRECTION ( 'NONE',  ( 0.000000000000000000, 0.000000000000000000, -1.000000000000000000 ) ) ;
#186656 = DIRECTION ( 'NONE',  ( 0.000000000000000000, -6.308085367188388072E-15, 1.000000000000000000 ) ) ;
#186657 = CARTESIAN_POINT ( 'NONE',  ( -20.54999999999999716, 7.128833340094563376, -233.7327013124401276 ) ) ;
#186658 = ORIENTED_EDGE ( 'NONE', *, *, #229851, .F. ) ;
#186659 = ORIENTED_EDGE ( 'NONE', *, *, #150844, .F. ) ;
#186660 = CIRCLE ( 'NONE', #228347, 1.749999999999999778 ) ;
#186662 = AXIS2_PLACEMENT_3D ( 'NONE', #242777, #82398, #202381 ) ;
#186661 = CARTESIAN_POINT ( 'NONE',  ( 23.24999999999999289, -4.149999999988843058, -167.4999999999999716 ) ) ;
#186663 = ORIENTED_EDGE ( 'NONE', *, *, #206925, .F. ) ;
#186664 = CARTESIAN_POINT ( 'NONE',  ( -23.25000000000000000, 76.00000000001168132, -73.57310748452432847 ) ) ;
#186665 = ORIENTED_EDGE ( 'NONE', *, *, #178541, .F. ) ;
#186666 = EDGE_CURVE ( 'NONE', #135320, #209723, #11357, .T. ) ;
#186668 = DIRECTION ( 'NONE',  ( -1.000000000000000000, 0.000000000000000000, -0.000000000000000000 ) ) ;
#186667 = CIRCLE ( 'NONE', #37013, 0.2000000000000005107 ) ;
#186669 = EDGE_CURVE ( 'NONE', #81651, #191031, #82061, .T. ) ;
#186670 = DIRECTION ( 'NONE',  ( 0.000000000000000000, 0.000000000000000000, -1.000000000000000000 ) ) ;
#186671 = DIRECTION ( 'NONE',  ( 0.000000000000000000, 0.9126074666063769270, 0.4088369013363282733 ) ) ;
#186672 = ORIENTED_EDGE ( 'NONE', *, *, #215716, .F. ) ;
#186673 = CARTESIAN_POINT ( 'NONE',  ( -21.05000000000000071, 76.00000000001247713, -174.1231074845243540 ) ) ;
#186674 = CARTESIAN_POINT ( 'NONE',  ( -21.05000000000138627, 65.53264477812935240, -241.9222181873227555 ) ) ;
#186675 = CARTESIAN_POINT ( 'NONE',  ( 19.88284271247461987, 11.69142135623731704, -24.75000000000000000 ) ) ;
#186676 = CARTESIAN_POINT ( 'NONE',  ( 18.59999999999997655, 64.25000000001244871, -170.0231074845244166 ) ) ;
#186677 = DIRECTION ( 'NONE',  ( -1.000000000000000000, 0.000000000000000000, 0.000000000000000000 ) ) ;
#186678 = EDGE_CURVE ( 'NONE', #96601, #161970, #126710, .T. ) ;
#186679 = CARTESIAN_POINT ( 'NONE',  ( 20.94999999999999929, 67.22371710471958295, -124.3731074845243683 ) ) ;
#186680 = CARTESIAN_POINT ( 'NONE',  ( -23.49999999999994316, 87.51781941433023349, -34.28670414799875488 ) ) ;
#186681 = VECTOR ( 'NONE', #244912, 1000.000000000000000 ) ;
#186683 = ORIENTED_EDGE ( 'NONE', *, *, #201935, .T. ) ;
#186682 = EDGE_CURVE ( 'NONE', #42519, #109393, #73738, .T. ) ;
#186685 = CARTESIAN_POINT ( 'NONE',  ( -22.48479450179659977, 75.95300841882587406, -215.1731059307759892 ) ) ;
#186684 = CARTESIAN_POINT ( 'NONE',  ( -18.50000000000000000, 74.16465844978765176, -124.9679561919613207 ) ) ;
#186687 = ORIENTED_EDGE ( 'NONE', *, *, #239573, .F. ) ;
#186686 = AXIS2_PLACEMENT_3D ( 'NONE', #39282, #1390, #22275 ) ;
#186689 = ORIENTED_EDGE ( 'NONE', *, *, #226665, .T. ) ;
#186688 = PLANE ( 'NONE',  #31536 ) ;
#186690 = CIRCLE ( 'NONE', #236533, 0.09999999999998898659 ) ;
#186691 = ORIENTED_EDGE ( 'NONE', *, *, #223452, .F. ) ;
#186692 = CARTESIAN_POINT ( 'NONE',  ( 21.05000000000000071, 48.89266972451527948, -253.5637804087949121 ) ) ;
#186693 = CARTESIAN_POINT ( 'NONE',  ( 18.52643265882457868, 10.31973158071402885, -72.55053347133544150 ) ) ;
#186694 = CARTESIAN_POINT ( 'NONE',  ( 20.94999999999999929, 6.650000000011155876, -188.7499999999999716 ) ) ;
#186695 = ORIENTED_EDGE ( 'NONE', *, *, #83131, .T. ) ;
#186696 = FACE_OUTER_BOUND ( 'NONE', #130306, .T. ) ;
#186697 = AXIS2_PLACEMENT_3D ( 'NONE', #249501, #150408, #172576 ) ;
#186698 = EDGE_CURVE ( 'NONE', #142313, #117463, #204516, .T. ) ;
#186699 = ORIENTED_EDGE ( 'NONE', *, *, #186901, .F. ) ;
#186700 = EDGE_CURVE ( 'NONE', #136780, #75197, #243566, .T. ) ;
#186701 = CARTESIAN_POINT ( 'NONE',  ( 18.42595409746875745, -9.499999812553152623, -174.4993623517493404 ) ) ;
#186702 = DIRECTION ( 'NONE',  ( -3.890533409366484652E-14, 0.1298341882520054891, 0.9915357197604850459 ) ) ;
#186703 = ADVANCED_FACE ( 'NONE', ( #105388 ), #94547, .T. ) ;
#186704 = VECTOR ( 'NONE', #47200, 1000.000000000000000 ) ;
#186705 = ORIENTED_EDGE ( 'NONE', *, *, #47501, .F. ) ;
#186706 = VECTOR ( 'NONE', #219258, 1000.000000000000000 ) ;
#186707 = DIRECTION ( 'NONE',  ( -1.000000000000000000, 0.000000000000000000, 0.000000000000000000 ) ) ;
#186708 = AXIS2_PLACEMENT_3D ( 'NONE', #207896, #149201, #166210 ) ;
#186709 = EDGE_LOOP ( 'NONE', ( #102175, #72017, #250649, #17978 ) ) ;
#186710 = CARTESIAN_POINT ( 'NONE',  ( -16.94107738177414291, 65.98576071487562444, -149.0731074845244279 ) ) ;
#186712 = ORIENTED_EDGE ( 'NONE', *, *, #157449, .T. ) ;
#186711 = AXIS2_PLACEMENT_3D ( 'NONE', #257116, #135919, #99354 ) ;
#186713 = SPHERICAL_SURFACE ( 'NONE', #21232, 0.1000000000000000056 ) ;
#186714 = DIRECTION ( 'NONE',  ( 6.938893903907222067E-15, -1.000000000000000000, -0.000000000000000000 ) ) ;
#186715 = DIRECTION ( 'NONE',  ( 1.000000000000000000, 0.000000000000000000, 0.000000000000000000 ) ) ;
#186716 = ADVANCED_FACE ( 'NONE', ( #85828 ), #227826, .T. ) ;
#186717 = DIRECTION ( 'NONE',  ( 0.000000000000000000, -0.9876197685951263461, 0.1568667991644794590 ) ) ;
#186718 = AXIS2_PLACEMENT_3D ( 'NONE', #172239, #251728, #152660 ) ;
#186719 = EDGE_CURVE ( 'NONE', #64921, #184441, #36320, .T. ) ;
#186720 = AXIS2_PLACEMENT_3D ( 'NONE', #90106, #109672, #92683 ) ;
#186721 = PLANE ( 'NONE',  #107156 ) ;
#186722 = CARTESIAN_POINT ( 'NONE',  ( 18.49999999999999289, 10.25000000001115552, -88.35000000000003695 ) ) ;
#186724 = DIRECTION ( 'NONE',  ( -1.000000000000000000, -0.000000000000000000, 0.000000000000000000 ) ) ;
#186723 = AXIS2_PLACEMENT_3D ( 'NONE', #233634, #254439, #13298 ) ;
#186725 = ORIENTED_EDGE ( 'NONE', *, *, #181535, .T. ) ;
#186727 = CARTESIAN_POINT ( 'NONE',  ( 18.49999999999999289, 6.649999999999999467, -21.15000000000000213 ) ) ;
#186726 = DIRECTION ( 'NONE',  ( -1.000000000000000000, 0.000000000000000000, 0.000000000000000000 ) ) ;
#186728 = AXIS2_PLACEMENT_3D ( 'NONE', #192000, #190720, #169894 ) ;
#186729 = EDGE_LOOP ( 'NONE', ( #210225, #217206, #243900, #135896 ) ) ;
#186730 = AXIS2_PLACEMENT_3D ( 'NONE', #113920, #253424, #12282 ) ;
#186731 = CIRCLE ( 'NONE', #20126, 0.3999999999999975797 ) ;
#186732 = CARTESIAN_POINT ( 'NONE',  ( 20.94999999999999929, 13.09728821260366161, -219.8956789487585013 ) ) ;
#186733 = TOROIDAL_SURFACE ( 'NONE', #178356, 0.2000000000000000111, 0.1000000000000000056 ) ;
#186734 = CARTESIAN_POINT ( 'NONE',  ( 18.39999999999999503, 8.822561741677553471, -124.7500000000000284 ) ) ;
#186735 = CARTESIAN_POINT ( 'NONE',  ( 18.69999999999999929, 3.362550747017869490, 28.82623795144604983 ) ) ;
#186737 = EDGE_LOOP ( 'NONE', ( #242057, #178567, #209007, #182011, #136414, #180436, #209942 ) ) ;
#186736 = CARTESIAN_POINT ( 'NONE',  ( -18.50000000000000000, -9.421290279512176014, -207.8238821790266115 ) ) ;
#186739 = ORIENTED_EDGE ( 'NONE', *, *, #132456, .F. ) ;
#186738 = DIRECTION ( 'NONE',  ( 0.000000000000000000, 0.8814952561688437216, -0.4721928772777334582 ) ) ;
#186740 = CIRCLE ( 'NONE', #28555, 12.87500000000000355 ) ;
#186741 = DIRECTION ( 'NONE',  ( -0.000000000000000000, 6.982962677686266711E-15, -1.000000000000000000 ) ) ;
#186742 = CARTESIAN_POINT ( 'NONE',  ( 19.75857864376268935, 64.35000000001220144, -145.2731074845244450 ) ) ;
#186744 = ORIENTED_EDGE ( 'NONE', *, *, #180645, .F. ) ;
#186743 = CARTESIAN_POINT ( 'NONE',  ( -16.89208623190940628, 9.951577948986638944, -154.8552722032183055 ) ) ;
#186745 = PRODUCT_DEFINITION_SHAPE ( 'NONE', 'NONE',  #195054 ) ;
#186746 = AXIS2_PLACEMENT_3D ( 'NONE', #64870, #189965, #165260 ) ;
#186747 = AXIS2_PLACEMENT_3D ( 'NONE', #217703, #155223, #97746 ) ;
#186748 = DIRECTION ( 'NONE',  ( 1.000000000000000000, 0.000000000000000000, 0.000000000000000000 ) ) ;
#186749 = CARTESIAN_POINT ( 'NONE',  ( -18.59999999999999787, -0.8760381862371811046, -190.6771195118613207 ) ) ;
#186750 = ORIENTED_EDGE ( 'NONE', *, *, #111925, .T. ) ;
#186751 = CARTESIAN_POINT ( 'NONE',  ( 22.39999999999999858, 7.790779598384538929, -33.39999999999999858 ) ) ;
#186752 = ORIENTED_EDGE ( 'NONE', *, *, #20064, .T. ) ;
#186753 = FACE_OUTER_BOUND ( 'NONE', #56020, .T. ) ;
#186754 = CARTESIAN_POINT ( 'NONE',  ( 21.05000000000000071, 22.90266353732884497, -230.0169390150674076 ) ) ;
#186755 = ORIENTED_EDGE ( 'NONE', *, *, #96188, .F. ) ;
#186756 = CARTESIAN_POINT ( 'NONE',  ( -20.00857864376270001, 52.22920805963557456, -232.3304987350788906 ) ) ;
#186757 = CIRCLE ( 'NONE', #116028, 0.5999999999999894307 ) ;
#186758 = AXIS2_PLACEMENT_3D ( 'NONE', #52471, #32978, #192028 ) ;
#186759 = DIRECTION ( 'NONE',  ( 0.000000000000000000, 0.000000000000000000, -1.000000000000000000 ) ) ;
#186761 = ORIENTED_EDGE ( 'NONE', *, *, #76995, .F. ) ;
#186760 = AXIS2_PLACEMENT_3D ( 'NONE', #118671, #95231, #233485 ) ;
#186762 = CARTESIAN_POINT ( 'NONE',  ( -18.59999999999999787, 76.00000000001190870, -103.0231074845243029 ) ) ;
#186763 = VERTEX_POINT ( 'NONE', #51846 ) ;
#186764 = VERTEX_POINT ( 'NONE', #209664 ) ;
#186765 = CARTESIAN_POINT ( 'NONE',  ( -21.05000000000001492, 61.01966792176285992, -234.1522517536919565 ) ) ;
#186766 = ORIENTED_EDGE ( 'NONE', *, *, #127702, .T. ) ;
#186767 = DIRECTION ( 'NONE',  ( 1.000000000000000000, 0.000000000000000000, 0.000000000000000000 ) ) ;
#186769 = EDGE_CURVE ( 'NONE', #106685, #258053, #193965, .T. ) ;
#186768 = VERTEX_POINT ( 'NONE', #229240 ) ;
#186771 = VERTEX_POINT ( 'NONE', #74039 ) ;
#186770 = DIRECTION ( 'NONE',  ( 0.000000000000000000, 0.000000000000000000, -1.000000000000000000 ) ) ;
#186772 = AXIS2_PLACEMENT_3D ( 'NONE', #159574, #239109, #171174 ) ;
#186773 = CARTESIAN_POINT ( 'NONE',  ( -20.94999999999999574, 11.75000000001115552, -73.84160068989719150 ) ) ;
#186774 = ORIENTED_EDGE ( 'NONE', *, *, #27000, .T. ) ;
#186775 = EDGE_CURVE ( 'NONE', #96700, #203969, #240318, .T. ) ;
#186776 = FACE_OUTER_BOUND ( 'NONE', #153830, .T. ) ;
#186778 = EDGE_CURVE ( 'NONE', #230675, #232353, #177791, .T. ) ;
#186777 = AXIS2_PLACEMENT_3D ( 'NONE', #119250, #198762, #163500 ) ;
#186779 = AXIS2_PLACEMENT_3D ( 'NONE', #22399, #242698, #224418 ) ;
#186780 = ORIENTED_EDGE ( 'NONE', *, *, #149677, .T. ) ;
#186783 = ORIENTED_EDGE ( 'NONE', *, *, #49510, .T. ) ;
#186782 = VERTEX_POINT ( 'NONE', #131401 ) ;
#186781 = CARTESIAN_POINT ( 'NONE',  ( 20.94999999999999574, -1.360870587180885716, -108.5729979270909951 ) ) ;
#186784 = CYLINDRICAL_SURFACE ( 'NONE', #190520, 0.09999999999999939493 ) ;
#186785 = TOROIDAL_SURFACE ( 'NONE', #74378, 11.65000000000000036, 0.1000000000000000056 ) ;
#186786 = DIRECTION ( 'NONE',  ( -0.000000000000000000, -1.000000000000000000, 6.308085367188393199E-16 ) ) ;
#186787 = ORIENTED_EDGE ( 'NONE', *, *, #61184, .F. ) ;
#186788 = CIRCLE ( 'NONE', #74382, 0.09999999999999939493 ) ;
#186789 = ORIENTED_EDGE ( 'NONE', *, *, #160936, .T. ) ;
#186790 = EDGE_CURVE ( 'NONE', #56536, #239317, #113131, .T. ) ;
#186791 = FACE_OUTER_BOUND ( 'NONE', #125193, .T. ) ;
#186792 = DIRECTION ( 'NONE',  ( 1.301042606982683418E-14, -0.8660254037844330455, 0.5000000000000096589 ) ) ;
#186794 = ORIENTED_EDGE ( 'NONE', *, *, #2783, .F. ) ;
#186793 = CARTESIAN_POINT ( 'NONE',  ( -18.59999999999999787, 1.115600667400684642E-11, -33.50000000000000000 ) ) ;
#186795 = DIRECTION ( 'NONE',  ( 0.000000000000000000, 0.9209589331071864615, -0.3896596508878908960 ) ) ;
#186796 = ORIENTED_EDGE ( 'NONE', *, *, #9236, .F. ) ;
#186797 = CARTESIAN_POINT ( 'NONE',  ( 18.59999999999999787, -10.84999999999999076, 31.59999999999999787 ) ) ;
#186798 = CARTESIAN_POINT ( 'NONE',  ( -23.25000000000000000, 76.10000000001203091, -114.6726782920691079 ) ) ;
#186799 = AXIS2_PLACEMENT_3D ( 'NONE', #11584, #10298, #192775 ) ;
#186800 = EDGE_LOOP ( 'NONE', ( #105355, #98946, #238332, #1687 ) ) ;
#186801 = CARTESIAN_POINT ( 'NONE',  ( -20.94999999999999929, 76.00000000001126921, -203.5231074845248997 ) ) ;
#186802 = CARTESIAN_POINT ( 'NONE',  ( 23.24999999999999289, -4.054946580484636520, -201.8831241301909074 ) ) ;
#186803 = ORIENTED_EDGE ( 'NONE', *, *, #32553, .T. ) ;
#186804 = CARTESIAN_POINT ( 'NONE',  ( -17.01825945287481545, 51.52760218553060412, -231.9873527057832234 ) ) ;
#186805 = CARTESIAN_POINT ( 'NONE',  ( 21.05000000000000071, 14.05000000001115623, -195.4863049292390542 ) ) ;
#186807 = ORIENTED_EDGE ( 'NONE', *, *, #178054, .T. ) ;
#186806 = ORIENTED_EDGE ( 'NONE', *, *, #4274, .F. ) ;
#186808 = ORIENTED_EDGE ( 'NONE', *, *, #201556, .F. ) ;
#186809 = DIRECTION ( 'NONE',  ( -1.000000000000000000, 3.448943450116728005E-16, 6.438528483529605672E-16 ) ) ;
#186810 = ADVANCED_FACE ( 'NONE', ( #92272 ), #115400, .F. ) ;
#186811 = ORIENTED_EDGE ( 'NONE', *, *, #102477, .F. ) ;
#186812 = EDGE_CURVE ( 'NONE', #129441, #247064, #12770, .T. ) ;
#186813 = CARTESIAN_POINT ( 'NONE',  ( -18.40000000000000213, 31.01370428745238783, -233.5116043003366713 ) ) ;
#186814 = ORIENTED_EDGE ( 'NONE', *, *, #239861, .T. ) ;
#186815 = FACE_OUTER_BOUND ( 'NONE', #257285, .T. ) ;
#186816 = DIRECTION ( 'NONE',  ( -1.000000000000000000, 0.000000000000000000, -0.000000000000000000 ) ) ;
#186817 = ORIENTED_EDGE ( 'NONE', *, *, #198245, .T. ) ;
#186819 = ADVANCED_FACE ( 'NONE', ( #171861 ), #65340, .T. ) ;
#186818 = ORIENTED_EDGE ( 'NONE', *, *, #177728, .T. ) ;
#186820 = AXIS2_PLACEMENT_3D ( 'NONE', #89779, #104204, #226725 ) ;
#186821 = VECTOR ( 'NONE', #139960, 1000.000000000000114 ) ;
#186822 = AXIS2_PLACEMENT_3D ( 'NONE', #250740, #13433, #229903 ) ;
#186823 = VERTEX_POINT ( 'NONE', #192679 ) ;
#186824 = AXIS2_PLACEMENT_3D ( 'NONE', #126926, #82620, #124365 ) ;
#186825 = CARTESIAN_POINT ( 'NONE',  ( -20.94999999999994600, 87.75000000001119815, -6.023107484524794941 ) ) ;
#186826 = ORIENTED_EDGE ( 'NONE', *, *, #151073, .F. ) ;
#186827 = DIRECTION ( 'NONE',  ( 1.000000000000000000, 0.000000000000000000, 0.000000000000000000 ) ) ;
#186829 = ORIENTED_EDGE ( 'NONE', *, *, #24502, .T. ) ;
#186828 = CARTESIAN_POINT ( 'NONE',  ( -15.55912972643740488, 29.60548742189585880, -236.1404802245173755 ) ) ;
#186830 = DIRECTION ( 'NONE',  ( 0.000000000000000000, -6.938893903907222067E-15, 1.000000000000000000 ) ) ;
#186831 = DIRECTION ( 'NONE',  ( -1.000000000000000000, 0.000000000000000000, 0.000000000000000000 ) ) ;
#186832 = DIRECTION ( 'NONE',  ( 1.000000000000000000, 0.000000000000000000, 0.000000000000000000 ) ) ;
#186833 = DIRECTION ( 'NONE',  ( -0.000000000000000000, -2.891205793294679805E-16, 1.000000000000000000 ) ) ;
#186835 = ADVANCED_FACE ( 'NONE', ( #111854 ), #191417, .F. ) ;
#186834 = CARTESIAN_POINT ( 'NONE',  ( -22.50000000000000000, 11.65000000001113278, -134.0000000000000284 ) ) ;
#186838 = DIRECTION ( 'NONE',  ( 4.408576920032447355E-17, 0.1350103645451807555, 0.9908441862701610203 ) ) ;
#186837 = CIRCLE ( 'NONE', #149432, 7.900000000000003908 ) ;
#186836 = FACE_OUTER_BOUND ( 'NONE', #193226, .T. ) ;
#186840 = CARTESIAN_POINT ( 'NONE',  ( -18.59999999999999787, 44.52640028187936849, -247.3006740988509193 ) ) ;
#186839 = AXIS2_PLACEMENT_3D ( 'NONE', #137141, #75876, #36792 ) ;
#186841 = CARTESIAN_POINT ( 'NONE',  ( -20.94999999999994245, 67.75000000001118394, -25.49719488170504533 ) ) ;
#186842 = AXIS2_PLACEMENT_3D ( 'NONE', #121294, #161685, #177405 ) ;
#186843 = CARTESIAN_POINT ( 'NONE',  ( 20.85000000000000142, 11.65000000001115943, -93.71613433702195550 ) ) ;
#186844 = ORIENTED_EDGE ( 'NONE', *, *, #207593, .T. ) ;
#186845 = VECTOR ( 'NONE', #98282, 1000.000000000000000 ) ;
#186846 = EDGE_CURVE ( 'NONE', #199945, #68874, #7074, .T. ) ;
#186847 = VERTEX_POINT ( 'NONE', #251344 ) ;
#186850 = ORIENTED_EDGE ( 'NONE', *, *, #75946, .T. ) ;
#186849 = ADVANCED_FACE ( 'NONE', ( #252627 ), #135242, .F. ) ;
#186848 = DIRECTION ( 'NONE',  ( 1.000000000000000000, -0.000000000000000000, -0.000000000000000000 ) ) ;
#186851 = ORIENTED_EDGE ( 'NONE', *, *, #188421, .T. ) ;
#186852 = PLANE ( 'NONE',  #157580 ) ;
#186853 = CARTESIAN_POINT ( 'NONE',  ( 20.30466543256828160, 9.304236939266628426, -142.2536626513920339 ) ) ;
#186854 = EDGE_CURVE ( 'NONE', #101496, #43638, #127895, .T. ) ;
#186855 = EDGE_CURVE ( 'NONE', #219593, #2430, #14047, .T. ) ;
#186857 = DIRECTION ( 'NONE',  ( 0.000000000000000000, 0.8814952561688476074, -0.4721928772777262417 ) ) ;
#186856 = DIRECTION ( 'NONE',  ( 1.000000000000000000, 0.000000000000000000, 0.000000000000000000 ) ) ;
#186858 = EDGE_LOOP ( 'NONE', ( #206372, #234257, #73234, #100107 ) ) ;
#186859 = CARTESIAN_POINT ( 'NONE',  ( 18.59999994388910238, -9.363566187060008872, -40.68111723680090108 ) ) ;
#186860 = CIRCLE ( 'NONE', #236714, 2.600000000000000089 ) ;
#186861 = DIRECTION ( 'NONE',  ( 1.000000000000000000, 0.000000000000000000, 0.000000000000000000 ) ) ;
#186862 = ORIENTED_EDGE ( 'NONE', *, *, #46408, .T. ) ;
#186863 = CIRCLE ( 'NONE', #140886, 0.1999999999999981515 ) ;
#186864 = VECTOR ( 'NONE', #227680, 1000.000000000000000 ) ;
#186865 = EDGE_CURVE ( 'NONE', #176854, #115699, #32049, .T. ) ;
#186866 = CARTESIAN_POINT ( 'NONE',  ( -23.15000000000000213, 1.115600667400684642E-11, -134.0000000000000284 ) ) ;
#186867 = DIRECTION ( 'NONE',  ( 1.000000000000000000, 0.000000000000000000, -0.000000000000000000 ) ) ;
#186868 = EDGE_CURVE ( 'NONE', #216334, #36408, #69642, .T. ) ;
#186869 = CYLINDRICAL_SURFACE ( 'NONE', #33215, 4.000000000000000000 ) ;
#186870 = CARTESIAN_POINT ( 'NONE',  ( 21.05000000000011795, 65.45624872451554666, -61.96671967585964325 ) ) ;
#186871 = CARTESIAN_POINT ( 'NONE',  ( -23.15000000000000213, 71.65000000001151648, -48.37310748452435405 ) ) ;
#186873 = VERTEX_POINT ( 'NONE', #94839 ) ;
#186872 = DIRECTION ( 'NONE',  ( 1.000000000000000000, 0.000000000000000000, 0.000000000000000000 ) ) ;
#186874 = AXIS2_PLACEMENT_3D ( 'NONE', #188748, #10122, #27152 ) ;
#186875 = EDGE_CURVE ( 'NONE', #249043, #142489, #10192, .T. ) ;
#186876 = CARTESIAN_POINT ( 'NONE',  ( 20.94999999999999929, 65.40605961984559258, -236.6728003091511425 ) ) ;
#186877 = DIRECTION ( 'NONE',  ( 0.000000000000000000, -0.8741572761215385956, 0.4856429311786307768 ) ) ;
#186878 = CARTESIAN_POINT ( 'NONE',  ( 20.94999999999999929, -4.161311414658873886, -226.0656773515597706 ) ) ;
#186879 = CARTESIAN_POINT ( 'NONE',  ( 21.05000000000000071, 1.162701749938009677, -8.099999999999999645 ) ) ;
#186880 = ORIENTED_EDGE ( 'NONE', *, *, #80333, .T. ) ;
#186881 = CARTESIAN_POINT ( 'NONE',  ( -17.78043020864320667, 10.85359211201683927, -77.33695083427984684 ) ) ;
#186882 = CARTESIAN_POINT ( 'NONE',  ( -18.40000000000000213, 13.84507122969784554, -210.9312241760660243 ) ) ;
#186883 = ADVANCED_FACE ( 'NONE', ( #40043 ), #152862, .F. ) ;
#186885 = CARTESIAN_POINT ( 'NONE',  ( -18.50000000000000000, 66.85000000001156195, -57.17310748452438673 ) ) ;
#186884 = CARTESIAN_POINT ( 'NONE',  ( 18.59999999999999076, 10.25000000001115552, -158.7500000000000284 ) ) ;
#186886 = CARTESIAN_POINT ( 'NONE',  ( 20.94999999999999929, 4.813084112149527805, -21.55848224347618114 ) ) ;
#186887 = FACE_OUTER_BOUND ( 'NONE', #80908, .T. ) ;
#186888 = FACE_OUTER_BOUND ( 'NONE', #128450, .T. ) ;
#186889 = DIRECTION ( 'NONE',  ( 0.000000000000000000, 1.000000000000000000, 0.000000000000000000 ) ) ;
#186890 = CIRCLE ( 'NONE', #78518, 11.90000000000000391 ) ;
#186891 = AXIS2_PLACEMENT_3D ( 'NONE', #58585, #18197, #138121 ) ;
#186892 = DIRECTION ( 'NONE',  ( 0.000000000000000000, 0.000000000000000000, -1.000000000000000000 ) ) ;
#186893 = CARTESIAN_POINT ( 'NONE',  ( 18.49999999999999645, 5.699452464332751767, -87.95772604343019907 ) ) ;
#186894 = EDGE_CURVE ( 'NONE', #169135, #136780, #111128, .T. ) ;
#186895 = EDGE_CURVE ( 'NONE', #65489, #245081, #256418, .T. ) ;
#186896 = CIRCLE ( 'NONE', #203620, 0.09999999999999939493 ) ;
#186897 = VERTEX_POINT ( 'NONE', #159985 ) ;
#186898 = VECTOR ( 'NONE', #136912, 1000.000000000000000 ) ;
#186899 = ORIENTED_EDGE ( 'NONE', *, *, #165227, .F. ) ;
#186900 = VERTEX_POINT ( 'NONE', #137805 ) ;
#186901 = EDGE_CURVE ( 'NONE', #38568, #159861, #2965, .T. ) ;
#186902 = CARTESIAN_POINT ( 'NONE',  ( 20.97250901189795513, 65.37543196631001763, -95.35856176755739000 ) ) ;
#186903 = DIRECTION ( 'NONE',  ( 0.000000000000000000, 0.8814952561688438326, -0.4721928772777331251 ) ) ;
#186904 = EDGE_LOOP ( 'NONE', ( #30581, #81716, #62998, #58069 ) ) ;
#186905 = EDGE_CURVE ( 'NONE', #220964, #115079, #123798, .T. ) ;
#186906 = AXIS2_PLACEMENT_3D ( 'NONE', #65622, #61777, #141316 ) ;
#186907 = VECTOR ( 'NONE', #247567, 1000.000000000000000 ) ;
#186908 = EDGE_CURVE ( 'NONE', #194263, #242169, #102919, .T. ) ;
#186909 = EDGE_LOOP ( 'NONE', ( #17413, #148509, #39504, #188681 ) ) ;
#186910 = SHAPE_REPRESENTATION_RELATIONSHIP ( 'NONE' , 'NONE' ,  #196772, #88633 ) ;
#186911 = EDGE_CURVE ( 'NONE', #8100, #156872, #17867, .T. ) ;
#186912 = ORIENTED_EDGE ( 'NONE', *, *, #189145, .F. ) ;
#186913 = DIRECTION ( 'NONE',  ( 1.000000000000000000, 0.000000000000000000, 0.000000000000000000 ) ) ;
#186914 = ORIENTED_EDGE ( 'NONE', *, *, #213966, .F. ) ;
#186916 = DIRECTION ( 'NONE',  ( 0.000000000000000000, -1.000000000000000000, 0.000000000000000000 ) ) ;
#186915 = TOROIDAL_SURFACE ( 'NONE', #145175, 4.099999999999999645, 0.1000000000000000056 ) ;
#186917 = CARTESIAN_POINT ( 'NONE',  ( -16.93826681692523195, 30.31948095044558045, -234.7979706876368766 ) ) ;
#186918 = VECTOR ( 'NONE', #105771, 1000.000000000000000 ) ;
#186919 = CIRCLE ( 'NONE', #78720, 11.80000000000000426 ) ;
#186920 = CARTESIAN_POINT ( 'NONE',  ( 20.73486653747088582, 7.250000000011182166, -154.8500000000000227 ) ) ;
#186921 = CARTESIAN_POINT ( 'NONE',  ( -21.05000000000000071, 1.115600667400684642E-11, -88.80000000000003979 ) ) ;
#186922 = VECTOR ( 'NONE', #45702, 1000.000000000000114 ) ;
#186923 = DIRECTION ( 'NONE',  ( 1.000000000000000000, -0.000000000000000000, -0.000000000000000000 ) ) ;
#186924 = CARTESIAN_POINT ( 'NONE',  ( -23.15000000000000213, 64.35000000001187459, -90.77310748452440237 ) ) ;
#186926 = EDGE_LOOP ( 'NONE', ( #154985, #85025, #67757, #124620 ) ) ;
#186925 = CARTESIAN_POINT ( 'NONE',  ( 20.95512828230157965, 44.16605519446306261, -236.4619169603685123 ) ) ;
#186928 = CARTESIAN_POINT ( 'NONE',  ( 22.39999999999999503, 56.01362831242965967, -232.7091905853083347 ) ) ;
#186927 = CARTESIAN_POINT ( 'NONE',  ( 20.94999999999999929, 11.63687328910416952, -26.67824078667522159 ) ) ;
#186929 = EDGE_CURVE ( 'NONE', #99499, #54789, #205466, .T. ) ;
#186930 = VECTOR ( 'NONE', #6894, 1000.000000000000000 ) ;
#186931 = FACE_OUTER_BOUND ( 'NONE', #126636, .T. ) ;
#186932 = ORIENTED_EDGE ( 'NONE', *, *, #31641, .F. ) ;
#186933 = DIRECTION ( 'NONE',  ( 1.000000000000000000, 0.000000000000000000, -0.000000000000000000 ) ) ;
#186934 = CARTESIAN_POINT ( 'NONE',  ( -14.56556274378147897, 9.446557523083686903, -115.5899419543459175 ) ) ;
#186935 = DIRECTION ( 'NONE',  ( 0.000000000000000000, 0.000000000000000000, -1.000000000000000000 ) ) ;
#186936 = ORIENTED_EDGE ( 'NONE', *, *, #72089, .F. ) ;
#186937 = DIRECTION ( 'NONE',  ( -1.000000000000000000, 0.000000000000000000, 0.000000000000000000 ) ) ;
#186938 = CARTESIAN_POINT ( 'NONE',  ( -16.82542659449974565, 66.06550010858438782, -82.26774308455044604 ) ) ;
#186939 = AXIS2_PLACEMENT_3D ( 'NONE', #153142, #71017, #173996 ) ;
#186941 = ORIENTED_EDGE ( 'NONE', *, *, #128877, .T. ) ;
#186940 = AXIS2_PLACEMENT_3D ( 'NONE', #241157, #82030, #25955 ) ;
#186942 = CARTESIAN_POINT ( 'NONE',  ( -23.25000000000000000, 70.57516910782925379, -223.5255282078080654 ) ) ;
#186943 = DIRECTION ( 'NONE',  ( 0.000000000000000000, 1.000000000000000000, -0.000000000000000000 ) ) ;
#186944 = CARTESIAN_POINT ( 'NONE',  ( -18.69999999999999929, -11.65000000000000036, 0.000000000000000000 ) ) ;
#186945 = CARTESIAN_POINT ( 'NONE',  ( 20.94999999999999574, 76.00000000001213607, -136.5231074845242745 ) ) ;
#186946 = EDGE_LOOP ( 'NONE', ( #159004, #107260, #187672, #2305 ) ) ;
#186947 = EDGE_LOOP ( 'NONE', ( #155304, #132630, #2502, #67615 ) ) ;
#186948 = AXIS2_PLACEMENT_3D ( 'NONE', #74055, #255161, #252640 ) ;
#186949 = VECTOR ( 'NONE', #115875, 1000.000000000000000 ) ;
#186950 = CYLINDRICAL_SURFACE ( 'NONE', #231773, 0.1000000000000028644 ) ;
#186951 = CARTESIAN_POINT ( 'NONE',  ( 22.39999999999999503, 11.75000000001116263, -67.10000000000005116 ) ) ;
#186952 = EDGE_CURVE ( 'NONE', #87569, #201070, #231958, .T. ) ;
#186953 = CARTESIAN_POINT ( 'NONE',  ( 18.59999999999996945, 43.35377423437995503, -245.1717807829448930 ) ) ;
#186954 = DIRECTION ( 'NONE',  ( 1.000000000000000000, 0.000000000000000000, 0.000000000000000000 ) ) ;
#186955 = AXIS2_PLACEMENT_3D ( 'NONE', #140780, #204592, #23434 ) ;
#186956 = EDGE_CURVE ( 'NONE', #22197, #5980, #138652, .T. ) ;
#186957 = CARTESIAN_POINT ( 'NONE',  ( 14.22916352759893144, 9.457410930301314522, -51.99991590874626723 ) ) ;
#186958 = DIRECTION ( 'NONE',  ( 0.000000000000000000, 1.000000000000000000, 0.000000000000000000 ) ) ;
#186959 = EDGE_LOOP ( 'NONE', ( #84094, #226406, #25161, #189921 ) ) ;
#186960 = FACE_BOUND ( 'NONE', #25186, .T. ) ;
#186961 = AXIS2_PLACEMENT_3D ( 'NONE', #183028, #146431, #224690 ) ;
#186963 = ORIENTED_EDGE ( 'NONE', *, *, #229436, .F. ) ;
#186962 = CARTESIAN_POINT ( 'NONE',  ( 23.14999999999999858, 30.43677443282724937, -239.5249545687858870 ) ) ;
#186964 = FACE_OUTER_BOUND ( 'NONE', #182649, .T. ) ;
#186965 = CARTESIAN_POINT ( 'NONE',  ( -16.80070461187855457, 66.05000000001085425, -90.37614365536641969 ) ) ;
#186966 = CARTESIAN_POINT ( 'NONE',  ( -15.55912972643741199, 8.490870273573719373, -113.1500000000000341 ) ) ;
#186967 = CARTESIAN_POINT ( 'NONE',  ( -16.97683809663752186, 66.05000000001207638, -123.1207434663278804 ) ) ;
#186968 = EDGE_CURVE ( 'NONE', #196244, #104087, #256821, .T. ) ;
#186969 = ADVANCED_FACE ( 'NONE', ( #180815 ), #73764, .T. ) ;
#186971 = ORIENTED_EDGE ( 'NONE', *, *, #105891, .F. ) ;
#186970 = DIRECTION ( 'NONE',  ( 0.000000000000000000, -0.2605042016806740079, 0.9654727137038698892 ) ) ;
#186972 = CARTESIAN_POINT ( 'NONE',  ( -18.79999999999999716, -10.84999999999999076, 32.89999999999999858 ) ) ;
#186973 = CARTESIAN_POINT ( 'NONE',  ( 21.09696443733127325, 10.72400988392963228, -179.7347775270482089 ) ) ;
#186974 = DIRECTION ( 'NONE',  ( 1.000000000000000000, 0.000000000000000000, 0.000000000000000000 ) ) ;
#186975 = CARTESIAN_POINT ( 'NONE',  ( 18.49999999999996803, 68.92903212821303782, -99.27654326265604823 ) ) ;
#186976 = EDGE_LOOP ( 'NONE', ( #133964, #203461, #238718, #160698 ) ) ;
#186977 = PLANE ( 'NONE',  #5588 ) ;
#186978 = CARTESIAN_POINT ( 'NONE',  ( -16.87998658237740912, 66.05000000001201954, -115.8867470522623080 ) ) ;
#186979 = CIRCLE ( 'NONE', #211902, 12.97499999999999964 ) ;
#186980 = AXIS2_PLACEMENT_3D ( 'NONE', #139429, #221526, #238548 ) ;
#186981 = CARTESIAN_POINT ( 'NONE',  ( 20.85000000000000142, 18.51199663233068193, -231.2535697180530292 ) ) ;
#186982 = AXIS2_PLACEMENT_3D ( 'NONE', #56522, #53981, #156963 ) ;
#186983 = DIRECTION ( 'NONE',  ( -1.000000000000000000, -0.000000000000000000, -0.000000000000000000 ) ) ;
#186984 = ORIENTED_EDGE ( 'NONE', *, *, #232260, .F. ) ;
#186985 = CARTESIAN_POINT ( 'NONE',  ( 23.14999999999999858, 74.06973020765583726, -202.9996014876918480 ) ) ;
#186986 = ORIENTED_EDGE ( 'NONE', *, *, #50165, .F. ) ;
#186987 = DIRECTION ( 'NONE',  ( 1.000000000000000000, 4.758098676964952635E-14, 0.000000000000000000 ) ) ;
#186988 = CARTESIAN_POINT ( 'NONE',  ( -20.54999999999999716, 1.115600667400684642E-11, -67.00000000000004263 ) ) ;
#186989 = SURFACE_STYLE_USAGE ( .BOTH. , #164838 ) ;
#186990 = DIRECTION ( 'NONE',  ( 0.000000000000000000, -1.000000000000000000, 0.000000000000000000 ) ) ;
#186991 = VERTEX_POINT ( 'NONE', #243337 ) ;
#186992 = CARTESIAN_POINT ( 'NONE',  ( -20.64999999999999858, 85.00000000001223555, -145.9170766071767389 ) ) ;
#186993 = DIRECTION ( 'NONE',  ( 1.000000000000000000, 0.000000000000000000, 0.000000000000000000 ) ) ;
#186994 = DIRECTION ( 'NONE',  ( 1.000000000000000000, 0.000000000000000000, 0.000000000000000000 ) ) ;
#186995 = DIRECTION ( 'NONE',  ( 0.000000000000000000, 0.000000000000000000, -1.000000000000000000 ) ) ;
#186996 = EDGE_CURVE ( 'NONE', #94420, #168199, #165291, .T. ) ;
#186997 = CARTESIAN_POINT ( 'NONE',  ( -21.14999999999999858, 1.115600667400684642E-11, -60.74142135623734617 ) ) ;
#186998 = ORIENTED_EDGE ( 'NONE', *, *, #1682, .F. ) ;
#187000 = VERTEX_POINT ( 'NONE', #103808 ) ;
#186999 = CARTESIAN_POINT ( 'NONE',  ( 20.94999027547553894, 10.29326151435327219, -105.9592822510415431 ) ) ;
#187001 = ORIENTED_EDGE ( 'NONE', *, *, #210862, .T. ) ;
#187002 = DIRECTION ( 'NONE',  ( 0.000000000000000000, 0.7049548389605068133, -0.7092521942342976393 ) ) ;
#187003 = ORIENTED_EDGE ( 'NONE', *, *, #192235, .F. ) ;
#187004 = DIRECTION ( 'NONE',  ( 0.000000000000000000, -1.000000000000000000, 0.000000000000000000 ) ) ;
#187005 = CARTESIAN_POINT ( 'NONE',  ( -18.34374000495059676, 11.47316190337362940, -124.7500000000000426 ) ) ;
#187006 = CYLINDRICAL_SURFACE ( 'NONE', #41442, 0.09999999999999939493 ) ;
#187007 = ORIENTED_EDGE ( 'NONE', *, *, #43470, .T. ) ;
#187008 = CARTESIAN_POINT ( 'NONE',  ( 21.05000000000000071, 67.54115598404673904, -214.0823964242964053 ) ) ;
#187009 = DIRECTION ( 'NONE',  ( 0.000000000000000000, -0.8814952561687088295, 0.4721928772779852013 ) ) ;
#187010 = CARTESIAN_POINT ( 'NONE',  ( 18.43709777086141344, -9.682403433465239573, -140.6568433774128550 ) ) ;
#187011 = EDGE_CURVE ( 'NONE', #191399, #166555, #182098, .T. ) ;
#187012 = ORIENTED_EDGE ( 'NONE', *, *, #55574, .F. ) ;
#187013 = DIRECTION ( 'NONE',  ( -0.000000000000000000, 1.000000000000000000, 6.982962677686266711E-15 ) ) ;
#187015 = ORIENTED_EDGE ( 'NONE', *, *, #238893, .T. ) ;
#187014 = CARTESIAN_POINT ( 'NONE',  ( 18.59999999999999787, 84.35952707724818822, -212.2592855339655671 ) ) ;
#187017 = EDGE_CURVE ( 'NONE', #127664, #37720, #244619, .T. ) ;
#187016 = DIRECTION ( 'NONE',  ( 0.000000000000000000, 0.000000000000000000, 1.000000000000000000 ) ) ;
#187018 = DIRECTION ( 'NONE',  ( 0.000000000000000000, -7.304098846218085561E-15, 1.000000000000000000 ) ) ;
#187019 = CONICAL_SURFACE ( 'NONE', #137101, 4.299999999999970512, 0.7853981633974466137 ) ;
#187020 = AXIS2_PLACEMENT_3D ( 'NONE', #56278, #36775, #255734 ) ;
#187021 = VECTOR ( 'NONE', #132766, 1000.000000000000000 ) ;
#187022 = AXIS2_PLACEMENT_3D ( 'NONE', #66599, #122736, #142270 ) ;
#187023 = ORIENTED_EDGE ( 'NONE', *, *, #29729, .T. ) ;
#187024 = CARTESIAN_POINT ( 'NONE',  ( 23.14999999999999858, 0.000000000000000000, -33.50000000000000000 ) ) ;
#187026 = EDGE_CURVE ( 'NONE', #239159, #161742, #119526, .T. ) ;
#187025 = FACE_OUTER_BOUND ( 'NONE', #231775, .T. ) ;
#187027 = AXIS2_PLACEMENT_3D ( 'NONE', #118930, #98029, #198444 ) ;
#187028 = DIRECTION ( 'NONE',  ( 0.000000000000000000, -0.2617529984165036239, -0.9651348961777156399 ) ) ;
#187029 = EDGE_LOOP ( 'NONE', ( #112306, #197692, #87957, #72280 ) ) ;
#187030 = CARTESIAN_POINT ( 'NONE',  ( -18.50000000000000000, 6.266619843005246437, -211.3861694115776402 ) ) ;
#187031 = ADVANCED_FACE ( 'NONE', ( #3435 ), #172028, .F. ) ;
#187032 = CARTESIAN_POINT ( 'NONE',  ( 18.39999999999999503, 31.17298305880675002, -240.2029303890703886 ) ) ;
#187033 = EDGE_CURVE ( 'NONE', #97608, #256235, #156944, .T. ) ;
#187034 = VERTEX_POINT ( 'NONE', #6001 ) ;
#187035 = VECTOR ( 'NONE', #187443, 1000.000000000000000 ) ;
#187036 = CIRCLE ( 'NONE', #82915, 0.5000000000000022204 ) ;
#187037 = TOROIDAL_SURFACE ( 'NONE', #124481, 12.77499999999999858, 0.1000000000000000056 ) ;
#187038 = EDGE_CURVE ( 'NONE', #36016, #168895, #44512, .T. ) ;
#187039 = VECTOR ( 'NONE', #168630, 1000.000000000000000 ) ;
#187040 = ORIENTED_EDGE ( 'NONE', *, *, #213032, .T. ) ;
#187041 = DIRECTION ( 'NONE',  ( 0.000000000000000000, 0.000000000000000000, 1.000000000000000000 ) ) ;
#187042 = EDGE_LOOP ( 'NONE', ( #246145, #51683, #1708, #145914 ) ) ;
#187043 = CARTESIAN_POINT ( 'NONE',  ( -18.40000000000000213, 8.822561741666397950, -24.25000000000000000 ) ) ;
#187045 = ADVANCED_FACE ( 'NONE', ( #185937 ), #123402, .F. ) ;
#187044 = CARTESIAN_POINT ( 'NONE',  ( -16.89155683852770551, 66.05000000001524540, -183.3004793340630556 ) ) ;
#187047 = ORIENTED_EDGE ( 'NONE', *, *, #145094, .T. ) ;
#187046 = CARTESIAN_POINT ( 'NONE',  ( 13.54556439290364267, 24.86329420051411532, -232.5114740807002818 ) ) ;
#187048 = CARTESIAN_POINT ( 'NONE',  ( 18.59999999999999787, 1.115600667400684642E-11, -167.4999999999999716 ) ) ;
#187049 = LINE ( 'NONE', #47487, #203139 ) ;
#187050 = CARTESIAN_POINT ( 'NONE',  ( -20.94999999999999929, 67.23127455305835554, -235.8551265064784559 ) ) ;
#187051 = DIRECTION ( 'NONE',  ( 0.000000000000000000, 0.000000000000000000, 1.000000000000000000 ) ) ;
#187052 = DIRECTION ( 'NONE',  ( 0.7071067811865474617, 0.7071067811865474617, 0.000000000000000000 ) ) ;
#187053 = DIRECTION ( 'NONE',  ( 0.000000000000000000, 0.2128009952263604232, -0.9770955615653316162 ) ) ;
#187054 = CARTESIAN_POINT ( 'NONE',  ( -18.40000000000000213, -9.519327731081286714, -107.4729763765593589 ) ) ;
#187056 = ORIENTED_EDGE ( 'NONE', *, *, #18803, .T. ) ;
#187055 = CARTESIAN_POINT ( 'NONE',  ( -22.48479450179659977, 75.95300841882514931, -114.6731059307759324 ) ) ;
#187057 = DIRECTION ( 'NONE',  ( 0.000000000000000000, 0.000000000000000000, -1.000000000000000000 ) ) ;
#187058 = ORIENTED_EDGE ( 'NONE', *, *, #169348, .T. ) ;
#187059 = AXIS2_PLACEMENT_3D ( 'NONE', #198008, #136748, #200585 ) ;
#187060 = CIRCLE ( 'NONE', #141246, 0.09999999999999939493 ) ;
#187061 = CARTESIAN_POINT ( 'NONE',  ( 18.49999999999999289, 68.87972903831429505, -99.36354444268502561 ) ) ;
#187062 = DIRECTION ( 'NONE',  ( 1.000000000000000000, 2.952720810173289112E-16, -0.000000000000000000 ) ) ;
#187063 = AXIS2_PLACEMENT_3D ( 'NONE', #231745, #115635, #248734 ) ;
#187064 = CYLINDRICAL_SURFACE ( 'NONE', #69811, 4.049999999999998046 ) ;
#187065 = ORIENTED_EDGE ( 'NONE', *, *, #235109, .F. ) ;
#187066 = LINE ( 'NONE', #167505, #94049 ) ;
#187067 = FACE_OUTER_BOUND ( 'NONE', #28790, .T. ) ;
#187068 = CIRCLE ( 'NONE', #141261, 0.09999999999999939493 ) ;
#187069 = ORIENTED_EDGE ( 'NONE', *, *, #256992, .F. ) ;
#187071 = EDGE_CURVE ( 'NONE', #29061, #184680, #140338, .T. ) ;
#187070 = CARTESIAN_POINT ( 'NONE',  ( 21.05000000000000071, 75.90220970870350925, -209.7809220950058773 ) ) ;
#187072 = AXIS2_PLACEMENT_3D ( 'NONE', #179003, #141130, #21205 ) ;
#187073 = DIRECTION ( 'NONE',  ( 1.000000000000000000, -0.000000000000000000, -0.000000000000000000 ) ) ;
#187074 = ORIENTED_EDGE ( 'NONE', *, *, #137908, .F. ) ;
#187075 = CYLINDRICAL_SURFACE ( 'NONE', #40255, 0.09999999999998898659 ) ;
#187076 = VERTEX_POINT ( 'NONE', #204209 ) ;
#187078 = ADVANCED_FACE ( 'NONE', ( #7295 ), #166410, .T. ) ;
#187077 = CARTESIAN_POINT ( 'NONE',  ( -15.39946565075090135, 9.389534562357855663, -49.17480930438996722 ) ) ;
#187079 = ORIENTED_EDGE ( 'NONE', *, *, #33485, .T. ) ;
#187080 = VECTOR ( 'NONE', #198420, 1000.000000000000000 ) ;
#187081 = DIRECTION ( 'NONE',  ( -1.000000000000000000, 0.000000000000000000, 0.000000000000000000 ) ) ;
#187082 = EDGE_CURVE ( 'NONE', #93827, #197206, #176522, .T. ) ;
#187083 = CARTESIAN_POINT ( 'NONE',  ( 21.00000000000000000, 9.749999999999998224, -21.15000000000000213 ) ) ;
#187084 = ADVANCED_FACE ( 'NONE', ( #257269 ), #22581, .F. ) ;
#187085 = ORIENTED_EDGE ( 'NONE', *, *, #507, .F. ) ;
#187086 = VERTEX_POINT ( 'NONE', #78669 ) ;
#187087 = FACE_OUTER_BOUND ( 'NONE', #7712, .T. ) ;
#187089 = ORIENTED_EDGE ( 'NONE', *, *, #95041, .F. ) ;
#187088 = CARTESIAN_POINT ( 'NONE',  ( 14.11444803880196552, 9.457431528860066550, -48.49991693789966263 ) ) ;
#187090 = CARTESIAN_POINT ( 'NONE',  ( 21.72449340488910252, 10.28395627750227526, -42.75000000000000000 ) ) ;
#187091 = ORIENTED_EDGE ( 'NONE', *, *, #148750, .T. ) ;
#187092 = AXIS2_PLACEMENT_3D ( 'NONE', #209967, #91296, #230822 ) ;
#187093 = CIRCLE ( 'NONE', #3725, 2.100000000000004530 ) ;
#187094 = AXIS2_PLACEMENT_3D ( 'NONE', #127526, #167965, #52775 ) ;
#187095 = AXIS2_PLACEMENT_3D ( 'NONE', #143202, #41575, #27155 ) ;
#187096 = EDGE_LOOP ( 'NONE', ( #127833, #251211, #127160, #121719 ) ) ;
#187097 = EDGE_CURVE ( 'NONE', #143423, #149669, #57818, .T. ) ;
#187099 = AXIS2_PLACEMENT_3D ( 'NONE', #163, #126209, #205749 ) ;
#187098 = DIRECTION ( 'NONE',  ( 1.000000000000000000, 0.000000000000000000, 0.000000000000000000 ) ) ;
#187100 = CYLINDRICAL_SURFACE ( 'NONE', #55361, 2.600000000000000089 ) ;
#187101 = PLANE ( 'NONE',  #24576 ) ;
#187102 = ADVANCED_FACE ( 'NONE', ( #120422 ), #199941, .T. ) ;
#187103 = DIRECTION ( 'NONE',  ( 0.000000000000000000, -8.326672684688666480E-14, 1.000000000000000000 ) ) ;
#187104 = DIRECTION ( 'NONE',  ( 1.000000000000000000, 0.000000000000000000, 0.000000000000000000 ) ) ;
#187105 = FACE_OUTER_BOUND ( 'NONE', #27269, .T. ) ;
#187106 = ORIENTED_EDGE ( 'NONE', *, *, #238272, .F. ) ;
#187107 = CARTESIAN_POINT ( 'NONE',  ( -16.94165728009536664, 66.01213024408876606, -182.6320524760142234 ) ) ;
#187108 = CARTESIAN_POINT ( 'NONE',  ( 21.05000000000000071, 1.162701749949165642, -142.1000000000000227 ) ) ;
#187110 = DIRECTION ( 'NONE',  ( 1.000000000000000000, 0.000000000000000000, 0.000000000000000000 ) ) ;
#187109 = PRODUCT_RELATED_PRODUCT_CATEGORY ( 'part', '', ( #170204 ) ) ;
#187111 = DIRECTION ( 'NONE',  ( -0.000000000000000000, 0.9969158384938637818, -0.07847809223010315804 ) ) ;
#187112 = ORIENTED_EDGE ( 'NONE', *, *, #179376, .F. ) ;
#187113 = CARTESIAN_POINT ( 'NONE',  ( 18.52643265882457868, 10.31973158071402885, -106.0505334713354983 ) ) ;
#187114 = ORIENTED_EDGE ( 'NONE', *, *, #18803, .F. ) ;
#187116 = AXIS2_PLACEMENT_3D ( 'NONE', #235366, #60576, #198813 ) ;
#187115 = SPHERICAL_SURFACE ( 'NONE', #248143, 0.1000000000000000056 ) ;
#187117 = ORIENTED_EDGE ( 'NONE', *, *, #171061, .F. ) ;
#187118 = CARTESIAN_POINT ( 'NONE',  ( 20.94999999999999929, 5.500000000011153745, -121.5947339810869465 ) ) ;
#187119 = CARTESIAN_POINT ( 'NONE',  ( -20.54999999999999716, 4.350000000011156054, -88.15000000000004832 ) ) ;
#187120 = ADVANCED_FACE ( 'NONE', ( #39600 ), #227133, .F. ) ;
#187121 = ORIENTED_EDGE ( 'NONE', *, *, #149078, .F. ) ;
#187122 = EDGE_LOOP ( 'NONE', ( #226123, #53032, #137367 ) ) ;
#187124 = VERTEX_POINT ( 'NONE', #159524 ) ;
#187123 = CARTESIAN_POINT ( 'NONE',  ( -21.05000000000000071, 1.835341550235567887, -145.5551512925629822 ) ) ;
#187125 = EDGE_CURVE ( 'NONE', #217763, #21148, #27267, .T. ) ;
#187126 = FACE_OUTER_BOUND ( 'NONE', #124087, .T. ) ;
#187127 = EDGE_LOOP ( 'NONE', ( #110045, #190556, #6468, #231828 ) ) ;
#187128 = EDGE_CURVE ( 'NONE', #220166, #184365, #218744, .T. ) ;
#187129 = CARTESIAN_POINT ( 'NONE',  ( -22.50000000000000000, 0.1000000000111554016, -21.85042919245520210 ) ) ;
#187130 = DIRECTION ( 'NONE',  ( -1.000000000000000000, 0.000000000000000000, 0.000000000000000000 ) ) ;
#187131 = AXIS2_PLACEMENT_3D ( 'NONE', #61311, #198244, #19626 ) ;
#187132 = ORIENTED_EDGE ( 'NONE', *, *, #242989, .T. ) ;
#187133 = DIRECTION ( 'NONE',  ( 0.000000000000000000, -1.000000000000000000, -6.982962677686265922E-15 ) ) ;
#187134 = ADVANCED_FACE ( 'NONE', ( #59082 ), #138625, .T. ) ;
#187135 = CARTESIAN_POINT ( 'NONE',  ( -20.85000000000000142, 87.65000000001214175, -136.5231074845242745 ) ) ;
#187136 = ORIENTED_EDGE ( 'NONE', *, *, #40547, .F. ) ;
#187137 = AXIS2_PLACEMENT_3D ( 'NONE', #254516, #176318, #155487 ) ;
#187138 = LINE ( 'NONE', #86701, #97256 ) ;
#187139 = DIRECTION ( 'NONE',  ( 1.000000000000000000, -0.000000000000000000, 0.000000000000000000 ) ) ;
#187140 = FACE_OUTER_BOUND ( 'NONE', #116258, .T. ) ;
#187142 = ORIENTED_EDGE ( 'NONE', *, *, #153015, .F. ) ;
#187141 = CARTESIAN_POINT ( 'NONE',  ( -23.25000000000000000, 87.65000000001165859, -69.52310748452424605 ) ) ;
#187143 = DIRECTION ( 'NONE',  ( 0.000000000000000000, 1.000000000000000000, 6.938893903907222067E-15 ) ) ;
#187144 = AXIS2_PLACEMENT_3D ( 'NONE', #38776, #195306, #37501 ) ;
#187145 = DIRECTION ( 'NONE',  ( 0.000000000000000000, -6.982962677686266711E-15, 1.000000000000000000 ) ) ;
#187147 = EDGE_CURVE ( 'NONE', #155798, #169470, #99504, .T. ) ;
#187146 = FACE_OUTER_BOUND ( 'NONE', #169586, .T. ) ;
#187148 = VECTOR ( 'NONE', #240029, 1000.000000000000000 ) ;
#187150 = LINE ( 'NONE', #245821, #107593 ) ;
#187149 = DIRECTION ( 'NONE',  ( -1.000000000000000000, 0.000000000000000000, 0.000000000000000000 ) ) ;
#187151 = CARTESIAN_POINT ( 'NONE',  ( -20.94983749550516450, 65.70233904877071041, -164.5487410911968595 ) ) ;
#187152 = LINE ( 'NONE', #166320, #81733 ) ;
#187153 = CARTESIAN_POINT ( 'NONE',  ( -20.85000000000000142, -11.64999999998884483, -200.9999999999999432 ) ) ;
#187154 = CARTESIAN_POINT ( 'NONE',  ( 20.94999999999999574, -10.76604040606816959, -206.3127087229280789 ) ) ;
#187155 = VECTOR ( 'NONE', #8094, 1000.000000000000000 ) ;
#187156 = VERTEX_POINT ( 'NONE', #119107 ) ;
#187157 = VERTEX_POINT ( 'NONE', #82507 ) ;
#187158 = EDGE_CURVE ( 'NONE', #12028, #38227, #219465, .T. ) ;
#187159 = EDGE_LOOP ( 'NONE', ( #236699, #22325, #241843, #45220, #99054 ) ) ;
#187160 = LINE ( 'NONE', #166329, #156797 ) ;
#187161 = ADVANCED_FACE ( 'NONE', ( #98206 ), #222022, .F. ) ;
#187162 = LINE ( 'NONE', #100195, #127684 ) ;
#187163 = ORIENTED_EDGE ( 'NONE', *, *, #234884, .F. ) ;
#187164 =( NAMED_UNIT ( * ) SI_UNIT ( $, .STERADIAN. ) SOLID_ANGLE_UNIT ( ) );
#187165 = DIRECTION ( 'NONE',  ( 1.000000000000000000, -7.930164461608253340E-15, 0.000000000000000000 ) ) ;
#187167 = DIRECTION ( 'NONE',  ( 0.000000000000000000, 1.000000000000000000, 6.982962677686266711E-15 ) ) ;
#187166 = AXIS2_PLACEMENT_3D ( 'NONE', #35024, #153708, #188926 ) ;
#187168 = LINE ( 'NONE', #8514, #246392 ) ;
#187169 = VERTEX_POINT ( 'NONE', #17425 ) ;
#187170 = ORIENTED_EDGE ( 'NONE', *, *, #154120, .F. ) ;
#187171 = EDGE_CURVE ( 'NONE', #9313, #67371, #148031, .T. ) ;
#187172 = DIRECTION ( 'NONE',  ( -1.000000000000000000, 0.000000000000000000, 0.000000000000000000 ) ) ;
#187173 = CARTESIAN_POINT ( 'NONE',  ( -23.15000000000000213, 2.500000000011154633, -154.2753780772379173 ) ) ;
#187175 = EDGE_CURVE ( 'NONE', #61112, #128191, #139631, .T. ) ;
#187174 = ORIENTED_EDGE ( 'NONE', *, *, #228054, .F. ) ;
#187176 = CARTESIAN_POINT ( 'NONE',  ( -21.05000000000000071, 1.749999999999999778, -11.66951155790164307 ) ) ;
#187178 = ORIENTED_EDGE ( 'NONE', *, *, #108515, .T. ) ;
#187177 = CARTESIAN_POINT ( 'NONE',  ( -18.39999999999999858, 85.50000000001186606, -96.42291809330220076 ) ) ;
#187179 = CARTESIAN_POINT ( 'NONE',  ( -5.899999999999938183, 64.75000000001119815, -36.02310748452479316 ) ) ;
#187180 = DIRECTION ( 'NONE',  ( 0.000000000000000000, -0.2617529984164856383, -0.9651348961777204138 ) ) ;
#187182 = VERTEX_POINT ( 'NONE', #1703 ) ;
#187181 = CARTESIAN_POINT ( 'NONE',  ( -18.59999999999999787, 68.97833521811159585, -65.88954208262707368 ) ) ;
#187183 = DIRECTION ( 'NONE',  ( 0.000000000000000000, -0.9893560106964500722, 0.1455152366551550613 ) ) ;
#187184 = FACE_OUTER_BOUND ( 'NONE', #35362, .T. ) ;
#187185 = AXIS2_PLACEMENT_3D ( 'NONE', #248534, #92024, #13779 ) ;
#187188 = LINE ( 'NONE', #151919, #141461 ) ;
#187187 = VECTOR ( 'NONE', #209950, 1000.000000000000000 ) ;
#187186 = DIRECTION ( 'NONE',  ( 0.000000000000000000, 6.769652589177795712E-15, -1.000000000000000000 ) ) ;
#187189 = DIRECTION ( 'NONE',  ( -0.000000000000000000, -1.000000000000000000, 6.308085367188393199E-16 ) ) ;
#187190 = AXIS2_PLACEMENT_3D ( 'NONE', #29223, #107426, #142681 ) ;
#187191 = AXIS2_PLACEMENT_3D ( 'NONE', #238499, #234651, #174732 ) ;
#187192 = DIRECTION ( 'NONE',  ( 2.952720810173289112E-16, -1.000000000000000000, -0.000000000000000000 ) ) ;
#187193 = DIRECTION ( 'NONE',  ( 0.000000000000000000, 0.2128009952263603677, -0.9770955615653313941 ) ) ;
#187194 = DIRECTION ( 'NONE',  ( 2.952720810173290098E-16, -0.4721928772777333472, -0.8814952561688437216 ) ) ;
#187195 = ADVANCED_FACE ( 'NONE', ( #197338 ), #252085, .T. ) ;
#187196 = EDGE_LOOP ( 'NONE', ( #152836, #41188, #213299, #21989, #207503, #120088 ) ) ;
#187197 = ORIENTED_EDGE ( 'NONE', *, *, #254331, .T. ) ;
#187198 = VERTEX_POINT ( 'NONE', #181653 ) ;
#187199 = DIRECTION ( 'NONE',  ( 0.000000000000000000, -0.2617529984164955192, -0.9651348961777178603 ) ) ;
#187200 = AXIS2_PLACEMENT_3D ( 'NONE', #193023, #75655, #57328 ) ;
#187201 = ORIENTED_EDGE ( 'NONE', *, *, #37815, .T. ) ;
#187202 = VERTEX_POINT ( 'NONE', #18713 ) ;
#187203 = EDGE_CURVE ( 'NONE', #77135, #221888, #156453, .T. ) ;
#187204 = FACE_OUTER_BOUND ( 'NONE', #45760, .T. ) ;
#187205 = CARTESIAN_POINT ( 'NONE',  ( -18.41431012584569515, 16.38972671430905947, -222.2727256927804262 ) ) ;
#187206 = AXIS2_PLACEMENT_3D ( 'NONE', #241951, #2043, #64592 ) ;
#187207 = EDGE_CURVE ( 'NONE', #47181, #24834, #235500, .T. ) ;
#187208 = ORIENTED_EDGE ( 'NONE', *, *, #64187, .T. ) ;
#187209 = VECTOR ( 'NONE', #209458, 1000.000000000000000 ) ;
#187210 = CARTESIAN_POINT ( 'NONE',  ( 12.68104795156995301, 9.396533993965077158, -151.9059397791733659 ) ) ;
#187211 = ADVANCED_FACE ( 'NONE', ( #23882 ), #97931, .F. ) ;
#187212 = ORIENTED_EDGE ( 'NONE', *, *, #52789, .T. ) ;
#187213 = AXIS2_PLACEMENT_3D ( 'NONE', #146416, #225941, #129448 ) ;
#187214 = ORIENTED_EDGE ( 'NONE', *, *, #214398, .F. ) ;
#187215 = ORIENTED_EDGE ( 'NONE', *, *, #3243, .T. ) ;
#187216 = FACE_OUTER_BOUND ( 'NONE', #61022, .T. ) ;
#187217 = DIRECTION ( 'NONE',  ( 0.000000000000000000, -5.551115123125777653E-14, 1.000000000000000000 ) ) ;
#187218 = FACE_OUTER_BOUND ( 'NONE', #140624, .T. ) ;
#187219 = CARTESIAN_POINT ( 'NONE',  ( -20.90000000000000213, -1.885425182446133885, -11.49641995933507843 ) ) ;
#187220 = FACE_OUTER_BOUND ( 'NONE', #29078, .T. ) ;
#187221 =( BOUNDED_CURVE ( )  B_SPLINE_CURVE ( 3, ( #135970, #134684, #211697, #214248 ),
 .UNSPECIFIED., .F., .F. ) 
 B_SPLINE_CURVE_WITH_KNOTS ( ( 4, 4 ),
 ( 3.752122642744585068, 4.712388980384675463 ),
 .UNSPECIFIED. ) 
 CURVE ( )  GEOMETRIC_REPRESENTATION_ITEM ( )  RATIONAL_B_SPLINE_CURVE ( ( 1.000000000000000000, 0.9246222802177217481, 0.9246222802177217481, 1.000000000000000000 ) ) 
 REPRESENTATION_ITEM ( '' )  );
#187223 = CARTESIAN_POINT ( 'NONE',  ( 18.54116936837188234, 85.46356419838508600, -196.4745649936360508 ) ) ;
#187222 = FACE_OUTER_BOUND ( 'NONE', #236327, .T. ) ;
#187224 = FACE_OUTER_BOUND ( 'NONE', #156680, .T. ) ;
#187226 = ORIENTED_EDGE ( 'NONE', *, *, #123019, .T. ) ;
#187225 = CARTESIAN_POINT ( 'NONE',  ( -20.92356734117541706, 10.31973158071402175, -139.5505334713354841 ) ) ;
#187228 = DIRECTION ( 'NONE',  ( -1.000000000000000000, 0.000000000000000000, -0.000000000000000000 ) ) ;
#187227 = CARTESIAN_POINT ( 'NONE',  ( -23.25000000000000000, 6.298909458711757559, -229.9220286223353185 ) ) ;
#187229 = EDGE_CURVE ( 'NONE', #196380, #50799, #5546, .T. ) ;
#187230 = LINE ( 'NONE', #64686, #186345 ) ;
#187231 = ADVANCED_FACE ( 'NONE', ( #225866 ), #123101, .T. ) ;
#187232 = EDGE_LOOP ( 'NONE', ( #94357, #237283, #145082, #69864 ) ) ;
#187233 = CARTESIAN_POINT ( 'NONE',  ( -23.25000000000000000, 76.00000000001237765, -170.0231074845243597 ) ) ;
#187234 = CARTESIAN_POINT ( 'NONE',  ( 22.49999999999999645, 64.35042919246716053, -103.1231074845243825 ) ) ;
#187235 = LINE ( 'NONE', #111528, #41518 ) ;
#187236 = ORIENTED_EDGE ( 'NONE', *, *, #82912, .F. ) ;
#187237 = LINE ( 'NONE', #32017, #228186 ) ;
#187238 = TOROIDAL_SURFACE ( 'NONE', #145510, 4.041421356237310469, 0.1000000000000000056 ) ;
#187239 = DIRECTION ( 'NONE',  ( 1.875376730785737719E-16, 1.000000000000000000, 6.982962677686266711E-15 ) ) ;
#187240 = CARTESIAN_POINT ( 'NONE',  ( -20.64999999999999858, 1.115600667400684642E-11, -67.00000000000000000 ) ) ;
#187241 = ORIENTED_EDGE ( 'NONE', *, *, #4499, .T. ) ;
#187242 = ORIENTED_EDGE ( 'NONE', *, *, #14809, .F. ) ;
#187243 = FACE_OUTER_BOUND ( 'NONE', #209462, .T. ) ;
#187244 = ORIENTED_EDGE ( 'NONE', *, *, #180201, .T. ) ;
#187245 = CARTESIAN_POINT ( 'NONE',  ( -17.22361732159832215, 10.34515565861359221, -178.8707845258671227 ) ) ;
#187246 = SPHERICAL_SURFACE ( 'NONE', #48986, 0.1000000000000000056 ) ;
#187247 = DIRECTION ( 'NONE',  ( 0.000000000000000000, 0.4721928772777343464, 0.8814952561688431665 ) ) ;
#187248 = ORIENTED_EDGE ( 'NONE', *, *, #116698, .T. ) ;
#187249 = CARTESIAN_POINT ( 'NONE',  ( -23.15000000000000213, -8.663551401858004652, -76.52410111806734960 ) ) ;
#187250 = DIRECTION ( 'NONE',  ( 0.000000000000000000, 0.000000000000000000, -1.000000000000000000 ) ) ;
#187251 = CARTESIAN_POINT ( 'NONE',  ( -23.15000000000000213, 74.00000000001229239, -157.2984855617622770 ) ) ;
#187252 = DIRECTION ( 'NONE',  ( -2.952720810173288619E-16, 1.000000000000000000, 0.000000000000000000 ) ) ;
#187253 = VECTOR ( 'NONE', #19565, 1000.000000000000000 ) ;
#187254 = EDGE_CURVE ( 'NONE', #49118, #11462, #207644, .T. ) ;
#187255 = ORIENTED_EDGE ( 'NONE', *, *, #146937, .F. ) ;
#187257 = CARTESIAN_POINT ( 'NONE',  ( 20.93975676684922504, 10.31104185822947450, -39.02045169831057336 ) ) ;
#187256 = AXIS2_PLACEMENT_3D ( 'NONE', #185379, #246625, #167136 ) ;
#187259 = VERTEX_POINT ( 'NONE', #223316 ) ;
#187258 = DIRECTION ( 'NONE',  ( -1.000000000000000000, -0.000000000000000000, -0.000000000000000000 ) ) ;
#187260 = CARTESIAN_POINT ( 'NONE',  ( 18.50000000000000000, -9.499999999988842703, -174.1001893912220737 ) ) ;
#187261 = CARTESIAN_POINT ( 'NONE',  ( 22.60000000000000142, 75.89914163091332000, -114.7726746080137019 ) ) ;
#187262 = CIRCLE ( 'NONE', #254417, 0.09999999999999939493 ) ;
#187263 = DIRECTION ( 'NONE',  ( 1.000000000000000000, 0.000000000000000000, 0.000000000000000000 ) ) ;
#187264 = FACE_OUTER_BOUND ( 'NONE', #105896, .T. ) ;
#187265 = CARTESIAN_POINT ( 'NONE',  ( 21.05000000000000071, 8.776282889868772585, -12.17621514106822467 ) ) ;
#187266 = VECTOR ( 'NONE', #18198, 1000.000000000000114 ) ;
#187267 = CARTESIAN_POINT ( 'NONE',  ( 20.94999999999999574, 87.48912529308769592, -66.42310748452423752 ) ) ;
#187268 = CARTESIAN_POINT ( 'NONE',  ( 20.04999999999999716, 11.24151875332161765, -211.4982501455723138 ) ) ;
#187269 = AXIS2_PLACEMENT_3D ( 'NONE', #230948, #66720, #88817 ) ;
#187270 = ORIENTED_EDGE ( 'NONE', *, *, #3190, .F. ) ;
#187271 = DIRECTION ( 'NONE',  ( 0.000000000000000000, 0.9770955615653313941, 0.2128009952263603677 ) ) ;
#187272 = CYLINDRICAL_SURFACE ( 'NONE', #6700, 0.09999999999999691080 ) ;
#187273 = DIRECTION ( 'NONE',  ( 0.000000000000000000, 0.9651348961777158619, -0.2617529984165031243 ) ) ;
#187274 = EDGE_CURVE ( 'NONE', #120029, #132925, #167247, .T. ) ;
#187275 = DIRECTION ( 'NONE',  ( -0.000000000000000000, -0.9910465087640860649, -0.1335171055202901413 ) ) ;
#187276 = CARTESIAN_POINT ( 'NONE',  ( -20.90000000000000213, -1.899104650876408451, -11.59795743183152972 ) ) ;
#187277 = VECTOR ( 'NONE', #14999, 1000.000000000000000 ) ;
#187278 = CIRCLE ( 'NONE', #120638, 0.09999999999999939493 ) ;
#187280 = VERTEX_POINT ( 'NONE', #168550 ) ;
#187279 = AXIS2_PLACEMENT_3D ( 'NONE', #177613, #75914, #155488 ) ;
#187281 = ORIENTED_EDGE ( 'NONE', *, *, #26092, .F. ) ;
#187282 = VECTOR ( 'NONE', #175628, 1000.000000000000000 ) ;
#187283 = TOROIDAL_SURFACE ( 'NONE', #228964, 0.2000000000000000111, 0.1000000000000000056 ) ;
#187284 = CARTESIAN_POINT ( 'NONE',  ( -18.79999999999999716, 5.488301202077013663, 16.40000000000000213 ) ) ;
#187285 = DIRECTION ( 'NONE',  ( 0.000000000000000000, 1.000000000000000000, 0.000000000000000000 ) ) ;
#187286 = CARTESIAN_POINT ( 'NONE',  ( 21.00000000000000000, 43.94346684630428967, -235.6041041703296344 ) ) ;
#187287 = AXIS2_PLACEMENT_3D ( 'NONE', #230457, #154800, #216008 ) ;
#187288 = CARTESIAN_POINT ( 'NONE',  ( 22.39999999999999858, -1.560176095955058129, -193.3663837337745122 ) ) ;
#187289 = CARTESIAN_POINT ( 'NONE',  ( -20.94999999999999929, 6.277629359189121239, -229.8243190661787878 ) ) ;
#187290 = CARTESIAN_POINT ( 'NONE',  ( 22.39999999999999503, 1.115600667400684642E-11, -59.20922040162666633 ) ) ;
#187291 = CARTESIAN_POINT ( 'NONE',  ( -16.91247567987037570, 9.959082683669246094, -12.62872445853733616 ) ) ;
#187292 = AXIS2_PLACEMENT_3D ( 'NONE', #97107, #98385, #256154 ) ;
#187293 = ORIENTED_EDGE ( 'NONE', *, *, #224821, .F. ) ;
#187294 = CARTESIAN_POINT ( 'NONE',  ( 21.05000000000000071, -8.730841121495320323, -23.90192528101566438 ) ) ;
#187295 = ORIENTED_EDGE ( 'NONE', *, *, #45535, .T. ) ;
#187296 = CARTESIAN_POINT ( 'NONE',  ( -23.15000000000000213, 1.115600667400684642E-11, -100.5000000000000426 ) ) ;
#187297 = FACE_OUTER_BOUND ( 'NONE', #97979, .T. ) ;
#187298 = DIRECTION ( 'NONE',  ( 0.000000000000000000, 2.168404344970946942E-15, 1.000000000000000000 ) ) ;
#187299 = CARTESIAN_POINT ( 'NONE',  ( 23.24999999999999645, 8.822561741677553471, -154.8500000000000227 ) ) ;
#187300 = CARTESIAN_POINT ( 'NONE',  ( 18.54999999999999716, 66.05000000001260219, -190.8731074845244962 ) ) ;
#187301 = DIRECTION ( 'NONE',  ( -0.000000000000000000, 1.000000000000000000, -0.000000000000000000 ) ) ;
#187302 = CARTESIAN_POINT ( 'NONE',  ( -17.11825945287481687, 66.05000000001182059, -82.17310748452439384 ) ) ;
#187304 = EDGE_LOOP ( 'NONE', ( #222037, #122556, #250105, #70431 ) ) ;
#187303 = VECTOR ( 'NONE', #38885, 1000.000000000000000 ) ;
#187305 = CARTESIAN_POINT ( 'NONE',  ( -16.94180778212363236, 22.95772180291950448, -230.8760158671809393 ) ) ;
#187306 = DIRECTION ( 'NONE',  ( -1.000000000000000000, 0.000000000000000000, 0.000000000000000000 ) ) ;
#187307 = AXIS2_PLACEMENT_3D ( 'NONE', #126879, #189427, #225938 ) ;
#187309 = EDGE_CURVE ( 'NONE', #13242, #202160, #160534, .T. ) ;
#187308 = CARTESIAN_POINT ( 'NONE',  ( -20.54999999999999716, 1.115600667400684642E-11, -33.50000000000000000 ) ) ;
#187310 = CARTESIAN_POINT ( 'NONE',  ( 23.14999999999999503, 11.65000000000000746, -26.48519422934606027 ) ) ;
#187311 = CARTESIAN_POINT ( 'NONE',  ( -21.65000000000000213, 68.75000000001182343, -82.17310748452436542 ) ) ;
#187312 = CIRCLE ( 'NONE', #253922, 7.899999999999990585 ) ;
#187313 = ORIENTED_EDGE ( 'NONE', *, *, #214522, .T. ) ;
#187314 =( BOUNDED_SURFACE ( )  B_SPLINE_SURFACE ( 3, 2, ( 
 ( #101232, #201665, #142952 ),
 ( #84229, #105096, #184664 ),
 ( #6021, #4728, #144241 ),
 ( #103829, #21765, #43884 ),
 ( #123421, #165115, #81681 ),
 ( #240805, #24339, #183401 ),
 ( #106396, #185960, #163836 ),
 ( #223784, #46435, #205509 ) ),
 .UNSPECIFIED., .F., .F., .F. ) 
 B_SPLINE_SURFACE_WITH_KNOTS ( ( 4, 2, 2, 4 ),
 ( 3, 3 ),
 ( 0.0001704874539069756818, 0.0003809798300636538649, 0.0004862260181419929836, 0.0005914722062203320481 ),
 ( 0.000000000000000000, 1.000000000000000000 ),
 .UNSPECIFIED. ) 
 GEOMETRIC_REPRESENTATION_ITEM ( )  RATIONAL_B_SPLINE_SURFACE ( (
 ( 1.000000000000000000, 0.7071067811864569785, 1.000000000000000000),
 ( 1.000000000000000000, 0.7670648383580433993, 1.000000000000000000),
 ( 1.000000000000000000, 0.8204820770247034378, 1.000000000000000000),
 ( 1.000000000000000000, 0.8877218296116180518, 1.000000000000000000),
 ( 1.000000000000000000, 0.9080815932668236945, 1.000000000000000000),
 ( 1.000000000000000000, 0.9395541505859680287, 1.000000000000000000),
 ( 1.000000000000000000, 0.9506520335380508335, 1.000000000000000000),
 ( 1.000000000000000000, 0.9504532311154547664, 1.000000000000000000) ) ) 
 REPRESENTATION_ITEM ( '' )  SURFACE ( )  );
#187315 = FACE_OUTER_BOUND ( 'NONE', #148845, .T. ) ;
#187317 = ADVANCED_FACE ( 'NONE', ( #143786 ), #110615, .T. ) ;
#187316 = CARTESIAN_POINT ( 'NONE',  ( -23.15000000000000213, 1.115600667400684642E-11, -67.00000000000004263 ) ) ;
#187318 = ORIENTED_EDGE ( 'NONE', *, *, #191450, .F. ) ;
#187319 = ORIENTED_EDGE ( 'NONE', *, *, #106192, .T. ) ;
#187321 = EDGE_CURVE ( 'NONE', #41664, #81229, #206304, .T. ) ;
#187320 = CARTESIAN_POINT ( 'NONE',  ( 18.59999999999996945, 65.66751761918668251, -97.42826094061121012 ) ) ;
#187322 = CARTESIAN_POINT ( 'NONE',  ( 18.39999999999999858, 78.24072131640578220, -231.5548844243369047 ) ) ;
#187323 = AXIS2_PLACEMENT_3D ( 'NONE', #71188, #8634, #226362 ) ;
#187324 = CARTESIAN_POINT ( 'NONE',  ( -22.59999999999999787, 0.1008583691098682150, -21.75043287651061164 ) ) ;
#187325 = AXIS2_PLACEMENT_3D ( 'NONE', #232033, #14272, #173373 ) ;
#187326 = ORIENTED_EDGE ( 'NONE', *, *, #175999, .F. ) ;
#187327 = DIRECTION ( 'NONE',  ( 0.000000000000000000, -0.9126074666063768159, -0.4088369013363282178 ) ) ;
#187328 = CARTESIAN_POINT ( 'NONE',  ( 21.14999999999999858, 11.65000000001115943, -33.60000000000000142 ) ) ;
#187329 = ADVANCED_FACE ( 'NONE', ( #48544 ), #202491, .T. ) ;
#187330 = ORIENTED_EDGE ( 'NONE', *, *, #76353, .F. ) ;
#187331 = CIRCLE ( 'NONE', #212281, 0.09999999999998898659 ) ;
#187332 = CARTESIAN_POINT ( 'NONE',  ( -18.79999999999999716, -11.65000000000000036, 30.09999999999999787 ) ) ;
#187333 = ORIENTED_EDGE ( 'NONE', *, *, #181160, .F. ) ;
#187334 = CARTESIAN_POINT ( 'NONE',  ( 19.97071067811865674, 11.72071067812981759, -158.7085786437627064 ) ) ;
#187336 = ADVANCED_FACE ( 'NONE', ( #246735 ), #189724, .F. ) ;
#187335 = CARTESIAN_POINT ( 'NONE',  ( -23.15000000000000213, 1.115600667400684642E-11, -180.3749999999999716 ) ) ;
#187337 = DIRECTION ( 'NONE',  ( -0.000000000000000000, 6.982962677686266711E-15, -1.000000000000000000 ) ) ;
#187338 = CARTESIAN_POINT ( 'NONE',  ( 20.94999999999999929, 36.12913288928921673, -236.0511878519285176 ) ) ;
#187339 = LINE ( 'NONE', #8686, #53685 ) ;
#187340 = CARTESIAN_POINT ( 'NONE',  ( -18.59999999999999787, 1.115600667400684642E-11, -33.50000000000000000 ) ) ;
#187341 = CARTESIAN_POINT ( 'NONE',  ( -21.05000000000000071, 76.00000000001197975, -107.3231074845242716 ) ) ;
#187342 = FACE_OUTER_BOUND ( 'NONE', #174676, .T. ) ;
#187343 = DIRECTION ( 'NONE',  ( 0.7071067811865795472, 0.3338907855511005218, 0.6233112732207110041 ) ) ;
#187344 = DIRECTION ( 'NONE',  ( 1.000000000000000000, -0.000000000000000000, -0.000000000000000000 ) ) ;
#187346 = ORIENTED_EDGE ( 'NONE', *, *, #99230, .F. ) ;
#187345 = DIRECTION ( 'NONE',  ( 2.915501640297155269E-16, -1.000000000000000000, 0.000000000000000000 ) ) ;
#187347 = EDGE_LOOP ( 'NONE', ( #4643, #100040, #130044, #213040 ) ) ;
#187350 = CARTESIAN_POINT ( 'NONE',  ( -23.25000000000000000, 0.8831241302008846494, -205.0549465804976421 ) ) ;
#187349 = PLANE ( 'NONE',  #53920 ) ;
#187348 = CIRCLE ( 'NONE', #12384, 12.77499999999999503 ) ;
#187351 = AXIS2_PLACEMENT_3D ( 'NONE', #172645, #214290, #151771 ) ;
#187353 = ORIENTED_EDGE ( 'NONE', *, *, #214696, .T. ) ;
#187352 = DIRECTION ( 'NONE',  ( 1.000000000000000000, -0.000000000000000000, -0.000000000000000000 ) ) ;
#187354 = VERTEX_POINT ( 'NONE', #242894 ) ;
#187355 = DIRECTION ( 'NONE',  ( 0.000000000000000000, -7.429790795770644761E-15, 1.000000000000000000 ) ) ;
#187356 = CARTESIAN_POINT ( 'NONE',  ( 21.08489247129321242, 67.12232480914178723, -90.67310748452436542 ) ) ;
#187357 = DIRECTION ( 'NONE',  ( 0.000000000000000000, 0.8814952561688476074, -0.4721928772777262417 ) ) ;
#187358 = DIRECTION ( 'NONE',  ( -1.000000000000000000, 2.952720810173289112E-16, 2.061873921506763405E-30 ) ) ;
#187359 = DIRECTION ( 'NONE',  ( -0.000000000000000000, 0.9126074666063771490, 0.4088369013363281623 ) ) ;
#187360 = DIRECTION ( 'NONE',  ( 1.000000000000000000, 0.000000000000000000, 0.000000000000000000 ) ) ;
#187361 = DIRECTION ( 'NONE',  ( 0.000000000000000000, -1.000000000000000000, 0.000000000000000000 ) ) ;
#187362 = AXIS2_PLACEMENT_3D ( 'NONE', #36938, #35651, #236377 ) ;
#187363 = ORIENTED_EDGE ( 'NONE', *, *, #121550, .F. ) ;
#187364 = ORIENTED_EDGE ( 'NONE', *, *, #98942, .F. ) ;
#187365 = AXIS2_PLACEMENT_3D ( 'NONE', #171487, #11099, #51469 ) ;
#187366 = DIRECTION ( 'NONE',  ( 1.000000000000000000, 1.836970198721029934E-16, 0.000000000000000000 ) ) ;
#187367 = VECTOR ( 'NONE', #4646, 1000.000000000000000 ) ;
#187368 = AXIS2_PLACEMENT_3D ( 'NONE', #127236, #67256, #106360 ) ;
#187369 = ORIENTED_EDGE ( 'NONE', *, *, #182922, .T. ) ;
#187370 = DIRECTION ( 'NONE',  ( -1.000000000000000000, -0.000000000000000000, -0.000000000000000000 ) ) ;
#187371 = VERTEX_POINT ( 'NONE', #147650 ) ;
#187372 = CARTESIAN_POINT ( 'NONE',  ( 20.94999999999999929, 18.71171618620643429, -229.8673829423568691 ) ) ;
#187373 = ADVANCED_FACE ( 'NONE', ( #6854 ), #165956, .F. ) ;
#187374 = CIRCLE ( 'NONE', #49990, 0.1000000000000124678 ) ;
#187375 = DIRECTION ( 'NONE',  ( 1.000000000000000000, 0.000000000000000000, 0.000000000000000000 ) ) ;
#187376 = CARTESIAN_POINT ( 'NONE',  ( -21.05000000000000071, 34.07612324756792077, -243.5412266404783566 ) ) ;
#187377 = DIRECTION ( 'NONE',  ( 1.000000000000000000, 0.000000000000000000, 0.000000000000000000 ) ) ;
#187378 = ORIENTED_EDGE ( 'NONE', *, *, #254181, .F. ) ;
#187380 = EDGE_CURVE ( 'NONE', #189010, #189515, #8148, .T. ) ;
#187379 = CARTESIAN_POINT ( 'NONE',  ( 23.14999999999999503, 11.65000000001116298, -160.4851942293460922 ) ) ;
#187381 = ORIENTED_EDGE ( 'NONE', *, *, #197823, .T. ) ;
#187382 = CIRCLE ( 'NONE', #37543, 0.09999999999998898659 ) ;
#187383 = CARTESIAN_POINT ( 'NONE',  ( -21.05000000000000071, -11.48912529306489994, -63.89999999999999858 ) ) ;
#187384 = CARTESIAN_POINT ( 'NONE',  ( 18.50000000000000000, 9.122720154857365316, -245.4644708025848274 ) ) ;
#187385 = ADVANCED_FACE ( 'NONE', ( #64264 ), #87659, .F. ) ;
#187386 = ORIENTED_EDGE ( 'NONE', *, *, #248022, .F. ) ;
#187387 = CARTESIAN_POINT ( 'NONE',  ( 18.59999999999999787, 67.23127455305841238, -235.8551265064783991 ) ) ;
#187388 = ORIENTED_EDGE ( 'NONE', *, *, #11738, .T. ) ;
#187391 = ORIENTED_EDGE ( 'NONE', *, *, #173626, .T. ) ;
#187390 = CARTESIAN_POINT ( 'NONE',  ( 18.51024323315077069, 46.39397692848790200, -243.0687461883537708 ) ) ;
#187389 = CARTESIAN_POINT ( 'NONE',  ( 18.54147908293629143, 46.96077838941292981, -255.3055355240929600 ) ) ;
#187392 = VECTOR ( 'NONE', #59517, 1000.000000000000114 ) ;
#187393 = FACE_OUTER_BOUND ( 'NONE', #70090, .T. ) ;
#187394 = VERTEX_POINT ( 'NONE', #148952 ) ;
#187395 = LINE ( 'NONE', #189953, #79716 ) ;
#187396 = ORIENTED_EDGE ( 'NONE', *, *, #97292, .F. ) ;
#187398 = EDGE_CURVE ( 'NONE', #253739, #125839, #247983, .T. ) ;
#187397 = CARTESIAN_POINT ( 'NONE',  ( 18.59999999999999076, 7.804459559388684298, -245.4620200072988325 ) ) ;
#187399 = CARTESIAN_POINT ( 'NONE',  ( 21.13736287352038445, 8.046642376383999817, -9.250000000000001776 ) ) ;
#187400 = CARTESIAN_POINT ( 'NONE',  ( -23.15000000000000213, 76.00000000001213607, -136.5231074845243313 ) ) ;
#187401 = EDGE_CURVE ( 'NONE', #231809, #17154, #118828, .T. ) ;
#187402 = EDGE_CURVE ( 'NONE', #152534, #210483, #192088, .T. ) ;
#187403 = CYLINDRICAL_SURFACE ( 'NONE', #247805, 0.1000000000000028644 ) ;
#187404 = VERTEX_POINT ( 'NONE', #190822 ) ;
#187405 = CARTESIAN_POINT ( 'NONE',  ( -18.79999999999999716, 10.31653824539117714, -11.82383137372478110 ) ) ;
#187406 = PRESENTATION_STYLE_ASSIGNMENT (( #145683 ) ) ;
#187407 = DIRECTION ( 'NONE',  ( 0.000000000000000000, -0.9651348961777157509, 0.2617529984165031243 ) ) ;
#187408 = CIRCLE ( 'NONE', #237297, 0.09999999999998898659 ) ;
#187409 = VERTEX_POINT ( 'NONE', #254578 ) ;
#187410 = CYLINDRICAL_SURFACE ( 'NONE', #134432, 0.5000000000000008882 ) ;
#187411 = VERTEX_POINT ( 'NONE', #235055 ) ;
#187412 = CARTESIAN_POINT ( 'NONE',  ( -23.25000000000000000, 74.00000000001254818, -183.2477294072864709 ) ) ;
#187413 = ADVANCED_FACE ( 'NONE', ( #94243 ), #92961, .F. ) ;
#187414 = CARTESIAN_POINT ( 'NONE',  ( 20.94999999999999929, 68.97833521811159585, -65.68954208262705663 ) ) ;
#187415 = DIRECTION ( 'NONE',  ( 0.000000000000000000, -6.938893903907222067E-15, 1.000000000000000000 ) ) ;
#187416 = AXIS2_PLACEMENT_3D ( 'NONE', #203544, #164424, #104412 ) ;
#187418 = VERTEX_POINT ( 'NONE', #51242 ) ;
#187417 = CARTESIAN_POINT ( 'NONE',  ( -16.85722902420148372, 44.24093119332965074, -235.2516915354734692 ) ) ;
#187419 = ADVANCED_FACE ( 'NONE', ( #253316 ), #115101, .F. ) ;
#187420 = CARTESIAN_POINT ( 'NONE',  ( -20.64999999999999858, 85.40000000001207070, -126.6291383618717816 ) ) ;
#187421 = EDGE_CURVE ( 'NONE', #83188, #257030, #252037, .T. ) ;
#187422 = DIRECTION ( 'NONE',  ( -1.000000000000000000, 0.000000000000000000, 0.000000000000000000 ) ) ;
#187423 = DIRECTION ( 'NONE',  ( 0.000000000000000000, -0.8814952561688430555, 0.4721928772777346239 ) ) ;
#187424 = VERTEX_POINT ( 'NONE', #16028 ) ;
#187425 = DIRECTION ( 'NONE',  ( -0.000000000000000000, -0.000000000000000000, -1.000000000000000000 ) ) ;
#187426 = CARTESIAN_POINT ( 'NONE',  ( 18.52928932188133970, 10.27928932189250411, -58.25000000000000000 ) ) ;
#187427 = ORIENTED_EDGE ( 'NONE', *, *, #86847, .F. ) ;
#187428 = CARTESIAN_POINT ( 'NONE',  ( -16.94107738177415712, 10.01423928514777728, -146.5500000000000114 ) ) ;
#187429 = CIRCLE ( 'NONE', #83333, 0.09999999999998898659 ) ;
#187430 = VECTOR ( 'NONE', #19266, 1000.000000000000000 ) ;
#187431 = ORIENTED_EDGE ( 'NONE', *, *, #70932, .F. ) ;
#187432 = CARTESIAN_POINT ( 'NONE',  ( -16.83199030136658436, 44.25509759139306709, -235.2665503012579507 ) ) ;
#187434 = VERTEX_POINT ( 'NONE', #12172 ) ;
#187433 = FACE_OUTER_BOUND ( 'NONE', #114842, .T. ) ;
#187435 = EDGE_CURVE ( 'NONE', #241950, #232157, #52163, .T. ) ;
#187436 = AXIS2_PLACEMENT_3D ( 'NONE', #137483, #235312, #56645 ) ;
#187437 = EDGE_CURVE ( 'NONE', #167528, #220874, #197097, .T. ) ;
#187438 = AXIS2_PLACEMENT_3D ( 'NONE', #104129, #101547, #241118 ) ;
#187439 = AXIS2_PLACEMENT_3D ( 'NONE', #195362, #175792, #255250 ) ;
#187442 = ORIENTED_EDGE ( 'NONE', *, *, #51399, .T. ) ;
#187441 = VERTEX_POINT ( 'NONE', #154277 ) ;
#187440 = DIRECTION ( 'NONE',  ( 1.000000000000000000, 0.000000000000000000, 0.000000000000000000 ) ) ;
#187443 = DIRECTION ( 'NONE',  ( 1.000000000000000000, -0.000000000000000000, -0.000000000000000000 ) ) ;
#187444 = DIRECTION ( 'NONE',  ( 1.000000000000000000, 0.000000000000000000, -0.000000000000000000 ) ) ;
#187446 = EDGE_CURVE ( 'NONE', #121060, #239691, #6374, .T. ) ;
#187445 = CARTESIAN_POINT ( 'NONE',  ( -21.05000000000000071, 76.00000000001168132, -65.52310748452430289 ) ) ;
#187448 = LINE ( 'NONE', #8798, #112786 ) ;
#187447 = CARTESIAN_POINT ( 'NONE',  ( -18.39999999999999858, -9.599999999988844124, -40.53206939669966857 ) ) ;
#187449 = DIRECTION ( 'NONE',  ( 0.000000000000000000, 0.2128009952263630322, -0.9770955615653309501 ) ) ;
#187450 = FACE_OUTER_BOUND ( 'NONE', #216584, .T. ) ;
#187451 = CARTESIAN_POINT ( 'NONE',  ( 13.99999999999999822, 66.15000000001228386, -153.2731074845244450 ) ) ;
#187452 = AXIS2_PLACEMENT_3D ( 'NONE', #141346, #6966, #104751 ) ;
#187453 = DIRECTION ( 'NONE',  ( -0.000000000000000000, 1.000000000000000000, -0.000000000000000000 ) ) ;
#187454 = AXIS2_PLACEMENT_3D ( 'NONE', #37219, #176732, #114167 ) ;
#187455 = CIRCLE ( 'NONE', #158435, 0.09999999999998898659 ) ;
#187456 = ORIENTED_EDGE ( 'NONE', *, *, #18531, .T. ) ;
#187457 = AXIS2_PLACEMENT_3D ( 'NONE', #8232, #125593, #69502 ) ;
#187459 = ORIENTED_EDGE ( 'NONE', *, *, #246975, .T. ) ;
#187458 = CIRCLE ( 'NONE', #16779, 12.87499999999999289 ) ;
#187460 = CARTESIAN_POINT ( 'NONE',  ( -20.65000000000000568, 7.250000000011138646, -188.3499999999999659 ) ) ;
#187462 = EDGE_LOOP ( 'NONE', ( #238758, #199653, #35465, #245960 ) ) ;
#187461 = CARTESIAN_POINT ( 'NONE',  ( -18.59999999999999787, -1.687074390080403941, -121.1854270334583674 ) ) ;
#187463 = ORIENTED_EDGE ( 'NONE', *, *, #170227, .T. ) ;
#187464 = TOROIDAL_SURFACE ( 'NONE', #233273, 3.899999999999999467, 0.1000000000000000056 ) ;
#187465 = CARTESIAN_POINT ( 'NONE',  ( -20.94999999999999929, 5.900000000011162093, -157.2809002353436654 ) ) ;
#187466 = EDGE_LOOP ( 'NONE', ( #61878, #31499, #189023, #26619 ) ) ;
#187467 = CYLINDRICAL_SURFACE ( 'NONE', #17156, 0.1000000000000053763 ) ;
#187468 = EDGE_CURVE ( 'NONE', #12767, #219135, #91684, .T. ) ;
#187469 = ORIENTED_EDGE ( 'NONE', *, *, #233427, .F. ) ;
#187470 = CARTESIAN_POINT ( 'NONE',  ( -16.90987985657661241, 66.04219248183207469, -82.15382039564075001 ) ) ;
#187472 = EDGE_CURVE ( 'NONE', #237169, #146785, #17298, .T. ) ;
#187471 = CARTESIAN_POINT ( 'NONE',  ( 18.39999999999999858, -9.599999999999997868, -7.032069396699667685 ) ) ;
#187474 = EDGE_LOOP ( 'NONE', ( #23599, #74888, #157018 ) ) ;
#187473 = EDGE_LOOP ( 'NONE', ( #196526, #15529, #45422, #62408 ) ) ;
#187475 = ORIENTED_EDGE ( 'NONE', *, *, #37917, .T. ) ;
#187476 = CARTESIAN_POINT ( 'NONE',  ( 21.05193202509564543, 10.72393601970834354, -45.67253460332576509 ) ) ;
#187477 = EDGE_LOOP ( 'NONE', ( #247732, #107328, #249992, #57110 ) ) ;
#187478 = ORIENTED_EDGE ( 'NONE', *, *, #183934, .T. ) ;
#187479 = EDGE_CURVE ( 'NONE', #137139, #178845, #65007, .T. ) ;
#187480 = DIRECTION ( 'NONE',  ( 7.304098846218132695E-16, 0.9770955615653315052, 0.2128009952263603954 ) ) ;
#187481 = DIRECTION ( 'NONE',  ( 0.000000000000000000, 0.000000000000000000, -1.000000000000000000 ) ) ;
#187482 = CARTESIAN_POINT ( 'NONE',  ( -13.54036565897076727, 9.451541661396669625, -185.9538754988305698 ) ) ;
#187485 = ADVANCED_FACE ( 'NONE', ( #112543 ), #175124, .T. ) ;
#187484 = ORIENTED_EDGE ( 'NONE', *, *, #155562, .T. ) ;
#187483 = DIRECTION ( 'NONE',  ( 0.000000000000000000, 0.000000000000000000, -1.000000000000000000 ) ) ;
#187486 = CARTESIAN_POINT ( 'NONE',  ( 21.05000000000000071, 87.48912529308871910, -200.4231074845242802 ) ) ;
#187487 = CYLINDRICAL_SURFACE ( 'NONE', #174212, 0.1000000000000024342 ) ;
#187489 = EDGE_LOOP ( 'NONE', ( #143193, #220780, #225119, #43787, #14896 ) ) ;
#187488 = DIRECTION ( 'NONE',  ( -1.000000000000000000, -1.186688945009010077E-16, -0.000000000000000000 ) ) ;
#187490 = DIRECTION ( 'NONE',  ( 1.000000000000000000, -7.304098846218135653E-16, -2.111765289898286048E-31 ) ) ;
#187491 = ORIENTED_EDGE ( 'NONE', *, *, #138283, .T. ) ;
#187492 = EDGE_CURVE ( 'NONE', #174581, #41411, #52337, .T. ) ;
#187493 = CYLINDRICAL_SURFACE ( 'NONE', #37044, 0.1000000000000038219 ) ;
#187494 = CIRCLE ( 'NONE', #41754, 0.1000000000000055844 ) ;
#187495 = ORIENTED_EDGE ( 'NONE', *, *, #179618, .T. ) ;
#187496 = CARTESIAN_POINT ( 'NONE',  ( -21.03922262424668688, 18.66391577654005829, -226.7251572270064912 ) ) ;
#187497 = LINE ( 'NONE', #128797, #195664 ) ;
#187498 = VECTOR ( 'NONE', #185165, 1000.000000000000114 ) ;
#187499 = ORIENTED_EDGE ( 'NONE', *, *, #11377, .F. ) ;
#187501 = CARTESIAN_POINT ( 'NONE',  ( 21.05000000000000071, 0.000000000000000000, 0.000000000000000000 ) ) ;
#187500 = CARTESIAN_POINT ( 'NONE',  ( 23.24999999999999645, 65.07363471106805264, -222.4165545841253220 ) ) ;
#187502 = DIRECTION ( 'NONE',  ( 0.000000000000000000, -0.4856429311786357728, -0.8741572761215358200 ) ) ;
#187503 = AXIS2_PLACEMENT_3D ( 'NONE', #190120, #147121, #169306 ) ;
#187504 = EDGE_CURVE ( 'NONE', #155258, #13363, #134635, .T. ) ;
#187505 = DIRECTION ( 'NONE',  ( 0.000000000000000000, -0.2965989261549410450, -0.9550021345545443019 ) ) ;
#187506 = DIRECTION ( 'NONE',  ( -0.7071067811865474617, -0.3338907855510734324, -0.6233112732207618523 ) ) ;
#187507 = ADVANCED_FACE ( 'NONE', ( #113812 ), #176381, .T. ) ;
#187508 = ORIENTED_EDGE ( 'NONE', *, *, #240275, .F. ) ;
#187509 = EDGE_LOOP ( 'NONE', ( #87710, #126323, #125590, #187554 ) ) ;
#187510 = DIRECTION ( 'NONE',  ( 0.000000000000000000, 0.9651348961777157509, -0.2617529984165031243 ) ) ;
#187511 = DIRECTION ( 'NONE',  ( 0.000000000000000000, -0.9651348961777161950, 0.2617529984165015700 ) ) ;
#187512 = EDGE_LOOP ( 'NONE', ( #247934, #20221, #136468, #125255 ) ) ;
#187513 = CARTESIAN_POINT ( 'NONE',  ( 23.14999999999999858, 76.00000000001170974, -69.52310748452431710 ) ) ;
#187514 = ORIENTED_EDGE ( 'NONE', *, *, #168412, .F. ) ;
#187515 = EDGE_CURVE ( 'NONE', #246378, #254139, #148211, .T. ) ;
#187516 = CARTESIAN_POINT ( 'NONE',  ( 18.39999999999999503, 5.650000000011139001, -79.65000000000004832 ) ) ;
#187517 = ORIENTED_EDGE ( 'NONE', *, *, #154310, .F. ) ;
#187518 = CYLINDRICAL_SURFACE ( 'NONE', #112678, 0.1000000000000028644 ) ;
#187519 = DIRECTION ( 'NONE',  ( 0.000000000000000000, 0.000000000000000000, 1.000000000000000000 ) ) ;
#187520 = DIRECTION ( 'NONE',  ( 0.000000000000000000, -1.243449787580175010E-14, -1.000000000000000000 ) ) ;
#187521 = AXIS2_PLACEMENT_3D ( 'NONE', #124283, #184239, #5576 ) ;
#187522 = ORIENTED_EDGE ( 'NONE', *, *, #90828, .T. ) ;
#187523 = CARTESIAN_POINT ( 'NONE',  ( 18.46932045258651200, -9.670685200254535374, -207.6738603729966712 ) ) ;
#187524 = EDGE_CURVE ( 'NONE', #150942, #214618, #201053, .T. ) ;
#187525 = AXIS2_PLACEMENT_3D ( 'NONE', #163433, #199993, #242952 ) ;
#187526 = ORIENTED_EDGE ( 'NONE', *, *, #35882, .F. ) ;
#187527 = EDGE_LOOP ( 'NONE', ( #216593, #48824, #38286, #81556 ) ) ;
#187528 = ORIENTED_EDGE ( 'NONE', *, *, #180033, .T. ) ;
#187529 = EDGE_CURVE ( 'NONE', #93827, #58001, #35802, .T. ) ;
#187530 = CARTESIAN_POINT ( 'NONE',  ( 21.14999999999999503, -11.64999999999999147, -2.900000000000003464 ) ) ;
#187531 = LINE ( 'NONE', #64984, #148980 ) ;
#187532 = CARTESIAN_POINT ( 'NONE',  ( -1.739115166359751801E-14, 11.65000000001114699, -45.75000000000000711 ) ) ;
#187533 = LINE ( 'NONE', #7587, #232020 ) ;
#187534 = FACE_OUTER_BOUND ( 'NONE', #149294, .T. ) ;
#187536 = FACE_OUTER_BOUND ( 'NONE', #182435, .T. ) ;
#187535 = DIRECTION ( 'NONE',  ( 0.000000000000000000, -0.9908441862701420355, -0.1350103645453197554 ) ) ;
#187537 = EDGE_CURVE ( 'NONE', #131693, #229311, #56590, .T. ) ;
#187539 = ORIENTED_EDGE ( 'NONE', *, *, #204546, .F. ) ;
#187538 = CARTESIAN_POINT ( 'NONE',  ( 19.75857864376268935, 11.65000000001115943, -192.3499999999999659 ) ) ;
#187540 = DIRECTION ( 'NONE',  ( 1.000000000000000000, 0.000000000000000000, 0.000000000000000000 ) ) ;
#187541 = ORIENTED_EDGE ( 'NONE', *, *, #77684, .F. ) ;
#187542 = DIRECTION ( 'NONE',  ( 0.000000000000000000, 0.000000000000000000, 1.000000000000000000 ) ) ;
#187543 = ADVANCED_FACE ( 'NONE', ( #161951 ), #22443, .T. ) ;
#187544 = ORIENTED_EDGE ( 'NONE', *, *, #231597, .T. ) ;
#187545 = ORIENTED_EDGE ( 'NONE', *, *, #122426, .F. ) ;
#187546 = CARTESIAN_POINT ( 'NONE',  ( 21.05000000000000071, 64.25000000001195133, -110.0379132551783243 ) ) ;
#187547 = DIRECTION ( 'NONE',  ( -0.000000000000000000, 0.9667078373770112698, 0.2558827019434132821 ) ) ;
#187548 = CARTESIAN_POINT ( 'NONE',  ( -16.86379686415369861, 66.02478224075841240, -56.95649737361467402 ) ) ;
#187549 = DIRECTION ( 'NONE',  ( 1.000000000000000000, 0.000000000000000000, 0.000000000000000000 ) ) ;
#187550 = AXIS2_PLACEMENT_3D ( 'NONE', #205732, #11406, #88329 ) ;
#187551 = VECTOR ( 'NONE', #180010, 1000.000000000000000 ) ;
#187552 = DIRECTION ( 'NONE',  ( 0.000000000000000000, -0.7397360091702647189, -0.6728971962616949742 ) ) ;
#187553 = VERTEX_POINT ( 'NONE', #241471 ) ;
#187554 = ORIENTED_EDGE ( 'NONE', *, *, #10788, .T. ) ;
#187555 = DIRECTION ( 'NONE',  ( 0.000000000000000000, -6.982962677686266711E-15, 1.000000000000000000 ) ) ;
#187557 = EDGE_CURVE ( 'NONE', #191947, #146391, #152343, .T. ) ;
#187556 = VERTEX_POINT ( 'NONE', #142356 ) ;
#187558 = CARTESIAN_POINT ( 'NONE',  ( 21.05000000000000071, 67.23127455305835554, -235.8551265064784559 ) ) ;
#187559 = CARTESIAN_POINT ( 'NONE',  ( -20.64999999999999858, 7.150000000011155876, -188.6499999999999488 ) ) ;
#187560 = ORIENTED_EDGE ( 'NONE', *, *, #207720, .F. ) ;
#187561 = DIRECTION ( 'NONE',  ( 0.000000000000000000, 0.000000000000000000, 1.000000000000000000 ) ) ;
#187562 = CYLINDRICAL_SURFACE ( 'NONE', #250437, 0.1000000000000028644 ) ;
#187563 = DIRECTION ( 'NONE',  ( 0.000000000000000000, -0.8103668758649578141, 0.5859227990963212784 ) ) ;
#187564 = CARTESIAN_POINT ( 'NONE',  ( -20.54999999999999716, 76.00000000001244871, -170.0231074845243597 ) ) ;
#187565 = ORIENTED_EDGE ( 'NONE', *, *, #176979, .F. ) ;
#187566 = CARTESIAN_POINT ( 'NONE',  ( 21.05000000000000071, 1.162701749949165642, -108.4000000000000341 ) ) ;
#187567 = DIRECTION ( 'NONE',  ( 7.304098846218134667E-16, -1.000000000000000000, 0.000000000000000000 ) ) ;
#187568 = LINE ( 'NONE', #127572, #245932 ) ;
#187570 = ADVANCED_FACE ( 'NONE', ( #103215 ), #177481, .F. ) ;
#187569 = CARTESIAN_POINT ( 'NONE',  ( 22.39999999999999858, 7.790779598384538929, -33.39999999999999858 ) ) ;
#187571 = VECTOR ( 'NONE', #143692, 1000.000000000000000 ) ;
#187572 = CIRCLE ( 'NONE', #208415, 0.1999999999999987899 ) ;
#187573 = DIRECTION ( 'NONE',  ( 0.000000000000000000, 0.000000000000000000, 1.000000000000000000 ) ) ;
#187574 = CARTESIAN_POINT ( 'NONE',  ( -23.15000000000000213, 87.65000000001246860, -173.1231074845242688 ) ) ;
#187575 = ORIENTED_EDGE ( 'NONE', *, *, #239591, .F. ) ;
#187576 = CIRCLE ( 'NONE', #20984, 0.09999999999999939493 ) ;
#187578 = EDGE_CURVE ( 'NONE', #255134, #256176, #231431, .T. ) ;
#187577 = DIRECTION ( 'NONE',  ( 0.5932847527679310229, 0.8049926720990042694, 6.257843056355992909E-15 ) ) ;
#187579 = ORIENTED_EDGE ( 'NONE', *, *, #11089, .T. ) ;
#187580 = DIRECTION ( 'NONE',  ( -1.000000000000000000, 0.000000000000000000, 0.000000000000000000 ) ) ;
#187581 = DIRECTION ( 'NONE',  ( 0.000000000000000000, 0.9651348961777158619, -0.2617529984165031243 ) ) ;
#187582 = FACE_OUTER_BOUND ( 'NONE', #102446, .T. ) ;
#187583 = CARTESIAN_POINT ( 'NONE',  ( 20.77766267348356166, 65.55095760939360616, -162.4303985686467513 ) ) ;
#187584 = AXIS2_PLACEMENT_3D ( 'NONE', #184031, #243998, #180199 ) ;
#187585 = ORIENTED_EDGE ( 'NONE', *, *, #224816, .F. ) ;
#187587 = AXIS2_PLACEMENT_3D ( 'NONE', #163750, #62079, #64636 ) ;
#187586 = FACE_OUTER_BOUND ( 'NONE', #70532, .T. ) ;
#187588 = CARTESIAN_POINT ( 'NONE',  ( -23.15000000000000213, 76.00000000001195133, -103.0231074845243171 ) ) ;
#187589 = DIRECTION ( 'NONE',  ( 0.000000000000000000, -0.8700118002898321601, 0.4930308989875230030 ) ) ;
#187590 = EDGE_CURVE ( 'NONE', #105026, #80105, #138482, .T. ) ;
#187591 = CARTESIAN_POINT ( 'NONE',  ( 18.59999999999999432, 77.83585931145570669, -125.0186683157258045 ) ) ;
#187592 = ORIENTED_EDGE ( 'NONE', *, *, #230181, .F. ) ;
#187593 = ORIENTED_EDGE ( 'NONE', *, *, #203575, .F. ) ;
#187594 = DIRECTION ( 'NONE',  ( 0.000000000000000000, 1.000000000000000000, 0.000000000000000000 ) ) ;
#187595 = DIRECTION ( 'NONE',  ( 0.000000000000000000, 0.000000000000000000, 1.000000000000000000 ) ) ;
#187596 = CARTESIAN_POINT ( 'NONE',  ( 22.40000000000010161, 1.020945317880167817E-11, -122.2495671075410968 ) ) ;
#187597 = DIRECTION ( 'NONE',  ( 1.000000000000000000, 0.000000000000000000, 0.000000000000000000 ) ) ;
#187598 = CARTESIAN_POINT ( 'NONE',  ( 23.14999999999999858, 35.97645343225767789, -235.9694016464868298 ) ) ;
#187599 = VERTEX_POINT ( 'NONE', #276 ) ;
#187600 = CARTESIAN_POINT ( 'NONE',  ( 22.49544290803764213, 11.74987023786834683, -33.43468804074238676 ) ) ;
#187601 = DIRECTION ( 'NONE',  ( -1.000000000000000000, 0.000000000000000000, 0.000000000000000000 ) ) ;
#187602 = EDGE_LOOP ( 'NONE', ( #161430, #10731, #188170, #43986 ) ) ;
#187603 = CYLINDRICAL_SURFACE ( 'NONE', #158732, 0.09999999999999939493 ) ;
#187604 = B_SPLINE_CURVE_WITH_KNOTS ( 'NONE', 3,
 ( #239637, #60980, #140509, #41452 ),
 .UNSPECIFIED., .F., .F.,
 ( 4, 4 ),
 ( 0.000000000000000000, 7.713889350929889021E-05 ),
 .UNSPECIFIED. ) ;
#187605 = CIRCLE ( 'NONE', #220885, 0.09999999999999939493 ) ;
#187606 = ORIENTED_EDGE ( 'NONE', *, *, #166967, .F. ) ;
#187607 = EDGE_LOOP ( 'NONE', ( #82823, #171705, #160696, #92548, #82749 ) ) ;
#187608 = TOROIDAL_SURFACE ( 'NONE', #175174, 12.77499999999999858, 0.1000000000000000056 ) ;
#187609 = ORIENTED_EDGE ( 'NONE', *, *, #132456, .T. ) ;
#187610 = CARTESIAN_POINT ( 'NONE',  ( 20.95512820512820085, 10.62384868372303615, -74.66491356908764487 ) ) ;
#187611 = DIRECTION ( 'NONE',  ( 0.000000000000000000, 0.000000000000000000, 1.000000000000000000 ) ) ;
#187612 = CARTESIAN_POINT ( 'NONE',  ( 21.05000000000000071, 10.72371710471867701, -112.6500000000000341 ) ) ;
#187613 = CARTESIAN_POINT ( 'NONE',  ( -23.25000000000000000, 1.115600667400684642E-11, -33.50000000000000000 ) ) ;
#187614 = CARTESIAN_POINT ( 'NONE',  ( -23.25000000000000000, 11.65000000001115588, -155.3500000000000227 ) ) ;
#187615 = CARTESIAN_POINT ( 'NONE',  ( 18.54999999999999716, 23.65833333334447985, -50.25000000000000000 ) ) ;
#187616 = EDGE_CURVE ( 'NONE', #227071, #236905, #98065, .T. ) ;
#187617 = DIRECTION ( 'NONE',  ( -7.304098846218134667E-16, 1.000000000000000000, -0.000000000000000000 ) ) ;
#187619 = DIRECTION ( 'NONE',  ( 0.000000000000000000, 0.000000000000000000, -1.000000000000000000 ) ) ;
#187618 = DIRECTION ( 'NONE',  ( 1.000000000000000000, 0.000000000000000000, 0.000000000000000000 ) ) ;
#187620 = CARTESIAN_POINT ( 'NONE',  ( 21.05000000000000071, -1.489567864901280680, -194.6304332222954372 ) ) ;
#187621 = LINE ( 'NONE', #6393, #65643 ) ;
#187622 = VECTOR ( 'NONE', #179617, 1000.000000000000000 ) ;
#187623 = ORIENTED_EDGE ( 'NONE', *, *, #83181, .T. ) ;
#187624 = ORIENTED_EDGE ( 'NONE', *, *, #98679, .T. ) ;
#187625 = DIRECTION ( 'NONE',  ( 1.000000000000000000, -0.000000000000000000, -0.000000000000000000 ) ) ;
#187626 = AXIS2_PLACEMENT_3D ( 'NONE', #92067, #33428, #109060 ) ;
#187627 = CARTESIAN_POINT ( 'NONE',  ( -18.79999999999999716, 1.149999999999999911, 21.90000000000000213 ) ) ;
#187629 = CARTESIAN_POINT ( 'NONE',  ( -14.56336952470180179, 13.14811317477304442, -216.9788617421937431 ) ) ;
#187628 = CARTESIAN_POINT ( 'NONE',  ( 18.49999999999999289, 7.120270961708750512, -171.1595630418393625 ) ) ;
#187630 = PRESENTATION_LAYER_ASSIGNMENT (  '', '', ( #33530 ) ) ;
#187631 = CARTESIAN_POINT ( 'NONE',  ( -23.15000000000000213, 4.250000000011156409, -112.7500000000000284 ) ) ;
#187633 = EDGE_CURVE ( 'NONE', #62333, #207338, #177674, .T. ) ;
#187632 = DIRECTION ( 'NONE',  ( -1.000000000000000000, -0.000000000000000000, -0.000000000000000000 ) ) ;
#187634 = LINE ( 'NONE', #228029, #73249 ) ;
#187635 = AXIS2_PLACEMENT_3D ( 'NONE', #2811, #245299, #66661 ) ;
#187636 = EDGE_LOOP ( 'NONE', ( #52994, #7869, #237196, #222993 ) ) ;
#187637 = TOROIDAL_SURFACE ( 'NONE', #187439, 3.899999999999999467, 0.1000000000000000056 ) ;
#187638 = ORIENTED_EDGE ( 'NONE', *, *, #75751, .F. ) ;
#187639 = EDGE_CURVE ( 'NONE', #108752, #39612, #164790, .T. ) ;
#187640 = CARTESIAN_POINT ( 'NONE',  ( -15.66061380678753245, 9.360723793986032604, -17.31392719460671970 ) ) ;
#187641 = ORIENTED_EDGE ( 'NONE', *, *, #196119, .T. ) ;
#187642 = LINE ( 'NONE', #8983, #168150 ) ;
#187643 = EDGE_CURVE ( 'NONE', #217845, #129019, #207013, .T. ) ;
#187644 = CIRCLE ( 'NONE', #29439, 0.1000000000000008937 ) ;
#187645 = CIRCLE ( 'NONE', #96022, 0.1000000000000024342 ) ;
#187647 = CIRCLE ( 'NONE', #104394, 0.1000000000000028644 ) ;
#187646 = CARTESIAN_POINT ( 'NONE',  ( 18.50000000000000000, 85.48068669529033059, -29.08199231576639932 ) ) ;
#187648 = CIRCLE ( 'NONE', #179448, 11.74999999999999645 ) ;
#187649 = VECTOR ( 'NONE', #243659, 1000.000000000000000 ) ;
#187650 = EDGE_CURVE ( 'NONE', #16549, #156950, #73246, .T. ) ;
#187651 = EDGE_CURVE ( 'NONE', #67239, #169135, #158125, .T. ) ;
#187652 = VERTEX_POINT ( 'NONE', #19868 ) ;
#187653 = FACE_BOUND ( 'NONE', #97558, .T. ) ;
#187654 = ORIENTED_EDGE ( 'NONE', *, *, #87360, .T. ) ;
#187655 = ADVANCED_FACE ( 'NONE', ( #240195 ), #61550, .F. ) ;
#187656 = DIRECTION ( 'NONE',  ( 1.000000000000000000, 7.304098846218134667E-16, -4.607487905232622991E-31 ) ) ;
#187657 = CARTESIAN_POINT ( 'NONE',  ( 20.94999999999999929, 69.35000000001159037, -59.50608031408435039 ) ) ;
#187658 = CARTESIAN_POINT ( 'NONE',  ( -18.40000000000000213, 64.51332499825393541, -60.27310748452440947 ) ) ;
#187659 = CARTESIAN_POINT ( 'NONE',  ( 23.15000000000000213, -9.599999999988842347, -90.60603087734760663 ) ) ;
#187660 = FACE_OUTER_BOUND ( 'NONE', #116934, .T. ) ;
#187661 = DIRECTION ( 'NONE',  ( 0.000000000000000000, -0.5826443254699606999, -0.8127272543711416830 ) ) ;
#187662 = EDGE_CURVE ( 'NONE', #162376, #150801, #120274, .T. ) ;
#187663 = CARTESIAN_POINT ( 'NONE',  ( -22.57320508075687115, 64.35000000001214460, -136.5231074845243313 ) ) ;
#187664 = DIRECTION ( 'NONE',  ( 1.000000000000000000, 0.000000000000000000, 0.000000000000000000 ) ) ;
#187666 = ORIENTED_EDGE ( 'NONE', *, *, #17488, .T. ) ;
#187665 = CARTESIAN_POINT ( 'NONE',  ( 20.96937028524355284, 65.37553062838541962, -129.0316813833547656 ) ) ;
#187668 = DIRECTION ( 'NONE',  ( 0.000000000000000000, 0.2128009952263403282, -0.9770955615653358350 ) ) ;
#187667 = DIRECTION ( 'NONE',  ( 1.000000000000000000, 0.000000000000000000, 0.000000000000000000 ) ) ;
#187669 = VERTEX_POINT ( 'NONE', #121555 ) ;
#187671 = VERTEX_POINT ( 'NONE', #101923 ) ;
#187670 = DIRECTION ( 'NONE',  ( 0.000000000000000000, 0.000000000000000000, -1.000000000000000000 ) ) ;
#187672 = ORIENTED_EDGE ( 'NONE', *, *, #175841, .F. ) ;
#187673 = DIRECTION ( 'NONE',  ( 0.000000000000000000, -0.6035730884107395333, -0.7973076739542406255 ) ) ;
#187674 = DIRECTION ( 'NONE',  ( 0.000000000000000000, 0.000000000000000000, -1.000000000000000000 ) ) ;
#187675 = CARTESIAN_POINT ( 'NONE',  ( 21.07928932188134397, 0.09889514566578949673, -127.6714833436012952 ) ) ;
#187676 = DIRECTION ( 'NONE',  ( 0.000000000000000000, 0.8814952561688428334, -0.4721928772777350125 ) ) ;
#187677 = CARTESIAN_POINT ( 'NONE',  ( -20.93284271247462058, 11.75000000001115019, -93.48519422934609224 ) ) ;
#187678 = CARTESIAN_POINT ( 'NONE',  ( 20.94999999999999929, 85.00000000001149658, -45.51707660717670478 ) ) ;
#187679 = DIRECTION ( 'NONE',  ( 1.000000000000000000, 0.000000000000000000, 0.000000000000000000 ) ) ;
#187680 = CIRCLE ( 'NONE', #208525, 0.09999999999998708533 ) ;
#187682 = EDGE_CURVE ( 'NONE', #170534, #208884, #25010, .T. ) ;
#187681 = FACE_OUTER_BOUND ( 'NONE', #208013, .T. ) ;
#187683 = AXIS2_PLACEMENT_3D ( 'NONE', #167887, #70067, #166603 ) ;
#187684 = DIRECTION ( 'NONE',  ( 1.000000000000000000, 0.000000000000000000, 0.000000000000000000 ) ) ;
#187685 = VERTEX_POINT ( 'NONE', #64116 ) ;
#187686 = ORIENTED_EDGE ( 'NONE', *, *, #149795, .T. ) ;
#187687 = CARTESIAN_POINT ( 'NONE',  ( -16.92925196614876171, 9.972331796421276096, -180.1167448477167454 ) ) ;
#187688 = CIRCLE ( 'NONE', #12908, 0.1000000000000028644 ) ;
#187689 = ORIENTED_EDGE ( 'NONE', *, *, #95491, .T. ) ;
#187690 = DIRECTION ( 'NONE',  ( 0.000000000000000000, 0.6728388485993177515, -0.7397890806274072251 ) ) ;
#187691 = ORIENTED_EDGE ( 'NONE', *, *, #113155, .T. ) ;
#187692 = CARTESIAN_POINT ( 'NONE',  ( 18.52928932188133970, 65.72071067813013201, -44.87310748452439668 ) ) ;
#187693 = EDGE_CURVE ( 'NONE', #172693, #100865, #189911, .T. ) ;
#187694 = CARTESIAN_POINT ( 'NONE',  ( 19.87657994472027312, 11.74999999999995204, -24.76578812462619439 ) ) ;
#187695 = CARTESIAN_POINT ( 'NONE',  ( 20.94999999999999929, 69.45000000001157048, -57.37310748452436115 ) ) ;
#187696 = FACE_OUTER_BOUND ( 'NONE', #102967, .T. ) ;
#187697 = DIRECTION ( 'NONE',  ( -1.186688945009010077E-16, 1.000000000000000000, 0.000000000000000000 ) ) ;
#187698 = ORIENTED_EDGE ( 'NONE', *, *, #19018, .T. ) ;
#187699 = CARTESIAN_POINT ( 'NONE',  ( -18.40000000000000213, 67.23581240663841641, -214.2531594801197627 ) ) ;
#187700 = AXIS2_PLACEMENT_3D ( 'NONE', #117545, #195827, #17182 ) ;
#187701 = CARTESIAN_POINT ( 'NONE',  ( 20.94999999999999929, 71.18691588786307989, -191.5815897280005800 ) ) ;
#187702 = CARTESIAN_POINT ( 'NONE',  ( 18.51997666896852479, 85.39233213153087831, -62.37970129704087441 ) ) ;
#187704 = EDGE_CURVE ( 'NONE', #246187, #239741, #106487, .T. ) ;
#187703 = FACE_OUTER_BOUND ( 'NONE', #184636, .T. ) ;
#187705 = ORIENTED_EDGE ( 'NONE', *, *, #136452, .F. ) ;
#187707 = CARTESIAN_POINT ( 'NONE',  ( 23.14999999999999503, 6.650000000011155876, -188.6499999999999488 ) ) ;
#187706 = CARTESIAN_POINT ( 'NONE',  ( 21.10320863425824811, 61.04759385288372187, -234.2039845577155859 ) ) ;
#187708 = ORIENTED_EDGE ( 'NONE', *, *, #213257, .T. ) ;
#187711 = ORIENTED_EDGE ( 'NONE', *, *, #109033, .F. ) ;
#187710 = CARTESIAN_POINT ( 'NONE',  ( -16.78493211734302903, 51.60783545504983039, -231.9559722212414385 ) ) ;
#187709 = CARTESIAN_POINT ( 'NONE',  ( 21.33487959338958717, 69.27444184810076422, -103.0231074845243597 ) ) ;
#187712 = EDGE_CURVE ( 'NONE', #116826, #43467, #98280, .T. ) ;
#187713 = ORIENTED_EDGE ( 'NONE', *, *, #7681, .F. ) ;
#187714 = CARTESIAN_POINT ( 'NONE',  ( -17.05016517656157404, 9.950000000013014656, -113.1726979960009629 ) ) ;
#187715 = AXIS2_PLACEMENT_3D ( 'NONE', #86392, #31625, #105963 ) ;
#187716 = CYLINDRICAL_SURFACE ( 'NONE', #202834, 0.09999999999999939493 ) ;
#187717 = DIRECTION ( 'NONE',  ( -4.391705002472927119E-16, -1.000000000000000000, -7.026728003956683390E-15 ) ) ;
#187718 = ORIENTED_EDGE ( 'NONE', *, *, #216766, .T. ) ;
#187719 = LINE ( 'NONE', #207282, #42986 ) ;
#187721 = EDGE_CURVE ( 'NONE', #200421, #126100, #192732, .T. ) ;
#187720 = CARTESIAN_POINT ( 'NONE',  ( -21.05000000000000071, 44.34387878855809362, -247.3824414791181994 ) ) ;
#187723 = CARTESIAN_POINT ( 'NONE',  ( -18.39999999999999858, 11.47867409999928157, -9.274693216340661905 ) ) ;
#187722 = FACE_OUTER_BOUND ( 'NONE', #253822, .T. ) ;
#187725 = ORIENTED_EDGE ( 'NONE', *, *, #101229, .T. ) ;
#187724 = DIRECTION ( 'NONE',  ( 0.000000000000000000, 0.000000000000000000, 1.000000000000000000 ) ) ;
#187726 = ADVANCED_FACE ( 'NONE', ( #65392 ), #28889, .F. ) ;
#187727 = EDGE_CURVE ( 'NONE', #94457, #13684, #10852, .T. ) ;
#187728 = CIRCLE ( 'NONE', #216910, 0.09999999999999939493 ) ;
#187729 = ORIENTED_EDGE ( 'NONE', *, *, #239245, .T. ) ;
#187730 = CARTESIAN_POINT ( 'NONE',  ( -16.87487986503753845, 9.950007555096753720, -79.64997473968678321 ) ) ;
#187731 = LINE ( 'NONE', #188998, #52213 ) ;
#187732 = DIRECTION ( 'NONE',  ( 0.000000000000000000, -0.4721928772777352346, -0.8814952561688428334 ) ) ;
#187733 = ORIENTED_EDGE ( 'NONE', *, *, #231771, .T. ) ;
#187734 = CARTESIAN_POINT ( 'NONE',  ( 21.14999999999999858, 11.65000000001115943, -146.1500000000000341 ) ) ;
#187735 = EDGE_CURVE ( 'NONE', #145681, #198700, #87505, .T. ) ;
#187736 = DIRECTION ( 'NONE',  ( 0.000000000000000000, -0.000000000000000000, -1.000000000000000000 ) ) ;
#187737 = VERTEX_POINT ( 'NONE', #26278 ) ;
#187738 = CARTESIAN_POINT ( 'NONE',  ( -18.50000000000000000, 64.25000000001260503, -191.3731074845244393 ) ) ;
#187739 = VECTOR ( 'NONE', #33128, 999.9999999999998863 ) ;
#187740 = CIRCLE ( 'NONE', #4539, 0.1000000000000028644 ) ;
#187741 = ORIENTED_EDGE ( 'NONE', *, *, #171239, .F. ) ;
#187742 = CIRCLE ( 'NONE', #204460, 0.1000000000000045852 ) ;
#187743 = CARTESIAN_POINT ( 'NONE',  ( -16.87683809663752399, 61.03587125567668181, -221.0679030354277188 ) ) ;
#187744 = CARTESIAN_POINT ( 'NONE',  ( -23.25000000000000000, 76.10000000001174669, -81.17267829206912211 ) ) ;
#187745 = ORIENTED_EDGE ( 'NONE', *, *, #8164, .F. ) ;
#187746 = VECTOR ( 'NONE', #96792, 1000.000000000000000 ) ;
#187747 = VERTEX_POINT ( 'NONE', #83632 ) ;
#187748 = CARTESIAN_POINT ( 'NONE',  ( -16.87036670365549895, 60.86740053880574663, -221.1564527318009254 ) ) ;
#187749 = ORIENTED_EDGE ( 'NONE', *, *, #144413, .T. ) ;
#187751 = ORIENTED_EDGE ( 'NONE', *, *, #87597, .F. ) ;
#187750 = CARTESIAN_POINT ( 'NONE',  ( 12.30626653967341610, 66.64320997496669463, -186.3182809759104543 ) ) ;
#187752 = ADVANCED_FACE ( 'NONE', ( #225725 ), #156638, .T. ) ;
#187753 = EDGE_CURVE ( 'NONE', #81578, #127685, #23354, .T. ) ;
#187754 = ORIENTED_EDGE ( 'NONE', *, *, #234752, .T. ) ;
#187755 = AXIS2_PLACEMENT_3D ( 'NONE', #20830, #256789, #100317 ) ;
#187757 = ORIENTED_EDGE ( 'NONE', *, *, #39632, .F. ) ;
#187756 = VERTEX_POINT ( 'NONE', #191472 ) ;
#187759 = ADVANCED_FACE ( 'NONE', ( #84920 ), #214844, .T. ) ;
#187758 = CARTESIAN_POINT ( 'NONE',  ( -18.58744394320964233, -9.566385154537629276, -107.3228480538757310 ) ) ;
#187760 = EDGE_LOOP ( 'NONE', ( #181776, #92423, #66281 ) ) ;
#187761 = CARTESIAN_POINT ( 'NONE',  ( -20.94999999999999929, 77.13501884592203339, -95.30613060109196510 ) ) ;
#187762 = DIRECTION ( 'NONE',  ( 0.000000000000000000, 0.8814952561688476074, -0.4721928772777262417 ) ) ;
#187763 = CARTESIAN_POINT ( 'NONE',  ( 21.05000000000000071, 69.45934304831071415, -102.9231074845243512 ) ) ;
#187764 = FACE_OUTER_BOUND ( 'NONE', #83421, .T. ) ;
#187765 = EDGE_LOOP ( 'NONE', ( #221337, #27118, #29221, #108877 ) ) ;
#187766 = ORIENTED_EDGE ( 'NONE', *, *, #153015, .T. ) ;
#187767 = DIRECTION ( 'NONE',  ( 0.000000000000000000, 0.000000000000000000, -1.000000000000000000 ) ) ;
#187769 = VERTEX_POINT ( 'NONE', #171912 ) ;
#187768 = LINE ( 'NONE', #7845, #70174 ) ;
#187770 = FACE_OUTER_BOUND ( 'NONE', #66238, .T. ) ;
#187772 = VERTEX_POINT ( 'NONE', #251408 ) ;
#187771 = CARTESIAN_POINT ( 'NONE',  ( 20.94999999999999929, 77.13501884592258762, -162.3061306010920362 ) ) ;
#187773 = AXIS2_PLACEMENT_3D ( 'NONE', #13136, #29212, #153969 ) ;
#187774 = VERTEX_POINT ( 'NONE', #147501 ) ;
#187775 = CARTESIAN_POINT ( 'NONE',  ( -20.94999999999999929, 74.16465844978715438, -57.96795619196135618 ) ) ;
#187776 = CIRCLE ( 'NONE', #183482, 0.09999999999999609201 ) ;
#187777 = VERTEX_POINT ( 'NONE', #206190 ) ;
#187779 = CONICAL_SURFACE ( 'NONE', #183686, 4.049999999999998046, 0.7853981633974604915 ) ;
#187778 = CARTESIAN_POINT ( 'NONE',  ( -16.80891096016330621, 9.950000000011137047, -180.1323371927318533 ) ) ;
#187781 = ADVANCED_FACE ( 'NONE', ( #8004 ), #244020, .T. ) ;
#187780 = DIRECTION ( 'NONE',  ( 1.000000000000000000, 0.000000000000000000, 0.000000000000000000 ) ) ;
#187783 = EDGE_LOOP ( 'NONE', ( #166953, #252446, #116635, #54544 ) ) ;
#187782 = ORIENTED_EDGE ( 'NONE', *, *, #135640, .T. ) ;
#187784 = ORIENTED_EDGE ( 'NONE', *, *, #219413, .T. ) ;
#187785 = DIRECTION ( 'NONE',  ( -3.469446951953677298E-14, -0.9908441862701782288, -0.1350103645450542456 ) ) ;
#187786 = ORIENTED_EDGE ( 'NONE', *, *, #36816, .T. ) ;
#187787 = EDGE_LOOP ( 'NONE', ( #173829, #165773, #177029, #43533 ) ) ;
#187788 = CARTESIAN_POINT ( 'NONE',  ( -20.07928932188135107, 9.220710678129810489, -79.35000000000005116 ) ) ;
#187789 = AXIS2_PLACEMENT_3D ( 'NONE', #243978, #87463, #83589 ) ;
#187792 = EDGE_CURVE ( 'NONE', #5771, #63364, #45829, .T. ) ;
#187791 = EDGE_LOOP ( 'NONE', ( #95239, #39178, #210843, #147833 ) ) ;
#187790 = LINE ( 'NONE', #106938, #60062 ) ;
#187793 = DIRECTION ( 'NONE',  ( 1.000000000000000000, 0.000000000000000000, 0.000000000000000000 ) ) ;
#187795 = DIRECTION ( 'NONE',  ( 0.000000000000000000, 0.000000000000000000, -1.000000000000000000 ) ) ;
#187794 = FACE_OUTER_BOUND ( 'NONE', #29885, .T. ) ;
#187796 = CARTESIAN_POINT ( 'NONE',  ( 21.05000000000000071, 44.18518595211054389, -258.7688298343402380 ) ) ;
#187797 = CARTESIAN_POINT ( 'NONE',  ( -12.25000000000000178, 62.59162599727320497, -217.2417264603073477 ) ) ;
#187798 = ORIENTED_EDGE ( 'NONE', *, *, #192949, .F. ) ;
#187799 = EDGE_CURVE ( 'NONE', #161314, #141916, #102381, .T. ) ;
#187800 = ORIENTED_EDGE ( 'NONE', *, *, #3966, .T. ) ;
#187801 = DIRECTION ( 'NONE',  ( 0.000000000000000000, 0.000000000000000000, -1.000000000000000000 ) ) ;
#187802 = DIRECTION ( 'NONE',  ( -0.000000000000000000, -0.9121259477928193027, 0.4099100576505185778 ) ) ;
#187803 = EDGE_CURVE ( 'NONE', #135750, #115507, #14951, .T. ) ;
#187805 = ORIENTED_EDGE ( 'NONE', *, *, #6174, .F. ) ;
#187804 = AXIS2_PLACEMENT_3D ( 'NONE', #121903, #3201, #22814 ) ;
#187806 = AXIS2_PLACEMENT_3D ( 'NONE', #140858, #176148, #80855 ) ;
#187807 = EDGE_CURVE ( 'NONE', #239082, #165621, #248175, .T. ) ;
#187808 = CIRCLE ( 'NONE', #254392, 0.1000000000000028644 ) ;
#187809 = DIRECTION ( 'NONE',  ( 1.000000000000000000, 0.000000000000000000, -0.000000000000000000 ) ) ;
#187811 = EDGE_CURVE ( 'NONE', #224621, #21018, #256478, .T. ) ;
#187810 = ADVANCED_FACE ( 'NONE', ( #175749 ), #108763, .T. ) ;
#187812 = ORIENTED_EDGE ( 'NONE', *, *, #12986, .F. ) ;
#187813 = ORIENTED_EDGE ( 'NONE', *, *, #171447, .T. ) ;
#187814 = TOROIDAL_SURFACE ( 'NONE', #75396, 0.2000000000000000111, 0.1000000000000000056 ) ;
#187815 = CARTESIAN_POINT ( 'NONE',  ( -20.94999999999999929, 64.25000000001264766, -196.5083017138704236 ) ) ;
#187816 = CARTESIAN_POINT ( 'NONE',  ( -5.900000000000003020, -11.65000000000000036, 9.900000000000002132 ) ) ;
#187817 = ORIENTED_EDGE ( 'NONE', *, *, #213375, .F. ) ;
#187818 = SPHERICAL_SURFACE ( 'NONE', #209708, 0.1000000000000000056 ) ;
#187819 = DIRECTION ( 'NONE',  ( -1.000000000000000000, 0.000000000000000000, 0.000000000000000000 ) ) ;
#187820 = VERTEX_POINT ( 'NONE', #196563 ) ;
#187821 = AXIS2_PLACEMENT_3D ( 'NONE', #89599, #90893, #149615 ) ;
#187822 = CYLINDRICAL_SURFACE ( 'NONE', #31442, 0.1000000000000028644 ) ;
#187824 = AXIS2_PLACEMENT_3D ( 'NONE', #63509, #179640, #81765 ) ;
#187823 = CARTESIAN_POINT ( 'NONE',  ( 20.85000000000000142, 77.83585931145526615, -58.01866831572577610 ) ) ;
#187825 = CARTESIAN_POINT ( 'NONE',  ( -21.05000000000000426, 6.332272273946816910, -67.03753606328571379 ) ) ;
#187826 = DIRECTION ( 'NONE',  ( -1.000000000000000000, 0.000000000000000000, 0.000000000000000000 ) ) ;
#187827 = DIRECTION ( 'NONE',  ( 0.000000000000000000, 0.4721928772777330696, 0.8814952561688438326 ) ) ;
#187828 = DIRECTION ( 'NONE',  ( 0.000000000000000000, -1.000000000000000000, 0.000000000000000000 ) ) ;
#187829 = CARTESIAN_POINT ( 'NONE',  ( -20.85000000000000142, 67.23127455305835554, -235.8551265064784559 ) ) ;
#187830 = ORIENTED_EDGE ( 'NONE', *, *, #211313, .T. ) ;
#187831 = VECTOR ( 'NONE', #185962, 1000.000000000000114 ) ;
#187832 = EDGE_CURVE ( 'NONE', #106227, #151804, #131460, .T. ) ;
#187834 = ADVANCED_FACE ( 'NONE', ( #77894 ), #98711, .T. ) ;
#187833 = CIRCLE ( 'NONE', #75410, 0.1000000000000028644 ) ;
#187835 = CIRCLE ( 'NONE', #212945, 0.09999999999999414912 ) ;
#187836 = AXIS2_PLACEMENT_3D ( 'NONE', #123393, #4700, #41315 ) ;
#187837 = AXIS2_PLACEMENT_3D ( 'NONE', #77906, #194043, #117053 ) ;
#187839 = ORIENTED_EDGE ( 'NONE', *, *, #206611, .T. ) ;
#187838 = ORIENTED_EDGE ( 'NONE', *, *, #52177, .T. ) ;
#187840 = ORIENTED_EDGE ( 'NONE', *, *, #24625, .T. ) ;
#187841 = EDGE_CURVE ( 'NONE', #250872, #160823, #119179, .T. ) ;
#187842 = DIRECTION ( 'NONE',  ( 0.000000000000000000, 0.000000000000000000, -1.000000000000000000 ) ) ;
#187844 = CARTESIAN_POINT ( 'NONE',  ( -23.25000000000000000, -1.851617760457748618, -179.1031897196036766 ) ) ;
#187843 = CARTESIAN_POINT ( 'NONE',  ( -16.87331047859651179, 66.05000000001187743, -90.37310748452438247 ) ) ;
#187845 = DIRECTION ( 'NONE',  ( 0.000000000000000000, 6.982962677686266711E-15, -1.000000000000000000 ) ) ;
#187846 = ORIENTED_EDGE ( 'NONE', *, *, #253487, .T. ) ;
#187847 = CARTESIAN_POINT ( 'NONE',  ( 18.50000000000000000, 85.40000000001208491, -129.6410656363516125 ) ) ;
#187848 = ADVANCED_FACE ( 'NONE', ( #178320 ), #44368, .T. ) ;
#187849 = AXIS2_PLACEMENT_3D ( 'NONE', #250298, #71684, #151211 ) ;
#187850 = ORIENTED_EDGE ( 'NONE', *, *, #161425, .F. ) ;
#187851 = CYLINDRICAL_SURFACE ( 'NONE', #100160, 0.09999999999999939493 ) ;
#187852 = CARTESIAN_POINT ( 'NONE',  ( -14.00000000000000178, 62.10905854918435409, -217.1108499610990918 ) ) ;
#187853 = EDGE_CURVE ( 'NONE', #1289, #139208, #185805, .T. ) ;
#187854 = ORIENTED_EDGE ( 'NONE', *, *, #22755, .F. ) ;
#187855 = DIRECTION ( 'NONE',  ( 1.000000000000000000, 0.000000000000000000, 0.000000000000000000 ) ) ;
#187856 = FACE_OUTER_BOUND ( 'NONE', #118514, .T. ) ;
#187857 = ORIENTED_EDGE ( 'NONE', *, *, #83693, .F. ) ;
#187858 = ORIENTED_EDGE ( 'NONE', *, *, #66330, .T. ) ;
#187859 = DIRECTION ( 'NONE',  ( 0.000000000000000000, 1.000000000000000000, 7.272083257015735086E-15 ) ) ;
#187860 = CARTESIAN_POINT ( 'NONE',  ( -21.07928932188134041, 1.596973512272247042, -230.6572452218044020 ) ) ;
#187861 = LINE ( 'NONE', #48324, #65409 ) ;
#187862 = EDGE_CURVE ( 'NONE', #103692, #250290, #51636, .T. ) ;
#187863 = DIRECTION ( 'NONE',  ( 0.000000000000000000, -1.000000000000000000, -0.000000000000000000 ) ) ;
#187864 = PLANE ( 'NONE',  #98374 ) ;
#187865 = CARTESIAN_POINT ( 'NONE',  ( -21.05000000000000071, 6.540656951701244282, -0.09999999999999939493 ) ) ;
#187866 = ORIENTED_EDGE ( 'NONE', *, *, #201903, .F. ) ;
#187867 = CYLINDRICAL_SURFACE ( 'NONE', #38120, 0.09999999999999939493 ) ;
#187868 = CIRCLE ( 'NONE', #96243, 0.1000000000000052097 ) ;
#187869 = CARTESIAN_POINT ( 'NONE',  ( -23.15000000000000213, 76.00000000001237765, -170.0231074845243597 ) ) ;
#187870 = FACE_OUTER_BOUND ( 'NONE', #97346, .T. ) ;
#187871 = DIRECTION ( 'NONE',  ( -0.000000000000000000, -0.8814952561688430555, 0.4721928772777346239 ) ) ;
#187873 = EDGE_CURVE ( 'NONE', #129900, #162791, #160886, .T. ) ;
#187872 = DIRECTION ( 'NONE',  ( -0.000000000000000000, 1.000000000000000000, -0.000000000000000000 ) ) ;
#187874 = DIRECTION ( 'NONE',  ( 0.000000000000000000, 6.982962677686266711E-15, -1.000000000000000000 ) ) ;
#187875 = CARTESIAN_POINT ( 'NONE',  ( 20.91682497891423154, 10.32263460347359185, -139.5605957968672328 ) ) ;
#187877 = ORIENTED_EDGE ( 'NONE', *, *, #16461, .T. ) ;
#187876 = DIRECTION ( 'NONE',  ( 1.476360405086644309E-16, -1.000000000000000000, -0.000000000000000000 ) ) ;
#187878 = VECTOR ( 'NONE', #24292, 1000.000000000000000 ) ;
#187879 = EDGE_CURVE ( 'NONE', #201767, #92552, #102567, .T. ) ;
#187880 = DIRECTION ( 'NONE',  ( -1.000000000000000000, 0.000000000000000000, 0.000000000000000000 ) ) ;
#187881 = DIRECTION ( 'NONE',  ( 0.000000000000000000, -1.000000000000000000, 0.000000000000000000 ) ) ;
#187882 = VECTOR ( 'NONE', #218614, 1000.000000000000000 ) ;
#187883 = EDGE_LOOP ( 'NONE', ( #220821, #186492, #143509, #190150 ) ) ;
#187884 = AXIS2_PLACEMENT_3D ( 'NONE', #141596, #20392, #219849 ) ;
#187885 = CYLINDRICAL_SURFACE ( 'NONE', #1613, 0.1000000000000055844 ) ;
#187886 = DIRECTION ( 'NONE',  ( 0.000000000000000000, 0.000000000000000000, 1.000000000000000000 ) ) ;
#187888 = CARTESIAN_POINT ( 'NONE',  ( 22.50000000000000000, 0.000000000000000000, 0.000000000000000000 ) ) ;
#187887 = AXIS2_PLACEMENT_3D ( 'NONE', #131532, #12899, #28639 ) ;
#187889 = VERTEX_POINT ( 'NONE', #114466 ) ;
#187890 = CARTESIAN_POINT ( 'NONE',  ( 21.00000000000000000, 9.750000000011153745, -45.75000000000000711 ) ) ;
#187892 = ORIENTED_EDGE ( 'NONE', *, *, #249335, .T. ) ;
#187891 = FACE_OUTER_BOUND ( 'NONE', #18346, .T. ) ;
#187893 = DIRECTION ( 'NONE',  ( 0.000000000000000000, -1.000000000000000000, -6.982962677686266711E-15 ) ) ;
#187894 = CARTESIAN_POINT ( 'NONE',  ( -17.22361732159832215, 10.34515565861359221, -145.3707845258671512 ) ) ;
#187895 = ORIENTED_EDGE ( 'NONE', *, *, #22600, .F. ) ;
#187896 = CARTESIAN_POINT ( 'NONE',  ( -16.85697194749126382, 66.09145628588898091, -190.5881032169105822 ) ) ;
#187897 = CARTESIAN_POINT ( 'NONE',  ( 0.000000000000000000, 0.000000000000000000, 0.000000000000000000 ) ) ;
#187898 = CARTESIAN_POINT ( 'NONE',  ( -20.94999027547553894, 65.70673848566956110, -64.06382523348288771 ) ) ;
#187899 = CARTESIAN_POINT ( 'NONE',  ( -20.64999999999999858, 85.00000000001159606, -59.62913836187181715 ) ) ;
#187900 = DIRECTION ( 'NONE',  ( 1.000000000000000000, 0.000000000000000000, 0.000000000000000000 ) ) ;
#187901 = CIRCLE ( 'NONE', #21322, 11.65000000000001990 ) ;
#187902 = EDGE_LOOP ( 'NONE', ( #200937, #193961, #251892, #129249 ) ) ;
#187903 = CARTESIAN_POINT ( 'NONE',  ( -21.05000000000000071, 1.835341550224413698, -11.55515129256298401 ) ) ;
#187904 = DIRECTION ( 'NONE',  ( 0.000000000000000000, 6.982962677686266711E-15, -1.000000000000000000 ) ) ;
#187905 = DIRECTION ( 'NONE',  ( 0.000000000000000000, 1.000000000000000000, 6.982962677686266711E-15 ) ) ;
#187906 = VERTEX_POINT ( 'NONE', #194027 ) ;
#187907 = ORIENTED_EDGE ( 'NONE', *, *, #110912, .T. ) ;
#187908 = DIRECTION ( 'NONE',  ( 1.000000000000000000, 0.000000000000000000, -0.000000000000000000 ) ) ;
#187909 = DIRECTION ( 'NONE',  ( 0.000000000000000000, -0.9999631594459057471, 0.008583690987121077309 ) ) ;
#187910 = CARTESIAN_POINT ( 'NONE',  ( 18.59999999999999432, 0.4879293624014888198, -209.1697915983179428 ) ) ;
#187911 = AXIS2_PLACEMENT_3D ( 'NONE', #122903, #23822, #182886 ) ;
#187912 = LINE ( 'NONE', #33694, #187021 ) ;
#187914 = CARTESIAN_POINT ( 'NONE',  ( 21.05000000000000071, 8.776282895303626930, -146.1500000000000341 ) ) ;
#187913 = VECTOR ( 'NONE', #154854, 1000.000000000000000 ) ;
#187916 = EDGE_CURVE ( 'NONE', #55596, #120848, #31903, .T. ) ;
#187915 = AXIS2_PLACEMENT_3D ( 'NONE', #257804, #158790, #238284 ) ;
#187919 = CARTESIAN_POINT ( 'NONE',  ( 22.39999999999999503, -2.479040261793999722, -189.6172560698084624 ) ) ;
#187918 = AXIS2_PLACEMENT_3D ( 'NONE', #20488, #16634, #96134 ) ;
#187917 = DIRECTION ( 'NONE',  ( 0.000000000000000000, 0.000000000000000000, 1.000000000000000000 ) ) ;
#187920 = LINE ( 'NONE', #202331, #10977 ) ;
#187921 = CARTESIAN_POINT ( 'NONE',  ( 19.99999999999998934, 11.75000000001115552, -54.85000000000000142 ) ) ;
#187922 = CARTESIAN_POINT ( 'NONE',  ( -22.48660254037843131, 64.35000000001213039, -136.5731074845243711 ) ) ;
#187924 = VERTEX_POINT ( 'NONE', #16667 ) ;
#187923 = CARTESIAN_POINT ( 'NONE',  ( -21.52071067811865746, 12.10185011759185691, -220.0101306172581417 ) ) ;
#187925 = CARTESIAN_POINT ( 'NONE',  ( 23.15000000000000213, -11.64999999998883595, -197.8999999999999773 ) ) ;
#187926 = CARTESIAN_POINT ( 'NONE',  ( 18.54999999999999716, 8.750000000011182166, -42.75000000000000000 ) ) ;
#187928 = CARTESIAN_POINT ( 'NONE',  ( 23.14999999999999503, 28.95347087985017609, -237.9930060266852081 ) ) ;
#187927 = CARTESIAN_POINT ( 'NONE',  ( 23.14999999999999858, 67.34812900481119868, -214.0300458246130972 ) ) ;
#187929 = EDGE_LOOP ( 'NONE', ( #47228, #17061, #232406, #164472, #112758, #115908, #183675, #68092, #192645, #88897, #213506, #191550 ) ) ;
#187930 = DIRECTION ( 'NONE',  ( 0.000000000000000000, 0.2617529984165027912, 0.9651348961777158619 ) ) ;
#187931 = CARTESIAN_POINT ( 'NONE',  ( -18.34374000495060386, 11.47316190337362585, -109.7500000000000284 ) ) ;
#187932 = CARTESIAN_POINT ( 'NONE',  ( 20.94999999999999929, 6.650000000011155876, -88.25000000000005684 ) ) ;
#187933 = FACE_OUTER_BOUND ( 'NONE', #204703, .T. ) ;
#187934 = CARTESIAN_POINT ( 'NONE',  ( 22.59066674512260064, 12.65021040783260275, -223.3607282225494544 ) ) ;
#187935 = ORIENTED_EDGE ( 'NONE', *, *, #221241, .T. ) ;
#187937 = ORIENTED_EDGE ( 'NONE', *, *, #160584, .F. ) ;
#187936 = AXIS2_PLACEMENT_3D ( 'NONE', #211004, #173207, #76612 ) ;
#187938 = EDGE_CURVE ( 'NONE', #50174, #94619, #198284, .T. ) ;
#187939 = DIRECTION ( 'NONE',  ( 0.000000000000000000, 0.4088369013363276072, -0.9126074666063773710 ) ) ;
#187940 = ORIENTED_EDGE ( 'NONE', *, *, #80906, .F. ) ;
#187941 = DIRECTION ( 'NONE',  ( 1.000000000000000000, 0.000000000000000000, 0.000000000000000000 ) ) ;
#187942 = VERTEX_POINT ( 'NONE', #42628 ) ;
#187943 = DIRECTION ( 'NONE',  ( -0.000000000000000000, 0.8660254037844502539, 0.4999999999999799605 ) ) ;
#187944 = LINE ( 'NONE', #84943, #23516 ) ;
#187945 = EDGE_CURVE ( 'NONE', #188576, #192766, #190106, .T. ) ;
#187947 = EDGE_CURVE ( 'NONE', #147639, #118755, #244237, .T. ) ;
#187946 = DIRECTION ( 'NONE',  ( 0.000000000000000000, -0.000000000000000000, -1.000000000000000000 ) ) ;
#187948 = EDGE_LOOP ( 'NONE', ( #32505, #32938, #136037, #131348 ) ) ;
#187949 = CIRCLE ( 'NONE', #171240, 0.1000000000000028644 ) ;
#187950 = EDGE_CURVE ( 'NONE', #12008, #20238, #23092, .T. ) ;
#187951 = CARTESIAN_POINT ( 'NONE',  ( -21.05000000000000071, 1.115600667400684642E-11, -62.90000000000001279 ) ) ;
#187952 = CARTESIAN_POINT ( 'NONE',  ( 21.14999999999999503, -0.09999999998884338825, -88.85042919245522341 ) ) ;
#187953 = DIRECTION ( 'NONE',  ( 0.000000000000000000, -7.487053152578127080E-15, 1.000000000000000000 ) ) ;
#187954 = CARTESIAN_POINT ( 'NONE',  ( -19.89999999999999858, 1.350000000000000089, 16.60000000000000142 ) ) ;
#187955 = FACE_OUTER_BOUND ( 'NONE', #173627, .T. ) ;
#187956 = EDGE_CURVE ( 'NONE', #163426, #127360, #81717, .T. ) ;
#187958 = CARTESIAN_POINT ( 'NONE',  ( 21.05095171578076574, 11.16407634812396488, -211.0196409686826371 ) ) ;
#187957 = CIRCLE ( 'NONE', #50553, 0.1000000000000021844 ) ;
#187959 = EDGE_LOOP ( 'NONE', ( #104636, #238181, #124236, #212167 ) ) ;
#187961 = FACE_OUTER_BOUND ( 'NONE', #85084, .T. ) ;
#187960 = LINE ( 'NONE', #84963, #53557 ) ;
#187962 = ORIENTED_EDGE ( 'NONE', *, *, #216663, .T. ) ;
#187964 = ORIENTED_EDGE ( 'NONE', *, *, #160385, .T. ) ;
#187963 = DIRECTION ( 'NONE',  ( 0.000000000000000000, 0.000000000000000000, -1.000000000000000000 ) ) ;
#187965 = ORIENTED_EDGE ( 'NONE', *, *, #210127, .T. ) ;
#187966 = CYLINDRICAL_SURFACE ( 'NONE', #103195, 0.1000000000000028644 ) ;
#187967 = TOROIDAL_SURFACE ( 'NONE', #117036, 11.65000000000000036, 0.1000000000000000056 ) ;
#187968 = EDGE_CURVE ( 'NONE', #34543, #74336, #60899, .T. ) ;
#187969 = CARTESIAN_POINT ( 'NONE',  ( 12.33938619321247998, 66.63927620602625268, -152.7091802899177537 ) ) ;
#187970 = DIRECTION ( 'NONE',  ( 0.000000000000000000, -6.982962677686266711E-15, 1.000000000000000000 ) ) ;
#187971 = CARTESIAN_POINT ( 'NONE',  ( -21.45000000000000284, 68.29142135624991283, -191.1731074845243938 ) ) ;
#187972 = AXIS2_PLACEMENT_3D ( 'NONE', #6342, #143294, #84559 ) ;
#187973 = ORIENTED_EDGE ( 'NONE', *, *, #246333, .F. ) ;
#187974 = CARTESIAN_POINT ( 'NONE',  ( 21.05000000000000071, 63.67931791018308019, -224.6923787560153585 ) ) ;
#187975 = CARTESIAN_POINT ( 'NONE',  ( 18.49999999999999289, 10.23906162413259402, -158.7543974345976494 ) ) ;
#187976 = B_SPLINE_CURVE_WITH_KNOTS ( 'NONE', 3,
 ( #257482, #73800, #38506, #54195, #213268, #15091, #256187, #34667, #234119, #77593, #114177, #94605, #253675, #75086 ),
 .UNSPECIFIED., .F., .F.,
 ( 4, 2, 2, 2, 2, 2, 4 ),
 ( 0.000000000000000000, 2.389617747645373272E-05, 4.779235495290746544E-05, 9.558470990578175430E-05, 0.0001911694198114850666, 0.0003823388396228845354, 0.0007646776792456835272 ),
 .UNSPECIFIED. ) ;
#187977 = VERTEX_POINT ( 'NONE', #140433 ) ;
#187979 = EDGE_CURVE ( 'NONE', #94336, #181665, #180868, .T. ) ;
#187978 = CARTESIAN_POINT ( 'NONE',  ( 18.48536876927993333, -9.463527249856051426, -174.5486182650826095 ) ) ;
#187980 = LINE ( 'NONE', #112298, #9930 ) ;
#187981 = AXIS2_PLACEMENT_3D ( 'NONE', #36627, #195694, #96538 ) ;
#187982 = ORIENTED_EDGE ( 'NONE', *, *, #63465, .F. ) ;
#187983 = DIRECTION ( 'NONE',  ( 0.000000000000000000, 0.000000000000000000, -1.000000000000000000 ) ) ;
#187984 = VECTOR ( 'NONE', #142130, 1000.000000000000000 ) ;
#187985 = ORIENTED_EDGE ( 'NONE', *, *, #229853, .T. ) ;
#187986 = FACE_OUTER_BOUND ( 'NONE', #167143, .T. ) ;
#187987 = ORIENTED_EDGE ( 'NONE', *, *, #202572, .T. ) ;
#187988 = CARTESIAN_POINT ( 'NONE',  ( 20.85000000000000142, -1.835859311432481045, -145.5044391687985694 ) ) ;
#187989 = CIRCLE ( 'NONE', #208830, 0.09999999999999939493 ) ;
#187990 = FACE_OUTER_BOUND ( 'NONE', #54778, .T. ) ;
#187991 = VECTOR ( 'NONE', #183184, 1000.000000000000000 ) ;
#187992 = DIRECTION ( 'NONE',  ( -0.000000000000000000, 7.172728831056617961E-15, -1.000000000000000000 ) ) ;
#187993 = DIRECTION ( 'NONE',  ( 0.000000000000000000, 0.000000000000000000, -1.000000000000000000 ) ) ;
#187994 = CARTESIAN_POINT ( 'NONE',  ( 18.49999999999999645, 1.162701749949165642, -41.60000000000000142 ) ) ;
#187995 = CIRCLE ( 'NONE', #212943, 0.09999999999999939493 ) ;
#187996 = ORIENTED_EDGE ( 'NONE', *, *, #86685, .T. ) ;
#187998 = DIRECTION ( 'NONE',  ( -1.000000000000000000, -0.000000000000000000, -0.000000000000000000 ) ) ;
#187997 = CIRCLE ( 'NONE', #137897, 0.1000000000000013933 ) ;
#187999 = CIRCLE ( 'NONE', #129725, 0.09999999999999939493 ) ;
#188000 = ORIENTED_EDGE ( 'NONE', *, *, #206805, .F. ) ;
#188002 = LINE ( 'NONE', #9345, #241962 ) ;
#188001 = CARTESIAN_POINT ( 'NONE',  ( -21.05000000000000071, 69.69503888732782571, -170.0017219185873216 ) ) ;
#188003 = AXIS2_PLACEMENT_3D ( 'NONE', #145582, #106435, #209412 ) ;
#188004 = EDGE_CURVE ( 'NONE', #47344, #249899, #219119, .T. ) ;
#188005 = EDGE_LOOP ( 'NONE', ( #114832, #98132, #177823, #201887, #185733 ) ) ;
#188006 = CARTESIAN_POINT ( 'NONE',  ( -17.04761207306820125, 10.02645087340892971, -46.15000000000000568 ) ) ;
#188007 = DIRECTION ( 'NONE',  ( 1.000000000000000000, 0.000000000000000000, 0.000000000000000000 ) ) ;
#188008 = DIRECTION ( 'NONE',  ( 1.000000000000000000, 0.000000000000000000, 0.000000000000000000 ) ) ;
#188009 = ORIENTED_EDGE ( 'NONE', *, *, #242721, .F. ) ;
#188011 = EDGE_LOOP ( 'NONE', ( #199253, #178274, #84147, #240211 ) ) ;
#188010 = FACE_OUTER_BOUND ( 'NONE', #176811, .T. ) ;
#188012 = ADVANCED_FACE ( 'NONE', ( #141722 ), #102566, .F. ) ;
#188015 = EDGE_CURVE ( 'NONE', #142715, #108824, #243390, .T. ) ;
#188014 = CARTESIAN_POINT ( 'NONE',  ( 20.99999999999999645, 66.25000000001230660, -157.3731074845244393 ) ) ;
#188013 =( BOUNDED_CURVE ( )  B_SPLINE_CURVE ( 3, ( #15228, #138971, #156030, #193857 ),
 .UNSPECIFIED., .F., .F. ) 
 B_SPLINE_CURVE_WITH_KNOTS ( ( 4, 4 ),
 ( 3.752122642744808445, 4.712388980384676351 ),
 .UNSPECIFIED. ) 
 CURVE ( )  GEOMETRIC_REPRESENTATION_ITEM ( )  RATIONAL_B_SPLINE_CURVE ( ( 1.000000000000000000, 0.9246222802177559430, 0.9246222802177559430, 1.000000000000000000 ) ) 
 REPRESENTATION_ITEM ( '' )  );
#188017 = CARTESIAN_POINT ( 'NONE',  ( 18.49999999999999289, 15.27230207784559113, -223.0085293587735009 ) ) ;
#188016 = CYLINDRICAL_SURFACE ( 'NONE', #51120, 0.09999999999999939493 ) ;
#188019 = ORIENTED_EDGE ( 'NONE', *, *, #229562, .T. ) ;
#188018 = CARTESIAN_POINT ( 'NONE',  ( -16.88005004766534967, 9.950100503332199864, -154.8503361119487920 ) ) ;
#188020 = EDGE_CURVE ( 'NONE', #101319, #43432, #256674, .T. ) ;
#188021 = ORIENTED_EDGE ( 'NONE', *, *, #195901, .T. ) ;
#188022 = EDGE_CURVE ( 'NONE', #83334, #67212, #182151, .T. ) ;
#188023 = EDGE_CURVE ( 'NONE', #186298, #82173, #2644, .T. ) ;
#188024 = CARTESIAN_POINT ( 'NONE',  ( 20.95512820512820795, 10.62384868372303615, -179.7001620194243969 ) ) ;
#188025 = DIRECTION ( 'NONE',  ( 0.000000000000000000, 0.000000000000000000, -1.000000000000000000 ) ) ;
#188026 = ORIENTED_EDGE ( 'NONE', *, *, #83471, .T. ) ;
#188027 = DIRECTION ( 'NONE',  ( 1.000000000000000000, 5.204170427930452838E-14, 0.000000000000000000 ) ) ;
#188028 = ORIENTED_EDGE ( 'NONE', *, *, #139969, .F. ) ;
#188029 = EDGE_CURVE ( 'NONE', #199333, #236302, #169292, .T. ) ;
#188030 = CARTESIAN_POINT ( 'NONE',  ( -23.25000000000000000, -11.64999999998884483, -88.75000000000004263 ) ) ;
#188031 = CARTESIAN_POINT ( 'NONE',  ( 21.14999999999999858, 10.21728496540352360, -227.9671432372868765 ) ) ;
#188032 = EDGE_LOOP ( 'NONE', ( #122649, #5922, #248239, #44723 ) ) ;
#188033 = FACE_OUTER_BOUND ( 'NONE', #25715, .T. ) ;
#188034 = VECTOR ( 'NONE', #85389, 1000.000000000000000 ) ;
#188035 = ORIENTED_EDGE ( 'NONE', *, *, #20023, .T. ) ;
#188036 = EDGE_CURVE ( 'NONE', #113184, #202471, #56779, .T. ) ;
#188037 = CARTESIAN_POINT ( 'NONE',  ( 21.11927991906888025, 6.298860988841674668, -199.6188786237795796 ) ) ;
#188038 =( BOUNDED_CURVE ( )  B_SPLINE_CURVE ( 3, ( #14769, #57697, #34332, #254604 ),
 .UNSPECIFIED., .F., .T. ) 
 B_SPLINE_CURVE_WITH_KNOTS ( ( 4, 4 ),
 ( 1.570796326794908992, 2.617993877991413587 ),
 .UNSPECIFIED. ) 
 CURVE ( )  GEOMETRIC_REPRESENTATION_ITEM ( )  RATIONAL_B_SPLINE_CURVE ( ( 1.000000000000000000, 0.9106836025229745335, 0.9106836025229745335, 1.000000000000000000 ) ) 
 REPRESENTATION_ITEM ( '' )  );
#188039 = EDGE_CURVE ( 'NONE', #112979, #13011, #181718, .T. ) ;
#188041 = EDGE_LOOP ( 'NONE', ( #17373, #242783, #142234 ) ) ;
#188040 = CIRCLE ( 'NONE', #129765, 0.1000000000000028644 ) ;
#188042 = ORIENTED_EDGE ( 'NONE', *, *, #223125, .F. ) ;
#188043 = DIRECTION ( 'NONE',  ( 1.000000000000000000, 0.000000000000000000, 0.000000000000000000 ) ) ;
#188044 = ORIENTED_EDGE ( 'NONE', *, *, #173862, .F. ) ;
#188045 = CARTESIAN_POINT ( 'NONE',  ( -16.80100426158792715, 23.00387470889453567, -230.9566579447254355 ) ) ;
#188046 = ORIENTED_EDGE ( 'NONE', *, *, #213514, .T. ) ;
#188047 = VERTEX_POINT ( 'NONE', #64754 ) ;
#188048 = EDGE_CURVE ( 'NONE', #26389, #38279, #25638, .T. ) ;
#188049 = ADVANCED_FACE ( 'NONE', ( #142985 ), #222528, .F. ) ;
#188050 = CARTESIAN_POINT ( 'NONE',  ( -20.97625342178416474, 11.60000000083146077, -73.92820322980200842 ) ) ;
#188051 = ORIENTED_EDGE ( 'NONE', *, *, #28797, .T. ) ;
#188052 = FACE_OUTER_BOUND ( 'NONE', #52966, .T. ) ;
#188053 = EDGE_LOOP ( 'NONE', ( #175110, #233339, #207779, #253842 ) ) ;
#188056 = ORIENTED_EDGE ( 'NONE', *, *, #95903, .T. ) ;
#188055 = ORIENTED_EDGE ( 'NONE', *, *, #59341, .T. ) ;
#188054 = LINE ( 'NONE', #88926, #97751 ) ;
#188057 = CARTESIAN_POINT ( 'NONE',  ( -23.24999999999999645, -0.8254770802754692882, -242.3223161824233500 ) ) ;
#188058 = AXIS2_PLACEMENT_3D ( 'NONE', #199075, #79100, #180802 ) ;
#188059 = ORIENTED_EDGE ( 'NONE', *, *, #204232, .T. ) ;
#188060 = AXIS2_PLACEMENT_3D ( 'NONE', #39138, #254288, #139480 ) ;
#188061 = ORIENTED_EDGE ( 'NONE', *, *, #157097, .F. ) ;
#188062 = CARTESIAN_POINT ( 'NONE',  ( -23.25000000000000000, 87.65000000001195701, -103.0231074845242318 ) ) ;
#188063 = CARTESIAN_POINT ( 'NONE',  ( 20.84999999999998721, 87.34033503009941057, -206.5987052159188124 ) ) ;
#188065 = ORIENTED_EDGE ( 'NONE', *, *, #124429, .F. ) ;
#188064 = DIRECTION ( 'NONE',  ( -0.000000000000000000, 1.000000000000000000, -0.000000000000000000 ) ) ;
#188066 = CARTESIAN_POINT ( 'NONE',  ( -0.8999999999999993561, -11.65000000000000036, 26.00000000000000355 ) ) ;
#188067 = ORIENTED_EDGE ( 'NONE', *, *, #239684, .F. ) ;
#188068 = DIRECTION ( 'NONE',  ( -0.000000000000000000, 6.982962677686266711E-15, -1.000000000000000000 ) ) ;
#188069 = DIRECTION ( 'NONE',  ( 0.000000000000000000, -0.8814952561688430555, 0.4721928772777346239 ) ) ;
#188070 = ORIENTED_EDGE ( 'NONE', *, *, #4367, .T. ) ;
#188071 = DIRECTION ( 'NONE',  ( -1.000000000000000000, 0.000000000000000000, -0.000000000000000000 ) ) ;
#188072 = LINE ( 'NONE', #68123, #65725 ) ;
#188073 = VECTOR ( 'NONE', #130169, 1000.000000000000000 ) ;
#188074 = ORIENTED_EDGE ( 'NONE', *, *, #197799, .T. ) ;
#188076 = ORIENTED_EDGE ( 'NONE', *, *, #72504, .F. ) ;
#188075 = DIRECTION ( 'NONE',  ( -1.000000000000000000, 0.000000000000000000, 0.000000000000000000 ) ) ;
#188077 = FACE_OUTER_BOUND ( 'NONE', #81799, .T. ) ;
#188079 = ORIENTED_EDGE ( 'NONE', *, *, #211233, .F. ) ;
#188078 = EDGE_LOOP ( 'NONE', ( #39986, #135085, #172294, #193784 ) ) ;
#188080 = ORIENTED_EDGE ( 'NONE', *, *, #135709, .F. ) ;
#188081 = DIRECTION ( 'NONE',  ( -1.000000000000000000, 0.000000000000000000, 0.000000000000000000 ) ) ;
#188082 = ORIENTED_EDGE ( 'NONE', *, *, #113805, .T. ) ;
#188083 = ORIENTED_EDGE ( 'NONE', *, *, #41153, .T. ) ;
#188084 = FACE_OUTER_BOUND ( 'NONE', #34774, .T. ) ;
#188085 = ORIENTED_EDGE ( 'NONE', *, *, #102947, .F. ) ;
#188086 = CARTESIAN_POINT ( 'NONE',  ( -23.39999999999994529, 87.50449464844290048, -34.18759587077607165 ) ) ;
#188087 = CYLINDRICAL_SURFACE ( 'NONE', #85745, 0.1000000000000028644 ) ;
#188088 = VERTEX_POINT ( 'NONE', #223816 ) ;
#188089 = EDGE_CURVE ( 'NONE', #253449, #57651, #210947, .T. ) ;
#188090 = CIRCLE ( 'NONE', #59049, 0.09999999999999982514 ) ;
#188091 = VECTOR ( 'NONE', #63442, 1000.000000000000000 ) ;
#188092 = ORIENTED_EDGE ( 'NONE', *, *, #64924, .F. ) ;
#188093 = PLANE ( 'NONE',  #204705 ) ;
#188094 = ADVANCED_FACE ( 'NONE', ( #105123 ), #89446, .F. ) ;
#188095 = EDGE_LOOP ( 'NONE', ( #78398, #242537, #59281, #216911, #227505, #249529, #202083, #27101, #169113, #175254, #21847, #18473, #140491, #198795, #154059, #63723, #237644, #256538, #51124, #186914, #132515, #112402, #159503 ) ) ;
#188096 = EDGE_CURVE ( 'NONE', #146711, #190547, #208144, .T. ) ;
#188097 = DIRECTION ( 'NONE',  ( -0.8660254037844653530, 0.000000000000000000, -0.4999999999999539257 ) ) ;
#188098 = EDGE_CURVE ( 'NONE', #168984, #50990, #150722, .T. ) ;
#188099 = ORIENTED_EDGE ( 'NONE', *, *, #14754, .T. ) ;
#188100 = CARTESIAN_POINT ( 'NONE',  ( -23.25000000000000000, 87.75000000001142553, -36.02310748452423894 ) ) ;
#188102 = ORIENTED_EDGE ( 'NONE', *, *, #214860, .T. ) ;
#188101 = FACE_OUTER_BOUND ( 'NONE', #184882, .T. ) ;
#188103 = DIRECTION ( 'NONE',  ( 0.000000000000000000, 0.000000000000000000, -1.000000000000000000 ) ) ;
#188104 = DIRECTION ( 'NONE',  ( -0.7071067811865456854, -0.6824534298470390503, 0.1850873201762214815 ) ) ;
#188105 = DIRECTION ( 'NONE',  ( 0.1538461538461484146, -0.9880948137434723000, 0.000000000000000000 ) ) ;
#188106 = VECTOR ( 'NONE', #231543, 1000.000000000000000 ) ;
#188107 = CARTESIAN_POINT ( 'NONE',  ( -23.15000000000000213, 85.50000000001232081, -160.1291383618718385 ) ) ;
#188109 = DIRECTION ( 'NONE',  ( 0.000000000000000000, 0.000000000000000000, 1.000000000000000000 ) ) ;
#188108 = DIRECTION ( 'NONE',  ( 1.000000000000000000, -3.265361837132813093E-16, -2.280189983783949500E-30 ) ) ;
#188110 = FACE_OUTER_BOUND ( 'NONE', #135357, .T. ) ;
#188111 = CARTESIAN_POINT ( 'NONE',  ( 22.40000000000010516, 76.00000000001340084, -181.7735403769832772 ) ) ;
#188112 = DIRECTION ( 'NONE',  ( 0.000000000000000000, 0.8700118002898321601, -0.4930308989875230030 ) ) ;
#188113 = ORIENTED_EDGE ( 'NONE', *, *, #16764, .F. ) ;
#188114 = EDGE_CURVE ( 'NONE', #127762, #56976, #7351, .T. ) ;
#188115 = ORIENTED_EDGE ( 'NONE', *, *, #87991, .T. ) ;
#188117 = EDGE_LOOP ( 'NONE', ( #101819, #11115, #75458, #237676 ) ) ;
#188116 = DIRECTION ( 'NONE',  ( 0.000000000000000000, -0.4791956752371546169, -0.8777080977375152360 ) ) ;
#188118 = ORIENTED_EDGE ( 'NONE', *, *, #149373, .F. ) ;
#188119 = B_SPLINE_CURVE_WITH_KNOTS ( 'NONE', 3,
 ( #56501, #78638, #180332, #95640, #139893, #96895, #218144, #77357, #199908, #198596, #60367, #197307, #38257, #175238, #39569, #119078, #40847, #81199, #235170 ),
 .UNSPECIFIED., .F., .F.,
 ( 4, 3, 3, 3, 3, 3, 4 ),
 ( 0.0001624081864585794055, 0.0001685232196531677375, 0.0001764526673566770378, 0.0001916878551483278104, 0.0002009890782182702088, 0.0002238845907555191150, 0.0002283406619926350520 ),
 .UNSPECIFIED. ) ;
#188120 = DIRECTION ( 'NONE',  ( 0.000000000000000000, 0.9126074666064696306, 0.4088369013361213278 ) ) ;
#188121 = CIRCLE ( 'NONE', #221409, 0.5000000000000013323 ) ;
#188122 = CARTESIAN_POINT ( 'NONE',  ( 20.44999100639894962, 10.43971070322319683, -141.7590757259705470 ) ) ;
#188124 = DIRECTION ( 'NONE',  ( 1.000000000000000000, -3.151514657663852580E-16, 8.547182517843351137E-17 ) ) ;
#188123 = CARTESIAN_POINT ( 'NONE',  ( -21.44999999999999929, 52.95562111564758823, -234.1965973584252652 ) ) ;
#188125 = ORIENTED_EDGE ( 'NONE', *, *, #188694, .F. ) ;
#188126 = VERTEX_POINT ( 'NONE', #107733 ) ;
#188127 =( NAMED_UNIT ( * ) PLANE_ANGLE_UNIT ( ) SI_UNIT ( $, .RADIAN. ) );
#188128 = EDGE_CURVE ( 'NONE', #243786, #20836, #202559, .T. ) ;
#188129 = DIRECTION ( 'NONE',  ( -1.000000000000000000, -0.000000000000000000, -0.000000000000000000 ) ) ;
#188130 = CIRCLE ( 'NONE', #96523, 0.1000000000000028644 ) ;
#188131 = EDGE_CURVE ( 'NONE', #138980, #107290, #231617, .T. ) ;
#188132 = LINE ( 'NONE', #9482, #70730 ) ;
#188133 = ORIENTED_EDGE ( 'NONE', *, *, #178669, .T. ) ;
#188134 = DIRECTION ( 'NONE',  ( 0.000000000000000000, 0.2128009952263485993, -0.9770955615653341697 ) ) ;
#188135 = FACE_OUTER_BOUND ( 'NONE', #186400, .T. ) ;
#188136 = CIRCLE ( 'NONE', #9072, 0.1000000000000028644 ) ;
#188137 = CARTESIAN_POINT ( 'NONE',  ( 20.04142135623730070, 64.35000000001198828, -115.1731074845243796 ) ) ;
#188138 = CARTESIAN_POINT ( 'NONE',  ( 21.05000000000000071, 76.00000000001264766, -199.2231074845243199 ) ) ;
#188139 = VECTOR ( 'NONE', #134000, 1000.000000000000000 ) ;
#188140 = LINE ( 'NONE', #130725, #187039 ) ;
#188142 = ORIENTED_EDGE ( 'NONE', *, *, #55320, .T. ) ;
#188141 = LINE ( 'NONE', #143857, #210271 ) ;
#188143 = CARTESIAN_POINT ( 'NONE',  ( 21.05000000000000071, 5.500000000011153745, -54.59473398108690390 ) ) ;
#188144 = EDGE_CURVE ( 'NONE', #206913, #47775, #89083, .T. ) ;
#188145 = DIRECTION ( 'NONE',  ( 0.000000000000000000, 0.5826443254699606999, 0.8127272543711416830 ) ) ;
#188146 = DIRECTION ( 'NONE',  ( 0.000000000000000000, -1.000000000000000000, -7.105427357601001859E-15 ) ) ;
#188148 = AXIS2_PLACEMENT_3D ( 'NONE', #14019, #89672, #29753 ) ;
#188147 = CARTESIAN_POINT ( 'NONE',  ( 18.50000000000000000, 85.40000000001188596, -95.72584772486098359 ) ) ;
#188149 = VERTEX_POINT ( 'NONE', #245972 ) ;
#188150 = SPHERICAL_SURFACE ( 'NONE', #256832, 0.1000000000000000056 ) ;
#188151 = ADVANCED_FACE ( 'NONE', ( #149457 ), #92020, .F. ) ;
#188152 = LINE ( 'NONE', #43505, #181945 ) ;
#188153 = CIRCLE ( 'NONE', #34244, 0.6000000000000015321 ) ;
#188155 = CARTESIAN_POINT ( 'NONE',  ( 18.49999999999999289, 68.87972903831482085, -166.3635444426850825 ) ) ;
#188154 = DIRECTION ( 'NONE',  ( 1.000000000000000000, 0.000000000000000000, 0.000000000000000000 ) ) ;
#188156 = FACE_OUTER_BOUND ( 'NONE', #82275, .T. ) ;
#188157 = LINE ( 'NONE', #190752, #161827 ) ;
#188159 = EDGE_CURVE ( 'NONE', #66177, #206485, #170330, .T. ) ;
#188158 = VECTOR ( 'NONE', #145630, 1000.000000000000000 ) ;
#188160 = DIRECTION ( 'NONE',  ( -1.020425574104004196E-15, -6.982962677686266711E-15, 1.000000000000000000 ) ) ;
#188161 = PLANE ( 'NONE',  #221375 ) ;
#188162 = CARTESIAN_POINT ( 'NONE',  ( 20.94999999999999929, 76.00000000001259082, -190.5481074845243654 ) ) ;
#188163 = AXIS2_PLACEMENT_3D ( 'NONE', #234179, #114249, #217179 ) ;
#188164 = ORIENTED_EDGE ( 'NONE', *, *, #15827, .F. ) ;
#188165 = ORIENTED_EDGE ( 'NONE', *, *, #188096, .F. ) ;
#188166 = AXIS2_PLACEMENT_3D ( 'NONE', #141689, #122145, #23065 ) ;
#188167 = ORIENTED_EDGE ( 'NONE', *, *, #188663, .F. ) ;
#188168 = CARTESIAN_POINT ( 'NONE',  ( -21.56666275994540172, 1.115600667400684642E-11, -160.5426315931066483 ) ) ;
#188169 = PLANE ( 'NONE',  #119366 ) ;
#188170 = ORIENTED_EDGE ( 'NONE', *, *, #103192, .F. ) ;
#188171 = EDGE_CURVE ( 'NONE', #60084, #80905, #127559, .T. ) ;
#188172 = VECTOR ( 'NONE', #186741, 1000.000000000000000 ) ;
#188173 = ORIENTED_EDGE ( 'NONE', *, *, #16400, .F. ) ;
#188174 = EDGE_CURVE ( 'NONE', #40304, #19526, #48440, .T. ) ;
#188175 = SHAPE_REPRESENTATION_RELATIONSHIP ( 'NONE' , 'NONE' ,  #125202, #14150 ) ;
#188177 = ORIENTED_EDGE ( 'NONE', *, *, #89826, .F. ) ;
#188176 = AXIS2_PLACEMENT_3D ( 'NONE', #253392, #53914, #57746 ) ;
#188178 = CARTESIAN_POINT ( 'NONE',  ( 21.07928932188134397, 75.90110485435735654, -109.3516241409230219 ) ) ;
#188179 = AXIS2_PLACEMENT_3D ( 'NONE', #111911, #171905, #205856 ) ;
#188180 = VERTEX_POINT ( 'NONE', #32080 ) ;
#188181 = AXIS2_PLACEMENT_3D ( 'NONE', #89161, #244381, #145276 ) ;
#188183 = DIRECTION ( 'NONE',  ( 0.000000000000000000, 0.9126074666063660468, 0.4088369013363524762 ) ) ;
#188182 = AXIS2_PLACEMENT_3D ( 'NONE', #183979, #5311, #144840 ) ;
#188184 = CARTESIAN_POINT ( 'NONE',  ( -16.80100914604136264, 30.17404316570091538, -234.7975225174889999 ) ) ;
#188185 = DIRECTION ( 'NONE',  ( 0.000000000000000000, 1.000000000000000000, 0.000000000000000000 ) ) ;
#188186 = CARTESIAN_POINT ( 'NONE',  ( 18.59999999999999076, -1.835859311432481045, -145.6044391687985637 ) ) ;
#188187 = CARTESIAN_POINT ( 'NONE',  ( -20.15000000000000568, 66.70857864377420299, -48.37310748452438247 ) ) ;
#188189 = ORIENTED_EDGE ( 'NONE', *, *, #73844, .F. ) ;
#188188 = CARTESIAN_POINT ( 'NONE',  ( 21.06277459767418136, 44.16883162190262624, -236.4642769761964303 ) ) ;
#188191 = CARTESIAN_POINT ( 'NONE',  ( 21.13461538461538325, 8.885417037985614996, -79.25000000000004263 ) ) ;
#188190 = CARTESIAN_POINT ( 'NONE',  ( -20.94999999999999929, -11.64999999998884483, -36.39999999999999858 ) ) ;
#188192 = CARTESIAN_POINT ( 'NONE',  ( 18.49999999999999289, 65.50857864377445594, -78.17310748452437963 ) ) ;
#188193 = ORIENTED_EDGE ( 'NONE', *, *, #221940, .T. ) ;
#188194 = CARTESIAN_POINT ( 'NONE',  ( -12.25000000000000178, 9.350000000011139178, -117.2500000000000284 ) ) ;
#188195 = DIRECTION ( 'NONE',  ( 0.000000000000000000, -0.5283051335750404975, 0.8490545835446967615 ) ) ;
#188196 = VERTEX_POINT ( 'NONE', #128590 ) ;
#188197 = CARTESIAN_POINT ( 'NONE',  ( -20.85000000000000142, 7.021664781911246322, -137.8335654018973457 ) ) ;
#188198 = DIRECTION ( 'NONE',  ( 0.000000000000000000, 0.000000000000000000, 1.000000000000000000 ) ) ;
#188199 = TOROIDAL_SURFACE ( 'NONE', #246453, 0.2000000000000000111, 0.1000000000000000056 ) ;
#188200 = ORIENTED_EDGE ( 'NONE', *, *, #240302, .T. ) ;
#188201 = FACE_OUTER_BOUND ( 'NONE', #168301, .T. ) ;
#188202 = FACE_OUTER_BOUND ( 'NONE', #135446, .T. ) ;
#188203 = DIRECTION ( 'NONE',  ( 1.000000000000000000, 0.000000000000000000, 0.000000000000000000 ) ) ;
#188204 = DIRECTION ( 'NONE',  ( 1.000000000000000000, 0.000000000000000000, 0.000000000000000000 ) ) ;
#188205 = ORIENTED_EDGE ( 'NONE', *, *, #172679, .T. ) ;
#188206 = ORIENTED_EDGE ( 'NONE', *, *, #172754, .T. ) ;
#188207 = CARTESIAN_POINT ( 'NONE',  ( 23.04999999999999716, 67.17743825834611471, -179.2731074845244166 ) ) ;
#188208 = CARTESIAN_POINT ( 'NONE',  ( -18.50000000000000000, -9.399999999988850163, -174.3820418481726904 ) ) ;
#188209 = DIRECTION ( 'NONE',  ( 1.000000000000000000, 0.000000000000000000, 0.000000000000000000 ) ) ;
#188210 = DIRECTION ( 'NONE',  ( 0.000000000000000000, -0.8814952561688476074, 0.4721928772777262417 ) ) ;
#188211 = EDGE_CURVE ( 'NONE', #122312, #182621, #11029, .T. ) ;
#188212 = DIRECTION ( 'NONE',  ( 0.000000000000000000, 0.000000000000000000, -1.000000000000000000 ) ) ;
#188213 = CARTESIAN_POINT ( 'NONE',  ( -20.54999999999999716, 85.00000000001179501, -79.41707660717668205 ) ) ;
#188214 = CARTESIAN_POINT ( 'NONE',  ( -22.50000000000000000, 31.85509083104287598, -238.8280249686205536 ) ) ;
#188215 = CARTESIAN_POINT ( 'NONE',  ( -23.15000000000000213, 71.85000000001254250, -182.3731074845244109 ) ) ;
#188216 = ORIENTED_EDGE ( 'NONE', *, *, #76576, .F. ) ;
#188217 = PLANE ( 'NONE',  #7661 ) ;
#188218 = AXIS2_PLACEMENT_3D ( 'NONE', #7981, #167080, #246569 ) ;
#188219 = VERTEX_POINT ( 'NONE', #109006 ) ;
#188220 = CARTESIAN_POINT ( 'NONE',  ( 18.49999999999999289, 65.50857864377520912, -178.6731074845244223 ) ) ;
#188221 = CARTESIAN_POINT ( 'NONE',  ( -15.55912972643741199, 8.490870273573719373, -146.5500000000000114 ) ) ;
#188222 = LINE ( 'NONE', #229918, #246177 ) ;
#188223 = CARTESIAN_POINT ( 'NONE',  ( -16.88783316861822215, 66.05000000001207638, -123.7708434425445745 ) ) ;
#188224 = EDGE_CURVE ( 'NONE', #68680, #46322, #156807, .T. ) ;
#188225 = CARTESIAN_POINT ( 'NONE',  ( 21.05000000000000071, 11.75000000001115907, -194.1583993101029080 ) ) ;
#188227 = ORIENTED_EDGE ( 'NONE', *, *, #4897, .F. ) ;
#188226 = CARTESIAN_POINT ( 'NONE',  ( 23.25000000000000000, 30.73962027982165424, -265.0781340245722504 ) ) ;
#188228 = CARTESIAN_POINT ( 'NONE',  ( -16.87036670365548474, 66.01058118071036063, -115.5435473672223168 ) ) ;
#188229 = CARTESIAN_POINT ( 'NONE',  ( -18.53317502108577486, 65.67736539654997330, -164.4625116876572406 ) ) ;
#188230 = LINE ( 'NONE', #47415, #26233 ) ;
#188231 = DIRECTION ( 'NONE',  ( -1.000000000000000000, 0.000000000000000000, -0.000000000000000000 ) ) ;
#188232 = ORIENTED_EDGE ( 'NONE', *, *, #30708, .T. ) ;
#188233 = DIRECTION ( 'NONE',  ( 0.000000000000000000, 0.1332476588733589318, -0.9910827722268049644 ) ) ;
#188234 = EDGE_CURVE ( 'NONE', #172249, #213320, #9919, .T. ) ;
#188236 = EDGE_CURVE ( 'NONE', #254970, #23444, #36177, .T. ) ;
#188235 = VERTEX_POINT ( 'NONE', #67325 ) ;
#188237 = FACE_OUTER_BOUND ( 'NONE', #209663, .T. ) ;
#188239 = AXIS2_PLACEMENT_3D ( 'NONE', #18219, #198132, #217670 ) ;
#188238 = CARTESIAN_POINT ( 'NONE',  ( -16.95709691156456955, 66.05000000001189164, -90.36304992201408481 ) ) ;
#188240 = VERTEX_POINT ( 'NONE', #129855 ) ;
#188241 = CARTESIAN_POINT ( 'NONE',  ( -20.85000000000000142, -1.263275465206102233, -141.9018646667464338 ) ) ;
#188242 = ORIENTED_EDGE ( 'NONE', *, *, #231689, .T. ) ;
#188243 = CIRCLE ( 'NONE', #63317, 0.1000000000000046685 ) ;
#188244 = DIRECTION ( 'NONE',  ( -1.000000000000000000, 0.000000000000000000, -0.000000000000000000 ) ) ;
#188245 = CARTESIAN_POINT ( 'NONE',  ( -23.15000000000000213, -1.269135479188211013, -224.5262296913251987 ) ) ;
#188246 = EDGE_CURVE ( 'NONE', #137467, #193899, #27813, .T. ) ;
#188247 = DIRECTION ( 'NONE',  ( 0.000000000000000000, -0.1568667991644355497, 0.9876197685951332295 ) ) ;
#188248 = ORIENTED_EDGE ( 'NONE', *, *, #53466, .F. ) ;
#188249 = CYLINDRICAL_SURFACE ( 'NONE', #12961, 12.87499999999999822 ) ;
#188250 = CIRCLE ( 'NONE', #67629, 0.1000000000000028644 ) ;
#188251 = CARTESIAN_POINT ( 'NONE',  ( 18.49999999999998934, 6.649999999999999467, -12.35000000000000320 ) ) ;
#188252 = CARTESIAN_POINT ( 'NONE',  ( 22.50497660315937409, -0.07871793022550384322, 11.74979550489544167 ) ) ;
#188253 = FACE_OUTER_BOUND ( 'NONE', #49207, .T. ) ;
#188254 = DIRECTION ( 'NONE',  ( -0.000000000000000000, 0.8814952561688430555, -0.4721928772777346239 ) ) ;
#188255 = ORIENTED_EDGE ( 'NONE', *, *, #12791, .T. ) ;
#188257 = ORIENTED_EDGE ( 'NONE', *, *, #29027, .T. ) ;
#188256 = CARTESIAN_POINT ( 'NONE',  ( -16.27683809663750480, 66.65000000001209912, -127.2731074845243597 ) ) ;
#188258 = ORIENTED_EDGE ( 'NONE', *, *, #217050, .T. ) ;
#188259 = ORIENTED_EDGE ( 'NONE', *, *, #111082, .T. ) ;
#188260 = EDGE_CURVE ( 'NONE', #92812, #171727, #152027, .T. ) ;
#188261 = DIRECTION ( 'NONE',  ( 0.000000000000000000, 0.000000000000000000, -1.000000000000000000 ) ) ;
#188262 = DIRECTION ( 'NONE',  ( 0.000000000000000000, -1.000000000000000000, -6.860497997771531562E-15 ) ) ;
#188263 = DIRECTION ( 'NONE',  ( 0.000000000000000000, 6.467318590049456648E-15, -1.000000000000000000 ) ) ;
#188264 = VERTEX_POINT ( 'NONE', #38477 ) ;
#188265 = FACE_OUTER_BOUND ( 'NONE', #248411, .T. ) ;
#188266 = SPHERICAL_SURFACE ( 'NONE', #201213, 0.1000000000000000056 ) ;
#188267 = CARTESIAN_POINT ( 'NONE',  ( 18.52351027002948669, -9.642162904684020930, -140.7150469505098158 ) ) ;
#188268 = ORIENTED_EDGE ( 'NONE', *, *, #244189, .T. ) ;
#188269 = CARTESIAN_POINT ( 'NONE',  ( -23.15000000000000213, 87.39257802171739797, -72.59705706435616435 ) ) ;
#188271 = EDGE_LOOP ( 'NONE', ( #242525, #195554, #256877, #19335 ) ) ;
#188270 = LINE ( 'NONE', #51298, #155069 ) ;
#188272 = CIRCLE ( 'NONE', #113446, 0.1000000000000054040 ) ;
#188273 = CARTESIAN_POINT ( 'NONE',  ( -21.05000000000000071, 18.27574494880468592, -237.6039235467692947 ) ) ;
#188275 = EDGE_CURVE ( 'NONE', #128415, #28381, #115261, .T. ) ;
#188274 = PLANE ( 'NONE',  #156336 ) ;
#188276 = ORIENTED_EDGE ( 'NONE', *, *, #174249, .F. ) ;
#188277 = CARTESIAN_POINT ( 'NONE',  ( -16.87331047859649757, 9.950000000011138823, -87.85000000000005116 ) ) ;
#188278 = CARTESIAN_POINT ( 'NONE',  ( 21.05000000000000071, 87.65000000001144542, -39.02310748452423894 ) ) ;
#188279 = DIRECTION ( 'NONE',  ( 1.000000000000000000, -1.335000415235278971E-16, 2.979993593738921214E-16 ) ) ;
#188280 = VERTEX_POINT ( 'NONE', #77568 ) ;
#188281 = CARTESIAN_POINT ( 'NONE',  ( 23.14999999999999858, 1.115600667400684642E-11, -67.00000000000000000 ) ) ;
#188282 = CARTESIAN_POINT ( 'NONE',  ( -16.77683809663752257, 9.945835743215303282, -121.3360509808958341 ) ) ;
#188283 = CIRCLE ( 'NONE', #75860, 12.97499999999999964 ) ;
#188284 = ORIENTED_EDGE ( 'NONE', *, *, #44245, .T. ) ;
#188285 = TOROIDAL_SURFACE ( 'NONE', #100762, 0.2000000000000000111, 0.1000000000000000056 ) ;
#188286 = ORIENTED_EDGE ( 'NONE', *, *, #123192, .F. ) ;
#188287 = CARTESIAN_POINT ( 'NONE',  ( 21.07928932188134397, 69.67148334361938566, -203.6220026301787982 ) ) ;
#188288 = EDGE_CURVE ( 'NONE', #185332, #145757, #78858, .T. ) ;
#188289 = EDGE_CURVE ( 'NONE', #43171, #158029, #198465, .T. ) ;
#188290 = ORIENTED_EDGE ( 'NONE', *, *, #35833, .F. ) ;
#188291 = CARTESIAN_POINT ( 'NONE',  ( -18.52139480978222252, -9.481358845055746443, -174.5245565671190491 ) ) ;
#188292 = CARTESIAN_POINT ( 'NONE',  ( -20.64999999999999858, 68.75000000001223555, -148.8731074845244109 ) ) ;
#188293 = AXIS2_PLACEMENT_3D ( 'NONE', #71680, #229454, #110778 ) ;
#188295 = ORIENTED_EDGE ( 'NONE', *, *, #214991, .F. ) ;
#188294 = CARTESIAN_POINT ( 'NONE',  ( 15.75000000000000000, 26.10487691728826221, -233.2906712717672519 ) ) ;
#188296 = CARTESIAN_POINT ( 'NONE',  ( -21.05000000000000071, -1.835341550213255957, -45.05515129256298223 ) ) ;
#188297 = CARTESIAN_POINT ( 'NONE',  ( 21.05000000000000071, 65.27628289530404970, -57.36191719039695158 ) ) ;
#188299 = EDGE_CURVE ( 'NONE', #217297, #137609, #194405, .T. ) ;
#188298 = FACE_OUTER_BOUND ( 'NONE', #220601, .T. ) ;
#188301 = EDGE_CURVE ( 'NONE', #229077, #248144, #257456, .T. ) ;
#188300 = FACE_OUTER_BOUND ( 'NONE', #63966, .T. ) ;
#188302 = CARTESIAN_POINT ( 'NONE',  ( 18.49999999999998934, 10.25000000001115552, -125.2500000000000284 ) ) ;
#188303 = AXIS2_PLACEMENT_3D ( 'NONE', #31071, #170598, #54437 ) ;
#188304 = CYLINDRICAL_SURFACE ( 'NONE', #26618, 0.1000000000000024342 ) ;
#188305 = CARTESIAN_POINT ( 'NONE',  ( -23.25000000000000355, 65.95000000001206786, -123.7731074845243739 ) ) ;
#188307 = VERTEX_POINT ( 'NONE', #217083 ) ;
#188306 = CARTESIAN_POINT ( 'NONE',  ( -20.94999999999999929, -11.29603075033528192, -30.45210084033612929 ) ) ;
#188308 = CARTESIAN_POINT ( 'NONE',  ( 21.05000000000000071, 22.92579362702542412, -230.0293291570564520 ) ) ;
#188309 = AXIS2_PLACEMENT_3D ( 'NONE', #19653, #256916, #116195 ) ;
#188310 = ADVANCED_FACE ( 'NONE', ( #254887 ), #252363, .F. ) ;
#188311 = VECTOR ( 'NONE', #195628, 1000.000000000000000 ) ;
#188312 = AXIS2_PLACEMENT_3D ( 'NONE', #128112, #68135, #70729 ) ;
#188313 = EDGE_CURVE ( 'NONE', #120605, #115342, #144455, .T. ) ;
#188316 = EDGE_CURVE ( 'NONE', #186991, #196305, #52892, .T. ) ;
#188315 = EDGE_CURVE ( 'NONE', #94890, #132176, #172897, .T. ) ;
#188314 = AXIS2_PLACEMENT_3D ( 'NONE', #230560, #210991, #192714 ) ;
#188317 = DIRECTION ( 'NONE',  ( 1.000000000000000000, 0.000000000000000000, 0.000000000000000000 ) ) ;
#188318 = DIRECTION ( 'NONE',  ( 1.000000000000000000, 1.159508501126949537E-16, 2.525285885220369759E-17 ) ) ;
#188319 = EDGE_CURVE ( 'NONE', #138276, #213072, #231807, .T. ) ;
#188320 = FACE_OUTER_BOUND ( 'NONE', #92224, .T. ) ;
#188321 = FACE_OUTER_BOUND ( 'NONE', #214978, .T. ) ;
#188322 = AXIS2_PLACEMENT_3D ( 'NONE', #244591, #201620, #225013 ) ;
#188323 = ORIENTED_EDGE ( 'NONE', *, *, #62942, .F. ) ;
#188324 = CARTESIAN_POINT ( 'NONE',  ( 23.14999999999998437, 1.115600667400684642E-11, -134.0000000000000000 ) ) ;
#188325 = CIRCLE ( 'NONE', #179972, 0.09999999999999939493 ) ;
#188326 = ADVANCED_FACE ( 'NONE', ( #37208 ), #236661, .F. ) ;
#188327 = TOROIDAL_SURFACE ( 'NONE', #75913, 0.4000000000000009104, 0.1000000000000000056 ) ;
#188328 = CIRCLE ( 'NONE', #117606, 0.09999999999998898659 ) ;
#188329 = EDGE_LOOP ( 'NONE', ( #20512, #44239, #100492, #253127 ) ) ;
#188330 = ADVANCED_FACE ( 'NONE', ( #211991, #153328, #114150 ), #234094, .T. ) ;
#188332 = EDGE_CURVE ( 'NONE', #145079, #65805, #253650, .T. ) ;
#188331 = CIRCLE ( 'NONE', #204510, 0.2000000000000057288 ) ;
#188333 = CARTESIAN_POINT ( 'NONE',  ( -23.25000000000000000, -3.642792592896924919, -226.5668142904084164 ) ) ;
#188334 = VECTOR ( 'NONE', #188527, 1000.000000000000000 ) ;
#188335 = CARTESIAN_POINT ( 'NONE',  ( -22.00411653962178704, 60.20480020221445017, -234.0521012187911651 ) ) ;
#188336 = EDGE_CURVE ( 'NONE', #175428, #152369, #154601, .T. ) ;
#188337 = ORIENTED_EDGE ( 'NONE', *, *, #74313, .F. ) ;
#188338 = CARTESIAN_POINT ( 'NONE',  ( -16.87036670365549895, 66.01058118071095748, -191.0026676018264880 ) ) ;
#188339 = ORIENTED_EDGE ( 'NONE', *, *, #56088, .T. ) ;
#188341 = AXIS2_PLACEMENT_3D ( 'NONE', #164801, #180513, #179246 ) ;
#188340 = CARTESIAN_POINT ( 'NONE',  ( 21.05000000000000071, 65.27628289530454708, -124.3731074845243825 ) ) ;
#188342 = ORIENTED_EDGE ( 'NONE', *, *, #201660, .F. ) ;
#188343 = EDGE_CURVE ( 'NONE', #108899, #44054, #247966, .T. ) ;
#188344 = FACE_OUTER_BOUND ( 'NONE', #70723, .T. ) ;
#188345 = CARTESIAN_POINT ( 'NONE',  ( 23.24999999999999645, 1.115600667400684642E-11, -167.5000000000000284 ) ) ;
#188347 = EDGE_LOOP ( 'NONE', ( #2851, #169262, #85028, #23093 ) ) ;
#188346 = EDGE_CURVE ( 'NONE', #177661, #256296, #116721, .T. ) ;
#188348 = ORIENTED_EDGE ( 'NONE', *, *, #255545, .T. ) ;
#188349 = DIRECTION ( 'NONE',  ( 1.000000000000000000, 0.000000000000000000, -0.000000000000000000 ) ) ;
#188351 = VERTEX_POINT ( 'NONE', #137552 ) ;
#188350 = CARTESIAN_POINT ( 'NONE',  ( 12.25000000000000000, 9.350000000011140955, -50.24999999999999289 ) ) ;
#188352 = DIRECTION ( 'NONE',  ( 0.000000000000000000, 0.000000000000000000, 1.000000000000000000 ) ) ;
#188354 = VERTEX_POINT ( 'NONE', #97117 ) ;
#188353 = CIRCLE ( 'NONE', #134355, 3.999999999999999112 ) ;
#188355 =( BOUNDED_CURVE ( )  B_SPLINE_CURVE ( 3, ( #136348, #37305, #236752, #55522 ),
 .UNSPECIFIED., .F., .T. ) 
 B_SPLINE_CURVE_WITH_KNOTS ( ( 4, 4 ),
 ( 2.589852378279006384, 2.850972632318390154 ),
 .UNSPECIFIED. ) 
 CURVE ( )  GEOMETRIC_REPRESENTATION_ITEM ( )  RATIONAL_B_SPLINE_CURVE ( ( 1.000000000000000000, 0.9943260843901262636, 0.9943260843901262636, 1.000000000000000000 ) ) 
 REPRESENTATION_ITEM ( '' )  );
#188356 = AXIS2_PLACEMENT_3D ( 'NONE', #108737, #164865, #86573 ) ;
#188357 = AXIS2_PLACEMENT_3D ( 'NONE', #59849, #62455, #141972 ) ;
#188358 = VERTEX_POINT ( 'NONE', #163562 ) ;
#188359 = ADVANCED_FACE ( 'NONE', ( #243086 ), #77836, .T. ) ;
#188360 = DIRECTION ( 'NONE',  ( 0.000000000000000000, 0.4999999999999799605, -0.8660254037844502539 ) ) ;
#188361 = DIRECTION ( 'NONE',  ( 0.000000000000000000, 0.000000000000000000, 1.000000000000000000 ) ) ;
#188362 = CARTESIAN_POINT ( 'NONE',  ( -20.85000000000000142, 11.75000000000000000, -33.50000000000000000 ) ) ;
#188363 = CARTESIAN_POINT ( 'NONE',  ( 23.24999999999999289, 42.94327155031035659, -233.8606566173841372 ) ) ;
#188364 = CARTESIAN_POINT ( 'NONE',  ( -18.40000000000000568, -9.499999999988851584, -73.99936209718016755 ) ) ;
#188365 = DIRECTION ( 'NONE',  ( 0.000000000000000000, -1.000000000000000000, -6.789366196018718420E-15 ) ) ;
#188366 = ORIENTED_EDGE ( 'NONE', *, *, #143479, .F. ) ;
#188367 = CARTESIAN_POINT ( 'NONE',  ( -18.59999999999999787, 79.19526988099229925, -196.1889237952725296 ) ) ;
#188368 = CARTESIAN_POINT ( 'NONE',  ( -21.05000000000000071, 76.00000000001179501, -81.32310748452431426 ) ) ;
#188369 = CARTESIAN_POINT ( 'NONE',  ( 20.95224633520496127, 67.09947783345485561, -128.0298310366030989 ) ) ;
#188370 = DIRECTION ( 'NONE',  ( 0.9880948137434723000, 0.1538461538461484146, -0.000000000000000000 ) ) ;
#188371 = ORIENTED_EDGE ( 'NONE', *, *, #59561, .T. ) ;
#188372 = DIRECTION ( 'NONE',  ( 1.000000000000000000, 0.000000000000000000, 0.000000000000000000 ) ) ;
#188373 = VERTEX_POINT ( 'NONE', #43616 ) ;
#188374 = CARTESIAN_POINT ( 'NONE',  ( -18.46946985241261174, -7.804742910430244152, -209.8502291530988373 ) ) ;
#188375 = ORIENTED_EDGE ( 'NONE', *, *, #220196, .T. ) ;
#188376 = DIRECTION ( 'NONE',  ( -0.000000000000000000, 1.000000000000000000, -1.224646799147352961E-16 ) ) ;
#188377 = LINE ( 'NONE', #89266, #131413 ) ;
#188378 = ORIENTED_EDGE ( 'NONE', *, *, #211308, .T. ) ;
#188379 = EDGE_LOOP ( 'NONE', ( #44016, #136473, #176512, #233633 ) ) ;
#188381 = ORIENTED_EDGE ( 'NONE', *, *, #250878, .F. ) ;
#188380 = CARTESIAN_POINT ( 'NONE',  ( 18.39999999999999858, 37.95493834378066111, -261.2294694241335264 ) ) ;
#188382 = CARTESIAN_POINT ( 'NONE',  ( -20.00857864376270001, 66.85000000001200249, -115.2731074845243597 ) ) ;
#188383 = VERTEX_POINT ( 'NONE', #80123 ) ;
#188384 = FACE_OUTER_BOUND ( 'NONE', #93124, .T. ) ;
#188385 = VERTEX_POINT ( 'NONE', #20205 ) ;
#188386 = EDGE_CURVE ( 'NONE', #203476, #218877, #61893, .T. ) ;
#188387 = LINE ( 'NONE', #9749, #68539 ) ;
#188388 = DIRECTION ( 'NONE',  ( 1.000000000000000000, 0.000000000000000000, 0.000000000000000000 ) ) ;
#188389 = EDGE_CURVE ( 'NONE', #256979, #179202, #252624, .T. ) ;
#188390 = EDGE_LOOP ( 'NONE', ( #48429, #110677, #159549, #133032 ) ) ;
#188391 = TOROIDAL_SURFACE ( 'NONE', #75975, 0.2000000000000000111, 0.1000000000000000056 ) ;
#188392 = DIRECTION ( 'NONE',  ( -0.000000000000000000, -6.982962677686266711E-15, 1.000000000000000000 ) ) ;
#188393 = EDGE_CURVE ( 'NONE', #136731, #160911, #123154, .T. ) ;
#188394 = FACE_OUTER_BOUND ( 'NONE', #184864, .T. ) ;
#188395 = ADVANCED_FACE ( 'NONE', ( #202676 ), #40286, .F. ) ;
#188396 = CARTESIAN_POINT ( 'NONE',  ( -23.25000000000000000, 76.00000000001237765, -170.0231074845243597 ) ) ;
#188398 = EDGE_LOOP ( 'NONE', ( #112342, #215263, #159890, #252951 ) ) ;
#188397 = DIRECTION ( 'NONE',  ( 0.000000000000000000, -0.2617529984165031243, -0.9651348961777158619 ) ) ;
#188399 = ADVANCED_FACE ( 'NONE', ( #104825 ), #184394, .T. ) ;
#188400 = CARTESIAN_POINT ( 'NONE',  ( -20.54999999999999716, 71.65000000001187175, -90.67310748452433700 ) ) ;
#188401 = CARTESIAN_POINT ( 'NONE',  ( -22.57320508075686760, 12.67709964810650902, -223.3751320524553705 ) ) ;
#188402 = DIRECTION ( 'NONE',  ( 0.000000000000000000, -0.9968797965484670343, -0.07893460099023182075 ) ) ;
#188404 = DIRECTION ( 'NONE',  ( 0.000000000000000000, -0.000000000000000000, 1.000000000000000000 ) ) ;
#188403 = DIRECTION ( 'NONE',  ( 0.000000000000000000, 0.000000000000000000, -1.000000000000000000 ) ) ;
#188405 = CARTESIAN_POINT ( 'NONE',  ( -20.87600722750343252, 65.66887361445387228, -164.4329845918269939 ) ) ;
#188406 = CARTESIAN_POINT ( 'NONE',  ( -20.15000000000000568, 63.82605078341359217, -212.9139525631556751 ) ) ;
#188407 = TOROIDAL_SURFACE ( 'NONE', #92546, 0.2000000000000000111, 0.1000000000000000056 ) ;
#188408 = CARTESIAN_POINT ( 'NONE',  ( 23.15000000000000213, 23.40438595358394736, -253.3416554127419431 ) ) ;
#188409 = DIRECTION ( 'NONE',  ( 4.504528286903030855E-15, 0.8127272543710891695, -0.5826443254700338636 ) ) ;
#188410 = EDGE_LOOP ( 'NONE', ( #18602, #44426, #197453, #152016, #118678, #184530, #247399, #75415 ) ) ;
#188411 = EDGE_CURVE ( 'NONE', #151730, #127649, #6921, .T. ) ;
#188413 = EDGE_LOOP ( 'NONE', ( #11695, #146288, #212868, #37569 ) ) ;
#188412 = VECTOR ( 'NONE', #98953, 1000.000000000000000 ) ;
#188414 = ORIENTED_EDGE ( 'NONE', *, *, #220508, .T. ) ;
#188415 = DIRECTION ( 'NONE',  ( 1.000000000000000000, -0.000000000000000000, -0.000000000000000000 ) ) ;
#188416 = CARTESIAN_POINT ( 'NONE',  ( -18.40000000000000213, 11.33174054713633261, -121.3500000000000369 ) ) ;
#188417 = VERTEX_POINT ( 'NONE', #124444 ) ;
#188418 = AXIS2_PLACEMENT_3D ( 'NONE', #72338, #172751, #252225 ) ;
#188419 = CARTESIAN_POINT ( 'NONE',  ( -21.14999999999999858, 11.75000000000000000, -6.783865662978153743 ) ) ;
#188420 = DIRECTION ( 'NONE',  ( 1.000000000000000000, -0.000000000000000000, 0.000000000000000000 ) ) ;
#188421 = EDGE_CURVE ( 'NONE', #143795, #188088, #185992, .T. ) ;
#188422 = FACE_OUTER_BOUND ( 'NONE', #144781, .T. ) ;
#188423 = ORIENTED_EDGE ( 'NONE', *, *, #42594, .F. ) ;
#188424 = VERTEX_POINT ( 'NONE', #241805 ) ;
#188425 = DIRECTION ( 'NONE',  ( -0.000000000000000000, -0.000000000000000000, 1.000000000000000000 ) ) ;
#188426 = DIRECTION ( 'NONE',  ( 0.000000000000000000, -1.000000000000000000, 0.000000000000000000 ) ) ;
#188427 = ORIENTED_EDGE ( 'NONE', *, *, #9129, .F. ) ;
#188428 = CIRCLE ( 'NONE', #171914, 0.1000000000000028644 ) ;
#188429 = DIRECTION ( 'NONE',  ( 0.000000000000000000, -0.9126074666063660468, -0.4088369013363524762 ) ) ;
#188431 = ORIENTED_EDGE ( 'NONE', *, *, #228316, .F. ) ;
#188430 = CARTESIAN_POINT ( 'NONE',  ( 20.09999999999999787, 66.25000000001185185, -90.37310748452436826 ) ) ;
#188432 = DIRECTION ( 'NONE',  ( 0.000000000000000000, -0.8814952561688476074, 0.4721928772777262417 ) ) ;
#188433 = DIRECTION ( 'NONE',  ( 0.000000000000000000, 0.000000000000000000, -1.000000000000000000 ) ) ;
#188434 = EDGE_CURVE ( 'NONE', #76969, #112394, #45553, .T. ) ;
#188436 = VERTEX_POINT ( 'NONE', #220945 ) ;
#188435 = DIRECTION ( 'NONE',  ( 1.000000000000000000, -0.000000000000000000, -0.000000000000000000 ) ) ;
#188437 = AXIS2_PLACEMENT_3D ( 'NONE', #188516, #245935, #244632 ) ;
#188438 =( NAMED_UNIT ( * ) PLANE_ANGLE_UNIT ( ) SI_UNIT ( $, .RADIAN. ) );
#188440 = CARTESIAN_POINT ( 'NONE',  ( -16.94226253665224391, 9.950000000011135270, -87.55326540438426264 ) ) ;
#188439 = AXIS2_PLACEMENT_3D ( 'NONE', #197919, #218760, #40175 ) ;
#188441 = AXIS2_PLACEMENT_3D ( 'NONE', #176094, #136211, #39147 ) ;
#188442 = DIRECTION ( 'NONE',  ( 0.000000000000000000, 0.8454177738465993297, 0.5341055959866553016 ) ) ;
#188443 = EDGE_CURVE ( 'NONE', #158190, #140279, #148600, .T. ) ;
#188444 = CARTESIAN_POINT ( 'NONE',  ( -21.05000000000000071, -11.74999999998884448, -198.0999999999999659 ) ) ;
#188445 = CIRCLE ( 'NONE', #254842, 0.1000000000000028644 ) ;
#188447 = CYLINDRICAL_SURFACE ( 'NONE', #12504, 0.1000000000000072220 ) ;
#188446 = CARTESIAN_POINT ( 'NONE',  ( -16.87683809663752399, 9.950000000011137047, -154.0976359818037054 ) ) ;
#188448 = DIRECTION ( 'NONE',  ( 1.000000000000000000, -0.000000000000000000, -0.000000000000000000 ) ) ;
#188449 = DIRECTION ( 'NONE',  ( 0.000000000000000000, 0.000000000000000000, -1.000000000000000000 ) ) ;
#188450 = DIRECTION ( 'NONE',  ( 1.000000000000000000, 0.000000000000000000, -0.000000000000000000 ) ) ;
#188451 = CARTESIAN_POINT ( 'NONE',  ( -18.40000000000000213, 64.25000000001222134, -145.7731074845244450 ) ) ;
#188452 = VERTEX_POINT ( 'NONE', #240529 ) ;
#188453 = EDGE_LOOP ( 'NONE', ( #62710, #224595, #227887, #56840 ) ) ;
#188454 = EDGE_CURVE ( 'NONE', #86491, #211613, #173589, .T. ) ;
#188455 = CARTESIAN_POINT ( 'NONE',  ( -23.25000000000000000, 76.10000000001276987, -215.1726782920691505 ) ) ;
#188456 = VERTEX_POINT ( 'NONE', #198826 ) ;
#188457 = DIRECTION ( 'NONE',  ( 0.000000000000000000, 1.000000000000000000, 0.000000000000000000 ) ) ;
#188458 = ORIENTED_EDGE ( 'NONE', *, *, #172480, .F. ) ;
#188459 = DIRECTION ( 'NONE',  ( 0.000000000000000000, -7.026728003956683390E-15, 1.000000000000000000 ) ) ;
#188460 = CYLINDRICAL_SURFACE ( 'NONE', #202557, 0.09999999999999986677 ) ;
#188461 = EDGE_CURVE ( 'NONE', #19990, #160249, #181356, .T. ) ;
#188462 = EDGE_CURVE ( 'NONE', #241914, #233103, #136079, .T. ) ;
#188463 = ORIENTED_EDGE ( 'NONE', *, *, #199825, .F. ) ;
#188464 = EDGE_CURVE ( 'NONE', #160655, #186823, #111172, .T. ) ;
#188465 = DIRECTION ( 'NONE',  ( 2.915501640297156255E-16, 1.000000000000000000, 6.997203936713175802E-15 ) ) ;
#188466 = VECTOR ( 'NONE', #159893, 1000.000000000000000 ) ;
#188467 = CIRCLE ( 'NONE', #34386, 3.900000000000000799 ) ;
#188468 = ORIENTED_EDGE ( 'NONE', *, *, #196421, .F. ) ;
#188469 = ORIENTED_EDGE ( 'NONE', *, *, #184992, .F. ) ;
#188470 = ORIENTED_EDGE ( 'NONE', *, *, #32685, .T. ) ;
#188471 = DIRECTION ( 'NONE',  ( 1.000000000000000000, 0.000000000000000000, 0.000000000000000000 ) ) ;
#188472 = DIRECTION ( 'NONE',  ( 1.000000000000000000, 0.000000000000000000, 0.000000000000000000 ) ) ;
#188473 = CARTESIAN_POINT ( 'NONE',  ( 21.05000000000000071, 60.91498325274309877, -225.4240842350366165 ) ) ;
#188474 = LINE ( 'NONE', #248460, #136291 ) ;
#188475 = DIRECTION ( 'NONE',  ( 1.000000000000000000, 0.000000000000000000, 0.000000000000000000 ) ) ;
#188476 = EDGE_CURVE ( 'NONE', #159790, #8351, #56973, .T. ) ;
#188477 = AXIS2_PLACEMENT_3D ( 'NONE', #129710, #209240, #48884 ) ;
#188479 = DIRECTION ( 'NONE',  ( -2.915501640297153790E-16, 1.000000000000000000, 0.000000000000000000 ) ) ;
#188478 = DIRECTION ( 'NONE',  ( 0.000000000000000000, 0.000000000000000000, 1.000000000000000000 ) ) ;
#188480 = FACE_OUTER_BOUND ( 'NONE', #135163, .T. ) ;
#188482 = ORIENTED_EDGE ( 'NONE', *, *, #105061, .T. ) ;
#188481 = DIRECTION ( 'NONE',  ( -1.000000000000000000, -0.000000000000000000, 0.000000000000000000 ) ) ;
#188484 = FACE_OUTER_BOUND ( 'NONE', #116978, .T. ) ;
#188483 = CARTESIAN_POINT ( 'NONE',  ( 20.72390388899108515, 10.58996311843486993, -74.51134829574417040 ) ) ;
#188485 = DIRECTION ( 'NONE',  ( 1.000000000000000000, 0.000000000000000000, 0.000000000000000000 ) ) ;
#188486 = VERTEX_POINT ( 'NONE', #100959 ) ;
#188487 = DIRECTION ( 'NONE',  ( -1.000000000000000000, -0.000000000000000000, 0.000000000000000000 ) ) ;
#188488 = CIRCLE ( 'NONE', #113477, 0.3999999999999975797 ) ;
#188489 = CARTESIAN_POINT ( 'NONE',  ( 21.14999999999999858, 64.35000000001267040, -203.4231074845244507 ) ) ;
#188490 = DIRECTION ( 'NONE',  ( 1.000000000000000000, -3.265361837132813093E-16, -2.280189983783949500E-30 ) ) ;
#188491 = B_SPLINE_CURVE_WITH_KNOTS ( 'NONE', 3,
 ( #23778, #103253, #6743, #86256, #107123, #101962, #186685, #87548, #83673, #182845, #242778, #167141, #68003, #147543, #245370, #203665 ),
 .UNSPECIFIED., .F., .F.,
 ( 4, 3, 3, 3, 3, 4 ),
 ( 0.000000000000000000, 2.209075297431620268E-05, 5.594258369009776820E-05, 8.979524372341989448E-05, 0.0001236472815274567327, 0.0001574990747609542811 ),
 .UNSPECIFIED. ) ;
#188492 = ORIENTED_EDGE ( 'NONE', *, *, #140386, .F. ) ;
#188493 = TOROIDAL_SURFACE ( 'NONE', #142680, 2.699999999999999734, 0.1000000000000000056 ) ;
#188495 = CARTESIAN_POINT ( 'NONE',  ( -16.87683809663753465, 61.18526039135985428, -220.4600993141388301 ) ) ;
#188494 = AXIS2_PLACEMENT_3D ( 'NONE', #147331, #69099, #123936 ) ;
#188496 = VECTOR ( 'NONE', #208639, 1000.000000000000000 ) ;
#188497 = FACE_OUTER_BOUND ( 'NONE', #220337, .T. ) ;
#188498 = CARTESIAN_POINT ( 'NONE',  ( 15.74999999999999645, 66.65000000001185754, -86.27310748452437394 ) ) ;
#188499 = CIRCLE ( 'NONE', #21917, 0.1000000000000043493 ) ;
#188500 = ORIENTED_EDGE ( 'NONE', *, *, #122954, .F. ) ;
#188501 = VERTEX_POINT ( 'NONE', #125709 ) ;
#188502 = AXIS2_PLACEMENT_3D ( 'NONE', #173298, #212385, #170732 ) ;
#188503 = CARTESIAN_POINT ( 'NONE',  ( -23.25000000000000000, 77.83585931145526615, -57.91866831572577468 ) ) ;
#188504 = CARTESIAN_POINT ( 'NONE',  ( -18.51024323315077424, 10.31104185824062469, -173.0204516983106373 ) ) ;
#188505 = DIRECTION ( 'NONE',  ( -1.000000000000000000, -0.000000000000000000, -0.000000000000000000 ) ) ;
#188506 = CARTESIAN_POINT ( 'NONE',  ( -20.94999999999999929, 10.29270135741298731, -206.4573618871519045 ) ) ;
#188507 = EDGE_LOOP ( 'NONE', ( #120469, #64275, #44135, #108237, #51603, #161171, #229728, #233179, #224516 ) ) ;
#188508 = AXIS2_PLACEMENT_3D ( 'NONE', #56631, #94502, #174098 ) ;
#188510 = AXIS2_PLACEMENT_3D ( 'NONE', #75656, #200720, #1204 ) ;
#188509 = CARTESIAN_POINT ( 'NONE',  ( -12.48127053791145258, 9.376580978055097049, -118.1269462470119862 ) ) ;
#188511 = FACE_OUTER_BOUND ( 'NONE', #7700, .T. ) ;
#188512 = DIRECTION ( 'NONE',  ( -0.000000000000000000, 1.000000000000000000, -0.000000000000000000 ) ) ;
#188513 = AXIS2_PLACEMENT_3D ( 'NONE', #203102, #221363, #102692 ) ;
#188514 = CARTESIAN_POINT ( 'NONE',  ( 20.85000000000000142, 67.85909929089923764, -227.8797997985275856 ) ) ;
#188515 = ORIENTED_EDGE ( 'NONE', *, *, #48834, .F. ) ;
#188516 = CARTESIAN_POINT ( 'NONE',  ( -22.94999999999999929, 3.461118860469513336, 28.84309995045515507 ) ) ;
#188517 = AXIS2_PLACEMENT_3D ( 'NONE', #40562, #220455, #183882 ) ;
#188518 = CIRCLE ( 'NONE', #55205, 11.74999999999999822 ) ;
#188520 = VERTEX_POINT ( 'NONE', #224800 ) ;
#188519 = CARTESIAN_POINT ( 'NONE',  ( -23.25000000000000000, 8.980461154494397746, -187.0187154576991304 ) ) ;
#188521 = DIRECTION ( 'NONE',  ( 0.000000000000000000, 0.1575546449569757979, 0.9875102702516471709 ) ) ;
#188522 = CARTESIAN_POINT ( 'NONE',  ( 21.14999999999999858, 64.35000000001237197, -169.9231074845244507 ) ) ;
#188523 = CARTESIAN_POINT ( 'NONE',  ( 21.05000000000000071, 71.00000000001223555, -148.5283735034374786 ) ) ;
#188524 = EDGE_CURVE ( 'NONE', #222021, #161463, #140181, .T. ) ;
#188525 = CARTESIAN_POINT ( 'NONE',  ( 20.04142135623730070, 62.34315093393704643, -208.9889535843037720 ) ) ;
#188526 = CARTESIAN_POINT ( 'NONE',  ( -23.25000000000000000, 87.65000000001215597, -139.6231074845242688 ) ) ;
#188527 = DIRECTION ( 'NONE',  ( -1.000000000000000000, 0.000000000000000000, 0.000000000000000000 ) ) ;
#188528 = DIRECTION ( 'NONE',  ( 0.000000000000000000, 6.982962677686266711E-15, -1.000000000000000000 ) ) ;
#188529 = ORIENTED_EDGE ( 'NONE', *, *, #141005, .F. ) ;
#188530 = CARTESIAN_POINT ( 'NONE',  ( -20.90000000000000213, -1.885425182446133885, -11.49641995933507843 ) ) ;
#188531 = CARTESIAN_POINT ( 'NONE',  ( 20.90000000000000213, -11.65000000000000036, 0.000000000000000000 ) ) ;
#188533 = ADVANCED_FACE ( 'NONE', ( #126999 ), #61089, .F. ) ;
#188532 = CARTESIAN_POINT ( 'NONE',  ( 19.92426406871192412, 11.75000000001116085, -58.35000000000000142 ) ) ;
#188534 = ADVANCED_FACE ( 'NONE', ( #129576 ), #163608, .F. ) ;
#188535 = CARTESIAN_POINT ( 'NONE',  ( -16.86420534634261514, 51.67279902237199707, -231.8997167030369155 ) ) ;
#188536 = FACE_OUTER_BOUND ( 'NONE', #48570, .T. ) ;
#188537 = VECTOR ( 'NONE', #133169, 1000.000000000000000 ) ;
#188538 = AXIS2_PLACEMENT_3D ( 'NONE', #35023, #118380, #54540 ) ;
#188539 = CARTESIAN_POINT ( 'NONE',  ( 18.59999999999999432, 1.162701749949165642, -175.5999999999999659 ) ) ;
#188540 = AXIS2_PLACEMENT_3D ( 'NONE', #80378, #240780, #159979 ) ;
#188541 = ORIENTED_EDGE ( 'NONE', *, *, #253503, .F. ) ;
#188542 = VERTEX_POINT ( 'NONE', #70911 ) ;
#188543 = CARTESIAN_POINT ( 'NONE',  ( 21.00000000000000000, 7.800000000000000711, -1.212568896937008089 ) ) ;
#188544 = DIRECTION ( 'NONE',  ( 0.000000000000000000, 0.000000000000000000, -1.000000000000000000 ) ) ;
#188545 = DIRECTION ( 'NONE',  ( 0.000000000000000000, -0.9126074666063769270, -0.4088369013363280513 ) ) ;
#188546 = ADVANCED_FACE ( 'NONE', ( #29230 ), #106127, .F. ) ;
#188547 = DIRECTION ( 'NONE',  ( 0.000000000000000000, 0.2617529984164915779, 0.9651348961777189706 ) ) ;
#188548 = CYLINDRICAL_SURFACE ( 'NONE', #109232, 0.1000000000000028644 ) ;
#188549 = DIRECTION ( 'NONE',  ( 1.000000000000000000, -7.304098846218134667E-16, -5.100424963727255829E-30 ) ) ;
#188550 = DIRECTION ( 'NONE',  ( 1.000000000000000000, -0.000000000000000000, -0.000000000000000000 ) ) ;
#188551 = TOROIDAL_SURFACE ( 'NONE', #138462, 3.899999999999999467, 0.1000000000000000056 ) ;
#188552 = LINE ( 'NONE', #89444, #173713 ) ;
#188553 = EDGE_LOOP ( 'NONE', ( #127454, #53886, #223892, #49767 ) ) ;
#188554 = DIRECTION ( 'NONE',  ( 1.000000000000000000, 0.000000000000000000, 0.000000000000000000 ) ) ;
#188555 = AXIS2_PLACEMENT_3D ( 'NONE', #229617, #228336, #249187 ) ;
#188556 = ORIENTED_EDGE ( 'NONE', *, *, #187504, .T. ) ;
#188557 = ADVANCED_FACE ( 'NONE', ( #147860 ), #228687, .F. ) ;
#188558 = DIRECTION ( 'NONE',  ( 1.000000000000000000, 0.000000000000000000, 0.000000000000000000 ) ) ;
#188559 = EDGE_CURVE ( 'NONE', #12719, #63408, #200365, .T. ) ;
#188560 = DIRECTION ( 'NONE',  ( 0.000000000000000000, 0.8814952561688442767, -0.4721928772777324035 ) ) ;
#188561 = LINE ( 'NONE', #209405, #157670 ) ;
#188562 = CARTESIAN_POINT ( 'NONE',  ( -20.64999999999999858, 4.349999999999999645, -12.35000000000000142 ) ) ;
#188563 = CARTESIAN_POINT ( 'NONE',  ( 21.05543885634738643, 22.01316703130699182, -231.7502803265042246 ) ) ;
#188564 = CARTESIAN_POINT ( 'NONE',  ( 13.40000000000005898, 67.75000000001118394, -16.98168612828748891 ) ) ;
#188565 = CARTESIAN_POINT ( 'NONE',  ( -17.05016517656045849, 66.05000000001182059, -82.19580548052314839 ) ) ;
#188566 = ORIENTED_EDGE ( 'NONE', *, *, #7213, .T. ) ;
#188567 = CARTESIAN_POINT ( 'NONE',  ( -16.93440969289731157, 22.94760179058243921, -230.8674840937281374 ) ) ;
#188568 = CARTESIAN_POINT ( 'NONE',  ( -18.50000000000000000, 68.87972903831483507, -166.3635444426850825 ) ) ;
#188569 = CARTESIAN_POINT ( 'NONE',  ( -22.50000000000000000, 11.64957080755595520, -167.3999999999999773 ) ) ;
#188571 = ADVANCED_FACE ( 'NONE', ( #46169 ), #50028, .F. ) ;
#188570 = DIRECTION ( 'NONE',  ( 1.000000000000000000, 0.000000000000000000, 0.000000000000000000 ) ) ;
#188572 = CARTESIAN_POINT ( 'NONE',  ( 21.05000000000000071, 76.00000000001247713, -174.1231074845243540 ) ) ;
#188573 = EDGE_LOOP ( 'NONE', ( #7755, #22418, #224287, #197939, #170765, #116564, #46096, #6269, #186761, #241999, #250310, #28706, #226511, #84479, #236390, #95932 ) ) ;
#188574 = DIRECTION ( 'NONE',  ( -1.000000000000000000, 2.952720810173289112E-16, 2.061873921506763405E-30 ) ) ;
#188575 = LINE ( 'NONE', #86888, #37789 ) ;
#188576 = VERTEX_POINT ( 'NONE', #248235 ) ;
#188577 = EDGE_LOOP ( 'NONE', ( #4594, #223651 ) ) ;
#188578 = CARTESIAN_POINT ( 'NONE',  ( -21.44999999999999929, 7.350000000011155166, -112.8500000000000369 ) ) ;
#188579 = CYLINDRICAL_SURFACE ( 'NONE', #40053, 0.1000000000000002554 ) ;
#188580 = ADVANCED_FACE ( 'NONE', ( #90427 ), #170030, .T. ) ;
#188581 = ORIENTED_EDGE ( 'NONE', *, *, #200054, .F. ) ;
#188582 = CARTESIAN_POINT ( 'NONE',  ( 20.99780126800938262, 64.39461131213495548, -42.93575491281916356 ) ) ;
#188583 = CYLINDRICAL_SURFACE ( 'NONE', #55817, 0.1000000000000002554 ) ;
#188584 = VECTOR ( 'NONE', #97091, 1000.000000000000000 ) ;
#188585 = ORIENTED_EDGE ( 'NONE', *, *, #167829, .T. ) ;
#188586 = AXIS2_PLACEMENT_3D ( 'NONE', #256547, #192794, #158820 ) ;
#188587 = CARTESIAN_POINT ( 'NONE',  ( 18.54286124688533377, -9.623917578786658211, -174.2412023318627234 ) ) ;
#188588 = ADVANCED_FACE ( 'NONE', ( #96827 ), #112585, .T. ) ;
#188589 = ORIENTED_EDGE ( 'NONE', *, *, #168100, .F. ) ;
#188590 = CARTESIAN_POINT ( 'NONE',  ( 21.07946286933444568, 75.92331615675576018, -142.8521448035320986 ) ) ;
#188591 = DIRECTION ( 'NONE',  ( -2.952720810173289112E-16, 1.000000000000000000, 0.000000000000000000 ) ) ;
#188593 = ORIENTED_EDGE ( 'NONE', *, *, #16380, .F. ) ;
#188592 = CARTESIAN_POINT ( 'NONE',  ( -18.59999999999999787, 11.76393579169289083, -211.0774408799668720 ) ) ;
#188594 = DIRECTION ( 'NONE',  ( 0.000000000000000000, 0.1568667991644863147, -0.9876197685951252359 ) ) ;
#188596 = DIRECTION ( 'NONE',  ( -4.239556034732056743E-17, -0.1298341882519953583, -0.9915357197604862671 ) ) ;
#188595 = UNCERTAINTY_MEASURE_WITH_UNIT (LENGTH_MEASURE( 1.000000000000000082E-05 ), #156740, 'distance_accuracy_value', 'NONE');
#188597 = EDGE_CURVE ( 'NONE', #155920, #88045, #253365, .T. ) ;
#188599 = EDGE_CURVE ( 'NONE', #256686, #62499, #34351, .T. ) ;
#188598 = CARTESIAN_POINT ( 'NONE',  ( -22.00411653962162362, 68.74655713164246151, -203.6221455902930302 ) ) ;
#188600 = CARTESIAN_POINT ( 'NONE',  ( -16.87401514999223195, 66.05000000001230376, -157.3031254770564829 ) ) ;
#188601 = DIRECTION ( 'NONE',  ( -1.000000000000000000, 0.000000000000000000, 0.000000000000000000 ) ) ;
#188602 = DIRECTION ( 'NONE',  ( 0.000000000000000000, 6.938893903907222067E-15, -1.000000000000000000 ) ) ;
#188603 = PLANE ( 'NONE',  #87356 ) ;
#188605 = EDGE_LOOP ( 'NONE', ( #28180, #150059, #52730, #138288, #61625, #114060, #257424, #3858, #71364, #26910, #217347, #233387, #54488, #180037, #74262, #144505, #168472, #79482, #155499, #254196, #250581, #226242, #53827, #90198, #83904 ) ) ;
#188604 = CARTESIAN_POINT ( 'NONE',  ( 18.58725287972329454, 87.01889655985287675, -199.4425632957462540 ) ) ;
#188606 = ORIENTED_EDGE ( 'NONE', *, *, #109410, .T. ) ;
#188608 = CARTESIAN_POINT ( 'NONE',  ( -12.26136940704871670, 9.351403174152810749, -83.97953043683850183 ) ) ;
#188607 = DIRECTION ( 'NONE',  ( -0.000000000000000000, -0.2617529984165031243, -0.9651348961777157509 ) ) ;
#188610 = ORIENTED_EDGE ( 'NONE', *, *, #69963, .F. ) ;
#188609 = CARTESIAN_POINT ( 'NONE',  ( -17.11825945287481332, 65.95000000001225260, -149.2731074845244450 ) ) ;
#188611 = EDGE_LOOP ( 'NONE', ( #186453, #135501, #27677, #147791 ) ) ;
#188612 = DIRECTION ( 'NONE',  ( 0.000000000000000000, 0.4999999999999956701, -0.8660254037844411501 ) ) ;
#188613 = CARTESIAN_POINT ( 'NONE',  ( -22.39999999999999858, 0.3085173699977072914, -229.9658011520297691 ) ) ;
#188614 = EDGE_CURVE ( 'NONE', #71577, #6826, #231412, .T. ) ;
#188615 = EDGE_CURVE ( 'NONE', #100865, #12967, #152329, .T. ) ;
#188616 = DIRECTION ( 'NONE',  ( -1.000000000000000000, 0.000000000000000000, 0.000000000000000000 ) ) ;
#188617 = AXIS2_PLACEMENT_3D ( 'NONE', #88357, #222743, #207055 ) ;
#188618 = CARTESIAN_POINT ( 'NONE',  ( -22.50000000000000000, 67.23127455305841238, -235.8551265064783991 ) ) ;
#188619 = FACE_OUTER_BOUND ( 'NONE', #6091, .T. ) ;
#188620 = ADVANCED_FACE ( 'NONE', ( #154321 ), #52590, .F. ) ;
#188621 = LINE ( 'NONE', #111657, #111317 ) ;
#188622 = AXIS2_PLACEMENT_3D ( 'NONE', #47398, #245623, #27893 ) ;
#188623 = AXIS2_PLACEMENT_3D ( 'NONE', #30242, #191900, #189308 ) ;
#188624 = CIRCLE ( 'NONE', #213763, 4.150000000000001243 ) ;
#188626 = AXIS2_PLACEMENT_3D ( 'NONE', #49236, #188746, #251278 ) ;
#188625 = DIRECTION ( 'NONE',  ( -1.000000000000000000, 0.000000000000000000, 0.000000000000000000 ) ) ;
#188628 = EDGE_LOOP ( 'NONE', ( #247470, #90062, #65493, #150303 ) ) ;
#188627 = EDGE_CURVE ( 'NONE', #151479, #84754, #187221, .T. ) ;
#188629 = ORIENTED_EDGE ( 'NONE', *, *, #216333, .T. ) ;
#188630 = DIRECTION ( 'NONE',  ( -1.000000000000000000, 0.000000000000000000, 0.000000000000000000 ) ) ;
#188631 = ORIENTED_EDGE ( 'NONE', *, *, #199968, .T. ) ;
#188632 = EDGE_CURVE ( 'NONE', #24156, #170856, #60405, .T. ) ;
#188633 = DIRECTION ( 'NONE',  ( -2.561896900575096011E-15, -0.5907332058517279494, 0.8068669527897025517 ) ) ;
#188635 = EDGE_CURVE ( 'NONE', #80949, #86681, #235099, .T. ) ;
#188634 = ORIENTED_EDGE ( 'NONE', *, *, #125791, .T. ) ;
#188636 = DIRECTION ( 'NONE',  ( 1.000000000000000000, 0.000000000000000000, 0.000000000000000000 ) ) ;
#188637 = DIRECTION ( 'NONE',  ( 1.000000000000000000, 0.000000000000000000, 0.000000000000000000 ) ) ;
#188638 = EDGE_CURVE ( 'NONE', #204085, #148976, #10657, .T. ) ;
#188639 = FACE_OUTER_BOUND ( 'NONE', #27736, .T. ) ;
#188640 = ORIENTED_EDGE ( 'NONE', *, *, #218600, .T. ) ;
#188641 = DIRECTION ( 'NONE',  ( -0.000000000000000000, 0.9887567792719327286, 0.1495327102803745423 ) ) ;
#188642 = VERTEX_POINT ( 'NONE', #171320 ) ;
#188643 = ADVANCED_FACE ( 'NONE', ( #215520 ), #57721, .F. ) ;
#188644 = CARTESIAN_POINT ( 'NONE',  ( 20.85000000000000142, 7.021664781911246322, -104.3335654018973315 ) ) ;
#188645 = CARTESIAN_POINT ( 'NONE',  ( 20.46382478191414833, 67.09862044130947822, -127.9773793896412712 ) ) ;
#188646 = EDGE_CURVE ( 'NONE', #192047, #97217, #113856, .T. ) ;
#188647 = DIRECTION ( 'NONE',  ( 1.301042606982683102E-14, -0.8496786552930133407, -0.5273008465188128158 ) ) ;
#188649 = VERTEX_POINT ( 'NONE', #216800 ) ;
#188648 = EDGE_CURVE ( 'NONE', #226630, #15834, #231260, .T. ) ;
#188650 = VECTOR ( 'NONE', #154193, 1000.000000000000000 ) ;
#188651 = DIRECTION ( 'NONE',  ( -0.7071067811865389130, 4.937700262164590641E-15, -0.7071067811865561215 ) ) ;
#188652 = ORIENTED_EDGE ( 'NONE', *, *, #254633, .F. ) ;
#188655 = VERTEX_POINT ( 'NONE', #38194 ) ;
#188654 = CARTESIAN_POINT ( 'NONE',  ( -17.71734398241074260, 10.84235722846456440, -23.22513825300560697 ) ) ;
#188653 = CARTESIAN_POINT ( 'NONE',  ( 18.39999999999998437, 46.91436717984748128, -255.3877622108296066 ) ) ;
#188656 = CARTESIAN_POINT ( 'NONE',  ( 21.14999999999999858, 69.35000000001186038, -90.87310748452435405 ) ) ;
#188657 = ORIENTED_EDGE ( 'NONE', *, *, #47982, .T. ) ;
#188658 = FACE_OUTER_BOUND ( 'NONE', #207670, .T. ) ;
#188659 = ORIENTED_EDGE ( 'NONE', *, *, #222745, .T. ) ;
#188660 = CIRCLE ( 'NONE', #221952, 0.09999999999999939493 ) ;
#188661 = AXIS2_PLACEMENT_3D ( 'NONE', #109831, #105965, #223357 ) ;
#188662 = CARTESIAN_POINT ( 'NONE',  ( 18.54999999999999716, 52.34166666667894674, -153.2731074845245303 ) ) ;
#188663 = EDGE_CURVE ( 'NONE', #49816, #32954, #179009, .T. ) ;
#188664 = CARTESIAN_POINT ( 'NONE',  ( -21.64999999999999858, 68.75000000001224976, -148.8731074845244109 ) ) ;
#188665 = ADVANCED_FACE ( 'NONE', ( #22486 ), #199837, .T. ) ;
#188666 = CARTESIAN_POINT ( 'NONE',  ( -16.87036670365548474, 51.72098459467786569, -231.8575261499355236 ) ) ;
#188667 = CIRCLE ( 'NONE', #205222, 0.1000000000000124678 ) ;
#188668 = DIRECTION ( 'NONE',  ( 0.000000000000000000, -0.9126074666063545004, -0.4088369013363783999 ) ) ;
#188669 = AXIS2_PLACEMENT_3D ( 'NONE', #84067, #81519, #22891 ) ;
#188670 = ORIENTED_EDGE ( 'NONE', *, *, #47352, .F. ) ;
#188671 = AXIS2_PLACEMENT_3D ( 'NONE', #249367, #150267, #244194 ) ;
#188672 = CIRCLE ( 'NONE', #47010, 0.09999999999999761857 ) ;
#188673 = DIRECTION ( 'NONE',  ( 0.000000000000000000, -0.9126074666063770380, -0.4088369013363281068 ) ) ;
#188674 = CARTESIAN_POINT ( 'NONE',  ( 21.08198257630413508, 6.336596734026219480, -33.42735667621539619 ) ) ;
#188675 = VERTEX_POINT ( 'NONE', #237662 ) ;
#188676 = CARTESIAN_POINT ( 'NONE',  ( -20.94999999999999929, 38.43293829866423295, -234.5626268121764895 ) ) ;
#188677 = ORIENTED_EDGE ( 'NONE', *, *, #145944, .T. ) ;
#188678 = CARTESIAN_POINT ( 'NONE',  ( 18.49999999999999645, 2.899901325892989767, -187.5321506284477096 ) ) ;
#188679 = ORIENTED_EDGE ( 'NONE', *, *, #48158, .F. ) ;
#188680 = CARTESIAN_POINT ( 'NONE',  ( -20.54999999999999716, 76.52350599684427834, -201.5928376921694678 ) ) ;
#188681 = ORIENTED_EDGE ( 'NONE', *, *, #172772, .T. ) ;
#188682 = DIRECTION ( 'NONE',  ( 0.000000000000000000, 1.000000000000000000, 0.000000000000000000 ) ) ;
#188683 = CIRCLE ( 'NONE', #247116, 0.09999999999999939493 ) ;
#188684 = CARTESIAN_POINT ( 'NONE',  ( -23.30000000000000426, -11.79999999999999893, -347.0000000000001137 ) ) ;
#188685 = AXIS2_PLACEMENT_3D ( 'NONE', #192482, #252436, #94654 ) ;
#188686 = FACE_OUTER_BOUND ( 'NONE', #90526, .T. ) ;
#188687 = ORIENTED_EDGE ( 'NONE', *, *, #142185, .F. ) ;
#188688 = AXIS2_PLACEMENT_3D ( 'NONE', #83474, #226865, #225559 ) ;
#188689 = ADVANCED_FACE ( 'NONE', ( #241511 ), #139825, .F. ) ;
#188690 = DIRECTION ( 'NONE',  ( 1.000000000000000000, -0.000000000000000000, -0.000000000000000000 ) ) ;
#188691 = DIRECTION ( 'NONE',  ( 0.000000000000000000, -1.000000000000000000, 0.000000000000000000 ) ) ;
#188692 = ORIENTED_EDGE ( 'NONE', *, *, #195767, .F. ) ;
#188693 = CARTESIAN_POINT ( 'NONE',  ( 21.05000000000000071, -8.999999999988844479, -43.39396912265245021 ) ) ;
#188694 = EDGE_CURVE ( 'NONE', #21878, #64265, #138527, .T. ) ;
#188695 = AXIS2_PLACEMENT_3D ( 'NONE', #166604, #164015, #226518 ) ;
#188696 = ORIENTED_EDGE ( 'NONE', *, *, #105586, .F. ) ;
#188697 = AXIS2_PLACEMENT_3D ( 'NONE', #2846, #242745, #26290 ) ;
#188698 = AXIS2_PLACEMENT_3D ( 'NONE', #97203, #178094, #137641 ) ;
#188699 = CARTESIAN_POINT ( 'NONE',  ( -16.85312841634288716, 44.37593289069839386, -235.2310913830144443 ) ) ;
#188700 = TOROIDAL_SURFACE ( 'NONE', #192818, 0.2000000000000000111, 0.1000000000000000056 ) ;
#188701 = DIRECTION ( 'NONE',  ( 0.000000000000000000, 0.9126074666063660468, 0.4088369013363524762 ) ) ;
#188704 = ORIENTED_EDGE ( 'NONE', *, *, #180284, .F. ) ;
#188703 = EDGE_LOOP ( 'NONE', ( #182502, #220568, #183902, #226107 ) ) ;
#188702 = CARTESIAN_POINT ( 'NONE',  ( -22.39999999999999858, 59.68594599439717285, -233.9123800762197902 ) ) ;
#188705 = DIRECTION ( 'NONE',  ( -1.000000000000000000, 0.000000000000000000, 0.000000000000000000 ) ) ;
#188706 = CARTESIAN_POINT ( 'NONE',  ( -22.46246831459151494, 0.02191216695058596786, -155.8501354387900051 ) ) ;
#188707 = DIRECTION ( 'NONE',  ( -0.000000000000000000, 0.03181660087583042251, -0.9994937237965568766 ) ) ;
#188709 = DIRECTION ( 'NONE',  ( 1.000000000000000000, 0.000000000000000000, 0.000000000000000000 ) ) ;
#188708 = CARTESIAN_POINT ( 'NONE',  ( 23.14999999999999858, 1.115649653272650466E-11, -196.9999999999999432 ) ) ;
#188711 = EDGE_CURVE ( 'NONE', #214700, #130026, #52322, .T. ) ;
#188710 = CARTESIAN_POINT ( 'NONE',  ( 20.27550659511089037, 9.216043722519994930, -121.3500000000000227 ) ) ;
#188712 = DIRECTION ( 'NONE',  ( 0.000000000000000000, 1.000000000000000000, 0.000000000000000000 ) ) ;
#188713 = CARTESIAN_POINT ( 'NONE',  ( -23.15000000000000213, 11.75000000000000000, 11.75000000000000000 ) ) ;
#188714 = VECTOR ( 'NONE', #110350, 1000.000000000000000 ) ;
#188715 = CARTESIAN_POINT ( 'NONE',  ( -23.25000000000000000, 11.75000000001115552, -134.0000000000000284 ) ) ;
#188716 = AXIS2_PLACEMENT_3D ( 'NONE', #143094, #996, #44013 ) ;
#188717 = VECTOR ( 'NONE', #46604, 1000.000000000000000 ) ;
#188718 = ORIENTED_EDGE ( 'NONE', *, *, #156369, .T. ) ;
#188719 = VERTEX_POINT ( 'NONE', #4172 ) ;
#188720 = LINE ( 'NONE', #110464, #179147 ) ;
#188722 = ORIENTED_EDGE ( 'NONE', *, *, #116803, .F. ) ;
#188721 = LINE ( 'NONE', #54338, #254306 ) ;
#188723 = ORIENTED_EDGE ( 'NONE', *, *, #233129, .F. ) ;
#188724 = PLANE ( 'NONE',  #147753 ) ;
#188725 =( BOUNDED_CURVE ( )  B_SPLINE_CURVE ( 3, ( #248508, #245954, #210666, #8623 ),
 .UNSPECIFIED., .F., .F. ) 
 B_SPLINE_CURVE_WITH_KNOTS ( ( 4, 4 ),
 ( 0.06456096931748313283, 3.077031684272310219 ),
 .UNSPECIFIED. ) 
 CURVE ( )  GEOMETRIC_REPRESENTATION_ITEM ( )  RATIONAL_B_SPLINE_CURVE ( ( 1.000000000000000000, 0.3763440860215094830, 0.3763440860215094830, 1.000000000000000000 ) ) 
 REPRESENTATION_ITEM ( '' )  );
#188726 = ORIENTED_EDGE ( 'NONE', *, *, #55778, .F. ) ;
#188727 = CARTESIAN_POINT ( 'NONE',  ( 21.93340585971645851, 33.66454284798804508, -242.8670914416629500 ) ) ;
#188728 = EDGE_LOOP ( 'NONE', ( #99912, #114548, #201846, #113657 ) ) ;
#188729 = FACE_OUTER_BOUND ( 'NONE', #252569, .T. ) ;
#188731 = ORIENTED_EDGE ( 'NONE', *, *, #72732, .T. ) ;
#188730 = ORIENTED_EDGE ( 'NONE', *, *, #125002, .F. ) ;
#188732 = ORIENTED_EDGE ( 'NONE', *, *, #154440, .T. ) ;
#188733 = DIRECTION ( 'NONE',  ( -1.000000000000000000, -0.000000000000000000, -0.000000000000000000 ) ) ;
#188734 = ORIENTED_EDGE ( 'NONE', *, *, #211279, .F. ) ;
#188735 = ORIENTED_EDGE ( 'NONE', *, *, #132501, .T. ) ;
#188736 = CARTESIAN_POINT ( 'NONE',  ( 23.14999999999998437, 76.00000000001267608, -203.5231074845243597 ) ) ;
#188737 = CARTESIAN_POINT ( 'NONE',  ( -20.00857864376270001, 11.74265569217025629, -210.9797313238103698 ) ) ;
#188738 = TOROIDAL_SURFACE ( 'NONE', #18053, 12.77500000000000036, 0.1000000000000000056 ) ;
#188739 = CARTESIAN_POINT ( 'NONE',  ( 18.59999999999999076, 64.35000000001251408, -178.6731074845244507 ) ) ;
#188741 = ORIENTED_EDGE ( 'NONE', *, *, #194042, .T. ) ;
#188740 = DIRECTION ( 'NONE',  ( 0.000000000000000000, -1.000000000000000000, -6.982962677686266711E-15 ) ) ;
#188742 = CYLINDRICAL_SURFACE ( 'NONE', #228234, 4.000000000000003553 ) ;
#188743 = CARTESIAN_POINT ( 'NONE',  ( 23.14999999999998437, 4.049999999999998934, 5.021051876504146399E-16 ) ) ;
#188745 = ORIENTED_EDGE ( 'NONE', *, *, #189403, .T. ) ;
#188744 = CARTESIAN_POINT ( 'NONE',  ( 23.14999999999999858, 70.50000000001199396, -115.4283735034374274 ) ) ;
#188746 = DIRECTION ( 'NONE',  ( 0.000000000000000000, 0.000000000000000000, 1.000000000000000000 ) ) ;
#188747 = ORIENTED_EDGE ( 'NONE', *, *, #95168, .T. ) ;
#188748 = CARTESIAN_POINT ( 'NONE',  ( -23.25000000000000000, 1.115600667400684642E-11, -167.5000000000000284 ) ) ;
#188749 = EDGE_CURVE ( 'NONE', #256979, #236175, #97797, .T. ) ;
#188750 = ORIENTED_EDGE ( 'NONE', *, *, #228064, .F. ) ;
#188751 = CARTESIAN_POINT ( 'NONE',  ( -20.94999999999999929, 18.70793820085226500, -226.6056871674032323 ) ) ;
#188752 = FACE_OUTER_BOUND ( 'NONE', #64388, .T. ) ;
#188753 = EDGE_CURVE ( 'NONE', #222155, #229760, #248153, .T. ) ;
#188754 = ORIENTED_EDGE ( 'NONE', *, *, #157382, .F. ) ;
#188756 = DIRECTION ( 'NONE',  ( 0.000000000000000000, 0.000000000000000000, -1.000000000000000000 ) ) ;
#188755 = CARTESIAN_POINT ( 'NONE',  ( -21.07094088545368749, 75.90110629746051529, -209.8432747064414912 ) ) ;
#188757 = AXIS2_PLACEMENT_3D ( 'NONE', #235773, #16753, #233244 ) ;
#188758 = CARTESIAN_POINT ( 'NONE',  ( -21.05000000000000071, -1.851028230129704522, -78.65391326942254580 ) ) ;
#188759 = CYLINDRICAL_SURFACE ( 'NONE', #172278, 0.09999999999999939493 ) ;
#188760 = DIRECTION ( 'NONE',  ( 0.000000000000000000, -0.8814952561688476074, 0.4721928772777262417 ) ) ;
#188761 = ORIENTED_EDGE ( 'NONE', *, *, #28842, .T. ) ;
#188762 = ORIENTED_EDGE ( 'NONE', *, *, #232087, .F. ) ;
#188763 = EDGE_CURVE ( 'NONE', #82856, #429, #62870, .T. ) ;
#188764 = CARTESIAN_POINT ( 'NONE',  ( -23.25000000000000355, 65.08943781962308606, -222.1672656287770451 ) ) ;
#188765 = DIRECTION ( 'NONE',  ( 0.000000000000000000, 0.2617529984165033463, 0.9651348961777157509 ) ) ;
#188766 = ORIENTED_EDGE ( 'NONE', *, *, #145676, .F. ) ;
#188767 = FACE_OUTER_BOUND ( 'NONE', #37399, .T. ) ;
#188768 = VERTEX_POINT ( 'NONE', #99407 ) ;
#188769 = DIRECTION ( 'NONE',  ( -1.000000000000000000, 0.000000000000000000, 0.000000000000000000 ) ) ;
#188770 = DIRECTION ( 'NONE',  ( 2.952720810173289112E-16, -1.000000000000000000, 0.000000000000000000 ) ) ;
#188771 = EDGE_CURVE ( 'NONE', #192673, #193662, #173201, .T. ) ;
#188772 = CARTESIAN_POINT ( 'NONE',  ( -18.59999999999999787, -1.835859311432481045, -78.60443916879853532 ) ) ;
#188773 = ORIENTED_EDGE ( 'NONE', *, *, #118940, .F. ) ;
#188774 = AXIS2_PLACEMENT_3D ( 'NONE', #198500, #60267, #254918 ) ;
#188775 = EDGE_CURVE ( 'NONE', #119848, #230655, #238953, .T. ) ;
#188776 = DIRECTION ( 'NONE',  ( 0.000000000000000000, 6.982962677686266711E-15, -1.000000000000000000 ) ) ;
#188777 = FILL_AREA_STYLE ('',( #248767 ) ) ;
#188778 = VECTOR ( 'NONE', #78914, 1000.000000000000000 ) ;
#188779 = VERTEX_POINT ( 'NONE', #40776 ) ;
#188780 = ORIENTED_EDGE ( 'NONE', *, *, #109799, .T. ) ;
#188781 = ORIENTED_EDGE ( 'NONE', *, *, #126284, .F. ) ;
#188782 = AXIS2_PLACEMENT_3D ( 'NONE', #190302, #135433, #251536 ) ;
#188783 = CARTESIAN_POINT ( 'NONE',  ( 22.48660254037844197, 64.35000000001213039, -136.5731074845243995 ) ) ;
#188784 = DIRECTION ( 'NONE',  ( 0.000000000000000000, -0.2617529984165152257, -0.9651348961777124202 ) ) ;
#188785 = CARTESIAN_POINT ( 'NONE',  ( 21.05000000000000071, 76.00000000001267608, -203.5231074845243597 ) ) ;
#188786 = CARTESIAN_POINT ( 'NONE',  ( -23.15000000000000213, 76.00000000001195133, -103.0231074845243171 ) ) ;
#188787 = CARTESIAN_POINT ( 'NONE',  ( -18.50000000000000000, 5.341242990002803559, -57.19334979351202719 ) ) ;
#188788 = ADVANCED_FACE ( 'NONE', ( #181557 ), #43318, .F. ) ;
#188790 = CARTESIAN_POINT ( 'NONE',  ( 18.59999999999999432, -2.275048162540885155, -230.1697641654749305 ) ) ;
#188789 = FACE_OUTER_BOUND ( 'NONE', #64291, .T. ) ;
#188792 = ORIENTED_EDGE ( 'NONE', *, *, #38822, .F. ) ;
#188791 = FACE_OUTER_BOUND ( 'NONE', #66618, .T. ) ;
#188793 = CARTESIAN_POINT ( 'NONE',  ( -22.24259225415828212, 10.57914693326955735, -227.0818154154764841 ) ) ;
#188794 = EDGE_LOOP ( 'NONE', ( #137073, #20967, #90008, #250690 ) ) ;
#188795 = CARTESIAN_POINT ( 'NONE',  ( -21.05000000000000071, 64.35000000001268461, -203.4231074845244507 ) ) ;
#188796 = ORIENTED_EDGE ( 'NONE', *, *, #186283, .T. ) ;
#188797 = VERTEX_POINT ( 'NONE', #163272 ) ;
#188798 = DIRECTION ( 'NONE',  ( 0.000000000000000000, 0.000000000000000000, -1.000000000000000000 ) ) ;
#188800 = CIRCLE ( 'NONE', #84709, 0.1000000000000028644 ) ;
#188799 = PLANE ( 'NONE',  #60119 ) ;
#188801 = CARTESIAN_POINT ( 'NONE',  ( -16.94165728009537020, 66.01213024408774288, -48.63205247601419501 ) ) ;
#188802 = AXIS2_PLACEMENT_3D ( 'NONE', #241624, #85080, #202499 ) ;
#188803 = CARTESIAN_POINT ( 'NONE',  ( 21.05000000000000071, 5.850000000011105428, -77.13249722427801203 ) ) ;
#188804 = AXIS2_PLACEMENT_3D ( 'NONE', #5440, #100683, #81139 ) ;
#188805 = DIRECTION ( 'NONE',  ( 0.000000000000000000, 6.982962677686266711E-15, -1.000000000000000000 ) ) ;
#188806 = ORIENTED_EDGE ( 'NONE', *, *, #135989, .F. ) ;
#188807 = EDGE_LOOP ( 'NONE', ( #121895, #175560, #47093, #116234 ) ) ;
#188808 = AXIS2_PLACEMENT_3D ( 'NONE', #215706, #56609, #176622 ) ;
#188809 = CARTESIAN_POINT ( 'NONE',  ( -17.04761207306817639, 10.02645087340892438, -188.3499999999999943 ) ) ;
#188810 = VERTEX_POINT ( 'NONE', #221916 ) ;
#188811 = DIRECTION ( 'NONE',  ( 1.000000000000000000, 0.000000000000000000, 0.000000000000000000 ) ) ;
#188812 = CARTESIAN_POINT ( 'NONE',  ( 23.14999999999999503, 11.65000000001116298, -146.1500000000000341 ) ) ;
#188813 = EDGE_LOOP ( 'NONE', ( #160810, #56723, #58798, #69782 ) ) ;
#188814 = DIRECTION ( 'NONE',  ( 1.073024830501117923E-15, 0.9126074666063771490, 0.4088369013363281623 ) ) ;
#188815 = CARTESIAN_POINT ( 'NONE',  ( -20.85000000000000142, 7.120270961708750512, -70.65956304183931991 ) ) ;
#188816 = DIRECTION ( 'NONE',  ( 1.000000000000000000, 0.000000000000000000, -0.000000000000000000 ) ) ;
#188817 = DIRECTION ( 'NONE',  ( -1.040834085586050557E-13, 0.1575546449569757979, -0.9875102702516471709 ) ) ;
#188818 = ORIENTED_EDGE ( 'NONE', *, *, #2964, .T. ) ;
#188819 = DIRECTION ( 'NONE',  ( 1.000000000000000000, 0.000000000000000000, 0.000000000000000000 ) ) ;
#188820 = CIRCLE ( 'NONE', #26514, 0.09999999999999939493 ) ;
#188822 = CARTESIAN_POINT ( 'NONE',  ( 18.59999999999999076, 10.20857864377385127, -88.35000000000003695 ) ) ;
#188821 = AXIS2_PLACEMENT_3D ( 'NONE', #181312, #82158, #144716 ) ;
#188824 = DIRECTION ( 'NONE',  ( 0.000000000000000000, -0.2617529984165031243, -0.9651348961777157509 ) ) ;
#188823 = CIRCLE ( 'NONE', #59794, 0.1000000000000000472 ) ;
#188825 = AXIS2_PLACEMENT_3D ( 'NONE', #5702, #142651, #201360 ) ;
#188826 = DIRECTION ( 'NONE',  ( 1.000000000000000000, 0.000000000000000000, 0.000000000000000000 ) ) ;
#188827 = FACE_OUTER_BOUND ( 'NONE', #240292, .T. ) ;
#188828 = CARTESIAN_POINT ( 'NONE',  ( 18.42636655943170965, 77.14547211592135056, -241.8200727776024621 ) ) ;
#188829 = EDGE_CURVE ( 'NONE', #89024, #68660, #122859, .T. ) ;
#188830 = VERTEX_POINT ( 'NONE', #240242 ) ;
#188831 =( BOUNDED_SURFACE ( )  B_SPLINE_SURFACE ( 3, 2, ( 
 ( #224015, #199346, #200618 ),
 ( #85759, #222729, #124937 ),
 ( #84466, #204450, #100198 ),
 ( #25837, #119817, #179785 ) ),
 .UNSPECIFIED., .F., .F., .T. ) 
 B_SPLINE_SURFACE_WITH_KNOTS ( ( 4, 4 ),
 ( 3, 3 ),
 ( 5.727910411845712702, 5.983100554402350113 ),
 ( 0.000000000000000000, 1.000000000000000000 ),
 .UNSPECIFIED. ) 
 GEOMETRIC_REPRESENTATION_ITEM ( )  RATIONAL_B_SPLINE_SURFACE ( (
 ( 1.000000000000000000, 0.8946697475931897348, 1.000000000000000000),
 ( 1.000000000000000000, 0.9035312726221080837, 1.000000000000000000),
 ( 1.000000000000000000, 0.9104333467450060891, 1.000000000000000000),
 ( 1.000000000000000000, 0.9152888060719425178, 1.000000000000000000) ) ) 
 REPRESENTATION_ITEM ( '' )  SURFACE ( )  );
#188832 = CARTESIAN_POINT ( 'NONE',  ( -22.47071067811865319, 68.27992525551407255, -136.6221999392269595 ) ) ;
#188833 = ORIENTED_EDGE ( 'NONE', *, *, #93786, .F. ) ;
#188834 = EDGE_CURVE ( 'NONE', #130315, #256678, #223011, .T. ) ;
#188835 = CARTESIAN_POINT ( 'NONE',  ( -16.93860193097148326, 14.21179149064447422, -219.2948891565064002 ) ) ;
#188836 = DIRECTION ( 'NONE',  ( 1.000000000000000000, 0.000000000000000000, 0.000000000000000000 ) ) ;
#188837 = FACE_OUTER_BOUND ( 'NONE', #231677, .T. ) ;
#188838 = EDGE_LOOP ( 'NONE', ( #231972, #735, #99900, #210477 ) ) ;
#188839 = DIRECTION ( 'NONE',  ( 0.000000000000000000, 0.000000000000000000, -1.000000000000000000 ) ) ;
#188840 = CIRCLE ( 'NONE', #26352, 11.65000000000000036 ) ;
#188841 = DIRECTION ( 'NONE',  ( 0.000000000000000000, 0.000000000000000000, -1.000000000000000000 ) ) ;
#188842 = EDGE_CURVE ( 'NONE', #58209, #230546, #223214, .T. ) ;
#188843 = ADVANCED_FACE ( 'NONE', ( #68005 ), #239790, .T. ) ;
#188844 = LINE ( 'NONE', #89731, #76847 ) ;
#188846 = AXIS2_PLACEMENT_3D ( 'NONE', #81007, #99284, #101847 ) ;
#188845 = DIRECTION ( 'NONE',  ( 0.000000000000000000, -6.608470384673580212E-15, 1.000000000000000000 ) ) ;
#188847 = AXIS2_PLACEMENT_3D ( 'NONE', #181549, #45865, #105811 ) ;
#188848 = FACE_OUTER_BOUND ( 'NONE', #179938, .T. ) ;
#188849 = ORIENTED_EDGE ( 'NONE', *, *, #142265, .F. ) ;
#188850 = VERTEX_POINT ( 'NONE', #206236 ) ;
#188851 = DIRECTION ( 'NONE',  ( 0.000000000000000000, -6.938893903907222067E-15, 1.000000000000000000 ) ) ;
#188852 = CIRCLE ( 'NONE', #180480, 0.1000000000000002554 ) ;
#188853 = CARTESIAN_POINT ( 'NONE',  ( 22.45463910399148943, 1.026727559903908566E-11, -122.3504291898146192 ) ) ;
#188854 = PLANE ( 'NONE',  #31182 ) ;
#188855 = TOROIDAL_SURFACE ( 'NONE', #122216, 0.2000000000000000111, 0.1000000000000000056 ) ;
#188856 = DIRECTION ( 'NONE',  ( 0.000000000000000000, 0.8814952561688444987, -0.4721928772777320149 ) ) ;
#188857 = ADVANCED_FACE ( 'NONE', ( #189247 ), #252231, .T. ) ;
#188858 = ORIENTED_EDGE ( 'NONE', *, *, #255019, .F. ) ;
#188859 = LINE ( 'NONE', #149760, #80477 ) ;
#188860 = CIRCLE ( 'NONE', #76407, 3.899999999999996803 ) ;
#188861 = EDGE_CURVE ( 'NONE', #143844, #44981, #143906, .T. ) ;
#188863 = AXIS2_PLACEMENT_3D ( 'NONE', #29029, #26431, #224605 ) ;
#188862 = DIRECTION ( 'NONE',  ( 0.7071067811865487940, -4.937700262164522799E-15, 0.7071067811865463515 ) ) ;
#188864 = ORIENTED_EDGE ( 'NONE', *, *, #197077, .F. ) ;
#188865 = AXIS2_PLACEMENT_3D ( 'NONE', #158003, #80965, #61422 ) ;
#188866 = AXIS2_PLACEMENT_3D ( 'NONE', #122332, #1066, #162757 ) ;
#188867 = AXIS2_PLACEMENT_3D ( 'NONE', #158023, #176280, #133277 ) ;
#188868 = PRODUCT ( 'Injection Molded Chain Links 7', 'Injection Molded Chain Links 7', '', ( #193033 ) ) ;
#188869 = VECTOR ( 'NONE', #52033, 1000.000000000000000 ) ;
#188870 = VERTEX_POINT ( 'NONE', #70607 ) ;
#188871 = EDGE_LOOP ( 'NONE', ( #220309, #234908, #151830, #35718 ) ) ;
#188872 = EDGE_CURVE ( 'NONE', #36086, #231042, #25058, .T. ) ;
#188873 = ORIENTED_EDGE ( 'NONE', *, *, #183118, .F. ) ;
#188874 = EDGE_CURVE ( 'NONE', #87673, #27504, #139809, .T. ) ;
#188875 = LINE ( 'NONE', #57029, #234990 ) ;
#188876 = ADVANCED_FACE ( 'NONE', ( #107125 ), #186688, .F. ) ;
#188877 = CARTESIAN_POINT ( 'NONE',  ( 21.05000000000000071, 6.450000000011156587, -144.0170271704400307 ) ) ;
#188879 = CIRCLE ( 'NONE', #255466, 2.000000000000006661 ) ;
#188878 = CARTESIAN_POINT ( 'NONE',  ( 21.11344571971228490, 10.61787902352632962, -112.7460208923997840 ) ) ;
#188880 = FACE_OUTER_BOUND ( 'NONE', #158485, .T. ) ;
#188881 = FACE_OUTER_BOUND ( 'NONE', #192074, .T. ) ;
#188882 = DIRECTION ( 'NONE',  ( 0.000000000000000000, -6.853228547068871147E-15, 1.000000000000000000 ) ) ;
#188883 = CARTESIAN_POINT ( 'NONE',  ( 18.79999999999999361, -11.65000000000000036, -15.00000000000000000 ) ) ;
#188885 = CARTESIAN_POINT ( 'NONE',  ( -21.05000000000000071, 74.16465844978787914, -158.4679561919613775 ) ) ;
#188884 = CARTESIAN_POINT ( 'NONE',  ( 20.95520789717937404, 65.42306940062692888, -95.44287451064953132 ) ) ;
#188886 = AXIS2_PLACEMENT_3D ( 'NONE', #116239, #220469, #56221 ) ;
#188887 = DIRECTION ( 'NONE',  ( 0.000000000000000000, 0.000000000000000000, -1.000000000000000000 ) ) ;
#188888 = LINE ( 'NONE', #10259, #135462 ) ;
#188889 = DIRECTION ( 'NONE',  ( 1.000000000000000000, 0.000000000000000000, 0.000000000000000000 ) ) ;
#188890 = CARTESIAN_POINT ( 'NONE',  ( -18.59999999999999787, 1.749999999999999778, -11.66951155790164307 ) ) ;
#188891 = ORIENTED_EDGE ( 'NONE', *, *, #175577, .T. ) ;
#188892 = ORIENTED_EDGE ( 'NONE', *, *, #162409, .T. ) ;
#188893 = CARTESIAN_POINT ( 'NONE',  ( -18.41817142474038960, -9.498703066602091738, -40.10396548763700508 ) ) ;
#188894 = DIRECTION ( 'NONE',  ( -0.000000000000000000, -0.000000000000000000, -1.000000000000000000 ) ) ;
#188896 = CARTESIAN_POINT ( 'NONE',  ( -23.25000000000000000, 77.14957036958736580, -61.70719500002233815 ) ) ;
#188895 = CARTESIAN_POINT ( 'NONE',  ( -18.59999999999999787, 74.74783850729542678, -233.7633982527047465 ) ) ;
#188897 = CIRCLE ( 'NONE', #43152, 0.1000000000000066530 ) ;
#188898 = AXIS2_PLACEMENT_3D ( 'NONE', #185326, #113170, #75357 ) ;
#188899 = ADVANCED_FACE ( 'NONE', ( #148842 ), #177274, .F. ) ;
#188900 = DIRECTION ( 'NONE',  ( -1.000000000000000000, 0.000000000000000000, 0.000000000000000000 ) ) ;
#188901 = DIRECTION ( 'NONE',  ( 1.000000000000000000, 0.000000000000000000, 0.000000000000000000 ) ) ;
#188902 = CARTESIAN_POINT ( 'NONE',  ( 23.25000000000000000, 85.00000000001197975, -112.9170766071766820 ) ) ;
#188903 = ORIENTED_EDGE ( 'NONE', *, *, #243284, .F. ) ;
#188904 = ORIENTED_EDGE ( 'NONE', *, *, #256246, .T. ) ;
#188905 = EDGE_CURVE ( 'NONE', #92370, #139006, #48238, .T. ) ;
#188906 = CARTESIAN_POINT ( 'NONE',  ( 21.00000000000000000, 66.25000000001223555, -148.8731074845244393 ) ) ;
#188907 = ORIENTED_EDGE ( 'NONE', *, *, #142213, .F. ) ;
#188908 = CARTESIAN_POINT ( 'NONE',  ( -23.15000000000000213, 76.00000000001145395, -40.02310748452431710 ) ) ;
#188909 = AXIS2_PLACEMENT_3D ( 'NONE', #36346, #14220, #31239 ) ;
#188910 = CIRCLE ( 'NONE', #159694, 0.09999999999999609201 ) ;
#188911 = CIRCLE ( 'NONE', #5721, 3.899999999999999467 ) ;
#188912 = AXIS2_PLACEMENT_3D ( 'NONE', #84105, #122010, #166308 ) ;
#188913 = CARTESIAN_POINT ( 'NONE',  ( -20.54999999999999716, 64.71492276886415596, -217.8175830568236506 ) ) ;
#188914 = VERTEX_POINT ( 'NONE', #10609 ) ;
#188915 = CARTESIAN_POINT ( 'NONE',  ( 21.05000000000005400, 76.00000000001119815, -31.87310748452479459 ) ) ;
#188916 = EDGE_CURVE ( 'NONE', #187737, #99123, #39888, .T. ) ;
#188917 = ORIENTED_EDGE ( 'NONE', *, *, #69917, .F. ) ;
#188918 = CARTESIAN_POINT ( 'NONE',  ( 18.59999999999999432, -1.261786168553869603, -108.5864989635455089 ) ) ;
#188919 = DIRECTION ( 'NONE',  ( 0.000000000000000000, -0.9915357197604853789, 0.1298341882520022694 ) ) ;
#188920 = DIRECTION ( 'NONE',  ( -1.000000000000000000, -0.000000000000000000, 0.000000000000000000 ) ) ;
#188921 = EDGE_CURVE ( 'NONE', #200640, #82011, #73225, .T. ) ;
#188922 = CARTESIAN_POINT ( 'NONE',  ( -18.40000000000000213, 64.25000000001182343, -82.17310748452439384 ) ) ;
#188923 = DIRECTION ( 'NONE',  ( -1.000000000000000000, -0.000000000000000000, -0.000000000000000000 ) ) ;
#188924 = CARTESIAN_POINT ( 'NONE',  ( -22.47007471830799474, 1.115297090792388701E-11, -59.27928934807356143 ) ) ;
#188925 = CYLINDRICAL_SURFACE ( 'NONE', #105110, 2.599999999999998312 ) ;
#188926 = DIRECTION ( 'NONE',  ( 0.000000000000000000, 0.2617529984165152257, 0.9651348961777124202 ) ) ;
#188927 = EDGE_CURVE ( 'NONE', #74197, #170856, #56577, .T. ) ;
#188929 = VERTEX_POINT ( 'NONE', #90115 ) ;
#188928 = CARTESIAN_POINT ( 'NONE',  ( 19.75857864376268935, 11.65000000001115943, -58.25000000000000000 ) ) ;
#188931 = CARTESIAN_POINT ( 'NONE',  ( 21.14999999999999858, -11.64999999999999147, 3.469446951953614189E-15 ) ) ;
#188930 = FACE_OUTER_BOUND ( 'NONE', #9056, .T. ) ;
#188932 = ORIENTED_EDGE ( 'NONE', *, *, #7022, .T. ) ;
#188934 = ORIENTED_EDGE ( 'NONE', *, *, #251052, .F. ) ;
#188933 = DIRECTION ( 'NONE',  ( -1.000000000000000000, 0.000000000000000000, 0.000000000000000000 ) ) ;
#188935 = B_SPLINE_CURVE_WITH_KNOTS ( 'NONE', 3,
 ( #122259, #203065, #21875, #201779, #24464, #60984 ),
 .UNSPECIFIED., .F., .F.,
 ( 4, 2, 4 ),
 ( 0.000000000000000000, 0.0001497467027049249823, 0.0002994934054098499646 ),
 .UNSPECIFIED. ) ;
#188936 = ORIENTED_EDGE ( 'NONE', *, *, #182694, .F. ) ;
#188937 = CARTESIAN_POINT ( 'NONE',  ( -23.49999999999994316, 83.80000000001119531, -51.02310748452479316 ) ) ;
#188938 = DIRECTION ( 'NONE',  ( 0.000000000000000000, 1.000000000000000000, 0.000000000000000000 ) ) ;
#188939 = ADVANCED_FACE ( 'NONE', ( #185385 ), #6745, .T. ) ;
#188940 = VECTOR ( 'NONE', #257173, 1000.000000000000000 ) ;
#188941 = EDGE_CURVE ( 'NONE', #27505, #51895, #69107, .T. ) ;
#188942 = CARTESIAN_POINT ( 'NONE',  ( 22.41477678272288188, 75.99917613424879903, -81.17269276903972752 ) ) ;
#188943 = DIRECTION ( 'NONE',  ( 1.186688945009009831E-16, -1.000000000000000000, 0.000000000000000000 ) ) ;
#188944 = CARTESIAN_POINT ( 'NONE',  ( -23.30000000000000426, -11.79999999999999893, -347.0000000000001137 ) ) ;
#188945 = CARTESIAN_POINT ( 'NONE',  ( 18.59999999999999076, 10.49142135624846439, -125.2500000000000284 ) ) ;
#188946 = DIRECTION ( 'NONE',  ( 0.000000000000000000, -7.147358527629766941E-15, 1.000000000000000000 ) ) ;
#188947 = CARTESIAN_POINT ( 'NONE',  ( -18.59999999999999787, 66.75000000001230660, -157.6731074845244223 ) ) ;
#188948 = DIRECTION ( 'NONE',  ( 2.557131231893037478E-16, -0.8660254037844385966, 0.5000000000000003331 ) ) ;
#188949 = ORIENTED_EDGE ( 'NONE', *, *, #19883, .F. ) ;
#188950 = ORIENTED_EDGE ( 'NONE', *, *, #70749, .F. ) ;
#188951 = CARTESIAN_POINT ( 'NONE',  ( -16.93658623642901873, 9.980381671668284937, -180.1119027291291559 ) ) ;
#188952 = AXIS2_PLACEMENT_3D ( 'NONE', #223278, #202450, #206306 ) ;
#188953 = ADVANCED_FACE ( 'NONE', ( #88827 ), #81517, .T. ) ;
#188954 = VERTEX_POINT ( 'NONE', #28932 ) ;
#188955 = DIRECTION ( 'NONE',  ( 0.000000000000000000, 0.000000000000000000, -1.000000000000000000 ) ) ;
#188957 = ADVANCED_FACE ( 'NONE', ( #247917 ), #30186, .F. ) ;
#188956 = EDGE_LOOP ( 'NONE', ( #227130, #209222, #200369 ) ) ;
#188958 = AXIS2_PLACEMENT_3D ( 'NONE', #103739, #47624, #250654 ) ;
#188959 = CARTESIAN_POINT ( 'NONE',  ( 19.75857864376269291, 11.75000000000000711, -24.85000000000000142 ) ) ;
#188960 = EDGE_CURVE ( 'NONE', #50839, #206018, #75722, .T. ) ;
#188961 = DIRECTION ( 'NONE',  ( -1.000000000000000000, 0.000000000000000000, 0.000000000000000000 ) ) ;
#188962 = CARTESIAN_POINT ( 'NONE',  ( 21.40925344232283223, 75.90104981139307938, -210.1816263439147860 ) ) ;
#188963 = ORIENTED_EDGE ( 'NONE', *, *, #236578, .T. ) ;
#188964 = LINE ( 'NONE', #10340, #241051 ) ;
#188965 = CARTESIAN_POINT ( 'NONE',  ( -18.79999999999999716, 8.000000000000000000, 1.212568896937007867 ) ) ;
#188967 = AXIS2_PLACEMENT_3D ( 'NONE', #215832, #100992, #217112 ) ;
#188966 = DIRECTION ( 'NONE',  ( 1.186688945009010077E-16, 1.000000000000000000, 6.982962677686266711E-15 ) ) ;
#188968 = CARTESIAN_POINT ( 'NONE',  ( -21.12757541349819590, 0.005161215820883788274, -27.02661942874843604 ) ) ;
#188969 = CARTESIAN_POINT ( 'NONE',  ( -18.50000000000000000, 31.49702336731128582, -233.4564499823349877 ) ) ;
#188971 = VERTEX_POINT ( 'NONE', #116133 ) ;
#188970 = EDGE_CURVE ( 'NONE', #82680, #174398, #35959, .T. ) ;
#188973 = DIRECTION ( 'NONE',  ( 1.000000000000000000, 0.000000000000000000, 0.000000000000000000 ) ) ;
#188972 = CARTESIAN_POINT ( 'NONE',  ( -20.94999999999999929, 4.273531877263399892, -211.9976340888692050 ) ) ;
#188975 = ORIENTED_EDGE ( 'NONE', *, *, #73680, .T. ) ;
#188974 = AXIS2_PLACEMENT_3D ( 'NONE', #159174, #196971, #60024 ) ;
#188978 = ORIENTED_EDGE ( 'NONE', *, *, #7129, .F. ) ;
#188977 = CARTESIAN_POINT ( 'NONE',  ( -20.94999999999999929, 68.48451787451661232, -224.2224406095231757 ) ) ;
#188976 = DIRECTION ( 'NONE',  ( 0.000000000000000000, -1.000000000000000000, 0.000000000000000000 ) ) ;
#188979 = CARTESIAN_POINT ( 'NONE',  ( -17.11825945287482753, 10.05000000001113847, -113.1500000000000483 ) ) ;
#188980 = AXIS2_PLACEMENT_3D ( 'NONE', #220067, #38877, #19300 ) ;
#188982 = DIRECTION ( 'NONE',  ( 0.000000000000000000, 0.000000000000000000, -1.000000000000000000 ) ) ;
#188981 = AXIS2_PLACEMENT_3D ( 'NONE', #172049, #173347, #252817 ) ;
#188983 = EDGE_CURVE ( 'NONE', #102606, #59053, #173376, .T. ) ;
#188984 = CARTESIAN_POINT ( 'NONE',  ( 21.05000000000000071, 0.000000000000000000, 0.000000000000000000 ) ) ;
#188985 = EDGE_LOOP ( 'NONE', ( #254438, #30159, #131911, #116967 ) ) ;
#188986 = DIRECTION ( 'NONE',  ( 0.000000000000000000, 6.308085367183347448E-16, 1.000000000000000000 ) ) ;
#188987 = CARTESIAN_POINT ( 'NONE',  ( 23.24999999999999645, 76.00000000001142553, -36.02310748452432421 ) ) ;
#188989 = DIRECTION ( 'NONE',  ( -1.000000000000000000, 0.000000000000000000, 0.000000000000000000 ) ) ;
#188988 = DIRECTION ( 'NONE',  ( 0.000000000000000000, 1.776356839400155604E-15, 1.000000000000000000 ) ) ;
#188990 = ADVANCED_FACE ( 'NONE', ( #76985 ), #232239, .T. ) ;
#188992 = ORIENTED_EDGE ( 'NONE', *, *, #231751, .T. ) ;
#188991 = DIRECTION ( 'NONE',  ( -1.000000000000000000, 0.000000000000000000, 0.000000000000000000 ) ) ;
#188993 = CIRCLE ( 'NONE', #89007, 0.1000000000000124678 ) ;
#188994 = AXIS2_PLACEMENT_3D ( 'NONE', #239717, #21961, #101429 ) ;
#188995 = VECTOR ( 'NONE', #107131, 1000.000000000000000 ) ;
#188996 = ORIENTED_EDGE ( 'NONE', *, *, #194355, .F. ) ;
#188997 = CARTESIAN_POINT ( 'NONE',  ( -18.59999999999999787, 70.65875701002055109, -146.3297576910123610 ) ) ;
#188998 = CARTESIAN_POINT ( 'NONE',  ( -18.50000000000000000, 59.07123845373075710, -221.0531397865252075 ) ) ;
#188999 = CARTESIAN_POINT ( 'NONE',  ( -23.25000000000000000, -11.64999999998884483, -197.8999999999999773 ) ) ;
#189000 = VERTEX_POINT ( 'NONE', #212665 ) ;
#189001 = CARTESIAN_POINT ( 'NONE',  ( -16.78493211734304680, 9.945835743215326374, -188.3360509808959762 ) ) ;
#189002 = CIRCLE ( 'NONE', #55676, 11.80000000000000426 ) ;
#189003 = CARTESIAN_POINT ( 'NONE',  ( -21.00000000000000000, 6.742993295648862961, 9.658650260582458458 ) ) ;
#189004 = FACE_OUTER_BOUND ( 'NONE', #18385, .T. ) ;
#189005 = ORIENTED_EDGE ( 'NONE', *, *, #19191, .F. ) ;
#189006 = CARTESIAN_POINT ( 'NONE',  ( 20.13684514580243246, 60.19795610438474398, -225.5104338443611596 ) ) ;
#189007 = AXIS2_PLACEMENT_3D ( 'NONE', #177469, #133175, #174925 ) ;
#189008 = AXIS2_PLACEMENT_3D ( 'NONE', #124161, #101980, #242801 ) ;
#189009 = VECTOR ( 'NONE', #126325, 1000.000000000000000 ) ;
#189010 = VERTEX_POINT ( 'NONE', #230958 ) ;
#189011 = DIRECTION ( 'NONE',  ( -1.000000000000000000, -0.000000000000000000, -0.000000000000000000 ) ) ;
#189012 = CARTESIAN_POINT ( 'NONE',  ( -20.64999999999999858, 68.96522873961046685, -235.0783363939394235 ) ) ;
#189013 = ORIENTED_EDGE ( 'NONE', *, *, #55160, .F. ) ;
#189014 = VERTEX_POINT ( 'NONE', #171011 ) ;
#189015 = DIRECTION ( 'NONE',  ( -0.000000000000000000, 6.982962677686266711E-15, -1.000000000000000000 ) ) ;
#189016 = EDGE_CURVE ( 'NONE', #41107, #211171, #195685, .T. ) ;
#189017 = VERTEX_POINT ( 'NONE', #154017 ) ;
#189019 = ORIENTED_EDGE ( 'NONE', *, *, #127973, .T. ) ;
#189018 = CARTESIAN_POINT ( 'NONE',  ( 12.42718393586867265, 66.62934494888909853, -185.9972842285435490 ) ) ;
#189020 = ORIENTED_EDGE ( 'NONE', *, *, #56798, .F. ) ;
#189023 = ORIENTED_EDGE ( 'NONE', *, *, #203900, .F. ) ;
#189022 = ORIENTED_EDGE ( 'NONE', *, *, #69908, .F. ) ;
#189021 = CARTESIAN_POINT ( 'NONE',  ( 21.00000000000000000, 0.000000000000000000, 0.000000000000000000 ) ) ;
#189024 = AXIS2_PLACEMENT_3D ( 'NONE', #195027, #16388, #76320 ) ;
#189025 = AXIS2_PLACEMENT_3D ( 'NONE', #194442, #193145, #232286 ) ;
#189026 = CARTESIAN_POINT ( 'NONE',  ( -18.40000000000000213, -9.499999999988849808, -107.4221498493304949 ) ) ;
#189027 = VERTEX_POINT ( 'NONE', #211376 ) ;
#189028 = DIRECTION ( 'NONE',  ( 0.000000000000000000, 0.8700118002898393765, -0.4930308989875104575 ) ) ;
#189030 = EDGE_CURVE ( 'NONE', #148114, #194623, #110777, .T. ) ;
#189029 = CARTESIAN_POINT ( 'NONE',  ( -22.50000000000000000, 25.98655542988603173, -254.2226763854395983 ) ) ;
#189031 = CIRCLE ( 'NONE', #251383, 0.1000000000000072220 ) ;
#189032 = DIRECTION ( 'NONE',  ( 1.000000000000000000, 0.000000000000000000, 0.000000000000000000 ) ) ;
#189033 = CARTESIAN_POINT ( 'NONE',  ( -18.34374000495060386, 64.52683809664912928, -60.27310748452440947 ) ) ;
#189034 = ORIENTED_EDGE ( 'NONE', *, *, #167886, .F. ) ;
#189036 = ORIENTED_EDGE ( 'NONE', *, *, #244800, .T. ) ;
#189035 = AXIS2_PLACEMENT_3D ( 'NONE', #71863, #213917, #170996 ) ;
#189037 = DIRECTION ( 'NONE',  ( 0.000000000000000000, 0.9998779222360096863, -0.01562500000001061998 ) ) ;
#189038 = AXIS2_PLACEMENT_3D ( 'NONE', #256703, #98933, #238475 ) ;
#189040 = EDGE_LOOP ( 'NONE', ( #178681, #182636, #17863, #236172 ) ) ;
#189039 = CARTESIAN_POINT ( 'NONE',  ( 18.56308993302911503, 63.68807297684761437, -209.2612623977875614 ) ) ;
#189041 = DIRECTION ( 'NONE',  ( -1.000000000000000000, -0.000000000000000000, -0.000000000000000000 ) ) ;
#189043 = ORIENTED_EDGE ( 'NONE', *, *, #239502, .F. ) ;
#189042 = DIRECTION ( 'NONE',  ( -0.000000000000000000, 0.5469332180710856361, -0.8371762388950169109 ) ) ;
#189044 = ORIENTED_EDGE ( 'NONE', *, *, #190314, .F. ) ;
#189045 = AXIS2_PLACEMENT_3D ( 'NONE', #149447, #167731, #166457 ) ;
#189046 = AXIS2_PLACEMENT_3D ( 'NONE', #43922, #160048, #120925 ) ;
#189047 = ORIENTED_EDGE ( 'NONE', *, *, #170924, .T. ) ;
#189048 = AXIS2_PLACEMENT_3D ( 'NONE', #213455, #173102, #54383 ) ;
#189049 = CARTESIAN_POINT ( 'NONE',  ( -16.89318236219974523, 66.04846474213709939, -149.1679778524185735 ) ) ;
#189050 = CARTESIAN_POINT ( 'NONE',  ( -21.65000000000000213, 21.65523568329831505, -232.7692078405380300 ) ) ;
#189051 = B_SPLINE_CURVE_WITH_KNOTS ( 'NONE', 3,
 ( #31403, #190467, #11834, #91354, #52194, #92604, #172216, #232151, #41660, #160330 ),
 .UNSPECIFIED., .F., .F.,
 ( 4, 2, 2, 2, 4 ),
 ( 0.000000000000000000, 0.0003916577441626807577, 0.0005874866162440115685, 0.0006854010522846854577, 0.0007833154883253592386 ),
 .UNSPECIFIED. ) ;
#189052 = AXIS2_PLACEMENT_3D ( 'NONE', #89570, #29643, #229100 ) ;
#189054 = ORIENTED_EDGE ( 'NONE', *, *, #64632, .F. ) ;
#189053 = ORIENTED_EDGE ( 'NONE', *, *, #253638, .F. ) ;
#189055 = EDGE_LOOP ( 'NONE', ( #144626, #158341, #66131, #171139 ) ) ;
#189056 = CARTESIAN_POINT ( 'NONE',  ( -18.38639463286148867, 13.18566125533467215, -207.5951360497712699 ) ) ;
#189057 = ORIENTED_EDGE ( 'NONE', *, *, #156232, .T. ) ;
#189058 = VERTEX_POINT ( 'NONE', #173581 ) ;
#189059 = CARTESIAN_POINT ( 'NONE',  ( -22.94999999999999929, 3.461118860469513336, 28.84309995045515507 ) ) ;
#189061 = VERTEX_POINT ( 'NONE', #54842 ) ;
#189060 = DIRECTION ( 'NONE',  ( 1.000000000000000000, -0.000000000000000000, -0.000000000000000000 ) ) ;
#189062 = CARTESIAN_POINT ( 'NONE',  ( -22.57320508075687115, 12.67709964810647882, -223.3751320524553705 ) ) ;
#189063 = AXIS2_PLACEMENT_3D ( 'NONE', #193017, #252966, #14397 ) ;
#189065 = DIRECTION ( 'NONE',  ( 0.000000000000000000, 0.8814952561688429444, -0.4721928772777348460 ) ) ;
#189064 = CARTESIAN_POINT ( 'NONE',  ( 18.59999999999999432, -1.866714910057309273, -11.75267524628200633 ) ) ;
#189066 = CARTESIAN_POINT ( 'NONE',  ( 23.24999999999999645, 76.00000000001170974, -69.52310748452431710 ) ) ;
#189067 = DIRECTION ( 'NONE',  ( 0.000000000000000000, -1.000000000000000000, -6.982962677686266711E-15 ) ) ;
#189068 = ORIENTED_EDGE ( 'NONE', *, *, #202249, .T. ) ;
#189069 = ADVANCED_FACE ( 'NONE', ( #194398 ), #31481, .F. ) ;
#189070 = ORIENTED_EDGE ( 'NONE', *, *, #128426, .T. ) ;
#189071 = CIRCLE ( 'NONE', #214016, 0.09999999999999481526 ) ;
#189072 = DIRECTION ( 'NONE',  ( -1.000000000000000000, 0.000000000000000000, 0.000000000000000000 ) ) ;
#189073 = CARTESIAN_POINT ( 'NONE',  ( 0.9000000000000547562, 64.25000000001119815, -12.72310748452479245 ) ) ;
#189074 = EDGE_LOOP ( 'NONE', ( #15557, #74510, #88443, #221533 ) ) ;
#189075 = AXIS2_PLACEMENT_3D ( 'NONE', #181380, #236502, #243887 ) ;
#189076 = AXIS2_PLACEMENT_3D ( 'NONE', #68096, #245465, #249316 ) ;
#189077 = VECTOR ( 'NONE', #219649, 1000.000000000000000 ) ;
#189078 = FACE_OUTER_BOUND ( 'NONE', #244367, .T. ) ;
#189079 = EDGE_LOOP ( 'NONE', ( #211373, #83769, #35408, #44647 ) ) ;
#189080 = EDGE_LOOP ( 'NONE', ( #56774, #200321, #163356 ) ) ;
#189081 = EDGE_CURVE ( 'NONE', #11322, #199652, #202541, .T. ) ;
#189082 = CARTESIAN_POINT ( 'NONE',  ( -21.14999999999999858, 64.25000000001264766, -196.7392418215462726 ) ) ;
#189083 = CARTESIAN_POINT ( 'NONE',  ( 20.94999999999999574, -1.835341550213255957, -145.5551512925629822 ) ) ;
#189084 = ORIENTED_EDGE ( 'NONE', *, *, #103227, .F. ) ;
#189085 = CARTESIAN_POINT ( 'NONE',  ( -20.85000000000000142, 77.13501884592184865, -61.80613060109197932 ) ) ;
#189087 = VERTEX_POINT ( 'NONE', #11910 ) ;
#189086 =( REPRESENTATION_RELATIONSHIP ('NONE','NONE', #36900, #125202 ) REPRESENTATION_RELATIONSHIP_WITH_TRANSFORMATION ( #209713 )SHAPE_REPRESENTATION_RELATIONSHIP( ) );
#189088 = CARTESIAN_POINT ( 'NONE',  ( 18.41815437325347204, -9.498709853130273828, -140.6039458388020194 ) ) ;
#189089 = DIRECTION ( 'NONE',  ( 0.000000000000000000, 0.9126074666063771490, 0.4088369013363281623 ) ) ;
#189091 = SPHERICAL_SURFACE ( 'NONE', #170587, 0.1000000000000000056 ) ;
#189090 = CARTESIAN_POINT ( 'NONE',  ( 23.14999999999999858, 2.739812813550880577, -213.5801053551551547 ) ) ;
#189092 = EDGE_CURVE ( 'NONE', #188373, #162902, #56751, .T. ) ;
#189093 = CARTESIAN_POINT ( 'NONE',  ( 23.24999999999999645, 35.66731937946609321, -251.4023027391979497 ) ) ;
#189094 = CARTESIAN_POINT ( 'NONE',  ( -20.54999999999999716, 7.249999999999999112, -21.15000000000000213 ) ) ;
#189095 = DIRECTION ( 'NONE',  ( 0.000000000000000000, 2.891205793294679805E-16, -1.000000000000000000 ) ) ;
#189096 = DIRECTION ( 'NONE',  ( -1.000000000000000000, -0.000000000000000000, -0.000000000000000000 ) ) ;
#189097 = EDGE_CURVE ( 'NONE', #39052, #37010, #31707, .T. ) ;
#189099 = EDGE_LOOP ( 'NONE', ( #221005, #248096, #244180, #87355 ) ) ;
#189098 = VECTOR ( 'NONE', #14841, 1000.000000000000000 ) ;
#189100 = AXIS2_PLACEMENT_3D ( 'NONE', #67387, #146899, #90783 ) ;
#189101 = AXIS2_PLACEMENT_3D ( 'NONE', #214383, #155730, #177848 ) ;
#189103 = ORIENTED_EDGE ( 'NONE', *, *, #56287, .T. ) ;
#189102 = ORIENTED_EDGE ( 'NONE', *, *, #245561, .T. ) ;
#189104 = ORIENTED_EDGE ( 'NONE', *, *, #193679, .T. ) ;
#189105 = CYLINDRICAL_SURFACE ( 'NONE', #3580, 0.1000000000000046685 ) ;
#189106 = CARTESIAN_POINT ( 'NONE',  ( -18.50000000000000000, 74.74783850729544099, -233.7633982527047465 ) ) ;
#189107 = EDGE_CURVE ( 'NONE', #218397, #97404, #90101, .T. ) ;
#189109 = DIRECTION ( 'NONE',  ( 1.000000000000000000, 0.000000000000000000, 0.000000000000000000 ) ) ;
#189108 = CARTESIAN_POINT ( 'NONE',  ( -20.94999999999999929, 74.83729825007462466, -195.6231074845243540 ) ) ;
#189110 = DIRECTION ( 'NONE',  ( -1.000000000000000000, 0.000000000000000000, 0.000000000000000000 ) ) ;
#189111 = ORIENTED_EDGE ( 'NONE', *, *, #189774, .T. ) ;
#189112 = DIRECTION ( 'NONE',  ( -0.000000000000000000, -0.000000000000000000, 1.000000000000000000 ) ) ;
#189113 = EDGE_LOOP ( 'NONE', ( #239173, #60960, #127206, #200796 ) ) ;
#189114 = DIRECTION ( 'NONE',  ( 0.000000000000000000, 0.000000000000000000, -1.000000000000000000 ) ) ;
#189115 = EDGE_CURVE ( 'NONE', #2253, #185818, #239981, .T. ) ;
#189116 = DIRECTION ( 'NONE',  ( 1.000000000000000000, 3.190570557967288949E-16, 6.948722487160392945E-17 ) ) ;
#189117 = CARTESIAN_POINT ( 'NONE',  ( 22.39999999999999503, 64.35000000001267040, -203.5231074845244166 ) ) ;
#189118 = ORIENTED_EDGE ( 'NONE', *, *, #244606, .T. ) ;
#189119 = CARTESIAN_POINT ( 'NONE',  ( -16.81744102076748959, 9.950000000011138823, -121.3500000000000369 ) ) ;
#189120 = CARTESIAN_POINT ( 'NONE',  ( -23.15000000000000213, 76.00000000001267608, -203.5231074845243597 ) ) ;
#189121 = ORIENTED_EDGE ( 'NONE', *, *, #203075, .T. ) ;
#189122 = ORIENTED_EDGE ( 'NONE', *, *, #101597, .T. ) ;
#189123 = DIRECTION ( 'NONE',  ( 1.000000000000000000, -0.000000000000000000, -0.000000000000000000 ) ) ;
#189124 = CARTESIAN_POINT ( 'NONE',  ( -16.92778301347283687, 10.00094491684646769, -54.42851810796843637 ) ) ;
#189125 = CARTESIAN_POINT ( 'NONE',  ( 20.73486653747088937, 68.25000000001229239, -160.7731074845244166 ) ) ;
#189126 = CARTESIAN_POINT ( 'NONE',  ( 20.95224633520496127, 67.09947783345437244, -61.02983103660312025 ) ) ;
#189127 = CARTESIAN_POINT ( 'NONE',  ( -18.59999999999999787, 43.44873802792533724, -245.1397081572968659 ) ) ;
#189128 = CARTESIAN_POINT ( 'NONE',  ( 23.14999999999999858, 71.00000000001186606, -90.61784146561124942 ) ) ;
#189129 = ORIENTED_EDGE ( 'NONE', *, *, #19425, .F. ) ;
#189130 = CARTESIAN_POINT ( 'NONE',  ( 21.14999999999999858, 6.650000000011155876, -146.1500000000000341 ) ) ;
#189132 = EDGE_CURVE ( 'NONE', #237457, #256235, #248329, .T. ) ;
#189131 = CARTESIAN_POINT ( 'NONE',  ( -0.8999999999999438449, 67.72071067812984779, -13.99381816264344813 ) ) ;
#189134 = CARTESIAN_POINT ( 'NONE',  ( -21.12844524849339223, 11.75000000001115197, -174.4044134708423996 ) ) ;
#189133 = CARTESIAN_POINT ( 'NONE',  ( -16.93589915522259304, 10.00862525870701170, -87.94056010196035800 ) ) ;
#189135 = CARTESIAN_POINT ( 'NONE',  ( 18.59999999999999076, 10.99842653345846699, -220.2504445088529792 ) ) ;
#189136 = DIRECTION ( 'NONE',  ( 7.304098846218134667E-16, 1.000000000000000000, 6.982962677686266711E-15 ) ) ;
#189137 = CARTESIAN_POINT ( 'NONE',  ( -20.54999999999999716, 74.07476635515223506, -123.7928639513981892 ) ) ;
#189138 = CARTESIAN_POINT ( 'NONE',  ( 20.94999675878240808, 10.29307482169071442, -139.4586421466940465 ) ) ;
#189139 = AXIS2_PLACEMENT_3D ( 'NONE', #129329, #52340, #207602 ) ;
#189141 = ORIENTED_EDGE ( 'NONE', *, *, #235572, .T. ) ;
#189140 = CYLINDRICAL_SURFACE ( 'NONE', #131909, 11.80000000000000426 ) ;
#189142 = CIRCLE ( 'NONE', #222410, 0.09999999999998898659 ) ;
#189143 = CIRCLE ( 'NONE', #255721, 0.1000000000000079159 ) ;
#189144 = CIRCLE ( 'NONE', #14387, 0.09999999999999976963 ) ;
#189145 = EDGE_CURVE ( 'NONE', #232784, #204695, #71876, .T. ) ;
#189146 = EDGE_CURVE ( 'NONE', #42365, #125683, #36618, .T. ) ;
#189147 = FACE_OUTER_BOUND ( 'NONE', #60571, .T. ) ;
#189148 = B_SPLINE_CURVE_WITH_KNOTS ( 'NONE', 3,
 ( #199402, #98959, #59839, #63712, #3742, #222775, #201954, #83251, #181120, #24626 ),
 .UNSPECIFIED., .F., .F.,
 ( 4, 3, 3, 4 ),
 ( 0.000000000000000000, 0.0002000000000002877026, 0.001000000000045112155, 0.001967863649472104820 ),
 .UNSPECIFIED. ) ;
#189150 = DIRECTION ( 'NONE',  ( 1.000000000000000000, 0.000000000000000000, 0.000000000000000000 ) ) ;
#189149 = AXIS2_PLACEMENT_3D ( 'NONE', #1626, #84998, #47161 ) ;
#189151 = ADVANCED_FACE ( 'NONE', ( #193101 ), #40086, .F. ) ;
#189152 = CARTESIAN_POINT ( 'NONE',  ( 21.10000000000000142, 6.223900101154157483, 12.00000000000000000 ) ) ;
#189153 = ORIENTED_EDGE ( 'NONE', *, *, #124860, .F. ) ;
#189154 = AXIS2_PLACEMENT_3D ( 'NONE', #160001, #238219, #217360 ) ;
#189155 = EDGE_CURVE ( 'NONE', #232204, #59020, #223199, .T. ) ;
#189156 = DIRECTION ( 'NONE',  ( 0.000000000000000000, 1.000000000000000000, 0.000000000000000000 ) ) ;
#189157 = CIRCLE ( 'NONE', #222432, 0.09999999999999983902 ) ;
#189158 = CARTESIAN_POINT ( 'NONE',  ( -20.94999999999999929, 76.00000000001142553, -36.02310748452432421 ) ) ;
#189159 = CARTESIAN_POINT ( 'NONE',  ( 20.94999999999999929, 1.115600667400684642E-11, -169.5000000000000284 ) ) ;
#189160 = AXIS2_PLACEMENT_3D ( 'NONE', #246111, #11345, #27088 ) ;
#189161 = CIRCLE ( 'NONE', #55852, 0.4999999999999970024 ) ;
#189162 = EDGE_LOOP ( 'NONE', ( #210377, #226889, #14170, #81958 ) ) ;
#189163 = CARTESIAN_POINT ( 'NONE',  ( -23.25000000000000000, 77.83585931145570669, -125.0186683157258329 ) ) ;
#189165 = ORIENTED_EDGE ( 'NONE', *, *, #4274, .T. ) ;
#189164 = CARTESIAN_POINT ( 'NONE',  ( -21.05000000000000071, 1.115600667400684642E-11, -200.9999999999999432 ) ) ;
#189166 = DIRECTION ( 'NONE',  ( 1.000000000000000000, 0.000000000000000000, 0.000000000000000000 ) ) ;
#189167 = EDGE_CURVE ( 'NONE', #134983, #17708, #164939, .T. ) ;
#189168 = DIRECTION ( 'NONE',  ( 1.000000000000000000, 0.000000000000000000, 0.000000000000000000 ) ) ;
#189169 = ORIENTED_EDGE ( 'NONE', *, *, #168708, .T. ) ;
#189170 = DIRECTION ( 'NONE',  ( 0.7071067811865487940, -4.937700262164522799E-15, 0.7071067811865463515 ) ) ;
#189171 = B_SPLINE_CURVE_WITH_KNOTS ( 'NONE', 3,
 ( #231800, #33634, #14034, #187548, #130106, #209654, #218617, #235620, #55669, #179532 ),
 .UNSPECIFIED., .F., .F.,
 ( 4, 3, 3, 4 ),
 ( 0.000000000000000000, 4.874959354402235258E-05, 9.785140065120555329E-05, 0.0001360444631936037936 ),
 .UNSPECIFIED. ) ;
#189172 = VECTOR ( 'NONE', #129471, 1000.000000000000000 ) ;
#189173 = EDGE_CURVE ( 'NONE', #97016, #249890, #256854, .T. ) ;
#189174 = APPLICATION_PROTOCOL_DEFINITION ( 'draft international standard', 'automotive_design', 1998, #163958 ) ;
#189176 = CARTESIAN_POINT ( 'NONE',  ( -20.85882249326303040, 65.66751761918648356, -63.92826094061123143 ) ) ;
#189175 = AXIS2_PLACEMENT_3D ( 'NONE', #85927, #204610, #228043 ) ;
#189177 = EDGE_CURVE ( 'NONE', #191642, #248843, #215012, .T. ) ;
#189179 = CIRCLE ( 'NONE', #39359, 0.1000000000000013933 ) ;
#189178 = CARTESIAN_POINT ( 'NONE',  ( -23.39999999999994529, 77.83551161375991967, -47.52760213295649550 ) ) ;
#189180 = CARTESIAN_POINT ( 'NONE',  ( 23.14999999999999503, 66.40155400966892785, -213.5088390336144073 ) ) ;
#189181 = ORIENTED_EDGE ( 'NONE', *, *, #232710, .F. ) ;
#189182 = DIRECTION ( 'NONE',  ( 1.000000000000000000, 0.000000000000000000, 0.000000000000000000 ) ) ;
#189183 = LINE ( 'NONE', #185324, #209065 ) ;
#189184 = VECTOR ( 'NONE', #237719, 1000.000000000000000 ) ;
#189185 = EDGE_CURVE ( 'NONE', #95323, #128128, #177461, .T. ) ;
#189186 = AXIS2_PLACEMENT_3D ( 'NONE', #79283, #218800, #177155 ) ;
#189187 = DIRECTION ( 'NONE',  ( 0.000000000000000000, 0.000000000000000000, -1.000000000000000000 ) ) ;
#189188 = ORIENTED_EDGE ( 'NONE', *, *, #252959, .F. ) ;
#189189 = VERTEX_POINT ( 'NONE', #219054 ) ;
#189190 = EDGE_CURVE ( 'NONE', #11282, #128551, #101653, .T. ) ;
#189191 = EDGE_CURVE ( 'NONE', #203844, #186652, #162969, .T. ) ;
#189192 = AXIS2_PLACEMENT_3D ( 'NONE', #157602, #72923, #55856 ) ;
#189193 = CARTESIAN_POINT ( 'NONE',  ( -15.55912972643740488, 8.490870273573721150, -54.35000000000000142 ) ) ;
#189194 = CIRCLE ( 'NONE', #89399, 0.1000000000000028644 ) ;
#189195 = VECTOR ( 'NONE', #160039, 1000.000000000000000 ) ;
#189196 = CARTESIAN_POINT ( 'NONE',  ( 21.05000000000000071, 1.115600667400684642E-11, -100.5000000000000426 ) ) ;
#189197 = CARTESIAN_POINT ( 'NONE',  ( 21.05000005001280172, 8.871279691782060439, -146.1779475882454733 ) ) ;
#189199 = DIRECTION ( 'NONE',  ( 0.000000000000000000, 0.000000000000000000, -1.000000000000000000 ) ) ;
#189198 = CARTESIAN_POINT ( 'NONE',  ( -18.59999999999999787, 52.17883100310857003, -232.4626431718731396 ) ) ;
#189200 = LINE ( 'NONE', #95224, #135862 ) ;
#189201 = DIRECTION ( 'NONE',  ( -0.000000000000000000, -0.000000000000000000, -1.000000000000000000 ) ) ;
#189202 = FACE_OUTER_BOUND ( 'NONE', #239031, .T. ) ;
#189203 = EDGE_LOOP ( 'NONE', ( #254297, #1462, #229719, #159430 ) ) ;
#189205 = EDGE_LOOP ( 'NONE', ( #50858, #247132, #109687, #111072, #256876 ) ) ;
#189204 = CARTESIAN_POINT ( 'NONE',  ( -16.87487986503753845, 12.41403543382080343, -211.2428626618309693 ) ) ;
#189206 = FACE_OUTER_BOUND ( 'NONE', #59972, .T. ) ;
#189207 = CARTESIAN_POINT ( 'NONE',  ( -21.08621493067320429, -1.296228415900023023, -194.7841744112582205 ) ) ;
#189209 = DIRECTION ( 'NONE',  ( -1.000000000000000000, -2.952720810173289112E-16, 0.000000000000000000 ) ) ;
#189208 = CYLINDRICAL_SURFACE ( 'NONE', #34476, 0.5000000000000004441 ) ;
#189210 = EDGE_CURVE ( 'NONE', #158708, #182323, #61282, .T. ) ;
#189211 = VERTEX_POINT ( 'NONE', #12 ) ;
#189212 = CARTESIAN_POINT ( 'NONE',  ( 23.24999999999999645, 2.100000000011158274, -200.9999999999999432 ) ) ;
#189214 = ADVANCED_FACE ( 'NONE', ( #181250 ), #37890, .T. ) ;
#189213 = CARTESIAN_POINT ( 'NONE',  ( -21.05000000000000071, 74.14897176987143723, -158.3691942151018850 ) ) ;
#189215 = CARTESIAN_POINT ( 'NONE',  ( -21.05000000000001492, 69.45934304831069994, -103.0231074845243597 ) ) ;
#189216 = CYLINDRICAL_SURFACE ( 'NONE', #131467, 2.600000000000001421 ) ;
#189217 = VERTEX_POINT ( 'NONE', #83378 ) ;
#189218 = ORIENTED_EDGE ( 'NONE', *, *, #199545, .F. ) ;
#189219 = CIRCLE ( 'NONE', #89232, 12.87499999999999822 ) ;
#189220 = AXIS2_PLACEMENT_3D ( 'NONE', #15814, #74515, #56170 ) ;
#189221 = EDGE_CURVE ( 'NONE', #55329, #182665, #2574, .T. ) ;
#189222 = CARTESIAN_POINT ( 'NONE',  ( -23.15000000000000213, 1.115600667400684642E-11, -200.9999999999999432 ) ) ;
#189223 = VERTEX_POINT ( 'NONE', #100378 ) ;
#189224 = DIRECTION ( 'NONE',  ( -0.000000000000000000, -0.000000000000000000, 1.000000000000000000 ) ) ;
#189225 = AXIS2_PLACEMENT_3D ( 'NONE', #178366, #240888, #122222 ) ;
#189226 = ORIENTED_EDGE ( 'NONE', *, *, #222191, .F. ) ;
#189227 = DIRECTION ( 'NONE',  ( 1.000000000000000000, 0.000000000000000000, 0.000000000000000000 ) ) ;
#189228 = CARTESIAN_POINT ( 'NONE',  ( 18.59999999999999432, 44.52640028187936849, -247.3006740988509193 ) ) ;
#189229 = CIRCLE ( 'NONE', #76779, 0.5000000000000004441 ) ;
#189230 = CIRCLE ( 'NONE', #164295, 0.09999999999999939493 ) ;
#189231 = CARTESIAN_POINT ( 'NONE',  ( 21.14999999999999858, 65.28660755661216797, -124.1731074845243654 ) ) ;
#189232 = ORIENTED_EDGE ( 'NONE', *, *, #249922, .F. ) ;
#189233 = AXIS2_PLACEMENT_3D ( 'NONE', #107420, #190852, #150426 ) ;
#189234 = FACE_OUTER_BOUND ( 'NONE', #140217, .T. ) ;
#189236 = AXIS2_PLACEMENT_3D ( 'NONE', #240714, #178197, #176914 ) ;
#189235 = CARTESIAN_POINT ( 'NONE',  ( -18.50016250449483479, 68.01715840423038628, -224.2192812407666054 ) ) ;
#189237 = EDGE_CURVE ( 'NONE', #172274, #167246, #140822, .T. ) ;
#189238 = DIRECTION ( 'NONE',  ( 0.000000000000000000, 0.8814952561688476074, -0.4721928772777262417 ) ) ;
#189240 = AXIS2_PLACEMENT_3D ( 'NONE', #252373, #13786, #257155 ) ;
#189239 = CARTESIAN_POINT ( 'NONE',  ( 18.39999999999999503, 5.649999999999983480, -20.85000000000000142 ) ) ;
#189241 = AXIS2_PLACEMENT_3D ( 'NONE', #193596, #78758, #76195 ) ;
#189242 = ADVANCED_FACE ( 'NONE', ( #241218 ), #39177, .T. ) ;
#189243 = ORIENTED_EDGE ( 'NONE', *, *, #171607, .F. ) ;
#189245 = CARTESIAN_POINT ( 'NONE',  ( -16.94225986326250322, 9.950000000011138823, -180.4467193756078416 ) ) ;
#189244 = DIRECTION ( 'NONE',  ( 1.000000000000000000, 0.000000000000000000, -0.000000000000000000 ) ) ;
#189246 = VERTEX_POINT ( 'NONE', #217761 ) ;
#189248 = ORIENTED_EDGE ( 'NONE', *, *, #251302, .F. ) ;
#189247 = FACE_OUTER_BOUND ( 'NONE', #147530, .T. ) ;
#189249 = VECTOR ( 'NONE', #127428, 1000.000000000000000 ) ;
#189250 = ORIENTED_EDGE ( 'NONE', *, *, #213288, .F. ) ;
#189251 = CARTESIAN_POINT ( 'NONE',  ( -18.79999999999999716, -11.75000000000000000, -15.00000000000000000 ) ) ;
#189252 = FACE_OUTER_BOUND ( 'NONE', #143502, .T. ) ;
#189253 = CARTESIAN_POINT ( 'NONE',  ( 18.49999999999999289, 65.75000000001175238, -78.37310748452439668 ) ) ;
#189254 = DIRECTION ( 'NONE',  ( 0.000000000000000000, 0.1575844902526560010, 0.9875055080513781558 ) ) ;
#189255 = ORIENTED_EDGE ( 'NONE', *, *, #116300, .T. ) ;
#189256 = EDGE_CURVE ( 'NONE', #245795, #14612, #189885, .T. ) ;
#189257 = FACE_OUTER_BOUND ( 'NONE', #123640, .T. ) ;
#189259 = CARTESIAN_POINT ( 'NONE',  ( 18.49999999999999289, 10.25000000263022670, -158.6871719496316189 ) ) ;
#189258 = TOROIDAL_SURFACE ( 'NONE', #18373, 0.2000000000000000111, 0.1000000000000000056 ) ;
#189260 = EDGE_CURVE ( 'NONE', #2690, #138100, #244048, .T. ) ;
#189261 = ORIENTED_EDGE ( 'NONE', *, *, #242116, .F. ) ;
#189262 = CARTESIAN_POINT ( 'NONE',  ( 18.43473516226061548, -9.494942282747109275, -174.5458986833494919 ) ) ;
#189263 = CIRCLE ( 'NONE', #5881, 0.09999999999999939493 ) ;
#189264 = ADVANCED_FACE ( 'NONE', ( #159126 ), #139973, .T. ) ;
#189265 = CARTESIAN_POINT ( 'NONE',  ( -23.15000000000000213, 74.08971962618080909, -190.8917396293254285 ) ) ;
#189266 = ORIENTED_EDGE ( 'NONE', *, *, #77341, .T. ) ;
#189267 = CARTESIAN_POINT ( 'NONE',  ( -20.54999999999999716, 85.00000000001197975, -112.9170766071766820 ) ) ;
#189268 = TOROIDAL_SURFACE ( 'NONE', #176799, 0.2000000000000000111, 0.1000000000000000056 ) ;
#189269 = ADVANCED_FACE ( 'NONE', ( #122555 ), #23473, .T. ) ;
#189270 = ORIENTED_EDGE ( 'NONE', *, *, #10581, .T. ) ;
#189271 = CIRCLE ( 'NONE', #85163, 0.1000000000000001860 ) ;
#189272 = CARTESIAN_POINT ( 'NONE',  ( -22.39999999999999858, 75.90000000001242597, -177.8138870828977360 ) ) ;
#189275 = EDGE_CURVE ( 'NONE', #138714, #124845, #29886, .T. ) ;
#189274 = EDGE_CURVE ( 'NONE', #107696, #49099, #60886, .T. ) ;
#189273 = ORIENTED_EDGE ( 'NONE', *, *, #74095, .T. ) ;
#189276 = DIRECTION ( 'NONE',  ( 1.000000000000000000, 0.000000000000000000, 0.000000000000000000 ) ) ;
#189277 = CARTESIAN_POINT ( 'NONE',  ( -18.40000000000000213, 11.48667500176882861, -191.7499999999999716 ) ) ;
#189278 = LINE ( 'NONE', #88856, #168350 ) ;
#189279 = DIRECTION ( 'NONE',  ( -1.000000000000000000, -3.265361837132813093E-16, 0.000000000000000000 ) ) ;
#189280 = FACE_OUTER_BOUND ( 'NONE', #247758, .T. ) ;
#189281 = CARTESIAN_POINT ( 'NONE',  ( 19.58285714285715073, 66.98499851036331165, -94.60245466844267526 ) ) ;
#189283 = ORIENTED_EDGE ( 'NONE', *, *, #176034, .F. ) ;
#189282 = ADVANCED_FACE ( 'NONE', ( #183796 ), #206636, .T. ) ;
#189284 = VECTOR ( 'NONE', #227220, 1000.000000000000000 ) ;
#189286 = EDGE_CURVE ( 'NONE', #199333, #216543, #44298, .T. ) ;
#189285 = CARTESIAN_POINT ( 'NONE',  ( -23.15000000000000213, 1.115600667400684642E-11, -167.4999999999999716 ) ) ;
#189287 = EDGE_LOOP ( 'NONE', ( #139414, #10425, #60591, #248883 ) ) ;
#189289 = CARTESIAN_POINT ( 'NONE',  ( -21.05000000000000071, 70.15000000001235492, -159.8906102602464330 ) ) ;
#189288 = CARTESIAN_POINT ( 'NONE',  ( -20.94999999999999929, -11.74999999998884448, -170.5999999999999659 ) ) ;
#189290 = ORIENTED_EDGE ( 'NONE', *, *, #71831, .T. ) ;
#189291 = DIRECTION ( 'NONE',  ( 0.000000000000000000, -0.1575844902526579161, -0.9875055080513779338 ) ) ;
#189292 = CARTESIAN_POINT ( 'NONE',  ( -23.25000000000000355, 64.25000000001151079, -45.27310748452440947 ) ) ;
#189293 = ADVANCED_FACE ( 'NONE', ( #89813 ), #145939, .T. ) ;
#189294 = CARTESIAN_POINT ( 'NONE',  ( -21.05000000000000071, 14.81796439977981272, -236.5325475414793743 ) ) ;
#189295 = AXIS2_PLACEMENT_3D ( 'NONE', #195292, #251380, #209695 ) ;
#189296 = ORIENTED_EDGE ( 'NONE', *, *, #112499, .F. ) ;
#189298 = VERTEX_POINT ( 'NONE', #204626 ) ;
#189297 = CARTESIAN_POINT ( 'NONE',  ( 21.14999999999999858, 10.30543449102040654, -228.0143625250146329 ) ) ;
#189299 = CARTESIAN_POINT ( 'NONE',  ( 21.05000000000005400, 77.16254490893143725, -43.82310748452479743 ) ) ;
#189300 = EDGE_CURVE ( 'NONE', #57574, #201690, #203364, .T. ) ;
#189301 = CARTESIAN_POINT ( 'NONE',  ( -16.94878442675512886, 66.00827089702160322, -190.9113270601623071 ) ) ;
#189302 = EDGE_CURVE ( 'NONE', #103641, #108161, #6434, .T. ) ;
#189304 = VERTEX_POINT ( 'NONE', #226766 ) ;
#189303 = DIRECTION ( 'NONE',  ( 0.000000000000000000, 0.000000000000000000, 1.000000000000000000 ) ) ;
#189305 = VERTEX_POINT ( 'NONE', #5120 ) ;
#189306 = DIRECTION ( 'NONE',  ( -0.000000000000000000, 0.000000000000000000, 1.000000000000000000 ) ) ;
#189307 = VECTOR ( 'NONE', #87890, 1000.000000000000000 ) ;
#189308 = DIRECTION ( 'NONE',  ( 0.000000000000000000, 0.000000000000000000, -1.000000000000000000 ) ) ;
#189309 = VERTEX_POINT ( 'NONE', #9009 ) ;
#189310 = CARTESIAN_POINT ( 'NONE',  ( -16.94107738177414291, 51.68386028857255354, -231.8469600742508021 ) ) ;
#189311 = ORIENTED_EDGE ( 'NONE', *, *, #216367, .F. ) ;
#189313 = ADVANCED_FACE ( 'NONE', ( #26017 ), #84648, .T. ) ;
#189312 = DIRECTION ( 'NONE',  ( 1.000000000000000000, 0.000000000000000000, 0.000000000000000000 ) ) ;
#189314 = FACE_OUTER_BOUND ( 'NONE', #111370, .T. ) ;
#189315 = EDGE_LOOP ( 'NONE', ( #196351, #176488, #217760 ) ) ;
#189316 = DIRECTION ( 'NONE',  ( 4.408576920032447355E-17, -0.1350103645451876666, -0.9908441862701600211 ) ) ;
#189317 = ADVANCED_FACE ( 'NONE', ( #28629 ), #128966, .T. ) ;
#189318 = ORIENTED_EDGE ( 'NONE', *, *, #72723, .T. ) ;
#189319 = AXIS2_PLACEMENT_3D ( 'NONE', #229417, #67767, #92452 ) ;
#189320 = CARTESIAN_POINT ( 'NONE',  ( -17.29158576265543346, 10.36474766602906783, -122.5827582447922026 ) ) ;
#189321 = CIRCLE ( 'NONE', #39516, 11.65000000000000746 ) ;
#189322 = AXIS2_PLACEMENT_3D ( 'NONE', #59844, #159006, #181123 ) ;
#189323 = VECTOR ( 'NONE', #157188, 1000.000000000000000 ) ;
#189324 = ORIENTED_EDGE ( 'NONE', *, *, #5024, .T. ) ;
#189325 = ORIENTED_EDGE ( 'NONE', *, *, #105832, .F. ) ;
#189326 = CARTESIAN_POINT ( 'NONE',  ( -21.05000000000000071, 61.15173430017006240, -234.1841440743729379 ) ) ;
#189327 = ORIENTED_EDGE ( 'NONE', *, *, #50018, .T. ) ;
#189328 = COLOUR_RGB ( '', 0.09019608, 0.27058824, 0.51372549) ;
#189330 = EDGE_CURVE ( 'NONE', #104211, #234183, #197106, .T. ) ;
#189329 = CARTESIAN_POINT ( 'NONE',  ( -21.14999999999999858, 76.10000000001198828, -109.2731074845243029 ) ) ;
#189331 = ORIENTED_EDGE ( 'NONE', *, *, #56557, .T. ) ;
#189333 = ORIENTED_EDGE ( 'NONE', *, *, #248356, .T. ) ;
#189332 = LINE ( 'NONE', #96607, #26616 ) ;
#189334 = ORIENTED_EDGE ( 'NONE', *, *, #189465, .T. ) ;
#189335 = DIRECTION ( 'NONE',  ( 0.000000000000000000, 1.000000000000000000, 0.000000000000000000 ) ) ;
#189336 = VERTEX_POINT ( 'NONE', #164248 ) ;
#189339 = EDGE_LOOP ( 'NONE', ( #121593, #38670, #66037, #184914 ) ) ;
#189338 = VERTEX_POINT ( 'NONE', #48128 ) ;
#189337 = FACE_OUTER_BOUND ( 'NONE', #170390, .T. ) ;
#189341 = DIRECTION ( 'NONE',  ( -1.000000000000000000, 0.000000000000000000, 0.000000000000000000 ) ) ;
#189340 = AXIS2_PLACEMENT_3D ( 'NONE', #15473, #55826, #74181 ) ;
#189342 = DIRECTION ( 'NONE',  ( -3.469446951953995998E-14, 0.000000000000000000, 1.000000000000000000 ) ) ;
#189343 = EDGE_LOOP ( 'NONE', ( #164754, #60316, #129141, #192342 ) ) ;
#189344 = AXIS2_PLACEMENT_3D ( 'NONE', #23294, #157691, #101470 ) ;
#189345 = ADVANCED_FACE ( 'NONE', ( #242472 ), #69007, .T. ) ;
#189346 = VECTOR ( 'NONE', #89881, 1000.000000000000000 ) ;
#189347 = AXIS2_PLACEMENT_3D ( 'NONE', #173547, #95236, #174827 ) ;
#189348 = ORIENTED_EDGE ( 'NONE', *, *, #106158, .F. ) ;
#189349 = CARTESIAN_POINT ( 'NONE',  ( -21.05000000000000071, -11.41227409413852989, -70.00000000000004263 ) ) ;
#189351 = EDGE_LOOP ( 'NONE', ( #229467, #63290, #182927, #104272 ) ) ;
#189350 = CARTESIAN_POINT ( 'NONE',  ( -21.65000000000000213, 68.75000000001261924, -190.8731074845244109 ) ) ;
#189352 = DIRECTION ( 'NONE',  ( 0.000000000000000000, 0.000000000000000000, 1.000000000000000000 ) ) ;
#189353 = EDGE_LOOP ( 'NONE', ( #161072, #97519, #62175 ) ) ;
#189354 = CARTESIAN_POINT ( 'NONE',  ( -22.50000000000000000, 1.115600667400684642E-11, -21.85042919245520210 ) ) ;
#189355 = DIRECTION ( 'NONE',  ( 0.000000000000000000, 0.000000000000000000, -1.000000000000000000 ) ) ;
#189356 = VECTOR ( 'NONE', #255230, 1000.000000000000000 ) ;
#189357 = ORIENTED_EDGE ( 'NONE', *, *, #162620, .F. ) ;
#189358 = AXIS2_PLACEMENT_3D ( 'NONE', #164229, #8989, #243749 ) ;
#189359 = DIRECTION ( 'NONE',  ( 0.000000000000000000, 1.000000000000000000, 0.000000000000000000 ) ) ;
#189360 = DIRECTION ( 'NONE',  ( 0.000000000000000000, 0.000000000000000000, 1.000000000000000000 ) ) ;
#189361 = CIRCLE ( 'NONE', #68732, 0.09999999999999939493 ) ;
#189362 = ORIENTED_EDGE ( 'NONE', *, *, #98861, .F. ) ;
#189364 = EDGE_LOOP ( 'NONE', ( #45135, #180045, #96343, #195920 ) ) ;
#189363 = PLANE ( 'NONE',  #18104 ) ;
#189365 = AXIS2_PLACEMENT_3D ( 'NONE', #208862, #69367, #151481 ) ;
#189366 = CARTESIAN_POINT ( 'NONE',  ( 20.85000000000000142, 69.01799029515568407, -132.8269553662681233 ) ) ;
#189369 = ORIENTED_EDGE ( 'NONE', *, *, #232459, .F. ) ;
#189368 = ORIENTED_EDGE ( 'NONE', *, *, #39146, .T. ) ;
#189367 = VECTOR ( 'NONE', #210803, 1000.000000000000000 ) ;
#189370 = ORIENTED_EDGE ( 'NONE', *, *, #146188, .T. ) ;
#189371 = DIRECTION ( 'NONE',  ( 0.000000000000000000, -1.000000000000000000, -6.982962677686265922E-15 ) ) ;
#189372 = ORIENTED_EDGE ( 'NONE', *, *, #230080, .F. ) ;
#189373 = ORIENTED_EDGE ( 'NONE', *, *, #67100, .T. ) ;
#189374 = CARTESIAN_POINT ( 'NONE',  ( -18.40000000000000213, 30.85877660472528916, -233.5890472672530507 ) ) ;
#189375 = VERTEX_POINT ( 'NONE', #126386 ) ;
#189376 = CARTESIAN_POINT ( 'NONE',  ( -18.40000000000000213, 64.52683809664901560, -45.34905355133235361 ) ) ;
#189377 = AXIS2_PLACEMENT_3D ( 'NONE', #167231, #169808, #10698 ) ;
#189378 = LINE ( 'NONE', #30309, #77566 ) ;
#189379 = ORIENTED_EDGE ( 'NONE', *, *, #141777, .T. ) ;
#189380 = EDGE_CURVE ( 'NONE', #103462, #98749, #7737, .T. ) ;
#189381 = ORIENTED_EDGE ( 'NONE', *, *, #230793, .T. ) ;
#189382 = CARTESIAN_POINT ( 'NONE',  ( -23.15000000000000213, 28.56975825374500388, -258.1421690862028413 ) ) ;
#189383 = ORIENTED_EDGE ( 'NONE', *, *, #204174, .T. ) ;
#189384 = ORIENTED_EDGE ( 'NONE', *, *, #135200, .T. ) ;
#189385 = ADVANCED_FACE ( 'NONE', ( #205920 ), #144653, .F. ) ;
#189387 = ORIENTED_EDGE ( 'NONE', *, *, #45499, .F. ) ;
#189386 = CARTESIAN_POINT ( 'NONE',  ( -20.94999999999999929, 76.00000000001244871, -170.0231074845243597 ) ) ;
#189388 = CARTESIAN_POINT ( 'NONE',  ( 21.05000000000000071, 1.115600667400684642E-11, -129.6999999999999886 ) ) ;
#189389 = CARTESIAN_POINT ( 'NONE',  ( 21.05000000000000071, 64.40000000001218439, -143.4513107147999449 ) ) ;
#189390 = DIRECTION ( 'NONE',  ( 1.000000000000000000, 0.000000000000000000, 0.000000000000000000 ) ) ;
#189391 = EDGE_CURVE ( 'NONE', #229099, #160408, #11201, .T. ) ;
#189392 = DIRECTION ( 'NONE',  ( 0.000000000000000000, 6.982962677686267499E-15, -1.000000000000000000 ) ) ;
#189393 = AXIS2_PLACEMENT_3D ( 'NONE', #194085, #214905, #196619 ) ;
#189394 = CARTESIAN_POINT ( 'NONE',  ( -21.05000000000000071, -11.64999999999999858, -30.39999999999999503 ) ) ;
#189395 = DIRECTION ( 'NONE',  ( -2.557131231893036492E-16, 0.8496786552930076786, 0.5273008465188220306 ) ) ;
#189396 = CARTESIAN_POINT ( 'NONE',  ( 18.41832399655350727, 37.95493863640855636, -261.2294693916588244 ) ) ;
#189397 = AXIS2_PLACEMENT_3D ( 'NONE', #75476, #110721, #233266 ) ;
#189398 = CARTESIAN_POINT ( 'NONE',  ( -23.15000000000000213, -11.48912529306489994, -197.8999999999999773 ) ) ;
#189399 = CIRCLE ( 'NONE', #101878, 0.5000000000000004441 ) ;
#189400 = EDGE_CURVE ( 'NONE', #74892, #36453, #94381, .T. ) ;
#189401 = ORIENTED_EDGE ( 'NONE', *, *, #253933, .T. ) ;
#189402 = CIRCLE ( 'NONE', #230936, 0.6000000000000139666 ) ;
#189403 = EDGE_CURVE ( 'NONE', #231604, #232502, #12887, .T. ) ;
#189404 = ORIENTED_EDGE ( 'NONE', *, *, #132995, .T. ) ;
#189405 = VECTOR ( 'NONE', #107635, 1000.000000000000000 ) ;
#189407 = ORIENTED_EDGE ( 'NONE', *, *, #253489, .F. ) ;
#189406 = CARTESIAN_POINT ( 'NONE',  ( -18.59999999999999787, -1.851617760457748618, -78.60318971960367662 ) ) ;
#189408 = EDGE_CURVE ( 'NONE', #28201, #158172, #114530, .T. ) ;
#189409 = ORIENTED_EDGE ( 'NONE', *, *, #84100, .F. ) ;
#189410 = CARTESIAN_POINT ( 'NONE',  ( -16.87036670365549540, 66.01058118071020431, -90.50266760182644532 ) ) ;
#189411 = CARTESIAN_POINT ( 'NONE',  ( 18.59999999999999076, 77.83585931145526615, -57.91866831572577468 ) ) ;
#189412 = EDGE_CURVE ( 'NONE', #22873, #21979, #27795, .T. ) ;
#189414 = CARTESIAN_POINT ( 'NONE',  ( 21.09610168723073187, 1.521674863716753423, -230.6909948682581444 ) ) ;
#189413 = FACE_OUTER_BOUND ( 'NONE', #200129, .T. ) ;
#189415 = VERTEX_POINT ( 'NONE', #51963 ) ;
#189417 = ORIENTED_EDGE ( 'NONE', *, *, #79568, .F. ) ;
#189416 = TOROIDAL_SURFACE ( 'NONE', #68612, 0.2000000000000000111, 0.1000000000000000056 ) ;
#189418 = CIRCLE ( 'NONE', #22269, 11.65000000000000036 ) ;
#189419 = CARTESIAN_POINT ( 'NONE',  ( 18.52165635395191146, -9.481150711271022047, -40.52483758286248161 ) ) ;
#189420 = EDGE_CURVE ( 'NONE', #236987, #11381, #15311, .T. ) ;
#189421 = AXIS2_PLACEMENT_3D ( 'NONE', #228575, #227270, #108615 ) ;
#189422 = DIRECTION ( 'NONE',  ( -0.000000000000000000, 0.000000000000000000, -1.000000000000000000 ) ) ;
#189423 = VERTEX_POINT ( 'NONE', #169410 ) ;
#189424 = VERTEX_POINT ( 'NONE', #149824 ) ;
#189425 = AXIS2_PLACEMENT_3D ( 'NONE', #192799, #194096, #154974 ) ;
#189426 = FACE_OUTER_BOUND ( 'NONE', #97284, .T. ) ;
#189427 = DIRECTION ( 'NONE',  ( 0.000000000000000000, 0.000000000000000000, -1.000000000000000000 ) ) ;
#189428 = CARTESIAN_POINT ( 'NONE',  ( 21.04999999999999716, 65.37049252075402705, -61.89512808452796122 ) ) ;
#189429 = DIRECTION ( 'NONE',  ( 0.000000000000000000, 0.000000000000000000, 1.000000000000000000 ) ) ;
#189431 = VERTEX_POINT ( 'NONE', #54548 ) ;
#189430 = DIRECTION ( 'NONE',  ( 0.000000000000000000, 0.4088369013363281068, -0.9126074666063770380 ) ) ;
#189432 = EDGE_CURVE ( 'NONE', #55636, #63493, #127736, .T. ) ;
#189433 = AXIS2_PLACEMENT_3D ( 'NONE', #52234, #131788, #167104 ) ;
#189434 = CARTESIAN_POINT ( 'NONE',  ( -16.87683809663752399, 52.34166666667870516, -119.7731074845244592 ) ) ;
#189435 = DIRECTION ( 'NONE',  ( -1.000000000000000000, -0.000000000000000000, 0.000000000000000000 ) ) ;
#189436 = DIRECTION ( 'NONE',  ( 0.000000000000000000, 0.000000000000000000, -1.000000000000000000 ) ) ;
#189437 = CARTESIAN_POINT ( 'NONE',  ( 18.47073956224743085, 85.47172941248386735, -95.91442173170634078 ) ) ;
#189438 = ORIENTED_EDGE ( 'NONE', *, *, #31096, .T. ) ;
#189439 = CARTESIAN_POINT ( 'NONE',  ( 12.33938619321247643, 66.63927620602579793, -85.70918028991771109 ) ) ;
#189441 = EDGE_CURVE ( 'NONE', #125538, #83513, #165137, .T. ) ;
#189440 = CARTESIAN_POINT ( 'NONE',  ( -20.94999999999999929, 1.835341550235567887, -179.1551512925629197 ) ) ;
#189443 = DIRECTION ( 'NONE',  ( 0.000000000000000000, -0.2128009952263650861, 0.9770955615653305060 ) ) ;
#189442 = DIRECTION ( 'NONE',  ( 3.265361837132813093E-16, -1.000000000000000000, -0.000000000000000000 ) ) ;
#189444 = DIRECTION ( 'NONE',  ( 0.000000000000000000, -0.4999999999999348299, 0.8660254037844762331 ) ) ;
#189445 = CARTESIAN_POINT ( 'NONE',  ( -16.80621392010910142, 9.942202577518921558, -54.31040803458306243 ) ) ;
#189446 = DIRECTION ( 'NONE',  ( -0.000000000000000000, 1.000000000000000000, 0.000000000000000000 ) ) ;
#189447 = CARTESIAN_POINT ( 'NONE',  ( -20.54999999999999716, 76.00000000001142553, -36.02310748452432421 ) ) ;
#189448 = CARTESIAN_POINT ( 'NONE',  ( 18.46921299892754931, 85.50937817783589878, -129.5365287751537835 ) ) ;
#189449 = LINE ( 'NONE', #249427, #30977 ) ;
#189451 = ORIENTED_EDGE ( 'NONE', *, *, #228711, .T. ) ;
#189450 = VECTOR ( 'NONE', #181404, 1000.000000000000000 ) ;
#189452 = AXIS2_PLACEMENT_3D ( 'NONE', #228354, #147525, #49707 ) ;
#189453 = ORIENTED_EDGE ( 'NONE', *, *, #151575, .F. ) ;
#189454 = EDGE_LOOP ( 'NONE', ( #146619, #69287, #40738, #36413 ) ) ;
#189455 = EDGE_CURVE ( 'NONE', #108089, #56290, #16725, .T. ) ;
#189456 = CARTESIAN_POINT ( 'NONE',  ( 20.21494484322215968, 66.69682926214304075, -94.68284229275414532 ) ) ;
#189457 = CARTESIAN_POINT ( 'NONE',  ( -23.25000000000000000, 76.00000000001213607, -136.5231074845243313 ) ) ;
#189458 = ORIENTED_EDGE ( 'NONE', *, *, #19572, .T. ) ;
#189459 = EDGE_LOOP ( 'NONE', ( #38318, #178864, #9584, #141815 ) ) ;
#189460 = SURFACE_STYLE_USAGE ( .BOTH. , #48645 ) ;
#189461 = VERTEX_POINT ( 'NONE', #152401 ) ;
#189462 = CARTESIAN_POINT ( 'NONE',  ( 21.11825140030105175, 75.99279637937921450, -109.4685150499444575 ) ) ;
#189463 = CIRCLE ( 'NONE', #135272, 0.1000000000000028644 ) ;
#189464 = ORIENTED_EDGE ( 'NONE', *, *, #76556, .T. ) ;
#189465 = EDGE_CURVE ( 'NONE', #66864, #57960, #174559, .T. ) ;
#189466 = DIRECTION ( 'NONE',  ( 0.000000000000000000, 0.000000000000000000, -1.000000000000000000 ) ) ;
#189467 = FACE_OUTER_BOUND ( 'NONE', #66458, .T. ) ;
#189468 = CARTESIAN_POINT ( 'NONE',  ( 18.59999999999999432, 77.16270174995034381, -161.9231074845243370 ) ) ;
#189469 = TOROIDAL_SURFACE ( 'NONE', #110159, 2.100000000000002309, 0.1000000000000000056 ) ;
#189470 =( BOUNDED_CURVE ( )  B_SPLINE_CURVE ( 3, ( #97631, #196751, #177228, #80638 ),
 .UNSPECIFIED., .F., .F. ) 
 B_SPLINE_CURVE_WITH_KNOTS ( ( 4, 4 ),
 ( 0.06456096931748304957, 3.077031684272310219 ),
 .UNSPECIFIED. ) 
 CURVE ( )  GEOMETRIC_REPRESENTATION_ITEM ( )  RATIONAL_B_SPLINE_CURVE ( ( 1.000000000000000000, 0.3763440860215093164, 0.3763440860215093164, 1.000000000000000000 ) ) 
 REPRESENTATION_ITEM ( '' )  );
#189471 = DIRECTION ( 'NONE',  ( 0.000000000000000000, -1.000000000000000000, -6.982962677686265922E-15 ) ) ;
#189472 = DIRECTION ( 'NONE',  ( 1.000000000000000000, 2.952720810173289112E-16, -0.000000000000000000 ) ) ;
#189474 = VERTEX_POINT ( 'NONE', #192790 ) ;
#189473 = CARTESIAN_POINT ( 'NONE',  ( -16.97683810757273193, 29.66546359879749772, -234.5173184515128071 ) ) ;
#189475 = CARTESIAN_POINT ( 'NONE',  ( 21.05315837374230981, 11.74999999956163244, -26.65835599938597866 ) ) ;
#189476 = LINE ( 'NONE', #13412, #119311 ) ;
#189477 = ADVANCED_FACE ( 'NONE', ( #70298 ), #256654, .F. ) ;
#189478 = EDGE_LOOP ( 'NONE', ( #107854, #116393, #19080, #26605 ) ) ;
#189479 = CARTESIAN_POINT ( 'NONE',  ( 14.45204356427541903, 66.54933111084451980, -121.4675609943170400 ) ) ;
#189480 = DIRECTION ( 'NONE',  ( -1.000000000000000000, 0.000000000000000000, 0.000000000000000000 ) ) ;
#189481 = LINE ( 'NONE', #167372, #208283 ) ;
#189482 = EDGE_LOOP ( 'NONE', ( #11992, #44301, #123240, #247212, #87787 ) ) ;
#189483 = EDGE_CURVE ( 'NONE', #205485, #25805, #48597, .T. ) ;
#189484 = FACE_OUTER_BOUND ( 'NONE', #103001, .T. ) ;
#189485 = EDGE_CURVE ( 'NONE', #66400, #151038, #85995, .T. ) ;
#189486 = CARTESIAN_POINT ( 'NONE',  ( 21.15000000000003055, 84.00000000001119815, -34.86056257560453986 ) ) ;
#189487 = EDGE_CURVE ( 'NONE', #152757, #47719, #252736, .T. ) ;
#189488 = ORIENTED_EDGE ( 'NONE', *, *, #223923, .F. ) ;
#189489 = CIRCLE ( 'NONE', #164554, 0.9000000000000014655 ) ;
#189491 = CARTESIAN_POINT ( 'NONE',  ( 23.14999999999998437, 4.050000000011155343, -134.0000000000000000 ) ) ;
#189490 = VECTOR ( 'NONE', #203719, 1000.000000000000000 ) ;
#189492 = EDGE_CURVE ( 'NONE', #20936, #26749, #198445, .T. ) ;
#189493 = CYLINDRICAL_SURFACE ( 'NONE', #248596, 0.1000000000000028644 ) ;
#189494 = CARTESIAN_POINT ( 'NONE',  ( -16.77683809663752257, 51.60783545504968117, -231.9559722212415522 ) ) ;
#189495 = ORIENTED_EDGE ( 'NONE', *, *, #103954, .T. ) ;
#189496 = ORIENTED_EDGE ( 'NONE', *, *, #13535, .F. ) ;
#189497 = LINE ( 'NONE', #48681, #85983 ) ;
#189498 = DIRECTION ( 'NONE',  ( 0.000000000000000000, 0.9126074666063769270, 0.4088369013363280513 ) ) ;
#189499 = CARTESIAN_POINT ( 'NONE',  ( 20.84999999999998721, 65.66751761918722252, -164.4282609406112670 ) ) ;
#189500 = CARTESIAN_POINT ( 'NONE',  ( -21.05000000000000071, 75.90220970870291239, -75.78092209500043452 ) ) ;
#189503 = DIRECTION ( 'NONE',  ( 0.000000000000000000, 0.000000000000000000, 1.000000000000000000 ) ) ;
#189502 = VECTOR ( 'NONE', #98517, 1000.000000000000000 ) ;
#189501 = CARTESIAN_POINT ( 'NONE',  ( 22.59999999999999432, 75.90000000001222702, -148.1726782920690937 ) ) ;
#189505 = MANIFOLD_SOLID_BREP ( 'Stock-MAS-200-1', #7473 ) ;
#189504 = DIRECTION ( 'NONE',  ( 0.000000000000000000, 1.000000000000000000, 0.000000000000000000 ) ) ;
#189506 = CIRCLE ( 'NONE', #77060, 0.09999999999999939493 ) ;
#189507 = FACE_OUTER_BOUND ( 'NONE', #124221, .T. ) ;
#189508 = DIRECTION ( 'NONE',  ( 0.000000000000000000, 0.000000000000000000, -1.000000000000000000 ) ) ;
#189510 = ORIENTED_EDGE ( 'NONE', *, *, #239908, .T. ) ;
#189509 = AXIS2_PLACEMENT_3D ( 'NONE', #219918, #17855, #3421 ) ;
#189511 = CARTESIAN_POINT ( 'NONE',  ( 21.05000000000000071, 66.10573665986744629, -240.0052065600425806 ) ) ;
#189512 = VECTOR ( 'NONE', #66612, 999.9999999999998863 ) ;
#189513 = EDGE_CURVE ( 'NONE', #179904, #145361, #102743, .T. ) ;
#189515 = VERTEX_POINT ( 'NONE', #19275 ) ;
#189514 = CARTESIAN_POINT ( 'NONE',  ( 20.94999999999999929, 43.35377423437995503, -245.1717807829448930 ) ) ;
#189516 = LINE ( 'NONE', #52546, #122805 ) ;
#189517 = CARTESIAN_POINT ( 'NONE',  ( -18.59999999999999787, 11.64999999999999680, 11.75000000000000000 ) ) ;
#189518 = CYLINDRICAL_SURFACE ( 'NONE', #141928, 11.74999999999999645 ) ;
#189519 = CARTESIAN_POINT ( 'NONE',  ( -16.96982749440708815, 66.05000000001207638, -123.3983290757124962 ) ) ;
#189520 = EDGE_CURVE ( 'NONE', #138795, #216178, #115239, .T. ) ;
#189521 = CARTESIAN_POINT ( 'NONE',  ( 20.94560253601876809, 11.75000000001115907, -194.0100835125150240 ) ) ;
#189523 = ORIENTED_EDGE ( 'NONE', *, *, #138807, .T. ) ;
#189522 = DIRECTION ( 'NONE',  ( 0.000000000000000000, 0.8814952561688430555, -0.4721928772777346239 ) ) ;
#189524 = DIRECTION ( 'NONE',  ( 1.000000000000000000, 0.000000000000000000, 0.000000000000000000 ) ) ;
#189526 = EDGE_CURVE ( 'NONE', #127870, #221991, #38853, .T. ) ;
#189525 = LINE ( 'NONE', #250764, #41335 ) ;
#189527 = CARTESIAN_POINT ( 'NONE',  ( 22.49999999999999645, 11.64957080755595520, -66.90000000000004832 ) ) ;
#189529 = B_SPLINE_CURVE_WITH_KNOTS ( 'NONE', 3,
 ( #228222, #89968, #170865, #10455, #134229, #229504, #31333, #110821 ),
 .UNSPECIFIED., .F., .F.,
 ( 4, 2, 2, 4 ),
 ( 0.000000000000000000, 9.550056980124721853E-05, 0.0001910011396024944371, 0.0003820022792050102329 ),
 .UNSPECIFIED. ) ;
#189528 = CARTESIAN_POINT ( 'NONE',  ( 23.14999999999999858, -1.999999999988846699, -200.9999999999999432 ) ) ;
#189531 = ORIENTED_EDGE ( 'NONE', *, *, #196590, .T. ) ;
#189530 = B_SPLINE_CURVE_WITH_KNOTS ( 'NONE', 3,
 ( #95142, #6294, #106669, #105368, #45438, #63709, #161555 ),
 .UNSPECIFIED., .F., .F.,
 ( 4, 3, 4 ),
 ( 0.000000000000000000, 1.860045280646151707E-05, 5.251155757303908953E-05 ),
 .UNSPECIFIED. ) ;
#189532 = CYLINDRICAL_SURFACE ( 'NONE', #213715, 0.09999999999999939493 ) ;
#189533 = ORIENTED_EDGE ( 'NONE', *, *, #142766, .T. ) ;
#189534 = CARTESIAN_POINT ( 'NONE',  ( 23.04999999999999716, 13.78091005366907140, -222.8171174488881832 ) ) ;
#189535 = ORIENTED_EDGE ( 'NONE', *, *, #195282, .T. ) ;
#189536 = CARTESIAN_POINT ( 'NONE',  ( 23.24999999999999645, 1.115600667400684642E-11, -167.5000000000000284 ) ) ;
#189537 = CIRCLE ( 'NONE', #256081, 12.87499999999999822 ) ;
#189538 = ORIENTED_EDGE ( 'NONE', *, *, #213436, .T. ) ;
#189539 = VECTOR ( 'NONE', #178494, 1000.000000000000000 ) ;
#189540 = CARTESIAN_POINT ( 'NONE',  ( 22.60000000000000142, 1.115600667400684642E-11, -100.5000000000000284 ) ) ;
#189542 = FACE_OUTER_BOUND ( 'NONE', #133468, .T. ) ;
#189541 = AXIS2_PLACEMENT_3D ( 'NONE', #3512, #118355, #23115 ) ;
#189543 = PLANE ( 'NONE',  #47542 ) ;
#189544 = ORIENTED_EDGE ( 'NONE', *, *, #186006, .F. ) ;
#189545 =( BOUNDED_SURFACE ( )  B_SPLINE_SURFACE ( 3, 2, ( 
 ( #222329, #224913, #43726 ),
 ( #221064, #161117, #60699 ),
 ( #45010, #183243, #2009 ),
 ( #124559, #123263, #121982 ),
 ( #125820, #202795, #4580 ),
 ( #713, #42437, #81532 ) ),
 .UNSPECIFIED., .F., .F., .F. ) 
 B_SPLINE_SURFACE_WITH_KNOTS ( ( 4, 2, 4 ),
 ( 3, 3 ),
 ( 0.0001792624049599507918, 0.0003686986002124736754, 0.0005581347954649965590 ),
 ( 0.000000000000000000, 1.000000000000000000 ),
 .UNSPECIFIED. ) 
 GEOMETRIC_REPRESENTATION_ITEM ( )  RATIONAL_B_SPLINE_SURFACE ( (
 ( 1.000000000000000000, 0.9238795325112831858, 1.000000000000000000),
 ( 1.000000000000000000, 0.9229318695239602244, 1.000000000000000000),
 ( 1.000000000000000000, 0.8926288119229300877, 1.000000000000000000),
 ( 1.000000000000000000, 0.8123777807272952733, 1.000000000000000000),
 ( 1.000000000000000000, 0.7629087100930300736, 1.000000000000000000),
 ( 1.000000000000000000, 0.7071067811865475727, 1.000000000000000000) ) ) 
 REPRESENTATION_ITEM ( '' )  SURFACE ( )  );
#189546 = CIRCLE ( 'NONE', #152136, 0.5000000000000004441 ) ;
#189547 = CIRCLE ( 'NONE', #164604, 0.5000000000000013323 ) ;
#189549 = CARTESIAN_POINT ( 'NONE',  ( 13.99999999999999822, 47.91805600923871822, -233.7139610577891631 ) ) ;
#189548 = VECTOR ( 'NONE', #168870, 1000.000000000000000 ) ;
#189550 = EDGE_CURVE ( 'NONE', #114575, #151679, #117100, .T. ) ;
#189551 = DIRECTION ( 'NONE',  ( 0.000000000000000000, 0.9999631594459056361, -0.008583690987128059571 ) ) ;
#189552 = CARTESIAN_POINT ( 'NONE',  ( -20.94999999999999929, 64.35000000001262777, -196.5083017138704236 ) ) ;
#189553 = CARTESIAN_POINT ( 'NONE',  ( -21.05000000000000071, 1.148907358139439339E-11, -201.0000000000015064 ) ) ;
#189554 = DIRECTION ( 'NONE',  ( -1.000000000000000000, 0.000000000000000000, 0.000000000000000000 ) ) ;
#189555 = ORIENTED_EDGE ( 'NONE', *, *, #106949, .F. ) ;
#189557 = ORIENTED_EDGE ( 'NONE', *, *, #199209, .F. ) ;
#189556 = CARTESIAN_POINT ( 'NONE',  ( -22.47007471830799830, 7.720710651937626068, -167.4999999999999432 ) ) ;
#189558 = AXIS2_PLACEMENT_3D ( 'NONE', #43419, #60399, #122967 ) ;
#189559 = VERTEX_POINT ( 'NONE', #57090 ) ;
#189560 = DIRECTION ( 'NONE',  ( 1.000000000000000000, 0.000000000000000000, -0.000000000000000000 ) ) ;
#189561 = ORIENTED_EDGE ( 'NONE', *, *, #256578, .F. ) ;
#189562 = AXIS2_PLACEMENT_3D ( 'NONE', #56720, #215810, #17615 ) ;
#189563 = CARTESIAN_POINT ( 'NONE',  ( 21.46681500597532377, 1.115542391533913547E-11, -26.64248884056870281 ) ) ;
#189564 = CARTESIAN_POINT ( 'NONE',  ( -21.05000000000000071, -11.48912529306489994, -197.8999999999999773 ) ) ;
#189565 = VERTEX_POINT ( 'NONE', #196620 ) ;
#189566 = CARTESIAN_POINT ( 'NONE',  ( -16.90257928357874562, 66.04589317890669520, -123.8868220544106720 ) ) ;
#189567 = PLANE ( 'NONE',  #205296 ) ;
#189568 = DIRECTION ( 'NONE',  ( 0.000000000000000000, -0.9151430362303984989, 0.4031292884906871321 ) ) ;
#189569 = AXIS2_PLACEMENT_3D ( 'NONE', #18966, #174248, #232921 ) ;
#189570 = ORIENTED_EDGE ( 'NONE', *, *, #61307, .F. ) ;
#189571 = EDGE_CURVE ( 'NONE', #59872, #2800, #123628, .T. ) ;
#189573 = ORIENTED_EDGE ( 'NONE', *, *, #255068, .T. ) ;
#189572 = CARTESIAN_POINT ( 'NONE',  ( 21.05000000000003979, 83.98667523412385094, -34.76145429838185663 ) ) ;
#189574 = CARTESIAN_POINT ( 'NONE',  ( -23.25000000000000000, 1.115650265596050101E-11, -96.45000000000003126 ) ) ;
#189575 = PLANE ( 'NONE',  #248062 ) ;
#189576 = EDGE_CURVE ( 'NONE', #46245, #255159, #65174, .T. ) ;
#189577 = ORIENTED_EDGE ( 'NONE', *, *, #150062, .F. ) ;
#189578 =( BOUNDED_CURVE ( )  B_SPLINE_CURVE ( 3, ( #81292, #141302, #177878, #180432 ),
 .UNSPECIFIED., .F., .F. ) 
 B_SPLINE_CURVE_WITH_KNOTS ( ( 4, 4 ),
 ( 4.712388980384690562, 6.283185307179586232 ),
 .UNSPECIFIED. ) 
 CURVE ( )  GEOMETRIC_REPRESENTATION_ITEM ( )  RATIONAL_B_SPLINE_CURVE ( ( 1.000000000000000000, 0.8047378541243652705, 0.8047378541243652705, 1.000000000000000000 ) ) 
 REPRESENTATION_ITEM ( '' )  );
#189579 = CARTESIAN_POINT ( 'NONE',  ( -21.05000000000000071, 87.65000000001192859, -105.9231074845242091 ) ) ;
#189581 = ADVANCED_FACE ( 'NONE', ( #79224 ), #202716, .F. ) ;
#189580 = DIRECTION ( 'NONE',  ( -0.8660254037844744568, -0.4563037333031724763, -0.2044184506680482571 ) ) ;
#189582 = DIRECTION ( 'NONE',  ( 0.000000000000000000, -0.2617529984164915779, -0.9651348961777189706 ) ) ;
#189584 = ADVANCED_FACE ( 'NONE', ( #40155 ), #237043, .T. ) ;
#189583 = VERTEX_POINT ( 'NONE', #97494 ) ;
#189585 = DIRECTION ( 'NONE',  ( 0.000000000000000000, 0.8660254037844377084, 0.5000000000000016653 ) ) ;
#189586 = CARTESIAN_POINT ( 'NONE',  ( -22.39999999999999858, -2.598867842139048534, -189.5410128746472083 ) ) ;
#189587 = DIRECTION ( 'NONE',  ( -1.000000000000000000, -0.000000000000000000, -0.000000000000000000 ) ) ;
#189588 = VECTOR ( 'NONE', #164584, 1000.000000000000000 ) ;
#189589 = EDGE_LOOP ( 'NONE', ( #218407, #145714, #100245, #157029 ) ) ;
#189590 = AXIS2_PLACEMENT_3D ( 'NONE', #18993, #80221, #256257 ) ;
#189591 = AXIS2_PLACEMENT_3D ( 'NONE', #53307, #51997, #149856 ) ;
#189592 = ADVANCED_FACE ( 'NONE', ( #163604 ), #156251, .F. ) ;
#189593 = ADVANCED_FACE ( 'NONE', ( #58369 ), #243126, .F. ) ;
#189594 = EDGE_LOOP ( 'NONE', ( #210277, #243489, #16831, #75497, #115947 ) ) ;
#189595 = DIRECTION ( 'NONE',  ( -1.000000000000000000, 2.952720810173289112E-16, 2.061873921506763405E-30 ) ) ;
#189596 = CIRCLE ( 'NONE', #18705, 4.049999999999994493 ) ;
#189597 = VECTOR ( 'NONE', #145823, 1000.000000000000000 ) ;
#189598 = ORIENTED_EDGE ( 'NONE', *, *, #161052, .T. ) ;
#189599 = CARTESIAN_POINT ( 'NONE',  ( -21.05000000000000071, 11.60000000001115517, -60.07179676972450011 ) ) ;
#189600 = PLANE ( 'NONE',  #253956 ) ;
#189602 = ORIENTED_EDGE ( 'NONE', *, *, #123062, .T. ) ;
#189601 = DIRECTION ( 'NONE',  ( 0.000000000000000000, 0.2617529984165152257, 0.9651348961777124202 ) ) ;
#189603 = DIRECTION ( 'NONE',  ( -1.000000000000000000, -3.265361837132813093E-16, 0.000000000000000000 ) ) ;
#189604 = CARTESIAN_POINT ( 'NONE',  ( 21.06490991615909536, 65.27510865242446414, -57.31939613099126518 ) ) ;
#189605 = CARTESIAN_POINT ( 'NONE',  ( 20.94999999999999574, 44.52640028187936849, -247.3006740988509193 ) ) ;
#189606 = DIRECTION ( 'NONE',  ( -1.000000000000000000, 0.000000000000000000, 0.000000000000000000 ) ) ;
#189607 = DIRECTION ( 'NONE',  ( 2.952720810173289112E-16, -1.000000000000000000, 0.000000000000000000 ) ) ;
#189608 = PLANE ( 'NONE',  #130457 ) ;
#189610 = ADVANCED_FACE ( 'NONE', ( #136638 ), #59653, .T. ) ;
#189609 = CARTESIAN_POINT ( 'NONE',  ( -21.37071067811865532, 8.070710678118656389, -21.25000000000000000 ) ) ;
#189612 = EDGE_LOOP ( 'NONE', ( #222944, #210856, #241884, #2533 ) ) ;
#189611 = DIRECTION ( 'NONE',  ( 0.000000000000000000, -0.000000000000000000, 1.000000000000000000 ) ) ;
#189613 = CIRCLE ( 'NONE', #156314, 0.1000000000000012546 ) ;
#189614 = ADVANCED_FACE ( 'NONE', ( #223547 ), #592, .F. ) ;
#189615 = DIRECTION ( 'NONE',  ( 0.000000000000000000, 0.000000000000000000, -1.000000000000000000 ) ) ;
#189616 = LINE ( 'NONE', #190920, #240346 ) ;
#189617 = AXIS2_PLACEMENT_3D ( 'NONE', #168849, #108816, #253462 ) ;
#189619 = EDGE_CURVE ( 'NONE', #134440, #195402, #223373, .T. ) ;
#189618 = DIRECTION ( 'NONE',  ( 1.000000000000000000, 0.000000000000000000, 0.000000000000000000 ) ) ;
#189620 = DIRECTION ( 'NONE',  ( 1.000000000000000000, 0.000000000000000000, 0.000000000000000000 ) ) ;
#189621 = ORIENTED_EDGE ( 'NONE', *, *, #72661, .F. ) ;
#189622 = DIRECTION ( 'NONE',  ( -1.000000000000000000, -0.000000000000000000, -0.000000000000000000 ) ) ;
#189623 = CARTESIAN_POINT ( 'NONE',  ( -20.94999999999999929, -11.39257802170566869, -30.42605042016806394 ) ) ;
#189624 = EDGE_CURVE ( 'NONE', #38825, #152824, #150485, .T. ) ;
#189626 = ORIENTED_EDGE ( 'NONE', *, *, #186460, .T. ) ;
#189625 = B_SPLINE_CURVE_WITH_KNOTS ( 'NONE', 3,
 ( #131266, #11325, #210808, #92141, #53005, #32194, #111707, #186112, #249937, #150832, #152145, #171716, #188674, #10036, #148265, #72602, #132560, #7466, #191275 ),
 .UNSPECIFIED., .F., .F.,
 ( 4, 3, 3, 3, 3, 3, 4 ),
 ( 0.000000000000000000, 7.110282409889913185E-05, 0.0001508797727291428831, 0.0002027344179858457109, 0.0002343294522349018149, 0.0002454816334821171078, 0.0002619873080085533793 ),
 .UNSPECIFIED. ) ;
#189627 = TOROIDAL_SURFACE ( 'NONE', #222927, 0.9750000000000019762, 0.1000000000000000056 ) ;
#189628 = DIRECTION ( 'NONE',  ( -4.336808689941751890E-15, -0.8660254037844445918, -0.4999999999999897304 ) ) ;
#189629 = VECTOR ( 'NONE', #211714, 1000.000000000000000 ) ;
#189630 = DIRECTION ( 'NONE',  ( -1.000000000000000000, 0.000000000000000000, 0.000000000000000000 ) ) ;
#189631 = ORIENTED_EDGE ( 'NONE', *, *, #124741, .T. ) ;
#189632 = DIRECTION ( 'NONE',  ( 0.000000000000000000, 0.000000000000000000, 1.000000000000000000 ) ) ;
#189633 = ORIENTED_EDGE ( 'NONE', *, *, #3460, .T. ) ;
#189634 = EDGE_CURVE ( 'NONE', #144497, #181396, #61069, .T. ) ;
#189635 = FACE_OUTER_BOUND ( 'NONE', #85827, .T. ) ;
#189637 = ORIENTED_EDGE ( 'NONE', *, *, #190461, .F. ) ;
#189636 = DIRECTION ( 'NONE',  ( 1.000000000000000000, 7.136802563874199107E-16, 1.554319503706929991E-16 ) ) ;
#189638 = FACE_OUTER_BOUND ( 'NONE', #33461, .T. ) ;
#189639 = ORIENTED_EDGE ( 'NONE', *, *, #162200, .T. ) ;
#189640 = DIRECTION ( 'NONE',  ( 2.342056488767301376E-15, 0.1350103645451835865, 0.9908441862701605762 ) ) ;
#189641 = ORIENTED_EDGE ( 'NONE', *, *, #78201, .F. ) ;
#189642 = ORIENTED_EDGE ( 'NONE', *, *, #225891, .T. ) ;
#189643 = CARTESIAN_POINT ( 'NONE',  ( 18.46082813848004278, 85.48074965091954880, -129.4387373818085791 ) ) ;
#189644 = ORIENTED_EDGE ( 'NONE', *, *, #195768, .T. ) ;
#189645 = ORIENTED_EDGE ( 'NONE', *, *, #50019, .T. ) ;
#189646 = AXIS2_PLACEMENT_3D ( 'NONE', #230592, #33711, #154924 ) ;
#189647 = VERTEX_POINT ( 'NONE', #249571 ) ;
#189648 = DIRECTION ( 'NONE',  ( 0.000000000000000000, -1.000000000000000000, 0.000000000000000000 ) ) ;
#189649 = DIRECTION ( 'NONE',  ( 1.000000000000000000, 2.952720810173289112E-16, -0.000000000000000000 ) ) ;
#189650 = CARTESIAN_POINT ( 'NONE',  ( 20.94999999999999574, 77.26178616857691850, -94.93660852097882241 ) ) ;
#189651 = ORIENTED_EDGE ( 'NONE', *, *, #257457, .T. ) ;
#189652 = DIRECTION ( 'NONE',  ( 0.000000000000000000, 0.000000000000000000, 1.000000000000000000 ) ) ;
#189653 = CARTESIAN_POINT ( 'NONE',  ( 20.94999999999999574, 1.849084418638171856, -179.1560105214470866 ) ) ;
#189654 = CYLINDRICAL_SURFACE ( 'NONE', #114598, 0.09999999999999939493 ) ;
#189655 = ORIENTED_EDGE ( 'NONE', *, *, #223906, .T. ) ;
#189656 = DIRECTION ( 'NONE',  ( 0.000000000000000000, -1.000000000000000000, -6.982962677686265922E-15 ) ) ;
#189657 = DIRECTION ( 'NONE',  ( -0.000000000000000000, -6.982962677686266711E-15, 1.000000000000000000 ) ) ;
#189658 = DIRECTION ( 'NONE',  ( 1.000000000000000000, 0.000000000000000000, 0.000000000000000000 ) ) ;
#189659 = CARTESIAN_POINT ( 'NONE',  ( -20.85000000000000142, 68.87972903831452243, -132.8635444426850825 ) ) ;
#189660 = ORIENTED_EDGE ( 'NONE', *, *, #175313, .T. ) ;
#189661 = CARTESIAN_POINT ( 'NONE',  ( 23.14999999999999503, 60.92570327216495230, -205.2374328603434890 ) ) ;
#189662 = ORIENTED_EDGE ( 'NONE', *, *, #204809, .F. ) ;
#189663 = CARTESIAN_POINT ( 'NONE',  ( -18.51991288638565081, -7.657214099531299389, -209.9783737948318389 ) ) ;
#189664 = ORIENTED_EDGE ( 'NONE', *, *, #1437, .T. ) ;
#189665 = AXIS2_PLACEMENT_3D ( 'NONE', #133549, #31912, #52718 ) ;
#189666 = CIRCLE ( 'NONE', #93790, 0.09999999999998898659 ) ;
#189667 = DIRECTION ( 'NONE',  ( 0.000000000000000000, -6.467318590049456648E-15, 1.000000000000000000 ) ) ;
#189668 = CARTESIAN_POINT ( 'NONE',  ( 18.39999999999999503, 64.52683809664952719, -115.6731074845243796 ) ) ;
#189669 = ORIENTED_EDGE ( 'NONE', *, *, #173799, .F. ) ;
#189670 = ORIENTED_EDGE ( 'NONE', *, *, #179694, .F. ) ;
#189671 = DIRECTION ( 'NONE',  ( 0.000000000000000000, 1.000000000000000000, -6.308085367188393199E-16 ) ) ;
#189672 = LINE ( 'NONE', #150551, #50627 ) ;
#189673 = EDGE_LOOP ( 'NONE', ( #202428, #168865, #34668, #244849 ) ) ;
#189674 = DIRECTION ( 'NONE',  ( 1.000000000000000000, 7.304098846218134667E-16, 0.000000000000000000 ) ) ;
#189675 = CARTESIAN_POINT ( 'NONE',  ( 18.59999999999999432, -1.162701749926853712, -75.10000000000003695 ) ) ;
#189676 = ORIENTED_EDGE ( 'NONE', *, *, #232919, .T. ) ;
#189677 = DIRECTION ( 'NONE',  ( 0.000000000000000000, 1.000000000000000000, 1.224646799147353207E-16 ) ) ;
#189678 = EDGE_CURVE ( 'NONE', #77791, #221278, #69475, .T. ) ;
#189679 = CIRCLE ( 'NONE', #168875, 0.1000000000000072220 ) ;
#189680 = VECTOR ( 'NONE', #203053, 1000.000000000000000 ) ;
#189681 = ORIENTED_EDGE ( 'NONE', *, *, #216873, .T. ) ;
#189682 = AXIS2_PLACEMENT_3D ( 'NONE', #18542, #177645, #257094 ) ;
#189683 = AXIS2_PLACEMENT_3D ( 'NONE', #110765, #252837, #212455 ) ;
#189684 = CARTESIAN_POINT ( 'NONE',  ( 21.15000000000005542, 87.51781941433023349, -37.75951082105083145 ) ) ;
#189685 = PRESENTATION_LAYER_ASSIGNMENT (  '', '', ( #98073 ) ) ;
#189687 = ADVANCED_FACE ( 'NONE', ( #107473, #245703 ), #110038, .F. ) ;
#189686 = CYLINDRICAL_SURFACE ( 'NONE', #209335, 0.09999999999999635569 ) ;
#189688 = CARTESIAN_POINT ( 'NONE',  ( -21.08479644141223019, 6.345038657743046429, -66.94144555743589819 ) ) ;
#189690 = ORIENTED_EDGE ( 'NONE', *, *, #173343, .T. ) ;
#189689 = DIRECTION ( 'NONE',  ( -1.000000000000000000, 0.000000000000000000, 0.000000000000000000 ) ) ;
#189691 = CARTESIAN_POINT ( 'NONE',  ( 23.14999999999999503, 11.65000000001116298, -179.6499999999999773 ) ) ;
#189692 = EDGE_CURVE ( 'NONE', #129910, #158778, #252788, .T. ) ;
#189693 = DIRECTION ( 'NONE',  ( 0.000000000000000000, -1.000000000000000000, 0.000000000000000000 ) ) ;
#189694 = PLANE ( 'NONE',  #86069 ) ;
#189696 = DIRECTION ( 'NONE',  ( 0.000000000000000000, 0.000000000000000000, -1.000000000000000000 ) ) ;
#189695 = CARTESIAN_POINT ( 'NONE',  ( -18.54270223418606633, -9.624105502871751483, -140.7409350504075007 ) ) ;
#189697 = DIRECTION ( 'NONE',  ( -0.000000000000000000, -6.982962677686266711E-15, 1.000000000000000000 ) ) ;
#189698 = CARTESIAN_POINT ( 'NONE',  ( 20.94999999999999574, 68.22930980752001062, -227.7331931781284879 ) ) ;
#189699 = CARTESIAN_POINT ( 'NONE',  ( 20.94999999999999929, 36.65892442174935439, -249.5511627012433848 ) ) ;
#189700 = DIRECTION ( 'NONE',  ( -1.000000000000000000, 0.000000000000000000, 0.000000000000000000 ) ) ;
#189701 = CIRCLE ( 'NONE', #73210, 0.1000000000000019901 ) ;
#189702 = ORIENTED_EDGE ( 'NONE', *, *, #61842, .T. ) ;
#189703 = TOROIDAL_SURFACE ( 'NONE', #177270, 0.4000000000000012990, 0.1000000000000000056 ) ;
#189704 = VERTEX_POINT ( 'NONE', #89186 ) ;
#189705 = EDGE_CURVE ( 'NONE', #108916, #238186, #23877, .T. ) ;
#189706 = ORIENTED_EDGE ( 'NONE', *, *, #15033, .F. ) ;
#189707 = EDGE_CURVE ( 'NONE', #164361, #149886, #243759, .T. ) ;
#189708 = AXIS2_PLACEMENT_3D ( 'NONE', #95574, #175167, #155594 ) ;
#189709 = AXIS2_PLACEMENT_3D ( 'NONE', #165540, #11603, #109383 ) ;
#189710 = EDGE_CURVE ( 'NONE', #207406, #79239, #149195, .T. ) ;
#189711 = AXIS2_PLACEMENT_3D ( 'NONE', #56152, #95297, #11934 ) ;
#189712 = DIRECTION ( 'NONE',  ( -0.000000000000000000, -1.000000000000000000, 0.000000000000000000 ) ) ;
#189713 = ORIENTED_EDGE ( 'NONE', *, *, #31519, .T. ) ;
#189714 = CARTESIAN_POINT ( 'NONE',  ( 20.94999999999999929, 11.65000000000000391, -26.65839931010294706 ) ) ;
#189715 = CARTESIAN_POINT ( 'NONE',  ( -16.88005004766534967, 63.08572333212228500, -213.1272708865124059 ) ) ;
#189716 = DIRECTION ( 'NONE',  ( 1.000000000000000000, 0.000000000000000000, 0.000000000000000000 ) ) ;
#189717 = ORIENTED_EDGE ( 'NONE', *, *, #176453, .F. ) ;
#189718 = ORIENTED_EDGE ( 'NONE', *, *, #95512, .T. ) ;
#189720 = DIRECTION ( 'NONE',  ( 0.000000000000000000, 0.1480365673253023762, -0.9889818879709281196 ) ) ;
#189719 = AXIS2_PLACEMENT_3D ( 'NONE', #225243, #187444, #87015 ) ;
#189721 = DIRECTION ( 'NONE',  ( -1.000000000000000000, -0.000000000000000000, -0.000000000000000000 ) ) ;
#189722 = ORIENTED_EDGE ( 'NONE', *, *, #157210, .F. ) ;
#189723 = EDGE_CURVE ( 'NONE', #242166, #143129, #44705, .T. ) ;
#189724 = TOROIDAL_SURFACE ( 'NONE', #48070, 11.70000000000000107, 0.1000000000000000056 ) ;
#189725 = CYLINDRICAL_SURFACE ( 'NONE', #216035, 0.9000000000000014655 ) ;
#189727 = ORIENTED_EDGE ( 'NONE', *, *, #109360, .T. ) ;
#189726 = DIRECTION ( 'NONE',  ( 1.000000000000000000, 0.000000000000000000, 0.000000000000000000 ) ) ;
#189728 = LINE ( 'NONE', #46346, #145852 ) ;
#189729 = TOROIDAL_SURFACE ( 'NONE', #106310, 0.4000000000000005773, 0.1000000000000000056 ) ;
#189730 = FACE_OUTER_BOUND ( 'NONE', #49091, .T. ) ;
#189731 = AXIS2_PLACEMENT_3D ( 'NONE', #27570, #126626, #66662 ) ;
#189733 = ORIENTED_EDGE ( 'NONE', *, *, #42323, .T. ) ;
#189732 = DIRECTION ( 'NONE',  ( 1.000000000000000000, 0.000000000000000000, 0.000000000000000000 ) ) ;
#189734 = CARTESIAN_POINT ( 'NONE',  ( -18.55807992284872299, 10.32898536001801304, -72.58266832227644727 ) ) ;
#189735 = CARTESIAN_POINT ( 'NONE',  ( 20.94999999999999929, 1.115600667400684642E-11, -208.7999999999999545 ) ) ;
#189737 = EDGE_CURVE ( 'NONE', #178041, #76531, #107037, .T. ) ;
#189736 = DIRECTION ( 'NONE',  ( 0.000000000000000000, 0.000000000000000000, 1.000000000000000000 ) ) ;
#189739 = CARTESIAN_POINT ( 'NONE',  ( 21.15000000000000213, 8.786607556611267356, -179.7500000000000000 ) ) ;
#189738 = DIRECTION ( 'NONE',  ( -1.000000000000000000, 0.000000000000000000, 0.000000000000000000 ) ) ;
#189740 = CARTESIAN_POINT ( 'NONE',  ( -18.50000000000000000, 64.35000000001141984, -36.02310748452440237 ) ) ;
#189741 = CARTESIAN_POINT ( 'NONE',  ( -18.58744394320977733, 85.56638515456042171, -163.2002594306475203 ) ) ;
#189742 = CARTESIAN_POINT ( 'NONE',  ( -20.64999999999999858, 4.350000000011156054, -179.7499999999999716 ) ) ;
#189743 = FACE_OUTER_BOUND ( 'NONE', #191437, .T. ) ;
#189744 = ORIENTED_EDGE ( 'NONE', *, *, #18038, .F. ) ;
#189745 = CARTESIAN_POINT ( 'NONE',  ( -17.29838795458690726, 10.37154985796053452, -78.39525871738324270 ) ) ;
#189746 = ORIENTED_EDGE ( 'NONE', *, *, #111279, .T. ) ;
#189747 = DIRECTION ( 'NONE',  ( -6.938893903907209445E-14, -0.9999176327611370985, -0.01283462868040260302 ) ) ;
#189748 = ORIENTED_EDGE ( 'NONE', *, *, #138023, .F. ) ;
#189749 = DIRECTION ( 'NONE',  ( -1.000000000000000000, 0.000000000000000000, 0.000000000000000000 ) ) ;
#189750 = CARTESIAN_POINT ( 'NONE',  ( -20.54999999999999716, 1.115600667400684642E-11, -134.0000000000000284 ) ) ;
#189751 = VECTOR ( 'NONE', #10643, 1000.000000000000000 ) ;
#189752 = VECTOR ( 'NONE', #128081, 1000.000000000000000 ) ;
#189753 = ORIENTED_EDGE ( 'NONE', *, *, #185961, .F. ) ;
#189754 = LINE ( 'NONE', #11124, #198548 ) ;
#189755 = TOROIDAL_SURFACE ( 'NONE', #52368, 0.2000000000000000111, 0.1000000000000000056 ) ;
#189756 = ORIENTED_EDGE ( 'NONE', *, *, #1473, .T. ) ;
#189757 = ORIENTED_EDGE ( 'NONE', *, *, #88278, .F. ) ;
#189758 = ORIENTED_EDGE ( 'NONE', *, *, #109462, .T. ) ;
#189759 = AXIS2_PLACEMENT_3D ( 'NONE', #96599, #19676, #220444 ) ;
#189760 = EDGE_CURVE ( 'NONE', #134179, #180463, #70954, .T. ) ;
#189761 = DIRECTION ( 'NONE',  ( -1.000000000000000000, 0.000000000000000000, 0.000000000000000000 ) ) ;
#189762 = CARTESIAN_POINT ( 'NONE',  ( 20.95595012432476523, 10.60417921308728495, -41.09576933021813971 ) ) ;
#189763 = DIRECTION ( 'NONE',  ( -1.652117596168391700E-15, -1.000000000000000000, 0.000000000000000000 ) ) ;
#189764 = ADVANCED_FACE ( 'NONE', ( #229989 ), #51321, .T. ) ;
#189765 = FACE_OUTER_BOUND ( 'NONE', #196024, .T. ) ;
#189766 = DIRECTION ( 'NONE',  ( 0.000000000000000000, -1.000000000000000000, 0.000000000000000000 ) ) ;
#189768 = CARTESIAN_POINT ( 'NONE',  ( -18.38204789744325396, 11.47950103717623982, -57.75000000000000000 ) ) ;
#189767 = CARTESIAN_POINT ( 'NONE',  ( 21.72449340488910607, 62.76341949586993962, -213.0402075299554951 ) ) ;
#189769 = CARTESIAN_POINT ( 'NONE',  ( -15.75000000000000355, 9.350000000011140955, -83.75000000000004263 ) ) ;
#189771 = ORIENTED_EDGE ( 'NONE', *, *, #149237, .F. ) ;
#189770 = CARTESIAN_POINT ( 'NONE',  ( -20.93975676684922504, 10.31104185824063002, -139.5204516983105805 ) ) ;
#189773 = PLANE ( 'NONE',  #54071 ) ;
#189772 = CARTESIAN_POINT ( 'NONE',  ( 20.77766267348356166, 10.44904239063021123, -74.59270891587755159 ) ) ;
#189774 = EDGE_CURVE ( 'NONE', #140474, #24921, #123810, .T. ) ;
#189775 = DIRECTION ( 'NONE',  ( 0.000000000000000000, 0.000000000000000000, 1.000000000000000000 ) ) ;
#189777 = EDGE_CURVE ( 'NONE', #217695, #232002, #48781, .T. ) ;
#189776 = AXIS2_PLACEMENT_3D ( 'NONE', #214733, #255091, #130387 ) ;
#189778 = ORIENTED_EDGE ( 'NONE', *, *, #21380, .T. ) ;
#189779 = CARTESIAN_POINT ( 'NONE',  ( -16.94107738177414291, 65.98576071487562444, -149.0731074845244279 ) ) ;
#189780 = AXIS2_PLACEMENT_3D ( 'NONE', #81646, #183364, #123385 ) ;
#189781 = DIRECTION ( 'NONE',  ( 1.000000000000000000, 2.885090398161910739E-16, 6.283419270304611573E-17 ) ) ;
#189782 = CARTESIAN_POINT ( 'NONE',  ( -20.94999999999999929, -11.48912529306489994, -130.9000000000000341 ) ) ;
#189783 = ORIENTED_EDGE ( 'NONE', *, *, #42243, .F. ) ;
#189784 = AXIS2_PLACEMENT_3D ( 'NONE', #26584, #108668, #189498 ) ;
#189785 = EDGE_CURVE ( 'NONE', #11679, #116798, #15501, .T. ) ;
#189786 = DIRECTION ( 'NONE',  ( 0.000000000000000000, 0.000000000000000000, -1.000000000000000000 ) ) ;
#189787 = EDGE_CURVE ( 'NONE', #142689, #28569, #90471, .T. ) ;
#189788 = DIRECTION ( 'NONE',  ( -1.000000000000000000, -1.836970198721029934E-16, 0.000000000000000000 ) ) ;
#189789 = DIRECTION ( 'NONE',  ( -1.000000000000000000, 0.000000000000000000, 0.000000000000000000 ) ) ;
#189791 = EDGE_CURVE ( 'NONE', #63493, #237457, #155630, .T. ) ;
#189790 = EDGE_CURVE ( 'NONE', #224679, #60113, #240339, .T. ) ;
#189792 = ORIENTED_EDGE ( 'NONE', *, *, #255243, .F. ) ;
#189793 = ORIENTED_EDGE ( 'NONE', *, *, #41578, .T. ) ;
#189794 = CARTESIAN_POINT ( 'NONE',  ( -20.64999999999999858, 71.65000000001207070, -124.2731074845243313 ) ) ;
#189795 = CARTESIAN_POINT ( 'NONE',  ( -17.71734398241073905, 10.84235722847571814, -177.7748617469943611 ) ) ;
#189796 = AXIS2_PLACEMENT_3D ( 'NONE', #125208, #204718, #67787 ) ;
#189797 = CARTESIAN_POINT ( 'NONE',  ( -18.59999999999999787, 74.65925378207852248, -146.7959699899454904 ) ) ;
#189798 = CARTESIAN_POINT ( 'NONE',  ( -20.86777300164944648, 10.33200063080771969, -206.5931674956642610 ) ) ;
#189799 = ORIENTED_EDGE ( 'NONE', *, *, #153401, .T. ) ;
#189800 = CARTESIAN_POINT ( 'NONE',  ( 20.94999999999999574, 74.16465844978715438, -57.96795619196134908 ) ) ;
#189801 = ADVANCED_FACE ( 'NONE', ( #215554 ), #100361, .F. ) ;
#189802 = CARTESIAN_POINT ( 'NONE',  ( -21.45000000000000284, 7.708578643773852157, -54.65000000000000568 ) ) ;
#189803 = DIRECTION ( 'NONE',  ( 0.000000000000000000, 0.000000000000000000, -1.000000000000000000 ) ) ;
#189804 = DIRECTION ( 'NONE',  ( 0.000000000000000000, 0.000000000000000000, -1.000000000000000000 ) ) ;
#189805 = ADVANCED_FACE ( 'NONE', ( #211732 ), #256834, .F. ) ;
#189806 = EDGE_CURVE ( 'NONE', #152443, #232528, #38226, .T. ) ;
#189807 = TOROIDAL_SURFACE ( 'NONE', #77352, 12.77500000000000036, 0.1000000000000000056 ) ;
#189808 = ORIENTED_EDGE ( 'NONE', *, *, #144447, .F. ) ;
#189809 = AXIS2_PLACEMENT_3D ( 'NONE', #64174, #121608, #241522 ) ;
#189810 = AXIS2_PLACEMENT_3D ( 'NONE', #72756, #55680, #115702 ) ;
#189811 = CARTESIAN_POINT ( 'NONE',  ( 20.89878130938411616, 10.32747123226657493, -39.07740328502492844 ) ) ;
#189812 = ADVANCED_FACE ( 'NONE', ( #136002 ), #236407, .F. ) ;
#189814 = ORIENTED_EDGE ( 'NONE', *, *, #13488, .T. ) ;
#189813 = CARTESIAN_POINT ( 'NONE',  ( -16.93589915522259304, 65.99137474131595127, -82.08254738256407279 ) ) ;
#189815 = FACE_OUTER_BOUND ( 'NONE', #14424, .T. ) ;
#189816 = CARTESIAN_POINT ( 'NONE',  ( 20.85000000000000142, 77.83585931145570669, -124.9186683157258102 ) ) ;
#189817 = CARTESIAN_POINT ( 'NONE',  ( 20.94999999999999929, 6.450000000011156587, -43.51702717044002355 ) ) ;
#189818 = CARTESIAN_POINT ( 'NONE',  ( 19.92426406871192412, 62.39550153362034024, -208.7959266050682743 ) ) ;
#189819 = ORIENTED_EDGE ( 'NONE', *, *, #191076, .F. ) ;
#189820 = ADVANCED_FACE ( 'NONE', ( #254653, #18647, #77321 ), #36965, .F. ) ;
#189821 = DIRECTION ( 'NONE',  ( 0.000000000000000000, 1.000000000000000000, 0.000000000000000000 ) ) ;
#189822 = CARTESIAN_POINT ( 'NONE',  ( -23.25000000000000000, 87.75000000001193712, -103.0231074845242318 ) ) ;
#189823 = ORIENTED_EDGE ( 'NONE', *, *, #38183, .T. ) ;
#189824 = DIRECTION ( 'NONE',  ( 0.000000000000000000, 0.000000000000000000, -1.000000000000000000 ) ) ;
#189825 = DIRECTION ( 'NONE',  ( 0.000000000000000000, 0.000000000000000000, -1.000000000000000000 ) ) ;
#189826 = DIRECTION ( 'NONE',  ( 0.000000000000000000, -0.000000000000000000, 1.000000000000000000 ) ) ;
#189827 = DIRECTION ( 'NONE',  ( 1.000000000000000000, 0.000000000000000000, 0.000000000000000000 ) ) ;
#189828 = AXIS2_PLACEMENT_3D ( 'NONE', #129453, #208984, #30369 ) ;
#189829 = CARTESIAN_POINT ( 'NONE',  ( 21.05000000000000071, 6.413978881499349249, -167.5857991162739609 ) ) ;
#189830 = CARTESIAN_POINT ( 'NONE',  ( 13.22461703343585349, 9.436662931810245070, -185.8230367322949235 ) ) ;
#189831 = VERTEX_POINT ( 'NONE', #212993 ) ;
#189832 = ORIENTED_EDGE ( 'NONE', *, *, #139723, .T. ) ;
#189833 = CARTESIAN_POINT ( 'NONE',  ( -20.54999999999999716, 87.75000000001202238, -119.7731074845242176 ) ) ;
#189835 = FACE_OUTER_BOUND ( 'NONE', #81916, .T. ) ;
#189834 = VECTOR ( 'NONE', #33393, 1000.000000000000000 ) ;
#189836 = CYLINDRICAL_SURFACE ( 'NONE', #149913, 0.09999999999999939493 ) ;
#189837 = CARTESIAN_POINT ( 'NONE',  ( -21.05000000000000071, 38.04609728753135300, -236.0545303518866547 ) ) ;
#189838 = DIRECTION ( 'NONE',  ( -1.000000000000000000, 0.000000000000000000, 0.000000000000000000 ) ) ;
#189839 = DIRECTION ( 'NONE',  ( -0.000000000000000000, -0.7106264324241465813, 0.7035695228903323661 ) ) ;
#189840 = DIRECTION ( 'NONE',  ( 1.000000000000000000, 0.000000000000000000, 0.000000000000000000 ) ) ;
#189841 = CARTESIAN_POINT ( 'NONE',  ( -18.40000000000000213, 11.48667500176882328, -109.7500000000000426 ) ) ;
#189842 = DIRECTION ( 'NONE',  ( -1.000000000000000000, 0.000000000000000000, -0.000000000000000000 ) ) ;
#189843 = AXIS2_PLACEMENT_3D ( 'NONE', #156991, #20043, #100797 ) ;
#189844 = VERTEX_POINT ( 'NONE', #17372 ) ;
#189845 = CARTESIAN_POINT ( 'NONE',  ( 23.24999999999999289, 2.319530388122574394, -217.8268657444419887 ) ) ;
#189846 = EDGE_LOOP ( 'NONE', ( #43041, #179134, #173353, #151392 ) ) ;
#189847 = CARTESIAN_POINT ( 'NONE',  ( 20.94999999999999929, 77.13501884592155022, -28.30613060109199353 ) ) ;
#189848 = CARTESIAN_POINT ( 'NONE',  ( 21.04999999999963478, 10.62950747926064032, -7.627979399996550391 ) ) ;
#189849 = CARTESIAN_POINT ( 'NONE',  ( 21.06600267594171783, 8.775166069211060460, -79.20426278237478357 ) ) ;
#189850 = DIRECTION ( 'NONE',  ( 0.000000000000000000, -1.000000000000000000, 0.000000000000000000 ) ) ;
#189851 = CARTESIAN_POINT ( 'NONE',  ( 21.10710606213542206, 22.06360055159736788, -231.7760222370280303 ) ) ;
#189852 = CARTESIAN_POINT ( 'NONE',  ( 18.43630871534871574, 85.67980087481460316, -62.86247541654014981 ) ) ;
#189853 = CARTESIAN_POINT ( 'NONE',  ( -20.94999999999999929, 74.16465844978745281, -91.36795619196134055 ) ) ;
#189854 = ORIENTED_EDGE ( 'NONE', *, *, #174587, .F. ) ;
#189855 = CARTESIAN_POINT ( 'NONE',  ( -21.64999999999999858, 68.75000000001158185, -57.27310748452437394 ) ) ;
#189856 = EDGE_CURVE ( 'NONE', #66860, #34745, #11380, .T. ) ;
#189857 = DIRECTION ( 'NONE',  ( 0.000000000000000000, 0.000000000000000000, -1.000000000000000000 ) ) ;
#189858 = CARTESIAN_POINT ( 'NONE',  ( -17.04761207306819770, 65.97354912661380411, -56.87310748452438247 ) ) ;
#189859 = DIRECTION ( 'NONE',  ( 1.000000000000000000, 0.000000000000000000, 0.000000000000000000 ) ) ;
#189860 = VECTOR ( 'NONE', #207336, 1000.000000000000000 ) ;
#189861 = EDGE_CURVE ( 'NONE', #1409, #135375, #83603, .T. ) ;
#189862 = TOROIDAL_SURFACE ( 'NONE', #169054, 0.2000000000000000111, 0.1000000000000000056 ) ;
#189863 = CARTESIAN_POINT ( 'NONE',  ( 18.59999999999999432, 85.48068669529082797, -96.08199231576637089 ) ) ;
#189864 = VECTOR ( 'NONE', #252651, 1000.000000000000000 ) ;
#189865 = VECTOR ( 'NONE', #111749, 1000.000000000000000 ) ;
#189866 = VERTEX_POINT ( 'NONE', #177751 ) ;
#189867 = CARTESIAN_POINT ( 'NONE',  ( -18.59999999999999787, -1.835859311432481045, -179.0044391687985410 ) ) ;
#189869 = EDGE_CURVE ( 'NONE', #90904, #120700, #63149, .T. ) ;
#189868 = DIRECTION ( 'NONE',  ( 0.000000000000000000, -5.214354714482140540E-14, 1.000000000000000000 ) ) ;
#189871 = EDGE_CURVE ( 'NONE', #18030, #116233, #110286, .T. ) ;
#189870 = VERTEX_POINT ( 'NONE', #74813 ) ;
#189872 = EDGE_LOOP ( 'NONE', ( #133236, #153150, #151741, #142263 ) ) ;
#189873 = DIRECTION ( 'NONE',  ( 0.000000000000000000, 0.9999631594459056361, -0.008583690987128059571 ) ) ;
#189874 = CARTESIAN_POINT ( 'NONE',  ( -18.59999999999999787, 52.91185528119410719, -244.1460391050142960 ) ) ;
#189875 = ORIENTED_EDGE ( 'NONE', *, *, #223610, .T. ) ;
#189876 = CARTESIAN_POINT ( 'NONE',  ( 21.05000000000000071, 76.00000000001126921, -203.5231074845248997 ) ) ;
#189877 = PLANE ( 'NONE',  #210000 ) ;
#189878 = VERTEX_POINT ( 'NONE', #83714 ) ;
#189879 = CIRCLE ( 'NONE', #156609, 0.2000000000000057288 ) ;
#189880 = ADVANCED_FACE ( 'NONE', ( #42089 ), #111149, .F. ) ;
#189882 = EDGE_CURVE ( 'NONE', #140162, #248221, #179044, .T. ) ;
#189881 = AXIS2_PLACEMENT_3D ( 'NONE', #20608, #43994, #4837 ) ;
#189883 = CARTESIAN_POINT ( 'NONE',  ( -21.05000000000000071, 14.05000000001115623, -39.01369507076099552 ) ) ;
#189884 = ORIENTED_EDGE ( 'NONE', *, *, #183646, .T. ) ;
#189885 = CIRCLE ( 'NONE', #77434, 0.09999999999999939493 ) ;
#189886 = CARTESIAN_POINT ( 'NONE',  ( 20.94999999999999574, 87.65000000001235492, -167.1231074845242688 ) ) ;
#189887 = DIRECTION ( 'NONE',  ( 0.000000000000000000, 0.000000000000000000, -1.000000000000000000 ) ) ;
#189889 = ORIENTED_EDGE ( 'NONE', *, *, #171366, .T. ) ;
#189888 = DIRECTION ( 'NONE',  ( -0.000000000000000000, 0.4856429311786307212, 0.8741572761215384846 ) ) ;
#189890 = PLANE ( 'NONE',  #240663 ) ;
#189891 = DIRECTION ( 'NONE',  ( -1.000000000000000000, 0.000000000000000000, 0.000000000000000000 ) ) ;
#189892 = CARTESIAN_POINT ( 'NONE',  ( 18.59999999999999787, 1.115600667400684642E-11, -167.4999999999999716 ) ) ;
#189893 = CIRCLE ( 'NONE', #256468, 0.4999999999999944489 ) ;
#189894 = CARTESIAN_POINT ( 'NONE',  ( -21.00000000000000000, 0.000000000000000000, 0.000000000000000000 ) ) ;
#189895 = DIRECTION ( 'NONE',  ( -1.000000000000000000, -0.000000000000000000, -0.000000000000000000 ) ) ;
#189896 = CARTESIAN_POINT ( 'NONE',  ( 18.49999999999999289, 11.65000000001115943, -55.25000000000004974 ) ) ;
#189897 = CARTESIAN_POINT ( 'NONE',  ( -20.54999999999999716, 76.00000000001213607, -136.5231074845242745 ) ) ;
#189900 = ORIENTED_EDGE ( 'NONE', *, *, #147262, .T. ) ;
#189899 = ADVANCED_FACE ( 'NONE', ( #43358 ), #99443, .T. ) ;
#189898 = CARTESIAN_POINT ( 'NONE',  ( 20.94999999999999929, 65.27628289530433392, -90.87310748452438247 ) ) ;
#189901 = ORIENTED_EDGE ( 'NONE', *, *, #233427, .T. ) ;
#189903 = CARTESIAN_POINT ( 'NONE',  ( -18.40000000000000213, 58.56629890316250453, -223.9209570932885356 ) ) ;
#189902 = DIRECTION ( 'NONE',  ( -1.000000000000000000, -0.000000000000000000, -0.000000000000000000 ) ) ;
#189905 = ORIENTED_EDGE ( 'NONE', *, *, #57199, .F. ) ;
#189904 = CARTESIAN_POINT ( 'NONE',  ( -23.15000000000000213, 8.751106741858205140, -220.7398867978735950 ) ) ;
#189906 = ORIENTED_EDGE ( 'NONE', *, *, #4860, .T. ) ;
#189907 = ADVANCED_FACE ( 'NONE', ( #218110 ), #119042, .T. ) ;
#189908 = CARTESIAN_POINT ( 'NONE',  ( -16.77779411440718249, 66.05389855290493983, -182.6861649015289402 ) ) ;
#189909 = DIRECTION ( 'NONE',  ( -0.000000000000000000, -6.982962677686266711E-15, 1.000000000000000000 ) ) ;
#189910 = AXIS2_PLACEMENT_3D ( 'NONE', #245817, #64593, #67176 ) ;
#189911 = CIRCLE ( 'NONE', #123270, 0.09999999999998898659 ) ;
#189912 = CARTESIAN_POINT ( 'NONE',  ( 20.94999999999999929, 69.55000000001187743, -93.00608031408432907 ) ) ;
#189913 = DIRECTION ( 'NONE',  ( 0.000000000000000000, -1.000000000000000000, -1.897661533703519897E-16 ) ) ;
#189914 = DIRECTION ( 'NONE',  ( 0.000000000000000000, -0.9908441862701782288, 0.1350103645450542456 ) ) ;
#189915 = VECTOR ( 'NONE', #15702, 1000.000000000000000 ) ;
#189917 = EDGE_CURVE ( 'NONE', #191282, #165976, #231981, .T. ) ;
#189916 = DIRECTION ( 'NONE',  ( 1.000000000000000000, 0.000000000000000000, 0.000000000000000000 ) ) ;
#189918 = EDGE_CURVE ( 'NONE', #85875, #63552, #7082, .T. ) ;
#189919 = CARTESIAN_POINT ( 'NONE',  ( 20.94999999999999574, 69.60000000001207354, -126.5926828544627654 ) ) ;
#189920 = ORIENTED_EDGE ( 'NONE', *, *, #150279, .F. ) ;
#189921 = ORIENTED_EDGE ( 'NONE', *, *, #4317, .T. ) ;
#189922 = CARTESIAN_POINT ( 'NONE',  ( -21.05000000000000071, 76.00000000001222134, -148.3231074845243427 ) ) ;
#189923 = CIRCLE ( 'NONE', #65583, 0.9000000000000014655 ) ;
#189924 = EDGE_CURVE ( 'NONE', #28183, #70441, #207010, .T. ) ;
#189925 = MANIFOLD_SOLID_BREP ( 'Stock-MAS-200-1', #49362 ) ;
#189926 = ORIENTED_EDGE ( 'NONE', *, *, #198586, .T. ) ;
#189927 = DIRECTION ( 'NONE',  ( -3.469446951953515108E-14, 0.000000000000000000, -1.000000000000000000 ) ) ;
#189928 = ORIENTED_EDGE ( 'NONE', *, *, #62555, .F. ) ;
#189929 = DIRECTION ( 'NONE',  ( -1.000000000000000000, -3.469446951953635646E-14, 0.000000000000000000 ) ) ;
#189930 = DIRECTION ( 'NONE',  ( 0.000000000000000000, 0.000000000000000000, -1.000000000000000000 ) ) ;
#189931 = CARTESIAN_POINT ( 'NONE',  ( 18.49999999999999289, 65.58283456529508726, -44.67310748510405460 ) ) ;
#189932 = VERTEX_POINT ( 'NONE', #201131 ) ;
#189933 = ADVANCED_FACE ( 'NONE', ( #181592 ), #37198, .T. ) ;
#189935 = CARTESIAN_POINT ( 'NONE',  ( -23.15000000000000213, -11.64999999998884483, -64.00000000000000000 ) ) ;
#189934 =( BOUNDED_CURVE ( )  B_SPLINE_CURVE ( 3, ( #82561, #183000, #163429, #85128 ),
 .UNSPECIFIED., .F., .F. ) 
 B_SPLINE_CURVE_WITH_KNOTS ( ( 4, 4 ),
 ( 1.570796326794908992, 2.617993877991481533 ),
 .UNSPECIFIED. ) 
 CURVE ( )  GEOMETRIC_REPRESENTATION_ITEM ( )  RATIONAL_B_SPLINE_CURVE ( ( 1.000000000000000000, 0.9106836025229633202, 0.9106836025229633202, 1.000000000000000000 ) ) 
 REPRESENTATION_ITEM ( '' )  );
#189936 = ORIENTED_EDGE ( 'NONE', *, *, #162436, .T. ) ;
#189937 = CIRCLE ( 'NONE', #231642, 0.2000000000000005107 ) ;
#189938 = DIRECTION ( 'NONE',  ( 1.186688945009010324E-16, -0.4721928772777346239, -0.8814952561688430555 ) ) ;
#189939 = CIRCLE ( 'NONE', #244096, 0.1000000000000028644 ) ;
#189940 = CARTESIAN_POINT ( 'NONE',  ( 21.05000000000000071, 8.926614585098253229, -108.9716830192231640 ) ) ;
#189941 = EDGE_CURVE ( 'NONE', #87571, #59101, #144436, .T. ) ;
#189942 = AXIS2_PLACEMENT_3D ( 'NONE', #179801, #1120, #80660 ) ;
#189943 = VECTOR ( 'NONE', #59367, 1000.000000000000000 ) ;
#189944 = ORIENTED_EDGE ( 'NONE', *, *, #144570, .T. ) ;
#189945 = CARTESIAN_POINT ( 'NONE',  ( -20.64999999999999858, 4.349999999999999645, -12.35000000000000142 ) ) ;
#189946 = ORIENTED_EDGE ( 'NONE', *, *, #207607, .T. ) ;
#189949 = ORIENTED_EDGE ( 'NONE', *, *, #23832, .T. ) ;
#189948 = CARTESIAN_POINT ( 'NONE',  ( 20.94999999999999929, 76.00000000001190870, -103.0231074845243029 ) ) ;
#189947 = FACE_OUTER_BOUND ( 'NONE', #245840, .T. ) ;
#189950 = CARTESIAN_POINT ( 'NONE',  ( -23.25000000000000000, 64.25000000001179501, -81.67310748452440805 ) ) ;
#189951 = ORIENTED_EDGE ( 'NONE', *, *, #67234, .T. ) ;
#189952 = AXIS2_PLACEMENT_3D ( 'NONE', #234545, #135437, #76752 ) ;
#189953 = CARTESIAN_POINT ( 'NONE',  ( -23.25000000000000000, 76.10085836911117951, -181.7726746080137445 ) ) ;
#189954 = EDGE_LOOP ( 'NONE', ( #207613, #17253, #237476 ) ) ;
#189955 = CARTESIAN_POINT ( 'NONE',  ( -18.59999999999999787, 18.60970618848720903, -231.2322896185303875 ) ) ;
#189956 = ORIENTED_EDGE ( 'NONE', *, *, #175582, .T. ) ;
#189957 = DIRECTION ( 'NONE',  ( 0.000000000000000000, 0.9651348961777159730, -0.2617529984165021806 ) ) ;
#189958 = CARTESIAN_POINT ( 'NONE',  ( -16.89268316805465986, 9.951721813253337601, -188.3557524785454973 ) ) ;
#189959 = AXIS2_PLACEMENT_3D ( 'NONE', #211883, #110184, #189736 ) ;
#189960 = DIRECTION ( 'NONE',  ( 0.000000000000000000, -7.086529944415886769E-15, 1.000000000000000000 ) ) ;
#189961 = DIRECTION ( 'NONE',  ( 0.000000000000000000, 0.000000000000000000, -1.000000000000000000 ) ) ;
#189962 = CIRCLE ( 'NONE', #10912, 0.1000000000000000472 ) ;
#189963 = VERTEX_POINT ( 'NONE', #204966 ) ;
#189964 = CARTESIAN_POINT ( 'NONE',  ( 20.94999999999999929, 65.27628289530501604, -182.2731074845244450 ) ) ;
#189965 = DIRECTION ( 'NONE',  ( 0.000000000000000000, 6.982962677686266711E-15, -1.000000000000000000 ) ) ;
#189966 = CARTESIAN_POINT ( 'NONE',  ( 18.53317502108576775, 10.32263460347359896, -139.5605957968672328 ) ) ;
#189967 = VERTEX_POINT ( 'NONE', #165882 ) ;
#189968 = FACE_OUTER_BOUND ( 'NONE', #185774, .T. ) ;
#189969 = ORIENTED_EDGE ( 'NONE', *, *, #40060, .F. ) ;
#189970 = DIRECTION ( 'NONE',  ( 0.000000000000000000, -0.07847809223012357227, -0.9969158384938622275 ) ) ;
#189971 = ORIENTED_EDGE ( 'NONE', *, *, #170007, .F. ) ;
#189972 = DIRECTION ( 'NONE',  ( -0.000000000000000000, -0.1335171055202901413, -0.9910465087640860649 ) ) ;
#189973 = LINE ( 'NONE', #88268, #251844 ) ;
#189974 = CIRCLE ( 'NONE', #135791, 0.5000000000000004441 ) ;
#189976 = VERTEX_POINT ( 'NONE', #6785 ) ;
#189975 = CARTESIAN_POINT ( 'NONE',  ( 18.59999999999999076, 10.49142135624846439, -58.25000000000000000 ) ) ;
#189977 = CARTESIAN_POINT ( 'NONE',  ( -23.25000000000000000, 65.66751761918722252, -164.4282609406112670 ) ) ;
#189978 = ORIENTED_EDGE ( 'NONE', *, *, #26193, .F. ) ;
#189979 = CARTESIAN_POINT ( 'NONE',  ( -20.94999999999999929, 36.14042471737580087, -236.0721279892244411 ) ) ;
#189980 = DIRECTION ( 'NONE',  ( 1.000000000000000000, 0.000000000000000000, 0.000000000000000000 ) ) ;
#189981 = ORIENTED_EDGE ( 'NONE', *, *, #206134, .F. ) ;
#189982 = CARTESIAN_POINT ( 'NONE',  ( -18.50000000000000000, 18.11150788191476124, -237.7585516551410478 ) ) ;
#189983 = CARTESIAN_POINT ( 'NONE',  ( -20.64999999999999858, 7.150000000011155876, -79.25000000000004263 ) ) ;
#189984 = EDGE_LOOP ( 'NONE', ( #157928, #144590, #257617, #32844, #112360 ) ) ;
#189985 = CARTESIAN_POINT ( 'NONE',  ( -16.93440969289731157, 9.995185175825108459, -146.5912341850108191 ) ) ;
#189986 = AXIS2_PLACEMENT_3D ( 'NONE', #22710, #40992, #239163 ) ;
#189987 = AXIS2_PLACEMENT_3D ( 'NONE', #157388, #176944, #255111 ) ;
#189988 = VECTOR ( 'NONE', #147243, 1000.000000000000000 ) ;
#189989 = CIRCLE ( 'NONE', #239891, 0.1000000000000002554 ) ;
#189990 = ORIENTED_EDGE ( 'NONE', *, *, #65568, .T. ) ;
#189991 = CARTESIAN_POINT ( 'NONE',  ( 14.22916352759893321, 9.457410930301314522, -118.9999159087462886 ) ) ;
#189992 = CARTESIAN_POINT ( 'NONE',  ( -22.57320508075687115, 64.25000000001237765, -170.0231074845244166 ) ) ;
#189993 = ADVANCED_FACE ( 'NONE', ( #86294 ), #130574, .F. ) ;
#189996 = ORIENTED_EDGE ( 'NONE', *, *, #118891, .F. ) ;
#189995 = VERTEX_POINT ( 'NONE', #90153 ) ;
#189994 = SPHERICAL_SURFACE ( 'NONE', #193016, 0.1000000000000000056 ) ;
#189997 = EDGE_CURVE ( 'NONE', #195194, #117855, #136244, .T. ) ;
#189998 = DIRECTION ( 'NONE',  ( 0.000000000000000000, 0.8814952561688476074, -0.4721928772777262417 ) ) ;
#189999 = EDGE_CURVE ( 'NONE', #33432, #360, #107162, .T. ) ;
#190000 = DIRECTION ( 'NONE',  ( 0.000000000000000000, 0.2617529984165031243, 0.9651348961777157509 ) ) ;
#190001 = DIRECTION ( 'NONE',  ( 0.000000000000000000, -0.9525900758537790836, 0.3042567129660269099 ) ) ;
#190002 = AXIS2_PLACEMENT_3D ( 'NONE', #112192, #191739, #133028 ) ;
#190004 = CARTESIAN_POINT ( 'NONE',  ( 20.09999999999999787, 51.70063031245850738, -232.1289905089708441 ) ) ;
#190003 = CYLINDRICAL_SURFACE ( 'NONE', #202338, 0.8750000000000007772 ) ;
#190005 = CYLINDRICAL_SURFACE ( 'NONE', #61876, 0.09999999999999976963 ) ;
#190006 = FACE_OUTER_BOUND ( 'NONE', #106410, .T. ) ;
#190007 = AXIS2_PLACEMENT_3D ( 'NONE', #22369, #100561, #144848 ) ;
#190008 = DIRECTION ( 'NONE',  ( 1.836970198721030427E-16, 0.4088369013363281623, -0.9126074666063771490 ) ) ;
#190009 = CARTESIAN_POINT ( 'NONE',  ( -21.93642651522410247, 68.67283376068633061, -136.5231074845243313 ) ) ;
#190010 = ORIENTED_EDGE ( 'NONE', *, *, #115142, .T. ) ;
#190011 = ORIENTED_EDGE ( 'NONE', *, *, #248310, .T. ) ;
#190012 = CARTESIAN_POINT ( 'NONE',  ( -23.25000000000000000, 14.73746888278882494, -235.8584165281851028 ) ) ;
#190013 = AXIS2_PLACEMENT_3D ( 'NONE', #5757, #85291, #63176 ) ;
#190015 = ORIENTED_EDGE ( 'NONE', *, *, #62339, .T. ) ;
#190014 = DIRECTION ( 'NONE',  ( 0.000000000000000000, 0.000000000000000000, -1.000000000000000000 ) ) ;
#190016 = EDGE_LOOP ( 'NONE', ( #213355, #83977, #59310, #22728 ) ) ;
#190017 = EDGE_CURVE ( 'NONE', #257664, #99817, #98630, .T. ) ;
#190018 = DIRECTION ( 'NONE',  ( 0.000000000000000000, 0.000000000000000000, 1.000000000000000000 ) ) ;
#190019 = ORIENTED_EDGE ( 'NONE', *, *, #194804, .T. ) ;
#190020 = CARTESIAN_POINT ( 'NONE',  ( 21.06089410995835820, 43.41001159599868231, -234.7743943900634065 ) ) ;
#190021 = ORIENTED_EDGE ( 'NONE', *, *, #145100, .T. ) ;
#190022 = FACE_OUTER_BOUND ( 'NONE', #30396, .T. ) ;
#190026 = ORIENTED_EDGE ( 'NONE', *, *, #115859, .F. ) ;
#190025 = ORIENTED_EDGE ( 'NONE', *, *, #3416, .T. ) ;
#190024 = AXIS2_PLACEMENT_3D ( 'NONE', #157990, #243893, #245192 ) ;
#190023 = B_SPLINE_CURVE_WITH_KNOTS ( 'NONE', 3,
 ( #164372, #66553, #24880, #43142, #125241, #182659, #122692, #103079, #4000, #104363 ),
 .UNSPECIFIED., .F., .F.,
 ( 4, 3, 3, 4 ),
 ( 1.886897567106814762E-15, 3.877043166999436273E-05, 7.336897548476632052E-05, 7.659383120240038272E-05 ),
 .UNSPECIFIED. ) ;
#190027 = VERTEX_POINT ( 'NONE', #189288 ) ;
#190028 = ORIENTED_EDGE ( 'NONE', *, *, #117554, .T. ) ;
#190029 = ORIENTED_EDGE ( 'NONE', *, *, #164779, .T. ) ;
#190030 = CARTESIAN_POINT ( 'NONE',  ( 21.14999999999999503, -3.275978944802464099, -228.2735455795363748 ) ) ;
#190031 = FACE_OUTER_BOUND ( 'NONE', #15745, .T. ) ;
#190032 = CARTESIAN_POINT ( 'NONE',  ( -12.68215100488890634, 9.396630376328873879, -185.4070573928183023 ) ) ;
#190034 = ORIENTED_EDGE ( 'NONE', *, *, #31823, .T. ) ;
#190033 = CARTESIAN_POINT ( 'NONE',  ( -23.25000000000000000, -9.682403433465239573, -207.6568433774127413 ) ) ;
#190035 = EDGE_CURVE ( 'NONE', #40759, #238428, #246671, .T. ) ;
#190036 = EDGE_CURVE ( 'NONE', #9569, #122995, #244410, .T. ) ;
#190037 = CARTESIAN_POINT ( 'NONE',  ( -18.40000000000000213, 16.36019599348126619, -222.2043791590202488 ) ) ;
#190038 = CARTESIAN_POINT ( 'NONE',  ( 21.05000000000000426, 11.90764318652833431, -206.0382540159556015 ) ) ;
#190040 = VERTEX_POINT ( 'NONE', #70649 ) ;
#190039 = DIRECTION ( 'NONE',  ( 0.000000000000000000, -0.9126074666063772600, -0.4088369013363276627 ) ) ;
#190041 = DIRECTION ( 'NONE',  ( 0.000000000000000000, 0.000000000000000000, -1.000000000000000000 ) ) ;
#190042 = ORIENTED_EDGE ( 'NONE', *, *, #207365, .F. ) ;
#190043 = DIRECTION ( 'NONE',  ( 0.000000000000000000, 0.000000000000000000, -1.000000000000000000 ) ) ;
#190044 = ORIENTED_EDGE ( 'NONE', *, *, #68328, .F. ) ;
#190045 = PLANE ( 'NONE',  #95489 ) ;
#190046 = ADVANCED_FACE ( 'NONE', ( #249259 ), #129306, .F. ) ;
#190047 = AXIS2_PLACEMENT_3D ( 'NONE', #127940, #9268, #168398 ) ;
#190048 = VERTEX_POINT ( 'NONE', #88868 ) ;
#190050 = CARTESIAN_POINT ( 'NONE',  ( 18.59999999999999432, 68.22930980752001062, -227.7331931781284879 ) ) ;
#190049 = CARTESIAN_POINT ( 'NONE',  ( -22.39999999999999858, 76.00000000001267608, -203.6231074845243540 ) ) ;
#190051 = DIRECTION ( 'NONE',  ( 1.000000000000000000, 0.000000000000000000, 0.000000000000000000 ) ) ;
#190052 = AXIS2_PLACEMENT_3D ( 'NONE', #137528, #241778, #21474 ) ;
#190053 = VECTOR ( 'NONE', #235234, 1000.000000000000000 ) ;
#190054 = CARTESIAN_POINT ( 'NONE',  ( 20.94999999999999929, 14.05000000000000071, -27.98630492923908619 ) ) ;
#190055 = DIRECTION ( 'NONE',  ( 0.000000000000000000, -0.000000000000000000, -1.000000000000000000 ) ) ;
#190056 = ORIENTED_EDGE ( 'NONE', *, *, #222553, .T. ) ;
#190057 = VERTEX_POINT ( 'NONE', #208843 ) ;
#190058 = PRESENTATION_LAYER_ASSIGNMENT (  '', '', ( #10981 ) ) ;
#190059 = DIRECTION ( 'NONE',  ( -0.000000000000000000, -0.000000000000000000, 1.000000000000000000 ) ) ;
#190060 = DIRECTION ( 'NONE',  ( 0.7071067811865474617, 0.3338907855510732658, 0.6233112732207619633 ) ) ;
#190061 = EDGE_LOOP ( 'NONE', ( #162697, #139828, #18353, #98988 ) ) ;
#190062 = DIRECTION ( 'NONE',  ( 0.000000000000000000, -0.9770955615653316162, -0.2128009952263604232 ) ) ;
#190063 = ORIENTED_EDGE ( 'NONE', *, *, #49348, .F. ) ;
#190064 = DIRECTION ( 'NONE',  ( 0.000000000000000000, 0.000000000000000000, -1.000000000000000000 ) ) ;
#190065 = CARTESIAN_POINT ( 'NONE',  ( -23.39999999999994529, 84.00000000001119815, -34.86056257560453986 ) ) ;
#190066 = CARTESIAN_POINT ( 'NONE',  ( 20.99999999999999645, 66.25000000001210765, -127.2731074845243597 ) ) ;
#190067 = EDGE_CURVE ( 'NONE', #84389, #136081, #128087, .T. ) ;
#190068 = ORIENTED_EDGE ( 'NONE', *, *, #158843, .F. ) ;
#190069 = CARTESIAN_POINT ( 'NONE',  ( 18.59999999999999076, 11.65000000001115943, -91.85000000000003695 ) ) ;
#190070 = VECTOR ( 'NONE', #219614, 1000.000000000000000 ) ;
#190071 = ORIENTED_EDGE ( 'NONE', *, *, #61494, .F. ) ;
#190072 = VERTEX_POINT ( 'NONE', #169754 ) ;
#190073 = CIRCLE ( 'NONE', #119335, 4.000000000000003553 ) ;
#190074 = VERTEX_POINT ( 'NONE', #150169 ) ;
#190075 = CIRCLE ( 'NONE', #27790, 0.09999999999999939493 ) ;
#190076 = EDGE_CURVE ( 'NONE', #112033, #143411, #229694, .T. ) ;
#190077 = DIRECTION ( 'NONE',  ( 1.000000000000000000, -0.000000000000000000, -0.000000000000000000 ) ) ;
#190078 = CARTESIAN_POINT ( 'NONE',  ( -20.54999999999999716, 68.75000000001151079, -48.37310748452436826 ) ) ;
#190079 = DIRECTION ( 'NONE',  ( 0.7071067811865463515, -0.7071067811865487940, 4.930380657631324879E-32 ) ) ;
#190080 = DIRECTION ( 'NONE',  ( 1.000000000000000000, -0.000000000000000000, -0.000000000000000000 ) ) ;
#190081 = AXIS2_PLACEMENT_3D ( 'NONE', #14171, #230636, #248915 ) ;
#190082 = CARTESIAN_POINT ( 'NONE',  ( 23.24999999999999289, 70.05000000001149374, -46.32880978955918039 ) ) ;
#190084 = CARTESIAN_POINT ( 'NONE',  ( 21.07199075132371746, 8.774944999116087274, -12.21353216161286426 ) ) ;
#190083 = CARTESIAN_POINT ( 'NONE',  ( -21.07016717456945898, 10.11353658153798918, -228.1608219491300531 ) ) ;
#190086 = VERTEX_POINT ( 'NONE', #11947 ) ;
#190085 = CARTESIAN_POINT ( 'NONE',  ( 18.39999999999999503, 11.47316190337363828, -57.75000000000000711 ) ) ;
#190087 = LINE ( 'NONE', #148395, #149968 ) ;
#190088 = ORIENTED_EDGE ( 'NONE', *, *, #235919, .T. ) ;
#190089 = AXIS2_PLACEMENT_3D ( 'NONE', #22853, #197600, #18962 ) ;
#190090 = ADVANCED_FACE ( 'NONE', ( #68043 ), #28971, .F. ) ;
#190091 = DIRECTION ( 'NONE',  ( 0.000000000000000000, 0.000000000000000000, -1.000000000000000000 ) ) ;
#190092 = ADVANCED_FACE ( 'NONE', ( #9344 ), #252976, .T. ) ;
#190093 = ORIENTED_EDGE ( 'NONE', *, *, #205273, .F. ) ;
#190094 = ORIENTED_EDGE ( 'NONE', *, *, #42559, .T. ) ;
#190095 = CYLINDRICAL_SURFACE ( 'NONE', #196232, 0.1000000000000001443 ) ;
#190096 = CARTESIAN_POINT ( 'NONE',  ( -16.93262454970420094, 10.00202046794151300, -46.07292377376269599 ) ) ;
#190097 = DIRECTION ( 'NONE',  ( -1.000000000000000000, 7.304098846218134667E-16, 5.100424963727256530E-30 ) ) ;
#190098 = CARTESIAN_POINT ( 'NONE',  ( -21.05000000000000071, -1.249999999988843369, -108.5000000000000426 ) ) ;
#190099 = EDGE_CURVE ( 'NONE', #210220, #237787, #63836, .T. ) ;
#190100 = CIRCLE ( 'NONE', #77443, 0.1000000000000055844 ) ;
#190101 = CARTESIAN_POINT ( 'NONE',  ( -21.14999999999999858, 76.00000000001169553, -75.78168612828702067 ) ) ;
#190102 = ADVANCED_FACE ( 'NONE', ( #215261 ), #250525, .T. ) ;
#190104 = VERTEX_POINT ( 'NONE', #18343 ) ;
#190103 = AXIS2_PLACEMENT_3D ( 'NONE', #243290, #107639, #4672 ) ;
#190105 = ORIENTED_EDGE ( 'NONE', *, *, #138444, .T. ) ;
#190106 = CIRCLE ( 'NONE', #77635, 4.100000000000006750 ) ;
#190107 = ORIENTED_EDGE ( 'NONE', *, *, #180063, .T. ) ;
#190108 = CARTESIAN_POINT ( 'NONE',  ( 21.14999999999999858, -11.74999999998884448, -112.7500000000000284 ) ) ;
#190109 = FACE_OUTER_BOUND ( 'NONE', #238114, .T. ) ;
#190110 = ORIENTED_EDGE ( 'NONE', *, *, #136240, .T. ) ;
#190111 = DIRECTION ( 'NONE',  ( 0.000000000000000000, 0.000000000000000000, 1.000000000000000000 ) ) ;
#190113 = EDGE_CURVE ( 'NONE', #97301, #98180, #140540, .T. ) ;
#190112 = CARTESIAN_POINT ( 'NONE',  ( -21.02374657821573933, 11.60000000083169702, -60.07179677019823316 ) ) ;
#190114 = CIRCLE ( 'NONE', #56784, 0.09999999999999939493 ) ;
#190115 = LINE ( 'NONE', #115705, #94581 ) ;
#190116 = FACE_OUTER_BOUND ( 'NONE', #129266, .T. ) ;
#190117 = VERTEX_POINT ( 'NONE', #32812 ) ;
#190118 = CARTESIAN_POINT ( 'NONE',  ( -18.59999999999999787, 64.35000000001222986, -148.6731074845244507 ) ) ;
#190119 = PLANE ( 'NONE',  #129181 ) ;
#190120 = CARTESIAN_POINT ( 'NONE',  ( 23.14999999999999503, 64.35000000001146248, -43.03791325517834565 ) ) ;
#190121 = DIRECTION ( 'NONE',  ( 1.000000000000000000, 0.000000000000000000, 0.000000000000000000 ) ) ;
#190122 = EDGE_CURVE ( 'NONE', #79286, #110943, #165512, .T. ) ;
#190123 = DIRECTION ( 'NONE',  ( 0.000000000000000000, 0.000000000000000000, 1.000000000000000000 ) ) ;
#190124 = VECTOR ( 'NONE', #60741, 1000.000000000000000 ) ;
#190125 = DIRECTION ( 'NONE',  ( -0.000000000000000000, 0.4088369013363281068, -0.9126074666063770380 ) ) ;
#190126 = EDGE_CURVE ( 'NONE', #3876, #231732, #230993, .T. ) ;
#190127 = EDGE_CURVE ( 'NONE', #122312, #8209, #155321, .T. ) ;
#190128 = EDGE_LOOP ( 'NONE', ( #98622, #61283, #107946, #193735 ) ) ;
#190129 = ADVANCED_FACE ( 'NONE', ( #232281 ), #53621, .F. ) ;
#190130 = CARTESIAN_POINT ( 'NONE',  ( -16.95709691156827148, 66.05000000001231797, -157.3630499220105037 ) ) ;
#190131 = ORIENTED_EDGE ( 'NONE', *, *, #163668, .F. ) ;
#190132 = CARTESIAN_POINT ( 'NONE',  ( -21.05000000000000071, 0.6656436123793473270, -212.6810495496487476 ) ) ;
#190133 = CARTESIAN_POINT ( 'NONE',  ( -16.87683809663752399, 23.65833333334447985, -184.2499999999999716 ) ) ;
#190134 = EDGE_CURVE ( 'NONE', #132923, #62069, #174909, .T. ) ;
#190136 = AXIS2_PLACEMENT_3D ( 'NONE', #58105, #193793, #252461 ) ;
#190135 = DIRECTION ( 'NONE',  ( 0.000000000000000000, 0.7397360091702792628, -0.6728971962616790981 ) ) ;
#190137 = CARTESIAN_POINT ( 'NONE',  ( 20.87631937322878883, 65.52850496324654728, -162.4433616099437927 ) ) ;
#190138 = EDGE_CURVE ( 'NONE', #193211, #225653, #194747, .T. ) ;
#190140 = ORIENTED_EDGE ( 'NONE', *, *, #178011, .F. ) ;
#190139 = AXIS2_PLACEMENT_3D ( 'NONE', #58120, #155990, #195120 ) ;
#190141 = DIRECTION ( 'NONE',  ( 1.000000000000000000, -0.000000000000000000, -0.000000000000000000 ) ) ;
#190142 = CARTESIAN_POINT ( 'NONE',  ( -18.59999999999999787, 77.83534155023700407, -191.9679561919613491 ) ) ;
#190143 = VECTOR ( 'NONE', #22670, 1000.000000000000000 ) ;
#190144 = AXIS2_PLACEMENT_3D ( 'NONE', #147628, #167227, #9392 ) ;
#190146 = EDGE_CURVE ( 'NONE', #108159, #109234, #254360, .T. ) ;
#190145 = LINE ( 'NONE', #14076, #160076 ) ;
#190147 = FACE_OUTER_BOUND ( 'NONE', #247636, .T. ) ;
#190148 = CARTESIAN_POINT ( 'NONE',  ( 21.00000000000000000, 66.25000000001253397, -182.2731074845244450 ) ) ;
#190149 = VECTOR ( 'NONE', #129382, 1000.000000000000000 ) ;
#190150 = ORIENTED_EDGE ( 'NONE', *, *, #59685, .T. ) ;
#190151 = VERTEX_POINT ( 'NONE', #36656 ) ;
#190152 = DIRECTION ( 'NONE',  ( -1.000000000000000000, 0.000000000000000000, 0.000000000000000000 ) ) ;
#190153 = DIRECTION ( 'NONE',  ( -1.000000000000000000, 0.000000000000000000, 0.000000000000000000 ) ) ;
#190154 = FACE_OUTER_BOUND ( 'NONE', #247361, .T. ) ;
#190155 = CARTESIAN_POINT ( 'NONE',  ( -16.87036670365549895, 44.00112830765706917, -235.3159266546824995 ) ) ;
#190156 = EDGE_CURVE ( 'NONE', #211199, #58126, #157335, .T. ) ;
#190157 = CIRCLE ( 'NONE', #77682, 0.09999999999999939493 ) ;
#190158 = EDGE_LOOP ( 'NONE', ( #75235, #236570, #155079, #138842 ) ) ;
#190159 = CARTESIAN_POINT ( 'NONE',  ( -21.65000000000000213, 7.250000000011138646, -143.2500000000000284 ) ) ;
#190160 = ITEM_DEFINED_TRANSFORMATION ( 'NONE', 'NONE', #236027,  #2425 ) ;
#190161 = TOROIDAL_SURFACE ( 'NONE', #223447, 0.2000000000000000111, 0.1000000000000000056 ) ;
#190162 = DIRECTION ( 'NONE',  ( 0.000000000000000000, -0.6728971962617483760, 0.7397360091702162022 ) ) ;
#190163 = CIRCLE ( 'NONE', #177710, 0.09999999999999939493 ) ;
#190164 = EDGE_LOOP ( 'NONE', ( #100794, #203453, #96170, #218606 ) ) ;
#190165 = DIRECTION ( 'NONE',  ( 1.000000000000000000, 0.000000000000000000, 0.000000000000000000 ) ) ;
#190166 = EDGE_LOOP ( 'NONE', ( #169602, #255108, #247952, #136607 ) ) ;
#190167 = ORIENTED_EDGE ( 'NONE', *, *, #58134, .T. ) ;
#190168 = CIRCLE ( 'NONE', #244307, 0.09999999999999892308 ) ;
#190169 = VERTEX_POINT ( 'NONE', #236102 ) ;
#190170 = CARTESIAN_POINT ( 'NONE',  ( -18.50000000000000000, 11.65000000001115232, -155.3500000000000227 ) ) ;
#190171 = LINE ( 'NONE', #192737, #188073 ) ;
#190172 = CARTESIAN_POINT ( 'NONE',  ( 20.94999999999999929, 28.51339163295720525, -258.4040038037771865 ) ) ;
#190173 = PLANE ( 'NONE',  #128082 ) ;
#190174 = DIRECTION ( 'NONE',  ( 8.673617379884087537E-15, -0.2617529984165031243, -0.9651348961777157509 ) ) ;
#190175 = CYLINDRICAL_SURFACE ( 'NONE', #207749, 0.1000000000000072220 ) ;
#190176 = DIRECTION ( 'NONE',  ( 1.000000000000000000, 0.000000000000000000, 0.000000000000000000 ) ) ;
#190178 = LINE ( 'NONE', #170657, #53798 ) ;
#190177 = CARTESIAN_POINT ( 'NONE',  ( -21.05000000000000071, 14.05000000001115623, -139.5136950707610026 ) ) ;
#190179 = EDGE_CURVE ( 'NONE', #30493, #137285, #173924, .T. ) ;
#190180 = CARTESIAN_POINT ( 'NONE',  ( -23.15000000000000213, 76.00000000001246292, -172.0231074845243597 ) ) ;
#190181 = DIRECTION ( 'NONE',  ( -6.938893903907222856E-15, 1.000000000000000000, 0.000000000000000000 ) ) ;
#190182 = CARTESIAN_POINT ( 'NONE',  ( 20.94999999999999929, 65.70729864261026876, -131.0657455973724836 ) ) ;
#190183 = FACE_OUTER_BOUND ( 'NONE', #33942, .T. ) ;
#190184 = CIRCLE ( 'NONE', #65266, 0.09999999999999939493 ) ;
#190185 = ORIENTED_EDGE ( 'NONE', *, *, #58673, .T. ) ;
#190186 = AXIS2_PLACEMENT_3D ( 'NONE', #158366, #16274, #197440 ) ;
#190187 = ADVANCED_FACE ( 'NONE', ( #116176 ), #86350, .T. ) ;
#190188 = ORIENTED_EDGE ( 'NONE', *, *, #32785, .F. ) ;
#190189 = CIRCLE ( 'NONE', #86085, 12.87500000000000000 ) ;
#190190 = CARTESIAN_POINT ( 'NONE',  ( -20.94999999999999929, 11.63687328911526109, -93.67824078667543120 ) ) ;
#190191 = AXIS2_PLACEMENT_3D ( 'NONE', #1132, #235909, #19450 ) ;
#190192 = LINE ( 'NONE', #228022, #36948 ) ;
#190193 = DIRECTION ( 'NONE',  ( 0.000000000000000000, 0.000000000000000000, -1.000000000000000000 ) ) ;
#190194 = DIRECTION ( 'NONE',  ( 1.000000000000000000, 0.000000000000000000, 0.000000000000000000 ) ) ;
#190195 = CARTESIAN_POINT ( 'NONE',  ( 21.05000000000000071, 5.000000000011153745, -54.59473398108690390 ) ) ;
#190196 = LINE ( 'NONE', #55764, #255931 ) ;
#190197 = ADVANCED_FACE ( 'NONE', ( #77023 ), #156611, .T. ) ;
#190198 = EDGE_LOOP ( 'NONE', ( #38509, #15878, #105869, #27134 ) ) ;
#190199 = ORIENTED_EDGE ( 'NONE', *, *, #51880, .T. ) ;
#190200 = CARTESIAN_POINT ( 'NONE',  ( -15.39126916658603506, 9.389571634546408418, -17.81764071236916536 ) ) ;
#190201 = TOROIDAL_SURFACE ( 'NONE', #19514, 7.800000000000000711, 0.1000000000000000056 ) ;
#190202 = VERTEX_POINT ( 'NONE', #74511 ) ;
#190203 = ADVANCED_FACE ( 'NONE', ( #137002 ), #144635, .F. ) ;
#190204 = DIRECTION ( 'NONE',  ( 0.000000000000000000, 0.5826443254699606999, 0.8127272543711416830 ) ) ;
#190205 = AXIS2_PLACEMENT_3D ( 'NONE', #188812, #7614, #145824 ) ;
#190206 = CIRCLE ( 'NONE', #156907, 0.09999999999999939493 ) ;
#190207 = ORIENTED_EDGE ( 'NONE', *, *, #173086, .T. ) ;
#190208 = LINE ( 'NONE', #191513, #18663 ) ;
#190209 = ORIENTED_EDGE ( 'NONE', *, *, #124860, .T. ) ;
#190210 = DIRECTION ( 'NONE',  ( -1.000000000000000000, 0.000000000000000000, 0.000000000000000000 ) ) ;
#190211 = CARTESIAN_POINT ( 'NONE',  ( 18.69999999999999929, 10.88519226655716565, -15.14794223642649840 ) ) ;
#190212 = FACE_OUTER_BOUND ( 'NONE', #150973, .T. ) ;
#190213 = CARTESIAN_POINT ( 'NONE',  ( 18.42595409746879298, -9.499999812553896916, -140.9993623517468961 ) ) ;
#190214 = DIRECTION ( 'NONE',  ( 0.000000000000000000, -0.2617529984165152257, -0.9651348961777124202 ) ) ;
#190215 = CARTESIAN_POINT ( 'NONE',  ( -23.25000000000000000, 11.75000000001115552, -88.75000000000004263 ) ) ;
#190216 = FACE_OUTER_BOUND ( 'NONE', #14593, .T. ) ;
#190217 = CYLINDRICAL_SURFACE ( 'NONE', #199647, 0.1000000000000200173 ) ;
#190219 = ORIENTED_EDGE ( 'NONE', *, *, #181874, .F. ) ;
#190218 = CARTESIAN_POINT ( 'NONE',  ( 18.40916198585734875, -0.7490475724413914183, -242.2033267618345747 ) ) ;
#190221 = FACE_OUTER_BOUND ( 'NONE', #21544, .T. ) ;
#190220 = DIRECTION ( 'NONE',  ( 0.000000000000000000, 7.162729191130010591E-15, -1.000000000000000000 ) ) ;
#190222 = VERTEX_POINT ( 'NONE', #134412 ) ;
#190223 = ORIENTED_EDGE ( 'NONE', *, *, #210950, .T. ) ;
#190224 = AXIS2_PLACEMENT_3D ( 'NONE', #58510, #216313, #155104 ) ;
#190225 = ORIENTED_EDGE ( 'NONE', *, *, #27115, .F. ) ;
#190226 = CARTESIAN_POINT ( 'NONE',  ( 18.54999999999999716, 19.41435213583508812, -230.3874019357809289 ) ) ;
#190227 = DIRECTION ( 'NONE',  ( -0.000000000000000000, -6.982962677686266711E-15, 1.000000000000000000 ) ) ;
#190228 = CARTESIAN_POINT ( 'NONE',  ( 20.96077737575322786, 62.98594959644118774, -207.1005776826179670 ) ) ;
#190229 = CARTESIAN_POINT ( 'NONE',  ( 13.99999999999999822, 9.850000000011137402, -117.2500000000000284 ) ) ;
#190230 = SPHERICAL_SURFACE ( 'NONE', #189709, 0.1000000000000000056 ) ;
#190232 = DIRECTION ( 'NONE',  ( 0.000000000000000000, 0.9167729611565434977, -0.3994087351226345284 ) ) ;
#190231 = VECTOR ( 'NONE', #95498, 1000.000000000000000 ) ;
#190234 = EDGE_CURVE ( 'NONE', #54914, #100676, #138266, .T. ) ;
#190233 = DIRECTION ( 'NONE',  ( -1.000000000000000000, -1.394253735153569469E-16, -2.602809386958778209E-16 ) ) ;
#190235 = DIRECTION ( 'NONE',  ( 1.000000000000000000, -0.000000000000000000, 0.000000000000000000 ) ) ;
#190236 = EDGE_CURVE ( 'NONE', #90690, #238394, #53060, .T. ) ;
#190238 = AXIS2_PLACEMENT_3D ( 'NONE', #114148, #172894, #252360 ) ;
#190237 = CARTESIAN_POINT ( 'NONE',  ( 23.14999999999999503, 14.10000000001115694, -94.89970238886068898 ) ) ;
#190239 = ORIENTED_EDGE ( 'NONE', *, *, #128009, .F. ) ;
#190240 = EDGE_LOOP ( 'NONE', ( #47899, #30388, #45710, #60327, #208686, #90974, #212688, #9085, #165171 ) ) ;
#190241 = CARTESIAN_POINT ( 'NONE',  ( 16.87683809663749557, 66.05000000001257376, -182.6731074845244223 ) ) ;
#190242 = CIRCLE ( 'NONE', #56917, 0.1000000000000020595 ) ;
#190243 = VECTOR ( 'NONE', #79374, 1000.000000000000000 ) ;
#190244 = ORIENTED_EDGE ( 'NONE', *, *, #151180, .T. ) ;
#190245 = CARTESIAN_POINT ( 'NONE',  ( 18.59999999999999432, 7.783179459866048866, -245.3643104511423303 ) ) ;
#190246 = ORIENTED_EDGE ( 'NONE', *, *, #180210, .F. ) ;
#190247 = CARTESIAN_POINT ( 'NONE',  ( 18.41815437325346849, -9.498709853141427573, -40.10394583880211172 ) ) ;
#190248 = AXIS2_PLACEMENT_3D ( 'NONE', #6669, #204861, #84889 ) ;
#190249 = EDGE_CURVE ( 'NONE', #80509, #220110, #157905, .T. ) ;
#190250 = B_SPLINE_CURVE_WITH_KNOTS ( 'NONE', 3,
 ( #72192, #52601, #153039, #207863, #188267, #132148, #187010, #50039 ),
 .UNSPECIFIED., .F., .F.,
 ( 4, 2, 2, 4 ),
 ( 0.000000000000000000, 0.0002181133598168738638, 0.0003271700397253405300, 0.0004362267196338071962 ),
 .UNSPECIFIED. ) ;
#190251 = CARTESIAN_POINT ( 'NONE',  ( -20.94999999999994600, 66.15000000001114699, -51.02310748452476474 ) ) ;
#190252 = DIRECTION ( 'NONE',  ( 0.000000000000000000, 1.265107689135680095E-16, -1.000000000000000000 ) ) ;
#190253 = AXIS2_PLACEMENT_3D ( 'NONE', #43867, #4711, #45143 ) ;
#190254 = DIRECTION ( 'NONE',  ( -1.000000000000000000, 0.000000000000000000, 0.000000000000000000 ) ) ;
#190255 = ADVANCED_FACE ( 'NONE', ( #140866 ), #239971, .F. ) ;
#190256 = DIRECTION ( 'NONE',  ( -1.000000000000000000, -0.000000000000000000, -0.000000000000000000 ) ) ;
#190257 = VERTEX_POINT ( 'NONE', #161733 ) ;
#190258 = EDGE_CURVE ( 'NONE', #159084, #47876, #44885, .T. ) ;
#190259 = CARTESIAN_POINT ( 'NONE',  ( 18.59999999999998366, 7.021664781911246322, -70.83356540189728889 ) ) ;
#190260 = DIRECTION ( 'NONE',  ( 1.186688945009009831E-16, 1.000000000000000000, 6.982962677686266711E-15 ) ) ;
#190261 = DIRECTION ( 'NONE',  ( 1.000000000000000000, 3.448943450116727019E-16, 6.438528483529604686E-16 ) ) ;
#190262 = EDGE_CURVE ( 'NONE', #198538, #168071, #78004, .T. ) ;
#190263 = DIRECTION ( 'NONE',  ( 0.000000000000000000, 0.000000000000000000, 1.000000000000000000 ) ) ;
#190264 = CARTESIAN_POINT ( 'NONE',  ( 20.85000000000000142, -1.736705739456431807, -112.0174225876237699 ) ) ;
#190265 = ORIENTED_EDGE ( 'NONE', *, *, #27861, .T. ) ;
#190267 = DIRECTION ( 'NONE',  ( 0.000000000000000000, -0.4721928772777346239, -0.8814952561688430555 ) ) ;
#190266 = CARTESIAN_POINT ( 'NONE',  ( -23.24999999999999645, 86.99291436658650412, -199.6658631664729739 ) ) ;
#190268 = CIRCLE ( 'NONE', #244210, 0.09999999999998898659 ) ;
#190269 = EDGE_LOOP ( 'NONE', ( #171020, #120219 ) ) ;
#190272 = VERTEX_POINT ( 'NONE', #163010 ) ;
#190271 = CARTESIAN_POINT ( 'NONE',  ( 20.95483826173899899, 67.12383379524233362, -161.4768319316249006 ) ) ;
#190270 = DIRECTION ( 'NONE',  ( 1.000000000000000000, -0.000000000000000000, -0.000000000000000000 ) ) ;
#190273 = DIRECTION ( 'NONE',  ( 0.000000000000000000, -1.000000000000000000, 0.000000000000000000 ) ) ;
#190274 = CIRCLE ( 'NONE', #248698, 0.2000000000000057288 ) ;
#190275 = CARTESIAN_POINT ( 'NONE',  ( 21.05000000000000071, -8.730841121484171907, -76.59807471898437825 ) ) ;
#190276 = AXIS2_PLACEMENT_3D ( 'NONE', #166039, #245560, #66907 ) ;
#190277 = CARTESIAN_POINT ( 'NONE',  ( -18.44448725179913495, 85.49008171549517954, -96.39414719046173730 ) ) ;
#190278 = EDGE_LOOP ( 'NONE', ( #172449, #96956, #152128, #227711, #61333 ) ) ;
#190279 = DIRECTION ( 'NONE',  ( 0.000000000000000000, 0.2617529984164915779, 0.9651348961777189706 ) ) ;
#190280 = AXIS2_PLACEMENT_3D ( 'NONE', #68357, #106166, #9659 ) ;
#190281 = ADVANCED_FACE ( 'NONE', ( #60019 ), #139554, .F. ) ;
#190283 = LINE ( 'NONE', #91164, #123815 ) ;
#190282 =( BOUNDED_SURFACE ( )  B_SPLINE_SURFACE ( 3, 2, ( 
 ( #216182, #77956, #153720 ),
 ( #37580, #237048, #234468 ),
 ( #97501, #14179, #157555 ),
 ( #137927, #217461, #38861 ),
 ( #191537, #16734, #12896 ),
 ( #231935, #92391, #35038 ),
 ( #171985, #251469, #114538 ),
 ( #72877, #53284, #54554 ) ),
 .UNSPECIFIED., .F., .F., .F. ) 
 B_SPLINE_SURFACE_WITH_KNOTS ( ( 4, 2, 2, 4 ),
 ( 3, 3 ),
 ( 0.0001704874539069866865, 0.0003809798300636611833, 0.0004862260181419984588, 0.0005914722062203357344 ),
 ( 0.000000000000000000, 1.000000000000000000 ),
 .UNSPECIFIED. ) 
 GEOMETRIC_REPRESENTATION_ITEM ( )  RATIONAL_B_SPLINE_SURFACE ( (
 ( 1.000000000000000000, 0.7071067811864942820, 1.000000000000000000),
 ( 1.000000000000000000, 0.7670648383578079210, 1.000000000000000000),
 ( 1.000000000000000000, 0.8204820770250040862, 1.000000000000000000),
 ( 1.000000000000000000, 0.8877218296114878227, 1.000000000000000000),
 ( 1.000000000000000000, 0.9080815932665453616, 1.000000000000000000),
 ( 1.000000000000000000, 0.9395541505861941811, 1.000000000000000000),
 ( 1.000000000000000000, 0.9506520335378926267, 1.000000000000000000),
 ( 1.000000000000000000, 0.9504532311154582080, 1.000000000000000000) ) ) 
 REPRESENTATION_ITEM ( '' )  SURFACE ( )  );
#190284 = AXIS2_PLACEMENT_3D ( 'NONE', #130913, #57463, #230012 ) ;
#190286 = DIRECTION ( 'NONE',  ( 0.000000000000000000, -0.4791956752371546169, -0.8777080977375152360 ) ) ;
#190285 = DIRECTION ( 'NONE',  ( -1.000000000000000000, 3.265361837132813093E-16, 2.280189983783949500E-30 ) ) ;
#190287 = AXIS2_PLACEMENT_3D ( 'NONE', #256041, #198692, #102127 ) ;
#190289 = ORIENTED_EDGE ( 'NONE', *, *, #46014, .F. ) ;
#190288 = CARTESIAN_POINT ( 'NONE',  ( -23.15000000000000213, 2.500000000011156409, -80.22462192276213955 ) ) ;
#190290 = VERTEX_POINT ( 'NONE', #53 ) ;
#190291 = CARTESIAN_POINT ( 'NONE',  ( 20.94999999999999929, 1.115600667400684642E-11, -171.5000000000000284 ) ) ;
#190292 = LINE ( 'NONE', #10373, #206171 ) ;
#190293 = TOROIDAL_SURFACE ( 'NONE', #31901, 0.2000000000000000111, 0.1000000000000000056 ) ;
#190294 = CYLINDRICAL_SURFACE ( 'NONE', #42680, 0.09999999999999939493 ) ;
#190295 = ORIENTED_EDGE ( 'NONE', *, *, #70438, .T. ) ;
#190296 = DIRECTION ( 'NONE',  ( 0.000000000000000000, 0.9126074666063770380, 0.4088369013363281068 ) ) ;
#190297 = VECTOR ( 'NONE', #35926, 1000.000000000000000 ) ;
#190298 = CARTESIAN_POINT ( 'NONE',  ( -23.25000000000000355, 11.75000000001113953, -143.2500000000000284 ) ) ;
#190299 = CARTESIAN_POINT ( 'NONE',  ( 18.59999999999999076, 35.94660524813656366, -234.4748257877825495 ) ) ;
#190300 = ORIENTED_EDGE ( 'NONE', *, *, #214497, .F. ) ;
#190301 = CARTESIAN_POINT ( 'NONE',  ( 20.59588692710267566, 59.22361013210799996, -225.7683383221924203 ) ) ;
#190302 = CARTESIAN_POINT ( 'NONE',  ( 20.94999999999999929, 5.850000000011105428, -144.1324972242779836 ) ) ;
#190303 = VECTOR ( 'NONE', #198680, 1000.000000000000000 ) ;
#190304 = ORIENTED_EDGE ( 'NONE', *, *, #117126, .F. ) ;
#190305 = DIRECTION ( 'NONE',  ( 1.000000000000000000, 0.000000000000000000, 0.000000000000000000 ) ) ;
#190306 = DIRECTION ( 'NONE',  ( -1.000000000000000000, 0.000000000000000000, 0.000000000000000000 ) ) ;
#190307 = EDGE_CURVE ( 'NONE', #165490, #182432, #217802, .T. ) ;
#190308 = ORIENTED_EDGE ( 'NONE', *, *, #128700, .F. ) ;
#190309 = VERTEX_POINT ( 'NONE', #199577 ) ;
#190310 = DIRECTION ( 'NONE',  ( 1.000000000000000000, 0.000000000000000000, 0.000000000000000000 ) ) ;
#190311 = EDGE_LOOP ( 'NONE', ( #186998, #61302, #167799, #254281 ) ) ;
#190313 = ORIENTED_EDGE ( 'NONE', *, *, #37865, .F. ) ;
#190312 = CARTESIAN_POINT ( 'NONE',  ( -20.94999999999999929, -1.736257131597395809, -11.56865232901749785 ) ) ;
#190314 = EDGE_CURVE ( 'NONE', #101718, #116556, #102997, .T. ) ;
#190315 = VERTEX_POINT ( 'NONE', #100419 ) ;
#190316 = TOROIDAL_SURFACE ( 'NONE', #136098, 2.100000000000002309, 0.1000000000000000056 ) ;
#190317 = AXIS2_PLACEMENT_3D ( 'NONE', #68122, #47249, #248034 ) ;
#190320 = ORIENTED_EDGE ( 'NONE', *, *, #47039, .F. ) ;
#190319 = ORIENTED_EDGE ( 'NONE', *, *, #85512, .F. ) ;
#190318 = CARTESIAN_POINT ( 'NONE',  ( 18.39999999999999858, -9.519327731081283162, -174.4729763765593020 ) ) ;
#190321 = EDGE_CURVE ( 'NONE', #32277, #50660, #200839, .T. ) ;
#190323 = ADVANCED_FACE ( 'NONE', ( #198255 ), #148947, .T. ) ;
#190322 = AXIS2_PLACEMENT_3D ( 'NONE', #124025, #64039, #203551 ) ;
#190324 = CIRCLE ( 'NONE', #65410, 0.09999999999998898659 ) ;
#190325 = CARTESIAN_POINT ( 'NONE',  ( -18.40000000000000213, -9.682403433465244902, -107.1568433774128266 ) ) ;
#190326 = ORIENTED_EDGE ( 'NONE', *, *, #34063, .T. ) ;
#190327 = CARTESIAN_POINT ( 'NONE',  ( 18.59999999999999076, 28.86532135423329493, -237.9457867389574517 ) ) ;
#190328 = DIRECTION ( 'NONE',  ( -1.000000000000000000, -0.000000000000000000, 0.000000000000000000 ) ) ;
#190329 = CARTESIAN_POINT ( 'NONE',  ( -23.25000000000000000, 11.75000000001115552, -193.9851942293460070 ) ) ;
#190330 = CIRCLE ( 'NONE', #77871, 0.1000000000000028644 ) ;
#190331 = CARTESIAN_POINT ( 'NONE',  ( -22.60000000000094289, 25.89494711235942148, -254.2627752153470055 ) ) ;
#190332 = EDGE_LOOP ( 'NONE', ( #145144, #257029, #82212 ) ) ;
#190333 = ORIENTED_EDGE ( 'NONE', *, *, #220280, .T. ) ;
#190334 = ORIENTED_EDGE ( 'NONE', *, *, #51650, .T. ) ;
#190335 = CARTESIAN_POINT ( 'NONE',  ( 21.08489247129320887, 8.877675190881227252, -146.3500000000000227 ) ) ;
#190337 = EDGE_LOOP ( 'NONE', ( #2832, #217005, #70380, #91251 ) ) ;
#190336 = CARTESIAN_POINT ( 'NONE',  ( -20.94999999999999929, 76.00000000001253397, -181.8231074845243711 ) ) ;
#190338 = DIRECTION ( 'NONE',  ( -0.000000000000000000, 0.000000000000000000, -1.000000000000000000 ) ) ;
#190340 = ORIENTED_EDGE ( 'NONE', *, *, #205067, .F. ) ;
#190339 = DIRECTION ( 'NONE',  ( -0.000000000000000000, 1.000000000000000000, 1.734723475976807292E-15 ) ) ;
#190341 = EDGE_CURVE ( 'NONE', #134542, #229965, #36542, .T. ) ;
#190342 = ORIENTED_EDGE ( 'NONE', *, *, #65579, .T. ) ;
#190343 = CARTESIAN_POINT ( 'NONE',  ( -18.40000000000000213, 65.08943781962308606, -222.1672656287770451 ) ) ;
#190344 = EDGE_CURVE ( 'NONE', #76136, #148869, #119724, .T. ) ;
#190345 = AXIS2_PLACEMENT_3D ( 'NONE', #148668, #208647, #155106 ) ;
#190346 = CIRCLE ( 'NONE', #169709, 11.65000000000000746 ) ;
#190347 = B_SPLINE_CURVE_WITH_KNOTS ( 'NONE', 3,
 ( #128717, #208261, #152149, #73903, #252489, #249942, #75179, #234212, #94705, #192540 ),
 .UNSPECIFIED., .F., .F.,
 ( 4, 3, 3, 4 ),
 ( 0.000000000000000000, 0.0002000000000008530056, 0.001000000000082974230, 0.001967863649483338456 ),
 .UNSPECIFIED. ) ;
#190349 = ORIENTED_EDGE ( 'NONE', *, *, #49432, .T. ) ;
#190348 = PRODUCT_DEFINITION ( 'UNKNOWN', '', #211277, #235731 ) ;
#190350 = CARTESIAN_POINT ( 'NONE',  ( -16.90202395485809816, 66.03405545546122823, -149.1200937632631565 ) ) ;
#190351 = DIRECTION ( 'NONE',  ( 0.000000000000000000, 0.000000000000000000, -1.000000000000000000 ) ) ;
#190352 = AXIS2_PLACEMENT_3D ( 'NONE', #49386, #191492, #134037 ) ;
#190354 = ORIENTED_EDGE ( 'NONE', *, *, #180665, .T. ) ;
#190353 = EDGE_LOOP ( 'NONE', ( #223693, #102604, #149805 ) ) ;
#190355 = ORIENTED_EDGE ( 'NONE', *, *, #31537, .F. ) ;
#190356 = CARTESIAN_POINT ( 'NONE',  ( 20.85000000000000142, -1.851617760457748618, -145.6031897196037050 ) ) ;
#190357 = ORIENTED_EDGE ( 'NONE', *, *, #33328, .T. ) ;
#190358 = ORIENTED_EDGE ( 'NONE', *, *, #50486, .F. ) ;
#190359 = EDGE_CURVE ( 'NONE', #17539, #156363, #153073, .T. ) ;
#190360 = CYLINDRICAL_SURFACE ( 'NONE', #63585, 0.1000000000000028644 ) ;
#190362 = ORIENTED_EDGE ( 'NONE', *, *, #231644, .T. ) ;
#190361 = FACE_OUTER_BOUND ( 'NONE', #159248, .T. ) ;
#190363 = EDGE_CURVE ( 'NONE', #76927, #143126, #186358, .T. ) ;
#190364 = CARTESIAN_POINT ( 'NONE',  ( -23.25000000000000000, 1.115600667400684642E-11, -67.00000000000000000 ) ) ;
#190365 = EDGE_CURVE ( 'NONE', #255583, #6746, #182261, .T. ) ;
#190367 = LINE ( 'NONE', #246465, #252545 ) ;
#190366 = CARTESIAN_POINT ( 'NONE',  ( 21.05000000000000071, 76.00000000001190870, -103.0231074845243029 ) ) ;
#190368 = CARTESIAN_POINT ( 'NONE',  ( -20.64999999999999858, 81.86853375790846599, -214.9828603846715964 ) ) ;
#190369 = CYLINDRICAL_SURFACE ( 'NONE', #94451, 1.749999999999999778 ) ;
#190370 = ORIENTED_EDGE ( 'NONE', *, *, #107230, .F. ) ;
#190371 = ORIENTED_EDGE ( 'NONE', *, *, #47248, .T. ) ;
#190372 = DIRECTION ( 'NONE',  ( 0.000000000000000000, 6.938893903907030216E-14, -1.000000000000000000 ) ) ;
#190373 = DIRECTION ( 'NONE',  ( -0.000000000000000000, 0.3848449534832665830, 0.9229812358756067647 ) ) ;
#190374 = EDGE_LOOP ( 'NONE', ( #101076, #39379, #150893, #206741, #131866 ) ) ;
#190375 = CIRCLE ( 'NONE', #11286, 0.09999999999999939493 ) ;
#190376 = CIRCLE ( 'NONE', #77911, 0.09999999999998898659 ) ;
#190377 = MANIFOLD_SOLID_BREP ( 'Stock-MAS-200-1', #224133 ) ;
#190378 = AXIS2_PLACEMENT_3D ( 'NONE', #23830, #105873, #124199 ) ;
#190379 = CIRCLE ( 'NONE', #52781, 0.1999999999999905742 ) ;
#190380 = CARTESIAN_POINT ( 'NONE',  ( -20.94999999999999929, 0.000000000000000000, -33.50000000000000000 ) ) ;
#190381 = CARTESIAN_POINT ( 'NONE',  ( 20.90000000000000213, 0.000000000000000000, 0.000000000000000000 ) ) ;
#190382 = ORIENTED_EDGE ( 'NONE', *, *, #116423, .T. ) ;
#190383 = VERTEX_POINT ( 'NONE', #6473 ) ;
#190384 =( BOUNDED_CURVE ( )  B_SPLINE_CURVE ( 3, ( #144122, #45044, #122016, #202830 ),
 .UNSPECIFIED., .F., .T. ) 
 B_SPLINE_CURVE_WITH_KNOTS ( ( 4, 4 ),
 ( 1.570796326794908992, 2.617993877991413587 ),
 .UNSPECIFIED. ) 
 CURVE ( )  GEOMETRIC_REPRESENTATION_ITEM ( )  RATIONAL_B_SPLINE_CURVE ( ( 1.000000000000000000, 0.9106836025229745335, 0.9106836025229745335, 1.000000000000000000 ) ) 
 REPRESENTATION_ITEM ( '' )  );
#190385 = CYLINDRICAL_SURFACE ( 'NONE', #42586, 0.1000000000000028644 ) ;
#190386 = CARTESIAN_POINT ( 'NONE',  ( -18.34374000495060386, 64.52683809664961245, -127.2731074845243882 ) ) ;
#190387 = ORIENTED_EDGE ( 'NONE', *, *, #12080, .T. ) ;
#190388 = CARTESIAN_POINT ( 'NONE',  ( -18.47653818581420282, -9.465280387751809243, -174.6259608161397807 ) ) ;
#190389 = VERTEX_POINT ( 'NONE', #228113 ) ;
#190390 = CARTESIAN_POINT ( 'NONE',  ( -21.05000000000000071, -5.011722593499800205, -233.2041167654973322 ) ) ;
#190391 = DIRECTION ( 'NONE',  ( 0.000000000000000000, 0.000000000000000000, -1.000000000000000000 ) ) ;
#190393 = DIRECTION ( 'NONE',  ( 1.000000000000000000, -0.000000000000000000, 0.000000000000000000 ) ) ;
#190392 = DIRECTION ( 'NONE',  ( 1.000000000000000000, 0.000000000000000000, 0.000000000000000000 ) ) ;
#190394 = CARTESIAN_POINT ( 'NONE',  ( 19.83283456528359423, 11.75000000001116263, -91.84999999941936721 ) ) ;
#190395 = DIRECTION ( 'NONE',  ( 1.000000000000000000, 0.000000000000000000, 0.000000000000000000 ) ) ;
#190396 = EDGE_CURVE ( 'NONE', #99286, #202617, #40813, .T. ) ;
#190397 = CARTESIAN_POINT ( 'NONE',  ( -20.94999999999999929, 1.115600667400684642E-11, -134.0000000000000284 ) ) ;
#190398 = AXIS2_PLACEMENT_3D ( 'NONE', #9339, #168476, #26356 ) ;
#190399 = CIRCLE ( 'NONE', #148700, 0.1000000000000028644 ) ;
#190400 = VECTOR ( 'NONE', #41341, 1000.000000000000227 ) ;
#190402 = ORIENTED_EDGE ( 'NONE', *, *, #223060, .T. ) ;
#190401 = CARTESIAN_POINT ( 'NONE',  ( -18.59999999999999787, 77.73670573947995877, -158.5056848969006182 ) ) ;
#190404 = ORIENTED_EDGE ( 'NONE', *, *, #34187, .T. ) ;
#190403 = ORIENTED_EDGE ( 'NONE', *, *, #200069, .F. ) ;
#190405 = AXIS2_PLACEMENT_3D ( 'NONE', #189898, #11266, #204307 ) ;
#190406 = EDGE_LOOP ( 'NONE', ( #25895, #8741, #255550, #250295 ) ) ;
#190407 = EDGE_CURVE ( 'NONE', #61807, #213807, #128281, .T. ) ;
#190408 = LINE ( 'NONE', #84826, #99042 ) ;
#190409 = DIRECTION ( 'NONE',  ( 0.000000000000000000, -0.1350103645451904977, 0.9908441862701596881 ) ) ;
#190411 = FACE_OUTER_BOUND ( 'NONE', #156456, .T. ) ;
#190410 = CARTESIAN_POINT ( 'NONE',  ( -23.25000000000000000, 1.115600667400684642E-11, -67.00000000000000000 ) ) ;
#190412 = LINE ( 'NONE', #74335, #120387 ) ;
#190413 = ORIENTED_EDGE ( 'NONE', *, *, #227048, .T. ) ;
#190414 = EDGE_CURVE ( 'NONE', #4366, #119120, #186544, .T. ) ;
#190415 = CARTESIAN_POINT ( 'NONE',  ( 21.72449340488910252, 10.28395627750227703, -79.65000000000004832 ) ) ;
#190416 = ORIENTED_EDGE ( 'NONE', *, *, #39696, .T. ) ;
#190417 = ORIENTED_EDGE ( 'NONE', *, *, #257212, .F. ) ;
#190418 = DIRECTION ( 'NONE',  ( -1.000000000000000000, -0.000000000000000000, -0.000000000000000000 ) ) ;
#190419 = CARTESIAN_POINT ( 'NONE',  ( -23.15000000000000213, 11.65000000001115588, -160.4851942293460638 ) ) ;
#190420 = EDGE_CURVE ( 'NONE', #51521, #36195, #198994, .T. ) ;
#190421 = DIRECTION ( 'NONE',  ( 0.000000000000000000, 0.000000000000000000, 1.000000000000000000 ) ) ;
#190422 = ORIENTED_EDGE ( 'NONE', *, *, #81405, .T. ) ;
#190423 = VECTOR ( 'NONE', #58857, 1000.000000000000000 ) ;
#190424 = DIRECTION ( 'NONE',  ( 0.000000000000000000, 0.000000000000000000, 1.000000000000000000 ) ) ;
#190425 = EDGE_CURVE ( 'NONE', #215026, #8175, #72423, .T. ) ;
#190426 = CARTESIAN_POINT ( 'NONE',  ( -18.59999999999999787, 7.021664781911246322, -137.8335654018973457 ) ) ;
#190427 = ADVANCED_FACE ( 'NONE', ( #205964 ), #211473, .T. ) ;
#190428 = EDGE_LOOP ( 'NONE', ( #46030, #63781, #35866, #168316 ) ) ;
#190429 = VERTEX_POINT ( 'NONE', #46874 ) ;
#190430 = CYLINDRICAL_SURFACE ( 'NONE', #166561, 0.09999999999999939493 ) ;
#190431 = CARTESIAN_POINT ( 'NONE',  ( -16.94107738177414291, 10.01423928514777373, -54.44999999999999574 ) ) ;
#190432 = CARTESIAN_POINT ( 'NONE',  ( 20.94999999999999574, 76.00000000001237765, -170.0231074845243597 ) ) ;
#190433 = DIRECTION ( 'NONE',  ( 1.000000000000000000, 0.000000000000000000, 0.000000000000000000 ) ) ;
#190434 = CIRCLE ( 'NONE', #11339, 2.600000000000001421 ) ;
#190435 = CARTESIAN_POINT ( 'NONE',  ( 18.59999999999998721, 69.06610602788535402, -65.73746165015079157 ) ) ;
#190436 = ORIENTED_EDGE ( 'NONE', *, *, #152796, .T. ) ;
#190437 = DIRECTION ( 'NONE',  ( -1.000000000000000000, 0.000000000000000000, -0.000000000000000000 ) ) ;
#190438 = CARTESIAN_POINT ( 'NONE',  ( -17.01473183483379970, 66.05000000001224691, -149.2731074845244450 ) ) ;
#190440 = DIRECTION ( 'NONE',  ( 0.000000000000000000, 0.1298341882520022972, 0.9915357197604853789 ) ) ;
#190439 = DIRECTION ( 'NONE',  ( -1.000000000000000000, -0.000000000000000000, -0.000000000000000000 ) ) ;
#190441 = DIRECTION ( 'NONE',  ( -0.000000000000000000, -1.000000000000000000, 0.000000000000000000 ) ) ;
#190442 = VECTOR ( 'NONE', #146240, 1000.000000000000000 ) ;
#190443 = FACE_OUTER_BOUND ( 'NONE', #67917, .T. ) ;
#190444 = DIRECTION ( 'NONE',  ( -0.000000000000000000, -6.982962677686266711E-15, 1.000000000000000000 ) ) ;
#190445 = CARTESIAN_POINT ( 'NONE',  ( 23.14999999999998437, 1.115600667400684642E-11, -33.50000000000000000 ) ) ;
#190446 = CIRCLE ( 'NONE', #53030, 0.1999999999999961531 ) ;
#190448 = ORIENTED_EDGE ( 'NONE', *, *, #251983, .T. ) ;
#190447 = CARTESIAN_POINT ( 'NONE',  ( -33.72168855820452649, 23.65833333334447985, -150.7500000000000284 ) ) ;
#190449 = CIRCLE ( 'NONE', #119692, 0.09999999999998898659 ) ;
#190450 = ADVANCED_FACE ( 'NONE', ( #27376 ), #243807, .F. ) ;
#190451 = ADVANCED_FACE ( 'NONE', ( #7777 ), #247662, .F. ) ;
#190452 = PRODUCT_DEFINITION_FORMATION_WITH_SPECIFIED_SOURCE ( 'ANY', '', #74532, .NOT_KNOWN. ) ;
#190453 = AXIS2_PLACEMENT_3D ( 'NONE', #147027, #66232, #84454 ) ;
#190454 = EDGE_CURVE ( 'NONE', #77793, #138330, #99014, .T. ) ;
#190455 = DIRECTION ( 'NONE',  ( 0.000000000000000000, -1.000000000000000000, 0.000000000000000000 ) ) ;
#190456 = CIRCLE ( 'NONE', #203064, 0.09999999999999062417 ) ;
#190457 = DIRECTION ( 'NONE',  ( -0.000000000000000000, 1.000000000000000000, -0.000000000000000000 ) ) ;
#190458 = ADVANCED_FACE ( 'NONE', ( #129008 ), #53254, .T. ) ;
#190459 = CARTESIAN_POINT ( 'NONE',  ( 23.14999999999999503, 31.44980407958351876, -233.5445995079518582 ) ) ;
#190461 = EDGE_CURVE ( 'NONE', #182938, #240363, #232343, .T. ) ;
#190460 = CARTESIAN_POINT ( 'NONE',  ( 20.04142135623730070, 61.57587952878035509, -212.2000740415318774 ) ) ;
#190462 = FACE_OUTER_BOUND ( 'NONE', #32955, .T. ) ;
#190463 = AXIS2_PLACEMENT_3D ( 'NONE', #168392, #32722, #191784 ) ;
#190464 = DIRECTION ( 'NONE',  ( -3.265361837132814079E-16, 0.4721928772777359007, 0.8814952561688425003 ) ) ;
#190465 = CIRCLE ( 'NONE', #65524, 11.74999999999999645 ) ;
#190466 = DIRECTION ( 'NONE',  ( 1.000000000000000000, 0.000000000000000000, 0.000000000000000000 ) ) ;
#190467 = CARTESIAN_POINT ( 'NONE',  ( -16.97683809663753252, 66.05000000001157900, -56.25158271585445391 ) ) ;
#190468 = EDGE_CURVE ( 'NONE', #214318, #255306, #132356, .T. ) ;
#190469 = AXIS2_PLACEMENT_3D ( 'NONE', #131652, #33887, #213754 ) ;
#190470 = VERTEX_POINT ( 'NONE', #57132 ) ;
#190471 = FACE_OUTER_BOUND ( 'NONE', #197990, .T. ) ;
#190474 = EDGE_LOOP ( 'NONE', ( #38752, #153989, #55566, #104899 ) ) ;
#190473 = DIRECTION ( 'NONE',  ( -1.000000000000000000, 7.304098846218134667E-16, 2.111765289898285610E-31 ) ) ;
#190472 = VECTOR ( 'NONE', #132177, 1000.000000000000000 ) ;
#190475 = DIRECTION ( 'NONE',  ( 1.000000000000000000, -0.000000000000000000, 0.000000000000000000 ) ) ;
#190476 = ADVANCED_FACE ( 'NONE', ( #55844 ), #54587, .F. ) ;
#190477 = AXIS2_PLACEMENT_3D ( 'NONE', #153764, #233275, #54597 ) ;
#190478 = DIRECTION ( 'NONE',  ( 1.186688945009009831E-16, -1.000000000000000000, 0.000000000000000000 ) ) ;
#190479 = ORIENTED_EDGE ( 'NONE', *, *, #243391, .T. ) ;
#190480 = CYLINDRICAL_SURFACE ( 'NONE', #146956, 0.5000000000000004441 ) ;
#190481 = ADVANCED_FACE ( 'NONE', ( #36337 ), #52008, .F. ) ;
#190482 = APPLICATION_PROTOCOL_DEFINITION ( 'draft international standard', 'automotive_design', 1998, #152560 ) ;
#190483 = CARTESIAN_POINT ( 'NONE',  ( -21.05000000000000071, 69.69257478044671927, -136.5062876161386498 ) ) ;
#190484 = FACE_OUTER_BOUND ( 'NONE', #52491, .T. ) ;
#190485 = CARTESIAN_POINT ( 'NONE',  ( -18.45037301276651576, 85.49020044755381775, -96.01043334810995589 ) ) ;
#190486 = EDGE_LOOP ( 'NONE', ( #173564, #7846, #249354, #98699 ) ) ;
#190487 = DIRECTION ( 'NONE',  ( -1.000000000000000000, 0.000000000000000000, 0.000000000000000000 ) ) ;
#190488 = DIRECTION ( 'NONE',  ( -0.000000000000000000, -0.1350103645451928291, -0.9908441862701594660 ) ) ;
#190489 = AXIS2_PLACEMENT_3D ( 'NONE', #56279, #197078, #195836 ) ;
#190490 = CIRCLE ( 'NONE', #182092, 0.1000000000000028644 ) ;
#190491 = CARTESIAN_POINT ( 'NONE',  ( -18.40000000000000213, 5.650000000011139001, -54.35000000000000142 ) ) ;
#190492 = VERTEX_POINT ( 'NONE', #214950 ) ;
#190493 = ORIENTED_EDGE ( 'NONE', *, *, #251889, .F. ) ;
#190494 = DIRECTION ( 'NONE',  ( 0.7071067811865456854, -0.7071067811865493491, -0.000000000000000000 ) ) ;
#190495 = FACE_OUTER_BOUND ( 'NONE', #209300, .T. ) ;
#190497 = CIRCLE ( 'NONE', #136270, 0.09999999999998898659 ) ;
#190496 = LINE ( 'NONE', #130484, #119413 ) ;
#190498 = DIRECTION ( 'NONE',  ( -1.836970198721029934E-16, -1.000000000000000000, -6.982962677686266711E-15 ) ) ;
#190499 = AXIS2_PLACEMENT_3D ( 'NONE', #23634, #1452, #43167 ) ;
#190501 = CARTESIAN_POINT ( 'NONE',  ( 21.15000000000005542, 77.26165318615413469, -44.00978271863746016 ) ) ;
#190500 = DIRECTION ( 'NONE',  ( 0.000000000000000000, -6.982962677686266711E-15, 1.000000000000000000 ) ) ;
#190502 = DIRECTION ( 'NONE',  ( 0.000000000000000000, 0.8660254037844383745, -0.5000000000000003331 ) ) ;
#190503 = CARTESIAN_POINT ( 'NONE',  ( -17.29838795458018907, 65.62845014206934025, -114.4183662019116809 ) ) ;
#190504 = DIRECTION ( 'NONE',  ( -1.000000000000000000, 0.000000000000000000, 0.000000000000000000 ) ) ;
#190505 = ORIENTED_EDGE ( 'NONE', *, *, #105477, .T. ) ;
#190506 = ADVANCED_FACE ( 'NONE', ( #134112 ), #203280, .T. ) ;
#190508 = ORIENTED_EDGE ( 'NONE', *, *, #2516, .T. ) ;
#190507 = CARTESIAN_POINT ( 'NONE',  ( 21.05000000000000071, 64.35000000001195986, -102.9231074845243938 ) ) ;
#190509 = CARTESIAN_POINT ( 'NONE',  ( -18.59999999999999787, 9.350000000011156942, -45.85000000000000142 ) ) ;
#190510 = DIRECTION ( 'NONE',  ( 1.000000000000000000, -0.000000000000000000, -0.000000000000000000 ) ) ;
#190512 = CARTESIAN_POINT ( 'NONE',  ( -20.94999999999999929, 11.75000000001115552, -141.0148057706540214 ) ) ;
#190511 = DIRECTION ( 'NONE',  ( 0.000000000000000000, 6.982962677686266711E-15, -1.000000000000000000 ) ) ;
#190513 = AXIS2_PLACEMENT_3D ( 'NONE', #92176, #200273, #77731 ) ;
#190514 = ORIENTED_EDGE ( 'NONE', *, *, #248266, .F. ) ;
#190515 = CARTESIAN_POINT ( 'NONE',  ( -21.05000000000000071, 67.23127455305841238, -235.8551265064783991 ) ) ;
#190516 = CARTESIAN_POINT ( 'NONE',  ( -23.15000000000000213, -8.999999999988844479, -57.10603087734755690 ) ) ;
#190517 = DIRECTION ( 'NONE',  ( 0.000000000000000000, -0.8814952561688437216, 0.4721928772777334582 ) ) ;
#190518 = CARTESIAN_POINT ( 'NONE',  ( -21.05000000000000071, 14.09264586382695938, -237.4630250429333671 ) ) ;
#190519 = VERTEX_POINT ( 'NONE', #132865 ) ;
#190520 = AXIS2_PLACEMENT_3D ( 'NONE', #8137, #49818, #15532 ) ;
#190521 = ORIENTED_EDGE ( 'NONE', *, *, #15294, .T. ) ;
#190522 = CIRCLE ( 'NONE', #48452, 0.4000000000000114575 ) ;
#190523 = AXIS2_PLACEMENT_3D ( 'NONE', #241109, #179846, #80706 ) ;
#190524 = AXIS2_PLACEMENT_3D ( 'NONE', #210923, #32316, #111832 ) ;
#190525 = CARTESIAN_POINT ( 'NONE',  ( 22.47071067811865319, 10.68684811775432664, -226.8807012965928323 ) ) ;
#190526 = VECTOR ( 'NONE', #77613, 1000.000000000000000 ) ;
#190527 = ORIENTED_EDGE ( 'NONE', *, *, #125913, .F. ) ;
#190528 = EDGE_CURVE ( 'NONE', #126736, #52328, #49150, .T. ) ;
#190529 = DIRECTION ( 'NONE',  ( -0.8660254037843878594, 0.000000000000000000, -0.5000000000000880407 ) ) ;
#190530 = CIRCLE ( 'NONE', #86409, 0.1000000000000002692 ) ;
#190531 = CARTESIAN_POINT ( 'NONE',  ( 18.59999999999999432, -1.866714910046153308, -112.2526752462820525 ) ) ;
#190532 = DIRECTION ( 'NONE',  ( -1.000000000000000000, 0.000000000000000000, 0.000000000000000000 ) ) ;
#190533 = CARTESIAN_POINT ( 'NONE',  ( 21.10000000000000142, 6.322468214605803993, 12.11686199900910488 ) ) ;
#190534 = ORIENTED_EDGE ( 'NONE', *, *, #197340, .F. ) ;
#190535 = DIRECTION ( 'NONE',  ( 0.000000000000000000, -1.000000000000000000, -6.982962677686266711E-15 ) ) ;
#190536 = DIRECTION ( 'NONE',  ( 0.000000000000000000, 0.000000000000000000, 1.000000000000000000 ) ) ;
#190537 = CARTESIAN_POINT ( 'NONE',  ( -21.05000000000000426, -0.09999999998884340213, -161.0229329788752182 ) ) ;
#190538 = LINE ( 'NONE', #232229, #37424 ) ;
#190539 = CARTESIAN_POINT ( 'NONE',  ( 23.14999999999999858, 5.599999999999996980, -21.09473398108690390 ) ) ;
#190540 = DIRECTION ( 'NONE',  ( -3.469446951953604722E-14, -0.9999176327611370985, -0.01283462868040260302 ) ) ;
#190541 = CARTESIAN_POINT ( 'NONE',  ( -16.96982749440682525, 66.05000000001224691, -149.6478858933352001 ) ) ;
#190542 = EDGE_LOOP ( 'NONE', ( #186796, #52656, #49071, #169147, #93405, #227780 ) ) ;
#190544 = FACE_OUTER_BOUND ( 'NONE', #227069, .T. ) ;
#190543 = DIRECTION ( 'NONE',  ( 1.000000000000000000, 0.000000000000000000, 0.000000000000000000 ) ) ;
#190545 = ORIENTED_EDGE ( 'NONE', *, *, #75821, .T. ) ;
#190547 = VERTEX_POINT ( 'NONE', #151143 ) ;
#190546 = DIRECTION ( 'NONE',  ( -0.000000000000000000, 0.4791956752371484551, 0.8777080977375184556 ) ) ;
#190548 = CIRCLE ( 'NONE', #132253, 0.1999999999999987899 ) ;
#190549 = ORIENTED_EDGE ( 'NONE', *, *, #169111, .F. ) ;
#190550 = DIRECTION ( 'NONE',  ( 0.000000000000000000, -0.9915357197604853789, 0.1298341882520022694 ) ) ;
#190551 = DIRECTION ( 'NONE',  ( 0.000000000000000000, 0.000000000000000000, -1.000000000000000000 ) ) ;
#190552 = CARTESIAN_POINT ( 'NONE',  ( -20.65000000000000568, 64.19947762500697763, -225.4487242757812737 ) ) ;
#190553 = DIRECTION ( 'NONE',  ( 1.000000000000000000, 0.000000000000000000, -0.000000000000000000 ) ) ;
#190554 = ORIENTED_EDGE ( 'NONE', *, *, #36871, .T. ) ;
#190555 = CARTESIAN_POINT ( 'NONE',  ( 21.04999999999999716, 69.69554417806499202, -203.5020720079843102 ) ) ;
#190556 = ORIENTED_EDGE ( 'NONE', *, *, #82790, .T. ) ;
#190557 = FACE_OUTER_BOUND ( 'NONE', #101264, .T. ) ;
#190558 = EDGE_CURVE ( 'NONE', #254810, #22846, #215729, .T. ) ;
#190559 = LINE ( 'NONE', #150148, #55688 ) ;
#190560 = VECTOR ( 'NONE', #130462, 1000.000000000000000 ) ;
#190561 = ORIENTED_EDGE ( 'NONE', *, *, #120686, .T. ) ;
#190562 = TOROIDAL_SURFACE ( 'NONE', #48877, 11.90000000000000213, 0.1000000000000000056 ) ;
#190563 = CARTESIAN_POINT ( 'NONE',  ( -21.05000000000000071, 87.48912529308817909, -133.4231074845242233 ) ) ;
#190564 = VECTOR ( 'NONE', #205824, 1000.000000000000114 ) ;
#190565 = EDGE_LOOP ( 'NONE', ( #244172, #57881, #123968, #233277 ) ) ;
#190566 = CARTESIAN_POINT ( 'NONE',  ( 23.14999999999999858, 76.00000000001126921, -203.5231074845248997 ) ) ;
#190567 = EDGE_LOOP ( 'NONE', ( #31300, #95368, #103978, #65952 ) ) ;
#190568 = LINE ( 'NONE', #114861, #117712 ) ;
#190569 = EDGE_CURVE ( 'NONE', #193742, #203294, #165710, .T. ) ;
#190570 = CARTESIAN_POINT ( 'NONE',  ( -20.85000000000000142, 7.476371755685457643, -241.7308184205399471 ) ) ;
#190571 = FACE_OUTER_BOUND ( 'NONE', #110644, .T. ) ;
#190572 = EDGE_CURVE ( 'NONE', #110145, #30493, #91153, .T. ) ;
#190573 = FACE_OUTER_BOUND ( 'NONE', #189339, .T. ) ;
#190574 = AXIS2_PLACEMENT_3D ( 'NONE', #101995, #187993, #6781 ) ;
#190576 = TOROIDAL_SURFACE ( 'NONE', #15624, 12.77499999999999858, 0.1000000000000000056 ) ;
#190575 = DIRECTION ( 'NONE',  ( 0.000000000000000000, 1.000000000000000000, 0.000000000000000000 ) ) ;
#190577 = ADVANCED_FACE ( 'NONE', ( #32509 ), #257206, .T. ) ;
#190578 = CARTESIAN_POINT ( 'NONE',  ( -20.64999999999999858, 62.04503132991428060, -248.4786563706009588 ) ) ;
#190579 = CARTESIAN_POINT ( 'NONE',  ( -20.64999999999999858, 7.250000000011155521, -146.3500000000000227 ) ) ;
#190580 = ORIENTED_EDGE ( 'NONE', *, *, #21415, .F. ) ;
#190581 = DIRECTION ( 'NONE',  ( -4.701977403289178058E-30, 1.734723475976807094E-14, -1.000000000000000000 ) ) ;
#190582 = VERTEX_POINT ( 'NONE', #252780 ) ;
#190584 = CARTESIAN_POINT ( 'NONE',  ( 23.24999999999999645, 70.35000000001201670, -115.6731074845243512 ) ) ;
#190583 = DIRECTION ( 'NONE',  ( 0.000000000000000000, 0.000000000000000000, 1.000000000000000000 ) ) ;
#190585 = ORIENTED_EDGE ( 'NONE', *, *, #240401, .T. ) ;
#190586 = CIRCLE ( 'NONE', #19894, 0.1000000000000042383 ) ;
#190587 = FACE_OUTER_BOUND ( 'NONE', #29303, .T. ) ;
#190588 = CYLINDRICAL_SURFACE ( 'NONE', #80602, 1.749999999999999778 ) ;
#190589 = CARTESIAN_POINT ( 'NONE',  ( -18.39999999999999858, 58.59921997668411819, -223.8511959880075608 ) ) ;
#190590 = LINE ( 'NONE', #11956, #16844 ) ;
#190591 = ORIENTED_EDGE ( 'NONE', *, *, #66941, .T. ) ;
#190593 = ORIENTED_EDGE ( 'NONE', *, *, #11489, .F. ) ;
#190592 = DIRECTION ( 'NONE',  ( 0.000000000000000000, 0.9908441862701596881, 0.1350103645451904977 ) ) ;
#190594 = EDGE_CURVE ( 'NONE', #29211, #68130, #149139, .T. ) ;
#190596 = CARTESIAN_POINT ( 'NONE',  ( 18.49999999999999289, 68.87972903831452243, -132.8635444426850825 ) ) ;
#190595 = LINE ( 'NONE', #176171, #101169 ) ;
#190598 = ORIENTED_EDGE ( 'NONE', *, *, #182773, .F. ) ;
#190597 = DIRECTION ( 'NONE',  ( -0.000000000000000000, 1.000000000000000000, 0.000000000000000000 ) ) ;
#190599 = EDGE_LOOP ( 'NONE', ( #24468, #30877, #135910, #46005 ) ) ;
#190600 = AXIS2_PLACEMENT_3D ( 'NONE', #150005, #229527, #50848 ) ;
#190601 = CIRCLE ( 'NONE', #91191, 0.09999999999999939493 ) ;
#190602 = CARTESIAN_POINT ( 'NONE',  ( -22.50000000000000000, 7.591056067193246548, -199.2444047917219052 ) ) ;
#190603 = DIRECTION ( 'NONE',  ( -1.000000000000000000, 0.000000000000000000, 0.000000000000000000 ) ) ;
#190604 = EDGE_LOOP ( 'NONE', ( #104623, #79575, #99991, #14555 ) ) ;
#190605 = DIRECTION ( 'NONE',  ( 1.000000000000000000, -1.541976423090492636E-14, 0.000000000000000000 ) ) ;
#190606 = ORIENTED_EDGE ( 'NONE', *, *, #225496, .F. ) ;
#190607 = CARTESIAN_POINT ( 'NONE',  ( -22.39999999999999503, 68.20922040163927136, -203.6231074845244109 ) ) ;
#190608 = DIRECTION ( 'NONE',  ( 0.000000000000000000, -7.116814260417668513E-15, 1.000000000000000000 ) ) ;
#190609 = CIRCLE ( 'NONE', #194881, 0.09999999999999939493 ) ;
#190610 = EDGE_LOOP ( 'NONE', ( #200253, #210302, #141965, #30780, #135681, #140489, #105069 ) ) ;
#190611 = FACE_OUTER_BOUND ( 'NONE', #172908, .T. ) ;
#190612 = ADVANCED_FACE ( 'NONE', ( #74201 ), #96268, .F. ) ;
#190613 = CIRCLE ( 'NONE', #115570, 0.2000000000000057288 ) ;
#190614 = VERTEX_POINT ( 'NONE', #153755 ) ;
#190615 = AXIS2_PLACEMENT_3D ( 'NONE', #209160, #87909, #10971 ) ;
#190616 = CIRCLE ( 'NONE', #15843, 0.1000000000000028644 ) ;
#190617 = DIRECTION ( 'NONE',  ( -1.000000000000000000, -8.673617379884087537E-15, 0.000000000000000000 ) ) ;
#190618 = B_SPLINE_CURVE_WITH_KNOTS ( 'NONE', 3,
 ( #105575, #111701, #84721, #191267, #242547, #185148, #12623 ),
 .UNSPECIFIED., .F., .F.,
 ( 4, 3, 4 ),
 ( 0.000000000000000000, 1.860045280646148997E-05, 5.251155757305323837E-05 ),
 .UNSPECIFIED. ) ;
#190619 = AXIS2_PLACEMENT_3D ( 'NONE', #167787, #30841, #85610 ) ;
#190620 = ADVANCED_FACE ( 'NONE', ( #152444 ), #12933, .F. ) ;
#190621 = VERTEX_POINT ( 'NONE', #255304 ) ;
#190622 = ORIENTED_EDGE ( 'NONE', *, *, #230156, .T. ) ;
#190624 = CARTESIAN_POINT ( 'NONE',  ( 20.54374330479345545, 18.89937786101421580, -228.1205973389425594 ) ) ;
#190623 = AXIS2_PLACEMENT_3D ( 'NONE', #16230, #10106, #216950 ) ;
#190625 = ORIENTED_EDGE ( 'NONE', *, *, #87220, .T. ) ;
#190626 = CARTESIAN_POINT ( 'NONE',  ( 23.15000000000000213, 87.48912529308798014, -106.1231074845242262 ) ) ;
#190627 = CIRCLE ( 'NONE', #223898, 0.9750000000000036415 ) ;
#190628 = ORIENTED_EDGE ( 'NONE', *, *, #108995, .T. ) ;
#190630 = ORIENTED_EDGE ( 'NONE', *, *, #212081, .F. ) ;
#190629 = DIRECTION ( 'NONE',  ( -7.304098846218134667E-16, -1.000000000000000000, 0.000000000000000000 ) ) ;
#190631 = APPLICATION_CONTEXT ( 'automotive_design' ) ;
#190632 = EDGE_CURVE ( 'NONE', #55890, #194521, #76710, .T. ) ;
#190633 = ORIENTED_EDGE ( 'NONE', *, *, #105356, .F. ) ;
#190634 = DIRECTION ( 'NONE',  ( 0.000000000000000000, 0.2617529984165152257, 0.9651348961777124202 ) ) ;
#190635 = ORIENTED_EDGE ( 'NONE', *, *, #89406, .T. ) ;
#190638 = ORIENTED_EDGE ( 'NONE', *, *, #54050, .T. ) ;
#190637 = ORIENTED_EDGE ( 'NONE', *, *, #51339, .F. ) ;
#190636 = LINE ( 'NONE', #249320, #151981 ) ;
#190639 = EDGE_CURVE ( 'NONE', #159934, #6279, #249095, .T. ) ;
#190640 = FACE_OUTER_BOUND ( 'NONE', #236181, .T. ) ;
#190642 = VERTEX_POINT ( 'NONE', #114573 ) ;
#190641 = CIRCLE ( 'NONE', #252964, 0.1000000000000091788 ) ;
#190643 = AXIS2_PLACEMENT_3D ( 'NONE', #82522, #124266, #203784 ) ;
#190644 = AXIS2_PLACEMENT_3D ( 'NONE', #198033, #98907, #257965 ) ;
#190645 = CARTESIAN_POINT ( 'NONE',  ( 0.000000000000000000, 1.250000000000000000, 0.000000000000000000 ) ) ;
#190646 = CIRCLE ( 'NONE', #253152, 0.09999999999999063804 ) ;
#190647 = ORIENTED_EDGE ( 'NONE', *, *, #126416, .F. ) ;
#190648 =( GEOMETRIC_REPRESENTATION_CONTEXT ( 3 ) GLOBAL_UNCERTAINTY_ASSIGNED_CONTEXT ( ( #126045 ) ) GLOBAL_UNIT_ASSIGNED_CONTEXT ( ( #164287, #106851, #185122 ) ) REPRESENTATION_CONTEXT ( 'NONE', 'WORKASPACE' ) );
#190649 = DIRECTION ( 'NONE',  ( -1.000000000000000000, 0.000000000000000000, 0.000000000000000000 ) ) ;
#190650 = ADVANCED_FACE ( 'NONE', ( #115855 ), #86543, .F. ) ;
#190652 = EDGE_LOOP ( 'NONE', ( #112836, #169062, #75273, #252775 ) ) ;
#190651 = CARTESIAN_POINT ( 'NONE',  ( -20.94999999999999929, -11.64999999998884483, -69.90000000000004832 ) ) ;
#190653 = DIRECTION ( 'NONE',  ( 1.000000000000000000, 7.304098846218134667E-16, 0.000000000000000000 ) ) ;
#190654 = ORIENTED_EDGE ( 'NONE', *, *, #144352, .T. ) ;
#190655 = CIRCLE ( 'NONE', #194928, 0.09999999999999939493 ) ;
#190656 = DIRECTION ( 'NONE',  ( 0.000000000000000000, 0.000000000000000000, -1.000000000000000000 ) ) ;
#190657 = FACE_OUTER_BOUND ( 'NONE', #118456, .T. ) ;
#190659 = ORIENTED_EDGE ( 'NONE', *, *, #21175, .T. ) ;
#190658 = EDGE_CURVE ( 'NONE', #198432, #85964, #253154, .T. ) ;
#190660 = EDGE_CURVE ( 'NONE', #225002, #49064, #70028, .T. ) ;
#190661 = FACE_OUTER_BOUND ( 'NONE', #149096, .T. ) ;
#190662 = LINE ( 'NONE', #173695, #36717 ) ;
#190663 = ORIENTED_EDGE ( 'NONE', *, *, #206907, .T. ) ;
#190665 = ORIENTED_EDGE ( 'NONE', *, *, #91497, .T. ) ;
#190664 = CARTESIAN_POINT ( 'NONE',  ( 19.90621891164687440, 54.51371537586219063, -228.6772403362143109 ) ) ;
#190666 = FACE_OUTER_BOUND ( 'NONE', #29423, .T. ) ;
#190667 = AXIS2_PLACEMENT_3D ( 'NONE', #252904, #138081, #135511 ) ;
#190668 = CIRCLE ( 'NONE', #223938, 0.1000000000000016431 ) ;
#190669 = AXIS2_PLACEMENT_3D ( 'NONE', #7297, #25595, #45145 ) ;
#190670 = EDGE_CURVE ( 'NONE', #246179, #152513, #170016, .T. ) ;
#190672 = ORIENTED_EDGE ( 'NONE', *, *, #186595, .T. ) ;
#190671 = ORIENTED_EDGE ( 'NONE', *, *, #84968, .T. ) ;
#190674 = CLOSED_SHELL ( 'NONE', ( #256682, #121188, #86046, #238067, #31342, #166247, #236399, #89743, #142586, #143679, #64716, #40104, #62963, #61498, #104214, #49157, #235022, #167898, #248925, #22599, #103878, #179905, #3581, #241122, #248270, #2262, #44863, #65837, #160150, #24941, #6593, #12323, #245033, #30913, #49466, #223343, #18934, #47307, #170060, #232570, #101279, #164186, #252762, #15831, #211855, #233045, #229561, #239094, #232628, #191848, #67972, #76240, #245422, #136440, #208574, #1300, #232279, #178450, #183396, #165691, #128504, #202983, #103527, #156900, #73700, #42177, #136866, #209562, #80146, #233120, #51619, #238863, #127386, #139858, #151983, #79958, #5821, #8090, #233736, #199440, #240323, #184303, #226284, #50192, #207191, #161596, #105828, #254192, #239084, #166824, #183459, #69873, #122885, #40009, #41833, #208083, #207547, #68926, #198807, #144480, #176598, #5006, #256524, #162103, #44595, #24071, #6788, #65855, #228682, #84474, #90184, #115020, #9906, #47342, #226044, #208018, #204199, #243780, #128605, #240612, #241686, #117012, #66057, #113862, #108486, #83704, #87976, #140559, #198877, #31007, #160737, #186835, #166135, #146327, #22525, #184559, #55173, #166527, #141098, #234428, #122284, #205354, #215215, #120630, #115366, #147909, #28408, #54634, #51024, #169706, #153357, #112931, #92408, #146484, #197861, #254743, #19607, #170497, #25990, #46995, #98292, #199537, #38463, #82049, #115972, #246699, #172008, #143663, #184653, #231630, #37106, #59234, #76041, #196394, #9829, #183706, #104399, #210686, #254294, #173644, #38605, #16786, #132193, #195669, #205425, #6049, #118722, #73498, #232870, #46204, #176670, #74409, #5181, #238112, #37166, #124668, #51975, #37660, #205177, #101743, #211682, #170722, #187336, #240724, #114480, #255699, #25824, #58492, #33148, #203300, #161401, #149007, #80462, #67314, #16941, #213705, #214096, #183305, #73336, #91922, #176532, #12391, #15299, #68400, #227673, #36062, #203640, #22628, #120826, #29927, #14786, #18494, #65771, #183042, #206315, #144998, #77076, #40221, #47863, #170091, #150589, #67012, #165821, #222157, #146620, #253295, #102966, #110757, #120230, #73824, #155580, #31713, #176829, #236802, #131240, #58701, #13254, #115240, #251229, #253393, #25302, #75102, #244081, #153367, #90324, #136569, #159777, #102399, #225118, #15747, #63212, #108236, #188580, #31431, #256002, #176823, #152002, #28181, #124648, #224090, #148535, #52063, #251076, #202765, #184682, #74379, #13096, #244899, #106548, #188557, #241986, #216750, #249903, #83166, #112871, #4886, #183046, #214558, #124062, #241387, #173959, #209363, #35564, #17993, #224296, #195718, #163778, #132947, #31862, #174504, #258094, #133748, #82368, #69449, #164708, #97525, #117568, #162489, #105791, #56763, #137700, #7496, #150510, #69557, #520, #163037, #7603, #45656, #145346, #95054, #148603, #125409, #204445, #3772, #133153, #62214, #210672, #193209, #256575, #175464, #21189, #76200, #179499, #30236, #10038, #200782, #127683, #83588, #100576, #1912, #50815, #114866, #177554, #47535, #16258, #12027, #248375, #245267, #5465, #26048, #118812, #211850, #19326, #246874, #72345, #255179, #233968, #203370, #155502, #188326, #76445, #185099, #73039, #143344, #196837, #255415, #135326, #226327, #121724, #51652, #20136, #158374, #162319, #155102, #111774, #28642, #228986, #141780, #224718, #200324, #252519, #200085, #27761, #51184, #29227, #146455, #106032, #2102, #72300, #213788, #177146, #173887, #63773, #181497, #131767, #80717, #83960, #217103, #242766, #80892, #237903, #16642, #74833, #86972, #42646, #50459, #106898, #26463, #176776, #242150, #201350, #244952, #215211, #14253, #55603, #177457, #231329, #153724, #188359, #63185, #82342, #232811, #114413, #170081, #55626, #182902, #59468, #250635, #121355, #100344, #125858, #75481, #91196, #123686, #14939, #236522, #238021, #241941, #118804, #207245, #206568, #220560, #31516, #238610, #67017, #212112, #106392, #73159, #12378, #218338, #158133, #154598, #207922, #194684, #153542, #47057, #133481, #127494, #180020, #212734, #163244, #190577, #11721, #37277, #145963, #255053, #153731, #251399 ) ) ;
#190673 = ORIENTED_EDGE ( 'NONE', *, *, #83032, .F. ) ;
#190675 = DIRECTION ( 'NONE',  ( 0.000000000000000000, -1.000000000000000000, -6.982962677686265922E-15 ) ) ;
#190676 = VERTEX_POINT ( 'NONE', #97534 ) ;
#190677 = ORIENTED_EDGE ( 'NONE', *, *, #214294, .F. ) ;
#190678 = DIRECTION ( 'NONE',  ( 0.000000000000000000, -0.9908441862701605762, 0.1350103645451835310 ) ) ;
#190679 = ORIENTED_EDGE ( 'NONE', *, *, #134585, .F. ) ;
#190680 = ADVANCED_FACE ( 'NONE', ( #101363 ), #38714, .T. ) ;
#190681 = CARTESIAN_POINT ( 'NONE',  ( 18.59999999999999787, -9.849999999999942801, -15.00000000000002309 ) ) ;
#190682 = EDGE_CURVE ( 'NONE', #233526, #168, #221341, .T. ) ;
#190683 = DIRECTION ( 'NONE',  ( 1.000000000000000000, -0.000000000000000000, -0.000000000000000000 ) ) ;
#190684 = ORIENTED_EDGE ( 'NONE', *, *, #65882, .T. ) ;
#190685 = VECTOR ( 'NONE', #61139, 1000.000000000000000 ) ;
#190686 = CIRCLE ( 'NONE', #144858, 0.09999999999998898659 ) ;
#190687 = ORIENTED_EDGE ( 'NONE', *, *, #14067, .T. ) ;
#190688 = DIRECTION ( 'NONE',  ( 0.7071067811865456854, -0.7071067811865493491, -0.000000000000000000 ) ) ;
#190689 = AXIS2_PLACEMENT_3D ( 'NONE', #25316, #66985, #27899 ) ;
#190690 = VERTEX_POINT ( 'NONE', #237085 ) ;
#190691 = AXIS2_PLACEMENT_3D ( 'NONE', #103406, #104676, #105973 ) ;
#190692 = CARTESIAN_POINT ( 'NONE',  ( 18.59999999999999076, 11.75000000001115907, -21.75000000000000355 ) ) ;
#190693 = EDGE_CURVE ( 'NONE', #162766, #231702, #140738, .T. ) ;
#190694 = ORIENTED_EDGE ( 'NONE', *, *, #161459, .T. ) ;
#190695 = EDGE_CURVE ( 'NONE', #168502, #234219, #61630, .T. ) ;
#190696 = CARTESIAN_POINT ( 'NONE',  ( 22.50497660315937409, -0.07871793021434793369, -122.2502044951045832 ) ) ;
#190698 = ORIENTED_EDGE ( 'NONE', *, *, #108553, .T. ) ;
#190697 = DIRECTION ( 'NONE',  ( -1.000000000000000000, 2.952720810173289112E-16, 2.061873921506763405E-30 ) ) ;
#190699 = CARTESIAN_POINT ( 'NONE',  ( 23.24999999999999645, 43.39957528361355799, -233.6562381667159798 ) ) ;
#190700 = LINE ( 'NONE', #10753, #172585 ) ;
#190701 = AXIS2_PLACEMENT_3D ( 'NONE', #104959, #224933, #122004 ) ;
#190702 = CARTESIAN_POINT ( 'NONE',  ( 20.95545211741311320, 65.41358668846814339, -128.9369606249360629 ) ) ;
#190703 = DIRECTION ( 'NONE',  ( 8.673617379884087537E-15, -0.000000000000000000, 1.000000000000000000 ) ) ;
#190704 = LINE ( 'NONE', #152869, #61082 ) ;
#190705 = DIRECTION ( 'NONE',  ( 0.000000000000000000, 0.000000000000000000, 1.000000000000000000 ) ) ;
#190706 = DIRECTION ( 'NONE',  ( -0.000000000000000000, -6.982962677686266711E-15, 1.000000000000000000 ) ) ;
#190707 = AXIS2_PLACEMENT_3D ( 'NONE', #192677, #136518, #217339 ) ;
#190708 = AXIS2_PLACEMENT_3D ( 'NONE', #112505, #9525, #227295 ) ;
#190709 = CARTESIAN_POINT ( 'NONE',  ( 22.45463910399148233, 76.00000000001334399, -181.6726782947127958 ) ) ;
#190710 = EDGE_CURVE ( 'NONE', #234902, #178867, #178421, .T. ) ;
#190712 = CARTESIAN_POINT ( 'NONE',  ( 22.39999999999999503, 11.65000000001116298, -100.4000000000000483 ) ) ;
#190711 = TOROIDAL_SURFACE ( 'NONE', #28397, 0.6000000000000006439, 0.1000000000000000056 ) ;
#190714 = ORIENTED_EDGE ( 'NONE', *, *, #171520, .T. ) ;
#190713 = AXIS2_PLACEMENT_3D ( 'NONE', #141589, #103720, #243248 ) ;
#190716 = ORIENTED_EDGE ( 'NONE', *, *, #189441, .F. ) ;
#190715 = ORIENTED_EDGE ( 'NONE', *, *, #16079, .F. ) ;
#190717 = VERTEX_POINT ( 'NONE', #83096 ) ;
#190718 = CARTESIAN_POINT ( 'NONE',  ( -17.22767730083219817, 65.65075578754462526, -91.66553617509441665 ) ) ;
#190719 = CARTESIAN_POINT ( 'NONE',  ( -18.59999999999999787, 68.68284540823283635, -224.2482512540334767 ) ) ;
#190721 = CARTESIAN_POINT ( 'NONE',  ( -18.50000000000000000, 14.61354176542825201, -235.9279552357344016 ) ) ;
#190720 = DIRECTION ( 'NONE',  ( 1.000000000000000000, -0.000000000000000000, 0.000000000000000000 ) ) ;
#190722 = ORIENTED_EDGE ( 'NONE', *, *, #152792, .T. ) ;
#190723 = ORIENTED_EDGE ( 'NONE', *, *, #35554, .F. ) ;
#190724 = AXIS2_PLACEMENT_3D ( 'NONE', #86567, #21507, #143989 ) ;
#190725 = EDGE_CURVE ( 'NONE', #126029, #64409, #19317, .T. ) ;
#190726 = FILL_AREA_STYLE ('',( #51151 ) ) ;
#190727 = DIRECTION ( 'NONE',  ( 7.304098846218134667E-16, 1.000000000000000000, 6.982962677686267499E-15 ) ) ;
#190728 = CARTESIAN_POINT ( 'NONE',  ( 18.57399277249656322, 10.33112638556969820, -173.0901228926974795 ) ) ;
#190729 = ADVANCED_FACE ( 'NONE', ( #238355 ), #62292, .T. ) ;
#190730 = DIRECTION ( 'NONE',  ( -0.000000000000000000, -6.982962677686266711E-15, 1.000000000000000000 ) ) ;
#190731 = EDGE_LOOP ( 'NONE', ( #158855, #94690, #10626, #56014 ) ) ;
#190732 = ORIENTED_EDGE ( 'NONE', *, *, #73648, .T. ) ;
#190733 = AXIS2_PLACEMENT_3D ( 'NONE', #166840, #9012, #67701 ) ;
#190734 = CARTESIAN_POINT ( 'NONE',  ( 21.05000000000000071, 69.55000000001230376, -160.0060803140843859 ) ) ;
#190735 = CARTESIAN_POINT ( 'NONE',  ( 18.58685178364169488, 8.967183825920946205, -245.3887925020941907 ) ) ;
#190736 = ADVANCED_FACE ( 'NONE', ( #239655 ), #2298, .F. ) ;
#190737 = ADVANCED_FACE ( 'NONE', ( #140530 ), #215379, .T. ) ;
#190738 = CARTESIAN_POINT ( 'NONE',  ( -23.15000000000000213, 76.00000000001142553, -36.02310748452432421 ) ) ;
#190740 = ORIENTED_EDGE ( 'NONE', *, *, #22746, .F. ) ;
#190739 = DIRECTION ( 'NONE',  ( -0.000000000000000000, 1.000000000000000000, 6.982962677686266711E-15 ) ) ;
#190741 = CARTESIAN_POINT ( 'NONE',  ( -20.94999999999999929, 77.83534155023627932, -91.46795619196130644 ) ) ;
#190742 = CARTESIAN_POINT ( 'NONE',  ( 18.39999999999999147, 67.17743825834568838, -127.2731074845243597 ) ) ;
#190744 = EDGE_CURVE ( 'NONE', #238726, #195194, #204356, .T. ) ;
#190743 = DIRECTION ( 'NONE',  ( 0.000000000000000000, 0.000000000000000000, -1.000000000000000000 ) ) ;
#190745 = LINE ( 'NONE', #10795, #45703 ) ;
#190746 = ORIENTED_EDGE ( 'NONE', *, *, #69986, .T. ) ;
#190747 = DIRECTION ( 'NONE',  ( 0.000000000000000000, -0.4088369013363280513, 0.9126074666063769270 ) ) ;
#190748 = CYLINDRICAL_SURFACE ( 'NONE', #148647, 0.1000000000000013933 ) ;
#190750 = FACE_OUTER_BOUND ( 'NONE', #208440, .T. ) ;
#190749 = SPHERICAL_SURFACE ( 'NONE', #107559, 0.1000000000000000056 ) ;
#190751 = LINE ( 'NONE', #233714, #108018 ) ;
#190752 = CARTESIAN_POINT ( 'NONE',  ( 23.24999999999999289, 64.25000000001259082, -191.3731074845244393 ) ) ;
#190753 = CARTESIAN_POINT ( 'NONE',  ( -18.50000000000000000, 11.75000000001115197, -188.8499999999999659 ) ) ;
#190754 = FACE_OUTER_BOUND ( 'NONE', #191162, .T. ) ;
#190755 = AXIS2_PLACEMENT_3D ( 'NONE', #104772, #184333, #166106 ) ;
#190756 = CARTESIAN_POINT ( 'NONE',  ( 21.05000000000000071, 41.42187432231294508, -260.1830396872097140 ) ) ;
#190757 = DIRECTION ( 'NONE',  ( -1.073024830501117725E-15, 0.000000000000000000, 1.000000000000000000 ) ) ;
#190758 = AXIS2_PLACEMENT_3D ( 'NONE', #212261, #91011, #170608 ) ;
#190759 = ORIENTED_EDGE ( 'NONE', *, *, #32920, .F. ) ;
#190760 = ADVANCED_FACE ( 'NONE', ( #246075 ), #186733, .T. ) ;
#190761 = EDGE_CURVE ( 'NONE', #50959, #81287, #244972, .T. ) ;
#190762 = ORIENTED_EDGE ( 'NONE', *, *, #107088, .F. ) ;
#190763 = ORIENTED_EDGE ( 'NONE', *, *, #69982, .T. ) ;
#190764 = CARTESIAN_POINT ( 'NONE',  ( 20.72390388899075475, 65.41003688158664886, -95.51175918877980564 ) ) ;
#190765 = DIRECTION ( 'NONE',  ( -0.000000000000000000, 1.000000000000000000, 6.982962677686266711E-15 ) ) ;
#190766 = ORIENTED_EDGE ( 'NONE', *, *, #25672, .F. ) ;
#190767 = EDGE_CURVE ( 'NONE', #89629, #31578, #244765, .T. ) ;
#190768 = ORIENTED_EDGE ( 'NONE', *, *, #218835, .F. ) ;
#190769 = AXIS2_PLACEMENT_3D ( 'NONE', #81810, #217491, #235783 ) ;
#190770 = AXIS2_PLACEMENT_3D ( 'NONE', #58985, #138524, #43316 ) ;
#190771 = ORIENTED_EDGE ( 'NONE', *, *, #21758, .F. ) ;
#190772 = EDGE_CURVE ( 'NONE', #83555, #82173, #247337, .T. ) ;
#190773 = DIRECTION ( 'NONE',  ( 0.000000000000000000, -1.000000000000000000, -6.982962677686266711E-15 ) ) ;
#190774 = EDGE_CURVE ( 'NONE', #201923, #87766, #232537, .T. ) ;
#190775 = ORIENTED_EDGE ( 'NONE', *, *, #127659, .T. ) ;
#190776 = CIRCLE ( 'NONE', #28277, 12.77499999999999503 ) ;
#190777 = DIRECTION ( 'NONE',  ( 0.000000000000000000, 0.2617529984165152257, 0.9651348961777124202 ) ) ;
#190778 = DIRECTION ( 'NONE',  ( 0.000000000000000000, 0.8660254037844378194, 0.5000000000000016653 ) ) ;
#190779 = CARTESIAN_POINT ( 'NONE',  ( -20.54999999999999716, -8.999999999988844479, -157.6060308773475924 ) ) ;
#190780 = EDGE_CURVE ( 'NONE', #114130, #197089, #174287, .T. ) ;
#190781 = DIRECTION ( 'NONE',  ( -1.000000000000000000, 0.000000000000000000, 0.000000000000000000 ) ) ;
#190782 = DIRECTION ( 'NONE',  ( 0.000000000000000000, 0.1568667991644355497, -0.9876197685951332295 ) ) ;
#190784 = EDGE_LOOP ( 'NONE', ( #80431, #246140 ) ) ;
#190783 = CYLINDRICAL_SURFACE ( 'NONE', #150916, 0.1000000000000106914 ) ;
#190786 = CARTESIAN_POINT ( 'NONE',  ( 21.04999999999999716, 8.871279686006799281, -79.15000000000004832 ) ) ;
#190785 = CARTESIAN_POINT ( 'NONE',  ( 18.49999999999999645, 5.950000000011100632, -77.30570230503489881 ) ) ;
#190787 = DIRECTION ( 'NONE',  ( 1.000000000000000000, -0.000000000000000000, -0.000000000000000000 ) ) ;
#190788 = EDGE_CURVE ( 'NONE', #250359, #193526, #225191, .T. ) ;
#190789 = VERTEX_POINT ( 'NONE', #165245 ) ;
#190790 = CARTESIAN_POINT ( 'NONE',  ( -20.54999999999999716, -9.400000000000003908, -9.893969122652444881 ) ) ;
#190791 = DIRECTION ( 'NONE',  ( 0.000000000000000000, 0.2617529984164915779, 0.9651348961777189706 ) ) ;
#190792 = PLANE ( 'NONE',  #116682 ) ;
#190793 = ORIENTED_EDGE ( 'NONE', *, *, #30436, .F. ) ;
#190794 = EDGE_CURVE ( 'NONE', #44063, #105532, #61816, .T. ) ;
#190795 = DIRECTION ( 'NONE',  ( -1.000000000000000000, 0.000000000000000000, -0.000000000000000000 ) ) ;
#190796 = AXIS2_PLACEMENT_3D ( 'NONE', #147083, #90972, #12752 ) ;
#190797 = CARTESIAN_POINT ( 'NONE',  ( -21.05000000000000071, 4.252251777740764460, -211.8999245327126744 ) ) ;
#190798 = ORIENTED_EDGE ( 'NONE', *, *, #222663, .T. ) ;
#190799 = CIRCLE ( 'NONE', #3293, 11.80000000000000426 ) ;
#190800 = CIRCLE ( 'NONE', #49294, 11.64999999999999325 ) ;
#190801 = FACE_OUTER_BOUND ( 'NONE', #201552, .T. ) ;
#190802 = DIRECTION ( 'NONE',  ( 1.000000000000000000, 0.000000000000000000, 0.000000000000000000 ) ) ;
#190803 = CARTESIAN_POINT ( 'NONE',  ( -21.05000000000000071, 64.37928932189367970, -163.1546908321834337 ) ) ;
#190804 = ADVANCED_FACE ( 'NONE', ( #127407 ), #126098, .F. ) ;
#190805 = ORIENTED_EDGE ( 'NONE', *, *, #184695, .T. ) ;
#190806 = TOROIDAL_SURFACE ( 'NONE', #236542, 7.791421356237335338, 0.1000000000000000056 ) ;
#190807 = ORIENTED_EDGE ( 'NONE', *, *, #183453, .F. ) ;
#190809 = EDGE_CURVE ( 'NONE', #75064, #148820, #226474, .T. ) ;
#190808 = DIRECTION ( 'NONE',  ( -1.000000000000000000, -0.000000000000000000, -0.000000000000000000 ) ) ;
#190810 = DIRECTION ( 'NONE',  ( 1.000000000000000000, 2.952720810173289112E-16, -0.000000000000000000 ) ) ;
#190811 = CARTESIAN_POINT ( 'NONE',  ( 20.94999999999999929, 65.70711192142420032, -164.5651054685122574 ) ) ;
#190812 = FACE_BOUND ( 'NONE', #28651, .T. ) ;
#190814 = DIRECTION ( 'NONE',  ( 1.000000000000000000, 0.000000000000000000, 0.000000000000000000 ) ) ;
#190813 = LINE ( 'NONE', #49978, #159326 ) ;
#190815 = AXIS2_PLACEMENT_3D ( 'NONE', #75785, #92758, #210164 ) ;
#190817 = LINE ( 'NONE', #250744, #32554 ) ;
#190816 = AXIS2_PLACEMENT_3D ( 'NONE', #92887, #232436, #96720 ) ;
#190818 = CARTESIAN_POINT ( 'NONE',  ( 21.05000000000000071, -11.64999999998883595, -97.50000000000004263 ) ) ;
#190819 = DIRECTION ( 'NONE',  ( 0.000000000000000000, -0.000000000000000000, 1.000000000000000000 ) ) ;
#190820 = CIRCLE ( 'NONE', #170163, 0.3999999999999975797 ) ;
#190821 = EDGE_LOOP ( 'NONE', ( #172602, #205803, #43198, #39491, #233602 ) ) ;
#190822 = CARTESIAN_POINT ( 'NONE',  ( -18.50000000000000000, 13.67914474873013475, -219.8713009340548865 ) ) ;
#190824 = VERTEX_POINT ( 'NONE', #85663 ) ;
#190823 = CARTESIAN_POINT ( 'NONE',  ( 17.23472005113827166, 10.30788195451192379, -55.54657686006867578 ) ) ;
#190825 = AXIS2_PLACEMENT_3D ( 'NONE', #11860, #93933, #249172 ) ;
#190826 = CARTESIAN_POINT ( 'NONE',  ( -20.64999999999999858, 23.49882452903949925, -253.1653563615082305 ) ) ;
#190827 = DIRECTION ( 'NONE',  ( 0.000000000000000000, -3.122502256758250246E-14, -1.000000000000000000 ) ) ;
#190828 = FACE_OUTER_BOUND ( 'NONE', #125794, .T. ) ;
#190829 = ADVANCED_FACE ( 'NONE', ( #148244 ), #24479, .T. ) ;
#190830 = LINE ( 'NONE', #92969, #37730 ) ;
#190832 = ORIENTED_EDGE ( 'NONE', *, *, #212731, .T. ) ;
#190831 = DIRECTION ( 'NONE',  ( 0.000000000000000000, 0.000000000000000000, -1.000000000000000000 ) ) ;
#190833 = CARTESIAN_POINT ( 'NONE',  ( -21.14999999999999858, 11.75000000001115552, -33.50000000000000000 ) ) ;
#190834 = CARTESIAN_POINT ( 'NONE',  ( -23.25000000000000355, 5.650000000011139001, -180.1499999999999773 ) ) ;
#190835 = CARTESIAN_POINT ( 'NONE',  ( 22.49999999999999645, 11.74956712350054744, -66.89914163090132604 ) ) ;
#190836 = DIRECTION ( 'NONE',  ( 1.000000000000000000, 0.000000000000000000, -0.000000000000000000 ) ) ;
#190837 = VERTEX_POINT ( 'NONE', #227778 ) ;
#190838 = CARTESIAN_POINT ( 'NONE',  ( -20.94999999999999929, -10.51247937907010233, -206.3598299697285654 ) ) ;
#190839 = ORIENTED_EDGE ( 'NONE', *, *, #77273, .F. ) ;
#190840 = CARTESIAN_POINT ( 'NONE',  ( -16.93388492042258164, 66.01145817749596745, -90.42365260771055091 ) ) ;
#190841 = AXIS2_PLACEMENT_3D ( 'NONE', #255875, #60281, #77279 ) ;
#190842 = ORIENTED_EDGE ( 'NONE', *, *, #252701, .T. ) ;
#190843 = ADVANCED_FACE ( 'NONE', ( #45300 ), #6151, .F. ) ;
#190844 = DIRECTION ( 'NONE',  ( 0.000000000000000000, 1.000000000000000000, 6.352154140967427193E-15 ) ) ;
#190845 = AXIS2_PLACEMENT_3D ( 'NONE', #138345, #181375, #127 ) ;
#190846 = ORIENTED_EDGE ( 'NONE', *, *, #140278, .F. ) ;
#190847 = TOROIDAL_SURFACE ( 'NONE', #86719, 7.791421356237316687, 0.1000000000000000056 ) ;
#190848 = CARTESIAN_POINT ( 'NONE',  ( -21.05000000000000071, 1.115600667400684642E-11, -167.4999999999999716 ) ) ;
#190850 = FACE_OUTER_BOUND ( 'NONE', #191515, .T. ) ;
#190849 = STYLED_ITEM ( 'NONE', ( #78376 ), #21812 ) ;
#190851 = AXIS2_PLACEMENT_3D ( 'NONE', #225501, #69046, #104277 ) ;
#190852 = DIRECTION ( 'NONE',  ( -0.000000000000000000, -0.000000000000000000, 1.000000000000000000 ) ) ;
#190853 = ORIENTED_EDGE ( 'NONE', *, *, #209246, .T. ) ;
#190854 = VECTOR ( 'NONE', #38163, 1000.000000000000000 ) ;
#190855 = DIRECTION ( 'NONE',  ( -0.000000000000000000, 0.7397360091702708251, 0.6728971962616883129 ) ) ;
#190856 = DIRECTION ( 'NONE',  ( 0.000000000000000000, 0.000000000000000000, -1.000000000000000000 ) ) ;
#190857 = DIRECTION ( 'NONE',  ( 1.000000000000000000, -0.000000000000000000, -0.000000000000000000 ) ) ;
#190858 = CARTESIAN_POINT ( 'NONE',  ( 12.68104795156994768, 9.396533993953923414, -17.90593977917329127 ) ) ;
#190859 = DIRECTION ( 'NONE',  ( -0.000000000000000000, 6.982962677686266711E-15, -1.000000000000000000 ) ) ;
#190860 = VERTEX_POINT ( 'NONE', #29615 ) ;
#190861 = DIRECTION ( 'NONE',  ( 1.000000000000000000, -3.469446951953718318E-14, 2.003086131649645455E-14 ) ) ;
#190862 = TOROIDAL_SURFACE ( 'NONE', #145020, 11.70000000000000639, 0.1000000000000000056 ) ;
#190863 = EDGE_LOOP ( 'NONE', ( #230236, #256259, #102923, #95266, #101484 ) ) ;
#190865 = VERTEX_POINT ( 'NONE', #149557 ) ;
#190864 = CARTESIAN_POINT ( 'NONE',  ( 20.94999999999999929, 10.29288807859936838, -105.9580020160122160 ) ) ;
#190866 = EDGE_LOOP ( 'NONE', ( #47918, #178807, #129490, #172300 ) ) ;
#190867 = CLOSED_SHELL ( 'NONE', ( #225451, #194907, #73982, #257478, #185871, #111415, #181150, #60140, #109057, #235634, #158075, #62580, #13006, #252021, #42842, #178140, #108398, #134167, #138258, #114437, #172513, #16364, #98542, #9610, #222313, #33946, #148253, #203896, #240164, #109934, #189993, #64232, #227119, #194534, #133842, #252176, #58894, #52575, #99638, #176303, #4770, #33184, #257677, #205680, #10914, #45355, #74459, #195900, #137402, #250812, #102664, #48223, #69092 ) ) ;
#190868 = ORIENTED_EDGE ( 'NONE', *, *, #118562, .F. ) ;
#190869 = CARTESIAN_POINT ( 'NONE',  ( -16.88815647973233780, 66.04916738069687199, -190.8758904211984202 ) ) ;
#190870 = CARTESIAN_POINT ( 'NONE',  ( 21.05000000000000071, -1.249999999988843369, -108.4000000000000341 ) ) ;
#190871 = ORIENTED_EDGE ( 'NONE', *, *, #238300, .F. ) ;
#190872 = DIRECTION ( 'NONE',  ( 1.000000000000000000, 0.000000000000000000, 0.000000000000000000 ) ) ;
#190873 = CYLINDRICAL_SURFACE ( 'NONE', #226950, 0.09999999999999939493 ) ;
#190874 = ORIENTED_EDGE ( 'NONE', *, *, #71146, .F. ) ;
#190876 = ORIENTED_EDGE ( 'NONE', *, *, #209856, .F. ) ;
#190875 = LINE ( 'NONE', #31804, #96742 ) ;
#190877 = EDGE_CURVE ( 'NONE', #55134, #35438, #86722, .T. ) ;
#190878 = PLANE ( 'NONE',  #131930 ) ;
#190879 = DIRECTION ( 'NONE',  ( 0.000000000000000000, 0.000000000000000000, 1.000000000000000000 ) ) ;
#190880 = TOROIDAL_SURFACE ( 'NONE', #153474, 0.9750000000000019762, 0.1000000000000000056 ) ;
#190881 = VERTEX_POINT ( 'NONE', #170432 ) ;
#190882 = AXIS2_PLACEMENT_3D ( 'NONE', #2728, #41901, #62727 ) ;
#190883 = FACE_OUTER_BOUND ( 'NONE', #183211, .T. ) ;
#190884 = CARTESIAN_POINT ( 'NONE',  ( -12.25000000000000178, 66.65000000001204228, -119.7731074845243739 ) ) ;
#190885 = DIRECTION ( 'NONE',  ( -1.000000000000000000, -0.000000000000000000, 0.000000000000000000 ) ) ;
#190886 = EDGE_LOOP ( 'NONE', ( #88265, #69124, #5578, #62496 ) ) ;
#190887 = CARTESIAN_POINT ( 'NONE',  ( 20.94999999999999929, -8.999999999988842703, -157.6060308773475640 ) ) ;
#190888 = ADVANCED_FACE ( 'NONE', ( #94680 ), #152122, .F. ) ;
#190889 = CARTESIAN_POINT ( 'NONE',  ( -22.50047199487510596, -2.456544280668254476, -189.5095247662567033 ) ) ;
#190890 = AXIS2_PLACEMENT_3D ( 'NONE', #206234, #4170, #202382 ) ;
#190891 = EDGE_CURVE ( 'NONE', #12756, #129607, #99201, .T. ) ;
#190892 = CARTESIAN_POINT ( 'NONE',  ( -23.25000000000000000, 79.24821784679178904, -196.3217825494968736 ) ) ;
#190893 = VECTOR ( 'NONE', #245919, 1000.000000000000000 ) ;
#190894 = CIRCLE ( 'NONE', #253398, 0.1000000000000028644 ) ;
#190895 = VECTOR ( 'NONE', #155191, 1000.000000000000227 ) ;
#190896 = ADVANCED_FACE ( 'NONE', ( #189947 ), #230342, .F. ) ;
#190897 = AXIS2_PLACEMENT_3D ( 'NONE', #207326, #108213, #187762 ) ;
#190898 = ORIENTED_EDGE ( 'NONE', *, *, #220846, .F. ) ;
#190899 = CARTESIAN_POINT ( 'NONE',  ( 21.07946286933444924, 0.07668384326756245983, -94.17096268099238898 ) ) ;
#190900 = EDGE_CURVE ( 'NONE', #16586, #169290, #255191, .T. ) ;
#190901 = ORIENTED_EDGE ( 'NONE', *, *, #29198, .T. ) ;
#190902 = EDGE_CURVE ( 'NONE', #3373, #86852, #140930, .T. ) ;
#190903 = CARTESIAN_POINT ( 'NONE',  ( -18.39999999999999858, -9.519327731081281385, -174.4729763765593020 ) ) ;
#190904 = DIRECTION ( 'NONE',  ( 0.000000000000000000, 0.000000000000000000, -1.000000000000000000 ) ) ;
#190906 = ORIENTED_EDGE ( 'NONE', *, *, #22600, .T. ) ;
#190905 = LINE ( 'NONE', #248278, #45930 ) ;
#190907 = DIRECTION ( 'NONE',  ( 0.000000000000000000, -0.000000000000000000, 1.000000000000000000 ) ) ;
#190908 = DIRECTION ( 'NONE',  ( -0.000000000000000000, -0.000000000000000000, 1.000000000000000000 ) ) ;
#190909 = ADVANCED_FACE ( 'NONE', ( #154694 ), #71300, .T. ) ;
#190910 = CARTESIAN_POINT ( 'NONE',  ( 18.49999999999999645, 67.23127455305841238, -235.8551265064783991 ) ) ;
#190911 = DIRECTION ( 'NONE',  ( 0.000000000000000000, 0.9651348961777379554, -0.2617529984164210233 ) ) ;
#190912 = DIRECTION ( 'NONE',  ( -1.000000000000000000, -0.000000000000000000, 0.000000000000000000 ) ) ;
#190913 = CIRCLE ( 'NONE', #7526, 4.000000000000003553 ) ;
#190914 = CARTESIAN_POINT ( 'NONE',  ( -20.54999999999999716, 36.65892442174935439, -249.5511627012433848 ) ) ;
#190915 = DIRECTION ( 'NONE',  ( -0.000000000000000000, -1.265107689135680095E-16, 1.000000000000000000 ) ) ;
#190917 = ORIENTED_EDGE ( 'NONE', *, *, #131801, .T. ) ;
#190916 = CARTESIAN_POINT ( 'NONE',  ( -22.41119224318417125, 76.00000000001203659, -114.6726782920691221 ) ) ;
#190918 = EDGE_CURVE ( 'NONE', #104591, #90311, #129945, .T. ) ;
#190919 = DIRECTION ( 'NONE',  ( 0.000000000000000000, -6.982962677686266711E-15, 1.000000000000000000 ) ) ;
#190920 = CARTESIAN_POINT ( 'NONE',  ( -21.05000000000000071, 1.115600667400684642E-11, -171.7999999999999545 ) ) ;
#190921 = CARTESIAN_POINT ( 'NONE',  ( -18.50000000000000000, 85.40000000001167280, -62.64106563635157698 ) ) ;
#190922 = CYLINDRICAL_SURFACE ( 'NONE', #105521, 0.09999999999999939493 ) ;
#190923 = VERTEX_POINT ( 'NONE', #92116 ) ;
#190924 = EDGE_CURVE ( 'NONE', #225321, #40998, #20129, .T. ) ;
#190925 = CARTESIAN_POINT ( 'NONE',  ( 20.85000000000000142, 0.1610488207298751417, -133.7158101556398151 ) ) ;
#190926 = DIRECTION ( 'NONE',  ( 0.000000000000000000, -6.982962677686266711E-15, 1.000000000000000000 ) ) ;
#190927 = VECTOR ( 'NONE', #235064, 1000.000000000000000 ) ;
#190928 = AXIS2_PLACEMENT_3D ( 'NONE', #189691, #12361, #171451 ) ;
#190929 = ORIENTED_EDGE ( 'NONE', *, *, #141565, .T. ) ;
#190930 = CARTESIAN_POINT ( 'NONE',  ( 23.24999999999999645, 64.25000000001210765, -127.2731074845243882 ) ) ;
#190931 = CARTESIAN_POINT ( 'NONE',  ( -16.93658211146646408, 9.994108662352344297, -79.59570493004436287 ) ) ;
#190932 = EDGE_CURVE ( 'NONE', #145377, #192844, #16059, .T. ) ;
#190933 = ORIENTED_EDGE ( 'NONE', *, *, #131491, .T. ) ;
#190934 = EDGE_LOOP ( 'NONE', ( #234809, #159990, #219857 ) ) ;
#190935 = LINE ( 'NONE', #30573, #217333 ) ;
#190937 = ORIENTED_EDGE ( 'NONE', *, *, #41430, .T. ) ;
#190936 = FACE_OUTER_BOUND ( 'NONE', #254322, .T. ) ;
#190938 = VERTEX_POINT ( 'NONE', #110395 ) ;
#190939 = CARTESIAN_POINT ( 'NONE',  ( 18.59999999999999432, 70.47363787294415260, -228.3418745167492432 ) ) ;
#190940 = VECTOR ( 'NONE', #6999, 1000.000000000000114 ) ;
#190941 = ORIENTED_EDGE ( 'NONE', *, *, #195783, .F. ) ;
#190943 = EDGE_LOOP ( 'NONE', ( #58096, #231435, #32900, #254200 ) ) ;
#190942 = EDGE_LOOP ( 'NONE', ( #188762, #144110, #202857, #118253, #26981 ) ) ;
#190945 = CARTESIAN_POINT ( 'NONE',  ( 18.47073956224740954, 85.47172941248408051, -129.4144217317060566 ) ) ;
#190944 = AXIS2_PLACEMENT_3D ( 'NONE', #220364, #199527, #23470 ) ;
#190946 = B_SPLINE_CURVE_WITH_KNOTS ( 'NONE', 3,
 ( #158498, #179339, #222262, #61944, #237992, #163614, #82743, #141469, #121923, #22838 ),
 .UNSPECIFIED., .F., .F.,
 ( 4, 3, 3, 4 ),
 ( 0.000000000000000000, 1.004626015990891703E-05, 1.831183478181717294E-05, 2.062343583994978553E-05 ),
 .UNSPECIFIED. ) ;
#190948 = ORIENTED_EDGE ( 'NONE', *, *, #180729, .F. ) ;
#190947 = CARTESIAN_POINT ( 'NONE',  ( 21.06490991615909181, 10.72489134759826790, -146.2037113535331514 ) ) ;
#190949 = FACE_OUTER_BOUND ( 'NONE', #103767, .T. ) ;
#190950 = ORIENTED_EDGE ( 'NONE', *, *, #120878, .T. ) ;
#190951 = ADVANCED_FACE ( 'NONE', ( #11307 ), #192510, .F. ) ;
#190952 = AXIS2_PLACEMENT_3D ( 'NONE', #174370, #197726, #135174 ) ;
#190953 = ORIENTED_EDGE ( 'NONE', *, *, #89221, .F. ) ;
#190954 = LINE ( 'NONE', #245770, #245026 ) ;
#190955 = DIRECTION ( 'NONE',  ( 0.000000000000000000, -0.9126074666063545004, -0.4088369013363783999 ) ) ;
#190956 = EDGE_CURVE ( 'NONE', #173891, #148222, #54266, .T. ) ;
#190957 = CARTESIAN_POINT ( 'NONE',  ( -18.39999999999999858, 37.99112772578902764, -261.0419300540664835 ) ) ;
#190958 = ORIENTED_EDGE ( 'NONE', *, *, #11387, .T. ) ;
#190959 = DIRECTION ( 'NONE',  ( 0.000000000000000000, 0.2617529984165031243, 0.9651348961777157509 ) ) ;
#190960 = CARTESIAN_POINT ( 'NONE',  ( -12.29659703204452015, 66.64411154551000038, -187.2344645877464018 ) ) ;
#190961 = DIRECTION ( 'NONE',  ( 0.000000000000000000, 0.000000000000000000, 1.000000000000000000 ) ) ;
#190963 = ORIENTED_EDGE ( 'NONE', *, *, #97709, .F. ) ;
#190962 = ADVANCED_FACE ( 'NONE', ( #34743 ), #114253, .T. ) ;
#190965 = EDGE_CURVE ( 'NONE', #219834, #231063, #185650, .T. ) ;
#190964 = DIRECTION ( 'NONE',  ( 0.000000000000000000, 0.01562500000001045344, 0.9998779222360096863 ) ) ;
#190966 = DIRECTION ( 'NONE',  ( -0.000000000000000000, -0.1350103645451835865, -0.9908441862701606873 ) ) ;
#190967 = DIRECTION ( 'NONE',  ( -1.000000000000000000, -7.304098846218134667E-16, 0.000000000000000000 ) ) ;
#190968 = LINE ( 'NONE', #30606, #17808 ) ;
#190969 = CIRCLE ( 'NONE', #107729, 0.1000000000000000472 ) ;
#190970 = ORIENTED_EDGE ( 'NONE', *, *, #197077, .T. ) ;
#190971 = ORIENTED_EDGE ( 'NONE', *, *, #54179, .T. ) ;
#190972 = DIRECTION ( 'NONE',  ( 0.000000000000000000, 0.000000000000000000, 1.000000000000000000 ) ) ;
#190973 = AXIS2_PLACEMENT_3D ( 'NONE', #144750, #127789, #225566 ) ;
#190974 = EDGE_LOOP ( 'NONE', ( #189901, #178991, #14524, #45501, #98397, #92170, #113616, #254994, #85822, #79559, #253592, #199646, #183019, #253754, #200807, #188907, #239725, #225543, #179072, #151734, #138523, #80578, #93545 ) ) ;
#190975 = CIRCLE ( 'NONE', #49485, 11.65000000000000036 ) ;
#190976 = CARTESIAN_POINT ( 'NONE',  ( -12.25000000000000178, 26.30888228346803714, -233.3999513616626587 ) ) ;
#190977 = LINE ( 'NONE', #157969, #98057 ) ;
#190978 = ADVANCED_FACE ( 'NONE', ( #65693 ), #248194, .F. ) ;
#190979 = ORIENTED_EDGE ( 'NONE', *, *, #72754, .T. ) ;
#190980 = VERTEX_POINT ( 'NONE', #49987 ) ;
#190981 = DIRECTION ( 'NONE',  ( 0.000000000000000000, -2.771150684185008344E-14, -1.000000000000000000 ) ) ;
#190982 = CARTESIAN_POINT ( 'NONE',  ( -18.50000000000000000, 4.252251777740764460, -211.8999245327126744 ) ) ;
#190983 = ORIENTED_EDGE ( 'NONE', *, *, #147961, .F. ) ;
#190984 = CARTESIAN_POINT ( 'NONE',  ( -18.50000000000000000, 64.25000000001223555, -148.6731074845244507 ) ) ;
#190985 =( NAMED_UNIT ( * ) SI_UNIT ( $, .STERADIAN. ) SOLID_ANGLE_UNIT ( ) );
#190986 = VERTEX_POINT ( 'NONE', #104785 ) ;
#190987 = VECTOR ( 'NONE', #117601, 1000.000000000000000 ) ;
#190989 = ORIENTED_EDGE ( 'NONE', *, *, #176839, .T. ) ;
#190988 = AXIS2_PLACEMENT_3D ( 'NONE', #161722, #164278, #122587 ) ;
#190991 = CARTESIAN_POINT ( 'NONE',  ( -20.85000000000000142, -11.74999999998884448, -200.9999999999999432 ) ) ;
#190990 = CIRCLE ( 'NONE', #32794, 0.09999999999999939493 ) ;
#190992 = CARTESIAN_POINT ( 'NONE',  ( 20.85000000000000142, 1.115600667400684642E-11, -67.00000000000000000 ) ) ;
#190993 = EDGE_CURVE ( 'NONE', #117705, #174077, #34512, .T. ) ;
#190994 = ADVANCED_FACE ( 'NONE', ( #226019, #186960 ), #7005, .F. ) ;
#190995 = CARTESIAN_POINT ( 'NONE',  ( -21.05000000000000071, 74.83729825007408465, -128.5231074845243029 ) ) ;
#190997 = ORIENTED_EDGE ( 'NONE', *, *, #20775, .F. ) ;
#190996 = DIRECTION ( 'NONE',  ( 1.000000000000000000, -0.000000000000000000, -0.000000000000000000 ) ) ;
#190999 = AXIS2_PLACEMENT_3D ( 'NONE', #65384, #144903, #224451 ) ;
#190998 = DIRECTION ( 'NONE',  ( 1.000000000000000000, 0.000000000000000000, 0.000000000000000000 ) ) ;
#191000 = FACE_OUTER_BOUND ( 'NONE', #98088, .T. ) ;
#191001 = CARTESIAN_POINT ( 'NONE',  ( 23.15000000000000213, 69.25640205380743453, -247.7135141964517402 ) ) ;
#191003 = LINE ( 'NONE', #86711, #82625 ) ;
#191002 = DIRECTION ( 'NONE',  ( 1.000000000000000000, 0.000000000000000000, 0.000000000000000000 ) ) ;
#191004 = DIRECTION ( 'NONE',  ( 1.000000000000000000, -0.000000000000000000, -0.000000000000000000 ) ) ;
#191005 = EDGE_CURVE ( 'NONE', #254127, #131694, #209064, .T. ) ;
#191006 = CIRCLE ( 'NONE', #165876, 12.87499999999999822 ) ;
#191007 = CARTESIAN_POINT ( 'NONE',  ( -20.94999999999999929, 11.65000000001115232, -167.5000000000000284 ) ) ;
#191008 = CARTESIAN_POINT ( 'NONE',  ( -23.15000000000000213, 76.00000000001244871, -170.0231074845243597 ) ) ;
#191009 = ORIENTED_EDGE ( 'NONE', *, *, #98244, .F. ) ;
#191010 = CIRCLE ( 'NONE', #207756, 1.749999999999998002 ) ;
#191011 = VECTOR ( 'NONE', #56382, 1000.000000000000000 ) ;
#191012 = AXIS2_PLACEMENT_3D ( 'NONE', #6596, #126554, #106973 ) ;
#191013 = AXIS2_PLACEMENT_3D ( 'NONE', #166123, #8312, #46125 ) ;
#191014 =( BOUNDED_SURFACE ( )  B_SPLINE_SURFACE ( 3, 2, ( 
 ( #256641, #157646, #139297 ),
 ( #78053, #199307, #220153 ),
 ( #95055, #174654, #41529 ),
 ( #237141, #194183, #155068 ),
 ( #135455, #75522, #15553 ),
 ( #218841, #58474, #40251 ) ),
 .UNSPECIFIED., .F., .F., .F. ) 
 B_SPLINE_SURFACE_WITH_KNOTS ( ( 4, 2, 4 ),
 ( 3, 3 ),
 ( 6.719893378901192380E-05, 0.0002757154632485820170, 0.0004842319927081520695 ),
 ( 0.000000000000000000, 1.000000000000000000 ),
 .UNSPECIFIED. ) 
 GEOMETRIC_REPRESENTATION_ITEM ( )  RATIONAL_B_SPLINE_SURFACE ( (
 ( 1.000000000000000000, 0.7250110520819756932, 1.000000000000000000),
 ( 1.000000000000000000, 0.7277932058358560496, 1.000000000000000000),
 ( 1.000000000000000000, 0.7278452872618367264, 1.000000000000000000),
 ( 1.000000000000000000, 0.7221445671548437639, 1.000000000000000000),
 ( 1.000000000000000000, 0.7163662143779749858, 1.000000000000000000),
 ( 1.000000000000000000, 0.7071067811865475727, 1.000000000000000000) ) ) 
 REPRESENTATION_ITEM ( '' )  SURFACE ( )  );
#191015 = VERTEX_POINT ( 'NONE', #189511 ) ;
#191016 = AXIS2_PLACEMENT_3D ( 'NONE', #204108, #85413, #2047 ) ;
#191017 = CYLINDRICAL_SURFACE ( 'NONE', #152701, 0.09999999999999881206 ) ;
#191018 = DIRECTION ( 'NONE',  ( 0.000000000000000000, 0.000000000000000000, 1.000000000000000000 ) ) ;
#191019 = EDGE_LOOP ( 'NONE', ( #10723, #71800, #130097, #177915 ) ) ;
#191020 =( NAMED_UNIT ( * ) PLANE_ANGLE_UNIT ( ) SI_UNIT ( $, .RADIAN. ) );
#191021 = DIRECTION ( 'NONE',  ( 0.000000000000000000, -0.9371753822965326330, 0.3488585713686107592 ) ) ;
#191022 = CARTESIAN_POINT ( 'NONE',  ( 20.93302460841142931, 10.31565961587945424, -206.5364194119177625 ) ) ;
#191023 = PRODUCT_DEFINITION_SHAPE ( 'NONE', 'NONE',  #198277 ) ;
#191024 = EDGE_CURVE ( 'NONE', #129272, #206025, #164806, .T. ) ;
#191025 = DIRECTION ( 'NONE',  ( 0.000000000000000000, 0.000000000000000000, -1.000000000000000000 ) ) ;
#191026 = VERTEX_POINT ( 'NONE', #70870 ) ;
#191027 = AXIS2_PLACEMENT_3D ( 'NONE', #132559, #54284, #212104 ) ;
#191028 = VECTOR ( 'NONE', #136903, 1000.000000000000000 ) ;
#191029 = ORIENTED_EDGE ( 'NONE', *, *, #216083, .F. ) ;
#191030 = CARTESIAN_POINT ( 'NONE',  ( 21.06490991615909536, 60.07466569438444992, -221.2696263483812515 ) ) ;
#191031 = VERTEX_POINT ( 'NONE', #244324 ) ;
#191032 = EDGE_CURVE ( 'NONE', #257480, #142373, #236759, .T. ) ;
#191033 = DIRECTION ( 'NONE',  ( 1.000000000000000000, 0.000000000000000000, 0.000000000000000000 ) ) ;
#191035 = ORIENTED_EDGE ( 'NONE', *, *, #66914, .F. ) ;
#191034 = FACE_OUTER_BOUND ( 'NONE', #15894, .T. ) ;
#191036 = CARTESIAN_POINT ( 'NONE',  ( 23.24999999999999289, 11.65000000001116298, -155.7499999999999716 ) ) ;
#191038 = ORIENTED_EDGE ( 'NONE', *, *, #224199, .T. ) ;
#191037 = FACE_OUTER_BOUND ( 'NONE', #86773, .T. ) ;
#191039 = VECTOR ( 'NONE', #160923, 1000.000000000000000 ) ;
#191041 = ADVANCED_FACE ( 'NONE', ( #128251 ), #47401, .T. ) ;
#191040 = CARTESIAN_POINT ( 'NONE',  ( -18.50000000000000000, 10.29270135741298375, -72.45736188715194714 ) ) ;
#191042 = CARTESIAN_POINT ( 'NONE',  ( 20.87155475150661132, 64.25000000001219291, -143.4275209553667878 ) ) ;
#191043 = DIRECTION ( 'NONE',  ( 0.000000000000000000, 0.3488585713686311318, 0.9371753822965249725 ) ) ;
#191044 = CARTESIAN_POINT ( 'NONE',  ( -18.59999999999999787, -26.43935341558978891, -51.64150860750746119 ) ) ;
#191046 = CARTESIAN_POINT ( 'NONE',  ( 21.08804582317324616, 8.878166167103060502, -179.8499998294057036 ) ) ;
#191045 = DIRECTION ( 'NONE',  ( 0.000000000000000000, 0.000000000000000000, 1.000000000000000000 ) ) ;
#191048 = ADVANCED_FACE ( 'NONE', ( #246892 ), #188217, .T. ) ;
#191047 = CARTESIAN_POINT ( 'NONE',  ( -16.87683809663752399, 9.950000000011142376, -46.15000000000000568 ) ) ;
#191049 = AXIS2_PLACEMENT_3D ( 'NONE', #245011, #3839, #225428 ) ;
#191050 = CARTESIAN_POINT ( 'NONE',  ( -18.37151313414632625, 85.57101412579078215, -163.2064445752853601 ) ) ;
#191051 = CARTESIAN_POINT ( 'NONE',  ( 21.05000000000000071, 1.371218861927975929, -230.7619483865794621 ) ) ;
#191052 = CARTESIAN_POINT ( 'NONE',  ( -20.54999999999999716, 7.250000000011155521, -112.7500000000000284 ) ) ;
#191054 = VERTEX_POINT ( 'NONE', #68274 ) ;
#191053 = VECTOR ( 'NONE', #32624, 1000.000000000000227 ) ;
#191055 = ADVANCED_FACE ( 'NONE', ( #207810 ), #149317, .T. ) ;
#191056 = DIRECTION ( 'NONE',  ( 0.000000000000000000, -0.4088369013363280513, 0.9126074666063771490 ) ) ;
#191058 = EDGE_CURVE ( 'NONE', #200852, #206061, #215904, .T. ) ;
#191057 = ADVANCED_FACE ( 'NONE', ( #238777 ), #176254, .T. ) ;
#191059 = ORIENTED_EDGE ( 'NONE', *, *, #62025, .F. ) ;
#191060 = DIRECTION ( 'NONE',  ( 1.000000000000000000, 0.000000000000000000, 0.000000000000000000 ) ) ;
#191061 = EDGE_LOOP ( 'NONE', ( #199174, #158028, #223460, #135440 ) ) ;
#191062 = CARTESIAN_POINT ( 'NONE',  ( 20.94999999999999574, 14.00000000001115730, -139.4270925303825663 ) ) ;
#191063 = AXIS2_PLACEMENT_3D ( 'NONE', #143305, #241149, #239856 ) ;
#191064 = CIRCLE ( 'NONE', #132801, 0.09999999999999939493 ) ;
#191065 = ORIENTED_EDGE ( 'NONE', *, *, #187435, .T. ) ;
#191066 = CARTESIAN_POINT ( 'NONE',  ( -21.07928932188134041, 30.84304088367083452, -252.0482413927653340 ) ) ;
#191067 = ORIENTED_EDGE ( 'NONE', *, *, #171634, .F. ) ;
#191068 = EDGE_CURVE ( 'NONE', #197139, #125446, #78558, .T. ) ;
#191069 = EDGE_CURVE ( 'NONE', #64897, #144682, #124361, .T. ) ;
#191070 = VERTEX_POINT ( 'NONE', #120149 ) ;
#191071 = CARTESIAN_POINT ( 'NONE',  ( 18.59999999999996945, 68.97833521811131163, -32.18954208262707795 ) ) ;
#191072 = DIRECTION ( 'NONE',  ( 0.000000000000000000, 0.9875055080513743810, -0.1575844902526802316 ) ) ;
#191073 = DIRECTION ( 'NONE',  ( 1.000000000000000000, -7.304098846218134667E-16, -0.000000000000000000 ) ) ;
#191074 = DIRECTION ( 'NONE',  ( 0.000000000000000000, -0.8774096236503307056, 0.4797419643160112934 ) ) ;
#191075 = CARTESIAN_POINT ( 'NONE',  ( -20.85000000000000142, 11.74999999999999645, -26.71613433702190576 ) ) ;
#191076 = EDGE_CURVE ( 'NONE', #58719, #69026, #136945, .T. ) ;
#191078 = CARTESIAN_POINT ( 'NONE',  ( 18.49999999999999645, 0.000000000000000000, 0.000000000000000000 ) ) ;
#191077 = DIRECTION ( 'NONE',  ( -0.000000000000000000, -6.982962677686266711E-15, 1.000000000000000000 ) ) ;
#191079 = CARTESIAN_POINT ( 'NONE',  ( -12.25000000000000178, 9.350000000011139178, -83.75000000000004263 ) ) ;
#191081 = ORIENTED_EDGE ( 'NONE', *, *, #43092, .F. ) ;
#191080 = DIRECTION ( 'NONE',  ( 0.000000000000000000, -0.4999999999999348299, 0.8660254037844762331 ) ) ;
#191083 = DIRECTION ( 'NONE',  ( -2.578261006436899437E-14, 0.1290532225515364784, 0.9916376685811524316 ) ) ;
#191082 = CARTESIAN_POINT ( 'NONE',  ( -18.40000000000000213, 64.52683809664932824, -82.13168612828711446 ) ) ;
#191084 = DIRECTION ( 'NONE',  ( 0.000000000000000000, 0.000000000000000000, -1.000000000000000000 ) ) ;
#191085 =( BOUNDED_SURFACE ( )  B_SPLINE_SURFACE ( 3, 2, ( 
 ( #131943, #211488, #112395 ),
 ( #191955, #92807, #244832 ),
 ( #241001, #205704, #45359 ),
 ( #24538, #44079, #225254 ) ),
 .UNSPECIFIED., .F., .F., .F. ) 
 B_SPLINE_SURFACE_WITH_KNOTS ( ( 4, 4 ),
 ( 3, 3 ),
 ( -5.692061405548898279E-19, 0.0003124336117481333599 ),
 ( 0.000000000000000000, 1.000000000000000000 ),
 .UNSPECIFIED. ) 
 GEOMETRIC_REPRESENTATION_ITEM ( )  RATIONAL_B_SPLINE_SURFACE ( (
 ( 1.000000000000000000, 0.7040654476015839602, 1.000000000000000000),
 ( 1.000000000000000000, 0.7039193538781748360, 1.000000000000000000),
 ( 1.000000000000000000, 0.7089171279145581872, 1.000000000000000000),
 ( 1.000000000000000000, 0.7071067811865509034, 1.000000000000000000) ) ) 
 REPRESENTATION_ITEM ( '' )  SURFACE ( )  );
#191086 = ORIENTED_EDGE ( 'NONE', *, *, #58551, .T. ) ;
#191087 = CARTESIAN_POINT ( 'NONE',  ( -18.49346865148320518, -9.443073798513781369, -174.6851962553152759 ) ) ;
#191088 = AXIS2_PLACEMENT_3D ( 'NONE', #217438, #41416, #220032 ) ;
#191089 = CARTESIAN_POINT ( 'NONE',  ( -22.50000000000000000, 76.00000000001217870, -142.7731074845243029 ) ) ;
#191090 = DIRECTION ( 'NONE',  ( 2.715809747126117987E-16, 1.000000000000000000, 8.690591190803577558E-15 ) ) ;
#191091 = ORIENTED_EDGE ( 'NONE', *, *, #164870, .F. ) ;
#191092 = ADVANCED_FACE ( 'NONE', ( #77123 ), #18437, .T. ) ;
#191093 = DIRECTION ( 'NONE',  ( 0.000000000000000000, 0.2605042016806715099, 0.9654727137038706664 ) ) ;
#191094 = EDGE_CURVE ( 'NONE', #111692, #150875, #111903, .T. ) ;
#191095 = DIRECTION ( 'NONE',  ( 1.000000000000000000, 0.000000000000000000, -0.000000000000000000 ) ) ;
#191096 = LINE ( 'NONE', #13711, #201019 ) ;
#191097 = ORIENTED_EDGE ( 'NONE', *, *, #219956, .T. ) ;
#191098 = ORIENTED_EDGE ( 'NONE', *, *, #113222, .T. ) ;
#191099 = DIRECTION ( 'NONE',  ( 0.000000000000000000, -0.8814952561688438326, 0.4721928772777334582 ) ) ;
#191100 = FACE_OUTER_BOUND ( 'NONE', #99935, .T. ) ;
#191102 = ADVANCED_FACE ( 'NONE', ( #17175 ), #97944, .T. ) ;
#191101 = LINE ( 'NONE', #210639, #42741 ) ;
#191103 = ORIENTED_EDGE ( 'NONE', *, *, #235202, .F. ) ;
#191104 = DIRECTION ( 'NONE',  ( 0.000000000000000000, 0.9126074666063771490, 0.4088369013363281623 ) ) ;
#191105 = CARTESIAN_POINT ( 'NONE',  ( -18.59999999999999787, 16.53615870702968138, -240.8540256063542984 ) ) ;
#191107 = EDGE_CURVE ( 'NONE', #234494, #221530, #145000, .T. ) ;
#191106 = CARTESIAN_POINT ( 'NONE',  ( -18.40000000000000213, 15.50909414388701890, -218.9610367925635330 ) ) ;
#191108 = CIRCLE ( 'NONE', #224397, 0.09999999999999939493 ) ;
#191109 = CARTESIAN_POINT ( 'NONE',  ( 21.05000000000000071, 71.14953271029261828, -148.5573748935260880 ) ) ;
#191110 = CIRCLE ( 'NONE', #174575, 0.09999999999999817368 ) ;
#191111 = CIRCLE ( 'NONE', #132839, 11.75000000000000000 ) ;
#191112 = ORIENTED_EDGE ( 'NONE', *, *, #210694, .T. ) ;
#191113 = CARTESIAN_POINT ( 'NONE',  ( -23.15000000000000213, 73.50000000001199396, -116.2477294072864140 ) ) ;
#191114 =( BOUNDED_SURFACE ( )  B_SPLINE_SURFACE ( 3, 2, ( 
 ( #75231, #70097, #30976 ),
 ( #174354, #213414, #188727 ),
 ( #192586, #251256, #72659 ),
 ( #110472, #152202, #231725 ) ),
 .UNSPECIFIED., .F., .F., .F. ) 
 B_SPLINE_SURFACE_WITH_KNOTS ( ( 4, 4 ),
 ( 3, 3 ),
 ( 0.04058434257139474644, 0.04256401539001599538 ),
 ( 0.000000000000000000, 1.000000000000000000 ),
 .UNSPECIFIED. ) 
 GEOMETRIC_REPRESENTATION_ITEM ( )  RATIONAL_B_SPLINE_SURFACE ( (
 ( 1.000000000000000000, 0.7103081912007761511, 1.000000000000000000),
 ( 1.000000000000000000, 0.7104998333555769818, 1.000000000000000000),
 ( 1.000000000000000000, 0.7107238315754760283, 1.000000000000000000),
 ( 1.000000000000000000, 0.7110073749539387311, 1.000000000000000000) ) ) 
 REPRESENTATION_ITEM ( '' )  SURFACE ( )  );
#191116 = ORIENTED_EDGE ( 'NONE', *, *, #109131, .F. ) ;
#191115 = CARTESIAN_POINT ( 'NONE',  ( -16.93658211146644987, 66.00589133767060446, -82.11881241456870839 ) ) ;
#191117 = CIRCLE ( 'NONE', #20230, 0.09999999999999938105 ) ;
#191118 = FACE_OUTER_BOUND ( 'NONE', #253288, .T. ) ;
#191119 = CARTESIAN_POINT ( 'NONE',  ( 22.50000000000000000, 31.80488924422933295, -238.9605610896540213 ) ) ;
#191120 = CARTESIAN_POINT ( 'NONE',  ( -18.59999999999999787, 11.74999999999999645, -7.014805770653998351 ) ) ;
#191121 = FACE_OUTER_BOUND ( 'NONE', #27472, .T. ) ;
#191122 = ADVANCED_FACE ( 'NONE', ( #118844 ), #95406, .T. ) ;
#191123 = DIRECTION ( 'NONE',  ( -1.000000000000000000, 0.000000000000000000, -0.000000000000000000 ) ) ;
#191124 = ORIENTED_EDGE ( 'NONE', *, *, #254682, .F. ) ;
#191125 = CARTESIAN_POINT ( 'NONE',  ( 21.04105312098496583, 8.875332623043611591, -12.32850674721203355 ) ) ;
#191126 = DIRECTION ( 'NONE',  ( 0.000000000000000000, -0.8660254037844377084, -0.5000000000000016653 ) ) ;
#191127 = CARTESIAN_POINT ( 'NONE',  ( 21.00000000000000000, 51.97441255244040548, -232.0063394385699667 ) ) ;
#191128 = ORIENTED_EDGE ( 'NONE', *, *, #82631, .T. ) ;
#191129 = CARTESIAN_POINT ( 'NONE',  ( -23.25000000000000000, 85.60000000001208775, -126.6291383618717816 ) ) ;
#191130 = CARTESIAN_POINT ( 'NONE',  ( -21.05000000000000071, 7.128833340094563376, -233.7327013124401276 ) ) ;
#191131 = DIRECTION ( 'NONE',  ( 0.000000000000000000, 6.982962677686266711E-15, -1.000000000000000000 ) ) ;
#191132 = CIRCLE ( 'NONE', #224409, 0.1000000000000094008 ) ;
#191133 = AXIS2_PLACEMENT_3D ( 'NONE', #108291, #88688, #168304 ) ;
#191134 = CARTESIAN_POINT ( 'NONE',  ( -16.86578989773640558, 51.70927543259747949, -231.8678220941709753 ) ) ;
#191135 = CIRCLE ( 'NONE', #211970, 0.3999999999999926392 ) ;
#191136 = CARTESIAN_POINT ( 'NONE',  ( 21.07954763557432543, 6.329290990048807686, -167.4341240813815546 ) ) ;
#191137 = CARTESIAN_POINT ( 'NONE',  ( -20.94999999999999929, 77.83534155023646406, -124.9679561919612922 ) ) ;
#191138 = CIRCLE ( 'NONE', #128573, 0.09999999999999938105 ) ;
#191139 = ORIENTED_EDGE ( 'NONE', *, *, #229229, .F. ) ;
#191140 = ORIENTED_EDGE ( 'NONE', *, *, #195401, .F. ) ;
#191141 = CARTESIAN_POINT ( 'NONE',  ( 20.94999999999999929, 70.50000000001151079, -48.42837350343745584 ) ) ;
#191142 = DIRECTION ( 'NONE',  ( -1.000000000000000000, 0.000000000000000000, 0.000000000000000000 ) ) ;
#191143 = CARTESIAN_POINT ( 'NONE',  ( -21.05000000000000071, 38.12692959845505669, -236.1422783512203125 ) ) ;
#191144 = DIRECTION ( 'NONE',  ( 0.000000000000000000, -0.2617529984165031243, -0.9651348961777157509 ) ) ;
#191145 = DIRECTION ( 'NONE',  ( -0.000000000000000000, -0.000000000000000000, 1.000000000000000000 ) ) ;
#191146 = DIRECTION ( 'NONE',  ( 0.000000000000000000, 0.2128009952263603677, -0.9770955615653313941 ) ) ;
#191147 = LINE ( 'NONE', #72477, #207872 ) ;
#191148 = AXIS2_PLACEMENT_3D ( 'NONE', #256652, #140604, #79336 ) ;
#191150 = DIRECTION ( 'NONE',  ( 0.000000000000000000, -0.000000000000000000, 1.000000000000000000 ) ) ;
#191149 = CIRCLE ( 'NONE', #20462, 2.000000000000001776 ) ;
#191151 = ORIENTED_EDGE ( 'NONE', *, *, #112439, .F. ) ;
#191152 = DIRECTION ( 'NONE',  ( -0.000000000000000000, -0.000000000000000000, -1.000000000000000000 ) ) ;
#191153 = VERTEX_POINT ( 'NONE', #79675 ) ;
#191154 = CARTESIAN_POINT ( 'NONE',  ( 21.05000000000000071, 61.88149656937974896, -248.1136133839584090 ) ) ;
#191155 = CARTESIAN_POINT ( 'NONE',  ( -20.94999999999999929, 77.16412189325360771, -162.3082593989527425 ) ) ;
#191156 = AXIS2_PLACEMENT_3D ( 'NONE', #26502, #183008, #42205 ) ;
#191157 = DIRECTION ( 'NONE',  ( 0.000000000000000000, -1.000000000000000000, -6.352154140967427193E-15 ) ) ;
#191158 = DIRECTION ( 'NONE',  ( -1.000000000000000000, 1.809991526360996944E-16, -4.908854824437060108E-17 ) ) ;
#191159 = CARTESIAN_POINT ( 'NONE',  ( 21.05281448260627641, 22.00373637783006586, -231.7449573266841583 ) ) ;
#191160 = CARTESIAN_POINT ( 'NONE',  ( 18.33996824403518744, 85.56963985944304341, -62.70404184700760908 ) ) ;
#191161 = FACE_OUTER_BOUND ( 'NONE', #64887, .T. ) ;
#191162 = EDGE_LOOP ( 'NONE', ( #145819, #81886, #131389, #209457, #212051 ) ) ;
#191163 = CARTESIAN_POINT ( 'NONE',  ( -18.50000000000000000, 64.35000000001187459, -90.77310748452440237 ) ) ;
#191164 = CARTESIAN_POINT ( 'NONE',  ( -21.05000000000000071, 5.850000000011108092, -77.13249722427801203 ) ) ;
#191165 = ADVANCED_FACE ( 'NONE', ( #199668 ), #236195, .F. ) ;
#191166 = CARTESIAN_POINT ( 'NONE',  ( -23.15000000000000213, 64.35000000001195986, -103.0231074845244024 ) ) ;
#191167 = FACE_OUTER_BOUND ( 'NONE', #116, .T. ) ;
#191168 = AXIS2_PLACEMENT_3D ( 'NONE', #153132, #113951, #232648 ) ;
#191169 = AXIS2_PLACEMENT_3D ( 'NONE', #50874, #107009, #125315 ) ;
#191170 = AXIS2_PLACEMENT_3D ( 'NONE', #152993, #134646, #90402 ) ;
#191171 = DIRECTION ( 'NONE',  ( -1.020425574104004196E-15, -6.982962677686266711E-15, 1.000000000000000000 ) ) ;
#191172 = CIRCLE ( 'NONE', #145344, 0.09999999999999961697 ) ;
#191173 = ORIENTED_EDGE ( 'NONE', *, *, #109595, .F. ) ;
#191174 = DIRECTION ( 'NONE',  ( 0.000000000000000000, -0.000000000000000000, 1.000000000000000000 ) ) ;
#191175 = DIRECTION ( 'NONE',  ( -0.000000000000000000, 0.7106264324241465813, -0.7035695228903323661 ) ) ;
#191176 = VERTEX_POINT ( 'NONE', #21033 ) ;
#191177 = VERTEX_POINT ( 'NONE', #78400 ) ;
#191178 = CARTESIAN_POINT ( 'NONE',  ( 22.59999999999999432, 55.86495732666938352, -232.8769840133977880 ) ) ;
#191179 = CARTESIAN_POINT ( 'NONE',  ( 18.47688499308725696, -9.464855950272974994, -174.2013477531374406 ) ) ;
#191180 = AXIS2_PLACEMENT_3D ( 'NONE', #203561, #144856, #243964 ) ;
#191181 = TOROIDAL_SURFACE ( 'NONE', #249438, 11.65000000000000036, 0.1000000000000000056 ) ;
#191182 = EDGE_CURVE ( 'NONE', #233025, #246137, #216106, .T. ) ;
#191183 = EDGE_CURVE ( 'NONE', #94854, #241978, #153634, .T. ) ;
#191184 = VERTEX_POINT ( 'NONE', #180097 ) ;
#191185 = DIRECTION ( 'NONE',  ( 1.000000000000000000, 0.000000000000000000, 0.000000000000000000 ) ) ;
#191186 = CARTESIAN_POINT ( 'NONE',  ( 21.05000000000000071, 1.115600667400684642E-11, -68.90000000000000568 ) ) ;
#191187 = CIRCLE ( 'NONE', #78714, 11.74999999999999645 ) ;
#191188 = ORIENTED_EDGE ( 'NONE', *, *, #164320, .F. ) ;
#191189 = AXIS2_PLACEMENT_3D ( 'NONE', #70160, #51825, #229217 ) ;
#191190 = TOROIDAL_SURFACE ( 'NONE', #157911, 4.099999999999999645, 0.1000000000000000056 ) ;
#191191 = AXIS2_PLACEMENT_3D ( 'NONE', #140662, #123681, #39018 ) ;
#191192 = CIRCLE ( 'NONE', #78721, 4.100000000000006750 ) ;
#191193 = CARTESIAN_POINT ( 'NONE',  ( 23.04999999999999716, 8.822561741677553471, -143.2500000000000284 ) ) ;
#191194 = EDGE_CURVE ( 'NONE', #115941, #118873, #1427, .T. ) ;
#191195 = ORIENTED_EDGE ( 'NONE', *, *, #76956, .T. ) ;
#191196 = EDGE_CURVE ( 'NONE', #18698, #178738, #224487, .T. ) ;
#191197 = FACE_OUTER_BOUND ( 'NONE', #76852, .T. ) ;
#191198 = AXIS2_PLACEMENT_3D ( 'NONE', #208952, #227225, #72024 ) ;
#191199 = FACE_OUTER_BOUND ( 'NONE', #204282, .T. ) ;
#191201 = EDGE_LOOP ( 'NONE', ( #253960, #84712, #23520, #193264 ) ) ;
#191200 = PLANE ( 'NONE',  #170893 ) ;
#191202 = CARTESIAN_POINT ( 'NONE',  ( 22.59999999999999432, 0.1000000000111554016, -88.85042919245522341 ) ) ;
#191203 = UNCERTAINTY_MEASURE_WITH_UNIT (LENGTH_MEASURE( 1.000000000000000082E-05 ), #133583, 'distance_accuracy_value', 'NONE');
#191204 = EDGE_CURVE ( 'NONE', #206620, #169705, #200931, .T. ) ;
#191205 = DIRECTION ( 'NONE',  ( 0.8049926720990050466, -0.5725998182664976399, 0.1552940629517993720 ) ) ;
#191206 = DIRECTION ( 'NONE',  ( -0.000000000000000000, -0.1298341882520022694, -0.9915357197604853789 ) ) ;
#191207 = CARTESIAN_POINT ( 'NONE',  ( -16.77779411503079388, 66.05389855308847302, -190.8600500669045914 ) ) ;
#191208 = DIRECTION ( 'NONE',  ( -1.000000000000000000, 0.000000000000000000, 0.000000000000000000 ) ) ;
#191209 = FACE_OUTER_BOUND ( 'NONE', #28853, .T. ) ;
#191211 = EDGE_LOOP ( 'NONE', ( #113715, #209865, #207087 ) ) ;
#191210 = CARTESIAN_POINT ( 'NONE',  ( -23.49999999999994316, 82.78482233730476025, -26.42994920107286916 ) ) ;
#191212 = VERTEX_POINT ( 'NONE', #82226 ) ;
#191214 = CARTESIAN_POINT ( 'NONE',  ( -12.92414019175886253, 9.417632963117446465, -85.14894846573231746 ) ) ;
#191213 = DIRECTION ( 'NONE',  ( 0.000000000000000000, 0.000000000000000000, -1.000000000000000000 ) ) ;
#191215 = EDGE_CURVE ( 'NONE', #135831, #21528, #103656, .T. ) ;
#191217 = ORIENTED_EDGE ( 'NONE', *, *, #37678, .T. ) ;
#191216 = DIRECTION ( 'NONE',  ( 1.000000000000000000, 0.000000000000000000, 0.000000000000000000 ) ) ;
#191218 = ADVANCED_BREP_SHAPE_REPRESENTATION ( '', ( #20981, #2425 ), #135129 ) ;
#191219 = ORIENTED_EDGE ( 'NONE', *, *, #199219, .T. ) ;
#191220 = CARTESIAN_POINT ( 'NONE',  ( 20.95512820512820440, 10.62384868372303615, -175.1649135690875880 ) ) ;
#191221 = STYLED_ITEM ( 'NONE', ( #39116 ), #110136 ) ;
#191222 = LINE ( 'NONE', #127369, #43049 ) ;
#191223 = ADVANCED_FACE ( 'NONE', ( #143514 ), #141121, .T. ) ;
#191224 = LINE ( 'NONE', #170400, #50933 ) ;
#191225 = CARTESIAN_POINT ( 'NONE',  ( 19.87657994472040457, 11.75000000001104716, -58.26578812462643242 ) ) ;
#191226 = FACE_OUTER_BOUND ( 'NONE', #39950, .T. ) ;
#191227 = DIRECTION ( 'NONE',  ( 0.000000000000000000, 1.000000000000000000, 0.000000000000000000 ) ) ;
#191228 = AXIS2_PLACEMENT_3D ( 'NONE', #172203, #251684, #15674 ) ;
#191229 = AXIS2_PLACEMENT_3D ( 'NONE', #71601, #91139, #212389 ) ;
#191230 = EDGE_CURVE ( 'NONE', #27940, #136731, #202218, .T. ) ;
#191231 = EDGE_LOOP ( 'NONE', ( #130031, #246165, #171326, #135434 ) ) ;
#191232 = ORIENTED_EDGE ( 'NONE', *, *, #21670, .T. ) ;
#191233 = PLANE ( 'NONE',  #31500 ) ;
#191234 = AXIS2_PLACEMENT_3D ( 'NONE', #194048, #55757, #216141 ) ;
#191235 = MANIFOLD_SOLID_BREP ( 'Stock-MAS-200-1', #190867 ) ;
#191236 = ORIENTED_EDGE ( 'NONE', *, *, #196385, .T. ) ;
#191237 = CYLINDRICAL_SURFACE ( 'NONE', #63536, 0.09999999999999939493 ) ;
#191238 = VERTEX_POINT ( 'NONE', #67835 ) ;
#191239 = CARTESIAN_POINT ( 'NONE',  ( -20.94999999999999929, 1.360870587203197646, -175.5729979270909382 ) ) ;
#191240 = CIRCLE ( 'NONE', #141156, 0.09999999999999939493 ) ;
#191241 = CARTESIAN_POINT ( 'NONE',  ( -18.50000000000000000, 64.35000000001230092, -157.7731074845244450 ) ) ;
#191242 = CARTESIAN_POINT ( 'NONE',  ( 18.58143601961878844, 65.56427058491688342, -44.77310748452440237 ) ) ;
#191243 = ORIENTED_EDGE ( 'NONE', *, *, #192964, .T. ) ;
#191244 = ORIENTED_EDGE ( 'NONE', *, *, #46253, .F. ) ;
#191245 = AXIS2_PLACEMENT_3D ( 'NONE', #12813, #67623, #28554 ) ;
#191246 = DIRECTION ( 'NONE',  ( 0.000000000000000000, -0.2617529984165031243, -0.9651348961777157509 ) ) ;
#191247 = DIRECTION ( 'NONE',  ( 0.000000000000000000, 0.9126074666063660468, 0.4088369013363524762 ) ) ;
#191248 = AXIS2_PLACEMENT_3D ( 'NONE', #174967, #255683, #195788 ) ;
#191249 = ORIENTED_EDGE ( 'NONE', *, *, #132643, .T. ) ;
#191250 = DIRECTION ( 'NONE',  ( -1.000000000000000000, 0.000000000000000000, 0.000000000000000000 ) ) ;
#191251 = ORIENTED_EDGE ( 'NONE', *, *, #105244, .T. ) ;
#191254 = ORIENTED_EDGE ( 'NONE', *, *, #33763, .F. ) ;
#191253 = CARTESIAN_POINT ( 'NONE',  ( -17.22361732159831504, 10.34515565860243314, -22.12921547413287371 ) ) ;
#191252 = DIRECTION ( 'NONE',  ( 1.000000000000000000, -0.000000000000000000, -0.000000000000000000 ) ) ;
#191255 = CARTESIAN_POINT ( 'NONE',  ( -23.15000000000000213, 84.66355140188147743, -160.4990063664569959 ) ) ;
#191256 = VECTOR ( 'NONE', #99449, 1000.000000000000114 ) ;
#191257 = ORIENTED_EDGE ( 'NONE', *, *, #103152, .F. ) ;
#191258 = EDGE_CURVE ( 'NONE', #27940, #79153, #166082, .T. ) ;
#191259 = ORIENTED_EDGE ( 'NONE', *, *, #130271, .T. ) ;
#191260 = EDGE_CURVE ( 'NONE', #67554, #971, #232699, .T. ) ;
#191261 = DIRECTION ( 'NONE',  ( 0.000000000000000000, 0.000000000000000000, -1.000000000000000000 ) ) ;
#191262 = ORIENTED_EDGE ( 'NONE', *, *, #19344, .F. ) ;
#191263 = DIRECTION ( 'NONE',  ( 1.000000000000000000, 0.000000000000000000, 0.000000000000000000 ) ) ;
#191264 = EDGE_CURVE ( 'NONE', #75744, #234336, #61999, .T. ) ;
#191265 = FACE_OUTER_BOUND ( 'NONE', #148973, .T. ) ;
#191266 = ADVANCED_FACE ( 'NONE', ( #105651 ), #5264, .F. ) ;
#191267 = CARTESIAN_POINT ( 'NONE',  ( -22.49436431346200038, 64.35004905235891215, -170.0900110142466986 ) ) ;
#191268 = FACE_OUTER_BOUND ( 'NONE', #195956, .T. ) ;
#191269 = CARTESIAN_POINT ( 'NONE',  ( 18.39999999999999503, 5.650000000011139001, -46.15000000000000568 ) ) ;
#191271 = ORIENTED_EDGE ( 'NONE', *, *, #233119, .T. ) ;
#191270 = EDGE_CURVE ( 'NONE', #115688, #196889, #224339, .T. ) ;
#191272 = CARTESIAN_POINT ( 'NONE',  ( -16.93909480342659890, 44.07255599751472630, -235.2799179410861541 ) ) ;
#191273 = DIRECTION ( 'NONE',  ( 0.000000000000000000, -0.2617529984165031243, -0.9651348961777157509 ) ) ;
#191274 = AXIS2_PLACEMENT_3D ( 'NONE', #106804, #207219, #162963 ) ;
#191275 = CARTESIAN_POINT ( 'NONE',  ( 21.07928932188134397, 6.328516656404459262, -33.40110485434561127 ) ) ;
#191276 = ADVANCED_FACE ( 'NONE', ( #125248 ), #7842, .F. ) ;
#191277 = ORIENTED_EDGE ( 'NONE', *, *, #161259, .F. ) ;
#191278 = FACE_OUTER_BOUND ( 'NONE', #104437, .T. ) ;
#191280 = EDGE_CURVE ( 'NONE', #248650, #217539, #228603, .T. ) ;
#191279 = VERTEX_POINT ( 'NONE', #165677 ) ;
#191281 = CARTESIAN_POINT ( 'NONE',  ( -18.40000000000000213, 51.08739888604760182, -230.5155363996569520 ) ) ;
#191282 = VERTEX_POINT ( 'NONE', #27476 ) ;
#191283 = LINE ( 'NONE', #92147, #239119 ) ;
#191284 = CARTESIAN_POINT ( 'NONE',  ( -22.40000000000000213, 76.00000000001246292, -181.7735403769829645 ) ) ;
#191285 = EDGE_CURVE ( 'NONE', #229697, #816, #41880, .T. ) ;
#191287 = ORIENTED_EDGE ( 'NONE', *, *, #69222, .F. ) ;
#191286 = LINE ( 'NONE', #152157, #173742 ) ;
#191288 = CARTESIAN_POINT ( 'NONE',  ( -22.19999999999999929, -11.65000000000000036, 12.09999999999999609 ) ) ;
#191289 = ORIENTED_EDGE ( 'NONE', *, *, #102713, .F. ) ;
#191290 = DIRECTION ( 'NONE',  ( 1.000000000000000000, 0.000000000000000000, 0.000000000000000000 ) ) ;
#191291 = ADVANCED_FACE ( 'NONE', ( #212500 ), #53629, .T. ) ;
#191292 = LINE ( 'NONE', #53022, #85382 ) ;
#191293 = EDGE_LOOP ( 'NONE', ( #223526, #204123, #236074 ) ) ;
#191294 = TOROIDAL_SURFACE ( 'NONE', #249550, 0.2000000000000000111, 0.1000000000000000056 ) ;
#191296 = CIRCLE ( 'NONE', #91498, 0.1000000000000024342 ) ;
#191295 = DIRECTION ( 'NONE',  ( -0.000000000000000000, -0.000000000000000000, -1.000000000000000000 ) ) ;
#191297 = DIRECTION ( 'NONE',  ( 1.186688945009009831E-16, -0.4721928772777346239, -0.8814952561688430555 ) ) ;
#191299 = ORIENTED_EDGE ( 'NONE', *, *, #209613, .F. ) ;
#191298 = EDGE_CURVE ( 'NONE', #158172, #253517, #199389, .T. ) ;
#191300 = AXIS2_PLACEMENT_3D ( 'NONE', #236984, #119616, #142982 ) ;
#191303 = EDGE_CURVE ( 'NONE', #69236, #248676, #13027, .T. ) ;
#191302 = CARTESIAN_POINT ( 'NONE',  ( 20.94999999999999929, 5.000000000011153745, -121.5947339810869465 ) ) ;
#191301 = CIRCLE ( 'NONE', #187022, 11.75000000000000000 ) ;
#191304 = ORIENTED_EDGE ( 'NONE', *, *, #86413, .T. ) ;
#191305 = EDGE_CURVE ( 'NONE', #210045, #217030, #169551, .T. ) ;
#191306 = CARTESIAN_POINT ( 'NONE',  ( 21.05000000000000071, 74.92681270650359693, -207.4801605588535551 ) ) ;
#191307 = DIRECTION ( 'NONE',  ( -1.000000000000000000, -0.000000000000000000, -0.000000000000000000 ) ) ;
#191308 = EDGE_CURVE ( 'NONE', #112295, #230417, #82789, .T. ) ;
#191309 = EDGE_CURVE ( 'NONE', #206150, #229990, #131661, .T. ) ;
#191312 = ORIENTED_EDGE ( 'NONE', *, *, #208667, .F. ) ;
#191311 = EDGE_LOOP ( 'NONE', ( #108111, #155998, #216283, #179242 ) ) ;
#191310 = CARTESIAN_POINT ( 'NONE',  ( -23.15000000000000213, -8.999999999988844479, -191.6060308773475356 ) ) ;
#191314 = AXIS2_PLACEMENT_3D ( 'NONE', #110450, #87012, #11362 ) ;
#191313 = FACE_OUTER_BOUND ( 'NONE', #55605, .T. ) ;
#191315 = CARTESIAN_POINT ( 'NONE',  ( -22.42253884134832020, 0.001932351146464877023, -155.8503943026515515 ) ) ;
#191316 = CARTESIAN_POINT ( 'NONE',  ( -18.50000000000000000, 43.92448011351754644, -236.0509145372394357 ) ) ;
#191317 = VECTOR ( 'NONE', #242163, 1000.000000000000000 ) ;
#191319 = DIRECTION ( 'NONE',  ( 0.000000000000000000, 0.1332476588733448597, -0.9910827722268067408 ) ) ;
#191318 = CARTESIAN_POINT ( 'NONE',  ( -20.94999999999999929, 77.83585931145498193, -24.51866831572578320 ) ) ;
#191320 = DIRECTION ( 'NONE',  ( 0.000000000000000000, 0.9126074666063660468, 0.4088369013363524762 ) ) ;
#191321 = DIRECTION ( 'NONE',  ( 1.000000000000000000, 0.000000000000000000, 0.000000000000000000 ) ) ;
#191322 = CARTESIAN_POINT ( 'NONE',  ( 20.04142135623730070, 11.65000000001115943, -54.75000000000000000 ) ) ;
#191323 = CARTESIAN_POINT ( 'NONE',  ( -23.15000000000000213, 73.40000000001222702, -149.7477294072864709 ) ) ;
#191324 = TOROIDAL_SURFACE ( 'NONE', #45549, 0.2000000000000000111, 0.1000000000000000056 ) ;
#191325 = ORIENTED_EDGE ( 'NONE', *, *, #41199, .F. ) ;
#191326 = VERTEX_POINT ( 'NONE', #209934 ) ;
#191327 = CARTESIAN_POINT ( 'NONE',  ( 18.59999999999999076, 7.070967871809997973, -137.7465642218683399 ) ) ;
#191329 = ORIENTED_EDGE ( 'NONE', *, *, #178844, .T. ) ;
#191328 = CARTESIAN_POINT ( 'NONE',  ( 20.94999999999999929, 10.38178547073510316, -206.5078453638841438 ) ) ;
#191330 = ORIENTED_EDGE ( 'NONE', *, *, #189856, .T. ) ;
#191331 = CARTESIAN_POINT ( 'NONE',  ( -21.05000000000000071, 76.00000000001165290, -69.52310748452431710 ) ) ;
#191332 = ORIENTED_EDGE ( 'NONE', *, *, #192868, .F. ) ;
#191333 = CYLINDRICAL_SURFACE ( 'NONE', #33747, 0.1000000000000046685 ) ;
#191334 = ORIENTED_EDGE ( 'NONE', *, *, #184046, .F. ) ;
#191335 = CARTESIAN_POINT ( 'NONE',  ( -20.94999999999999929, 1.851028230152016674, -179.1539132694224463 ) ) ;
#191336 = CIRCLE ( 'NONE', #249759, 0.1000000000000106498 ) ;
#191338 = VERTEX_POINT ( 'NONE', #88658 ) ;
#191337 = EDGE_LOOP ( 'NONE', ( #245925, #254685, #140372, #232447 ) ) ;
#191339 = ORIENTED_EDGE ( 'NONE', *, *, #194657, .F. ) ;
#191340 = ORIENTED_EDGE ( 'NONE', *, *, #110290, .T. ) ;
#191341 = ORIENTED_EDGE ( 'NONE', *, *, #233542, .F. ) ;
#191342 = LINE ( 'NONE', #73965, #246929 ) ;
#191343 = CYLINDRICAL_SURFACE ( 'NONE', #24070, 0.09999999999999939493 ) ;
#191344 = B_SPLINE_CURVE_WITH_KNOTS ( 'NONE', 3,
 ( #24813, #5182, #41801, #84707, #65181, #121352, #22230, #61340, #164301, #198275 ),
 .UNSPECIFIED., .F., .F.,
 ( 4, 3, 3, 4 ),
 ( 1.734723475976807094E-18, 0.0002000000000008561227, 0.001000000000082977483, 0.001967863649483316338 ),
 .UNSPECIFIED. ) ;
#191345 = CARTESIAN_POINT ( 'NONE',  ( -14.45422546970483957, 9.450602096099679272, -185.9438959630966792 ) ) ;
#191347 = ORIENTED_EDGE ( 'NONE', *, *, #202665, .T. ) ;
#191346 = CARTESIAN_POINT ( 'NONE',  ( -23.49999999999994316, 83.97335046823651794, -34.66234602115918051 ) ) ;
#191348 = DIRECTION ( 'NONE',  ( 0.000000000000000000, 0.000000000000000000, -1.000000000000000000 ) ) ;
#191349 = CARTESIAN_POINT ( 'NONE',  ( 21.05000000000000071, 12.10919762232931163, -206.2073353557311748 ) ) ;
#191351 = ORIENTED_EDGE ( 'NONE', *, *, #137705, .T. ) ;
#191350 = CARTESIAN_POINT ( 'NONE',  ( -16.94445028196808778, 60.88759175473954599, -221.0718995934454938 ) ) ;
#191352 = DIRECTION ( 'NONE',  ( 0.000000000000000000, 0.2128009952263604232, -0.9770955615653316162 ) ) ;
#191353 = ORIENTED_EDGE ( 'NONE', *, *, #75751, .T. ) ;
#191354 = CARTESIAN_POINT ( 'NONE',  ( 20.94999999999999929, 11.65000000001115943, -127.2161343370219413 ) ) ;
#191355 = VERTEX_POINT ( 'NONE', #251610 ) ;
#191356 = DIRECTION ( 'NONE',  ( 0.000000000000000000, 0.000000000000000000, -1.000000000000000000 ) ) ;
#191358 = ADVANCED_FACE ( 'NONE', ( #49560 ), #157914, .T. ) ;
#191357 = CARTESIAN_POINT ( 'NONE',  ( -16.94107738177414291, 30.32481141862674789, -234.7976376674202186 ) ) ;
#191359 = EDGE_LOOP ( 'NONE', ( #15739, #43822, #195721, #254632 ) ) ;
#191361 = CARTESIAN_POINT ( 'NONE',  ( 21.05000000000000071, 38.42191493408704872, -250.4955484557988541 ) ) ;
#191360 = DIRECTION ( 'NONE',  ( 0.000000000000000000, 0.000000000000000000, 1.000000000000000000 ) ) ;
#191362 = EDGE_CURVE ( 'NONE', #171424, #116117, #66282, .T. ) ;
#191363 = VECTOR ( 'NONE', #191804, 1000.000000000000000 ) ;
#191364 = CARTESIAN_POINT ( 'NONE',  ( 21.05000000000000071, 85.00000000001222134, -146.4170766071767389 ) ) ;
#191365 = DIRECTION ( 'NONE',  ( 0.000000000000000000, -0.000000000000000000, 1.000000000000000000 ) ) ;
#191366 = CARTESIAN_POINT ( 'NONE',  ( -18.59999999999999787, 77.16270174995034381, -162.0231074845243313 ) ) ;
#191367 = ORIENTED_EDGE ( 'NONE', *, *, #174273, .F. ) ;
#191368 = EDGE_LOOP ( 'NONE', ( #143101, #10532, #165062, #59614 ) ) ;
#191369 = EDGE_CURVE ( 'NONE', #214271, #208794, #236769, .T. ) ;
#191370 = CARTESIAN_POINT ( 'NONE',  ( -21.05000000000000071, 0.09779029131994597390, -127.7421853895238968 ) ) ;
#191372 = ADVANCED_FACE ( 'NONE', ( #93809 ), #170847, .T. ) ;
#191371 = CARTESIAN_POINT ( 'NONE',  ( 20.94999999999999929, 82.09643798151613225, -215.4278993322501208 ) ) ;
#191373 = EDGE_LOOP ( 'NONE', ( #175008, #37387, #222761 ) ) ;
#191374 = CARTESIAN_POINT ( 'NONE',  ( -23.25000000000000000, 1.115600667400684642E-11, -71.05000000000003979 ) ) ;
#191375 = ORIENTED_EDGE ( 'NONE', *, *, #75607, .F. ) ;
#191376 = LINE ( 'NONE', #53107, #227398 ) ;
#191377 = LINE ( 'NONE', #17826, #71182 ) ;
#191378 = CIRCLE ( 'NONE', #24785, 0.09999999999998898659 ) ;
#191379 = AXIS2_PLACEMENT_3D ( 'NONE', #218688, #40108, #119626 ) ;
#191380 = DIRECTION ( 'NONE',  ( 0.000000000000000000, 0.000000000000000000, 1.000000000000000000 ) ) ;
#191381 = ORIENTED_EDGE ( 'NONE', *, *, #235639, .T. ) ;
#191382 = CARTESIAN_POINT ( 'NONE',  ( 21.05000000000000071, -3.664072692419559907, -226.4691047342518857 ) ) ;
#191383 = SURFACE_STYLE_USAGE ( .BOTH. , #29745 ) ;
#191384 = VERTEX_POINT ( 'NONE', #191672 ) ;
#191385 = ORIENTED_EDGE ( 'NONE', *, *, #224877, .F. ) ;
#191387 = ADVANCED_FACE ( 'NONE', ( #127821, #28765 ), #71710, .F. ) ;
#191386 = VECTOR ( 'NONE', #76308, 1000.000000000000114 ) ;
#191388 = ORIENTED_EDGE ( 'NONE', *, *, #142096, .F. ) ;
#191389 = CIRCLE ( 'NONE', #78893, 0.09999999999999910349 ) ;
#191390 = DIRECTION ( 'NONE',  ( 0.000000000000000000, 0.8814952561688476074, -0.4721928772777262417 ) ) ;
#191391 = CARTESIAN_POINT ( 'NONE',  ( 14.87567385445976953, 66.56923500458921694, -54.29257008977393184 ) ) ;
#191392 = FACE_OUTER_BOUND ( 'NONE', #215982, .T. ) ;
#191393 = DIRECTION ( 'NONE',  ( 1.000000000000000000, -0.000000000000000000, -0.000000000000000000 ) ) ;
#191394 = CYLINDRICAL_SURFACE ( 'NONE', #171897, 0.1000000000000028644 ) ;
#191395 = AXIS2_PLACEMENT_3D ( 'NONE', #255737, #77140, #257017 ) ;
#191397 = DIRECTION ( 'NONE',  ( 0.000000000000000000, 0.9654727137038715545, 0.2605042016806676242 ) ) ;
#191396 = CARTESIAN_POINT ( 'NONE',  ( -22.00356870141395049, 10.55423491370564726, -227.3381210828049177 ) ) ;
#191399 = VERTEX_POINT ( 'NONE', #189073 ) ;
#191398 = CARTESIAN_POINT ( 'NONE',  ( 18.54999999999999716, 67.25000000001205080, -123.8731074845243683 ) ) ;
#191400 = DIRECTION ( 'NONE',  ( 0.000000000000000000, -0.9910827722268055195, 0.1332476588733540468 ) ) ;
#191401 = EDGE_LOOP ( 'NONE', ( #154125, #11437, #55592, #255661 ) ) ;
#191402 = CARTESIAN_POINT ( 'NONE',  ( -12.60206096961792177, 9.389686005666813884, -149.6728435063513132 ) ) ;
#191403 = ORIENTED_EDGE ( 'NONE', *, *, #169356, .T. ) ;
#191404 = EDGE_LOOP ( 'NONE', ( #197634, #70282, #158284, #190853 ) ) ;
#191405 = CARTESIAN_POINT ( 'NONE',  ( -23.15000000000000213, 1.148907358139439339E-11, -201.0000000000015064 ) ) ;
#191406 = FACE_OUTER_BOUND ( 'NONE', #229434, .T. ) ;
#191407 = DIRECTION ( 'NONE',  ( 0.000000000000000000, 0.2617529984165432588, 0.9651348961777048707 ) ) ;
#191408 = EDGE_CURVE ( 'NONE', #104140, #40848, #12137, .T. ) ;
#191409 = FACE_OUTER_BOUND ( 'NONE', #138075, .T. ) ;
#191410 = EDGE_CURVE ( 'NONE', #33467, #34181, #191192, .T. ) ;
#191411 = AXIS2_PLACEMENT_3D ( 'NONE', #246488, #67850, #6589 ) ;
#191412 = CARTESIAN_POINT ( 'NONE',  ( 20.91682497891423154, 18.39833411442327105, -236.9692678682430085 ) ) ;
#191413 = EDGE_LOOP ( 'NONE', ( #149188, #129680, #178505, #140532 ) ) ;
#191414 = ORIENTED_EDGE ( 'NONE', *, *, #155045, .T. ) ;
#191415 = FACE_OUTER_BOUND ( 'NONE', #142050, .T. ) ;
#191416 = EDGE_LOOP ( 'NONE', ( #96636, #224928, #134840, #148811 ) ) ;
#191417 = PLANE ( 'NONE',  #211090 ) ;
#191418 = DIRECTION ( 'NONE',  ( -1.000000000000000000, -0.000000000000000000, -0.000000000000000000 ) ) ;
#191419 = ORIENTED_EDGE ( 'NONE', *, *, #168294, .F. ) ;
#191420 = CARTESIAN_POINT ( 'NONE',  ( -21.04999999999999716, -9.600000000000001421, -7.032069396699667685 ) ) ;
#191421 = LINE ( 'NONE', #209668, #242058 ) ;
#191422 = FACE_OUTER_BOUND ( 'NONE', #107054, .T. ) ;
#191424 = EDGE_CURVE ( 'NONE', #168071, #137676, #151244, .T. ) ;
#191423 = LINE ( 'NONE', #94845, #180134 ) ;
#191425 = EDGE_LOOP ( 'NONE', ( #85741, #205246, #74540, #149591 ) ) ;
#191426 = FACE_OUTER_BOUND ( 'NONE', #166472, .T. ) ;
#191427 = DIRECTION ( 'NONE',  ( 1.000000000000000000, 0.000000000000000000, 0.000000000000000000 ) ) ;
#191428 = CARTESIAN_POINT ( 'NONE',  ( -21.05000000000000071, -11.65000000000000036, -3.000000000000002665 ) ) ;
#191429 = EDGE_CURVE ( 'NONE', #181753, #61045, #232066, .T. ) ;
#191430 = VECTOR ( 'NONE', #83081, 1000.000000000000000 ) ;
#191431 = LINE ( 'NONE', #12781, #100299 ) ;
#191432 = CARTESIAN_POINT ( 'NONE',  ( -21.04999999999994387, 78.11805852053666399, -49.62915779269638961 ) ) ;
#191433 = VECTOR ( 'NONE', #130722, 1000.000000000000000 ) ;
#191434 = EDGE_CURVE ( 'NONE', #34074, #4792, #178750, .T. ) ;
#191435 = CARTESIAN_POINT ( 'NONE',  ( -16.97683809663752186, 9.850000000011137402, -53.59763598180368405 ) ) ;
#191436 = AXIS2_PLACEMENT_3D ( 'NONE', #10801, #229844, #51173 ) ;
#191437 = EDGE_LOOP ( 'NONE', ( #200386, #46162, #18071, #54265 ) ) ;
#191438 = CARTESIAN_POINT ( 'NONE',  ( 21.05000000000000071, 1.115649653272650466E-11, -63.00000000000000000 ) ) ;
#191439 = ORIENTED_EDGE ( 'NONE', *, *, #8490, .T. ) ;
#191440 = CARTESIAN_POINT ( 'NONE',  ( 14.56326696814971733, 66.55335100938343373, -154.9339441886012310 ) ) ;
#191441 = EDGE_CURVE ( 'NONE', #207618, #200406, #211847, .T. ) ;
#191442 = DIRECTION ( 'NONE',  ( 0.000000000000000000, -1.000000000000000000, 0.000000000000000000 ) ) ;
#191443 = CARTESIAN_POINT ( 'NONE',  ( -18.59999999999999787, -4.963776450181787148, -229.1688993039521449 ) ) ;
#191444 = DIRECTION ( 'NONE',  ( 0.000000000000000000, 0.000000000000000000, -1.000000000000000000 ) ) ;
#191445 = CARTESIAN_POINT ( 'NONE',  ( -23.15000000000000213, -9.500000000000003553, -9.893969122652444881 ) ) ;
#191446 = CARTESIAN_POINT ( 'NONE',  ( -18.39999999999999858, -9.499999999988849808, -174.4992856778388273 ) ) ;
#191447 = AXIS2_PLACEMENT_3D ( 'NONE', #239226, #223501, #3163 ) ;
#191448 = EDGE_LOOP ( 'NONE', ( #4002, #94491, #146550, #86566 ) ) ;
#191449 = DIRECTION ( 'NONE',  ( -1.000000000000000000, -0.000000000000000000, -0.000000000000000000 ) ) ;
#191450 = EDGE_CURVE ( 'NONE', #56792, #147060, #182993, .T. ) ;
#191451 = AXIS2_PLACEMENT_3D ( 'NONE', #141889, #37689, #18093 ) ;
#191452 = LINE ( 'NONE', #33677, #189864 ) ;
#191453 = DIRECTION ( 'NONE',  ( 0.000000000000000000, -0.1350103645451835865, -0.9908441862701605762 ) ) ;
#191454 = DIRECTION ( 'NONE',  ( 0.000000000000000000, 0.01562500000001045344, 0.9998779222360096863 ) ) ;
#191455 = CIRCLE ( 'NONE', #145603, 0.09999999999999993616 ) ;
#191456 = CARTESIAN_POINT ( 'NONE',  ( 18.59999999999999076, 14.51805813080544638, -219.6885945441820809 ) ) ;
#191457 =( BOUNDED_CURVE ( )  B_SPLINE_CURVE ( 3, ( #252314, #13719, #32028, #253598 ),
 .UNSPECIFIED., .F., .T. ) 
 B_SPLINE_CURVE_WITH_KNOTS ( ( 4, 4 ),
 ( 2.589852378279005496, 2.850972632318389710 ),
 .UNSPECIFIED. ) 
 CURVE ( )  GEOMETRIC_REPRESENTATION_ITEM ( )  RATIONAL_B_SPLINE_CURVE ( ( 1.000000000000000000, 0.9943260843901261525, 0.9943260843901261525, 1.000000000000000000 ) ) 
 REPRESENTATION_ITEM ( '' )  );
#191458 = ORIENTED_EDGE ( 'NONE', *, *, #9337, .T. ) ;
#191459 = EDGE_LOOP ( 'NONE', ( #54447, #212650, #182775, #114498 ) ) ;
#191460 = DIRECTION ( 'NONE',  ( 0.000000000000000000, 0.000000000000000000, 1.000000000000000000 ) ) ;
#191461 = LINE ( 'NONE', #151022, #50920 ) ;
#191462 = CARTESIAN_POINT ( 'NONE',  ( 18.39999999999999503, 31.05627573922685514, -233.2203535436961488 ) ) ;
#191463 = CARTESIAN_POINT ( 'NONE',  ( 23.14999999999999503, 21.13195309841794867, -243.6318585593223816 ) ) ;
#191464 = CARTESIAN_POINT ( 'NONE',  ( -20.64999999999999858, 4.350000000011156054, -112.8500000000000369 ) ) ;
#191465 = ORIENTED_EDGE ( 'NONE', *, *, #38925, .T. ) ;
#191466 = DIRECTION ( 'NONE',  ( 0.000000000000000000, 1.000000000000000000, 0.000000000000000000 ) ) ;
#191467 = CARTESIAN_POINT ( 'NONE',  ( 21.05000000000000071, 64.35000000001164722, -69.52310748452440237 ) ) ;
#191468 = ORIENTED_EDGE ( 'NONE', *, *, #177478, .T. ) ;
#191469 = DIRECTION ( 'NONE',  ( 1.000000000000000000, 0.000000000000000000, 0.000000000000000000 ) ) ;
#191470 = CIRCLE ( 'NONE', #229037, 0.1000000000000035444 ) ;
#191471 = ORIENTED_EDGE ( 'NONE', *, *, #21277, .T. ) ;
#191473 = ORIENTED_EDGE ( 'NONE', *, *, #253659, .T. ) ;
#191472 = CARTESIAN_POINT ( 'NONE',  ( -21.55000000000000071, 68.65000000001222702, -148.8731074845244109 ) ) ;
#191474 = ORIENTED_EDGE ( 'NONE', *, *, #112734, .T. ) ;
#191475 = CARTESIAN_POINT ( 'NONE',  ( 20.94999999999999929, 78.17003882911672008, -228.8770135013149911 ) ) ;
#191476 = CYLINDRICAL_SURFACE ( 'NONE', #183975, 4.049999999999998934 ) ;
#191477 = CARTESIAN_POINT ( 'NONE',  ( 21.06089410995848255, 10.72529553213474429, -112.7023807310433625 ) ) ;
#191478 = FACE_OUTER_BOUND ( 'NONE', #96466, .T. ) ;
#191479 = CARTESIAN_POINT ( 'NONE',  ( 22.50000000000000000, 76.00000000001237765, -170.0231074845243597 ) ) ;
#191480 = LINE ( 'NONE', #213568, #24597 ) ;
#191481 = DIRECTION ( 'NONE',  ( 0.000000000000000000, 1.000000000000000000, 0.000000000000000000 ) ) ;
#191483 = DIRECTION ( 'NONE',  ( -1.000000000000000000, -0.000000000000000000, -0.000000000000000000 ) ) ;
#191482 = CARTESIAN_POINT ( 'NONE',  ( -21.14999999999999858, 6.390846877240202950, -199.6081416912452653 ) ) ;
#191484 = CIRCLE ( 'NONE', #124813, 12.87499999999999822 ) ;
#191485 = LINE ( 'NONE', #246296, #212947 ) ;
#191486 = EDGE_CURVE ( 'NONE', #237528, #35657, #16399, .T. ) ;
#191487 = DIRECTION ( 'NONE',  ( 0.000000000000000000, 0.000000000000000000, -1.000000000000000000 ) ) ;
#191488 = CYLINDRICAL_SURFACE ( 'NONE', #25628, 0.09999999999999939493 ) ;
#191490 = CARTESIAN_POINT ( 'NONE',  ( 20.95575313997065336, 18.85908140503239494, -227.9747421143725887 ) ) ;
#191489 = CIRCLE ( 'NONE', #224752, 0.09999999999998898659 ) ;
#191491 = EDGE_LOOP ( 'NONE', ( #234754, #25307, #56535, #94054 ) ) ;
#191492 = DIRECTION ( 'NONE',  ( 1.000000000000000000, 0.000000000000000000, 0.000000000000000000 ) ) ;
#191493 = DIRECTION ( 'NONE',  ( 1.000000000000000000, -3.265361837132813093E-16, -2.280189983783949500E-30 ) ) ;
#191494 = DIRECTION ( 'NONE',  ( 0.000000000000000000, 0.9994937237965569876, 0.03181660087583042945 ) ) ;
#191495 = DIRECTION ( 'NONE',  ( 0.000000000000000000, -6.661338147750933721E-15, 1.000000000000000000 ) ) ;
#191496 = DIRECTION ( 'NONE',  ( 0.000000000000000000, 0.000000000000000000, -1.000000000000000000 ) ) ;
#191498 = EDGE_CURVE ( 'NONE', #161829, #42440, #162153, .T. ) ;
#191497 = CARTESIAN_POINT ( 'NONE',  ( -23.15000000000000213, 64.35000000001187459, -90.87310748452438247 ) ) ;
#191499 = ORIENTED_EDGE ( 'NONE', *, *, #107291, .T. ) ;
#191500 =( BOUNDED_SURFACE ( )  B_SPLINE_SURFACE ( 3, 2, ( 
 ( #180846, #74400, #221226 ),
 ( #173517, #215152, #54781 ),
 ( #36554, #76917, #93917 ),
 ( #240817, #176055, #13114 ) ),
 .UNSPECIFIED., .F., .F., .F. ) 
 B_SPLINE_SURFACE_WITH_KNOTS ( ( 4, 4 ),
 ( 3, 3 ),
 ( 0.0006461284895273737604, 0.0007503702773985880276 ),
 ( 0.000000000000000000, 1.000000000000000000 ),
 .UNSPECIFIED. ) 
 GEOMETRIC_REPRESENTATION_ITEM ( )  RATIONAL_B_SPLINE_SURFACE ( (
 ( 1.000000000000000000, 0.7071067811865318076, 1.000000000000000000),
 ( 1.000000000000000000, 0.7076476444648033270, 1.000000000000000000),
 ( 1.000000000000000000, 0.7075727925192996093, 1.000000000000000000),
 ( 1.000000000000000000, 0.7071067811865210384, 1.000000000000000000) ) ) 
 REPRESENTATION_ITEM ( '' )  SURFACE ( )  );
#191501 = VERTEX_POINT ( 'NONE', #135492 ) ;
#191502 = EDGE_CURVE ( 'NONE', #177022, #76927, #220414, .T. ) ;
#191504 = EDGE_CURVE ( 'NONE', #182088, #49212, #158957, .T. ) ;
#191503 = VECTOR ( 'NONE', #44198, 1000.000000000000000 ) ;
#191506 = CIRCLE ( 'NONE', #70699, 0.09999999999999939493 ) ;
#191505 = CYLINDRICAL_SURFACE ( 'NONE', #180443, 0.1000000000000054040 ) ;
#191507 = ORIENTED_EDGE ( 'NONE', *, *, #183639, .T. ) ;
#191508 = CARTESIAN_POINT ( 'NONE',  ( 23.24999999999999645, 36.65892442174935439, -249.5511627012433848 ) ) ;
#191509 = FACE_OUTER_BOUND ( 'NONE', #120492, .T. ) ;
#191510 = CIRCLE ( 'NONE', #195598, 0.09999999999999961697 ) ;
#191511 = B_SPLINE_CURVE_WITH_KNOTS ( 'NONE', 3,
 ( #204432, #6231, #85743, #59774, #139318, #199325, #20699, #179766, #1082, #220167, #187470, #111772, #11390 ),
 .UNSPECIFIED., .F., .F.,
 ( 4, 3, 3, 3, 4 ),
 ( -3.224855718275878119E-06, 0.000000000000000000, 6.199515528664636366E-06, 4.034952380127537373E-05, 7.452715123699773787E-05 ),
 .UNSPECIFIED. ) ;
#191512 = ORIENTED_EDGE ( 'NONE', *, *, #797, .F. ) ;
#191513 = CARTESIAN_POINT ( 'NONE',  ( 20.94999999999999929, 76.00000000001210765, -132.5231074845243313 ) ) ;
#191514 = EDGE_CURVE ( 'NONE', #168923, #191279, #124727, .T. ) ;
#191515 = EDGE_LOOP ( 'NONE', ( #229478, #92728, #100060, #248045 ) ) ;
#191516 = DIRECTION ( 'NONE',  ( 1.000000000000000000, 0.000000000000000000, 0.000000000000000000 ) ) ;
#191517 = DIRECTION ( 'NONE',  ( 0.000000000000000000, -0.000000000000000000, -1.000000000000000000 ) ) ;
#191518 = DIRECTION ( 'NONE',  ( -1.000000000000000000, 3.265361837132813093E-16, 2.280189983783949500E-30 ) ) ;
#191519 = CARTESIAN_POINT ( 'NONE',  ( -20.94999999999999929, 76.00000000001210765, -133.6231074845243256 ) ) ;
#191520 = DIRECTION ( 'NONE',  ( 1.000000000000000000, 0.000000000000000000, -0.000000000000000000 ) ) ;
#191521 = CARTESIAN_POINT ( 'NONE',  ( -20.85000000000000142, 77.26327546522934142, -128.6212428177779543 ) ) ;
#191522 = CARTESIAN_POINT ( 'NONE',  ( -22.60000000000080433, 64.10952111376602147, -247.1829669476428251 ) ) ;
#191524 = EDGE_LOOP ( 'NONE', ( #220752, #155983, #149769, #107488 ) ) ;
#191523 = CARTESIAN_POINT ( 'NONE',  ( -18.39999999999999858, -9.499999999988849808, -40.53206939669966857 ) ) ;
#191526 = CARTESIAN_POINT ( 'NONE',  ( -18.40000000000000213, 64.51332499825393541, -60.27310748452440947 ) ) ;
#191525 = CARTESIAN_POINT ( 'NONE',  ( 18.59999999999999787, 78.48087866980282001, -232.8271061603568910 ) ) ;
#191527 = VERTEX_POINT ( 'NONE', #195517 ) ;
#191529 = ORIENTED_EDGE ( 'NONE', *, *, #138454, .F. ) ;
#191528 = FILL_AREA_STYLE_COLOUR ( '', #11004 ) ;
#191530 = VECTOR ( 'NONE', #161354, 1000.000000000000000 ) ;
#191531 = ORIENTED_EDGE ( 'NONE', *, *, #241636, .T. ) ;
#191532 = CARTESIAN_POINT ( 'NONE',  ( -21.65000000000000213, 68.75000000001159606, -56.87310748452436826 ) ) ;
#191533 = CYLINDRICAL_SURFACE ( 'NONE', #9523, 11.80000000000000426 ) ;
#191534 = ADVANCED_FACE ( 'NONE', ( #97640 ), #54686, .T. ) ;
#191536 = EDGE_CURVE ( 'NONE', #169154, #246179, #16866, .T. ) ;
#191535 = CARTESIAN_POINT ( 'NONE',  ( 18.69999999999999929, -10.63400887967554986, 6.002871413764276909 ) ) ;
#191537 = CARTESIAN_POINT ( 'NONE',  ( 18.46082813847998594, -9.480749650907464243, -7.084370102715693562 ) ) ;
#191538 = CIRCLE ( 'NONE', #50035, 0.1000000000000055844 ) ;
#191539 = CARTESIAN_POINT ( 'NONE',  ( 21.14999999999999503, -0.09999999998884338825, -155.8504291924551808 ) ) ;
#191540 = DIRECTION ( 'NONE',  ( 1.000000000000000000, 0.000000000000000000, 0.000000000000000000 ) ) ;
#191541 = DIRECTION ( 'NONE',  ( 0.000000000000000000, 0.000000000000000000, -1.000000000000000000 ) ) ;
#191542 = EDGE_CURVE ( 'NONE', #71456, #213068, #76816, .T. ) ;
#191543 = DIRECTION ( 'NONE',  ( 0.000000000000000000, -1.000000000000000000, 0.000000000000000000 ) ) ;
#191544 = ORIENTED_EDGE ( 'NONE', *, *, #59141, .F. ) ;
#191545 = EDGE_LOOP ( 'NONE', ( #81925, #177581, #246425, #124302 ) ) ;
#191546 = DIRECTION ( 'NONE',  ( -1.000000000000000000, -0.000000000000000000, -0.000000000000000000 ) ) ;
#191547 = AXIS2_PLACEMENT_3D ( 'NONE', #122831, #182809, #124113 ) ;
#191548 = ORIENTED_EDGE ( 'NONE', *, *, #151558, .T. ) ;
#191550 = ORIENTED_EDGE ( 'NONE', *, *, #167107, .T. ) ;
#191549 = AXIS2_PLACEMENT_3D ( 'NONE', #80811, #97798, #40467 ) ;
#191551 = CIRCLE ( 'NONE', #54137, 0.09999999999999939493 ) ;
#191552 = DIRECTION ( 'NONE',  ( 0.000000000000000000, -1.000000000000000000, 0.000000000000000000 ) ) ;
#191553 = CARTESIAN_POINT ( 'NONE',  ( -21.07094088545304444, 69.67983277809545939, -103.1220011870765774 ) ) ;
#191554 = DIRECTION ( 'NONE',  ( 0.000000000000000000, 0.000000000000000000, 1.000000000000000000 ) ) ;
#191555 = DIRECTION ( 'NONE',  ( 1.000000000000000000, 0.000000000000000000, 0.000000000000000000 ) ) ;
#191556 = ORIENTED_EDGE ( 'NONE', *, *, #218829, .T. ) ;
#191557 = VECTOR ( 'NONE', #64398, 1000.000000000000000 ) ;
#191559 = VECTOR ( 'NONE', #25048, 1000.000000000000114 ) ;
#191558 = CARTESIAN_POINT ( 'NONE',  ( -18.43459694179555797, -9.494210124986887323, -207.6170052026610620 ) ) ;
#191560 = CARTESIAN_POINT ( 'NONE',  ( 23.14999999999998437, 1.115600667400684642E-11, -67.00000000000004263 ) ) ;
#191561 = DIRECTION ( 'NONE',  ( 1.000000000000000000, 0.000000000000000000, 0.000000000000000000 ) ) ;
#191562 = CARTESIAN_POINT ( 'NONE',  ( -17.11825945287481332, 66.05000000001255955, -182.7731074845244450 ) ) ;
#191563 = DIRECTION ( 'NONE',  ( 1.000000000000000000, 0.000000000000000000, 0.000000000000000000 ) ) ;
#191564 = VERTEX_POINT ( 'NONE', #96363 ) ;
#191566 = CARTESIAN_POINT ( 'NONE',  ( -18.50000000000000000, 85.42129027953377829, -29.19922530549827755 ) ) ;
#191565 = CARTESIAN_POINT ( 'NONE',  ( -16.93388492042258164, 60.88892937063719302, -221.0804221601966901 ) ) ;
#191567 = ORIENTED_EDGE ( 'NONE', *, *, #3805, .F. ) ;
#191570 = ORIENTED_EDGE ( 'NONE', *, *, #22855, .F. ) ;
#191569 = DIRECTION ( 'NONE',  ( 0.000000000000000000, 0.000000000000000000, -1.000000000000000000 ) ) ;
#191568 = DIRECTION ( 'NONE',  ( 0.7071067811865487940, 0.7071067811865462405, -7.215498431451186046E-16 ) ) ;
#191571 = AXIS2_PLACEMENT_3D ( 'NONE', #140722, #113768, #79449 ) ;
#191572 = CARTESIAN_POINT ( 'NONE',  ( -18.59999999999999787, 61.57587952878036930, -212.2000740415318774 ) ) ;
#191573 = AXIS2_PLACEMENT_3D ( 'NONE', #46183, #246949, #224815 ) ;
#191574 = AXIS2_PLACEMENT_3D ( 'NONE', #254518, #236266, #38089 ) ;
#191575 = VECTOR ( 'NONE', #98288, 1000.000000000000000 ) ;
#191576 = AXIS2_PLACEMENT_3D ( 'NONE', #131205, #112941, #150779 ) ;
#191577 = EDGE_CURVE ( 'NONE', #240390, #208327, #8031, .T. ) ;
#191578 = CARTESIAN_POINT ( 'NONE',  ( 21.00000000000000000, 9.750000000011153745, -155.2500000000000284 ) ) ;
#191579 = ORIENTED_EDGE ( 'NONE', *, *, #6666, .T. ) ;
#191581 = EDGE_CURVE ( 'NONE', #252315, #146049, #120472, .T. ) ;
#191580 = DIRECTION ( 'NONE',  ( -0.000000000000000000, -0.000000000000000000, -1.000000000000000000 ) ) ;
#191582 = AXIS2_PLACEMENT_3D ( 'NONE', #190050, #90938, #227890 ) ;
#191583 = CARTESIAN_POINT ( 'NONE',  ( 20.94999999999999574, 1.250000000011155299, -75.00000000000004263 ) ) ;
#191584 = ADVANCED_FACE ( 'NONE', ( #35172 ), #217590, .T. ) ;
#191585 = DIRECTION ( 'NONE',  ( -1.073024830501117725E-15, 6.982962677686266711E-15, -1.000000000000000000 ) ) ;
#191586 = ADVANCED_FACE ( 'NONE', ( #117239 ), #57234, .F. ) ;
#191588 = ORIENTED_EDGE ( 'NONE', *, *, #77961, .T. ) ;
#191587 = DIRECTION ( 'NONE',  ( 0.000000000000000000, -0.2617529984165152257, -0.9651348961777124202 ) ) ;
#191590 = ORIENTED_EDGE ( 'NONE', *, *, #131290, .T. ) ;
#191589 = ADVANCED_FACE ( 'NONE', ( #119822, #174695, #254159, #138062 ), #198042, .T. ) ;
#191591 = CARTESIAN_POINT ( 'NONE',  ( -18.44085059012131822, 11.51401249349495437, -109.7596946808784963 ) ) ;
#191592 = CARTESIAN_POINT ( 'NONE',  ( 23.14999999999999503, 11.65000000001116298, -188.7499999999999716 ) ) ;
#191593 = DIRECTION ( 'NONE',  ( 0.000000000000000000, 0.9126074666063771490, 0.4088369013363281623 ) ) ;
#191594 = ADVANCED_FACE ( 'NONE', ( #20720 ), #37724, .F. ) ;
#191595 = DIRECTION ( 'NONE',  ( -1.000000000000000000, 0.000000000000000000, 0.000000000000000000 ) ) ;
#191598 = EDGE_CURVE ( 'NONE', #206936, #61341, #62188, .T. ) ;
#191597 = ADVANCED_FACE ( 'NONE', ( #203181 ), #221439, .F. ) ;
#191596 = ORIENTED_EDGE ( 'NONE', *, *, #102875, .F. ) ;
#191599 = DIRECTION ( 'NONE',  ( -1.000000000000000000, 0.000000000000000000, 0.000000000000000000 ) ) ;
#191600 = DIRECTION ( 'NONE',  ( 0.000000000000000000, 1.000000000000000000, 6.352154140967427193E-15 ) ) ;
#191601 = DIRECTION ( 'NONE',  ( 0.000000000000000000, 0.000000000000000000, -1.000000000000000000 ) ) ;
#191602 = ADVANCED_FACE ( 'NONE', ( #161514 ), #204456, .F. ) ;
#191603 = VERTEX_POINT ( 'NONE', #144472 ) ;
#191604 = LINE ( 'NONE', #74228, #118044 ) ;
#191605 = EDGE_CURVE ( 'NONE', #89005, #8389, #145555, .T. ) ;
#191606 = AXIS2_PLACEMENT_3D ( 'NONE', #15536, #95042, #16812 ) ;
#191607 = ORIENTED_EDGE ( 'NONE', *, *, #110318, .T. ) ;
#191608 = CARTESIAN_POINT ( 'NONE',  ( -20.94999999999999929, -1.362429037193305881, -41.38888124792119783 ) ) ;
#191609 = DIRECTION ( 'NONE',  ( 0.000000000000000000, -0.8814952561688430555, 0.4721928772777348460 ) ) ;
#191610 = EDGE_CURVE ( 'NONE', #154016, #224589, #24804, .T. ) ;
#191611 = ADVANCED_FACE ( 'NONE', ( #106626 ), #205745, .T. ) ;
#191612 = VECTOR ( 'NONE', #59864, 1000.000000000000000 ) ;
#191613 = ORIENTED_EDGE ( 'NONE', *, *, #60540, .T. ) ;
#191614 = ORIENTED_EDGE ( 'NONE', *, *, #216492, .T. ) ;
#191615 = EDGE_CURVE ( 'NONE', #244869, #21878, #99739, .T. ) ;
#191616 = DIRECTION ( 'NONE',  ( -1.000000000000000000, 0.000000000000000000, 0.000000000000000000 ) ) ;
#191617 = ORIENTED_EDGE ( 'NONE', *, *, #36188, .T. ) ;
#191619 = VERTEX_POINT ( 'NONE', #241043 ) ;
#191618 = CARTESIAN_POINT ( 'NONE',  ( -23.15000000000000213, 76.00000000001244871, -170.0231074845243597 ) ) ;
#191621 = EDGE_CURVE ( 'NONE', #163131, #70073, #112270, .T. ) ;
#191620 = ORIENTED_EDGE ( 'NONE', *, *, #71153, .T. ) ;
#191622 = CIRCLE ( 'NONE', #70993, 0.1000000000000051958 ) ;
#191625 = ORIENTED_EDGE ( 'NONE', *, *, #132721, .T. ) ;
#191624 = EDGE_LOOP ( 'NONE', ( #215479, #196279, #153768, #59311, #15164, #99485, #65193, #55292, #169799, #31325 ) ) ;
#191623 = DIRECTION ( 'NONE',  ( -0.000000000000000000, 0.9770955615653313941, 0.2128009952263603954 ) ) ;
#191626 = CIRCLE ( 'NONE', #237572, 0.09999999999998898659 ) ;
#191627 = ADVANCED_FACE ( 'NONE', ( #186199 ), #74693, .T. ) ;
#191628 = DIRECTION ( 'NONE',  ( 0.000000000000000000, 0.000000000000000000, -1.000000000000000000 ) ) ;
#191629 = ORIENTED_EDGE ( 'NONE', *, *, #161191, .F. ) ;
#191630 = DIRECTION ( 'NONE',  ( -0.000000000000000000, 1.000000000000000000, -0.000000000000000000 ) ) ;
#191631 = CYLINDRICAL_SURFACE ( 'NONE', #245030, 0.1000000000000028644 ) ;
#191632 = AXIS2_PLACEMENT_3D ( 'NONE', #97989, #254491, #74645 ) ;
#191633 = SPHERICAL_SURFACE ( 'NONE', #163940, 0.1000000000000000056 ) ;
#191634 = AXIS2_PLACEMENT_3D ( 'NONE', #44513, #124048, #203572 ) ;
#191635 = CYLINDRICAL_SURFACE ( 'NONE', #80486, 0.09999999999999939493 ) ;
#191636 = CYLINDRICAL_SURFACE ( 'NONE', #100953, 0.5000000000000004441 ) ;
#191637 = ORIENTED_EDGE ( 'NONE', *, *, #138717, .T. ) ;
#191638 = ORIENTED_EDGE ( 'NONE', *, *, #169463, .F. ) ;
#191639 = ORIENTED_EDGE ( 'NONE', *, *, #170804, .F. ) ;
#191640 = CARTESIAN_POINT ( 'NONE',  ( 18.59999999999999076, 69.55000000001199112, -115.2731074845243455 ) ) ;
#191642 = VERTEX_POINT ( 'NONE', #61105 ) ;
#191641 = LINE ( 'NONE', #12994, #32956 ) ;
#191643 = DIRECTION ( 'NONE',  ( 0.000000000000000000, 0.000000000000000000, 1.000000000000000000 ) ) ;
#191645 = ORIENTED_EDGE ( 'NONE', *, *, #212137, .T. ) ;
#191644 = CARTESIAN_POINT ( 'NONE',  ( 18.59999999999999787, 46.62132166459547733, -243.0426574061995950 ) ) ;
#191646 = EDGE_CURVE ( 'NONE', #212023, #70808, #45394, .T. ) ;
#191647 = ORIENTED_EDGE ( 'NONE', *, *, #57426, .F. ) ;
#191648 = CARTESIAN_POINT ( 'NONE',  ( -18.47690164073607022, -0.6931637155149755758, -242.2947192224642379 ) ) ;
#191649 = VERTEX_POINT ( 'NONE', #25844 ) ;
#191650 = AXIS2_PLACEMENT_3D ( 'NONE', #156069, #251271, #17789 ) ;
#191651 = CIRCLE ( 'NONE', #241680, 11.80000000000000604 ) ;
#191652 = DIRECTION ( 'NONE',  ( -0.000000000000000000, 1.000000000000000000, 7.272083257015735086E-15 ) ) ;
#191653 = CARTESIAN_POINT ( 'NONE',  ( 18.39999999999999503, 64.52683809665012404, -190.8731074845244393 ) ) ;
#191655 = ORIENTED_EDGE ( 'NONE', *, *, #257457, .F. ) ;
#191654 = ORIENTED_EDGE ( 'NONE', *, *, #58668, .T. ) ;
#191656 = ORIENTED_EDGE ( 'NONE', *, *, #92123, .T. ) ;
#191657 = CARTESIAN_POINT ( 'NONE',  ( -20.00857864376270001, 44.09750824044544970, -236.1925523404271132 ) ) ;
#191658 = ORIENTED_EDGE ( 'NONE', *, *, #121053, .T. ) ;
#191659 = ORIENTED_EDGE ( 'NONE', *, *, #44114, .T. ) ;
#191660 = CARTESIAN_POINT ( 'NONE',  ( 20.04142135623730070, 11.65000000001115943, -155.3500000000000227 ) ) ;
#191662 = ORIENTED_EDGE ( 'NONE', *, *, #149757, .F. ) ;
#191661 = DIRECTION ( 'NONE',  ( 0.000000000000000000, -1.000000000000000000, -6.860497997771531562E-15 ) ) ;
#191663 = DIRECTION ( 'NONE',  ( 0.000000000000000000, 0.000000000000000000, -1.000000000000000000 ) ) ;
#191664 = DIRECTION ( 'NONE',  ( 0.000000000000000000, -6.982962677686266711E-15, 1.000000000000000000 ) ) ;
#191665 = CARTESIAN_POINT ( 'NONE',  ( 23.15000000000000213, -11.48912529306489994, -164.5000000000000000 ) ) ;
#191666 = DIRECTION ( 'NONE',  ( 1.000000000000000000, 0.000000000000000000, 0.000000000000000000 ) ) ;
#191667 = EDGE_LOOP ( 'NONE', ( #90124, #13440, #158156, #202050 ) ) ;
#191668 = VERTEX_POINT ( 'NONE', #21999 ) ;
#191669 = CARTESIAN_POINT ( 'NONE',  ( 18.46163235739473407, 85.48015080693014056, -96.36549694464677884 ) ) ;
#191671 = AXIS2_PLACEMENT_3D ( 'NONE', #219373, #116445, #156877 ) ;
#191670 = DIRECTION ( 'NONE',  ( 0.000000000000000000, -0.2617529984165152257, -0.9651348961777124202 ) ) ;
#191673 = ADVANCED_FACE ( 'NONE', ( #62398 ), #184907, .T. ) ;
#191672 = CARTESIAN_POINT ( 'NONE',  ( -21.44999999999999929, 9.712035112405693837, -211.5243229699422614 ) ) ;
#191674 = AXIS2_PLACEMENT_3D ( 'NONE', #55027, #75903, #155480 ) ;
#191675 = AXIS2_PLACEMENT_3D ( 'NONE', #77280, #76009, #198520 ) ;
#191676 = CIRCLE ( 'NONE', #154087, 0.1000000000000028644 ) ;
#191677 = ORIENTED_EDGE ( 'NONE', *, *, #12279, .T. ) ;
#191678 = EDGE_CURVE ( 'NONE', #52922, #229236, #101471, .T. ) ;
#191679 = CARTESIAN_POINT ( 'NONE',  ( -18.59999999999999787, 7.576017155224048061, -241.7224044826512284 ) ) ;
#191680 = AXIS2_PLACEMENT_3D ( 'NONE', #168049, #50607, #225392 ) ;
#191681 = CYLINDRICAL_SURFACE ( 'NONE', #217499, 11.80000000000000426 ) ;
#191682 = VERTEX_POINT ( 'NONE', #3693 ) ;
#191683 = VERTEX_POINT ( 'NONE', #83204 ) ;
#191684 = ADVANCED_FACE ( 'NONE', ( #181078 ), #2396, .F. ) ;
#191685 = CARTESIAN_POINT ( 'NONE',  ( -22.50000000000000000, 76.00000000001242029, -176.2731074845243597 ) ) ;
#191687 = EDGE_CURVE ( 'NONE', #204739, #231683, #123661, .T. ) ;
#191686 = CARTESIAN_POINT ( 'NONE',  ( -16.77779411503079032, 66.05389855308793301, -123.8600500669045346 ) ) ;
#191688 = ORIENTED_EDGE ( 'NONE', *, *, #71062, .T. ) ;
#191689 = DIRECTION ( 'NONE',  ( -1.000000000000000000, 0.000000000000000000, -0.000000000000000000 ) ) ;
#191690 = VERTEX_POINT ( 'NONE', #110497 ) ;
#191691 = CARTESIAN_POINT ( 'NONE',  ( 18.33683296300430854, -9.511149971121708901, -140.9057074127098304 ) ) ;
#191692 = CARTESIAN_POINT ( 'NONE',  ( -16.80939487329395021, 9.950000000011138823, -154.8500000000009038 ) ) ;
#191694 = CARTESIAN_POINT ( 'NONE',  ( -21.05000000000000071, -1.489567864901281791, -194.6304332222954372 ) ) ;
#191693 = LINE ( 'NONE', #226926, #90488 ) ;
#191696 = DIRECTION ( 'NONE',  ( 0.000000000000000000, 0.2617529984165031243, 0.9651348961777157509 ) ) ;
#191695 = VECTOR ( 'NONE', #84217, 999.9999999999998863 ) ;
#191697 = CARTESIAN_POINT ( 'NONE',  ( 18.39999999999999858, -9.499999999988842703, -174.5320693966996259 ) ) ;
#191698 = CARTESIAN_POINT ( 'NONE',  ( 23.14999999999999858, 0.000000000000000000, -33.50000000000000000 ) ) ;
#191700 = VERTEX_POINT ( 'NONE', #50502 ) ;
#191699 = DIRECTION ( 'NONE',  ( 0.000000000000000000, 0.8814952561688438326, -0.4721928772777334582 ) ) ;
#191701 = ADVANCED_FACE ( 'NONE', ( #188752 ), #174660, .T. ) ;
#191703 = ORIENTED_EDGE ( 'NONE', *, *, #4499, .F. ) ;
#191702 = ORIENTED_EDGE ( 'NONE', *, *, #92103, .F. ) ;
#191704 = ORIENTED_EDGE ( 'NONE', *, *, #240140, .T. ) ;
#191705 = CARTESIAN_POINT ( 'NONE',  ( 20.94999999999999929, 76.00000000001139711, -31.92310748452432279 ) ) ;
#191706 = CARTESIAN_POINT ( 'NONE',  ( -20.54999999999999716, 74.07476635515273244, -182.7533510176504876 ) ) ;
#191708 = CYLINDRICAL_SURFACE ( 'NONE', #7401, 4.049999999999998046 ) ;
#191707 = CARTESIAN_POINT ( 'NONE',  ( -16.81931177881022066, 66.06300394050866487, -182.7498896059072422 ) ) ;
#191709 = DIRECTION ( 'NONE',  ( 0.000000000000000000, 0.000000000000000000, -1.000000000000000000 ) ) ;
#191710 = ORIENTED_EDGE ( 'NONE', *, *, #83535, .T. ) ;
#191711 = CARTESIAN_POINT ( 'NONE',  ( 18.59999999999996945, 46.46967969402478360, -243.0849751855955674 ) ) ;
#191712 = ORIENTED_EDGE ( 'NONE', *, *, #17454, .F. ) ;
#191713 = ORIENTED_EDGE ( 'NONE', *, *, #242373, .T. ) ;
#191714 = DIRECTION ( 'NONE',  ( 0.000000000000000000, -0.1495327102803078179, -0.9887567792719429427 ) ) ;
#191715 = CARTESIAN_POINT ( 'NONE',  ( -20.64999999999999858, -8.663551401858004652, -177.0241011180672785 ) ) ;
#191716 = CIRCLE ( 'NONE', #83491, 0.1000000000000124678 ) ;
#191717 = ADVANCED_FACE ( 'NONE', ( #148348 ), #190045, .F. ) ;
#191718 = DIRECTION ( 'NONE',  ( -0.000000000000000000, -0.000000000000000000, 1.000000000000000000 ) ) ;
#191719 = CARTESIAN_POINT ( 'NONE',  ( 18.59999999999999076, 6.450000000011156587, -155.1500000000000057 ) ) ;
#191720 = EDGE_LOOP ( 'NONE', ( #103636, #199057 ) ) ;
#191721 = ORIENTED_EDGE ( 'NONE', *, *, #215972, .T. ) ;
#191722 = DIRECTION ( 'NONE',  ( 0.000000000000000000, 1.000000000000000000, 6.352154140967427193E-15 ) ) ;
#191723 = CARTESIAN_POINT ( 'NONE',  ( -16.89797118371569695, 9.976380722655314059, -54.43729336755813364 ) ) ;
#191724 = AXIS2_PLACEMENT_3D ( 'NONE', #208393, #148406, #48002 ) ;
#191725 = CARTESIAN_POINT ( 'NONE',  ( -0.8999999999999993561, -11.65000000000000036, 23.40000000000000568 ) ) ;
#191726 = DIRECTION ( 'NONE',  ( 3.469446951953635015E-14, 0.000000000000000000, 1.000000000000000000 ) ) ;
#191727 = DIRECTION ( 'NONE',  ( 0.7071359030027629666, -0.6824253222083883630, 0.1850796971394867152 ) ) ;
#191728 = CYLINDRICAL_SURFACE ( 'NONE', #75328, 0.09999999999999939493 ) ;
#191729 = ORIENTED_EDGE ( 'NONE', *, *, #211769, .F. ) ;
#191731 = ADVANCED_FACE ( 'NONE', ( #149654 ), #72225, .T. ) ;
#191730 = LINE ( 'NONE', #74354, #50730 ) ;
#191732 = DIRECTION ( 'NONE',  ( 1.000000000000000000, 0.000000000000000000, 0.000000000000000000 ) ) ;
#191734 = DIRECTION ( 'NONE',  ( 1.000000000000000000, 0.000000000000000000, 0.000000000000000000 ) ) ;
#191733 = CARTESIAN_POINT ( 'NONE',  ( -22.49510344025093644, 0.06712767819425934090, 11.64997010511425835 ) ) ;
#191735 = DIRECTION ( 'NONE',  ( 0.000000000000000000, 0.9770955615653551529, 0.2128009952262517601 ) ) ;
#191736 = EDGE_CURVE ( 'NONE', #77400, #152331, #113075, .T. ) ;
#191737 = CARTESIAN_POINT ( 'NONE',  ( 19.99999999999998934, 61.54970422893870818, -212.2965875311496688 ) ) ;
#191738 = DIRECTION ( 'NONE',  ( 1.073024830501117725E-15, -0.000000000000000000, -1.000000000000000000 ) ) ;
#191739 = DIRECTION ( 'NONE',  ( 1.000000000000000000, 0.000000000000000000, 0.000000000000000000 ) ) ;
#191740 = AXIS2_PLACEMENT_3D ( 'NONE', #109338, #250159, #230602 ) ;
#191742 = ORIENTED_EDGE ( 'NONE', *, *, #82853, .F. ) ;
#191741 = FACE_BOUND ( 'NONE', #221211, .T. ) ;
#191743 = CIRCLE ( 'NONE', #79243, 0.09999999999999939493 ) ;
#191744 = EDGE_CURVE ( 'NONE', #231078, #47961, #247444, .T. ) ;
#191745 = CIRCLE ( 'NONE', #224992, 0.09999999999999489853 ) ;
#191746 = CARTESIAN_POINT ( 'NONE',  ( -18.50000000000000000, 11.76393579169289083, -211.0774408799668720 ) ) ;
#191747 = ADVANCED_FACE ( 'NONE', ( #147047 ), #241268, .F. ) ;
#191748 = AXIS2_PLACEMENT_3D ( 'NONE', #104466, #221844, #62802 ) ;
#191749 = EDGE_CURVE ( 'NONE', #139380, #232784, #128826, .T. ) ;
#191750 = CIRCLE ( 'NONE', #237512, 0.09999999999999854838 ) ;
#191751 = CARTESIAN_POINT ( 'NONE',  ( 20.85000000000000142, 76.00000000001170974, -69.52310748452431710 ) ) ;
#191752 = CARTESIAN_POINT ( 'NONE',  ( -21.05000000000000071, 76.00000000001267608, -203.5231074845243597 ) ) ;
#191753 = EDGE_CURVE ( 'NONE', #222808, #142144, #88343, .T. ) ;
#191754 = CARTESIAN_POINT ( 'NONE',  ( 15.74999999999999645, 9.350000000011133849, -83.86574316727394773 ) ) ;
#191755 = PLANE ( 'NONE',  #46111 ) ;
#191756 = AXIS2_PLACEMENT_3D ( 'NONE', #87770, #167360, #246854 ) ;
#191757 = AXIS2_PLACEMENT_3D ( 'NONE', #44637, #181593, #45915 ) ;
#191758 = VECTOR ( 'NONE', #108321, 1000.000000000000000 ) ;
#191759 = CARTESIAN_POINT ( 'NONE',  ( -18.60000000000000142, -8.350000000000004974, 32.89999999999999858 ) ) ;
#191760 = DIRECTION ( 'NONE',  ( 0.000000000000000000, 0.000000000000000000, -1.000000000000000000 ) ) ;
#191761 = CIRCLE ( 'NONE', #41715, 0.1000000000000054040 ) ;
#191762 = AXIS2_PLACEMENT_3D ( 'NONE', #176315, #96718, #159315 ) ;
#191763 = ORIENTED_EDGE ( 'NONE', *, *, #14754, .F. ) ;
#191764 = CARTESIAN_POINT ( 'NONE',  ( -17.11825945287482753, 66.05000000001159322, -56.77310748452439526 ) ) ;
#191766 = EDGE_LOOP ( 'NONE', ( #226294, #232869 ) ) ;
#191765 = FACE_OUTER_BOUND ( 'NONE', #144145, .T. ) ;
#191767 = FACE_OUTER_BOUND ( 'NONE', #251219, .T. ) ;
#191768 = ADVANCED_FACE ( 'NONE', ( #11418 ), #170568, .T. ) ;
#191769 = DIRECTION ( 'NONE',  ( 0.000000000000000000, 1.000000000000000000, 0.000000000000000000 ) ) ;
#191770 = ORIENTED_EDGE ( 'NONE', *, *, #40372, .T. ) ;
#191771 = CARTESIAN_POINT ( 'NONE',  ( -16.87683809663752399, 66.15000000001182912, -82.92547150272068279 ) ) ;
#191772 = SHAPE_DEFINITION_REPRESENTATION ( #91051, #10216 ) ;
#191773 = CIRCLE ( 'NONE', #21080, 0.2000000000000057288 ) ;
#191774 = CARTESIAN_POINT ( 'NONE',  ( 23.14999999999999858, 4.000000000011155521, -200.9999999999999432 ) ) ;
#191775 = CARTESIAN_POINT ( 'NONE',  ( 21.05000000000000071, 67.22371710471941242, -94.46447848938342418 ) ) ;
#191776 = EDGE_LOOP ( 'NONE', ( #171335, #63240, #141116 ) ) ;
#191777 = CARTESIAN_POINT ( 'NONE',  ( -18.59999999999999787, 9.350000000000001421, -12.34999999999999964 ) ) ;
#191778 = DIRECTION ( 'NONE',  ( -0.000000000000000000, -0.000000000000000000, 1.000000000000000000 ) ) ;
#191779 = DIRECTION ( 'NONE',  ( -1.000000000000000000, -0.000000000000000000, -0.000000000000000000 ) ) ;
#191780 = ORIENTED_EDGE ( 'NONE', *, *, #4964, .T. ) ;
#191781 = ORIENTED_EDGE ( 'NONE', *, *, #67408, .T. ) ;
#191782 = CARTESIAN_POINT ( 'NONE',  ( -23.25000000000000355, 20.83093076766827423, -227.7429161672744442 ) ) ;
#191783 = VECTOR ( 'NONE', #118773, 1000.000000000000000 ) ;
#191784 = DIRECTION ( 'NONE',  ( 0.000000000000000000, -0.9126074666063660468, -0.4088369013363524762 ) ) ;
#191785 = CARTESIAN_POINT ( 'NONE',  ( 21.05000000000000071, -11.64999999998883595, -100.5000000000000284 ) ) ;
#191786 = FACE_OUTER_BOUND ( 'NONE', #175045, .T. ) ;
#191787 = VECTOR ( 'NONE', #171740, 1000.000000000000000 ) ;
#191789 = DIRECTION ( 'NONE',  ( 0.000000000000000000, 0.2128009952263485993, -0.9770955615653341697 ) ) ;
#191788 = CARTESIAN_POINT ( 'NONE',  ( 21.97500000000000497, 66.25000000001199396, -115.2731074845243597 ) ) ;
#191790 = CARTESIAN_POINT ( 'NONE',  ( -20.94999999999999929, 14.05000000001115623, -195.4863049292390542 ) ) ;
#191791 = DIRECTION ( 'NONE',  ( -0.7071067811865475727, 0.7071067811865475727, 4.937700262164531476E-15 ) ) ;
#191792 = DIRECTION ( 'NONE',  ( -0.000000000000000000, 0.8660254037844411501, 0.4999999999999956701 ) ) ;
#191793 = ORIENTED_EDGE ( 'NONE', *, *, #24088, .F. ) ;
#191794 = CIRCLE ( 'NONE', #33592, 11.80000000000000959 ) ;
#191796 = ORIENTED_EDGE ( 'NONE', *, *, #6477, .F. ) ;
#191795 = CARTESIAN_POINT ( 'NONE',  ( 12.93279065517211102, 62.89055100415843924, -215.8809258249640379 ) ) ;
#191797 = CARTESIAN_POINT ( 'NONE',  ( 21.08198257630413508, 69.66340326599731725, -170.0957508083090204 ) ) ;
#191798 = PLANE ( 'NONE',  #111731 ) ;
#191800 = DIRECTION ( 'NONE',  ( 1.000000000000000000, -0.000000000000000000, 0.000000000000000000 ) ) ;
#191799 = DIRECTION ( 'NONE',  ( 1.000000000000000000, 0.000000000000000000, 0.000000000000000000 ) ) ;
#191801 = AXIS2_PLACEMENT_3D ( 'NONE', #170569, #248774, #46696 ) ;
#191802 = ORIENTED_EDGE ( 'NONE', *, *, #120611, .T. ) ;
#191803 = DIRECTION ( 'NONE',  ( -0.000000000000000000, 0.000000000000000000, 1.000000000000000000 ) ) ;
#191804 = DIRECTION ( 'NONE',  ( -0.000000000000000000, 6.982962677686266711E-15, -1.000000000000000000 ) ) ;
#191805 = CARTESIAN_POINT ( 'NONE',  ( -22.47071067811865319, 0.3704148268516976872, -229.9999874772930752 ) ) ;
#191807 = EDGE_CURVE ( 'NONE', #83518, #187424, #191389, .T. ) ;
#191806 = DIRECTION ( 'NONE',  ( 0.000000000000000000, 0.4721928772777346239, 0.8814952561688430555 ) ) ;
#191808 = ORIENTED_EDGE ( 'NONE', *, *, #111081, .F. ) ;
#191809 = ORIENTED_EDGE ( 'NONE', *, *, #238439, .T. ) ;
#191810 = AXIS2_PLACEMENT_3D ( 'NONE', #234936, #112425, #38037 ) ;
#191811 = ADVANCED_FACE ( 'NONE', ( #90932 ), #207043, .F. ) ;
#191812 = EDGE_CURVE ( 'NONE', #224580, #23498, #187497, .T. ) ;
#191813 = DIRECTION ( 'NONE',  ( 1.000000000000000000, 2.952720810173289112E-16, -0.000000000000000000 ) ) ;
#191814 = ORIENTED_EDGE ( 'NONE', *, *, #15764, .T. ) ;
#191815 = CARTESIAN_POINT ( 'NONE',  ( -20.94999999999999929, 0.6656436123793491033, -212.6810495496487476 ) ) ;
#191816 = CIRCLE ( 'NONE', #233499, 0.5000000000000004441 ) ;
#191817 = VECTOR ( 'NONE', #225310, 1000.000000000000000 ) ;
#191818 = CARTESIAN_POINT ( 'NONE',  ( -21.45000000000000284, 29.41239393758413811, -236.9245051605820720 ) ) ;
#191819 = DIRECTION ( 'NONE',  ( -1.000000000000000000, 0.000000000000000000, -0.000000000000000000 ) ) ;
#191820 = AXIS2_PLACEMENT_3D ( 'NONE', #115601, #158611, #178173 ) ;
#191821 = ORIENTED_EDGE ( 'NONE', *, *, #126280, .F. ) ;
#191822 = CARTESIAN_POINT ( 'NONE',  ( 18.59999999999999076, 64.35000000001251408, -178.6731074845244507 ) ) ;
#191823 = EDGE_CURVE ( 'NONE', #198469, #247693, #237338, .T. ) ;
#191824 =( BOUNDED_CURVE ( )  B_SPLINE_CURVE ( 3, ( #640, #178046, #235414, #176759 ),
 .UNSPECIFIED., .F., .F. ) 
 B_SPLINE_CURVE_WITH_KNOTS ( ( 4, 4 ),
 ( 3.141592653589793116, 4.712388980384689674 ),
 .UNSPECIFIED. ) 
 CURVE ( )  GEOMETRIC_REPRESENTATION_ITEM ( )  RATIONAL_B_SPLINE_CURVE ( ( 1.000000000000000000, 0.8047378541243649375, 0.8047378541243649375, 1.000000000000000000 ) ) 
 REPRESENTATION_ITEM ( '' )  );
#191825 = ADVANCED_FACE ( 'NONE', ( #231750 ), #53091, .F. ) ;
#191826 = DIRECTION ( 'NONE',  ( 0.000000000000000000, -8.267618268485210697E-15, 1.000000000000000000 ) ) ;
#191827 = DIRECTION ( 'NONE',  ( 1.000000000000000000, 0.000000000000000000, 0.000000000000000000 ) ) ;
#191828 = CARTESIAN_POINT ( 'NONE',  ( 22.24259225415828922, 75.90093411655936961, -144.0150453550897112 ) ) ;
#191829 = DIRECTION ( 'NONE',  ( 0.000000000000000000, 0.000000000000000000, 1.000000000000000000 ) ) ;
#191830 = AXIS2_PLACEMENT_3D ( 'NONE', #84701, #144701, #3926 ) ;
#191831 = CYLINDRICAL_SURFACE ( 'NONE', #103085, 0.8750000000000007772 ) ;
#191832 = B_SPLINE_CURVE_WITH_KNOTS ( 'NONE', 3,
 ( #132730, #212269, #133990, #33668, #173178, #210972, #113150, #75340, #154875, #229263, #169318, #55697, #29805, #188835, #170616, #15353 ),
 .UNSPECIFIED., .F., .F.,
 ( 4, 3, 3, 3, 3, 4 ),
 ( 0.000000000000000000, 1.810570668010099324E-05, 2.740575833572219257E-05, 4.256816319435903717E-05, 5.213463471026593917E-05, 6.641585710720939166E-05 ),
 .UNSPECIFIED. ) ;
#191833 = ORIENTED_EDGE ( 'NONE', *, *, #18960, .F. ) ;
#191835 = CARTESIAN_POINT ( 'NONE',  ( -16.86132326855786090, 9.950000000011137047, -180.1986357846682836 ) ) ;
#191834 = CARTESIAN_POINT ( 'NONE',  ( -16.94445028196808778, 9.992063609697733995, -12.60733017841845438 ) ) ;
#191837 = VERTEX_POINT ( 'NONE', #154793 ) ;
#191836 = B_SPLINE_CURVE_WITH_KNOTS ( 'NONE', 3,
 ( #79504, #238595, #18269, #142055, #122517, #202043, #3841 ),
 .UNSPECIFIED., .F., .F.,
 ( 4, 3, 4 ),
 ( 0.000000000000000000, 0.0009834301579439998740, 0.001767853679402675614 ),
 .UNSPECIFIED. ) ;
#191839 = ORIENTED_EDGE ( 'NONE', *, *, #232087, .T. ) ;
#191838 = DIRECTION ( 'NONE',  ( 1.000000000000000000, 2.885090398161910739E-16, 6.283419270304611573E-17 ) ) ;
#191840 = VERTEX_POINT ( 'NONE', #115640 ) ;
#191841 = CARTESIAN_POINT ( 'NONE',  ( 18.59999999999999432, 4.064367954407507533, -211.9684786640956418 ) ) ;
#191842 = CARTESIAN_POINT ( 'NONE',  ( 13.12229106158774883, 66.56936289831551790, -151.7548468664635095 ) ) ;
#191843 = CARTESIAN_POINT ( 'NONE',  ( -23.15000000000000213, 61.57587952878036219, -212.2000740415318774 ) ) ;
#191844 = ADVANCED_FACE ( 'NONE', ( #54375 ), #27312, .T. ) ;
#191845 = CARTESIAN_POINT ( 'NONE',  ( 21.05000000000000071, 65.37049252075115646, -128.8951280845284941 ) ) ;
#191846 = B_SPLINE_CURVE_WITH_KNOTS ( 'NONE', 3,
 ( #69017, #148541, #169421, #84662, #89825, #45584, #70311, #228078, #226779, #49431 ),
 .UNSPECIFIED., .F., .F.,
 ( 4, 3, 3, 4 ),
 ( -2.000561356215401283E-06, 0.000000000000000000, 1.787822682428326401E-05, 4.206475347089222807E-05 ),
 .UNSPECIFIED. ) ;
#191847 = ORIENTED_EDGE ( 'NONE', *, *, #179237, .T. ) ;
#191848 = ADVANCED_FACE ( 'NONE', ( #116923 ), #235571, .F. ) ;
#191849 = EDGE_CURVE ( 'NONE', #239382, #195448, #196447, .T. ) ;
#191850 = CARTESIAN_POINT ( 'NONE',  ( -21.05000000000000071, -11.64999999998884483, -136.9000000000000341 ) ) ;
#191851 = CARTESIAN_POINT ( 'NONE',  ( 18.52928932304149967, 10.27928932305266407, -158.6762534328032643 ) ) ;
#191852 = ORIENTED_EDGE ( 'NONE', *, *, #178106, .F. ) ;
#191853 = SPHERICAL_SURFACE ( 'NONE', #202461, 0.1000000000000000056 ) ;
#191854 = CIRCLE ( 'NONE', #125188, 0.09999999999999439892 ) ;
#191855 = AXIS2_PLACEMENT_3D ( 'NONE', #63732, #217647, #161578 ) ;
#191856 = ADVANCED_FACE ( 'NONE', ( #55624 ), #174379, .F. ) ;
#191858 = AXIS2_PLACEMENT_3D ( 'NONE', #48662, #27860, #31711 ) ;
#191857 = DIRECTION ( 'NONE',  ( -3.265361837132813586E-16, 0.9770955615653313941, 0.2128009952263610893 ) ) ;
#191859 = VERTEX_POINT ( 'NONE', #214732 ) ;
#191860 = CARTESIAN_POINT ( 'NONE',  ( -20.54999999999999716, 73.50000000001199396, -116.2477294072864140 ) ) ;
#191861 = EDGE_LOOP ( 'NONE', ( #80971, #37496, #108887, #250796 ) ) ;
#191862 = AXIS2_PLACEMENT_3D ( 'NONE', #132407, #69884, #231516 ) ;
#191863 = CARTESIAN_POINT ( 'NONE',  ( 18.51024323315077069, 65.68895814178237913, -97.50265578621377927 ) ) ;
#191864 = ORIENTED_EDGE ( 'NONE', *, *, #209680, .F. ) ;
#191865 = CARTESIAN_POINT ( 'NONE',  ( 21.05000000000005400, 65.15000000001120384, -4.523107484524794053 ) ) ;
#191866 = DIRECTION ( 'NONE',  ( -0.000000000000000000, -0.7397360091702755991, -0.6728971962616832059 ) ) ;
#191867 = FACE_OUTER_BOUND ( 'NONE', #149480, .T. ) ;
#191868 = CARTESIAN_POINT ( 'NONE',  ( -20.54999999999999716, 85.00000000001232081, -160.1291383618718385 ) ) ;
#191869 = AXIS2_PLACEMENT_3D ( 'NONE', #214486, #115383, #194951 ) ;
#191870 = EDGE_CURVE ( 'NONE', #66650, #442, #91585, .T. ) ;
#191871 = DIRECTION ( 'NONE',  ( -1.000000000000000000, 0.000000000000000000, 0.000000000000000000 ) ) ;
#191872 = CARTESIAN_POINT ( 'NONE',  ( 18.43466021071411021, -9.494190690445394765, -73.61706156012773761 ) ) ;
#191873 = CARTESIAN_POINT ( 'NONE',  ( -20.00857864376270001, 22.43030315632513094, -231.3223027016406093 ) ) ;
#191874 = ORIENTED_EDGE ( 'NONE', *, *, #161570, .T. ) ;
#191875 = LINE ( 'NONE', #232278, #139662 ) ;
#191876 = ORIENTED_EDGE ( 'NONE', *, *, #192449, .T. ) ;
#191879 = VERTEX_POINT ( 'NONE', #216002 ) ;
#191878 = FACE_OUTER_BOUND ( 'NONE', #101362, .T. ) ;
#191877 = CARTESIAN_POINT ( 'NONE',  ( 18.59999999999999076, 18.24178995542692050, -237.7003448530951459 ) ) ;
#191880 = EDGE_LOOP ( 'NONE', ( #53339, #135276, #210111, #76559 ) ) ;
#191881 = CARTESIAN_POINT ( 'NONE',  ( -20.54999999999999716, 1.115600667400684642E-11, -200.9999999999999432 ) ) ;
#191882 = CARTESIAN_POINT ( 'NONE',  ( -21.14999999999999858, 6.540656951701240729, 0.000000000000000000 ) ) ;
#191883 = DIRECTION ( 'NONE',  ( 0.000000000000000000, 0.000000000000000000, -1.000000000000000000 ) ) ;
#191884 = EDGE_CURVE ( 'NONE', #9696, #229956, #257645, .T. ) ;
#191885 = CARTESIAN_POINT ( 'NONE',  ( 20.94999999999999574, 59.10678033798691189, -225.7992625810339575 ) ) ;
#191886 = ORIENTED_EDGE ( 'NONE', *, *, #238403, .T. ) ;
#191888 = VERTEX_POINT ( 'NONE', #195205 ) ;
#191887 = CARTESIAN_POINT ( 'NONE',  ( 20.95512820512820440, 67.12384868372450342, -194.9644784893834810 ) ) ;
#191889 = VECTOR ( 'NONE', #201370, 1000.000000000000000 ) ;
#191890 = EDGE_CURVE ( 'NONE', #52358, #75284, #141457, .T. ) ;
#191892 = DIRECTION ( 'NONE',  ( -1.000000000000000000, 0.000000000000000000, 0.000000000000000000 ) ) ;
#191891 = DIRECTION ( 'NONE',  ( -0.000000000000000000, 1.000000000000000000, -0.000000000000000000 ) ) ;
#191894 = ORIENTED_EDGE ( 'NONE', *, *, #220625, .F. ) ;
#191893 = DIRECTION ( 'NONE',  ( 0.000000000000000000, 0.000000000000000000, 1.000000000000000000 ) ) ;
#191895 = TOROIDAL_SURFACE ( 'NONE', #121167, 0.2000000000000000111, 0.1000000000000000056 ) ;
#191896 = ORIENTED_EDGE ( 'NONE', *, *, #190767, .T. ) ;
#191897 = CIRCLE ( 'NONE', #54483, 0.09999999999999982514 ) ;
#191899 = EDGE_CURVE ( 'NONE', #34148, #248047, #49880, .T. ) ;
#191898 = CARTESIAN_POINT ( 'NONE',  ( 20.95132126680579887, 11.86065605514014898, -206.1646587338731251 ) ) ;
#191900 = DIRECTION ( 'NONE',  ( 1.000000000000000000, 0.000000000000000000, 0.000000000000000000 ) ) ;
#191902 = EDGE_CURVE ( 'NONE', #254689, #109261, #104022, .T. ) ;
#191901 = EDGE_LOOP ( 'NONE', ( #83178, #61530, #75095 ) ) ;
#191903 = DIRECTION ( 'NONE',  ( 0.000000000000000000, 0.4999999999999689138, -0.8660254037844565822 ) ) ;
#191904 = ORIENTED_EDGE ( 'NONE', *, *, #178085, .F. ) ;
#191905 = AXIS2_PLACEMENT_3D ( 'NONE', #207754, #249443, #169942 ) ;
#191906 = DIRECTION ( 'NONE',  ( 0.000000000000000000, 0.000000000000000000, -1.000000000000000000 ) ) ;
#191907 = CARTESIAN_POINT ( 'NONE',  ( -18.79999999999999716, 5.488301202077012775, 16.40000000000000213 ) ) ;
#191908 = ORIENTED_EDGE ( 'NONE', *, *, #214551, .F. ) ;
#191909 = CARTESIAN_POINT ( 'NONE',  ( 18.49999999999996803, 68.92903212821255465, -32.27654326265606954 ) ) ;
#191910 = EDGE_CURVE ( 'NONE', #175346, #255664, #245702, .T. ) ;
#191911 = AXIS2_PLACEMENT_3D ( 'NONE', #120940, #126027, #161337 ) ;
#191912 = CARTESIAN_POINT ( 'NONE',  ( 21.87500000000000355, 9.750000000011153745, -54.75000000000000000 ) ) ;
#191914 = ADVANCED_FACE ( 'NONE', ( #76497 ), #252567, .T. ) ;
#191913 = AXIS2_PLACEMENT_3D ( 'NONE', #20254, #240576, #179340 ) ;
#191916 = ORIENTED_EDGE ( 'NONE', *, *, #156886, .T. ) ;
#191915 = AXIS2_PLACEMENT_3D ( 'NONE', #201121, #2907, #120346 ) ;
#191917 = VERTEX_POINT ( 'NONE', #58207 ) ;
#191918 = CARTESIAN_POINT ( 'NONE',  ( 20.97217846901852312, 18.81354558019653211, -229.9232606961761860 ) ) ;
#191919 = ORIENTED_EDGE ( 'NONE', *, *, #170342, .T. ) ;
#191920 = ADVANCED_FACE ( 'NONE', ( #217279 ), #197736, .F. ) ;
#191921 = DIRECTION ( 'NONE',  ( 0.000000000000000000, -0.9126074666063770380, -0.4088369013363281068 ) ) ;
#191922 = EDGE_LOOP ( 'NONE', ( #232903, #82386, #89695, #83095 ) ) ;
#191924 = ORIENTED_EDGE ( 'NONE', *, *, #3589, .F. ) ;
#191923 = CARTESIAN_POINT ( 'NONE',  ( 21.05000000000000071, 87.75000000001215028, -139.4231074845242802 ) ) ;
#191925 = AXIS2_PLACEMENT_3D ( 'NONE', #122327, #201859, #45353 ) ;
#191926 = AXIS2_PLACEMENT_3D ( 'NONE', #34689, #16410, #95909 ) ;
#191927 = ORIENTED_EDGE ( 'NONE', *, *, #208223, .F. ) ;
#191928 = FACE_OUTER_BOUND ( 'NONE', #49271, .T. ) ;
#191930 = VERTEX_POINT ( 'NONE', #62085 ) ;
#191929 = EDGE_CURVE ( 'NONE', #221470, #228853, #124627, .T. ) ;
#191933 = ORIENTED_EDGE ( 'NONE', *, *, #135292, .F. ) ;
#191932 = ORIENTED_EDGE ( 'NONE', *, *, #126569, .F. ) ;
#191931 = FACE_OUTER_BOUND ( 'NONE', #234442, .T. ) ;
#191934 = EDGE_CURVE ( 'NONE', #66731, #188219, #83163, .T. ) ;
#191935 = DIRECTION ( 'NONE',  ( -1.000000000000000000, 7.510212038922875604E-17, -1.676432719286210708E-16 ) ) ;
#191936 = ORIENTED_EDGE ( 'NONE', *, *, #51602, .F. ) ;
#191937 = VECTOR ( 'NONE', #57453, 1000.000000000000000 ) ;
#191938 = CIRCLE ( 'NONE', #54330, 0.09999999999999939493 ) ;
#191939 = AXIS2_PLACEMENT_3D ( 'NONE', #135232, #156130, #15326 ) ;
#191940 = AXIS2_PLACEMENT_3D ( 'NONE', #106699, #62466, #7622 ) ;
#191941 = CARTESIAN_POINT ( 'NONE',  ( 23.15000000000000213, -9.499999999988844479, -57.10603087734755690 ) ) ;
#191942 = ORIENTED_EDGE ( 'NONE', *, *, #24372, .T. ) ;
#191943 = CARTESIAN_POINT ( 'NONE',  ( -16.93415306273742260, 9.995622260023671046, -154.9100569423604270 ) ) ;
#191945 = VERTEX_POINT ( 'NONE', #222402 ) ;
#191944 = DIRECTION ( 'NONE',  ( 2.952720810173289112E-16, 0.4088369013363266635, -0.9126074666063777041 ) ) ;
#191946 = CARTESIAN_POINT ( 'NONE',  ( 20.94999999999999929, -8.999999999988844479, -76.89396912265249284 ) ) ;
#191947 = VERTEX_POINT ( 'NONE', #183316 ) ;
#191948 = ADVANCED_FACE ( 'NONE', ( #224978 ), #2090, .T. ) ;
#191949 = FACE_OUTER_BOUND ( 'NONE', #242468, .T. ) ;
#191950 = ADVANCED_FACE ( 'NONE', ( #244558 ), #112446, .T. ) ;
#191951 = ORIENTED_EDGE ( 'NONE', *, *, #97972, .F. ) ;
#191952 = CARTESIAN_POINT ( 'NONE',  ( -1.820710678118657944, 85.92928932189330737, -111.7731074845242176 ) ) ;
#191953 = CARTESIAN_POINT ( 'NONE',  ( -20.93284271247462058, 64.25000000001220712, -143.5379132551784096 ) ) ;
#191954 = EDGE_LOOP ( 'NONE', ( #112570, #18262, #179760 ) ) ;
#191956 = EDGE_LOOP ( 'NONE', ( #140844, #225516, #152141, #244141 ) ) ;
#191955 = CARTESIAN_POINT ( 'NONE',  ( -22.45437739390954590, 76.00000000001222134, -148.1726782961185052 ) ) ;
#191957 = DIRECTION ( 'NONE',  ( 1.000000000000000000, 0.000000000000000000, 0.000000000000000000 ) ) ;
#191959 = ORIENTED_EDGE ( 'NONE', *, *, #59360, .F. ) ;
#191958 = ORIENTED_EDGE ( 'NONE', *, *, #130729, .F. ) ;
#191960 = ORIENTED_EDGE ( 'NONE', *, *, #257733, .F. ) ;
#191961 = DIRECTION ( 'NONE',  ( 0.000000000000000000, -0.9915357197604892647, 0.1298341882519715440 ) ) ;
#191962 = ORIENTED_EDGE ( 'NONE', *, *, #205901, .F. ) ;
#191963 = ORIENTED_EDGE ( 'NONE', *, *, #131381, .T. ) ;
#191964 = ORIENTED_EDGE ( 'NONE', *, *, #29248, .T. ) ;
#191965 = DIRECTION ( 'NONE',  ( 0.000000000000000000, 0.000000000000000000, 1.000000000000000000 ) ) ;
#191966 = DIRECTION ( 'NONE',  ( 1.000000000000000000, 0.000000000000000000, 0.000000000000000000 ) ) ;
#191967 = VERTEX_POINT ( 'NONE', #22987 ) ;
#191968 = ORIENTED_EDGE ( 'NONE', *, *, #226588, .T. ) ;
#191969 = CARTESIAN_POINT ( 'NONE',  ( -23.25000000000000000, -11.74999999998884448, -103.6000000000000369 ) ) ;
#191970 = VERTEX_POINT ( 'NONE', #145454 ) ;
#191971 = TOROIDAL_SURFACE ( 'NONE', #25376, 0.2000000000000000111, 0.1000000000000000056 ) ;
#191972 = EDGE_CURVE ( 'NONE', #11734, #201436, #16590, .T. ) ;
#191973 = AXIS2_PLACEMENT_3D ( 'NONE', #199060, #38708, #42539 ) ;
#191974 = LINE ( 'NONE', #151568, #222149 ) ;
#191975 = ORIENTED_EDGE ( 'NONE', *, *, #167872, .F. ) ;
#191976 = ORIENTED_EDGE ( 'NONE', *, *, #65002, .T. ) ;
#191977 = DIRECTION ( 'NONE',  ( 0.000000000000000000, 0.8454177738465993297, 0.5341055959866553016 ) ) ;
#191979 = ORIENTED_EDGE ( 'NONE', *, *, #164098, .F. ) ;
#191978 = CARTESIAN_POINT ( 'NONE',  ( 18.40000000000000568, 85.51932773110476660, -163.0501311079649724 ) ) ;
#191980 = CARTESIAN_POINT ( 'NONE',  ( 21.12230431290518595, 0.005209851700164400135, -127.5424333467069857 ) ) ;
#191981 = CARTESIAN_POINT ( 'NONE',  ( -20.54999999999999716, 76.00000000001213607, -136.5231074845243313 ) ) ;
#191982 = CARTESIAN_POINT ( 'NONE',  ( 20.94999999999999574, 65.52661458509918191, -128.9444530202758301 ) ) ;
#191983 = CYLINDRICAL_SURFACE ( 'NONE', #57965, 0.1000000000000026007 ) ;
#191984 = LINE ( 'NONE', #150276, #90295 ) ;
#191985 = CARTESIAN_POINT ( 'NONE',  ( 19.97071067811864609, 11.72071067812981404, -58.15000000000000568 ) ) ;
#191986 = DIRECTION ( 'NONE',  ( 0.000000000000000000, 0.000000000000000000, 1.000000000000000000 ) ) ;
#191987 = CARTESIAN_POINT ( 'NONE',  ( 20.94999999999999929, -8.663551401857999323, -157.9758988819327215 ) ) ;
#191988 = CARTESIAN_POINT ( 'NONE',  ( 18.50000000000000355, 38.30077178631847801, -261.1858881914067183 ) ) ;
#191989 = CARTESIAN_POINT ( 'NONE',  ( -6.100000000000006750, -11.75000000000000000, 10.10000000000000142 ) ) ;
#191990 = FACE_OUTER_BOUND ( 'NONE', #138311, .T. ) ;
#191991 = EDGE_CURVE ( 'NONE', #140686, #89189, #164713, .T. ) ;
#191992 = VERTEX_POINT ( 'NONE', #80324 ) ;
#191993 = AXIS2_PLACEMENT_3D ( 'NONE', #99909, #235592, #137768 ) ;
#191994 = CIRCLE ( 'NONE', #196237, 0.1000000000000028644 ) ;
#191996 = ORIENTED_EDGE ( 'NONE', *, *, #183556, .T. ) ;
#191995 = ORIENTED_EDGE ( 'NONE', *, *, #219423, .T. ) ;
#191997 = ORIENTED_EDGE ( 'NONE', *, *, #253132, .F. ) ;
#191998 = CARTESIAN_POINT ( 'NONE',  ( 21.07946286933444924, 75.92331615675632861, -209.8521448035321555 ) ) ;
#191999 = CARTESIAN_POINT ( 'NONE',  ( 20.94999999999999929, 71.00000000001260503, -191.1178414656112921 ) ) ;
#192001 = DIRECTION ( 'NONE',  ( -0.000000000000000000, -0.9126074666063770380, -0.4088369013363281068 ) ) ;
#192000 = CARTESIAN_POINT ( 'NONE',  ( -21.05000000000000071, 87.48912529308749697, -39.12310748452424747 ) ) ;
#192002 = EDGE_LOOP ( 'NONE', ( #207895, #98733, #136345, #144003 ) ) ;
#192003 = ORIENTED_EDGE ( 'NONE', *, *, #125960, .F. ) ;
#192004 = B_SPLINE_CURVE_WITH_KNOTS ( 'NONE', 3,
 ( #170501, #212152, #113042, #209577 ),
 .UNSPECIFIED., .F., .F.,
 ( 4, 4 ),
 ( 0.000000000000000000, 0.0001048066582182386071 ),
 .UNSPECIFIED. ) ;
#192005 = DIRECTION ( 'NONE',  ( -0.000000000000000000, 1.000000000000000000, 7.272083257015735086E-15 ) ) ;
#192007 = CIRCLE ( 'NONE', #46225, 7.900000000000003908 ) ;
#192006 = DIRECTION ( 'NONE',  ( 1.000000000000000000, 0.000000000000000000, 0.000000000000000000 ) ) ;
#192008 = CARTESIAN_POINT ( 'NONE',  ( -22.50000000000000000, 36.65892442174472876, -249.5511627012454596 ) ) ;
#192009 = ORIENTED_EDGE ( 'NONE', *, *, #33811, .T. ) ;
#192010 = ORIENTED_EDGE ( 'NONE', *, *, #208697, .F. ) ;
#192011 = CARTESIAN_POINT ( 'NONE',  ( 23.40000000000005542, 82.74366731733570646, -26.36310895752070138 ) ) ;
#192012 = FACE_OUTER_BOUND ( 'NONE', #93011, .T. ) ;
#192013 = FACE_OUTER_BOUND ( 'NONE', #168363, .T. ) ;
#192015 = ORIENTED_EDGE ( 'NONE', *, *, #133541, .T. ) ;
#192014 = CARTESIAN_POINT ( 'NONE',  ( 21.05000000000000071, 11.65000000001116298, -167.4999999999999716 ) ) ;
#192016 = CARTESIAN_POINT ( 'NONE',  ( -21.00000000000000000, -0.04453801223857078301, 0.3305886640091971196 ) ) ;
#192017 = DIRECTION ( 'NONE',  ( 0.000000000000000000, -0.1350103645451974088, 0.9908441862701587999 ) ) ;
#192018 = CARTESIAN_POINT ( 'NONE',  ( 20.95000000000005258, 65.35000000001120668, -4.523107484524794053 ) ) ;
#192019 = EDGE_LOOP ( 'NONE', ( #236797, #164380, #150417, #124017 ) ) ;
#192020 = DIRECTION ( 'NONE',  ( 2.879366945564059217E-14, -0.9875055080513751582, 0.1575844902526747915 ) ) ;
#192021 = DIRECTION ( 'NONE',  ( 1.000000000000000000, 0.000000000000000000, 0.000000000000000000 ) ) ;
#192022 = DIRECTION ( 'NONE',  ( 0.000000000000000000, 0.000000000000000000, -1.000000000000000000 ) ) ;
#192025 = FACE_OUTER_BOUND ( 'NONE', #106932, .T. ) ;
#192024 = CIRCLE ( 'NONE', #191855, 0.1000000000000028644 ) ;
#192023 = LINE ( 'NONE', #94171, #124335 ) ;
#192027 = FACE_OUTER_BOUND ( 'NONE', #31186, .T. ) ;
#192026 = AXIS2_PLACEMENT_3D ( 'NONE', #64458, #145254, #185687 ) ;
#192029 = EDGE_CURVE ( 'NONE', #106650, #223391, #4095, .T. ) ;
#192028 = DIRECTION ( 'NONE',  ( 0.000000000000000000, -6.467318590049456648E-15, 1.000000000000000000 ) ) ;
#192030 = AXIS2_PLACEMENT_3D ( 'NONE', #34280, #74699, #77209 ) ;
#192031 = CARTESIAN_POINT ( 'NONE',  ( 21.05000000000000071, 76.00000000001172396, -71.42310748452430857 ) ) ;
#192032 = CARTESIAN_POINT ( 'NONE',  ( -23.25000000000000000, 1.115600667400684642E-11, -100.5000000000000284 ) ) ;
#192033 = CARTESIAN_POINT ( 'NONE',  ( 12.25000000000000000, 66.15000000001185754, -86.27310748452437394 ) ) ;
#192034 = ORIENTED_EDGE ( 'NONE', *, *, #153644, .T. ) ;
#192035 = CIRCLE ( 'NONE', #29539, 11.75000000000000533 ) ;
#192036 = ORIENTED_EDGE ( 'NONE', *, *, #140570, .T. ) ;
#192037 = ORIENTED_EDGE ( 'NONE', *, *, #76956, .F. ) ;
#192038 = EDGE_CURVE ( 'NONE', #254024, #44597, #179103, .T. ) ;
#192039 = CARTESIAN_POINT ( 'NONE',  ( 20.94999999999999929, 84.73084112150681335, -45.62118220350859588 ) ) ;
#192040 = DIRECTION ( 'NONE',  ( 1.000000000000000000, 0.000000000000000000, 0.000000000000000000 ) ) ;
#192041 = ORIENTED_EDGE ( 'NONE', *, *, #239697, .F. ) ;
#192042 = EDGE_CURVE ( 'NONE', #107953, #189223, #28038, .T. ) ;
#192043 = CARTESIAN_POINT ( 'NONE',  ( -21.05000000000000071, 86.43238724539048690, -209.5644480942280836 ) ) ;
#192044 = CIRCLE ( 'NONE', #133741, 0.9750000000000036415 ) ;
#192045 = ORIENTED_EDGE ( 'NONE', *, *, #35870, .F. ) ;
#192046 = EDGE_CURVE ( 'NONE', #64807, #119168, #133105, .T. ) ;
#192047 = VERTEX_POINT ( 'NONE', #149344 ) ;
#192048 = CARTESIAN_POINT ( 'NONE',  ( 20.94999999999999574, 43.57568952063339651, -245.1784935019914826 ) ) ;
#192049 = ORIENTED_EDGE ( 'NONE', *, *, #198337, .T. ) ;
#192050 = DIRECTION ( 'NONE',  ( 0.000000000000000000, 0.2128009952263403282, -0.9770955615653358350 ) ) ;
#192051 = DIRECTION ( 'NONE',  ( -7.304098846218134667E-16, 1.000000000000000000, 6.982962677686266711E-15 ) ) ;
#192052 = CARTESIAN_POINT ( 'NONE',  ( -20.85000000000000142, 43.08613539620618837, -254.3146655184800409 ) ) ;
#192053 = CARTESIAN_POINT ( 'NONE',  ( -23.25000000000000000, 36.65892442174935439, -249.5511627012433848 ) ) ;
#192054 = CARTESIAN_POINT ( 'NONE',  ( 20.85000000000000142, -1.362429037182151470, -208.8888812479211765 ) ) ;
#192056 = EDGE_LOOP ( 'NONE', ( #187001, #231703, #228063, #215940 ) ) ;
#192055 = CARTESIAN_POINT ( 'NONE',  ( -16.77308656112213825, 30.20615826255785663, -234.8069537810542613 ) ) ;
#192057 = LINE ( 'NONE', #73405, #233715 ) ;
#192058 = ADVANCED_FACE ( 'NONE', ( #67214 ), #24973, .T. ) ;
#192060 = CARTESIAN_POINT ( 'NONE',  ( -16.87036670365548474, 9.989418819312801290, -154.9795601173020714 ) ) ;
#192059 = AXIS2_PLACEMENT_3D ( 'NONE', #186981, #167412, #5714 ) ;
#192061 = DIRECTION ( 'NONE',  ( 0.000000000000000000, -1.000000000000000000, 0.000000000000000000 ) ) ;
#192062 = DIRECTION ( 'NONE',  ( -0.000000000000000000, -6.982962677686266711E-15, 1.000000000000000000 ) ) ;
#192063 = LINE ( 'NONE', #34285, #16751 ) ;
#192064 = VERTEX_POINT ( 'NONE', #148041 ) ;
#192065 = TOROIDAL_SURFACE ( 'NONE', #475, 0.2000000000000000111, 0.1000000000000000056 ) ;
#192066 = DIRECTION ( 'NONE',  ( 0.000000000000000000, -1.000000000000000000, 0.000000000000000000 ) ) ;
#192067 = EDGE_LOOP ( 'NONE', ( #113932, #16000, #36994, #140103 ) ) ;
#192068 = AXIS2_PLACEMENT_3D ( 'NONE', #52977, #112969, #13866 ) ;
#192069 = DIRECTION ( 'NONE',  ( 0.000000000000000000, 1.000000000000000000, 6.982962677686267499E-15 ) ) ;
#192070 = ORIENTED_EDGE ( 'NONE', *, *, #205065, .T. ) ;
#192071 = DIRECTION ( 'NONE',  ( 0.000000000000000000, 0.2617529984165152257, 0.9651348961777124202 ) ) ;
#192072 = DIRECTION ( 'NONE',  ( 1.000000000000000000, 0.000000000000000000, 0.000000000000000000 ) ) ;
#192073 = VERTEX_POINT ( 'NONE', #127196 ) ;
#192074 = EDGE_LOOP ( 'NONE', ( #54272, #94735, #211605, #33641 ) ) ;
#192075 = TOROIDAL_SURFACE ( 'NONE', #100448, 11.65000000000000036, 0.1000000000000000056 ) ;
#192076 = CARTESIAN_POINT ( 'NONE',  ( -21.65000000000000213, 68.75000000001189449, -93.77310748452435973 ) ) ;
#192077 = CARTESIAN_POINT ( 'NONE',  ( -21.14999999999999858, -0.09999999998884338825, -155.8504291924551808 ) ) ;
#192078 = DIRECTION ( 'NONE',  ( -1.000000000000000000, 0.000000000000000000, 0.000000000000000000 ) ) ;
#192079 = CARTESIAN_POINT ( 'NONE',  ( -16.92778301347301451, 65.99905508317638692, -90.45162559249260426 ) ) ;
#192081 = CARTESIAN_POINT ( 'NONE',  ( 18.59999999999999432, 44.52640028187936849, -247.3006740988509193 ) ) ;
#192080 = DIRECTION ( 'NONE',  ( 0.000000000000000000, -1.000000000000000000, -0.000000000000000000 ) ) ;
#192082 = AXIS2_PLACEMENT_3D ( 'NONE', #133736, #93325, #154625 ) ;
#192084 = MANIFOLD_SOLID_BREP ( 'Stock-MAS-200-1', #203484 ) ;
#192083 = CARTESIAN_POINT ( 'NONE',  ( 21.05000000000000071, 14.05000000001115623, -161.9863049292391111 ) ) ;
#192085 = CARTESIAN_POINT ( 'NONE',  ( 15.57250062127603307, 9.370689921613767126, -51.02646512666105849 ) ) ;
#192086 = CARTESIAN_POINT ( 'NONE',  ( -18.59999999999999787, 78.12133356376091342, -231.3112718935514636 ) ) ;
#192087 = VERTEX_POINT ( 'NONE', #129753 ) ;
#192088 = LINE ( 'NONE', #155546, #31552 ) ;
#192089 = EDGE_CURVE ( 'NONE', #91918, #248466, #6298, .T. ) ;
#192091 = VERTEX_POINT ( 'NONE', #30685 ) ;
#192090 = DIRECTION ( 'NONE',  ( 0.000000000000000000, 0.000000000000000000, -1.000000000000000000 ) ) ;
#192092 = FACE_BOUND ( 'NONE', #201444, .T. ) ;
#192093 = CARTESIAN_POINT ( 'NONE',  ( -23.25000000000000000, 0.000000000000000000, 0.000000000000000000 ) ) ;
#192095 = CARTESIAN_POINT ( 'NONE',  ( 20.94999999999999929, 76.00000000001170974, -69.52310748452431710 ) ) ;
#192094 = DIRECTION ( 'NONE',  ( -1.000000000000000000, -0.000000000000000000, 0.000000000000000000 ) ) ;
#192096 = AXIS2_PLACEMENT_3D ( 'NONE', #139440, #100310, #160339 ) ;
#192097 = DIRECTION ( 'NONE',  ( 1.000000000000000000, 0.000000000000000000, 0.000000000000000000 ) ) ;
#192099 = ORIENTED_EDGE ( 'NONE', *, *, #127025, .F. ) ;
#192098 = CARTESIAN_POINT ( 'NONE',  ( -23.15000000000000213, -3.770473190032741062, -225.9805569534692324 ) ) ;
#192100 = CARTESIAN_POINT ( 'NONE',  ( 20.05000000000002913, 7.250000000011171508, -42.75000000000000000 ) ) ;
#192101 = CARTESIAN_POINT ( 'NONE',  ( -16.90138253750126296, 51.49252402576821197, -232.0030672891792847 ) ) ;
#192102 = CARTESIAN_POINT ( 'NONE',  ( 20.94999999999999574, -11.48912529306490349, -69.90000000000004832 ) ) ;
#192103 = DIRECTION ( 'NONE',  ( 0.000000000000000000, 0.000000000000000000, -1.000000000000000000 ) ) ;
#192106 = EDGE_CURVE ( 'NONE', #238459, #137271, #88030, .T. ) ;
#192105 = CARTESIAN_POINT ( 'NONE',  ( -18.43707690579160641, 85.68240343348828958, -96.36626410711146207 ) ) ;
#192104 = AXIS2_PLACEMENT_3D ( 'NONE', #253411, #74822, #190911 ) ;
#192107 = ORIENTED_EDGE ( 'NONE', *, *, #94129, .F. ) ;
#192108 = SPHERICAL_SURFACE ( 'NONE', #230478, 0.1000000000000000056 ) ;
#192109 = ORIENTED_EDGE ( 'NONE', *, *, #83734, .F. ) ;
#192110 = EDGE_CURVE ( 'NONE', #177470, #15173, #37434, .T. ) ;
#192111 = EDGE_CURVE ( 'NONE', #70952, #4561, #108165, .T. ) ;
#192112 = EDGE_LOOP ( 'NONE', ( #10428, #116321, #183137, #131203 ) ) ;
#192114 = CARTESIAN_POINT ( 'NONE',  ( -23.25000000000000000, 4.959819536546777642E-16, 4.049999999999998934 ) ) ;
#192113 = TOROIDAL_SURFACE ( 'NONE', #71304, 0.2000000000000000111, 0.1000000000000000056 ) ;
#192115 = TOROIDAL_SURFACE ( 'NONE', #79633, 0.6000000000000004219, 0.1000000000000000056 ) ;
#192116 = VECTOR ( 'NONE', #88092, 1000.000000000000000 ) ;
#192117 = VERTEX_POINT ( 'NONE', #249705 ) ;
#192118 = AXIS2_PLACEMENT_3D ( 'NONE', #34987, #153671, #235701 ) ;
#192119 = FACE_OUTER_BOUND ( 'NONE', #46916, .T. ) ;
#192120 = CARTESIAN_POINT ( 'NONE',  ( 23.14999999999999503, 69.35000000001186038, -90.77310748452435973 ) ) ;
#192121 = EDGE_CURVE ( 'NONE', #234345, #32328, #162329, .T. ) ;
#192122 = CARTESIAN_POINT ( 'NONE',  ( -20.64999999999999858, 76.00000000001244871, -170.0231074845243597 ) ) ;
#192123 = ORIENTED_EDGE ( 'NONE', *, *, #37960, .T. ) ;
#192124 = ADVANCED_FACE ( 'NONE', ( #194884 ), #231441, .T. ) ;
#192125 = EDGE_CURVE ( 'NONE', #249345, #50955, #216476, .T. ) ;
#192126 = CARTESIAN_POINT ( 'NONE',  ( -16.77308656112214891, 9.949999999999979750, -12.65019319170230716 ) ) ;
#192127 = CARTESIAN_POINT ( 'NONE',  ( 21.05000000000000071, 5.000000000011153745, -88.09473398108696074 ) ) ;
#192128 = CARTESIAN_POINT ( 'NONE',  ( -20.64999999999999858, 2.000000000011154189, -180.7246219227620543 ) ) ;
#192129 = CARTESIAN_POINT ( 'NONE',  ( 21.76363531954645936, 6.831241477096051895, -199.4109058311904619 ) ) ;
#192130 = DIRECTION ( 'NONE',  ( 0.000000000000000000, -0.09425075112713271475, -0.9955484899852801162 ) ) ;
#192131 = ORIENTED_EDGE ( 'NONE', *, *, #19944, .F. ) ;
#192132 = DIRECTION ( 'NONE',  ( 0.000000000000000000, 0.000000000000000000, 1.000000000000000000 ) ) ;
#192133 = ORIENTED_EDGE ( 'NONE', *, *, #27936, .T. ) ;
#192135 = ORIENTED_EDGE ( 'NONE', *, *, #1863, .T. ) ;
#192134 = CARTESIAN_POINT ( 'NONE',  ( 21.05543885634738643, 67.22422895316432800, -90.83872301380968395 ) ) ;
#192136 = ADVANCED_FACE ( 'NONE', ( #95740 ), #17500, .F. ) ;
#192137 = EDGE_LOOP ( 'NONE', ( #119838, #226536, #243853, #93971 ) ) ;
#192138 = CARTESIAN_POINT ( 'NONE',  ( 20.94999999999999929, 70.60000000001157616, -57.11784146561126363 ) ) ;
#192139 = FACE_OUTER_BOUND ( 'NONE', #98515, .T. ) ;
#192140 = CARTESIAN_POINT ( 'NONE',  ( 22.47007471830798053, 1.115784124149148083E-11, -25.77928934807354722 ) ) ;
#192141 = EDGE_CURVE ( 'NONE', #79398, #156548, #154491, .T. ) ;
#192142 = CARTESIAN_POINT ( 'NONE',  ( -20.54999999999999716, 76.00000000001190870, -103.0231074845243029 ) ) ;
#192143 = ORIENTED_EDGE ( 'NONE', *, *, #241072, .F. ) ;
#192144 = EDGE_CURVE ( 'NONE', #207209, #59363, #53033, .T. ) ;
#192145 = EDGE_CURVE ( 'NONE', #44901, #2619, #14960, .T. ) ;
#192146 = DIRECTION ( 'NONE',  ( 0.000000000000000000, 0.000000000000000000, -1.000000000000000000 ) ) ;
#192147 = DIRECTION ( 'NONE',  ( 0.000000000000000000, 0.000000000000000000, -1.000000000000000000 ) ) ;
#192149 = ORIENTED_EDGE ( 'NONE', *, *, #212566, .T. ) ;
#192148 = CIRCLE ( 'NONE', #225413, 0.1000000000000000472 ) ;
#192151 = EDGE_LOOP ( 'NONE', ( #152211, #185386, #111756, #227869 ) ) ;
#192150 = LINE ( 'NONE', #175181, #30166 ) ;
#192152 = FACE_OUTER_BOUND ( 'NONE', #226641, .T. ) ;
#192153 = DIRECTION ( 'NONE',  ( -1.000000000000000000, 0.000000000000000000, 0.000000000000000000 ) ) ;
#192154 = CARTESIAN_POINT ( 'NONE',  ( 20.94999999999999574, 87.48912529308842068, -166.9231074845242802 ) ) ;
#192155 = ORIENTED_EDGE ( 'NONE', *, *, #59452, .F. ) ;
#192156 = ORIENTED_EDGE ( 'NONE', *, *, #165984, .T. ) ;
#192157 = LINE ( 'NONE', #108743, #10445 ) ;
#192158 = AXIS2_PLACEMENT_3D ( 'NONE', #116641, #155799, #235295 ) ;
#192159 = CARTESIAN_POINT ( 'NONE',  ( -6.000000000000002665, -11.34999999999999964, 13.90000000000000213 ) ) ;
#192160 = ORIENTED_EDGE ( 'NONE', *, *, #225261, .F. ) ;
#192161 = DIRECTION ( 'NONE',  ( 1.000000000000000000, -1.335000415235278971E-16, 2.979993593738921214E-16 ) ) ;
#192162 = EDGE_CURVE ( 'NONE', #67785, #110689, #112095, .T. ) ;
#192163 = EDGE_CURVE ( 'NONE', #67428, #6622, #35813, .T. ) ;
#192164 = SPHERICAL_SURFACE ( 'NONE', #176507, 0.1000000000000000056 ) ;
#192165 = DIRECTION ( 'NONE',  ( 0.000000000000000000, 0.9915357197604973694, -0.1298341882519105928 ) ) ;
#192166 = ADVANCED_FACE ( 'NONE', ( #74945 ), #133597, .T. ) ;
#192167 = VECTOR ( 'NONE', #221186, 1000.000000000000000 ) ;
#192168 = CIRCLE ( 'NONE', #129610, 0.09999999999999939493 ) ;
#192170 = ORIENTED_EDGE ( 'NONE', *, *, #188476, .T. ) ;
#192169 = AXIS2_PLACEMENT_3D ( 'NONE', #200126, #59277, #197540 ) ;
#192171 = CARTESIAN_POINT ( 'NONE',  ( 21.04999999999999716, 67.12791932463382238, -61.00206006569352013 ) ) ;
#192172 = EDGE_LOOP ( 'NONE', ( #176044, #17184, #200857, #179124 ) ) ;
#192173 = DIRECTION ( 'NONE',  ( 1.000000000000000000, -0.000000000000000000, 0.000000000000000000 ) ) ;
#192174 = DIRECTION ( 'NONE',  ( 1.000000000000000000, 0.000000000000000000, 0.000000000000000000 ) ) ;
#192176 = VERTEX_POINT ( 'NONE', #136139 ) ;
#192175 = CARTESIAN_POINT ( 'NONE',  ( -23.25000000000000000, 71.85000000001198828, -115.3731074845243256 ) ) ;
#192177 = DIRECTION ( 'NONE',  ( 1.000000000000000000, 0.000000000000000000, 0.000000000000000000 ) ) ;
#192178 = DIRECTION ( 'NONE',  ( -1.000000000000000000, 0.000000000000000000, 0.000000000000000000 ) ) ;
#192179 = CARTESIAN_POINT ( 'NONE',  ( 23.24999999999999289, 11.65000000000000746, -26.48519422934606027 ) ) ;
#192180 = DIRECTION ( 'NONE',  ( -1.000000000000000000, 7.136802563874200093E-16, 1.554319503706930238E-16 ) ) ;
#192181 = DIRECTION ( 'NONE',  ( 0.000000000000000000, -6.938893903907222067E-15, -1.000000000000000000 ) ) ;
#192182 = EDGE_CURVE ( 'NONE', #157060, #138430, #254783, .T. ) ;
#192183 = CARTESIAN_POINT ( 'NONE',  ( -18.50000000000000000, 85.50000000001209344, -128.4231074845242233 ) ) ;
#192184 = CARTESIAN_POINT ( 'NONE',  ( 21.10320863425824811, 6.400277386470322405, -66.97497774877291477 ) ) ;
#192186 = ORIENTED_EDGE ( 'NONE', *, *, #236248, .F. ) ;
#192185 = CARTESIAN_POINT ( 'NONE',  ( -23.15000000000000213, 32.87160343532826801, -251.2478358417912148 ) ) ;
#192187 = AXIS2_PLACEMENT_3D ( 'NONE', #190626, #133202, #172374 ) ;
#192188 = EDGE_CURVE ( 'NONE', #196796, #97301, #55313, .T. ) ;
#192190 = ADVANCED_FACE ( 'NONE', ( #97003 ), #229140, .F. ) ;
#192189 = DIRECTION ( 'NONE',  ( 1.000000000000000000, -0.000000000000000000, 0.000000000000000000 ) ) ;
#192191 = EDGE_CURVE ( 'NONE', #85468, #74786, #116609, .T. ) ;
#192192 = DIRECTION ( 'NONE',  ( 0.000000000000000000, 0.000000000000000000, -1.000000000000000000 ) ) ;
#192193 = LINE ( 'NONE', #150492, #30753 ) ;
#192194 = EDGE_CURVE ( 'NONE', #190470, #93357, #175026, .T. ) ;
#192195 = ORIENTED_EDGE ( 'NONE', *, *, #212347, .T. ) ;
#192196 = CARTESIAN_POINT ( 'NONE',  ( -20.65000000000000568, 68.75000000001207923, -123.8731074845243540 ) ) ;
#192197 = AXIS2_PLACEMENT_3D ( 'NONE', #184493, #227474, #247034 ) ;
#192198 = CIRCLE ( 'NONE', #79734, 0.1000000000000124678 ) ;
#192199 = FACE_OUTER_BOUND ( 'NONE', #91880, .T. ) ;
#192200 = DIRECTION ( 'NONE',  ( 0.000000000000000000, -0.8660254037844383745, 0.5000000000000003331 ) ) ;
#192201 = AXIS2_PLACEMENT_3D ( 'NONE', #873, #21769, #225062 ) ;
#192202 = ORIENTED_EDGE ( 'NONE', *, *, #147127, .F. ) ;
#192204 = EDGE_CURVE ( 'NONE', #15753, #168569, #191761, .T. ) ;
#192203 = FACE_OUTER_BOUND ( 'NONE', #13598, .T. ) ;
#192205 = ADVANCED_FACE ( 'NONE', ( #140002 ), #180440, .T. ) ;
#192206 = LINE ( 'NONE', #9689, #184572 ) ;
#192207 = ORIENTED_EDGE ( 'NONE', *, *, #140415, .F. ) ;
#192208 = CARTESIAN_POINT ( 'NONE',  ( 21.05000000000000071, -8.999999999988844479, -76.89396912265249284 ) ) ;
#192209 = VERTEX_POINT ( 'NONE', #179183 ) ;
#192210 = ADVANCED_FACE ( 'NONE', ( #80013 ), #79272, .F. ) ;
#192211 = CARTESIAN_POINT ( 'NONE',  ( 20.97468175916167255, 65.37473483564103560, -124.2683460491115852 ) ) ;
#192212 = ORIENTED_EDGE ( 'NONE', *, *, #165048, .T. ) ;
#192213 = AXIS2_PLACEMENT_3D ( 'NONE', #42622, #97429, #21793 ) ;
#192214 = DIRECTION ( 'NONE',  ( 0.000000000000000000, 0.000000000000000000, -1.000000000000000000 ) ) ;
#192215 = ORIENTED_EDGE ( 'NONE', *, *, #120904, .F. ) ;
#192216 = DIRECTION ( 'NONE',  ( 1.284434275755705789E-16, -0.7071067811865472397, -0.7071067811865479058 ) ) ;
#192217 = EDGE_LOOP ( 'NONE', ( #102816, #26711, #132301, #210860 ) ) ;
#192219 = ORIENTED_EDGE ( 'NONE', *, *, #116265, .T. ) ;
#192218 = EDGE_LOOP ( 'NONE', ( #19465, #3399, #21674, #245578 ) ) ;
#192221 = ORIENTED_EDGE ( 'NONE', *, *, #98583, .F. ) ;
#192220 = FACE_OUTER_BOUND ( 'NONE', #240611, .T. ) ;
#192222 = ADVANCED_FACE ( 'NONE', ( #22673 ), #16778, .T. ) ;
#192223 = DIRECTION ( 'NONE',  ( -1.000000000000000000, 0.000000000000000000, 0.000000000000000000 ) ) ;
#192224 = ORIENTED_EDGE ( 'NONE', *, *, #186124, .F. ) ;
#192225 = EDGE_CURVE ( 'NONE', #148648, #221167, #58420, .T. ) ;
#192226 = ORIENTED_EDGE ( 'NONE', *, *, #225001, .T. ) ;
#192227 = CARTESIAN_POINT ( 'NONE',  ( -18.40000000000000213, 11.47316190336247388, -12.55000000000000249 ) ) ;
#192229 = DIRECTION ( 'NONE',  ( 1.000000000000000000, 0.000000000000000000, 0.000000000000000000 ) ) ;
#192228 = AXIS2_PLACEMENT_3D ( 'NONE', #86735, #166336, #245839 ) ;
#192231 = ADVANCED_FACE ( 'NONE', ( #141309 ), #202568, .F. ) ;
#192230 = CARTESIAN_POINT ( 'NONE',  ( 18.59999999999999787, -1.835341550213255957, -145.5551512925629822 ) ) ;
#192232 = VERTEX_POINT ( 'NONE', #223396 ) ;
#192233 = DIRECTION ( 'NONE',  ( -0.000000000000000000, 0.8814952561688430555, -0.4721928772777346239 ) ) ;
#192234 = CARTESIAN_POINT ( 'NONE',  ( 21.05000012384952512, 65.37127970113704123, -57.34513015448907680 ) ) ;
#192235 = EDGE_CURVE ( 'NONE', #52715, #58661, #225010, .T. ) ;
#192236 = DIRECTION ( 'NONE',  ( 0.000000000000000000, -1.000000000000000000, 0.000000000000000000 ) ) ;
#192237 = TOROIDAL_SURFACE ( 'NONE', #21542, 0.4000000000000012990, 0.1000000000000000056 ) ;
#192238 = ORIENTED_EDGE ( 'NONE', *, *, #178440, .T. ) ;
#192239 = DIRECTION ( 'NONE',  ( 0.000000000000000000, 0.000000000000000000, 1.000000000000000000 ) ) ;
#192240 = CARTESIAN_POINT ( 'NONE',  ( 18.39999999999999503, 11.75000000001113953, -79.65000000000004832 ) ) ;
#192241 =( LENGTH_UNIT ( ) NAMED_UNIT ( * ) SI_UNIT ( .MILLI., .METRE. ) );
#192242 = VECTOR ( 'NONE', #168389, 1000.000000000000000 ) ;
#192243 = VERTEX_POINT ( 'NONE', #138697 ) ;
#192244 = LINE ( 'NONE', #254719, #230509 ) ;
#192245 = ORIENTED_EDGE ( 'NONE', *, *, #10989, .T. ) ;
#192246 = CARTESIAN_POINT ( 'NONE',  ( -21.05000000000000071, 0.000000000000000000, 0.000000000000000000 ) ) ;
#192247 = ORIENTED_EDGE ( 'NONE', *, *, #164172, .T. ) ;
#192248 = CARTESIAN_POINT ( 'NONE',  ( -18.50000000000000000, -1.866714910046153308, -45.25267524628200988 ) ) ;
#192249 = CARTESIAN_POINT ( 'NONE',  ( 20.85000000000000142, -1.835859311432481045, -145.5044391687985694 ) ) ;
#192250 = ORIENTED_EDGE ( 'NONE', *, *, #193163, .T. ) ;
#192251 = CIRCLE ( 'NONE', #208813, 0.09999999999999949207 ) ;
#192252 = ORIENTED_EDGE ( 'NONE', *, *, #195110, .F. ) ;
#192253 = CARTESIAN_POINT ( 'NONE',  ( 20.94999999999999929, 4.813084112160684214, -122.0584822434762060 ) ) ;
#192254 = EDGE_CURVE ( 'NONE', #128354, #141210, #119187, .T. ) ;
#192255 = DIRECTION ( 'NONE',  ( 1.000000000000000000, 0.000000000000000000, 0.000000000000000000 ) ) ;
#192256 = ORIENTED_EDGE ( 'NONE', *, *, #185988, .T. ) ;
#192257 = VERTEX_POINT ( 'NONE', #184280 ) ;
#192258 = DIRECTION ( 'NONE',  ( 0.000000000000000000, 0.000000000000000000, 1.000000000000000000 ) ) ;
#192259 = CIRCLE ( 'NONE', #221256, 0.09999999999999939493 ) ;
#192260 =( LENGTH_UNIT ( ) NAMED_UNIT ( * ) SI_UNIT ( .MILLI., .METRE. ) );
#192261 = ORIENTED_EDGE ( 'NONE', *, *, #27564, .T. ) ;
#192262 = VECTOR ( 'NONE', #219062, 1000.000000000000000 ) ;
#192263 = CIRCLE ( 'NONE', #100630, 0.09999999999999939493 ) ;
#192264 = ORIENTED_EDGE ( 'NONE', *, *, #114067, .T. ) ;
#192265 = DIRECTION ( 'NONE',  ( -2.952720810173289112E-16, -0.4088369013363281068, 0.9126074666063770380 ) ) ;
#192266 = AXIS2_PLACEMENT_3D ( 'NONE', #129834, #232821, #209379 ) ;
#192267 = ADVANCED_FACE ( 'NONE', ( #220836 ), #239128, .F. ) ;
#192268 = FACE_OUTER_BOUND ( 'NONE', #247045, .T. ) ;
#192269 = AXIS2_PLACEMENT_3D ( 'NONE', #221961, #102013, #181602 ) ;
#192270 = PLANE ( 'NONE',  #167659 ) ;
#192272 = ORIENTED_EDGE ( 'NONE', *, *, #240429, .T. ) ;
#192271 = DIRECTION ( 'NONE',  ( 0.000000000000000000, 0.000000000000000000, -1.000000000000000000 ) ) ;
#192273 = DIRECTION ( 'NONE',  ( 0.000000000000000000, -0.8660254037844468122, -0.4999999999999859557 ) ) ;
#192274 = DIRECTION ( 'NONE',  ( 1.000000000000000000, 0.000000000000000000, 0.000000000000000000 ) ) ;
#192275 = DIRECTION ( 'NONE',  ( 0.000000000000000000, 0.9910465087640860649, 0.1335171055202901413 ) ) ;
#192277 = LINE ( 'NONE', #31930, #120120 ) ;
#192276 = CARTESIAN_POINT ( 'NONE',  ( 21.05000000000000071, 76.02138556594965735, -75.82806859720888326 ) ) ;
#192278 = CARTESIAN_POINT ( 'NONE',  ( -20.64999999999999858, 1.115600667400684642E-11, -167.5000000000000284 ) ) ;
#192279 = CARTESIAN_POINT ( 'NONE',  ( -18.39999999999999858, 64.52683809664912928, -60.19716141771643692 ) ) ;
#192280 = DIRECTION ( 'NONE',  ( 1.000000000000000000, 0.000000000000000000, 0.000000000000000000 ) ) ;
#192281 = ADVANCED_FACE ( 'NONE', ( #183020 ), #60470, .F. ) ;
#192282 = CIRCLE ( 'NONE', #225557, 0.5000000000000004441 ) ;
#192283 = CARTESIAN_POINT ( 'NONE',  ( -21.05000000000000071, 76.01465611852547966, -176.5197940702919084 ) ) ;
#192285 = EDGE_LOOP ( 'NONE', ( #154117, #96371, #105824, #230214 ) ) ;
#192284 = VECTOR ( 'NONE', #226390, 1000.000000000000114 ) ;
#192286 = AXIS2_PLACEMENT_3D ( 'NONE', #86131, #126579, #108304 ) ;
#192287 = EDGE_LOOP ( 'NONE', ( #13721, #49904, #30893 ) ) ;
#192288 = CARTESIAN_POINT ( 'NONE',  ( -18.59999999999999787, 77.83585931145526615, -58.01866831572577610 ) ) ;
#192289 = DIRECTION ( 'NONE',  ( 0.000000000000000000, 0.000000000000000000, 1.000000000000000000 ) ) ;
#192290 = ORIENTED_EDGE ( 'NONE', *, *, #164978, .T. ) ;
#192291 = DIRECTION ( 'NONE',  ( 0.000000000000000000, 1.000000000000000000, 0.000000000000000000 ) ) ;
#192292 = FACE_OUTER_BOUND ( 'NONE', #115974, .T. ) ;
#192294 = ORIENTED_EDGE ( 'NONE', *, *, #22204, .F. ) ;
#192293 = CIRCLE ( 'NONE', #71513, 0.09999999999998902822 ) ;
#192295 = ORIENTED_EDGE ( 'NONE', *, *, #56567, .T. ) ;
#192296 = LINE ( 'NONE', #153197, #225621 ) ;
#192297 = DIRECTION ( 'NONE',  ( 0.000000000000000000, 0.1575844902526835067, 0.9875055080513738259 ) ) ;
#192298 = CARTESIAN_POINT ( 'NONE',  ( 22.24259225415828567, 0.09906588346399246292, -93.00806212943462015 ) ) ;
#192300 = ORIENTED_EDGE ( 'NONE', *, *, #151762, .F. ) ;
#192299 = DIRECTION ( 'NONE',  ( 3.469446951953635015E-14, -0.000000000000000000, 1.000000000000000000 ) ) ;
#192301 = DIRECTION ( 'NONE',  ( 4.377807931758638789E-15, 0.2605042016806672911, 0.9654727137038716656 ) ) ;
#192303 = ORIENTED_EDGE ( 'NONE', *, *, #72032, .T. ) ;
#192302 = CARTESIAN_POINT ( 'NONE',  ( 20.85000000000000142, 87.24382154048164750, -206.5725299160771726 ) ) ;
#192304 = DIRECTION ( 'NONE',  ( -0.000000000000000000, -0.2128009952263603677, 0.9770955615653313941 ) ) ;
#192305 = CARTESIAN_POINT ( 'NONE',  ( 21.05193202509564543, 10.72393601969718802, -12.17253460332576331 ) ) ;
#192306 = ADVANCED_FACE ( 'NONE', ( #222098 ), #43502, .F. ) ;
#192307 = LINE ( 'NONE', #170224, #61645 ) ;
#192308 = CARTESIAN_POINT ( 'NONE',  ( -20.94999999999999929, 76.00000000001244871, -170.0231074845243597 ) ) ;
#192310 = CARTESIAN_POINT ( 'NONE',  ( 20.13684514579998464, 9.495855392759668945, -108.6430316856869922 ) ) ;
#192309 = DIRECTION ( 'NONE',  ( 0.000000000000000000, 0.000000000000000000, -1.000000000000000000 ) ) ;
#192311 = CARTESIAN_POINT ( 'NONE',  ( -18.59999999999999787, 1.162701749949165642, -41.60000000000000142 ) ) ;
#192312 = DIRECTION ( 'NONE',  ( 0.000000000000000000, -1.000000000000000000, -6.982962677686265922E-15 ) ) ;
#192313 = CARTESIAN_POINT ( 'NONE',  ( -18.52309608778521266, 85.64247632006754429, -163.3085111433545933 ) ) ;
#192314 = LINE ( 'NONE', #51479, #114139 ) ;
#192315 = FACE_OUTER_BOUND ( 'NONE', #74478, .T. ) ;
#192316 = ORIENTED_EDGE ( 'NONE', *, *, #255386, .T. ) ;
#192318 = VECTOR ( 'NONE', #74404, 1000.000000000000227 ) ;
#192317 = SPHERICAL_SURFACE ( 'NONE', #130546, 0.1000000000000000056 ) ;
#192319 = ORIENTED_EDGE ( 'NONE', *, *, #14185, .F. ) ;
#192320 = DIRECTION ( 'NONE',  ( 0.000000000000000000, -0.9947597004326491632, 0.1022405907413782566 ) ) ;
#192321 = ORIENTED_EDGE ( 'NONE', *, *, #166935, .T. ) ;
#192322 = EDGE_CURVE ( 'NONE', #73777, #206383, #25152, .T. ) ;
#192323 = DIRECTION ( 'NONE',  ( -0.000000000000000000, 0.1350103645451807555, 0.9908441862701610203 ) ) ;
#192324 = DIRECTION ( 'NONE',  ( 0.000000000000000000, 0.000000000000000000, 1.000000000000000000 ) ) ;
#192325 = ADVANCED_FACE ( 'NONE', ( #5618 ), #233269, .T. ) ;
#192326 = ORIENTED_EDGE ( 'NONE', *, *, #257453, .T. ) ;
#192327 = CARTESIAN_POINT ( 'NONE',  ( -21.05000000000000071, 30.73599169745032356, -252.2206231971132127 ) ) ;
#192328 =( NAMED_UNIT ( * ) SI_UNIT ( $, .STERADIAN. ) SOLID_ANGLE_UNIT ( ) );
#192329 = EDGE_CURVE ( 'NONE', #26762, #199945, #96336, .T. ) ;
#192331 = ORIENTED_EDGE ( 'NONE', *, *, #147262, .F. ) ;
#192330 = CIRCLE ( 'NONE', #79870, 0.09999999999999990841 ) ;
#192332 = ORIENTED_EDGE ( 'NONE', *, *, #207088, .F. ) ;
#192333 = CIRCLE ( 'NONE', #34153, 4.000000000000003553 ) ;
#192334 = LINE ( 'NONE', #56629, #67226 ) ;
#192335 = CARTESIAN_POINT ( 'NONE',  ( -16.77732147278574715, 66.05403306743814085, -56.85959872764858147 ) ) ;
#192336 = PLANE ( 'NONE',  #205054 ) ;
#192337 = CARTESIAN_POINT ( 'NONE',  ( 12.84435279558019616, 27.50042447306175220, -233.9693577020172199 ) ) ;
#192338 = CARTESIAN_POINT ( 'NONE',  ( -23.15000000000000213, 71.85000000001173248, -81.27310748452434552 ) ) ;
#192339 = DIRECTION ( 'NONE',  ( 0.000000000000000000, 1.000000000000000000, 0.000000000000000000 ) ) ;
#192340 = CARTESIAN_POINT ( 'NONE',  ( -14.77738660682463667, 9.436552840015579591, -82.17795547276035961 ) ) ;
#192342 = ORIENTED_EDGE ( 'NONE', *, *, #35631, .F. ) ;
#192341 = DIRECTION ( 'NONE',  ( 1.000000000000000000, 0.000000000000000000, 0.000000000000000000 ) ) ;
#192344 = DIRECTION ( 'NONE',  ( 0.000000000000000000, 0.4088369013363783999, -0.9126074666063545004 ) ) ;
#192343 = CARTESIAN_POINT ( 'NONE',  ( -18.39999999999999858, 20.76715588789282307, -228.0228088279911560 ) ) ;
#192345 = EDGE_CURVE ( 'NONE', #46675, #76969, #106006, .T. ) ;
#192346 = DIRECTION ( 'NONE',  ( 0.000000000000000000, 0.008583690987124100932, -0.9999631594459055250 ) ) ;
#192347 = EDGE_LOOP ( 'NONE', ( #71027, #175843, #173541, #248131 ) ) ;
#192348 = CARTESIAN_POINT ( 'NONE',  ( -18.50000000000000355, -9.399999999988818189, -174.7972597596632625 ) ) ;
#192349 = CARTESIAN_POINT ( 'NONE',  ( -20.54999999999999716, -8.999999999988846255, -143.8939691226524644 ) ) ;
#192350 = CARTESIAN_POINT ( 'NONE',  ( -23.15000000000000213, 62.86885547537413288, -207.0505773246641752 ) ) ;
#192351 = VERTEX_POINT ( 'NONE', #248108 ) ;
#192352 = EDGE_CURVE ( 'NONE', #81417, #113044, #9495, .T. ) ;
#192353 = AXIS2_PLACEMENT_3D ( 'NONE', #144592, #7683, #128909 ) ;
#192354 = DIRECTION ( 'NONE',  ( 0.000000000000000000, -0.2617529984165026247, -0.9651348961777158619 ) ) ;
#192355 = CARTESIAN_POINT ( 'NONE',  ( -23.15000000000000213, -11.48912529306489816, -197.8999999999999773 ) ) ;
#192356 = CARTESIAN_POINT ( 'NONE',  ( 15.74999999999999289, 66.65000000001187175, -86.50453852712173841 ) ) ;
#192357 = ORIENTED_EDGE ( 'NONE', *, *, #238975, .F. ) ;
#192358 = ORIENTED_EDGE ( 'NONE', *, *, #152519, .T. ) ;
#192359 = CARTESIAN_POINT ( 'NONE',  ( 22.50927854361890113, 64.25313177404581211, -247.2214436579493224 ) ) ;
#192360 = DIRECTION ( 'NONE',  ( 0.000000000000000000, -0.000000000000000000, -1.000000000000000000 ) ) ;
#192361 = DIRECTION ( 'NONE',  ( 1.000000000000000000, 0.000000000000000000, 0.000000000000000000 ) ) ;
#192362 = CARTESIAN_POINT ( 'NONE',  ( -20.00857864376270001, 9.150000000011157653, -88.15000000000004832 ) ) ;
#192363 = EDGE_LOOP ( 'NONE', ( #246266, #230370, #213994 ) ) ;
#192364 = EDGE_CURVE ( 'NONE', #37872, #216320, #170934, .T. ) ;
#192365 = DIRECTION ( 'NONE',  ( 1.000000000000000000, 0.000000000000000000, 0.000000000000000000 ) ) ;
#192366 = CIRCLE ( 'NONE', #79896, 0.09999999999998900047 ) ;
#192368 = CARTESIAN_POINT ( 'NONE',  ( -22.48660254037843131, 64.35000000001237197, -170.0731074845244279 ) ) ;
#192367 = CIRCLE ( 'NONE', #242234, 1.899999999999999023 ) ;
#192369 = AXIS2_PLACEMENT_3D ( 'NONE', #219635, #223482, #63123 ) ;
#192370 = DIRECTION ( 'NONE',  ( 1.000000000000000000, 0.000000000000000000, 0.000000000000000000 ) ) ;
#192371 = LINE ( 'NONE', #174133, #211758 ) ;
#192372 = DIRECTION ( 'NONE',  ( 0.000000000000000000, 6.982962677686266711E-15, -1.000000000000000000 ) ) ;
#192373 = EDGE_CURVE ( 'NONE', #219574, #68492, #100112, .T. ) ;
#192375 = VERTEX_POINT ( 'NONE', #186878 ) ;
#192374 = DIRECTION ( 'NONE',  ( 1.000000000000000000, 0.000000000000000000, 0.000000000000000000 ) ) ;
#192376 = DIRECTION ( 'NONE',  ( -1.000000000000000000, -0.000000000000000000, -0.000000000000000000 ) ) ;
#192377 = CARTESIAN_POINT ( 'NONE',  ( -20.54999999999999716, 84.73084112150785074, -179.6211822035086243 ) ) ;
#192378 = FACE_OUTER_BOUND ( 'NONE', #79513, .T. ) ;
#192379 = DIRECTION ( 'NONE',  ( 0.5932847527679310229, 0.8049926720990042694, 5.621233785078285907E-15 ) ) ;
#192380 = LINE ( 'NONE', #11180, #25499 ) ;
#192382 = VERTEX_POINT ( 'NONE', #128173 ) ;
#192381 = CARTESIAN_POINT ( 'NONE',  ( -21.14999999999999858, 69.45934304831089889, -136.4231074845243654 ) ) ;
#192383 = DIRECTION ( 'NONE',  ( 0.000000000000000000, -0.2617529984164506107, -0.9651348961777299618 ) ) ;
#192384 = DIRECTION ( 'NONE',  ( 0.000000000000000000, 0.000000000000000000, 1.000000000000000000 ) ) ;
#192385 = CARTESIAN_POINT ( 'NONE',  ( 23.14999999999999503, 2.319530388122574394, -217.8268657444419887 ) ) ;
#192386 = EDGE_CURVE ( 'NONE', #37719, #60608, #216666, .T. ) ;
#192387 = TOROIDAL_SURFACE ( 'NONE', #46603, 0.4000000000000017431, 0.1000000000000000056 ) ;
#192388 = ORIENTED_EDGE ( 'NONE', *, *, #255105, .F. ) ;
#192389 = DIRECTION ( 'NONE',  ( -0.5932847527679299127, -0.8049926720990051576, -6.257843056355997642E-15 ) ) ;
#192390 = CARTESIAN_POINT ( 'NONE',  ( 22.57320508075687115, 11.75000000000000000, 0.000000000000000000 ) ) ;
#192391 = DIRECTION ( 'NONE',  ( 0.000000000000000000, 0.4721928772777346794, 0.8814952561688431665 ) ) ;
#192392 = CARTESIAN_POINT ( 'NONE',  ( -21.65000000000000213, 7.250000000011138646, -180.1499999999999773 ) ) ;
#192393 = ADVANCED_FACE ( 'NONE', ( #87736 ), #83359, .T. ) ;
#192394 = CARTESIAN_POINT ( 'NONE',  ( -21.05000000000000071, -5.616267472387885817, -233.5404684641580673 ) ) ;
#192395 = B_SPLINE_CURVE_WITH_KNOTS ( 'NONE', 3,
 ( #236844, #256348, #55611, #233029, #75241, #36103, #116908, #77758 ),
 .UNSPECIFIED., .F., .F.,
 ( 4, 2, 2, 4 ),
 ( 0.000000000000000000, 0.0001049670497870001246, 0.0002099340995740002491, 0.0004198681991479959446 ),
 .UNSPECIFIED. ) ;
#192396 = ADVANCED_FACE ( 'NONE', ( #146421 ), #112618, .T. ) ;
#192397 = CARTESIAN_POINT ( 'NONE',  ( -20.54999999999999716, 74.00000000001180922, -82.74772940728641402 ) ) ;
#192398 = VERTEX_POINT ( 'NONE', #109872 ) ;
#192399 = VERTEX_POINT ( 'NONE', #150314 ) ;
#192400 = CARTESIAN_POINT ( 'NONE',  ( -18.45068461519106506, -9.486506529077926686, -141.0687771689047452 ) ) ;
#192401 = DIRECTION ( 'NONE',  ( 0.000000000000000000, 0.000000000000000000, -1.000000000000000000 ) ) ;
#192402 = ADVANCED_FACE ( 'NONE', ( #27819 ), #62551, .T. ) ;
#192403 = CARTESIAN_POINT ( 'NONE',  ( 18.45139536634708577, -0.7268675243558969656, -242.2397633716003327 ) ) ;
#192404 = FACE_OUTER_BOUND ( 'NONE', #102878, .T. ) ;
#192405 = LINE ( 'NONE', #194993, #75933 ) ;
#192406 = CIRCLE ( 'NONE', #96690, 1.900000000000012790 ) ;
#192407 = ADVANCED_FACE ( 'NONE', ( #225946 ), #244244, .T. ) ;
#192409 = EDGE_CURVE ( 'NONE', #33086, #49193, #254072, .T. ) ;
#192408 = DIRECTION ( 'NONE',  ( -1.000000000000000000, -0.000000000000000000, 0.000000000000000000 ) ) ;
#192410 = AXIS2_PLACEMENT_3D ( 'NONE', #11964, #17097, #156627 ) ;
#192411 = CARTESIAN_POINT ( 'NONE',  ( -20.00857864376270001, 66.65000000001229807, -157.6731074845244223 ) ) ;
#192412 = VECTOR ( 'NONE', #14426, 1000.000000000000000 ) ;
#192413 = CIRCLE ( 'NONE', #234091, 0.1000000000000028644 ) ;
#192414 = AXIS2_PLACEMENT_3D ( 'NONE', #58620, #235980, #142020 ) ;
#192415 = ORIENTED_EDGE ( 'NONE', *, *, #43398, .F. ) ;
#192416 = CARTESIAN_POINT ( 'NONE',  ( -23.15000000000000213, 51.38014393322265505, -230.1906178717505611 ) ) ;
#192417 = EDGE_CURVE ( 'NONE', #174920, #164268, #130732, .T. ) ;
#192418 = ORIENTED_EDGE ( 'NONE', *, *, #10400, .T. ) ;
#192419 = CARTESIAN_POINT ( 'NONE',  ( 23.04999999999999716, 8.822561741666397950, -24.25000000000000000 ) ) ;
#192420 = CARTESIAN_POINT ( 'NONE',  ( 20.95262331984765325, 10.50415726278985851, -7.560888329593319135 ) ) ;
#192422 = EDGE_LOOP ( 'NONE', ( #251778, #97583, #232374, #119757 ) ) ;
#192421 = DIRECTION ( 'NONE',  ( -1.000000000000000000, -0.000000000000000000, -0.000000000000000000 ) ) ;
#192423 = ADVANCED_FACE ( 'NONE', ( #129454 ), #66827, .T. ) ;
#192424 = CARTESIAN_POINT ( 'NONE',  ( -21.64999999999999858, 44.87429835298447500, -237.9265065269792103 ) ) ;
#192426 = DIRECTION ( 'NONE',  ( 0.000000000000000000, 0.000000000000000000, -1.000000000000000000 ) ) ;
#192425 = CIRCLE ( 'NONE', #859, 0.09999999999999939493 ) ;
#192427 = ORIENTED_EDGE ( 'NONE', *, *, #158069, .T. ) ;
#192428 = CARTESIAN_POINT ( 'NONE',  ( -16.87331047859651179, 9.950000000011142376, -79.65000000000004832 ) ) ;
#192429 = TOROIDAL_SURFACE ( 'NONE', #67339, 0.9750000000000019762, 0.1000000000000000056 ) ;
#192430 = CARTESIAN_POINT ( 'NONE',  ( 21.15000000000005542, 87.51781941433023349, -34.28670414799875488 ) ) ;
#192431 = DIRECTION ( 'NONE',  ( -1.000000000000000000, 0.000000000000000000, 0.000000000000000000 ) ) ;
#192432 = CARTESIAN_POINT ( 'NONE',  ( 20.94999999999999929, 70.50000000001205080, -124.1178414656112352 ) ) ;
#192433 = CIRCLE ( 'NONE', #113317, 0.1000000000000054040 ) ;
#192434 = AXIS2_PLACEMENT_3D ( 'NONE', #109946, #210351, #51235 ) ;
#192435 = DIRECTION ( 'NONE',  ( 1.000000000000000000, 2.952720810173289112E-16, -0.000000000000000000 ) ) ;
#192436 = ORIENTED_EDGE ( 'NONE', *, *, #162827, .T. ) ;
#192437 = AXIS2_PLACEMENT_3D ( 'NONE', #243360, #25613, #106399 ) ;
#192438 = CARTESIAN_POINT ( 'NONE',  ( -22.57848426163147693, 76.00426432929532439, -148.2731657914146126 ) ) ;
#192439 = CARTESIAN_POINT ( 'NONE',  ( -18.40000000000000213, 11.47316190337364183, -154.9500000000000455 ) ) ;
#192440 = ORIENTED_EDGE ( 'NONE', *, *, #235512, .T. ) ;
#192441 = EDGE_CURVE ( 'NONE', #24478, #21030, #227259, .T. ) ;
#192442 = EDGE_CURVE ( 'NONE', #164661, #147767, #48622, .T. ) ;
#192443 = AXIS2_PLACEMENT_3D ( 'NONE', #64414, #184345, #21455 ) ;
#192444 = EDGE_LOOP ( 'NONE', ( #60422, #223567, #179417, #214411 ) ) ;
#192445 = CARTESIAN_POINT ( 'NONE',  ( -16.97683809663752186, 9.850000000011140955, -79.65000000000004832 ) ) ;
#192446 = DIRECTION ( 'NONE',  ( 0.000000000000000000, 0.000000000000000000, -1.000000000000000000 ) ) ;
#192447 = EDGE_LOOP ( 'NONE', ( #205475, #230595, #92400, #213154 ) ) ;
#192448 = DIRECTION ( 'NONE',  ( 0.000000000000000000, -0.9915357197604982575, 0.1298341882519033486 ) ) ;
#192449 = EDGE_CURVE ( 'NONE', #223676, #208027, #20882, .T. ) ;
#192450 = ORIENTED_EDGE ( 'NONE', *, *, #152095, .T. ) ;
#192451 = VECTOR ( 'NONE', #74085, 1000.000000000000000 ) ;
#192452 = VECTOR ( 'NONE', #193717, 1000.000000000000000 ) ;
#192453 = CIRCLE ( 'NONE', #200844, 2.600000000000000089 ) ;
#192454 = ORIENTED_EDGE ( 'NONE', *, *, #64115, .F. ) ;
#192455 = CARTESIAN_POINT ( 'NONE',  ( -20.64999999999999858, 0.000000000000000000, -33.50000000000000000 ) ) ;
#192456 = CARTESIAN_POINT ( 'NONE',  ( -20.54999999999999716, 1.115600667400684642E-11, -100.5000000000000426 ) ) ;
#192458 = VERTEX_POINT ( 'NONE', #210287 ) ;
#192457 = CARTESIAN_POINT ( 'NONE',  ( 18.59999999999999076, 1.750000000011155743, -45.16951155790165018 ) ) ;
#192459 = FACE_OUTER_BOUND ( 'NONE', #34094, .T. ) ;
#192460 = CARTESIAN_POINT ( 'NONE',  ( -22.48970261584618058, 11.65000000001115588, -133.9446305117826341 ) ) ;
#192461 = FACE_OUTER_BOUND ( 'NONE', #223080, .T. ) ;
#192462 = CARTESIAN_POINT ( 'NONE',  ( 23.50000000000005684, 76.00000000001119815, -36.02310748452479316 ) ) ;
#192463 = CARTESIAN_POINT ( 'NONE',  ( 21.05000000000000071, 85.00000000001179501, -79.41707660717668205 ) ) ;
#192464 = EDGE_CURVE ( 'NONE', #65123, #59718, #141644, .T. ) ;
#192465 = DIRECTION ( 'NONE',  ( 0.000000000000000000, -1.000000000000000000, 0.000000000000000000 ) ) ;
#192466 = CARTESIAN_POINT ( 'NONE',  ( -16.79184697841823848, 66.05123833835389746, -157.3689652139219106 ) ) ;
#192468 = ORIENTED_EDGE ( 'NONE', *, *, #32862, .F. ) ;
#192467 = DIRECTION ( 'NONE',  ( -1.000000000000000000, 0.000000000000000000, 0.000000000000000000 ) ) ;
#192469 = ORIENTED_EDGE ( 'NONE', *, *, #24910, .F. ) ;
#192471 = CARTESIAN_POINT ( 'NONE',  ( -16.84981964351488770, 51.43181437145960899, -232.0660758826369943 ) ) ;
#192470 = CARTESIAN_POINT ( 'NONE',  ( -21.93642651522410247, 68.67283376068584744, -69.52310748452435973 ) ) ;
#192473 = ORIENTED_EDGE ( 'NONE', *, *, #163467, .F. ) ;
#192472 = DIRECTION ( 'NONE',  ( 1.000000000000000000, 0.000000000000000000, 0.000000000000000000 ) ) ;
#192474 = EDGE_CURVE ( 'NONE', #244466, #240031, #79414, .T. ) ;
#192475 = VERTEX_POINT ( 'NONE', #52461 ) ;
#192476 = DIRECTION ( 'NONE',  ( 0.000000000000000000, 0.9126074666063632712, 0.4088369013363589710 ) ) ;
#192477 = AXIS2_PLACEMENT_3D ( 'NONE', #177281, #198091, #237227 ) ;
#192478 = LINE ( 'NONE', #252427, #93097 ) ;
#192479 = DIRECTION ( 'NONE',  ( 1.000000000000000000, -3.265361837132813093E-16, -2.280189983783949500E-30 ) ) ;
#192480 = DIRECTION ( 'NONE',  ( -0.7071067811865463515, 0.6824534298470381621, -0.1850873201762220366 ) ) ;
#192481 = EDGE_CURVE ( 'NONE', #143844, #162306, #19473, .T. ) ;
#192482 = CARTESIAN_POINT ( 'NONE',  ( 20.94999999999999574, 39.23476235320398331, -236.9756760510740037 ) ) ;
#192483 = CARTESIAN_POINT ( 'NONE',  ( -20.00857864376270001, 13.44116543737180081, -219.7184420207870801 ) ) ;
#192484 = EDGE_CURVE ( 'NONE', #151938, #26951, #95839, .T. ) ;
#192485 = DIRECTION ( 'NONE',  ( 1.000000000000000000, -0.000000000000000000, -0.000000000000000000 ) ) ;
#192486 = ORIENTED_EDGE ( 'NONE', *, *, #46103, .T. ) ;
#192487 = ORIENTED_EDGE ( 'NONE', *, *, #190780, .T. ) ;
#192488 = EDGE_CURVE ( 'NONE', #77303, #68117, #129192, .T. ) ;
#192489 = CARTESIAN_POINT ( 'NONE',  ( -20.54999999999999716, 1.115625160336667635E-11, -102.5000000000000426 ) ) ;
#192490 = ORIENTED_EDGE ( 'NONE', *, *, #220121, .F. ) ;
#192491 = CARTESIAN_POINT ( 'NONE',  ( -18.50000000000000000, 9.350000000011156942, -54.65000000000000568 ) ) ;
#192492 = EDGE_LOOP ( 'NONE', ( #18313, #126249, #169484, #186228 ) ) ;
#192493 = CYLINDRICAL_SURFACE ( 'NONE', #88992, 0.09999999999999939493 ) ;
#192494 = EDGE_CURVE ( 'NONE', #40541, #86338, #4455, .T. ) ;
#192495 = CIRCLE ( 'NONE', #175957, 0.09999999999999907574 ) ;
#192497 = EDGE_CURVE ( 'NONE', #131784, #196598, #198098, .T. ) ;
#192496 = EDGE_CURVE ( 'NONE', #223374, #186212, #108512, .T. ) ;
#192498 = DIRECTION ( 'NONE',  ( 1.652117596168391897E-15, -0.4088369013363281068, 0.9126074666063770380 ) ) ;
#192499 = LINE ( 'NONE', #16450, #81695 ) ;
#192500 = ORIENTED_EDGE ( 'NONE', *, *, #25169, .F. ) ;
#192501 = APPLICATION_CONTEXT ( 'automotive_design' ) ;
#192502 = CARTESIAN_POINT ( 'NONE',  ( -21.05000000000000071, -1.162701749926853712, -75.10000000000003695 ) ) ;
#192503 = ORIENTED_EDGE ( 'NONE', *, *, #114632, .F. ) ;
#192504 = CYLINDRICAL_SURFACE ( 'NONE', #198133, 0.09999999999999939493 ) ;
#192505 = CARTESIAN_POINT ( 'NONE',  ( 18.47073956224749480, 8.922622944725832284, -245.4386566365344322 ) ) ;
#192506 = ORIENTED_EDGE ( 'NONE', *, *, #51435, .F. ) ;
#192508 = LINE ( 'NONE', #11305, #244268 ) ;
#192507 = AXIS2_PLACEMENT_3D ( 'NONE', #168039, #67606, #244958 ) ;
#192509 = ORIENTED_EDGE ( 'NONE', *, *, #140643, .F. ) ;
#192512 = ORIENTED_EDGE ( 'NONE', *, *, #201225, .T. ) ;
#192511 = CARTESIAN_POINT ( 'NONE',  ( -18.50000000000000000, 1.637172712970379918, -11.58215336547201879 ) ) ;
#192510 = PLANE ( 'NONE',  #3531 ) ;
#192513 = EDGE_CURVE ( 'NONE', #176327, #210749, #140689, .T. ) ;
#192514 = CARTESIAN_POINT ( 'NONE',  ( -20.99780126800933644, 64.39461131213499812, -42.93575491281912804 ) ) ;
#192515 = EDGE_CURVE ( 'NONE', #12539, #241392, #229334, .T. ) ;
#192516 = ORIENTED_EDGE ( 'NONE', *, *, #72612, .F. ) ;
#192517 = AXIS2_PLACEMENT_3D ( 'NONE', #195689, #19604, #237360 ) ;
#192518 = VERTEX_POINT ( 'NONE', #235933 ) ;
#192519 = VECTOR ( 'NONE', #71433, 1000.000000000000227 ) ;
#192520 = EDGE_CURVE ( 'NONE', #74531, #235411, #75221, .T. ) ;
#192522 = CARTESIAN_POINT ( 'NONE',  ( 22.47071067811864964, 0.09909245470260576172, 7.720074744498039543 ) ) ;
#192521 =( BOUNDED_CURVE ( )  B_SPLINE_CURVE ( 3, ( #180359, #142492, #120418, #102071 ),
 .UNSPECIFIED., .F., .F. ) 
 B_SPLINE_CURVE_WITH_KNOTS ( ( 4, 4 ),
 ( 2.589852378279006384, 2.850972632318390154 ),
 .UNSPECIFIED. ) 
 CURVE ( )  GEOMETRIC_REPRESENTATION_ITEM ( )  RATIONAL_B_SPLINE_CURVE ( ( 1.000000000000000000, 0.9943260843901262636, 0.9943260843901262636, 1.000000000000000000 ) ) 
 REPRESENTATION_ITEM ( '' )  );
#192523 = VERTEX_POINT ( 'NONE', #40355 ) ;
#192524 = CARTESIAN_POINT ( 'NONE',  ( -18.59999999999999787, 7.788796164756791818, -245.4641525896719543 ) ) ;
#192525 = CARTESIAN_POINT ( 'NONE',  ( 21.04999999999999716, 69.65564095796813149, -69.53796311941867714 ) ) ;
#192527 = ADVANCED_FACE ( 'NONE', ( #20768 ), #175996, .T. ) ;
#192526 = LINE ( 'NONE', #112990, #211821 ) ;
#192528 = CARTESIAN_POINT ( 'NONE',  ( -20.94999999999999929, 44.06250559941687328, -258.7395785465160429 ) ) ;
#192529 = CARTESIAN_POINT ( 'NONE',  ( -16.94107738177415712, 65.98576071487543970, -123.9731074845243626 ) ) ;
#192530 = EDGE_CURVE ( 'NONE', #227362, #209114, #58614, .T. ) ;
#192531 = AXIS2_PLACEMENT_3D ( 'NONE', #229136, #106591, #186155 ) ;
#192532 = VERTEX_POINT ( 'NONE', #100252 ) ;
#192533 = AXIS2_PLACEMENT_3D ( 'NONE', #186114, #184819, #46580 ) ;
#192534 = DIRECTION ( 'NONE',  ( 0.000000000000000000, 1.000000000000000000, -0.000000000000000000 ) ) ;
#192535 = CARTESIAN_POINT ( 'NONE',  ( 18.59999999999999787, 77.83585931145600512, -158.5186683157258187 ) ) ;
#192536 = DIRECTION ( 'NONE',  ( -1.000000000000000000, 0.000000000000000000, 0.000000000000000000 ) ) ;
#192537 = VERTEX_POINT ( 'NONE', #121169 ) ;
#192538 = CARTESIAN_POINT ( 'NONE',  ( 23.15000000000000213, -12.41227409413852811, -130.9000000000000341 ) ) ;
#192539 = ORIENTED_EDGE ( 'NONE', *, *, #118914, .F. ) ;
#192540 = CARTESIAN_POINT ( 'NONE',  ( -22.47071067811865319, 33.41224047107334627, -242.5462774987836383 ) ) ;
#192541 = ORIENTED_EDGE ( 'NONE', *, *, #102265, .T. ) ;
#192542 = FACE_OUTER_BOUND ( 'NONE', #249220, .T. ) ;
#192543 = DIRECTION ( 'NONE',  ( 1.000000000000000000, -0.000000000000000000, -0.000000000000000000 ) ) ;
#192545 = ORIENTED_EDGE ( 'NONE', *, *, #127898, .T. ) ;
#192544 = CARTESIAN_POINT ( 'NONE',  ( 18.59999999999999432, 72.10920423909969657, -225.0008277277438822 ) ) ;
#192546 = EDGE_CURVE ( 'NONE', #170720, #235551, #167006, .T. ) ;
#192547 = CARTESIAN_POINT ( 'NONE',  ( 23.14999999999999503, 64.35000000001176090, -76.53791325517833855 ) ) ;
#192548 = ORIENTED_EDGE ( 'NONE', *, *, #126539, .T. ) ;
#192549 = DIRECTION ( 'NONE',  ( 0.000000000000000000, 0.8814952561688476074, -0.4721928772777262417 ) ) ;
#192550 = CIRCLE ( 'NONE', #163334, 0.09999999999999990841 ) ;
#192551 = CIRCLE ( 'NONE', #100736, 0.09999999999999939493 ) ;
#192552 = DIRECTION ( 'NONE',  ( -1.284434275755705789E-16, 0.7071067811865472397, 0.7071067811865479058 ) ) ;
#192553 = EDGE_LOOP ( 'NONE', ( #123234, #10084, #122318, #48328 ) ) ;
#192554 = CIRCLE ( 'NONE', #213380, 0.09999999999998898659 ) ;
#192555 = EDGE_CURVE ( 'NONE', #43988, #210362, #62736, .T. ) ;
#192556 = DIRECTION ( 'NONE',  ( 1.000000000000000000, -0.000000000000000000, -0.000000000000000000 ) ) ;
#192557 = CARTESIAN_POINT ( 'NONE',  ( -22.39999999999999858, -3.275978944802464987, -228.2735455795363748 ) ) ;
#192558 = VERTEX_POINT ( 'NONE', #195558 ) ;
#192559 = CARTESIAN_POINT ( 'NONE',  ( 21.05000000000000071, 1.658775325997237315, -230.6916041481598540 ) ) ;
#192560 = EDGE_LOOP ( 'NONE', ( #18731, #245396, #122712, #196873, #116278 ) ) ;
#192561 = DIRECTION ( 'NONE',  ( 0.000000000000000000, -0.9651348961777157509, 0.2617529984165032353 ) ) ;
#192562 = CARTESIAN_POINT ( 'NONE',  ( -18.45140287520618472, -9.486077739518409047, -73.64052312668613354 ) ) ;
#192563 = EDGE_CURVE ( 'NONE', #106654, #71518, #16909, .T. ) ;
#192565 = ORIENTED_EDGE ( 'NONE', *, *, #70889, .F. ) ;
#192564 = DIRECTION ( 'NONE',  ( 0.000000000000000000, 7.147358527629766941E-15, -1.000000000000000000 ) ) ;
#192566 = CARTESIAN_POINT ( 'NONE',  ( 18.39999999999999858, 85.60000000001166143, -62.82291809330219223 ) ) ;
#192567 = DIRECTION ( 'NONE',  ( -0.000000000000000000, -0.000000000000000000, -1.000000000000000000 ) ) ;
#192568 = CARTESIAN_POINT ( 'NONE',  ( 20.95512820512820440, 67.12384868372377866, -94.46447848938342418 ) ) ;
#192570 = DIRECTION ( 'NONE',  ( -1.000000000000000000, 0.000000000000000000, 0.000000000000000000 ) ) ;
#192569 = DIRECTION ( 'NONE',  ( 0.000000000000000000, 0.1480365673253065395, -0.9889818879709274535 ) ) ;
#192571 = DIRECTION ( 'NONE',  ( -2.952720810173289112E-16, -1.000000000000000000, -6.982962677686266711E-15 ) ) ;
#192572 = CARTESIAN_POINT ( 'NONE',  ( -23.15000000000000213, 71.65000000001207070, -124.1731074845243228 ) ) ;
#192573 = CIRCLE ( 'NONE', #255037, 0.09999999999999907574 ) ;
#192574 = CARTESIAN_POINT ( 'NONE',  ( -21.05000000000000071, -11.48912529306489994, -164.5000000000000000 ) ) ;
#192575 = AXIS2_PLACEMENT_3D ( 'NONE', #166983, #104374, #84800 ) ;
#192576 = CARTESIAN_POINT ( 'NONE',  ( 20.94999999999999929, -11.64999999999999147, -30.50000000000000000 ) ) ;
#192577 = VERTEX_POINT ( 'NONE', #256737 ) ;
#192578 = ORIENTED_EDGE ( 'NONE', *, *, #53564, .F. ) ;
#192579 = FACE_OUTER_BOUND ( 'NONE', #172762, .T. ) ;
#192581 = ORIENTED_EDGE ( 'NONE', *, *, #240226, .T. ) ;
#192580 = CARTESIAN_POINT ( 'NONE',  ( -20.94999999999999929, 76.00000000001199396, -114.7231074845243057 ) ) ;
#192582 = EDGE_LOOP ( 'NONE', ( #182224, #129554, #157949, #251914 ) ) ;
#192584 = DIRECTION ( 'NONE',  ( 0.000000000000000000, 0.9910827722268055195, 0.1332476588733540468 ) ) ;
#192583 = VECTOR ( 'NONE', #164981, 1000.000000000000000 ) ;
#192585 = ORIENTED_EDGE ( 'NONE', *, *, #178011, .T. ) ;
#192586 = CARTESIAN_POINT ( 'NONE',  ( 21.53752568617646901, 33.79390208801449091, -243.3979355726051494 ) ) ;
#192587 = VECTOR ( 'NONE', #256423, 1000.000000000000000 ) ;
#192588 = ORIENTED_EDGE ( 'NONE', *, *, #213592, .T. ) ;
#192589 = CIRCLE ( 'NONE', #238372, 0.09999999999999939493 ) ;
#192590 = DIRECTION ( 'NONE',  ( 1.000000000000000000, 0.000000000000000000, 0.000000000000000000 ) ) ;
#192592 = EDGE_LOOP ( 'NONE', ( #244246, #247906, #56989, #35102 ) ) ;
#192591 = EDGE_LOOP ( 'NONE', ( #113336, #160089, #176153, #14547 ) ) ;
#192593 = ORIENTED_EDGE ( 'NONE', *, *, #184531, .F. ) ;
#192594 = CIRCLE ( 'NONE', #34410, 0.1999999999999987899 ) ;
#192595 = ORIENTED_EDGE ( 'NONE', *, *, #249384, .F. ) ;
#192597 = VERTEX_POINT ( 'NONE', #238507 ) ;
#192596 = VECTOR ( 'NONE', #161395, 1000.000000000000000 ) ;
#192598 = CARTESIAN_POINT ( 'NONE',  ( -22.39999999999999858, 7.176052627820866725, -233.6445517868224044 ) ) ;
#192599 = DIRECTION ( 'NONE',  ( 0.000000000000000000, 0.2617529984165055668, 0.9651348961777150848 ) ) ;
#192600 = CARTESIAN_POINT ( 'NONE',  ( 21.05000000000000071, 8.776282895303632259, -75.55862899514100661 ) ) ;
#192602 = EDGE_LOOP ( 'NONE', ( #245707, #36228, #173552, #8545, #145688, #236627, #122683, #243748, #6377 ) ) ;
#192601 = FACE_OUTER_BOUND ( 'NONE', #67006, .T. ) ;
#192603 = DIRECTION ( 'NONE',  ( -1.000000000000000000, -0.000000000000000000, -0.000000000000000000 ) ) ;
#192604 = DIRECTION ( 'NONE',  ( -0.000000000000000000, 0.8700118002898356018, -0.4930308989875170078 ) ) ;
#192606 = ORIENTED_EDGE ( 'NONE', *, *, #153010, .T. ) ;
#192605 = CARTESIAN_POINT ( 'NONE',  ( 20.94999999999999574, 10.47338541492405994, -141.5786544642485580 ) ) ;
#192607 = DIRECTION ( 'NONE',  ( 1.000000000000000000, 0.000000000000000000, -0.000000000000000000 ) ) ;
#192608 = ORIENTED_EDGE ( 'NONE', *, *, #189790, .T. ) ;
#192609 = DIRECTION ( 'NONE',  ( 0.000000000000000000, 1.000000000000000000, 0.000000000000000000 ) ) ;
#192611 = ORIENTED_EDGE ( 'NONE', *, *, #125804, .F. ) ;
#192610 = DIRECTION ( 'NONE',  ( 1.000000000000000000, 0.000000000000000000, 0.000000000000000000 ) ) ;
#192612 = AXIS2_PLACEMENT_3D ( 'NONE', #1519, #101888, #160639 ) ;
#192613 = DIRECTION ( 'NONE',  ( 0.000000000000000000, -1.000000000000000000, 0.000000000000000000 ) ) ;
#192614 = CARTESIAN_POINT ( 'NONE',  ( -16.86445178670641809, 9.962211629127180501, -113.1092225618826319 ) ) ;
#192615 = ADVANCED_FACE ( 'NONE', ( #78135 ), #145305, .F. ) ;
#192617 = ORIENTED_EDGE ( 'NONE', *, *, #217735, .F. ) ;
#192616 = AXIS2_PLACEMENT_3D ( 'NONE', #133780, #35987, #179352 ) ;
#192618 = TOROIDAL_SURFACE ( 'NONE', #238396, 2.699999999999999734, 0.1000000000000000056 ) ;
#192620 = CARTESIAN_POINT ( 'NONE',  ( -18.47690164073607022, -9.464844538001084828, -140.7013809398361275 ) ) ;
#192619 = CARTESIAN_POINT ( 'NONE',  ( -22.47007471830798409, 76.00000000001273293, -211.2438181364508409 ) ) ;
#192621 = CIRCLE ( 'NONE', #34253, 0.09999999999998898659 ) ;
#192622 = FACE_OUTER_BOUND ( 'NONE', #182897, .T. ) ;
#192623 = CARTESIAN_POINT ( 'NONE',  ( -23.15000000000000213, 7.128833340094563376, -233.7327013124401276 ) ) ;
#192624 = CARTESIAN_POINT ( 'NONE',  ( -18.59999999999999787, 11.65000000001115232, -88.35000000000003695 ) ) ;
#192626 = ORIENTED_EDGE ( 'NONE', *, *, #188648, .F. ) ;
#192625 = TOROIDAL_SURFACE ( 'NONE', #218104, 0.9750000000000019762, 0.1000000000000000056 ) ;
#192627 = ORIENTED_EDGE ( 'NONE', *, *, #176541, .F. ) ;
#192629 =( BOUNDED_SURFACE ( )  B_SPLINE_SURFACE ( 3, 2, ( 
 ( #99889, #77774, #238139 ),
 ( #59475, #159922, #2092 ),
 ( #202868, #217283, #197738 ),
 ( #182035, #178209, #19098 ),
 ( #62087, #179485, #790 ),
 ( #118207, #139008, #24261 ) ),
 .UNSPECIFIED., .F., .F., .F. ) 
 B_SPLINE_SURFACE_WITH_KNOTS ( ( 4, 2, 4 ),
 ( 3, 3 ),
 ( -1.776356839400250465E-15, 0.7853981633974468357, 1.570796326794895448 ),
 ( 0.000000000000000000, 1.000000000000000000 ),
 .UNSPECIFIED. ) 
 GEOMETRIC_REPRESENTATION_ITEM ( )  RATIONAL_B_SPLINE_SURFACE ( (
 ( 1.000000000000000000, 0.4999999999999960587, 1.000000000000000000),
 ( 1.000000000000000000, 0.4993418825336311540, 1.000000000000000000),
 ( 1.000000000000000000, 0.5278258667054654962, 1.000000000000000000),
 ( 1.000000000000000000, 0.6092287576699327856, 1.000000000000000000),
 ( 1.000000000000000000, 0.6611148371776465194, 1.000000000000000000),
 ( 1.000000000000000000, 0.7071067811865658914, 1.000000000000000000) ) ) 
 REPRESENTATION_ITEM ( '' )  SURFACE ( )  );
#192628 = AXIS2_PLACEMENT_3D ( 'NONE', #34614, #59239, #154574 ) ;
#192630 = CARTESIAN_POINT ( 'NONE',  ( -21.05000000000000071, 77.85102823015273543, -91.36919421510179973 ) ) ;
#192631 = CARTESIAN_POINT ( 'NONE',  ( -21.05000000000000071, 30.48950451747912993, -239.6099224343151946 ) ) ;
#192632 = EDGE_LOOP ( 'NONE', ( #49882, #198409, #176202, #159127 ) ) ;
#192633 = DIRECTION ( 'NONE',  ( -0.000000000000000000, 0.9908441862701591329, 0.1350103645451946055 ) ) ;
#192634 = ORIENTED_EDGE ( 'NONE', *, *, #71695, .F. ) ;
#192635 = EDGE_CURVE ( 'NONE', #169096, #94374, #162848, .T. ) ;
#192636 = DIRECTION ( 'NONE',  ( 1.000000000000000000, 0.000000000000000000, 0.000000000000000000 ) ) ;
#192637 = AXIS2_PLACEMENT_3D ( 'NONE', #773, #125879, #80310 ) ;
#192638 = CARTESIAN_POINT ( 'NONE',  ( 21.08489834409762409, 60.21194861419059663, -221.1552854090853657 ) ) ;
#192639 = EDGE_CURVE ( 'NONE', #77200, #56652, #25897, .T. ) ;
#192640 = FACE_OUTER_BOUND ( 'NONE', #210345, .T. ) ;
#192641 = VERTEX_POINT ( 'NONE', #62449 ) ;
#192642 = CARTESIAN_POINT ( 'NONE',  ( 21.05000000000000071, -0.09999999998884338825, -88.85042919245522341 ) ) ;
#192643 = TOROIDAL_SURFACE ( 'NONE', #201190, 4.041421356237312246, 0.1000000000000000056 ) ;
#192644 = TOROIDAL_SURFACE ( 'NONE', #21956, 0.6000000000000013101, 0.1000000000000000056 ) ;
#192645 = ORIENTED_EDGE ( 'NONE', *, *, #212427, .F. ) ;
#192647 = ORIENTED_EDGE ( 'NONE', *, *, #203329, .T. ) ;
#192646 = CIRCLE ( 'NONE', #5170, 0.1000000000000055844 ) ;
#192648 = ORIENTED_EDGE ( 'NONE', *, *, #67164, .F. ) ;
#192649 = EDGE_CURVE ( 'NONE', #85729, #116639, #221492, .T. ) ;
#192650 = CARTESIAN_POINT ( 'NONE',  ( -23.25000000000000000, 77.83585931145600512, -158.4186683157258244 ) ) ;
#192651 = CARTESIAN_POINT ( 'NONE',  ( 15.39793903038208001, 66.61031399435591993, -53.85026397817310340 ) ) ;
#192652 = DIRECTION ( 'NONE',  ( 1.000000000000000000, -0.000000000000000000, -0.000000000000000000 ) ) ;
#192654 = EDGE_CURVE ( 'NONE', #36652, #116043, #137712, .T. ) ;
#192653 = DIRECTION ( 'NONE',  ( -0.000000000000000000, 1.000000000000000000, -1.224646799147352961E-16 ) ) ;
#192655 = DIRECTION ( 'NONE',  ( 0.000000000000000000, -0.8660254037844411501, -0.4999999999999956146 ) ) ;
#192657 = DIRECTION ( 'NONE',  ( 1.000000000000000000, 0.000000000000000000, 0.000000000000000000 ) ) ;
#192656 = CARTESIAN_POINT ( 'NONE',  ( 22.44352723754029810, -3.135960183319440375, -228.2236081556235376 ) ) ;
#192659 = VERTEX_POINT ( 'NONE', #5005 ) ;
#192658 = FACE_OUTER_BOUND ( 'NONE', #11394, .T. ) ;
#192660 = CARTESIAN_POINT ( 'NONE',  ( -16.86757978335471719, 9.965650379045438712, -79.59800465316754980 ) ) ;
#192661 = ORIENTED_EDGE ( 'NONE', *, *, #208436, .T. ) ;
#192662 = ADVANCED_FACE ( 'NONE', ( #243641 ), #145814, .T. ) ;
#192663 = DIRECTION ( 'NONE',  ( 1.000000000000000000, 0.000000000000000000, 0.000000000000000000 ) ) ;
#192664 = VERTEX_POINT ( 'NONE', #147095 ) ;
#192665 = ORIENTED_EDGE ( 'NONE', *, *, #239629, .F. ) ;
#192666 = CARTESIAN_POINT ( 'NONE',  ( -20.94999999999999929, -1.835341550224413698, -11.55515129256298046 ) ) ;
#192667 = CARTESIAN_POINT ( 'NONE',  ( -23.15000000000000213, 87.39257802171711376, -39.09705706435617856 ) ) ;
#192668 = LINE ( 'NONE', #248791, #250173 ) ;
#192669 = DIRECTION ( 'NONE',  ( -0.000000000000000000, 0.000000000000000000, -1.000000000000000000 ) ) ;
#192670 = ADVANCED_FACE ( 'NONE', ( #224066 ), #71118, .T. ) ;
#192671 = VECTOR ( 'NONE', #200320, 1000.000000000000000 ) ;
#192672 = FACE_OUTER_BOUND ( 'NONE', #957, .T. ) ;
#192673 = VERTEX_POINT ( 'NONE', #101529 ) ;
#192675 = ORIENTED_EDGE ( 'NONE', *, *, #95399, .T. ) ;
#192674 = ADVANCED_FACE ( 'NONE', ( #225342 ), #180361, .T. ) ;
#192676 = VECTOR ( 'NONE', #65397, 1000.000000000000000 ) ;
#192677 = CARTESIAN_POINT ( 'NONE',  ( -20.85000000000000142, 67.65998959290219261, -227.8609496483021530 ) ) ;
#192678 = ORIENTED_EDGE ( 'NONE', *, *, #216935, .T. ) ;
#192679 = CARTESIAN_POINT ( 'NONE',  ( -20.94999999999999929, 7.120270961708750512, -171.1595630418393625 ) ) ;
#192680 = DIRECTION ( 'NONE',  ( 0.000000000000000000, -1.000000000000000000, -6.982962677686266711E-15 ) ) ;
#192681 = ORIENTED_EDGE ( 'NONE', *, *, #223574, .T. ) ;
#192682 = CARTESIAN_POINT ( 'NONE',  ( 20.94999999999999929, 11.65000000001115943, -93.65839931010299324 ) ) ;
#192683 = DIRECTION ( 'NONE',  ( 1.000000000000000000, -0.000000000000000000, -0.000000000000000000 ) ) ;
#192684 = CARTESIAN_POINT ( 'NONE',  ( -23.15000000000000213, 7.128833340094563376, -233.7327013124401276 ) ) ;
#192685 = CARTESIAN_POINT ( 'NONE',  ( -21.45000000000000284, 7.708578643773852157, -188.6499999999999488 ) ) ;
#192686 = ORIENTED_EDGE ( 'NONE', *, *, #229306, .T. ) ;
#192687 = EDGE_CURVE ( 'NONE', #246301, #234345, #247496, .T. ) ;
#192688 = FACE_OUTER_BOUND ( 'NONE', #38166, .T. ) ;
#192689 = DIRECTION ( 'NONE',  ( -1.000000000000000000, 0.000000000000000000, 0.000000000000000000 ) ) ;
#192690 = CARTESIAN_POINT ( 'NONE',  ( -21.12844524849339223, 57.69819045127058388, -226.1158383967348016 ) ) ;
#192692 = ORIENTED_EDGE ( 'NONE', *, *, #242913, .T. ) ;
#192691 = CIRCLE ( 'NONE', #113572, 0.1000000000000028644 ) ;
#192693 = FACE_OUTER_BOUND ( 'NONE', #17764, .T. ) ;
#192694 = ORIENTED_EDGE ( 'NONE', *, *, #210911, .T. ) ;
#192695 = CARTESIAN_POINT ( 'NONE',  ( 14.77516762759922386, 66.56332574816944714, -154.8462455535252502 ) ) ;
#192696 = FACE_OUTER_BOUND ( 'NONE', #72885, .T. ) ;
#192697 = CARTESIAN_POINT ( 'NONE',  ( -16.87683809663752399, 66.15000000001182912, -82.92547150272068279 ) ) ;
#192698 = DIRECTION ( 'NONE',  ( 0.000000000000000000, -7.086529944415886769E-15, 1.000000000000000000 ) ) ;
#192699 = DIRECTION ( 'NONE',  ( 1.000000000000000000, -3.265361837132813093E-16, -2.280189983783949500E-30 ) ) ;
#192700 = DIRECTION ( 'NONE',  ( -0.000000000000000000, 0.000000000000000000, 1.000000000000000000 ) ) ;
#192701 = VERTEX_POINT ( 'NONE', #88394 ) ;
#192702 = CARTESIAN_POINT ( 'NONE',  ( -16.93302609847409457, 66.00331747920884595, -123.9367189891618182 ) ) ;
#192703 = CARTESIAN_POINT ( 'NONE',  ( -16.87665923198281348, 66.05000000001182059, -82.17310748452439384 ) ) ;
#192704 = DIRECTION ( 'NONE',  ( 0.000000000000000000, 6.982962677686266711E-15, -1.000000000000000000 ) ) ;
#192705 = DIRECTION ( 'NONE',  ( 1.875376730785737966E-16, 0.9651348961777157509, -0.2617529984165031243 ) ) ;
#192706 = CIRCLE ( 'NONE', #146873, 0.1000000000000075273 ) ;
#192708 = CARTESIAN_POINT ( 'NONE',  ( 25.10847955711010115, 9.068702471349586958, -347.0000000000001137 ) ) ;
#192707 = AXIS2_PLACEMENT_3D ( 'NONE', #151100, #32467, #12894 ) ;
#192709 = ADVANCED_FACE ( 'NONE', ( #32332 ), #227936, .F. ) ;
#192710 = ORIENTED_EDGE ( 'NONE', *, *, #177769, .F. ) ;
#192711 = ORIENTED_EDGE ( 'NONE', *, *, #23608, .F. ) ;
#192712 = CARTESIAN_POINT ( 'NONE',  ( 23.40000000000005187, 74.16448838626247664, -47.52760213295649550 ) ) ;
#192714 = DIRECTION ( 'NONE',  ( -1.000000000000000000, 0.000000000000000000, 0.000000000000000000 ) ) ;
#192713 = AXIS2_PLACEMENT_3D ( 'NONE', #98020, #21111, #135872 ) ;
#192715 = DIRECTION ( 'NONE',  ( -1.836970198721029934E-16, 0.9770955615653316162, 0.2128009952263604232 ) ) ;
#192716 = DIRECTION ( 'NONE',  ( 0.000000000000000000, -1.000000000000000000, 0.000000000000000000 ) ) ;
#192717 = EDGE_CURVE ( 'NONE', #14082, #245837, #10179, .T. ) ;
#192718 = EDGE_CURVE ( 'NONE', #115079, #213491, #90981, .T. ) ;
#192719 = ORIENTED_EDGE ( 'NONE', *, *, #21302, .F. ) ;
#192720 = DIRECTION ( 'NONE',  ( 0.000000000000000000, -1.734723475976757554E-14, 1.000000000000000000 ) ) ;
#192721 = DIRECTION ( 'NONE',  ( 0.000000000000000000, 0.9910465087640865089, -0.1335171055202864221 ) ) ;
#192722 = AXIS2_PLACEMENT_3D ( 'NONE', #141278, #215661, #198682 ) ;
#192723 = ADVANCED_FACE ( 'NONE', ( #111846 ), #74032, .T. ) ;
#192724 = ORIENTED_EDGE ( 'NONE', *, *, #71303, .T. ) ;
#192725 = CIRCLE ( 'NONE', #225995, 0.1000000000000028644 ) ;
#192727 = EDGE_CURVE ( 'NONE', #43098, #73251, #131392, .T. ) ;
#192726 = DIRECTION ( 'NONE',  ( 0.000000000000000000, 0.9126074666063660468, 0.4088369013363524762 ) ) ;
#192728 = CARTESIAN_POINT ( 'NONE',  ( -23.15000000000000213, 64.25000000001203659, -114.7731074845243882 ) ) ;
#192729 = EDGE_CURVE ( 'NONE', #108241, #4288, #200280, .T. ) ;
#192730 = EDGE_CURVE ( 'NONE', #178019, #158625, #71448, .T. ) ;
#192731 = ORIENTED_EDGE ( 'NONE', *, *, #39592, .T. ) ;
#192732 = LINE ( 'NONE', #48388, #244072 ) ;
#192733 = EDGE_CURVE ( 'NONE', #117242, #230514, #192668, .T. ) ;
#192734 = AXIS2_PLACEMENT_3D ( 'NONE', #135690, #193126, #151439 ) ;
#192735 = EDGE_LOOP ( 'NONE', ( #138983, #58008, #36795, #41643 ) ) ;
#192736 = CARTESIAN_POINT ( 'NONE',  ( 18.49999999999998934, 56.14960075277880946, -167.7428044267231257 ) ) ;
#192737 = CARTESIAN_POINT ( 'NONE',  ( 20.73486653747088226, 68.75000000001227818, -157.3731074845244109 ) ) ;
#192738 = DIRECTION ( 'NONE',  ( -1.000000000000000000, -3.469446951953635015E-14, 0.000000000000000000 ) ) ;
#192739 = CARTESIAN_POINT ( 'NONE',  ( 21.40925344232282868, 75.90104981139276674, -176.6816263439148145 ) ) ;
#192741 = CIRCLE ( 'NONE', #80257, 0.09999999999998898659 ) ;
#192740 = CARTESIAN_POINT ( 'NONE',  ( 21.05000000000000071, 76.00000000001190870, -103.0231074845243029 ) ) ;
#192742 = DIRECTION ( 'NONE',  ( 0.000000000000000000, 0.000000000000000000, 1.000000000000000000 ) ) ;
#192744 = DIRECTION ( 'NONE',  ( 1.000000000000000000, 0.000000000000000000, 0.000000000000000000 ) ) ;
#192743 = CIRCLE ( 'NONE', #76028, 0.1999999999999987899 ) ;
#192745 = VECTOR ( 'NONE', #142376, 1000.000000000000000 ) ;
#192746 = DIRECTION ( 'NONE',  ( 0.000000000000000000, -7.026728003956686545E-15, 1.000000000000000000 ) ) ;
#192749 = DIRECTION ( 'NONE',  ( 0.000000000000000000, 0.000000000000000000, -1.000000000000000000 ) ) ;
#192748 = CIRCLE ( 'NONE', #59411, 0.09999999999998898659 ) ;
#192747 = CARTESIAN_POINT ( 'NONE',  ( 20.95378194480896639, 10.53491199155394220, -108.0650541481478939 ) ) ;
#192750 = CARTESIAN_POINT ( 'NONE',  ( -20.64999999999999858, 76.00000000001189449, -101.1231074845242972 ) ) ;
#192751 = DIRECTION ( 'NONE',  ( 0.000000000000000000, 1.000000000000000000, 0.000000000000000000 ) ) ;
#192752 = CARTESIAN_POINT ( 'NONE',  ( -21.05000000000000071, 76.00000000001267608, -203.5231074845243597 ) ) ;
#192753 = VERTEX_POINT ( 'NONE', #53143 ) ;
#192754 = CARTESIAN_POINT ( 'NONE',  ( -18.33981767444264932, -9.569575789804277477, -40.31916184372506251 ) ) ;
#192755 = CARTESIAN_POINT ( 'NONE',  ( 21.14999999999999858, -0.09999999998884338825, -100.5000000000000284 ) ) ;
#192756 = CARTESIAN_POINT ( 'NONE',  ( -21.05000000000000071, 1.736257131608553550, -179.0686523290174819 ) ) ;
#192757 = B_SPLINE_CURVE_WITH_KNOTS ( 'NONE', 3,
 ( #135102, #214649, #36039, #115552, #104942, #82810, #164955, #219781, #184506, #46277, #21608, #223623, #142796, #65849, #102376, #239361, #201506, #5864, #85378 ),
 .UNSPECIFIED., .F., .F.,
 ( 4, 3, 3, 3, 3, 3, 4 ),
 ( 1.387778780781445521E-17, 2.646747978908830373E-05, 5.271166642130153582E-05, 9.008788829885479505E-05, 0.0001426648776561217978, 0.0001897378458660037217, 0.0001917382627806517032 ),
 .UNSPECIFIED. ) ;
#192758 = ADVANCED_FACE ( 'NONE', ( #233095 ), #241788, .F. ) ;
#192759 = LINE ( 'NONE', #132794, #43601 ) ;
#192760 = CARTESIAN_POINT ( 'NONE',  ( 23.14999999999999858, 67.23127455305835554, -235.8551265064784559 ) ) ;
#192761 = DIRECTION ( 'NONE',  ( -1.000000000000000000, -1.394253735153569469E-16, -2.602809386958778209E-16 ) ) ;
#192762 = EDGE_CURVE ( 'NONE', #98576, #14611, #161489, .T. ) ;
#192763 = EDGE_CURVE ( 'NONE', #249506, #187671, #189171, .T. ) ;
#192764 = ORIENTED_EDGE ( 'NONE', *, *, #246037, .T. ) ;
#192765 = DIRECTION ( 'NONE',  ( 0.000000000000000000, 1.000000000000000000, 6.982962677686266711E-15 ) ) ;
#192766 = VERTEX_POINT ( 'NONE', #253900 ) ;
#192767 = DIRECTION ( 'NONE',  ( 1.000000000000000000, 0.000000000000000000, 0.000000000000000000 ) ) ;
#192768 = CIRCLE ( 'NONE', #234248, 12.77500000000000924 ) ;
#192769 = ORIENTED_EDGE ( 'NONE', *, *, #175706, .F. ) ;
#192770 = CARTESIAN_POINT ( 'NONE',  ( 23.14999999999999503, 64.25000000001151079, -48.17310748452440805 ) ) ;
#192771 = VECTOR ( 'NONE', #8190, 1000.000000000000000 ) ;
#192772 = ORIENTED_EDGE ( 'NONE', *, *, #125401, .F. ) ;
#192773 = CARTESIAN_POINT ( 'NONE',  ( 20.94999999999999574, -11.74999999999999112, -3.100000000000001865 ) ) ;
#192774 = CARTESIAN_POINT ( 'NONE',  ( 21.05000000000000071, 67.22371711014432094, -124.3468923434561617 ) ) ;
#192776 = VECTOR ( 'NONE', #236605, 1000.000000000000000 ) ;
#192775 = DIRECTION ( 'NONE',  ( 0.000000000000000000, 0.1568667991644355497, -0.9876197685951332295 ) ) ;
#192777 = CARTESIAN_POINT ( 'NONE',  ( 22.39999999999999858, 1.115600667400684642E-11, -100.5000000000000284 ) ) ;
#192778 = CARTESIAN_POINT ( 'NONE',  ( 18.69999999999999574, -11.65000000000000036, 30.00000000000000000 ) ) ;
#192779 = DIRECTION ( 'NONE',  ( -0.000000000000000000, 0.000000000000000000, -1.000000000000000000 ) ) ;
#192780 = AXIS2_PLACEMENT_3D ( 'NONE', #204059, #25446, #163666 ) ;
#192781 = CARTESIAN_POINT ( 'NONE',  ( 20.95000000000005613, 67.75000000001118394, -25.49719488170504533 ) ) ;
#192783 = CARTESIAN_POINT ( 'NONE',  ( -23.15000000000000213, 85.50000000001197975, -112.9170766071766820 ) ) ;
#192782 = CIRCLE ( 'NONE', #188494, 11.79999999999999716 ) ;
#192784 = AXIS2_PLACEMENT_3D ( 'NONE', #71385, #55609, #51776 ) ;
#192786 = ORIENTED_EDGE ( 'NONE', *, *, #70889, .T. ) ;
#192785 = DIRECTION ( 'NONE',  ( -1.836970198721029934E-16, 1.000000000000000000, 0.000000000000000000 ) ) ;
#192788 = DIRECTION ( 'NONE',  ( 0.000000000000000000, -1.000000000000000000, 0.000000000000000000 ) ) ;
#192787 = DIRECTION ( 'NONE',  ( 1.000000000000000000, 0.000000000000000000, 0.000000000000000000 ) ) ;
#192789 = EDGE_LOOP ( 'NONE', ( #57996, #161348, #130243, #105303 ) ) ;
#192791 = ORIENTED_EDGE ( 'NONE', *, *, #129870, .F. ) ;
#192790 = CARTESIAN_POINT ( 'NONE',  ( -22.39999999999999858, 1.115600667400684642E-11, -59.20922040162664501 ) ) ;
#192792 = ORIENTED_EDGE ( 'NONE', *, *, #111579, .F. ) ;
#192793 = DIRECTION ( 'NONE',  ( -0.000000000000000000, 1.000000000000000000, -0.000000000000000000 ) ) ;
#192794 = DIRECTION ( 'NONE',  ( 1.000000000000000000, 0.000000000000000000, 0.000000000000000000 ) ) ;
#192795 = AXIS2_PLACEMENT_3D ( 'NONE', #6137, #85646, #227761 ) ;
#192796 = DIRECTION ( 'NONE',  ( 2.952720810173289112E-16, -1.000000000000000000, 0.000000000000000000 ) ) ;
#192797 = DIRECTION ( 'NONE',  ( 0.000000000000000000, -1.000000000000000000, -1.734723475976807292E-15 ) ) ;
#192798 = CARTESIAN_POINT ( 'NONE',  ( 23.14999999999999858, 3.900000000011155432, -134.0000000000000284 ) ) ;
#192799 = CARTESIAN_POINT ( 'NONE',  ( -20.64999999999999858, 47.91013932883114990, -242.3192343197862044 ) ) ;
#192800 = AXIS2_PLACEMENT_3D ( 'NONE', #196182, #197456, #134892 ) ;
#192801 = FACE_OUTER_BOUND ( 'NONE', #149055, .T. ) ;
#192802 = AXIS2_PLACEMENT_3D ( 'NONE', #160334, #159050, #199453 ) ;
#192803 = EDGE_CURVE ( 'NONE', #181065, #101672, #158608, .T. ) ;
#192804 = DIRECTION ( 'NONE',  ( 0.000000000000000000, 0.000000000000000000, -1.000000000000000000 ) ) ;
#192805 = TOROIDAL_SURFACE ( 'NONE', #230205, 0.2000000000000000111, 0.1000000000000000056 ) ;
#192806 = ORIENTED_EDGE ( 'NONE', *, *, #147768, .T. ) ;
#192807 = ORIENTED_EDGE ( 'NONE', *, *, #145437, .T. ) ;
#192808 = EDGE_CURVE ( 'NONE', #61026, #62345, #176977, .T. ) ;
#192809 = LINE ( 'NONE', #14188, #139770 ) ;
#192810 = VERTEX_POINT ( 'NONE', #40035 ) ;
#192811 = CYLINDRICAL_SURFACE ( 'NONE', #205180, 0.09999999999999691080 ) ;
#192812 = ORIENTED_EDGE ( 'NONE', *, *, #100972, .F. ) ;
#192814 = AXIS2_PLACEMENT_3D ( 'NONE', #78349, #254400, #152801 ) ;
#192813 = CARTESIAN_POINT ( 'NONE',  ( 23.14999999999999858, 1.115600667400684642E-11, -100.5000000000000426 ) ) ;
#192815 = AXIS2_PLACEMENT_3D ( 'NONE', #73449, #212932, #233789 ) ;
#192816 = VECTOR ( 'NONE', #254372, 1000.000000000000000 ) ;
#192817 = EDGE_CURVE ( 'NONE', #220350, #117708, #36168, .T. ) ;
#192818 = AXIS2_PLACEMENT_3D ( 'NONE', #151674, #211623, #108658 ) ;
#192819 = EDGE_CURVE ( 'NONE', #18698, #29243, #29445, .T. ) ;
#192820 = DIRECTION ( 'NONE',  ( 1.000000000000000000, 0.000000000000000000, 0.000000000000000000 ) ) ;
#192821 = CARTESIAN_POINT ( 'NONE',  ( -20.85000000000000142, 0.1610488207298751417, -133.7158101556398151 ) ) ;
#192822 = CARTESIAN_POINT ( 'NONE',  ( -21.05000000000000071, 64.40000000001195701, -109.9513107147998880 ) ) ;
#192823 = DIRECTION ( 'NONE',  ( 1.000000000000000000, 3.190570557967288949E-16, 6.948722487160392945E-17 ) ) ;
#192824 = ORIENTED_EDGE ( 'NONE', *, *, #53617, .T. ) ;
#192825 = CARTESIAN_POINT ( 'NONE',  ( -18.48408745364673678, -9.664322258651997899, -207.6830785333282563 ) ) ;
#192826 = CARTESIAN_POINT ( 'NONE',  ( -20.00857864376270001, 9.350000000000001421, -12.34999999999999964 ) ) ;
#192827 = LINE ( 'NONE', #14204, #50580 ) ;
#192828 = CARTESIAN_POINT ( 'NONE',  ( -20.54999999999999716, -9.499999999988846255, -157.6060308773475924 ) ) ;
#192829 = ORIENTED_EDGE ( 'NONE', *, *, #215686, .T. ) ;
#192831 = DIRECTION ( 'NONE',  ( 1.000000000000000000, 3.190570557967288949E-16, 6.948722487160392945E-17 ) ) ;
#192830 = DIRECTION ( 'NONE',  ( 1.000000000000000000, 0.000000000000000000, 0.000000000000000000 ) ) ;
#192832 = AXIS2_PLACEMENT_3D ( 'NONE', #10362, #148578, #24808 ) ;
#192833 = EDGE_LOOP ( 'NONE', ( #103363, #139037, #48537, #106710 ) ) ;
#192836 = ORIENTED_EDGE ( 'NONE', *, *, #71303, .F. ) ;
#192835 = DIRECTION ( 'NONE',  ( 0.000000000000000000, -6.982962677686266711E-15, 1.000000000000000000 ) ) ;
#192834 = CARTESIAN_POINT ( 'NONE',  ( 21.15000000000005542, 77.16254490893143725, -43.82310748452479743 ) ) ;
#192837 = CIRCLE ( 'NONE', #96918, 0.09999999999999939493 ) ;
#192839 = ADVANCED_FACE ( 'NONE', ( #214779 ), #76550, .T. ) ;
#192838 = CIRCLE ( 'NONE', #176283, 0.09999999999999939493 ) ;
#192840 = DIRECTION ( 'NONE',  ( 0.000000000000000000, -0.008583690987162452199, -0.9999631594459053030 ) ) ;
#192841 = AXIS2_PLACEMENT_3D ( 'NONE', #10395, #209878, #194176 ) ;
#192842 = EDGE_CURVE ( 'NONE', #189967, #163063, #38727, .T. ) ;
#192843 = CARTESIAN_POINT ( 'NONE',  ( -20.94999999999999929, 7.128833340094563376, -233.7327013124401276 ) ) ;
#192844 = VERTEX_POINT ( 'NONE', #154841 ) ;
#192845 = CARTESIAN_POINT ( 'NONE',  ( -21.14999999999994174, 87.50449464844290048, -37.85861909827351468 ) ) ;
#192846 = DIRECTION ( 'NONE',  ( 1.000000000000000000, 1.186688945009010077E-16, 0.000000000000000000 ) ) ;
#192847 = CARTESIAN_POINT ( 'NONE',  ( -22.47886152344871036, -3.122868706952835360, -228.1986027551170935 ) ) ;
#192849 = ORIENTED_EDGE ( 'NONE', *, *, #21985, .F. ) ;
#192848 = CARTESIAN_POINT ( 'NONE',  ( -20.94999999999999929, -1.162701749926853712, -75.00000000000004263 ) ) ;
#192850 = EDGE_CURVE ( 'NONE', #76825, #110925, #187648, .T. ) ;
#192851 = VERTEX_POINT ( 'NONE', #841 ) ;
#192852 = ADVANCED_FACE ( 'NONE', ( #158698 ), #94832, .F. ) ;
#192854 = SPHERICAL_SURFACE ( 'NONE', #78381, 0.1000000000000000056 ) ;
#192853 = AXIS2_PLACEMENT_3D ( 'NONE', #232114, #96414, #92569 ) ;
#192855 = PLANE ( 'NONE',  #176980 ) ;
#192856 = CARTESIAN_POINT ( 'NONE',  ( 23.25000000000000000, -9.599999999988849453, -155.7499999999999716 ) ) ;
#192857 = VERTEX_POINT ( 'NONE', #54424 ) ;
#192858 = CARTESIAN_POINT ( 'NONE',  ( -21.05000000000000071, 6.257814610487270279, -167.4022097086911742 ) ) ;
#192859 = AXIS2_PLACEMENT_3D ( 'NONE', #13496, #232560, #229962 ) ;
#192860 = CARTESIAN_POINT ( 'NONE',  ( -18.50000000000000000, 70.17424292862648372, -198.1782849070719124 ) ) ;
#192861 = CARTESIAN_POINT ( 'NONE',  ( -17.11825945287482753, 9.950000000011131718, -46.15000000000000568 ) ) ;
#192862 = ORIENTED_EDGE ( 'NONE', *, *, #149871, .T. ) ;
#192863 = ADVANCED_FACE ( 'NONE', ( #59527 ), #99943, .F. ) ;
#192864 = DIRECTION ( 'NONE',  ( 0.000000000000000000, -0.2128009952263603677, 0.9770955615653313941 ) ) ;
#192865 = EDGE_CURVE ( 'NONE', #177524, #112449, #212764, .T. ) ;
#192866 = LINE ( 'NONE', #32535, #105548 ) ;
#192867 = ORIENTED_EDGE ( 'NONE', *, *, #163052, .F. ) ;
#192868 = EDGE_CURVE ( 'NONE', #248032, #58200, #175677, .T. ) ;
#192869 = CARTESIAN_POINT ( 'NONE',  ( 23.15000000000000213, 85.50000000001232081, -160.1291383618718385 ) ) ;
#192870 = CARTESIAN_POINT ( 'NONE',  ( -17.71734398241074615, 65.15764277154733009, -92.74824573752999868 ) ) ;
#192871 = B_SPLINE_CURVE_WITH_KNOTS ( 'NONE', 3,
 ( #114592, #98832, #177160, #194149, #18048, #16793, #15514, #96286, #95017, #158873, #218805, #234527, #97557 ),
 .UNSPECIFIED., .F., .F.,
 ( 4, 3, 3, 3, 4 ),
 ( 1.084445006577768341E-16, 1.946463881814435723E-05, 3.922356109944349927E-05, 4.215060953239166332E-05, 4.415117091093087289E-05 ),
 .UNSPECIFIED. ) ;
#192873 = ORIENTED_EDGE ( 'NONE', *, *, #118024, .T. ) ;
#192872 = AXIS2_PLACEMENT_3D ( 'NONE', #146225, #52248, #190529 ) ;
#192874 = ORIENTED_EDGE ( 'NONE', *, *, #10707, .T. ) ;
#192875 = CARTESIAN_POINT ( 'NONE',  ( 19.58285714285715073, 65.61500148966089796, -162.3934228171344785 ) ) ;
#192876 = VERTEX_POINT ( 'NONE', #133953 ) ;
#192878 = ORIENTED_EDGE ( 'NONE', *, *, #140878, .T. ) ;
#192877 = DIRECTION ( 'NONE',  ( 0.000000000000000000, 1.000000000000000000, 2.891205793294679805E-16 ) ) ;
#192879 = ADVANCED_FACE ( 'NONE', ( #216056 ), #37453, .T. ) ;
#192881 = ORIENTED_EDGE ( 'NONE', *, *, #255791, .F. ) ;
#192880 = EDGE_LOOP ( 'NONE', ( #124927, #26901, #5471, #108794 ) ) ;
#192882 = EDGE_CURVE ( 'NONE', #200649, #84649, #8563, .T. ) ;
#192883 = DIRECTION ( 'NONE',  ( 1.000000000000000000, 0.000000000000000000, -0.000000000000000000 ) ) ;
#192884 = CIRCLE ( 'NONE', #76325, 0.2000000000000000944 ) ;
#192885 = VERTEX_POINT ( 'NONE', #256410 ) ;
#192886 = CARTESIAN_POINT ( 'NONE',  ( 18.79999999999999716, 6.726092018229619107, 9.512212474619550662 ) ) ;
#192887 = CARTESIAN_POINT ( 'NONE',  ( 18.49999999999999289, 10.20857864377385127, -88.75000000000004263 ) ) ;
#192888 = DIRECTION ( 'NONE',  ( 1.000000000000000000, 0.000000000000000000, 0.000000000000000000 ) ) ;
#192889 = AXIS2_PLACEMENT_3D ( 'NONE', #128663, #90789, #208204 ) ;
#192890 = CARTESIAN_POINT ( 'NONE',  ( 20.94999999999999929, 71.00000000001199396, -115.4283735034374274 ) ) ;
#192891 = ORIENTED_EDGE ( 'NONE', *, *, #214391, .F. ) ;
#192892 = EDGE_LOOP ( 'NONE', ( #11067, #210794, #140647, #112519 ) ) ;
#192893 = EDGE_LOOP ( 'NONE', ( #168072, #30670, #107900, #147316 ) ) ;
#192894 = AXIS2_PLACEMENT_3D ( 'NONE', #113313, #91188, #174630 ) ;
#192895 = FACE_OUTER_BOUND ( 'NONE', #211717, .T. ) ;
#192897 = ORIENTED_EDGE ( 'NONE', *, *, #79970, .F. ) ;
#192896 = DIRECTION ( 'NONE',  ( 2.952720810173289112E-16, 0.9651348961777157509, -0.2617529984165031243 ) ) ;
#192898 = PLANE ( 'NONE',  #217317 ) ;
#192899 = ORIENTED_EDGE ( 'NONE', *, *, #53200, .T. ) ;
#192900 = VERTEX_POINT ( 'NONE', #20458 ) ;
#192901 = CARTESIAN_POINT ( 'NONE',  ( -18.39999999999999858, 64.52683809665015247, -194.2232782360584622 ) ) ;
#192902 = AXIS2_PLACEMENT_3D ( 'NONE', #142548, #222065, #184250 ) ;
#192903 = TOROIDAL_SURFACE ( 'NONE', #213736, 12.77499999999999858, 0.1000000000000000056 ) ;
#192904 = ORIENTED_EDGE ( 'NONE', *, *, #198157, .T. ) ;
#192905 = AXIS2_PLACEMENT_3D ( 'NONE', #86564, #245671, #64473 ) ;
#192906 = CARTESIAN_POINT ( 'NONE',  ( -22.50000000000000000, 0.000000000000000000, 6.249999999999998224 ) ) ;
#192907 = CARTESIAN_POINT ( 'NONE',  ( -21.05000000000000071, 75.90220970870363715, -176.2809220950004487 ) ) ;
#192909 = ORIENTED_EDGE ( 'NONE', *, *, #92994, .F. ) ;
#192908 = ORIENTED_EDGE ( 'NONE', *, *, #172982, .T. ) ;
#192910 = EDGE_LOOP ( 'NONE', ( #137903, #58683, #3837, #59450, #232377 ) ) ;
#192911 = LINE ( 'NONE', #232050, #90454 ) ;
#192912 = ORIENTED_EDGE ( 'NONE', *, *, #147310, .F. ) ;
#192913 = VERTEX_POINT ( 'NONE', #137797 ) ;
#192915 = LINE ( 'NONE', #74278, #159299 ) ;
#192914 = AXIS2_PLACEMENT_3D ( 'NONE', #89653, #187510, #124954 ) ;
#192917 = ORIENTED_EDGE ( 'NONE', *, *, #34645, .T. ) ;
#192916 = CARTESIAN_POINT ( 'NONE',  ( 18.39999999999999858, -9.682403433465237796, -107.1568433774128408 ) ) ;
#192918 = CARTESIAN_POINT ( 'NONE',  ( 18.49999999999998934, 69.45000000001252261, -182.3731074845244109 ) ) ;
#192919 = PLANE ( 'NONE',  #248701 ) ;
#192920 = CARTESIAN_POINT ( 'NONE',  ( -22.50000000000000000, 76.00000000001267608, -203.5231074845243597 ) ) ;
#192921 = CARTESIAN_POINT ( 'NONE',  ( 20.94999999999999929, 76.00000000001126921, -203.5231074845248997 ) ) ;
#192922 = DIRECTION ( 'NONE',  ( 0.000000000000000000, 0.2617529984165031243, 0.9651348961777157509 ) ) ;
#192923 = ORIENTED_EDGE ( 'NONE', *, *, #6503, .T. ) ;
#192924 = CIRCLE ( 'NONE', #213761, 11.90000000000000746 ) ;
#192925 = AXIS2_PLACEMENT_3D ( 'NONE', #69368, #130605, #112344 ) ;
#192926 = AXIS2_PLACEMENT_3D ( 'NONE', #135642, #93955, #116106 ) ;
#192927 = ORIENTED_EDGE ( 'NONE', *, *, #159583, .T. ) ;
#192929 = CIRCLE ( 'NONE', #80443, 0.1999999999999987899 ) ;
#192928 = DIRECTION ( 'NONE',  ( 0.000000000000000000, 0.000000000000000000, 1.000000000000000000 ) ) ;
#192930 = FACE_OUTER_BOUND ( 'NONE', #179831, .T. ) ;
#192931 = DIRECTION ( 'NONE',  ( 1.000000000000000000, 0.000000000000000000, 0.000000000000000000 ) ) ;
#192932 = EDGE_CURVE ( 'NONE', #228315, #150739, #208497, .T. ) ;
#192933 = ORIENTED_EDGE ( 'NONE', *, *, #230937, .T. ) ;
#192934 = DIRECTION ( 'NONE',  ( 1.000000000000000000, 0.000000000000000000, 0.000000000000000000 ) ) ;
#192935 = CARTESIAN_POINT ( 'NONE',  ( 20.94999999999999929, 5.900000000000005684, -23.28090023534362629 ) ) ;
#192936 = VERTEX_POINT ( 'NONE', #200361 ) ;
#192937 = ORIENTED_EDGE ( 'NONE', *, *, #210980, .F. ) ;
#192938 = CARTESIAN_POINT ( 'NONE',  ( 23.14999999999999147, 1.115600667400684642E-11, -167.4999999999999716 ) ) ;
#192939 = ADVANCED_FACE ( 'NONE', ( #223753 ), #4079, .T. ) ;
#192940 = CARTESIAN_POINT ( 'NONE',  ( -16.77732147278574715, 66.05403306743862402, -123.8595987276485744 ) ) ;
#192941 = ORIENTED_EDGE ( 'NONE', *, *, #40273, .T. ) ;
#192942 = LINE ( 'NONE', #151255, #147156 ) ;
#192943 = ORIENTED_EDGE ( 'NONE', *, *, #113023, .F. ) ;
#192944 = CARTESIAN_POINT ( 'NONE',  ( -20.85000000000000142, 68.97833521811203639, -132.7895420826271220 ) ) ;
#192946 = DIRECTION ( 'NONE',  ( 1.000000000000000000, 0.000000000000000000, 0.000000000000000000 ) ) ;
#192945 = DIRECTION ( 'NONE',  ( 0.000000000000000000, 0.000000000000000000, 1.000000000000000000 ) ) ;
#192947 = EDGE_CURVE ( 'NONE', #59363, #63340, #243322, .T. ) ;
#192949 = EDGE_CURVE ( 'NONE', #143721, #48376, #122111, .T. ) ;
#192948 = CARTESIAN_POINT ( 'NONE',  ( 21.05000000000000071, 64.25000000001146816, -43.03791325517834565 ) ) ;
#192950 = LINE ( 'NONE', #74315, #49178 ) ;
#192951 = DIRECTION ( 'NONE',  ( 0.000000000000000000, -0.4721928772777346239, -0.8814952561688430555 ) ) ;
#192952 = CIRCLE ( 'NONE', #51260, 0.09999999999998898659 ) ;
#192953 = AXIS2_PLACEMENT_3D ( 'NONE', #83847, #200000, #163438 ) ;
#192955 = ORIENTED_EDGE ( 'NONE', *, *, #99740, .T. ) ;
#192954 = DIRECTION ( 'NONE',  ( 1.000000000000000000, 0.000000000000000000, 0.000000000000000000 ) ) ;
#192957 = ORIENTED_EDGE ( 'NONE', *, *, #149911, .T. ) ;
#192956 = ORIENTED_EDGE ( 'NONE', *, *, #8430, .F. ) ;
#192958 = ORIENTED_EDGE ( 'NONE', *, *, #11698, .F. ) ;
#192959 = AXIS2_PLACEMENT_3D ( 'NONE', #228803, #172719, #115262 ) ;
#192960 = ADVANCED_FACE ( 'NONE', ( #182087 ), #140371, .F. ) ;
#192961 = FACE_OUTER_BOUND ( 'NONE', #96650, .T. ) ;
#192962 = CARTESIAN_POINT ( 'NONE',  ( 22.41477678272288188, 0.0008238657629441799605, 11.64958528451539976 ) ) ;
#192963 = AXIS2_PLACEMENT_3D ( 'NONE', #21044, #180107, #80972 ) ;
#192964 = EDGE_CURVE ( 'NONE', #113714, #176243, #195647, .T. ) ;
#192965 = DIRECTION ( 'NONE',  ( 0.000000000000000000, 0.000000000000000000, -1.000000000000000000 ) ) ;
#192966 = CARTESIAN_POINT ( 'NONE',  ( -16.87683809663752399, 66.15000000001255387, -183.4254715027207396 ) ) ;
#192967 = DIRECTION ( 'NONE',  ( 1.000000000000000000, 0.000000000000000000, 0.000000000000000000 ) ) ;
#192968 = ORIENTED_EDGE ( 'NONE', *, *, #235707, .F. ) ;
#192969 = CIRCLE ( 'NONE', #159641, 0.2000000000000057288 ) ;
#192970 = DIRECTION ( 'NONE',  ( 1.000000000000000000, 0.000000000000000000, 0.000000000000000000 ) ) ;
#192971 = VERTEX_POINT ( 'NONE', #62138 ) ;
#192972 = ORIENTED_EDGE ( 'NONE', *, *, #42049, .F. ) ;
#192973 = FACE_OUTER_BOUND ( 'NONE', #233321, .T. ) ;
#192974 = CIRCLE ( 'NONE', #51449, 0.1000000000000028644 ) ;
#192975 = DIRECTION ( 'NONE',  ( 1.000000000000000000, 0.000000000000000000, 0.000000000000000000 ) ) ;
#192976 = CIRCLE ( 'NONE', #205400, 0.1000000000000028644 ) ;
#192977 = VECTOR ( 'NONE', #36401, 1000.000000000000000 ) ;
#192978 = CARTESIAN_POINT ( 'NONE',  ( 21.53699400385212570, 76.00000000000815703, -210.3108192777586964 ) ) ;
#192979 = AXIS2_PLACEMENT_3D ( 'NONE', #252224, #78715, #34502 ) ;
#192980 = CARTESIAN_POINT ( 'NONE',  ( 22.39999999999999503, 7.790779598384535376, -33.50000000000000000 ) ) ;
#192981 = VECTOR ( 'NONE', #248988, 1000.000000000000000 ) ;
#192982 = CARTESIAN_POINT ( 'NONE',  ( 22.40000000000010516, 1.020945751984553285E-11, -155.8504291924548397 ) ) ;
#192983 = ORIENTED_EDGE ( 'NONE', *, *, #191486, .T. ) ;
#192985 = ORIENTED_EDGE ( 'NONE', *, *, #90233, .T. ) ;
#192984 = ADVANCED_FACE ( 'NONE', ( #202921 ), #21730, .T. ) ;
#192986 = CARTESIAN_POINT ( 'NONE',  ( 22.57856590037848576, -0.004128330053175016841, -88.74994153732457391 ) ) ;
#192987 = CARTESIAN_POINT ( 'NONE',  ( -21.52071067811865746, 68.22071067813087097, -148.8731074845244109 ) ) ;
#192988 = DIRECTION ( 'NONE',  ( -1.000000000000000000, -0.000000000000000000, 0.000000000000000000 ) ) ;
#192990 = CIRCLE ( 'NONE', #34784, 0.09999999999999761857 ) ;
#192989 = CARTESIAN_POINT ( 'NONE',  ( -16.97683809663752186, 9.950000000011138823, -187.5976359818036485 ) ) ;
#192991 = DIRECTION ( 'NONE',  ( 1.000000000000000000, 0.000000000000000000, 0.000000000000000000 ) ) ;
#192992 = CARTESIAN_POINT ( 'NONE',  ( -21.07016717456946608, 6.320940838111406279, -33.50000000000000711 ) ) ;
#192994 = DIRECTION ( 'NONE',  ( -1.000000000000000000, -0.000000000000000000, 0.000000000000000000 ) ) ;
#192993 = DIRECTION ( 'NONE',  ( 1.000000000000000000, -0.000000000000000000, -0.000000000000000000 ) ) ;
#192995 = DIRECTION ( 'NONE',  ( -0.000000000000000000, 0.1298341882519953583, 0.9915357197604862671 ) ) ;
#192996 = ADVANCED_FACE ( 'NONE', ( #222455 ), #12077, .T. ) ;
#192997 = DIRECTION ( 'NONE',  ( 1.186688945009009831E-16, -0.9770955615653316162, -0.2128009952263604232 ) ) ;
#192998 = CIRCLE ( 'NONE', #101335, 0.1000000000000033362 ) ;
#192999 = CARTESIAN_POINT ( 'NONE',  ( -20.54999999999999716, 44.87429835298446790, -237.9265065269792103 ) ) ;
#193000 = PLANE ( 'NONE',  #98373 ) ;
#193002 = ORIENTED_EDGE ( 'NONE', *, *, #42364, .T. ) ;
#193001 = CARTESIAN_POINT ( 'NONE',  ( 20.94999999999999574, -11.48912529306490349, -136.9000000000000341 ) ) ;
#193003 = CIRCLE ( 'NONE', #34794, 0.09999999999999939493 ) ;
#193004 = AXIS2_PLACEMENT_3D ( 'NONE', #156199, #36248, #177043 ) ;
#193005 = AXIS2_PLACEMENT_3D ( 'NONE', #204049, #161092, #222299 ) ;
#193006 = AXIS2_PLACEMENT_3D ( 'NONE', #105115, #7340, #221233 ) ;
#193007 = DIRECTION ( 'NONE',  ( 1.000000000000000000, -0.000000000000000000, -0.000000000000000000 ) ) ;
#193008 = DIRECTION ( 'NONE',  ( -1.000000000000000000, 0.000000000000000000, -0.000000000000000000 ) ) ;
#193009 = ADVANCED_FACE ( 'NONE', ( #239495 ), #60831, .T. ) ;
#193010 = DIRECTION ( 'NONE',  ( -0.7071067811865475727, -0.7071067811865475727, 0.000000000000000000 ) ) ;
#193011 = CARTESIAN_POINT ( 'NONE',  ( 18.50000000000000000, 85.40000000001262492, -196.2258477248610120 ) ) ;
#193012 = DIRECTION ( 'NONE',  ( 0.000000000000000000, 0.000000000000000000, 1.000000000000000000 ) ) ;
#193013 = AXIS2_PLACEMENT_3D ( 'NONE', #151152, #155014, #230688 ) ;
#193014 = VECTOR ( 'NONE', #34694, 1000.000000000000000 ) ;
#193015 = AXIS2_PLACEMENT_3D ( 'NONE', #98492, #24159, #180650 ) ;
#193017 = CARTESIAN_POINT ( 'NONE',  ( -20.94999999999999929, 14.05000000001115623, -61.48630492923908974 ) ) ;
#193016 = AXIS2_PLACEMENT_3D ( 'NONE', #188702, #89588, #10068 ) ;
#193018 = CARTESIAN_POINT ( 'NONE',  ( 18.49999999999999289, 10.34378108835317711, -24.82844527787753464 ) ) ;
#193019 = LINE ( 'NONE', #33982, #232069 ) ;
#193020 = EDGE_CURVE ( 'NONE', #18100, #186991, #203991, .T. ) ;
#193021 = EDGE_CURVE ( 'NONE', #168971, #224344, #170731, .T. ) ;
#193022 = ORIENTED_EDGE ( 'NONE', *, *, #253639, .F. ) ;
#193023 = CARTESIAN_POINT ( 'NONE',  ( -18.59999999999999787, 15.92646454033039305, -219.3818586450342707 ) ) ;
#193025 = ORIENTED_EDGE ( 'NONE', *, *, #52572, .F. ) ;
#193024 = CARTESIAN_POINT ( 'NONE',  ( -20.64999999999999858, 4.250000000011156409, -179.7499999999999716 ) ) ;
#193026 = CARTESIAN_POINT ( 'NONE',  ( 21.14999999999999858, 69.35000000001205933, -124.2731074845243455 ) ) ;
#193027 = CARTESIAN_POINT ( 'NONE',  ( -23.15000000000000213, 64.40000000001195701, -109.9513107147998880 ) ) ;
#193029 = ADVANCED_FACE ( 'NONE', ( #25583 ), #242043, .T. ) ;
#193028 = CARTESIAN_POINT ( 'NONE',  ( 23.15000000000000213, 86.30329675166747450, -209.4258251677035787 ) ) ;
#193030 = ADVANCED_FACE ( 'NONE', ( #65981 ), #9855, .T. ) ;
#193031 = ORIENTED_EDGE ( 'NONE', *, *, #71531, .F. ) ;
#193032 = DIRECTION ( 'NONE',  ( 1.000000000000000000, 1.875376730785737719E-16, 0.000000000000000000 ) ) ;
#193033 = PRODUCT_CONTEXT ( 'NONE', #100702, 'mechanical' ) ;
#193034 = LINE ( 'NONE', #96463, #177303 ) ;
#193035 = DIRECTION ( 'NONE',  ( 1.000000000000000000, 0.000000000000000000, 0.000000000000000000 ) ) ;
#193036 = ADVANCED_FACE ( 'NONE', ( #148090 ), #116512, .T. ) ;
#193037 = ORIENTED_EDGE ( 'NONE', *, *, #146782, .T. ) ;
#193038 = DIRECTION ( 'NONE',  ( -3.265361837132813093E-16, -1.000000000000000000, -6.982962677686266711E-15 ) ) ;
#193039 = DIRECTION ( 'NONE',  ( 0.000000000000000000, 1.000000000000000000, 0.000000000000000000 ) ) ;
#193040 = EDGE_CURVE ( 'NONE', #223782, #27458, #89378, .T. ) ;
#193042 = EDGE_CURVE ( 'NONE', #156856, #157570, #74846, .T. ) ;
#193041 = ADVANCED_FACE ( 'NONE', ( #127243 ), #233611, .F. ) ;
#193043 = CIRCLE ( 'NONE', #213873, 0.1000000000000028644 ) ;
#193044 = CARTESIAN_POINT ( 'NONE',  ( 18.59999999999999787, 1.115600667400684642E-11, -67.00000000000004263 ) ) ;
#193045 = ORIENTED_EDGE ( 'NONE', *, *, #188039, .F. ) ;
#193046 = ORIENTED_EDGE ( 'NONE', *, *, #78182, .T. ) ;
#193047 = DIRECTION ( 'NONE',  ( -1.073024830501117725E-15, 6.982962677686266711E-15, -1.000000000000000000 ) ) ;
#193048 = DIRECTION ( 'NONE',  ( 1.000000000000000000, -0.000000000000000000, -0.000000000000000000 ) ) ;
#193049 = LINE ( 'NONE', #191785, #144139 ) ;
#193050 = ADVANCED_FACE ( 'NONE', ( #90664 ), #87266, .T. ) ;
#193051 = DIRECTION ( 'NONE',  ( -0.7071067811865474617, 0.7071067811865474617, 4.937700262164531476E-15 ) ) ;
#193053 = CARTESIAN_POINT ( 'NONE',  ( 22.49436431346199683, -2.413750014042771230, -189.6026474988864550 ) ) ;
#193052 = LINE ( 'NONE', #75679, #28704 ) ;
#193054 = DIRECTION ( 'NONE',  ( 1.000000000000000000, 0.000000000000000000, 0.000000000000000000 ) ) ;
#193056 = EDGE_CURVE ( 'NONE', #109071, #106852, #62348, .T. ) ;
#193055 = DIRECTION ( 'NONE',  ( 1.000000000000000000, -0.000000000000000000, -0.000000000000000000 ) ) ;
#193057 = DIRECTION ( 'NONE',  ( -1.000000000000000000, 0.000000000000000000, 0.000000000000000000 ) ) ;
#193060 = EDGE_CURVE ( 'NONE', #11869, #40953, #24958, .T. ) ;
#193059 = DIRECTION ( 'NONE',  ( 0.000000000000000000, 0.2128009952263403282, -0.9770955615653358350 ) ) ;
#193058 = CIRCLE ( 'NONE', #234739, 0.1000000000000001582 ) ;
#193061 = EDGE_LOOP ( 'NONE', ( #113667, #135700, #218116, #110776 ) ) ;
#193062 = AXIS2_PLACEMENT_3D ( 'NONE', #237333, #155259, #58662 ) ;
#193063 = EDGE_LOOP ( 'NONE', ( #226471, #57448, #71330, #101303 ) ) ;
#193064 = CARTESIAN_POINT ( 'NONE',  ( 18.59999999999997655, 76.00000000001244871, -170.0231074845243597 ) ) ;
#193065 = CARTESIAN_POINT ( 'NONE',  ( -21.09813707148783735, -1.328114159632769020, -194.7545125258655219 ) ) ;
#193068 = DIRECTION ( 'NONE',  ( 0.000000000000000000, 0.2617529984164980728, 0.9651348961777171942 ) ) ;
#193067 = DIRECTION ( 'NONE',  ( 2.952720810173289112E-16, 1.000000000000000000, -6.088138035986627436E-46 ) ) ;
#193066 = CIRCLE ( 'NONE', #105527, 0.09999999999999939493 ) ;
#193069 = EDGE_CURVE ( 'NONE', #239682, #251232, #128525, .T. ) ;
#193070 = ORIENTED_EDGE ( 'NONE', *, *, #121948, .T. ) ;
#193071 = DIRECTION ( 'NONE',  ( 1.000000000000000000, -0.000000000000000000, -0.000000000000000000 ) ) ;
#193072 = DIRECTION ( 'NONE',  ( -1.000000000000000000, -0.000000000000000000, 0.000000000000000000 ) ) ;
#193073 = CARTESIAN_POINT ( 'NONE',  ( 12.84435279558019261, 13.04030727965138503, -216.6527351471937095 ) ) ;
#193074 = ORIENTED_EDGE ( 'NONE', *, *, #177860, .F. ) ;
#193075 = EDGE_CURVE ( 'NONE', #220463, #4416, #187262, .T. ) ;
#193076 = ORIENTED_EDGE ( 'NONE', *, *, #148630, .F. ) ;
#193078 = AXIS2_PLACEMENT_3D ( 'NONE', #9651, #246968, #150465 ) ;
#193077 = CARTESIAN_POINT ( 'NONE',  ( -21.00857864376268935, 64.40000000001188596, -96.09490425424884563 ) ) ;
#193079 = ORIENTED_EDGE ( 'NONE', *, *, #248094, .T. ) ;
#193080 = DIRECTION ( 'NONE',  ( 1.000000000000000000, 0.000000000000000000, 0.000000000000000000 ) ) ;
#193081 = AXIS2_PLACEMENT_3D ( 'NONE', #158510, #60643, #224545 ) ;
#193082 = CARTESIAN_POINT ( 'NONE',  ( -23.15000000000000213, 1.115600667400684642E-11, -63.00000000000000000 ) ) ;
#193083 = FACE_OUTER_BOUND ( 'NONE', #10572, .T. ) ;
#193084 = CIRCLE ( 'NONE', #222253, 0.09999999999998898659 ) ;
#193085 = ORIENTED_EDGE ( 'NONE', *, *, #75245, .F. ) ;
#193086 = CARTESIAN_POINT ( 'NONE',  ( -16.87331047859651179, 9.949999999999986855, -12.65000000000000213 ) ) ;
#193087 = DIRECTION ( 'NONE',  ( 0.000000000000000000, -0.1455152366551522025, -0.9893560106964505163 ) ) ;
#193088 = DIRECTION ( 'NONE',  ( 0.000000000000000000, 0.2128009952263568427, -0.9770955615653322823 ) ) ;
#193089 = CIRCLE ( 'NONE', #88814, 0.5000000000000004441 ) ;
#193091 = CARTESIAN_POINT ( 'NONE',  ( 19.97071067811864609, 11.72071067812981404, -155.3500000000000227 ) ) ;
#193090 = VECTOR ( 'NONE', #39815, 1000.000000000000000 ) ;
#193092 = DIRECTION ( 'NONE',  ( 1.000000000000000000, 0.000000000000000000, 0.000000000000000000 ) ) ;
#193095 = DIRECTION ( 'NONE',  ( 0.000000000000000000, 0.000000000000000000, -1.000000000000000000 ) ) ;
#193094 = TOROIDAL_SURFACE ( 'NONE', #80624, 4.149999999999999467, 0.1000000000000000056 ) ;
#193093 = FACE_OUTER_BOUND ( 'NONE', #206177, .T. ) ;
#193096 = CARTESIAN_POINT ( 'NONE',  ( -16.89935556175703368, 66.05000000001224691, -149.6627838474101964 ) ) ;
#193097 = ORIENTED_EDGE ( 'NONE', *, *, #233872, .T. ) ;
#193099 = DIRECTION ( 'NONE',  ( -3.265361837132813093E-16, 1.000000000000000000, 0.000000000000000000 ) ) ;
#193098 = FACE_OUTER_BOUND ( 'NONE', #190166, .T. ) ;
#193100 = ORIENTED_EDGE ( 'NONE', *, *, #126371, .T. ) ;
#193102 = ORIENTED_EDGE ( 'NONE', *, *, #122082, .F. ) ;
#193101 = FACE_OUTER_BOUND ( 'NONE', #132636, .T. ) ;
#193103 = ORIENTED_EDGE ( 'NONE', *, *, #95479, .F. ) ;
#193104 = CARTESIAN_POINT ( 'NONE',  ( 21.05000000000000071, 76.00000000001142553, -36.02310748452432421 ) ) ;
#193105 = CARTESIAN_POINT ( 'NONE',  ( -21.05000000000000071, 87.48912529308852015, -173.0231074845243029 ) ) ;
#193106 = DIRECTION ( 'NONE',  ( 0.000000000000000000, -0.6626775042260708570, -0.7489048840758791847 ) ) ;
#193107 = CIRCLE ( 'NONE', #176360, 0.09999999999998708533 ) ;
#193108 = CARTESIAN_POINT ( 'NONE',  ( 21.05000000000000071, 5.000000000011153745, -146.4052660189131245 ) ) ;
#193109 = ORIENTED_EDGE ( 'NONE', *, *, #6824, .T. ) ;
#193110 = CARTESIAN_POINT ( 'NONE',  ( 21.12400222705968389, 8.778511907088480726, -112.7500000000000284 ) ) ;
#193111 = DIRECTION ( 'NONE',  ( 0.000000000000000000, 0.9910465087640868420, -0.1335171055202844237 ) ) ;
#193112 = VECTOR ( 'NONE', #87504, 1000.000000000000000 ) ;
#193113 = ORIENTED_EDGE ( 'NONE', *, *, #215932, .T. ) ;
#193114 = CIRCLE ( 'NONE', #205544, 0.09999999999999939493 ) ;
#193115 = VECTOR ( 'NONE', #167772, 1000.000000000000000 ) ;
#193116 = DIRECTION ( 'NONE',  ( 0.000000000000000000, 6.982962677686266711E-15, -1.000000000000000000 ) ) ;
#193117 = CIRCLE ( 'NONE', #80649, 0.2000000000000057288 ) ;
#193118 = EDGE_CURVE ( 'NONE', #145505, #119288, #171531, .T. ) ;
#193119 = CARTESIAN_POINT ( 'NONE',  ( 21.11101077988997332, 6.423684734726043288, 0.01528526891430725086 ) ) ;
#193120 = ORIENTED_EDGE ( 'NONE', *, *, #5696, .T. ) ;
#193121 = EDGE_CURVE ( 'NONE', #182942, #14587, #187235, .T. ) ;
#193122 = CARTESIAN_POINT ( 'NONE',  ( -21.65000000000000213, 9.950000000011140600, -54.25000000000000711 ) ) ;
#193123 = ORIENTED_EDGE ( 'NONE', *, *, #202981, .T. ) ;
#193124 = LINE ( 'NONE', #53604, #254670 ) ;
#193125 = ORIENTED_EDGE ( 'NONE', *, *, #93607, .F. ) ;
#193126 = DIRECTION ( 'NONE',  ( 1.224646799147353454E-16, 0.9770955615653316162, 0.2128009952263604232 ) ) ;
#193127 = EDGE_CURVE ( 'NONE', #75618, #163761, #37420, .T. ) ;
#193128 = ADVANCED_FACE ( 'NONE', ( #88078 ), #245911, .T. ) ;
#193129 = CARTESIAN_POINT ( 'NONE',  ( -22.84999999999999787, 0.000000000000000000, 0.000000000000000000 ) ) ;
#193130 = DIRECTION ( 'NONE',  ( 0.000000000000000000, 0.000000000000000000, 1.000000000000000000 ) ) ;
#193131 = CARTESIAN_POINT ( 'NONE',  ( 20.94999999999999574, 74.83729825007462466, -195.4231074845243654 ) ) ;
#193132 = VECTOR ( 'NONE', #212550, 1000.000000000000227 ) ;
#193133 = CARTESIAN_POINT ( 'NONE',  ( 23.24999999999999289, 64.35000000001258513, -191.3731074845244393 ) ) ;
#193134 = DIRECTION ( 'NONE',  ( 0.000000000000000000, 0.9915357197604973694, -0.1298341882519105928 ) ) ;
#193135 = DIRECTION ( 'NONE',  ( 0.000000000000000000, -0.2128009952263678062, 0.9770955615653298398 ) ) ;
#193136 = CIRCLE ( 'NONE', #101498, 11.74999999999999645 ) ;
#193137 = ORIENTED_EDGE ( 'NONE', *, *, #53108, .T. ) ;
#193139 = DIRECTION ( 'NONE',  ( 0.000000000000000000, 0.000000000000000000, -1.000000000000000000 ) ) ;
#193138 = LINE ( 'NONE', #134408, #91522 ) ;
#193140 = VERTEX_POINT ( 'NONE', #249755 ) ;
#193142 = VERTEX_POINT ( 'NONE', #167672 ) ;
#193141 = CARTESIAN_POINT ( 'NONE',  ( -20.94999999999994600, 64.35000000001119247, -5.923107484524795296 ) ) ;
#193143 = EDGE_CURVE ( 'NONE', #55154, #252148, #216458, .T. ) ;
#193144 = ORIENTED_EDGE ( 'NONE', *, *, #241275, .T. ) ;
#193145 = DIRECTION ( 'NONE',  ( 1.000000000000000000, 0.000000000000000000, 0.000000000000000000 ) ) ;
#193146 = ADVANCED_FACE ( 'NONE', ( #51517 ), #251011, .F. ) ;
#193147 = CARTESIAN_POINT ( 'NONE',  ( -21.10257677756356642, 6.398381742532730065, 0.02495074956798192661 ) ) ;
#193148 = AXIS2_PLACEMENT_3D ( 'NONE', #25093, #225801, #223249 ) ;
#193150 = B_SPLINE_CURVE_WITH_KNOTS ( 'NONE', 3,
 ( #192605, #73971, #193898, #96049, #233036, #54366, #133900, #213438, #34840, #141604, #222393, #217270, #779, #122050, #99879, #201574, #162474, #82878, #123337, #120790, #219854, #97310 ),
 .UNSPECIFIED., .F., .F.,
 ( 4, 3, 3, 3, 3, 3, 3, 4 ),
 ( 0.000000000000000000, 7.307836821080902015E-06, 4.161455748548337322E-05, 7.576591810647894819E-05, 0.0001098090429817568715, 0.0001438003617351259287, 0.0001777914035423789891, 0.0002117966137403053117 ),
 .UNSPECIFIED. ) ;
#193149 = FACE_OUTER_BOUND ( 'NONE', #103102, .T. ) ;
#193151 = FACE_OUTER_BOUND ( 'NONE', #206235, .T. ) ;
#193152 = AXIS2_PLACEMENT_3D ( 'NONE', #2412, #61117, #161527 ) ;
#193153 = ORIENTED_EDGE ( 'NONE', *, *, #176453, .T. ) ;
#193155 = VERTEX_POINT ( 'NONE', #247171 ) ;
#193154 = CARTESIAN_POINT ( 'NONE',  ( -16.88460203013675454, 66.04524099677627191, -115.6572156749861477 ) ) ;
#193156 = AXIS2_PLACEMENT_3D ( 'NONE', #146835, #47735, #223810 ) ;
#193158 = CARTESIAN_POINT ( 'NONE',  ( -16.85718274719454257, 66.02385768539078015, -190.9597611523421392 ) ) ;
#193157 = DIRECTION ( 'NONE',  ( 1.000000000000000000, 0.000000000000000000, 0.000000000000000000 ) ) ;
#193160 = ORIENTED_EDGE ( 'NONE', *, *, #41414, .T. ) ;
#193159 = DIRECTION ( 'NONE',  ( 1.000000000000000000, -0.000000000000000000, -0.000000000000000000 ) ) ;
#193161 = CIRCLE ( 'NONE', #105809, 11.69999999999998863 ) ;
#193162 = AXIS2_PLACEMENT_3D ( 'NONE', #33706, #113194, #233168 ) ;
#193163 = EDGE_CURVE ( 'NONE', #70645, #168421, #132371, .T. ) ;
#193164 = TOROIDAL_SURFACE ( 'NONE', #209719, 0.4000000000000009104, 0.1000000000000000056 ) ;
#193165 = PRODUCT_DEFINITION_SHAPE ( 'NONE', 'NONE',  #152080 ) ;
#193166 = ORIENTED_EDGE ( 'NONE', *, *, #225730, .F. ) ;
#193167 = ADVANCED_FACE ( 'NONE', ( #73711 ), #241964, .F. ) ;
#193168 = VECTOR ( 'NONE', #222656, 1000.000000000000000 ) ;
#193169 = DIRECTION ( 'NONE',  ( 0.000000000000000000, 0.000000000000000000, -1.000000000000000000 ) ) ;
#193170 = DIRECTION ( 'NONE',  ( 0.000000000000000000, -1.000000000000000000, 0.000000000000000000 ) ) ;
#193171 = ORIENTED_EDGE ( 'NONE', *, *, #169021, .T. ) ;
#193172 = DIRECTION ( 'NONE',  ( 1.000000000000000000, 0.000000000000000000, 0.000000000000000000 ) ) ;
#193173 = EDGE_LOOP ( 'NONE', ( #251174, #160504, #78209, #88911, #99986, #220863 ) ) ;
#193174 = PLANE ( 'NONE',  #161765 ) ;
#193175 = DIRECTION ( 'NONE',  ( -0.000000000000000000, 0.4088369013363286064, -0.9126074666063768159 ) ) ;
#193176 = CIRCLE ( 'NONE', #9991, 0.09999999999999939493 ) ;
#193177 = ORIENTED_EDGE ( 'NONE', *, *, #175234, .T. ) ;
#193178 = EDGE_CURVE ( 'NONE', #182882, #100505, #93235, .T. ) ;
#193179 = LINE ( 'NONE', #11980, #220960 ) ;
#193180 = ADVANCED_FACE ( 'NONE', ( #54109 ), #94514, .T. ) ;
#193181 = CIRCLE ( 'NONE', #118144, 12.87499999999999822 ) ;
#193182 = EDGE_CURVE ( 'NONE', #97606, #137421, #158391, .T. ) ;
#193183 = AXIS2_PLACEMENT_3D ( 'NONE', #94731, #174329, #75199 ) ;
#193184 = CIRCLE ( 'NONE', #114041, 0.09999999999999939493 ) ;
#193185 = EDGE_CURVE ( 'NONE', #178200, #32893, #208683, .T. ) ;
#193186 = ORIENTED_EDGE ( 'NONE', *, *, #144793, .F. ) ;
#193187 = CIRCLE ( 'NONE', #18381, 0.1000000000000028644 ) ;
#193188 = ORIENTED_EDGE ( 'NONE', *, *, #205926, .T. ) ;
#193189 = FACE_OUTER_BOUND ( 'NONE', #48069, .T. ) ;
#193190 = ORIENTED_EDGE ( 'NONE', *, *, #189275, .F. ) ;
#193191 = CARTESIAN_POINT ( 'NONE',  ( 12.25000000000000000, 62.10905854918434699, -217.1108499610991203 ) ) ;
#193192 = EDGE_LOOP ( 'NONE', ( #187241, #162946, #213732, #58141 ) ) ;
#193194 = ORIENTED_EDGE ( 'NONE', *, *, #52348, .F. ) ;
#193193 = CARTESIAN_POINT ( 'NONE',  ( -18.50000000000000000, 11.65000000001115232, -40.51480577065400013 ) ) ;
#193195 = EDGE_CURVE ( 'NONE', #38899, #69280, #17144, .T. ) ;
#193196 = ORIENTED_EDGE ( 'NONE', *, *, #195282, .F. ) ;
#193197 = DIRECTION ( 'NONE',  ( 0.000000000000000000, -0.2128009952263403282, 0.9770955615653358350 ) ) ;
#193198 = ORIENTED_EDGE ( 'NONE', *, *, #21428, .T. ) ;
#193201 = ORIENTED_EDGE ( 'NONE', *, *, #186769, .F. ) ;
#193200 = EDGE_LOOP ( 'NONE', ( #64169, #110841, #236187, #220487 ) ) ;
#193199 = CARTESIAN_POINT ( 'NONE',  ( -23.25000000000000000, 1.115600667400684642E-11, -100.5000000000000426 ) ) ;
#193202 = EDGE_CURVE ( 'NONE', #211829, #117589, #162898, .T. ) ;
#193203 = VERTEX_POINT ( 'NONE', #177932 ) ;
#193204 = AXIS2_PLACEMENT_3D ( 'NONE', #189904, #204313, #85624 ) ;
#193205 = CIRCLE ( 'NONE', #134888, 12.97499999999999609 ) ;
#193206 = CARTESIAN_POINT ( 'NONE',  ( 21.07199075132371746, 8.774944999127242795, -45.71353216161286070 ) ) ;
#193207 = ORIENTED_EDGE ( 'NONE', *, *, #188711, .T. ) ;
#193208 = CARTESIAN_POINT ( 'NONE',  ( -16.93521499325732549, 9.994786119814676795, -154.9071085410935780 ) ) ;
#193209 = ADVANCED_FACE ( 'NONE', ( #59206 ), #193633, .F. ) ;
#193211 = VERTEX_POINT ( 'NONE', #55359 ) ;
#193210 = CARTESIAN_POINT ( 'NONE',  ( 21.05000000000000071, 7.128833340094563376, -233.7327013124401276 ) ) ;
#193212 = DIRECTION ( 'NONE',  ( 0.000000000000000000, 0.000000000000000000, -1.000000000000000000 ) ) ;
#193213 = ORIENTED_EDGE ( 'NONE', *, *, #237052, .T. ) ;
#193214 = ORIENTED_EDGE ( 'NONE', *, *, #197695, .T. ) ;
#193215 = ORIENTED_EDGE ( 'NONE', *, *, #242261, .T. ) ;
#193216 = FACE_OUTER_BOUND ( 'NONE', #127483, .T. ) ;
#193217 = CARTESIAN_POINT ( 'NONE',  ( 18.50000972452444969, 18.34807417603286339, -236.8765254748878704 ) ) ;
#193218 = ORIENTED_EDGE ( 'NONE', *, *, #11161, .F. ) ;
#193219 = ORIENTED_EDGE ( 'NONE', *, *, #209137, .F. ) ;
#193220 = DIRECTION ( 'NONE',  ( 1.000000000000000000, 0.000000000000000000, 0.000000000000000000 ) ) ;
#193222 = ORIENTED_EDGE ( 'NONE', *, *, #138232, .T. ) ;
#193221 = ORIENTED_EDGE ( 'NONE', *, *, #245728, .T. ) ;
#193223 = AXIS2_PLACEMENT_3D ( 'NONE', #27341, #130232, #67705 ) ;
#193224 = ORIENTED_EDGE ( 'NONE', *, *, #209757, .T. ) ;
#193225 = DIRECTION ( 'NONE',  ( 1.000000000000000000, -0.000000000000000000, 0.000000000000000000 ) ) ;
#193226 = EDGE_LOOP ( 'NONE', ( #69084, #142339, #167705, #16186 ) ) ;
#193227 = EDGE_LOOP ( 'NONE', ( #78898, #99418, #229520, #63362 ) ) ;
#193228 = CARTESIAN_POINT ( 'NONE',  ( -23.25000000000000355, 9.950000000011138823, -109.7500000000000426 ) ) ;
#193229 = EDGE_LOOP ( 'NONE', ( #46804, #151525, #24590 ) ) ;
#193230 = CYLINDRICAL_SURFACE ( 'NONE', #14940, 0.09999999999999939493 ) ;
#193231 = DIRECTION ( 'NONE',  ( -1.000000000000000000, -3.448943450116723568E-16, -6.438528483529607644E-16 ) ) ;
#193232 = ORIENTED_EDGE ( 'NONE', *, *, #212828, .T. ) ;
#193233 = VERTEX_POINT ( 'NONE', #138745 ) ;
#193234 = DIRECTION ( 'NONE',  ( -0.000000000000000000, -0.000000000000000000, -1.000000000000000000 ) ) ;
#193235 = AXIS2_PLACEMENT_3D ( 'NONE', #145027, #22541, #220727 ) ;
#193236 = ORIENTED_EDGE ( 'NONE', *, *, #221811, .T. ) ;
#193237 = AXIS2_PLACEMENT_3D ( 'NONE', #213590, #136612, #17956 ) ;
#193238 = DIRECTION ( 'NONE',  ( 2.952720810173289112E-16, 1.000000000000000000, 6.467318590049456648E-15 ) ) ;
#193239 = EDGE_LOOP ( 'NONE', ( #199022, #12807, #203740, #148177, #147341, #57148, #131397, #254701, #75280, #245275, #18273, #211041, #112120, #55143, #142288, #139607, #161974, #133768, #50003, #236688, #244266, #130071, #122681, #37286, #164335, #11213, #79964 ) ) ;
#193240 = ORIENTED_EDGE ( 'NONE', *, *, #435, .T. ) ;
#193241 = CARTESIAN_POINT ( 'NONE',  ( -18.40000000000000213, 59.20211495293902004, -220.5705723384363921 ) ) ;
#193242 = EDGE_CURVE ( 'NONE', #24198, #68117, #134906, .T. ) ;
#193244 = ORIENTED_EDGE ( 'NONE', *, *, #177821, .F. ) ;
#193243 = CARTESIAN_POINT ( 'NONE',  ( -16.86133551771148475, 9.950000000011137047, -121.3013434345467090 ) ) ;
#193245 = CARTESIAN_POINT ( 'NONE',  ( 23.24999999999999645, 67.23127455305835554, -235.8551265064784559 ) ) ;
#193246 = CARTESIAN_POINT ( 'NONE',  ( -17.29838795456134193, 31.51142988880226170, -235.0279307012797005 ) ) ;
#193247 = DIRECTION ( 'NONE',  ( 1.000000000000000000, 0.000000000000000000, 0.000000000000000000 ) ) ;
#193248 = CARTESIAN_POINT ( 'NONE',  ( 18.49999999999999289, 33.98796489282362643, -236.2185561567993091 ) ) ;
#193249 = CARTESIAN_POINT ( 'NONE',  ( -20.65000000000000568, 68.75000000001153921, -48.67310748452437252 ) ) ;
#193250 = DIRECTION ( 'NONE',  ( 0.000000000000000000, 0.000000000000000000, -1.000000000000000000 ) ) ;
#193251 = EDGE_CURVE ( 'NONE', #127664, #4373, #8186, .T. ) ;
#193252 = CYLINDRICAL_SURFACE ( 'NONE', #232889, 0.1000000000000028644 ) ;
#193254 = EDGE_CURVE ( 'NONE', #25377, #70370, #241425, .T. ) ;
#193253 = DIRECTION ( 'NONE',  ( 0.000000000000000000, 1.000000000000000000, 0.000000000000000000 ) ) ;
#193255 = DIRECTION ( 'NONE',  ( 0.000000000000000000, 0.000000000000000000, 1.000000000000000000 ) ) ;
#193256 = AXIS2_PLACEMENT_3D ( 'NONE', #22200, #162996, #5151 ) ;
#193257 = CARTESIAN_POINT ( 'NONE',  ( 18.54116936837188589, -9.463564198361288149, -74.04854249088833740 ) ) ;
#193258 = AXIS2_PLACEMENT_3D ( 'NONE', #64722, #185959, #162564 ) ;
#193259 = ORIENTED_EDGE ( 'NONE', *, *, #68420, .T. ) ;
#193260 = CIRCLE ( 'NONE', #234763, 0.09999999999999817368 ) ;
#193261 = AXIS2_PLACEMENT_3D ( 'NONE', #82831, #42453, #119441 ) ;
#193263 = ORIENTED_EDGE ( 'NONE', *, *, #146256, .F. ) ;
#193262 = ORIENTED_EDGE ( 'NONE', *, *, #45816, .T. ) ;
#193264 = ORIENTED_EDGE ( 'NONE', *, *, #14122, .F. ) ;
#193265 = ADVANCED_FACE ( 'NONE', ( #37144 ), #155812, .F. ) ;
#193266 = FACE_OUTER_BOUND ( 'NONE', #12303, .T. ) ;
#193267 = CARTESIAN_POINT ( 'NONE',  ( -20.94999999999999929, 42.90983634497242605, -254.2202269430244996 ) ) ;
#193269 = DIRECTION ( 'NONE',  ( 1.000000000000000000, 0.000000000000000000, -0.000000000000000000 ) ) ;
#193268 = SPHERICAL_SURFACE ( 'NONE', #90829, 0.1000000000000000056 ) ;
#193270 = ORIENTED_EDGE ( 'NONE', *, *, #198602, .F. ) ;
#193271 = ORIENTED_EDGE ( 'NONE', *, *, #1803, .F. ) ;
#193273 = CIRCLE ( 'NONE', #80807, 0.09999999999999939493 ) ;
#193272 =( NAMED_UNIT ( * ) PLANE_ANGLE_UNIT ( ) SI_UNIT ( $, .RADIAN. ) );
#193275 = AXIS2_PLACEMENT_3D ( 'NONE', #194406, #18306, #133126 ) ;
#193274 = LINE ( 'NONE', #118883, #170802 ) ;
#193276 = CARTESIAN_POINT ( 'NONE',  ( -16.87331047859651179, 9.950000000011142376, -180.1499999999999773 ) ) ;
#193277 = CARTESIAN_POINT ( 'NONE',  ( 18.50000000000000000, -9.399999999988843058, -73.88204184817267617 ) ) ;
#193278 = ORIENTED_EDGE ( 'NONE', *, *, #237302, .T. ) ;
#193279 = ORIENTED_EDGE ( 'NONE', *, *, #116425, .T. ) ;
#193280 = CARTESIAN_POINT ( 'NONE',  ( 20.94999999999999929, 77.13501884592227498, -128.8061306010920362 ) ) ;
#193281 = FACE_OUTER_BOUND ( 'NONE', #89640, .T. ) ;
#193282 = AXIS2_PLACEMENT_3D ( 'NONE', #137036, #99164, #20968 ) ;
#193283 = ORIENTED_EDGE ( 'NONE', *, *, #246957, .F. ) ;
#193284 = EDGE_CURVE ( 'NONE', #67110, #247198, #174826, .T. ) ;
#193285 = CARTESIAN_POINT ( 'NONE',  ( 20.94999999999999574, 87.48912529308817909, -133.4231074845242233 ) ) ;
#193287 = EDGE_LOOP ( 'NONE', ( #73775, #211775, #152735, #222049 ) ) ;
#193286 = FACE_OUTER_BOUND ( 'NONE', #128694, .T. ) ;
#193288 = EDGE_CURVE ( 'NONE', #60368, #143581, #116656, .T. ) ;
#193289 = CARTESIAN_POINT ( 'NONE',  ( 22.60000000000000142, 11.74956712350054744, -33.39914163090129762 ) ) ;
#193290 = CARTESIAN_POINT ( 'NONE',  ( -23.25000000000000000, 32.87160343532826090, -251.2478358417912148 ) ) ;
#193291 = TOROIDAL_SURFACE ( 'NONE', #139079, 4.149999999999999467, 0.1000000000000000056 ) ;
#193292 = DIRECTION ( 'NONE',  ( -2.827886303505248273E-16, 0.7397890806274222131, 0.6728388485993010981 ) ) ;
#193294 = ORIENTED_EDGE ( 'NONE', *, *, #192649, .F. ) ;
#193293 = TOROIDAL_SURFACE ( 'NONE', #14240, 0.2000000000000000111, 0.1000000000000000056 ) ;
#193295 = CARTESIAN_POINT ( 'NONE',  ( 13.77030915526558630, 66.54399267394252604, -84.53447399037763432 ) ) ;
#193296 = CARTESIAN_POINT ( 'NONE',  ( 20.94999999999999929, -1.835341550213257733, -112.0551512925630249 ) ) ;
#193297 = CARTESIAN_POINT ( 'NONE',  ( -20.64999999999999858, 85.40000000001148805, -45.91707660717669626 ) ) ;
#193298 = AXIS2_PLACEMENT_3D ( 'NONE', #200426, #41378, #21800 ) ;
#193300 = DIRECTION ( 'NONE',  ( -1.000000000000000000, 0.000000000000000000, 0.000000000000000000 ) ) ;
#193299 = DIRECTION ( 'NONE',  ( -0.000000000000000000, 0.8454177738465993297, 0.5341055959866553016 ) ) ;
#193301 = DIRECTION ( 'NONE',  ( 1.000000000000000000, 7.304098846218105085E-16, 4.217023435051676515E-16 ) ) ;
#193302 = EDGE_CURVE ( 'NONE', #227126, #33556, #137514, .T. ) ;
#193303 = CARTESIAN_POINT ( 'NONE',  ( -16.90987985657661952, 9.957807518190888274, -121.3692870888836666 ) ) ;
#193304 = DIRECTION ( 'NONE',  ( 2.259780016855445309E-14, 0.9875055080513753802, -0.1575844902526748192 ) ) ;
#193305 = CARTESIAN_POINT ( 'NONE',  ( 20.85000000000000142, 68.87972903831452243, -132.8635444426850825 ) ) ;
#193306 = EDGE_LOOP ( 'NONE', ( #19583, #103099, #203983, #239578 ) ) ;
#193307 = VERTEX_POINT ( 'NONE', #256099 ) ;
#193308 = CARTESIAN_POINT ( 'NONE',  ( 20.94999999999999574, 1.115600667400684642E-11, -100.5000000000000284 ) ) ;
#193309 = DIRECTION ( 'NONE',  ( 0.000000000000000000, -7.026728003956695223E-15, 1.000000000000000000 ) ) ;
#193310 = ORIENTED_EDGE ( 'NONE', *, *, #18379, .F. ) ;
#193311 = CARTESIAN_POINT ( 'NONE',  ( 21.07928932188134397, 7.128833340093095217, -233.7327013124392749 ) ) ;
#193313 = EDGE_CURVE ( 'NONE', #62787, #235390, #166606, .T. ) ;
#193312 = ORIENTED_EDGE ( 'NONE', *, *, #145704, .F. ) ;
#193314 = VECTOR ( 'NONE', #213933, 1000.000000000000000 ) ;
#193315 = CIRCLE ( 'NONE', #60008, 0.09999999999999939493 ) ;
#193316 = VERTEX_POINT ( 'NONE', #236589 ) ;
#193317 = CARTESIAN_POINT ( 'NONE',  ( 21.05000000000000071, 76.09999993531907592, -109.5011857056189086 ) ) ;
#193318 = VERTEX_POINT ( 'NONE', #239175 ) ;
#193319 = CARTESIAN_POINT ( 'NONE',  ( 18.43565242384935488, -7.817436562502985353, -209.8389866835000532 ) ) ;
#193320 = CARTESIAN_POINT ( 'NONE',  ( 18.59999999999999787, 1.115600667400684642E-11, -100.5000000000000284 ) ) ;
#193321 = LINE ( 'NONE', #253271, #144339 ) ;
#193322 = AXIS2_PLACEMENT_3D ( 'NONE', #18337, #179994, #159160 ) ;
#193323 = EDGE_CURVE ( 'NONE', #185627, #210872, #21438, .T. ) ;
#193324 = CIRCLE ( 'NONE', #139305, 0.1000000000000055844 ) ;
#193325 = DIRECTION ( 'NONE',  ( 0.000000000000000000, 0.000000000000000000, -1.000000000000000000 ) ) ;
#193326 = DIRECTION ( 'NONE',  ( 1.000000000000000000, -0.000000000000000000, 0.000000000000000000 ) ) ;
#193328 = ORIENTED_EDGE ( 'NONE', *, *, #68038, .F. ) ;
#193327 = CARTESIAN_POINT ( 'NONE',  ( -16.82542659449991262, 30.11558868677414225, -234.7760220207075861 ) ) ;
#193330 = CARTESIAN_POINT ( 'NONE',  ( 19.75857864376269291, 11.65000000001116476, -192.2499999999999716 ) ) ;
#193329 = DIRECTION ( 'NONE',  ( 1.000000000000000000, 0.000000000000000000, 0.000000000000000000 ) ) ;
#193331 = CARTESIAN_POINT ( 'NONE',  ( -23.25000000000000000, -9.682403433465239573, -174.1568433774127982 ) ) ;
#193332 =( BOUNDED_CURVE ( )  B_SPLINE_CURVE ( 3, ( #175913, #198001, #37682, #239716 ),
 .UNSPECIFIED., .F., .F. ) 
 B_SPLINE_CURVE_WITH_KNOTS ( ( 4, 4 ),
 ( 3.141592653589791784, 4.712388980384688786 ),
 .UNSPECIFIED. ) 
 CURVE ( )  GEOMETRIC_REPRESENTATION_ITEM ( )  RATIONAL_B_SPLINE_CURVE ( ( 1.000000000000000000, 0.8047378541243649375, 0.8047378541243649375, 1.000000000000000000 ) ) 
 REPRESENTATION_ITEM ( '' )  );
#193333 = CARTESIAN_POINT ( 'NONE',  ( 23.14999999999999503, 64.35000000001258513, -191.3731074845244393 ) ) ;
#193334 = VECTOR ( 'NONE', #156855, 1000.000000000000114 ) ;
#193335 = DIRECTION ( 'NONE',  ( -0.000000000000000000, -0.2617529984165031243, -0.9651348961777157509 ) ) ;
#193337 = EDGE_CURVE ( 'NONE', #118383, #66864, #70941, .T. ) ;
#193336 = DIRECTION ( 'NONE',  ( 1.000000000000000000, 3.469446951953704435E-14, -2.003086131649669752E-14 ) ) ;
#193338 = EDGE_CURVE ( 'NONE', #155087, #148690, #80056, .T. ) ;
#193339 = ORIENTED_EDGE ( 'NONE', *, *, #76111, .T. ) ;
#193340 = VECTOR ( 'NONE', #5924, 1000.000000000000114 ) ;
#193341 = SURFACE_STYLE_USAGE ( .BOTH. , #111224 ) ;
#193342 = DIRECTION ( 'NONE',  ( 1.000000000000000000, 0.000000000000000000, 0.000000000000000000 ) ) ;
#193343 = AXIS2_PLACEMENT_3D ( 'NONE', #146238, #223207, #82393 ) ;
#193344 = CIRCLE ( 'NONE', #80883, 0.1000000000000055844 ) ;
#193345 = EDGE_LOOP ( 'NONE', ( #106326, #215637, #83379, #179 ) ) ;
#193346 = DIRECTION ( 'NONE',  ( 0.000000000000000000, 1.000000000000000000, 0.000000000000000000 ) ) ;
#193347 = ORIENTED_EDGE ( 'NONE', *, *, #100846, .T. ) ;
#193348 = VECTOR ( 'NONE', #225215, 1000.000000000000000 ) ;
#193349 = ADVANCED_FACE ( 'NONE', ( #547 ), #83903, .F. ) ;
#193350 = FACE_OUTER_BOUND ( 'NONE', #120204, .T. ) ;
#193351 = EDGE_CURVE ( 'NONE', #200569, #86393, #133259, .T. ) ;
#193352 =( BOUNDED_CURVE ( )  B_SPLINE_CURVE ( 3, ( #238997, #241554, #60337, #139867 ),
 .UNSPECIFIED., .F., .F. ) 
 B_SPLINE_CURVE_WITH_KNOTS ( ( 4, 4 ),
 ( 3.752122642744676995, 4.712388980384671910 ),
 .UNSPECIFIED. ) 
 CURVE ( )  GEOMETRIC_REPRESENTATION_ITEM ( )  RATIONAL_B_SPLINE_CURVE ( ( 1.000000000000000000, 0.9246222802177364031, 0.9246222802177364031, 1.000000000000000000 ) ) 
 REPRESENTATION_ITEM ( '' )  );
#193353 = CARTESIAN_POINT ( 'NONE',  ( -16.94333152882356330, 9.990342011457666871, -20.89203153110148747 ) ) ;
#193354 = FACE_OUTER_BOUND ( 'NONE', #150211, .T. ) ;
#193355 = ORIENTED_EDGE ( 'NONE', *, *, #231466, .F. ) ;
#193356 = ADVANCED_FACE ( 'NONE', ( #181774 ), #223446, .F. ) ;
#193357 = ORIENTED_EDGE ( 'NONE', *, *, #47184, .F. ) ;
#193358 = CARTESIAN_POINT ( 'NONE',  ( 20.04142135623730070, 64.35000000001222986, -148.7731074845244450 ) ) ;
#193359 = CARTESIAN_POINT ( 'NONE',  ( 18.59999999999999432, -1.162701749926853712, -41.60000000000000142 ) ) ;
#193360 = EDGE_CURVE ( 'NONE', #23846, #253904, #145195, .T. ) ;
#193361 = CARTESIAN_POINT ( 'NONE',  ( 20.85000000000000142, 64.75617845954087670, -200.4736850529726269 ) ) ;
#193362 = CARTESIAN_POINT ( 'NONE',  ( -18.54118089899633048, -9.463537631836938857, -141.0485775978681602 ) ) ;
#193364 = DIRECTION ( 'NONE',  ( 0.000000000000000000, 1.000000000000000000, 0.000000000000000000 ) ) ;
#193363 = DIRECTION ( 'NONE',  ( 0.000000000000000000, -0.008583690987162452199, -0.9999631594459053030 ) ) ;
#193366 = MANIFOLD_SOLID_BREP ( 'Stock-MAS-200-1', #190674 ) ;
#193365 = DIRECTION ( 'NONE',  ( 0.000000000000000000, -0.2128009952263485993, 0.9770955615653341697 ) ) ;
#193367 = EDGE_CURVE ( 'NONE', #67142, #62135, #12475, .T. ) ;
#193369 = EDGE_CURVE ( 'NONE', #161116, #24547, #43553, .T. ) ;
#193368 = CARTESIAN_POINT ( 'NONE',  ( -17.78043020864321022, 32.67194018624805096, -235.1027381854017335 ) ) ;
#193370 = AXIS2_PLACEMENT_3D ( 'NONE', #62698, #224328, #136093 ) ;
#193371 = ORIENTED_EDGE ( 'NONE', *, *, #199194, .T. ) ;
#193373 =( BOUNDED_SURFACE ( )  B_SPLINE_SURFACE ( 3, 2, ( 
 ( #22061, #101544, #104126 ),
 ( #45456, #125009, #147113 ),
 ( #85833, #105391, #127567 ),
 ( #48016, #168016, #225360 ) ),
 .UNSPECIFIED., .F., .F., .F. ) 
 B_SPLINE_SURFACE_WITH_KNOTS ( ( 4, 4 ),
 ( 3, 3 ),
 ( 4.712388980384689674, 5.765869716888531116 ),
 ( 0.000000000000000000, 1.000000000000000000 ),
 .UNSPECIFIED. ) 
 GEOMETRIC_REPRESENTATION_ITEM ( )  RATIONAL_B_SPLINE_SURFACE ( (
 ( 1.000000000000000000, 0.7071067811865475727, 1.000000000000000000),
 ( 1.000000000000000000, 0.7953136715913434740, 1.000000000000000000),
 ( 1.000000000000000000, 0.8646876308615311091, 1.000000000000000000),
 ( 1.000000000000000000, 0.8984936768950603225, 1.000000000000000000) ) ) 
 REPRESENTATION_ITEM ( '' )  SURFACE ( )  );
#193372 = CARTESIAN_POINT ( 'NONE',  ( 21.14999999999999858, 64.35000000001221565, -148.2731074845243882 ) ) ;
#193374 = AXIS2_PLACEMENT_3D ( 'NONE', #257946, #217564, #97607 ) ;
#193376 = ORIENTED_EDGE ( 'NONE', *, *, #48963, .T. ) ;
#193375 = FACE_OUTER_BOUND ( 'NONE', #153138, .T. ) ;
#193377 = AXIS2_PLACEMENT_3D ( 'NONE', #252065, #89138, #31774 ) ;
#193378 = DIRECTION ( 'NONE',  ( 1.000000000000000000, 0.000000000000000000, 0.000000000000000000 ) ) ;
#193379 = DIRECTION ( 'NONE',  ( 0.000000000000000000, 7.056502275159890832E-15, -1.000000000000000000 ) ) ;
#193381 = CARTESIAN_POINT ( 'NONE',  ( -18.39999999999999858, -0.9152171842607024210, -242.2974985173726452 ) ) ;
#193380 = DIRECTION ( 'NONE',  ( 0.000000000000000000, 0.000000000000000000, -1.000000000000000000 ) ) ;
#193382 = EDGE_CURVE ( 'NONE', #244668, #19771, #229118, .T. ) ;
#193384 = ORIENTED_EDGE ( 'NONE', *, *, #141502, .T. ) ;
#193383 = CARTESIAN_POINT ( 'NONE',  ( 22.47007471830798409, 68.27928934808569750, -136.5231074845243597 ) ) ;
#193385 = DIRECTION ( 'NONE',  ( -1.000000000000000000, -0.000000000000000000, -0.000000000000000000 ) ) ;
#193386 = DIRECTION ( 'NONE',  ( 0.000000000000000000, -1.000000000000000000, 0.000000000000000000 ) ) ;
#193387 = FACE_OUTER_BOUND ( 'NONE', #65086, .T. ) ;
#193388 = CARTESIAN_POINT ( 'NONE',  ( -23.15000000000000213, 64.35000000001195986, -110.0379132551783243 ) ) ;
#193389 = CARTESIAN_POINT ( 'NONE',  ( -18.50016250449483479, 10.29766095125289738, -139.4743663933276139 ) ) ;
#193390 = ORIENTED_EDGE ( 'NONE', *, *, #254426, .T. ) ;
#193391 = DIRECTION ( 'NONE',  ( 1.000000000000000000, 0.000000000000000000, 0.000000000000000000 ) ) ;
#193392 = EDGE_CURVE ( 'NONE', #6741, #254308, #8375, .T. ) ;
#193393 = EDGE_LOOP ( 'NONE', ( #9039, #218221, #53754, #214210 ) ) ;
#193394 = EDGE_CURVE ( 'NONE', #149274, #169179, #243015, .T. ) ;
#193395 = EDGE_CURVE ( 'NONE', #73952, #201073, #5668, .T. ) ;
#193396 = B_SPLINE_CURVE_WITH_KNOTS ( 'NONE', 3,
 ( #94233, #9563, #168697, #248187, #91673, #228640 ),
 .UNSPECIFIED., .F., .F.,
 ( 4, 2, 4 ),
 ( 0.000000000000000000, 0.0001891491689349576852, 0.0003782983378699153704 ),
 .UNSPECIFIED. ) ;
#193397 = LINE ( 'NONE', #18593, #71777 ) ;
#193398 = ORIENTED_EDGE ( 'NONE', *, *, #225133, .F. ) ;
#193399 = CARTESIAN_POINT ( 'NONE',  ( -23.25000000000000000, 4.350000000011156054, -79.35000000000005116 ) ) ;
#193400 = CIRCLE ( 'NONE', #85006, 0.1000000000000052097 ) ;
#193401 = ORIENTED_EDGE ( 'NONE', *, *, #111278, .F. ) ;
#193402 = CARTESIAN_POINT ( 'NONE',  ( -21.17356465864818205, 6.422803126252873973, -167.4010887589861056 ) ) ;
#193403 = VECTOR ( 'NONE', #151011, 1000.000000000000114 ) ;
#193404 = CARTESIAN_POINT ( 'NONE',  ( -21.14999999999994174, 65.87745128126655914, -37.09527722473000466 ) ) ;
#193405 = ORIENTED_EDGE ( 'NONE', *, *, #56019, .T. ) ;
#193406 = ADVANCED_FACE ( 'NONE', ( #104762 ), #86486, .T. ) ;
#193407 = DIRECTION ( 'NONE',  ( 0.000000000000000000, -6.467318590049456648E-15, 1.000000000000000000 ) ) ;
#193408 = CARTESIAN_POINT ( 'NONE',  ( -21.14999999999999858, 64.35000000001195986, -102.9231074845243938 ) ) ;
#193409 = FACE_OUTER_BOUND ( 'NONE', #142443, .T. ) ;
#193410 = CYLINDRICAL_SURFACE ( 'NONE', #174639, 0.1000000000000024342 ) ;
#193411 = DIRECTION ( 'NONE',  ( 1.000000000000000000, 0.000000000000000000, 0.000000000000000000 ) ) ;
#193412 = ORIENTED_EDGE ( 'NONE', *, *, #79942, .F. ) ;
#193413 = DIRECTION ( 'NONE',  ( -1.073024830501117725E-15, -0.000000000000000000, -1.000000000000000000 ) ) ;
#193414 = ORIENTED_EDGE ( 'NONE', *, *, #255629, .T. ) ;
#193416 = ORIENTED_EDGE ( 'NONE', *, *, #93580, .F. ) ;
#193415 = DIRECTION ( 'NONE',  ( 0.000000000000000000, 0.000000000000000000, 1.000000000000000000 ) ) ;
#193417 = ORIENTED_EDGE ( 'NONE', *, *, #130190, .T. ) ;
#193418 = CIRCLE ( 'NONE', #10424, 0.1000000000000124678 ) ;
#193419 = CARTESIAN_POINT ( 'NONE',  ( 21.53699400385583118, 6.353297217273429908E-12, -60.21228820676886784 ) ) ;
#193420 = CARTESIAN_POINT ( 'NONE',  ( -21.05000000000000071, 14.72981487416292623, -236.4853282537515895 ) ) ;
#193421 = DIRECTION ( 'NONE',  ( -1.000000000000000000, 0.000000000000000000, 0.000000000000000000 ) ) ;
#193422 = CARTESIAN_POINT ( 'NONE',  ( -22.59999970745345976, 76.00935637733928729, -81.27362069219354623 ) ) ;
#193423 = ORIENTED_EDGE ( 'NONE', *, *, #8165, .F. ) ;
#193424 = PLANE ( 'NONE',  #217946 ) ;
#193425 = CYLINDRICAL_SURFACE ( 'NONE', #68728, 0.09999999999998898659 ) ;
#193426 = ORIENTED_EDGE ( 'NONE', *, *, #153904, .F. ) ;
#193428 = ORIENTED_EDGE ( 'NONE', *, *, #190932, .F. ) ;
#193427 = DIRECTION ( 'NONE',  ( -1.000000000000000000, -0.000000000000000000, -0.000000000000000000 ) ) ;
#193429 = CARTESIAN_POINT ( 'NONE',  ( 21.05000000000000071, 77.73625713160926409, -91.45445515550680682 ) ) ;
#193430 = CARTESIAN_POINT ( 'NONE',  ( 21.05000000000000071, 1.115600667400684642E-11, -200.9999999999999432 ) ) ;
#193431 = EDGE_CURVE ( 'NONE', #251013, #237327, #12660, .T. ) ;
#193433 = CIRCLE ( 'NONE', #147612, 0.09999999999999971412 ) ;
#193432 = DIRECTION ( 'NONE',  ( 0.000000000000000000, 0.7397360091702755991, -0.6728971962616832059 ) ) ;
#193434 = EDGE_CURVE ( 'NONE', #227881, #123705, #158238, .T. ) ;
#193435 = CIRCLE ( 'NONE', #110189, 0.09999999999999939493 ) ;
#193436 = ORIENTED_EDGE ( 'NONE', *, *, #16107, .T. ) ;
#193437 = AXIS2_PLACEMENT_3D ( 'NONE', #216055, #233094, #94831 ) ;
#193438 = VECTOR ( 'NONE', #31013, 1000.000000000000000 ) ;
#193439 = DIRECTION ( 'NONE',  ( -1.000000000000000000, 7.510212038922875604E-17, -1.676432719286210708E-16 ) ) ;
#193440 = ORIENTED_EDGE ( 'NONE', *, *, #96220, .F. ) ;
#193441 = DIRECTION ( 'NONE',  ( 0.000000000000000000, 0.000000000000000000, -1.000000000000000000 ) ) ;
#193442 = PRESENTATION_LAYER_ASSIGNMENT (  '', '', ( #180948 ) ) ;
#193443 = CARTESIAN_POINT ( 'NONE',  ( 21.02374657821565407, 64.39999999919231755, -176.9513107143264108 ) ) ;
#193444 = LINE ( 'NONE', #35670, #134293 ) ;
#193445 = AXIS2_PLACEMENT_3D ( 'NONE', #230662, #128993, #226790 ) ;
#193446 = ADVANCED_FACE ( 'NONE', ( #169958 ), #129505, .F. ) ;
#193447 = CIRCLE ( 'NONE', #68534, 0.09999999999999939493 ) ;
#193448 = AXIS2_PLACEMENT_3D ( 'NONE', #179366, #137628, #238025 ) ;
#193449 = ORIENTED_EDGE ( 'NONE', *, *, #124166, .T. ) ;
#193450 = CARTESIAN_POINT ( 'NONE',  ( 20.85000000000000142, 11.75000000001115907, -60.21613433702191287 ) ) ;
#193451 = CIRCLE ( 'NONE', #222630, 0.1000000000000028644 ) ;
#193452 = AXIS2_PLACEMENT_3D ( 'NONE', #249189, #127952, #70574 ) ;
#193453 = ORIENTED_EDGE ( 'NONE', *, *, #248014, .F. ) ;
#193454 = CARTESIAN_POINT ( 'NONE',  ( -23.15000000000000213, 84.59626168225506149, -127.0729799673739677 ) ) ;
#193455 = DIRECTION ( 'NONE',  ( -3.265361837132813093E-16, 1.000000000000000000, 0.000000000000000000 ) ) ;
#193457 = VERTEX_POINT ( 'NONE', #231191 ) ;
#193456 = DIRECTION ( 'NONE',  ( 1.000000000000000000, -0.000000000000000000, 0.000000000000000000 ) ) ;
#193458 = DIRECTION ( 'NONE',  ( 0.000000000000000000, -0.1350103645451807555, -0.9908441862701610203 ) ) ;
#193459 = LINE ( 'NONE', #72229, #24111 ) ;
#193460 = CARTESIAN_POINT ( 'NONE',  ( -20.94999999999999929, 68.48451787451661232, -224.2224406095231757 ) ) ;
#193461 = DIRECTION ( 'NONE',  ( 1.000000000000000000, 0.000000000000000000, 0.000000000000000000 ) ) ;
#193462 = CARTESIAN_POINT ( 'NONE',  ( 21.05000000000000071, 6.540656951712399803, -33.50000000000000000 ) ) ;
#193463 = AXIS2_PLACEMENT_3D ( 'NONE', #168101, #224162, #106781 ) ;
#193464 = CIRCLE ( 'NONE', #122541, 0.1000000000000118433 ) ;
#193465 = SPHERICAL_SURFACE ( 'NONE', #130640, 0.1000000000000000056 ) ;
#193466 = CIRCLE ( 'NONE', #31172, 4.049999999999998046 ) ;
#193467 = DIRECTION ( 'NONE',  ( 0.000000000000000000, -0.4721928772777346794, -0.8814952561688431665 ) ) ;
#193469 = ORIENTED_EDGE ( 'NONE', *, *, #213959, .T. ) ;
#193468 = DIRECTION ( 'NONE',  ( 0.000000000000000000, 0.000000000000000000, -1.000000000000000000 ) ) ;
#193470 = AXIS2_PLACEMENT_3D ( 'NONE', #17650, #135017, #119342 ) ;
#193471 = DIRECTION ( 'NONE',  ( -0.000000000000000000, -0.8814952561688430555, 0.4721928772777346239 ) ) ;
#193472 = AXIS2_PLACEMENT_3D ( 'NONE', #85680, #42742, #206954 ) ;
#193473 = DIRECTION ( 'NONE',  ( 0.000000000000000000, -1.000000000000000000, 0.000000000000000000 ) ) ;
#193474 = DIRECTION ( 'NONE',  ( -4.408576920032447972E-17, -0.1350103645451946055, 0.9908441862701591329 ) ) ;
#193475 = VECTOR ( 'NONE', #197956, 1000.000000000000000 ) ;
#193477 = ORIENTED_EDGE ( 'NONE', *, *, #29972, .F. ) ;
#193476 = AXIS2_PLACEMENT_3D ( 'NONE', #72884, #169422, #248934 ) ;
#193478 = EDGE_CURVE ( 'NONE', #140944, #157963, #29163, .T. ) ;
#193479 = CARTESIAN_POINT ( 'NONE',  ( 21.05000000000000071, 69.45934304831143891, -203.4231074845244223 ) ) ;
#193480 = DIRECTION ( 'NONE',  ( 0.000000000000000000, 0.000000000000000000, 1.000000000000000000 ) ) ;
#193481 = EDGE_CURVE ( 'NONE', #80879, #200341, #191551, .T. ) ;
#193482 = LINE ( 'NONE', #115208, #153437 ) ;
#193483 = ORIENTED_EDGE ( 'NONE', *, *, #75342, .T. ) ;
#193484 = CARTESIAN_POINT ( 'NONE',  ( -23.15000000000000213, 2.599999999999998312, -20.27537807723789953 ) ) ;
#193485 = FACE_OUTER_BOUND ( 'NONE', #56040, .T. ) ;
#193486 = EDGE_CURVE ( 'NONE', #221706, #53335, #148514, .T. ) ;
#193487 = VERTEX_POINT ( 'NONE', #210334 ) ;
#193488 = DIRECTION ( 'NONE',  ( 0.000000000000000000, 0.2128009952263603677, -0.9770955615653315052 ) ) ;
#193489 = ORIENTED_EDGE ( 'NONE', *, *, #88754, .T. ) ;
#193491 = ORIENTED_EDGE ( 'NONE', *, *, #246576, .T. ) ;
#193490 = DIRECTION ( 'NONE',  ( 0.000000000000000000, 0.000000000000000000, -1.000000000000000000 ) ) ;
#193492 = EDGE_CURVE ( 'NONE', #144388, #11973, #83342, .T. ) ;
#193493 = EDGE_CURVE ( 'NONE', #196143, #97864, #129178, .T. ) ;
#193494 = DIRECTION ( 'NONE',  ( 1.000000000000000000, 0.000000000000000000, 0.000000000000000000 ) ) ;
#193495 = ORIENTED_EDGE ( 'NONE', *, *, #24063, .F. ) ;
#193496 = CIRCLE ( 'NONE', #197757, 0.1000000000000052097 ) ;
#193497 = DIRECTION ( 'NONE',  ( -1.000000000000000000, 2.952720810173289112E-16, 2.061873921506763405E-30 ) ) ;
#193498 = EDGE_LOOP ( 'NONE', ( #235816, #67638, #80153, #48864 ) ) ;
#193499 = AXIS2_PLACEMENT_3D ( 'NONE', #224241, #207277, #123881 ) ;
#193501 = ORIENTED_EDGE ( 'NONE', *, *, #99646, .F. ) ;
#193500 = ORIENTED_EDGE ( 'NONE', *, *, #23451, .F. ) ;
#193502 = DIRECTION ( 'NONE',  ( 0.000000000000000000, 0.9126074666063781482, 0.4088369013363256643 ) ) ;
#193503 = EDGE_CURVE ( 'NONE', #69705, #148316, #228616, .T. ) ;
#193505 = VERTEX_POINT ( 'NONE', #107356 ) ;
#193504 = DIRECTION ( 'NONE',  ( 0.7070776581709138364, -0.3339045366652431679, -0.6233369439636203824 ) ) ;
#193506 = CARTESIAN_POINT ( 'NONE',  ( 20.84999999999998721, 87.75000000001215028, -136.5231074845242745 ) ) ;
#193507 = ORIENTED_EDGE ( 'NONE', *, *, #88206, .F. ) ;
#193508 = AXIS2_PLACEMENT_3D ( 'NONE', #179367, #41146, #157246 ) ;
#193509 = AXIS2_PLACEMENT_3D ( 'NONE', #40670, #221800, #38077 ) ;
#193510 = ORIENTED_EDGE ( 'NONE', *, *, #78744, .T. ) ;
#193511 = CARTESIAN_POINT ( 'NONE',  ( -20.54999999999999716, 1.115600667400684642E-11, -167.5000000000000284 ) ) ;
#193512 = EDGE_CURVE ( 'NONE', #223817, #7829, #79064, .T. ) ;
#193513 = DIRECTION ( 'NONE',  ( 1.000000000000000000, 0.000000000000000000, 0.000000000000000000 ) ) ;
#193514 = LINE ( 'NONE', #134782, #228185 ) ;
#193515 = ORIENTED_EDGE ( 'NONE', *, *, #254107, .F. ) ;
#193516 = DIRECTION ( 'NONE',  ( 1.000000000000000000, -0.000000000000000000, -0.000000000000000000 ) ) ;
#193517 = CARTESIAN_POINT ( 'NONE',  ( -18.50000000000001066, -9.421308209727946803, -74.24236321405062711 ) ) ;
#193518 = CARTESIAN_POINT ( 'NONE',  ( 20.94999999999999929, 65.49732036650624423, -236.6319166190174883 ) ) ;
#193519 = TOROIDAL_SURFACE ( 'NONE', #72743, 6.258578643762700899, 0.1000000000000000056 ) ;
#193520 = ORIENTED_EDGE ( 'NONE', *, *, #149056, .F. ) ;
#193521 = DIRECTION ( 'NONE',  ( 0.000000000000000000, 0.000000000000000000, -1.000000000000000000 ) ) ;
#193522 = CIRCLE ( 'NONE', #47739, 0.2000000000000003997 ) ;
#193523 = DIRECTION ( 'NONE',  ( 0.000000000000000000, 0.8659859643398428730, -0.5000683049008328718 ) ) ;
#193524 = CARTESIAN_POINT ( 'NONE',  ( -23.25000000000000000, 76.00000000001216449, -140.5731074845242858 ) ) ;
#193525 = CIRCLE ( 'NONE', #60224, 0.09999999999998898659 ) ;
#193526 = VERTEX_POINT ( 'NONE', #168679 ) ;
#193527 = DIRECTION ( 'NONE',  ( 0.000000000000000000, -0.2617529984165031243, -0.9651348961777158619 ) ) ;
#193528 = ORIENTED_EDGE ( 'NONE', *, *, #185720, .F. ) ;
#193529 = ORIENTED_EDGE ( 'NONE', *, *, #97871, .F. ) ;
#193530 = DIRECTION ( 'NONE',  ( -1.000000000000000000, 0.000000000000000000, 0.000000000000000000 ) ) ;
#193531 = ORIENTED_EDGE ( 'NONE', *, *, #86065, .T. ) ;
#193532 = ORIENTED_EDGE ( 'NONE', *, *, #106884, .F. ) ;
#193533 = CARTESIAN_POINT ( 'NONE',  ( -22.48970261584617703, 11.37138061004976208, -198.4667671244310441 ) ) ;
#193534 = PLANE ( 'NONE',  #212599 ) ;
#193535 = VERTEX_POINT ( 'NONE', #69545 ) ;
#193536 = ORIENTED_EDGE ( 'NONE', *, *, #185744, .F. ) ;
#193537 = DIRECTION ( 'NONE',  ( 1.000000000000000000, -0.000000000000000000, -0.000000000000000000 ) ) ;
#193538 = DIRECTION ( 'NONE',  ( 0.000000000000000000, -6.982962677686266711E-15, 1.000000000000000000 ) ) ;
#193539 = VERTEX_POINT ( 'NONE', #8281 ) ;
#193540 = AXIS2_PLACEMENT_3D ( 'NONE', #18757, #215660, #177859 ) ;
#193542 = ORIENTED_EDGE ( 'NONE', *, *, #726, .F. ) ;
#193541 = AXIS2_PLACEMENT_3D ( 'NONE', #64938, #20708, #42822 ) ;
#193543 = CIRCLE ( 'NONE', #247697, 0.09999999999999530098 ) ;
#193544 = ADVANCED_FACE ( 'NONE', ( #149082 ), #179080, .T. ) ;
#193545 = AXIS2_PLACEMENT_3D ( 'NONE', #107748, #212006, #189859 ) ;
#193546 = DIRECTION ( 'NONE',  ( 0.000000000000000000, 0.000000000000000000, -1.000000000000000000 ) ) ;
#193547 = CARTESIAN_POINT ( 'NONE',  ( -21.05000000000000071, -11.39257802169451139, -197.9260504201680249 ) ) ;
#193548 = EDGE_CURVE ( 'NONE', #66273, #178841, #189481, .T. ) ;
#193549 = DIRECTION ( 'NONE',  ( 0.000000000000000000, 1.000000000000000000, 6.938893903907222067E-15 ) ) ;
#193550 = DIRECTION ( 'NONE',  ( 0.000000000000000000, -7.086529944415894657E-15, 1.000000000000000000 ) ) ;
#193551 = CARTESIAN_POINT ( 'NONE',  ( -23.15000000000000213, 76.00000000001126921, -203.5231074845248997 ) ) ;
#193552 = CARTESIAN_POINT ( 'NONE',  ( -22.49533356619859603, 12.57247511773151061, -223.4325311539369352 ) ) ;
#193553 = CARTESIAN_POINT ( 'NONE',  ( -20.94999999999999929, -11.39257802169451317, -130.9260504201681101 ) ) ;
#193554 = ADVANCED_FACE ( 'NONE', ( #111220 ), #190792, .F. ) ;
#193556 = CARTESIAN_POINT ( 'NONE',  ( 20.85000000000000142, -1.736705739456431807, -212.5174225876236846 ) ) ;
#193555 = DIRECTION ( 'NONE',  ( 0.000000000000000000, 0.8700118002898356018, -0.4930308989875170078 ) ) ;
#193558 = EDGE_CURVE ( 'NONE', #214079, #79078, #6976, .T. ) ;
#193557 = CARTESIAN_POINT ( 'NONE',  ( 22.47071067811865319, 7.720074744509199505, -100.4009075452974287 ) ) ;
#193559 = DIRECTION ( 'NONE',  ( -1.000000000000000000, 0.000000000000000000, 0.000000000000000000 ) ) ;
#193560 = CARTESIAN_POINT ( 'NONE',  ( -21.05000000000000071, 75.90220970870363715, -176.2809220950004772 ) ) ;
#193561 = AXIS2_PLACEMENT_3D ( 'NONE', #43160, #41892, #240075 ) ;
#193562 = ORIENTED_EDGE ( 'NONE', *, *, #132726, .T. ) ;
#193563 = VECTOR ( 'NONE', #252033, 1000.000000000000000 ) ;
#193565 = ORIENTED_EDGE ( 'NONE', *, *, #239776, .F. ) ;
#193564 = CARTESIAN_POINT ( 'NONE',  ( -18.59999999999999787, 3.912899247244609580, -111.9818229730110062 ) ) ;
#193566 = ADVANCED_FACE ( 'NONE', ( #147790 ), #156795, .F. ) ;
#193567 = DIRECTION ( 'NONE',  ( 0.000000000000000000, -0.9908441862701420355, -0.1350103645453197554 ) ) ;
#193568 = EDGE_CURVE ( 'NONE', #102067, #89168, #141629, .T. ) ;
#193569 = CARTESIAN_POINT ( 'NONE',  ( -18.50000000000000000, 74.65925378207876406, -180.2959699899455472 ) ) ;
#193570 = ORIENTED_EDGE ( 'NONE', *, *, #62476, .T. ) ;
#193571 = CARTESIAN_POINT ( 'NONE',  ( 20.85000000000000142, 7.120270961708750512, -70.65956304183931991 ) ) ;
#193572 = CYLINDRICAL_SURFACE ( 'NONE', #216246, 0.09999999999999939493 ) ;
#193573 = ORIENTED_EDGE ( 'NONE', *, *, #119771, .T. ) ;
#193575 = CARTESIAN_POINT ( 'NONE',  ( 18.59999999999999076, 6.550000000011156231, -88.25000000000005684 ) ) ;
#193574 = CIRCLE ( 'NONE', #18771, 0.1000000000000028644 ) ;
#193576 = VECTOR ( 'NONE', #162044, 1000.000000000000000 ) ;
#193577 = LINE ( 'NONE', #215680, #117235 ) ;
#193578 = EDGE_CURVE ( 'NONE', #41950, #45390, #96755, .T. ) ;
#193579 = EDGE_CURVE ( 'NONE', #112707, #163200, #192063, .T. ) ;
#193580 = CARTESIAN_POINT ( 'NONE',  ( -21.10257677756357353, 10.12810965763892668, -228.0807765930105973 ) ) ;
#193582 = ORIENTED_EDGE ( 'NONE', *, *, #186160, .F. ) ;
#193581 = DIRECTION ( 'NONE',  ( -0.000000000000000000, -0.000000000000000000, -1.000000000000000000 ) ) ;
#193583 = CARTESIAN_POINT ( 'NONE',  ( 18.79999999999999716, 1.800000000000000044, -11.61130914238355771 ) ) ;
#193584 = EDGE_CURVE ( 'NONE', #224935, #15812, #177646, .T. ) ;
#193586 = EDGE_LOOP ( 'NONE', ( #109126, #155609, #141997 ) ) ;
#193585 = FACE_OUTER_BOUND ( 'NONE', #35974, .T. ) ;
#193587 = CARTESIAN_POINT ( 'NONE',  ( -21.05000000000000071, -11.64999999998884306, -164.6000000000000227 ) ) ;
#193588 = DIRECTION ( 'NONE',  ( 0.000000000000000000, -0.9651348961777157509, 0.2617529984165031243 ) ) ;
#193589 = DIRECTION ( 'NONE',  ( -1.000000000000000000, -7.304098846218134667E-16, 0.000000000000000000 ) ) ;
#193590 = CARTESIAN_POINT ( 'NONE',  ( -21.65000000000000213, 7.708578643773852157, -112.8500000000000369 ) ) ;
#193592 = DIRECTION ( 'NONE',  ( -0.000000000000000000, 1.000000000000000000, 6.352154140967427193E-15 ) ) ;
#193591 = CARTESIAN_POINT ( 'NONE',  ( 18.44364597020194196, 8.869066854935326205, -245.4312477487408728 ) ) ;
#193593 = CARTESIAN_POINT ( 'NONE',  ( -18.59999999999999787, 77.63717271298267519, -158.4409541190523214 ) ) ;
#193594 = AXIS2_PLACEMENT_3D ( 'NONE', #63284, #248355, #210517 ) ;
#193595 = CARTESIAN_POINT ( 'NONE',  ( -23.15000000000000213, 11.65000000000000036, -21.35000000000000142 ) ) ;
#193596 = CARTESIAN_POINT ( 'NONE',  ( -18.59999999999999787, 76.00000000001170974, -69.52310748452431710 ) ) ;
#193597 = AXIS2_PLACEMENT_3D ( 'NONE', #204948, #103277, #165862 ) ;
#193598 = FACE_OUTER_BOUND ( 'NONE', #2237, .T. ) ;
#193599 = LINE ( 'NONE', #13669, #59339 ) ;
#193600 = CIRCLE ( 'NONE', #73014, 11.79999999999999716 ) ;
#193601 = ORIENTED_EDGE ( 'NONE', *, *, #213114, .F. ) ;
#193602 = CIRCLE ( 'NONE', #97711, 0.2000000000000005107 ) ;
#193603 = DIRECTION ( 'NONE',  ( -0.5932847527679298016, 0.7865547670005542669, 0.1713032417725954826 ) ) ;
#193604 = ORIENTED_EDGE ( 'NONE', *, *, #130602, .F. ) ;
#193605 = ORIENTED_EDGE ( 'NONE', *, *, #7670, .F. ) ;
#193606 = DIRECTION ( 'NONE',  ( 0.000000000000000000, -0.09425075112713271475, -0.9955484899852801162 ) ) ;
#193607 = CARTESIAN_POINT ( 'NONE',  ( 20.94999999999999929, 16.44800918141279666, -240.8068063186265135 ) ) ;
#193608 = ORIENTED_EDGE ( 'NONE', *, *, #37874, .F. ) ;
#193610 = EDGE_CURVE ( 'NONE', #160790, #53948, #150038, .T. ) ;
#193609 = EDGE_LOOP ( 'NONE', ( #137900, #22905, #171151, #13034 ) ) ;
#193611 = CARTESIAN_POINT ( 'NONE',  ( 20.94999999999999929, 69.55000000001159322, -59.50608031408435039 ) ) ;
#193612 = ORIENTED_EDGE ( 'NONE', *, *, #190572, .T. ) ;
#193613 = VECTOR ( 'NONE', #256926, 1000.000000000000000 ) ;
#193614 = ORIENTED_EDGE ( 'NONE', *, *, #212308, .T. ) ;
#193615 = VECTOR ( 'NONE', #164974, 1000.000000000000000 ) ;
#193616 = SPHERICAL_SURFACE ( 'NONE', #163111, 0.1000000000000000056 ) ;
#193617 = DIRECTION ( 'NONE',  ( 0.000000000000000000, 0.000000000000000000, 1.000000000000000000 ) ) ;
#193618 = CYLINDRICAL_SURFACE ( 'NONE', #34591, 0.09999999999999939493 ) ;
#193619 = VECTOR ( 'NONE', #250158, 1000.000000000000000 ) ;
#193620 = CARTESIAN_POINT ( 'NONE',  ( -20.94999999999999929, 5.850000000011160495, -90.36750277572211587 ) ) ;
#193621 = DIRECTION ( 'NONE',  ( 1.000000000000000000, 0.000000000000000000, -0.000000000000000000 ) ) ;
#193622 = EDGE_CURVE ( 'NONE', #51613, #60391, #235027, .T. ) ;
#193624 = DIRECTION ( 'NONE',  ( 0.000000000000000000, -6.467318590049456648E-15, 1.000000000000000000 ) ) ;
#193623 = DIRECTION ( 'NONE',  ( 1.000000000000000000, 0.000000000000000000, 0.000000000000000000 ) ) ;
#193625 = CARTESIAN_POINT ( 'NONE',  ( -21.05000000000000071, 61.95000000001234497, -164.5094124137634708 ) ) ;
#193627 = ORIENTED_EDGE ( 'NONE', *, *, #65408, .F. ) ;
#193626 = DIRECTION ( 'NONE',  ( -0.000000000000000000, 0.2128009952263603677, -0.9770955615653313941 ) ) ;
#193629 = DIRECTION ( 'NONE',  ( 0.000000000000000000, -0.8814952561688423893, 0.4721928772777357897 ) ) ;
#193628 = CARTESIAN_POINT ( 'NONE',  ( -22.45305610364634674, -0.1008583690987139569, 11.74956712348939192 ) ) ;
#193630 = DIRECTION ( 'NONE',  ( 1.000000000000000000, 0.000000000000000000, 0.000000000000000000 ) ) ;
#193631 = ORIENTED_EDGE ( 'NONE', *, *, #7523, .F. ) ;
#193632 = CARTESIAN_POINT ( 'NONE',  ( 21.05995757104869881, 8.775389244732430427, -146.1949051229912016 ) ) ;
#193634 = EDGE_CURVE ( 'NONE', #47998, #168551, #241764, .T. ) ;
#193633 = CYLINDRICAL_SURFACE ( 'NONE', #220570, 0.09999999999999939493 ) ;
#193635 = VERTEX_POINT ( 'NONE', #195911 ) ;
#193636 = AXIS2_PLACEMENT_3D ( 'NONE', #193454, #194748, #361 ) ;
#193637 = CARTESIAN_POINT ( 'NONE',  ( 23.14999999999999503, 11.75000000001116263, -88.75000000000004263 ) ) ;
#193638 = EDGE_CURVE ( 'NONE', #172639, #138742, #65358, .T. ) ;
#193639 = LINE ( 'NONE', #172839, #40189 ) ;
#193640 = DIRECTION ( 'NONE',  ( 1.000000000000000000, 0.000000000000000000, 0.000000000000000000 ) ) ;
#193641 = ORIENTED_EDGE ( 'NONE', *, *, #85815, .T. ) ;
#193642 = ORIENTED_EDGE ( 'NONE', *, *, #194981, .T. ) ;
#193644 = EDGE_CURVE ( 'NONE', #144138, #52663, #53813, .T. ) ;
#193643 = B_SPLINE_CURVE_WITH_KNOTS ( 'NONE', 3,
 ( #53731, #94135, #34204, #233666, #171163, #173735, #229796 ),
 .UNSPECIFIED., .F., .F.,
 ( 4, 3, 4 ),
 ( 0.000000000000000000, 0.0007844235214594282848, 0.001767853679404336829 ),
 .UNSPECIFIED. ) ;
#193645 = AXIS2_PLACEMENT_3D ( 'NONE', #140225, #115544, #56826 ) ;
#193647 = ADVANCED_FACE ( 'NONE', ( #254546 ), #154347, .F. ) ;
#193646 = DIRECTION ( 'NONE',  ( 1.000000000000000000, -0.000000000000000000, -0.000000000000000000 ) ) ;
#193648 = CIRCLE ( 'NONE', #6182, 6.258578643762700011 ) ;
#193649 = DIRECTION ( 'NONE',  ( 0.000000000000000000, 0.000000000000000000, 1.000000000000000000 ) ) ;
#193650 = CARTESIAN_POINT ( 'NONE',  ( 23.15000000000000213, 87.65000000001215597, -139.6231074845242688 ) ) ;
#193651 = LINE ( 'NONE', #115379, #217689 ) ;
#193652 = ORIENTED_EDGE ( 'NONE', *, *, #190772, .T. ) ;
#193653 = AXIS2_PLACEMENT_3D ( 'NONE', #99188, #94067, #65213 ) ;
#193654 = AXIS2_PLACEMENT_3D ( 'NONE', #230317, #69991, #27020 ) ;
#193655 = CARTESIAN_POINT ( 'NONE',  ( -22.50014994444008565, 64.25028026812007909, -170.1061876412429399 ) ) ;
#193656 = CYLINDRICAL_SURFACE ( 'NONE', #78695, 0.5000000000000007772 ) ;
#193657 = DIRECTION ( 'NONE',  ( 0.000000000000000000, 0.2617529984165152257, 0.9651348961777124202 ) ) ;
#193658 = EDGE_CURVE ( 'NONE', #94125, #66196, #196004, .T. ) ;
#193660 = EDGE_CURVE ( 'NONE', #224594, #61798, #129339, .T. ) ;
#193659 = DIRECTION ( 'NONE',  ( -1.000000000000000000, 0.000000000000000000, 0.000000000000000000 ) ) ;
#193662 = VERTEX_POINT ( 'NONE', #95502 ) ;
#193661 = CARTESIAN_POINT ( 'NONE',  ( -16.93262454970419384, 65.99797953208144463, -82.09603125828706993 ) ) ;
#193663 = CARTESIAN_POINT ( 'NONE',  ( -23.15000000000000213, 64.35000000001198828, -115.1731074845243796 ) ) ;
#193664 = DIRECTION ( 'NONE',  ( 2.952720810173289112E-16, 0.9651348961777174162, -0.2617529984164969070 ) ) ;
#193665 = CARTESIAN_POINT ( 'NONE',  ( -18.59999999999999787, 77.16412189325330928, -128.6082593989527254 ) ) ;
#193666 = DIRECTION ( 'NONE',  ( 0.000000000000000000, 0.2128009952263585358, -0.9770955615653319493 ) ) ;
#193667 = ADVANCED_FACE ( 'NONE', ( #14718 ), #253284, .T. ) ;
#193668 = CARTESIAN_POINT ( 'NONE',  ( 18.59999999999999787, -10.64999999999999325, 31.50000000000000000 ) ) ;
#193670 = VERTEX_POINT ( 'NONE', #155517 ) ;
#193669 = DIRECTION ( 'NONE',  ( -1.000000000000000000, 2.952720810173289112E-16, 2.061873921506763405E-30 ) ) ;
#193671 = DIRECTION ( 'NONE',  ( 0.000000000000000000, -1.000000000000000000, 0.000000000000000000 ) ) ;
#193672 = CARTESIAN_POINT ( 'NONE',  ( -18.59999999999999787, 14.70949956575304185, -235.9560995168023112 ) ) ;
#193673 = CARTESIAN_POINT ( 'NONE',  ( -18.59999999999999787, 11.65000000001115232, -155.3500000000000227 ) ) ;
#193674 = ORIENTED_EDGE ( 'NONE', *, *, #104245, .T. ) ;
#193675 = LINE ( 'NONE', #55403, #109468 ) ;
#193676 = AXIS2_PLACEMENT_3D ( 'NONE', #162032, #175495, #176775 ) ;
#193677 = DIRECTION ( 'NONE',  ( 1.000000000000000000, 0.000000000000000000, 0.000000000000000000 ) ) ;
#193678 = DIRECTION ( 'NONE',  ( -1.000000000000000000, 0.000000000000000000, 0.000000000000000000 ) ) ;
#193679 = EDGE_CURVE ( 'NONE', #145681, #227928, #46133, .T. ) ;
#193681 = AXIS2_PLACEMENT_3D ( 'NONE', #238359, #141822, #23196 ) ;
#193680 = DIRECTION ( 'NONE',  ( -1.284434275755705296E-16, 0.7071067811865471286, 0.7071067811865479058 ) ) ;
#193682 = CIRCLE ( 'NONE', #143774, 0.09999999999999939493 ) ;
#193683 = ADVANCED_FACE ( 'NONE', ( #117637 ), #96004, .T. ) ;
#193684 = DIRECTION ( 'NONE',  ( 0.000000000000000000, 0.9770955615653316162, 0.2128009952263604232 ) ) ;
#193685 = DIRECTION ( 'NONE',  ( 0.000000000000000000, 0.9915357197604973694, -0.1298341882519105928 ) ) ;
#193686 = EDGE_LOOP ( 'NONE', ( #201429, #46550, #237024, #151610 ) ) ;
#193687 = ORIENTED_EDGE ( 'NONE', *, *, #9940, .F. ) ;
#193688 = VECTOR ( 'NONE', #53655, 1000.000000000000000 ) ;
#193689 = ADVANCED_FACE ( 'NONE', ( #57644 ), #237591, .F. ) ;
#193690 = CARTESIAN_POINT ( 'NONE',  ( -23.25000000000000000, 2.319530388122572617, -217.8268657444419887 ) ) ;
#193691 = VECTOR ( 'NONE', #177299, 1000.000000000000000 ) ;
#193692 = CARTESIAN_POINT ( 'NONE',  ( -21.05000000000000071, 1.115600667400684642E-11, -100.5000000000000284 ) ) ;
#193693 = LINE ( 'NONE', #75056, #87125 ) ;
#193694 = FACE_OUTER_BOUND ( 'NONE', #125275, .T. ) ;
#193695 = EDGE_CURVE ( 'NONE', #201851, #95314, #208482, .T. ) ;
#193697 = AXIS2_PLACEMENT_3D ( 'NONE', #224678, #89023, #142569 ) ;
#193696 = CARTESIAN_POINT ( 'NONE',  ( 18.59999999999999432, -1.637172712959223952, -179.0821533654719815 ) ) ;
#193698 = CARTESIAN_POINT ( 'NONE',  ( 21.14999999999999858, 67.32778804267617545, -235.8813018063200388 ) ) ;
#193699 = CARTESIAN_POINT ( 'NONE',  ( -16.93440969289731513, 9.995185175825110235, -113.0912341850108191 ) ) ;
#193701 = VECTOR ( 'NONE', #53286, 1000.000000000000000 ) ;
#193700 = DIRECTION ( 'NONE',  ( 1.000000000000000000, 0.000000000000000000, 0.000000000000000000 ) ) ;
#193702 = B_SPLINE_CURVE_WITH_KNOTS ( 'NONE', 3,
 ( #2490, #20811, #148119, #127269, #108973, #22090, #239848, #82008, #160329, #88104, #140732, #241142, #220292, #8609, #208109, #227639 ),
 .UNSPECIFIED., .F., .F.,
 ( 4, 3, 3, 3, 3, 4 ),
 ( 0.000000000000000000, 1.810570668009715449E-05, 2.740575833571675123E-05, 4.256816319436012815E-05, 5.213463471026095184E-05, 6.641585710718307266E-05 ),
 .UNSPECIFIED. ) ;
#193703 = ORIENTED_EDGE ( 'NONE', *, *, #154257, .F. ) ;
#193704 = DIRECTION ( 'NONE',  ( 1.000000000000000000, 0.000000000000000000, 0.000000000000000000 ) ) ;
#193705 = ORIENTED_EDGE ( 'NONE', *, *, #15540, .T. ) ;
#193706 = CARTESIAN_POINT ( 'NONE',  ( 23.14999999999999858, 76.00000000001244871, -170.0231074845243597 ) ) ;
#193707 = CARTESIAN_POINT ( 'NONE',  ( -25.10847955711009760, 9.068702471349583405, -347.0000000000001137 ) ) ;
#193708 = CARTESIAN_POINT ( 'NONE',  ( 20.95429693346636668, 10.54330487989576781, -7.560882538313035361 ) ) ;
#193711 = ORIENTED_EDGE ( 'NONE', *, *, #238321, .F. ) ;
#193710 = AXIS2_PLACEMENT_3D ( 'NONE', #194364, #177375, #256814 ) ;
#193709 = CARTESIAN_POINT ( 'NONE',  ( -20.94999999999999929, -11.48912529306489994, -97.40000000000004832 ) ) ;
#193712 = CARTESIAN_POINT ( 'NONE',  ( -23.15000000000000213, 85.00000000001197975, -112.3170766071766735 ) ) ;
#193713 = FILL_AREA_STYLE_COLOUR ( '', #114536 ) ;
#193714 = CARTESIAN_POINT ( 'NONE',  ( 18.33683296300430854, 85.51114997114436278, -62.61740007181408174 ) ) ;
#193715 = EDGE_LOOP ( 'NONE', ( #250357, #196814, #94566 ) ) ;
#193716 = DIRECTION ( 'NONE',  ( 0.000000000000000000, 0.000000000000000000, 1.000000000000000000 ) ) ;
#193717 = DIRECTION ( 'NONE',  ( 0.000000000000000000, 6.982962677686266711E-15, -1.000000000000000000 ) ) ;
#193718 = CARTESIAN_POINT ( 'NONE',  ( 20.04142135623730070, 11.65000000001115943, -88.35000000000003695 ) ) ;
#193719 = CARTESIAN_POINT ( 'NONE',  ( -18.39999999999999858, 85.50000000001233502, -162.9910380878246485 ) ) ;
#193720 = DIRECTION ( 'NONE',  ( 0.000000000000000000, -0.2128009952263609783, 0.9770955615653315052 ) ) ;
#193721 = AXIS2_PLACEMENT_3D ( 'NONE', #137121, #77136, #159268 ) ;
#193722 = TOROIDAL_SURFACE ( 'NONE', #102102, 1.900000000000002576, 0.1000000000000000056 ) ;
#193723 = VERTEX_POINT ( 'NONE', #203590 ) ;
#193724 = DIRECTION ( 'NONE',  ( 1.000000000000000000, 0.000000000000000000, 0.000000000000000000 ) ) ;
#193725 = CYLINDRICAL_SURFACE ( 'NONE', #25481, 0.1000000000000028644 ) ;
#193726 = EDGE_CURVE ( 'NONE', #188486, #44729, #40708, .T. ) ;
#193727 = ORIENTED_EDGE ( 'NONE', *, *, #195361, .T. ) ;
#193728 = FACE_OUTER_BOUND ( 'NONE', #40330, .T. ) ;
#193729 = CARTESIAN_POINT ( 'NONE',  ( 22.49999999999999645, 55.96597777900657888, -232.8853806925633307 ) ) ;
#193730 = DIRECTION ( 'NONE',  ( 0.000000000000000000, -1.000000000000000000, 0.000000000000000000 ) ) ;
#193731 = VERTEX_POINT ( 'NONE', #121515 ) ;
#193732 = CARTESIAN_POINT ( 'NONE',  ( 18.46932045258650490, -9.670685200254538927, -174.1738603729967565 ) ) ;
#193733 = DIRECTION ( 'NONE',  ( 0.000000000000000000, 0.000000000000000000, -1.000000000000000000 ) ) ;
#193734 = EDGE_CURVE ( 'NONE', #232638, #111080, #200083, .T. ) ;
#193735 = ORIENTED_EDGE ( 'NONE', *, *, #27222, .F. ) ;
#193736 = VECTOR ( 'NONE', #69799, 999.9999999999998863 ) ;
#193737 = AXIS2_PLACEMENT_3D ( 'NONE', #2527, #39127, #79496 ) ;
#193738 = VERTEX_POINT ( 'NONE', #241447 ) ;
#193739 = LINE ( 'NONE', #49079, #139251 ) ;
#193740 = DIRECTION ( 'NONE',  ( -1.000000000000000000, 0.000000000000000000, 0.000000000000000000 ) ) ;
#193742 = VERTEX_POINT ( 'NONE', #221840 ) ;
#193741 = FACE_OUTER_BOUND ( 'NONE', #121439, .T. ) ;
#193743 = LINE ( 'NONE', #175481, #249067 ) ;
#193745 = CARTESIAN_POINT ( 'NONE',  ( -18.59999999999999787, -11.65000000000000036, 30.09999999999999787 ) ) ;
#193744 = UNCERTAINTY_MEASURE_WITH_UNIT (LENGTH_MEASURE( 1.000000000000000082E-05 ), #47303, 'distance_accuracy_value', 'NONE');
#193746 = DIRECTION ( 'NONE',  ( -1.000000000000000000, 0.000000000000000000, 0.000000000000000000 ) ) ;
#193747 = CARTESIAN_POINT ( 'NONE',  ( -18.35235881385853318, 11.47341900772405054, -76.25000000000004263 ) ) ;
#193748 = DIRECTION ( 'NONE',  ( 1.000000000000000000, 0.000000000000000000, 0.000000000000000000 ) ) ;
#193749 = DIRECTION ( 'NONE',  ( 0.000000000000000000, 0.8700118002898357128, -0.4930308989875170633 ) ) ;
#193751 = VERTEX_POINT ( 'NONE', #217992 ) ;
#193750 = CYLINDRICAL_SURFACE ( 'NONE', #244527, 0.09999999999999939493 ) ;
#193752 = VERTEX_POINT ( 'NONE', #161921 ) ;
#193754 = CARTESIAN_POINT ( 'NONE',  ( -16.80891096016315700, 51.63498214198624225, -231.9392478082567948 ) ) ;
#193753 = DIRECTION ( 'NONE',  ( 1.000000000000000000, 0.000000000000000000, 0.000000000000000000 ) ) ;
#193756 = ORIENTED_EDGE ( 'NONE', *, *, #184409, .F. ) ;
#193755 = CARTESIAN_POINT ( 'NONE',  ( -20.94999999999999929, 76.00000000001199396, -114.8231074845243000 ) ) ;
#193757 = ORIENTED_EDGE ( 'NONE', *, *, #90581, .F. ) ;
#193758 = DIRECTION ( 'NONE',  ( 0.000000000000000000, -1.000000000000000000, -0.000000000000000000 ) ) ;
#193759 = B_SPLINE_CURVE_WITH_KNOTS ( 'NONE', 3,
 ( #103173, #82313, #124054, #204843, #184008, #66637, #221824, #44515, #241430, #203576, #201016, #161910, #107025, #27551, #146160, #225673, #47049, #43225, #5345, #122778, #126607, #223128, #182749, #62785, #41958, #164460 ),
 .UNSPECIFIED., .F., .F.,
 ( 4, 2, 2, 2, 2, 2, 2, 2, 2, 2, 2, 2, 4 ),
 ( 0.005476422646581339572, 0.006160811967703579139, 0.006845201288825817840, 0.007187395949386908567, 0.007529590609947999294, 0.007871785270509090021, 0.008213979931070179014, 0.008556174591631269741, 0.008898369252192360468, 0.009240563912753451195, 0.009582758573314541922, 0.01026714789443678062, 0.01095153721555902106 ),
 .UNSPECIFIED. ) ;
#193760 = CARTESIAN_POINT ( 'NONE',  ( -23.15000000000000213, 87.75000000001247713, -173.1231074845242688 ) ) ;
#193761 = CIRCLE ( 'NONE', #189843, 0.09999999999999739653 ) ;
#193762 = VECTOR ( 'NONE', #220289, 1000.000000000000000 ) ;
#193763 = CARTESIAN_POINT ( 'NONE',  ( -22.49806830649814415, 64.35011034517287953, -103.1005718008498917 ) ) ;
#193764 = DIRECTION ( 'NONE',  ( -1.000000000000000000, 0.000000000000000000, -0.000000000000000000 ) ) ;
#193765 = CARTESIAN_POINT ( 'NONE',  ( -21.45000000000000284, 68.29142135624991283, -191.2731074845244166 ) ) ;
#193766 = CARTESIAN_POINT ( 'NONE',  ( -18.50000000000000000, 2.319530388122570841, -217.8268657444419887 ) ) ;
#193767 = DIRECTION ( 'NONE',  ( -0.000000000000000000, -1.000000000000000000, -0.000000000000000000 ) ) ;
#193768 = ORIENTED_EDGE ( 'NONE', *, *, #27036, .T. ) ;
#193769 = ORIENTED_EDGE ( 'NONE', *, *, #167054, .T. ) ;
#193770 = CARTESIAN_POINT ( 'NONE',  ( 18.49999999999999289, 65.70729864260985664, -64.06574559737245522 ) ) ;
#193771 = EDGE_CURVE ( 'NONE', #177816, #185056, #87629, .T. ) ;
#193772 = AXIS2_PLACEMENT_3D ( 'NONE', #7156, #110122, #5869 ) ;
#193773 = MANIFOLD_SOLID_BREP ( 'Stock-MAS-200-1', #24444 ) ;
#193774 = AXIS2_PLACEMENT_3D ( 'NONE', #111992, #128984, #166856 ) ;
#193775 = ORIENTED_EDGE ( 'NONE', *, *, #192817, .F. ) ;
#193776 = DIRECTION ( 'NONE',  ( 0.000000000000000000, 0.000000000000000000, -1.000000000000000000 ) ) ;
#193777 = ORIENTED_EDGE ( 'NONE', *, *, #25622, .F. ) ;
#193778 = DIRECTION ( 'NONE',  ( 1.000000000000000000, -0.000000000000000000, 0.000000000000000000 ) ) ;
#193779 = AXIS2_PLACEMENT_3D ( 'NONE', #130777, #252005, #189480 ) ;
#193780 = AXIS2_PLACEMENT_3D ( 'NONE', #209982, #133015, #52164 ) ;
#193781 = DIRECTION ( 'NONE',  ( 0.000000000000000000, -0.2128009952263603677, 0.9770955615653313941 ) ) ;
#193782 = MECHANICAL_DESIGN_GEOMETRIC_PRESENTATION_REPRESENTATION (  '', ( #235458 ), #252208 ) ;
#193783 = ADVANCED_FACE ( 'NONE', ( #82326 ), #145903, .T. ) ;
#193784 = ORIENTED_EDGE ( 'NONE', *, *, #62321, .F. ) ;
#193785 = LINE ( 'NONE', #13864, #148381 ) ;
#193786 = EDGE_LOOP ( 'NONE', ( #168878, #27401, #15778 ) ) ;
#193787 = DIRECTION ( 'NONE',  ( 1.000000000000000000, 0.000000000000000000, 0.000000000000000000 ) ) ;
#193788 = VERTEX_POINT ( 'NONE', #202310 ) ;
#193789 = EDGE_CURVE ( 'NONE', #5207, #148744, #245872, .T. ) ;
#193790 = DIRECTION ( 'NONE',  ( 0.000000000000000000, 0.000000000000000000, -1.000000000000000000 ) ) ;
#193791 = B_SPLINE_CURVE_WITH_KNOTS ( 'NONE', 3,
 ( #20448, #99934, #830, #140361, #240770, #82933, #178248, #41307, #3413, #80367 ),
 .UNSPECIFIED., .F., .F.,
 ( 4, 3, 3, 4 ),
 ( 0.000000000000000000, 0.0002000000000002908468, 0.001000000000045115191, 0.001967863649472098748 ),
 .UNSPECIFIED. ) ;
#193792 = ORIENTED_EDGE ( 'NONE', *, *, #102336, .T. ) ;
#193793 = DIRECTION ( 'NONE',  ( 1.000000000000000000, 0.000000000000000000, 0.000000000000000000 ) ) ;
#193794 = EDGE_CURVE ( 'NONE', #212805, #103755, #103186, .T. ) ;
#193795 = ORIENTED_EDGE ( 'NONE', *, *, #108537, .F. ) ;
#193798 = VERTEX_POINT ( 'NONE', #182761 ) ;
#193797 = DIRECTION ( 'NONE',  ( 0.000000000000000000, -0.2617529984165031243, -0.9651348961777158619 ) ) ;
#193796 = DIRECTION ( 'NONE',  ( -0.000000000000000000, 0.6922311945860614157, 0.7216758089626911232 ) ) ;
#193799 = CARTESIAN_POINT ( 'NONE',  ( -20.96428641294161110, 64.25000000001148237, -42.84821430658328012 ) ) ;
#193801 = ORIENTED_EDGE ( 'NONE', *, *, #75537, .T. ) ;
#193800 = AXIS2_PLACEMENT_3D ( 'NONE', #119746, #140558, #122296 ) ;
#193802 = B_SPLINE_CURVE_WITH_KNOTS ( 'NONE', 3,
 ( #215193, #104215, #65104, #183776, #219034, #159098, #224173, #164222 ),
 .UNSPECIFIED., .F., .F.,
 ( 4, 2, 2, 4 ),
 ( 0.000000000000000000, 0.0001094981963948490336, 0.0002189963927896980671, 0.0004379927855793961343 ),
 .UNSPECIFIED. ) ;
#193803 = CIRCLE ( 'NONE', #164589, 0.09999999999999939493 ) ;
#193804 = ORIENTED_EDGE ( 'NONE', *, *, #120083, .F. ) ;
#193805 = AXIS2_PLACEMENT_3D ( 'NONE', #205558, #123475, #124766 ) ;
#193806 = FACE_OUTER_BOUND ( 'NONE', #102803, .T. ) ;
#193807 = ORIENTED_EDGE ( 'NONE', *, *, #162146, .T. ) ;
#193808 = DIRECTION ( 'NONE',  ( 0.000000000000000000, 0.000000000000000000, -1.000000000000000000 ) ) ;
#193809 = EDGE_CURVE ( 'NONE', #208387, #16660, #175195, .T. ) ;
#193810 = CARTESIAN_POINT ( 'NONE',  ( -18.40000000000000213, 70.35000000001151932, -45.27310748452435973 ) ) ;
#193811 = CYLINDRICAL_SURFACE ( 'NONE', #249240, 7.899999999999990585 ) ;
#193812 = CARTESIAN_POINT ( 'NONE',  ( 18.49999999999999289, 67.49463558145296815, -195.5618716440587548 ) ) ;
#193813 = VECTOR ( 'NONE', #62883, 1000.000000000000114 ) ;
#193814 = VECTOR ( 'NONE', #129894, 1000.000000000000000 ) ;
#193815 = VECTOR ( 'NONE', #76137, 1000.000000000000000 ) ;
#193816 = CARTESIAN_POINT ( 'NONE',  ( -21.07928932188134041, 0.09889514566555068775, -60.67148334360675221 ) ) ;
#193817 = ORIENTED_EDGE ( 'NONE', *, *, #2039, .T. ) ;
#193818 = CARTESIAN_POINT ( 'NONE',  ( -18.59999999999999787, -10.84999999999999076, 31.59999999999999787 ) ) ;
#193819 = LINE ( 'NONE', #254997, #73946 ) ;
#193820 = LINE ( 'NONE', #218481, #13728 ) ;
#193821 = ORIENTED_EDGE ( 'NONE', *, *, #165644, .F. ) ;
#193822 = CARTESIAN_POINT ( 'NONE',  ( -23.25000000000000355, 5.650000000011139001, -154.8500000000000227 ) ) ;
#193823 = ORIENTED_EDGE ( 'NONE', *, *, #248356, .F. ) ;
#193824 = CARTESIAN_POINT ( 'NONE',  ( -20.64999999999999858, 4.350000000011156054, -121.6500000000000341 ) ) ;
#193825 = ORIENTED_EDGE ( 'NONE', *, *, #172201, .T. ) ;
#193826 = AXIS2_PLACEMENT_3D ( 'NONE', #107532, #87948, #172706 ) ;
#193827 = VECTOR ( 'NONE', #163370, 1000.000000000000000 ) ;
#193828 = PLANE ( 'NONE',  #139125 ) ;
#193829 = CARTESIAN_POINT ( 'NONE',  ( -20.94999999999999929, -11.74999999998884448, -197.8999999999999773 ) ) ;
#193831 = EDGE_LOOP ( 'NONE', ( #96070, #207570, #195639, #45583 ) ) ;
#193830 = FACE_OUTER_BOUND ( 'NONE', #60235, .T. ) ;
#193832 = CARTESIAN_POINT ( 'NONE',  ( -18.58693740092109081, 8.967674985626857165, -245.3887142130325287 ) ) ;
#193833 = VERTEX_POINT ( 'NONE', #180192 ) ;
#193834 = AXIS2_PLACEMENT_3D ( 'NONE', #60075, #219142, #40565 ) ;
#193835 = AXIS2_PLACEMENT_3D ( 'NONE', #8713, #226444, #88214 ) ;
#193836 = ADVANCED_FACE ( 'NONE', ( #1524 ), #54313, .T. ) ;
#193837 = DIRECTION ( 'NONE',  ( 1.000000000000000000, 0.000000000000000000, 0.000000000000000000 ) ) ;
#193838 = CARTESIAN_POINT ( 'NONE',  ( -16.87683809663752399, 9.850000000011123191, -113.9023640181965220 ) ) ;
#193839 = ORIENTED_EDGE ( 'NONE', *, *, #53519, .T. ) ;
#193840 = DIRECTION ( 'NONE',  ( 1.000000000000000000, 0.000000000000000000, 0.000000000000000000 ) ) ;
#193841 = DIRECTION ( 'NONE',  ( 1.000000000000000000, -0.000000000000000000, -0.000000000000000000 ) ) ;
#193842 = VERTEX_POINT ( 'NONE', #240161 ) ;
#193843 = SPHERICAL_SURFACE ( 'NONE', #157390, 0.1000000000000000056 ) ;
#193844 = B_SPLINE_CURVE_WITH_KNOTS ( 'NONE', 3,
 ( #126635, #26264, #202319, #165786, #103199, #45813, #206176, #125359, #181493, #141072, #86195, #201038, #160661, #83614, #220608, #84901 ),
 .UNSPECIFIED., .F., .F.,
 ( 4, 3, 3, 3, 3, 4 ),
 ( 0.000000000000000000, 2.209075297430758666E-05, 5.594258369009635874E-05, 8.979524372342026039E-05, 0.0001236472815274586843, 0.0001574990747609555279 ),
 .UNSPECIFIED. ) ;
#193845 = ORIENTED_EDGE ( 'NONE', *, *, #174601, .T. ) ;
#193846 = ADVANCED_FACE ( 'NONE', ( #141059 ), #2806, .T. ) ;
#193847 = CARTESIAN_POINT ( 'NONE',  ( 12.68104795156993880, 9.396533993965071829, -118.4059397791733090 ) ) ;
#193848 = CARTESIAN_POINT ( 'NONE',  ( 23.24999999999999289, 6.650000000011155876, -155.3500000000000227 ) ) ;
#193849 = EDGE_CURVE ( 'NONE', #88823, #138980, #152200, .T. ) ;
#193851 = ORIENTED_EDGE ( 'NONE', *, *, #112417, .F. ) ;
#193850 = LINE ( 'NONE', #17748, #217926 ) ;
#193852 = VECTOR ( 'NONE', #82136, 1000.000000000000000 ) ;
#193853 = DIRECTION ( 'NONE',  ( 0.000000000000000000, 0.000000000000000000, -1.000000000000000000 ) ) ;
#193854 = CARTESIAN_POINT ( 'NONE',  ( -21.52071067811865746, 52.78011179951285214, -233.8048247179419548 ) ) ;
#193855 = CIRCLE ( 'NONE', #97968, 0.3999999999999994671 ) ;
#193856 = CARTESIAN_POINT ( 'NONE',  ( 16.27683809663749770, 9.350000000011137402, -76.25000000000005684 ) ) ;
#193858 = DIRECTION ( 'NONE',  ( 0.000000000000000000, -0.3848449534832868446, -0.9229812358755982160 ) ) ;
#193857 = CARTESIAN_POINT ( 'NONE',  ( -17.11825945287481332, 62.98921886345645760, -213.1014462870871569 ) ) ;
#193860 = ADVANCED_FACE ( 'NONE', ( #245295 ), #162670, .T. ) ;
#193859 = DIRECTION ( 'NONE',  ( 0.000000000000000000, 0.4999999999999608646, -0.8660254037844612451 ) ) ;
#193861 = TOROIDAL_SURFACE ( 'NONE', #119039, 7.791421356237316687, 0.1000000000000000056 ) ;
#193862 = DIRECTION ( 'NONE',  ( -1.000000000000000000, 0.000000000000000000, 0.000000000000000000 ) ) ;
#193863 = DIRECTION ( 'NONE',  ( 1.000000000000000000, 0.000000000000000000, 0.000000000000000000 ) ) ;
#193864 = PLANE ( 'NONE',  #121641 ) ;
#193865 = ORIENTED_EDGE ( 'NONE', *, *, #46136, .F. ) ;
#193866 = ORIENTED_EDGE ( 'NONE', *, *, #250046, .F. ) ;
#193867 = DIRECTION ( 'NONE',  ( -2.952720810173288619E-16, 1.000000000000000000, 0.000000000000000000 ) ) ;
#193869 = ORIENTED_EDGE ( 'NONE', *, *, #4826, .F. ) ;
#193868 = DIRECTION ( 'NONE',  ( -0.000000000000000000, 1.000000000000000000, 6.982962677686266711E-15 ) ) ;
#193870 = EDGE_LOOP ( 'NONE', ( #22108, #184099, #220492, #198022 ) ) ;
#193871 = CARTESIAN_POINT ( 'NONE',  ( -18.59999999999999787, 14.05000000001115623, -72.51369507076104526 ) ) ;
#193872 = EDGE_CURVE ( 'NONE', #111080, #146711, #41887, .T. ) ;
#193873 = VERTEX_POINT ( 'NONE', #10538 ) ;
#193874 = CARTESIAN_POINT ( 'NONE',  ( 20.94999999999999929, 36.65892442174935439, -249.5511627012433848 ) ) ;
#193875 = CIRCLE ( 'NONE', #35687, 0.1000000000000028644 ) ;
#193876 = CIRCLE ( 'NONE', #114770, 0.2000000000000057288 ) ;
#193877 = ADVANCED_FACE ( 'NONE', ( #224429 ), #212574, .F. ) ;
#193878 = EDGE_CURVE ( 'NONE', #11411, #107983, #45800, .T. ) ;
#193879 = ORIENTED_EDGE ( 'NONE', *, *, #82606, .F. ) ;
#193880 = VECTOR ( 'NONE', #44206, 1000.000000000000000 ) ;
#193881 = DIRECTION ( 'NONE',  ( -1.000000000000000000, 0.000000000000000000, 0.000000000000000000 ) ) ;
#193882 = TOROIDAL_SURFACE ( 'NONE', #77166, 0.2000000000000000111, 0.1000000000000000056 ) ;
#193884 = ORIENTED_EDGE ( 'NONE', *, *, #127211, .T. ) ;
#193883 = VERTEX_POINT ( 'NONE', #225685 ) ;
#193885 = ORIENTED_EDGE ( 'NONE', *, *, #116787, .F. ) ;
#193886 = ORIENTED_EDGE ( 'NONE', *, *, #220810, .T. ) ;
#193887 = ORIENTED_EDGE ( 'NONE', *, *, #52069, .F. ) ;
#193888 = EDGE_CURVE ( 'NONE', #158615, #25415, #45951, .T. ) ;
#193889 = CARTESIAN_POINT ( 'NONE',  ( -20.64999999999999858, 54.18117728009210055, -239.0715820348696923 ) ) ;
#193890 = CYLINDRICAL_SURFACE ( 'NONE', #15886, 0.1000000000000000194 ) ;
#193891 = CARTESIAN_POINT ( 'NONE',  ( 18.59999999999999076, 69.45000000001260787, -193.5060803140843859 ) ) ;
#193893 = ORIENTED_EDGE ( 'NONE', *, *, #200889, .F. ) ;
#193892 = CARTESIAN_POINT ( 'NONE',  ( -17.71734398241074970, 65.15764277154774220, -159.7482457375300555 ) ) ;
#193894 = AXIS2_PLACEMENT_3D ( 'NONE', #116542, #60400, #257273 ) ;
#193895 = CARTESIAN_POINT ( 'NONE',  ( 20.74625933824008328, 40.83477453765030418, -237.9468798847826179 ) ) ;
#193896 = EDGE_CURVE ( 'NONE', #140147, #219486, #21040, .T. ) ;
#193897 = CARTESIAN_POINT ( 'NONE',  ( 15.06592377766031099, 12.47014700295942369, -214.0015173037735394 ) ) ;
#193899 = VERTEX_POINT ( 'NONE', #247852 ) ;
#193898 = CARTESIAN_POINT ( 'NONE',  ( 20.95035502843362707, 10.47763832678762164, -141.5762997087363999 ) ) ;
#193900 = CYLINDRICAL_SURFACE ( 'NONE', #70890, 0.1000000000000033362 ) ;
#193902 = EDGE_CURVE ( 'NONE', #126, #208096, #91361, .T. ) ;
#193901 = ORIENTED_EDGE ( 'NONE', *, *, #13690, .T. ) ;
#193903 = CARTESIAN_POINT ( 'NONE',  ( 21.05000000000000071, 11.60000000001116227, -127.0717967697245143 ) ) ;
#193905 = VERTEX_POINT ( 'NONE', #210027 ) ;
#193904 = LINE ( 'NONE', #94781, #147770 ) ;
#193906 = CARTESIAN_POINT ( 'NONE',  ( -21.14999999999999858, 69.45934304831041572, -69.52310748452435973 ) ) ;
#193907 = CARTESIAN_POINT ( 'NONE',  ( -16.87036670365549895, 9.989418819312803066, -113.0204398826979855 ) ) ;
#193908 = ORIENTED_EDGE ( 'NONE', *, *, #30576, .F. ) ;
#193910 = FACE_OUTER_BOUND ( 'NONE', #158631, .T. ) ;
#193909 = CARTESIAN_POINT ( 'NONE',  ( -16.93388492042257454, 9.988541822527057690, -121.4005451231862054 ) ) ;
#193911 = DIRECTION ( 'NONE',  ( -1.000000000000000000, -0.000000000000000000, -0.000000000000000000 ) ) ;
#193912 = AXIS2_PLACEMENT_3D ( 'NONE', #175104, #132075, #232479 ) ;
#193913 = AXIS2_PLACEMENT_3D ( 'NONE', #119841, #139355, #138078 ) ;
#193914 = CARTESIAN_POINT ( 'NONE',  ( -18.59999999999999787, 74.83729825007388570, -94.92310748452432279 ) ) ;
#193915 = CIRCLE ( 'NONE', #214740, 0.1000000000000054040 ) ;
#193916 = LINE ( 'NONE', #94793, #193438 ) ;
#193917 = ORIENTED_EDGE ( 'NONE', *, *, #103698, .F. ) ;
#193918 = ORIENTED_EDGE ( 'NONE', *, *, #248597, .T. ) ;
#193919 = CARTESIAN_POINT ( 'NONE',  ( 22.50000000000000000, 75.90000000001202807, -114.6726782920691221 ) ) ;
#193920 = CARTESIAN_POINT ( 'NONE',  ( -22.50000000000000000, 1.115600667400684642E-11, -33.50000000000000000 ) ) ;
#193922 = VERTEX_POINT ( 'NONE', #243991 ) ;
#193921 = EDGE_CURVE ( 'NONE', #68733, #80663, #116870, .T. ) ;
#193923 = DIRECTION ( 'NONE',  ( 0.000000000000000000, 0.9915357197604883766, -0.1298341882519788160 ) ) ;
#193924 = ORIENTED_EDGE ( 'NONE', *, *, #58403, .T. ) ;
#193925 = EDGE_CURVE ( 'NONE', #69086, #23447, #191745, .T. ) ;
#193926 = CARTESIAN_POINT ( 'NONE',  ( 21.05000000000000071, 23.68770167995059239, -252.8127582590406348 ) ) ;
#193927 = CARTESIAN_POINT ( 'NONE',  ( -20.99142135623731065, 56.16603649944111254, -228.1013850343386196 ) ) ;
#193929 = EDGE_CURVE ( 'NONE', #20965, #58429, #48364, .T. ) ;
#193928 = ORIENTED_EDGE ( 'NONE', *, *, #197098, .T. ) ;
#193930 = CARTESIAN_POINT ( 'NONE',  ( 21.05000000000000071, 67.18454772081454962, -128.1027149319100999 ) ) ;
#193931 =( NAMED_UNIT ( * ) SI_UNIT ( $, .STERADIAN. ) SOLID_ANGLE_UNIT ( ) );
#193932 = TOROIDAL_SURFACE ( 'NONE', #148131, 11.90000000000000213, 0.1000000000000000056 ) ;
#193933 = ORIENTED_EDGE ( 'NONE', *, *, #166225, .T. ) ;
#193934 = EDGE_LOOP ( 'NONE', ( #5608, #223990, #131061, #128851 ) ) ;
#193935 = ORIENTED_EDGE ( 'NONE', *, *, #39375, .F. ) ;
#193936 = DIRECTION ( 'NONE',  ( 0.000000000000000000, 0.000000000000000000, -1.000000000000000000 ) ) ;
#193937 = DIRECTION ( 'NONE',  ( 1.000000000000000000, 0.000000000000000000, 0.000000000000000000 ) ) ;
#193938 = AXIS2_PLACEMENT_3D ( 'NONE', #9937, #128606, #245988 ) ;
#193939 = CARTESIAN_POINT ( 'NONE',  ( 21.14999999999999503, 56.01362831242965967, -232.7091905853083347 ) ) ;
#193940 = DIRECTION ( 'NONE',  ( 0.000000000000000000, 0.000000000000000000, 1.000000000000000000 ) ) ;
#193941 = FACE_OUTER_BOUND ( 'NONE', #96095, .T. ) ;
#193943 = PLANE ( 'NONE',  #257326 ) ;
#193942 = FACE_OUTER_BOUND ( 'NONE', #212780, .T. ) ;
#193945 = ORIENTED_EDGE ( 'NONE', *, *, #25797, .F. ) ;
#193944 = DIRECTION ( 'NONE',  ( 2.952720810173289112E-16, -1.000000000000000000, 0.000000000000000000 ) ) ;
#193946 = CARTESIAN_POINT ( 'NONE',  ( -23.25000000000000000, 71.85000000001178933, -81.87310748452433984 ) ) ;
#193947 = ORIENTED_EDGE ( 'NONE', *, *, #190138, .F. ) ;
#193948 = DIRECTION ( 'NONE',  ( -0.000000000000000000, 0.4721928772777347350, 0.8814952561688429444 ) ) ;
#193949 = ORIENTED_EDGE ( 'NONE', *, *, #95372, .F. ) ;
#193950 = ORIENTED_EDGE ( 'NONE', *, *, #168901, .F. ) ;
#193951 = LINE ( 'NONE', #152271, #150468 ) ;
#193952 = CARTESIAN_POINT ( 'NONE',  ( -21.11825140030074266, 6.445407565431249708, -133.9927963793674053 ) ) ;
#193954 = EDGE_CURVE ( 'NONE', #252254, #249301, #8546, .T. ) ;
#193953 = DIRECTION ( 'NONE',  ( 0.000000000000000000, -0.9667078373770112698, -0.2558827019434132821 ) ) ;
#193955 = DIRECTION ( 'NONE',  ( -1.000000000000000000, 0.000000000000000000, 0.000000000000000000 ) ) ;
#193956 = ADVANCED_FACE ( 'NONE', ( #31412 ), #100087, .F. ) ;
#193957 = VECTOR ( 'NONE', #172419, 1000.000000000000000 ) ;
#193958 = VECTOR ( 'NONE', #235659, 1000.000000000000000 ) ;
#193959 = DIRECTION ( 'NONE',  ( 1.000000000000000000, 0.000000000000000000, 0.000000000000000000 ) ) ;
#193960 = ORIENTED_EDGE ( 'NONE', *, *, #63365, .T. ) ;
#193961 = ORIENTED_EDGE ( 'NONE', *, *, #91758, .F. ) ;
#193963 = EDGE_CURVE ( 'NONE', #147930, #75879, #241946, .T. ) ;
#193962 = DIRECTION ( 'NONE',  ( 0.000000000000000000, -1.000000000000000000, 0.000000000000000000 ) ) ;
#193964 = ORIENTED_EDGE ( 'NONE', *, *, #140522, .T. ) ;
#193965 = LINE ( 'NONE', #31064, #98615 ) ;
#193966 = CARTESIAN_POINT ( 'NONE',  ( -18.59999999999999787, 68.75000000001253397, -182.1731074845244223 ) ) ;
#193967 = VERTEX_POINT ( 'NONE', #109617 ) ;
#193968 = DIRECTION ( 'NONE',  ( 1.000000000000000000, -7.304098846218134667E-16, -4.639676173203993355E-30 ) ) ;
#193969 = CARTESIAN_POINT ( 'NONE',  ( -21.04386569057627909, 11.75000000001120526, -60.14283735177934886 ) ) ;
#193970 = CARTESIAN_POINT ( 'NONE',  ( 20.94999999999999929, 67.23127455305835554, -235.8551265064784559 ) ) ;
#193971 = CARTESIAN_POINT ( 'NONE',  ( -20.54999999999999716, 48.98768910550767686, -253.5949463715719787 ) ) ;
#193972 = ORIENTED_EDGE ( 'NONE', *, *, #47618, .F. ) ;
#193973 = EDGE_CURVE ( 'NONE', #43985, #22565, #200260, .T. ) ;
#193974 = CARTESIAN_POINT ( 'NONE',  ( -20.94999999999999929, 4.252251777740766236, -211.8999245327126744 ) ) ;
#193976 = EDGE_CURVE ( 'NONE', #229941, #188850, #216993, .T. ) ;
#193975 = CARTESIAN_POINT ( 'NONE',  ( 18.59999999999999432, 77.73625713161000306, -191.9544551555068495 ) ) ;
#193977 = VECTOR ( 'NONE', #192446, 1000.000000000000000 ) ;
#193978 = CARTESIAN_POINT ( 'NONE',  ( -21.05000000000000071, 57.66663670110953177, -226.2321832927624996 ) ) ;
#193979 = CIRCLE ( 'NONE', #98060, 0.1999999999999987899 ) ;
#193980 = AXIS2_PLACEMENT_3D ( 'NONE', #101239, #103838, #878 ) ;
#193981 = VECTOR ( 'NONE', #43103, 1000.000000000000000 ) ;
#193982 = EDGE_CURVE ( 'NONE', #217509, #158454, #17124, .T. ) ;
#193983 = ORIENTED_EDGE ( 'NONE', *, *, #27153, .T. ) ;
#193985 = ADVANCED_FACE ( 'NONE', ( #92613 ), #96195, .F. ) ;
#193984 = EDGE_CURVE ( 'NONE', #95434, #117714, #225173, .T. ) ;
#193986 =( GEOMETRIC_REPRESENTATION_CONTEXT ( 3 ) GLOBAL_UNCERTAINTY_ASSIGNED_CONTEXT ( ( #58357 ) ) GLOBAL_UNIT_ASSIGNED_CONTEXT ( ( #175355, #132341, #192328 ) ) REPRESENTATION_CONTEXT ( 'NONE', 'WORKASPACE' ) );
#193987 = DIRECTION ( 'NONE',  ( 1.000000000000000000, 0.000000000000000000, 0.000000000000000000 ) ) ;
#193988 = VERTEX_POINT ( 'NONE', #193028 ) ;
#193989 = FACE_OUTER_BOUND ( 'NONE', #24152, .T. ) ;
#193990 = DIRECTION ( 'NONE',  ( 1.000000000000000000, 0.000000000000000000, 0.000000000000000000 ) ) ;
#193991 = CARTESIAN_POINT ( 'NONE',  ( -21.05000000000000071, 74.16465844978765176, -124.9679561919613207 ) ) ;
#193992 = CYLINDRICAL_SURFACE ( 'NONE', #73290, 0.1000000000000003525 ) ;
#193993 = DIRECTION ( 'NONE',  ( 0.000000000000000000, -1.000000000000000000, -6.352154140967427193E-15 ) ) ;
#193994 = CARTESIAN_POINT ( 'NONE',  ( 20.94999999999999929, 76.00000000001247713, -172.9231074845243654 ) ) ;
#193995 = EDGE_LOOP ( 'NONE', ( #219836, #245480, #30187, #44695 ) ) ;
#193996 = CARTESIAN_POINT ( 'NONE',  ( -16.95709691156811871, 66.05000000001224691, -149.1831650470383295 ) ) ;
#193997 = CARTESIAN_POINT ( 'NONE',  ( -16.89208623190940273, 66.04842205103632580, -82.16783528130611103 ) ) ;
#193998 = DIRECTION ( 'NONE',  ( -1.000000000000000000, -0.000000000000000000, -0.000000000000000000 ) ) ;
#193999 = DIRECTION ( 'NONE',  ( 0.000000000000000000, 0.000000000000000000, 1.000000000000000000 ) ) ;
#194000 = EDGE_CURVE ( 'NONE', #151911, #250000, #141994, .T. ) ;
#194001 = EDGE_CURVE ( 'NONE', #92189, #252923, #73107, .T. ) ;
#194002 = AXIS2_PLACEMENT_3D ( 'NONE', #715, #159841, #17723 ) ;
#194003 = DIRECTION ( 'NONE',  ( 1.000000000000000000, -0.000000000000000000, -0.000000000000000000 ) ) ;
#194004 = TOROIDAL_SURFACE ( 'NONE', #10651, 11.65000000000000036, 0.1000000000000000056 ) ;
#194005 = ORIENTED_EDGE ( 'NONE', *, *, #197065, .T. ) ;
#194006 = ORIENTED_EDGE ( 'NONE', *, *, #158180, .T. ) ;
#194007 = CARTESIAN_POINT ( 'NONE',  ( -21.14999999999999503, 64.25000000001161027, -62.60396023856562664 ) ) ;
#194008 = CARTESIAN_POINT ( 'NONE',  ( -21.10000000000000142, 6.223900101154155706, 12.00000000000000178 ) ) ;
#194010 = ADVANCED_FACE ( 'NONE', ( #174788 ), #71803, .F. ) ;
#194009 = CARTESIAN_POINT ( 'NONE',  ( 18.39999999999999858, -9.682403433476396870, -40.15684337741279109 ) ) ;
#194011 = CARTESIAN_POINT ( 'NONE',  ( -23.25000000000000000, 86.52890073500824997, -209.5906233940697234 ) ) ;
#194012 = DIRECTION ( 'NONE',  ( 1.441126678808780685E-14, 0.3280696808754172689, 0.9446535261620007118 ) ) ;
#194013 = AXIS2_PLACEMENT_3D ( 'NONE', #245373, #129270, #208806 ) ;
#194014 = ORIENTED_EDGE ( 'NONE', *, *, #200825, .F. ) ;
#194016 = ADVANCED_FACE ( 'NONE', ( #57335 ), #233679, .T. ) ;
#194015 = CARTESIAN_POINT ( 'NONE',  ( -20.64999999999999858, -9.399999999988846611, -90.60603087734760663 ) ) ;
#194017 = VECTOR ( 'NONE', #27343, 1000.000000000000000 ) ;
#194018 = CIRCLE ( 'NONE', #98100, 4.000000000000000000 ) ;
#194019 = CIRCLE ( 'NONE', #110607, 0.4999999999999978351 ) ;
#194020 = EDGE_CURVE ( 'NONE', #51208, #129128, #196162, .T. ) ;
#194021 = CARTESIAN_POINT ( 'NONE',  ( 22.39999999999999503, -1.560176095955058129, -193.3663837337745122 ) ) ;
#194022 = VERTEX_POINT ( 'NONE', #18237 ) ;
#194023 = FACE_OUTER_BOUND ( 'NONE', #180726, .T. ) ;
#194024 = DIRECTION ( 'NONE',  ( -0.000000000000000000, 6.982962677686266711E-15, -1.000000000000000000 ) ) ;
#194025 = AXIS2_PLACEMENT_3D ( 'NONE', #242255, #8794, #3646 ) ;
#194026 = ORIENTED_EDGE ( 'NONE', *, *, #95404, .F. ) ;
#194028 = VECTOR ( 'NONE', #118965, 1000.000000000000227 ) ;
#194027 = CARTESIAN_POINT ( 'NONE',  ( -23.25000000000000000, 64.35000000001176090, -76.53791325517833855 ) ) ;
#194029 = ORIENTED_EDGE ( 'NONE', *, *, #108785, .F. ) ;
#194030 = EDGE_CURVE ( 'NONE', #214994, #254425, #179431, .T. ) ;
#194031 = CARTESIAN_POINT ( 'NONE',  ( -23.25000000000000000, 87.65000000001215597, -139.6231074845242688 ) ) ;
#194032 = AXIS2_PLACEMENT_3D ( 'NONE', #31152, #105472, #46800 ) ;
#194033 = DIRECTION ( 'NONE',  ( 0.1538461538461510236, 0.9880948137434718559, 0.000000000000000000 ) ) ;
#194034 = CARTESIAN_POINT ( 'NONE',  ( -21.07928932188134041, 0.09889514566555068775, -127.6714833436067238 ) ) ;
#194035 = CIRCLE ( 'NONE', #252252, 0.09999999999999990841 ) ;
#194036 = CARTESIAN_POINT ( 'NONE',  ( 20.94999999999999574, 74.83729825007388570, -95.12310748452432563 ) ) ;
#194037 = DIRECTION ( 'NONE',  ( 0.000000000000000000, 7.026728003956695223E-15, -1.000000000000000000 ) ) ;
#194038 = DIRECTION ( 'NONE',  ( 0.000000000000000000, -1.000000000000000000, 0.000000000000000000 ) ) ;
#194039 = LINE ( 'NONE', #36250, #251582 ) ;
#194041 = CARTESIAN_POINT ( 'NONE',  ( 18.79999999999999716, 2.524878688533307880, -16.24283924587617989 ) ) ;
#194040 = DIRECTION ( 'NONE',  ( -1.000000000000000000, 0.000000000000000000, -0.000000000000000000 ) ) ;
#194042 = EDGE_CURVE ( 'NONE', #157579, #199005, #66987, .T. ) ;
#194043 = DIRECTION ( 'NONE',  ( 1.000000000000000000, 0.000000000000000000, 0.000000000000000000 ) ) ;
#194044 = CARTESIAN_POINT ( 'NONE',  ( 18.59999999999999076, 74.25000000001259082, -191.8535959266227451 ) ) ;
#194045 = DIRECTION ( 'NONE',  ( 0.000000000000000000, 0.008583690987128059571, -0.9999631594459056361 ) ) ;
#194046 = LINE ( 'NONE', #188890, #107157 ) ;
#194047 = ORIENTED_EDGE ( 'NONE', *, *, #57280, .F. ) ;
#194048 = CARTESIAN_POINT ( 'NONE',  ( -23.25000000000000000, 1.115600667400684642E-11, -167.5000000000000284 ) ) ;
#194049 = DIRECTION ( 'NONE',  ( 0.000000000000000000, 0.9910465087640860649, 0.1335171055202901413 ) ) ;
#194050 = ORIENTED_EDGE ( 'NONE', *, *, #231410, .F. ) ;
#194051 = DIRECTION ( 'NONE',  ( 0.000000000000000000, -6.517943393102675675E-15, 1.000000000000000000 ) ) ;
#194052 = DIRECTION ( 'NONE',  ( -3.265361837132813093E-16, 1.000000000000000000, -0.000000000000000000 ) ) ;
#194053 = ADVANCED_FACE ( 'NONE', ( #113474 ), #255504, .F. ) ;
#194054 = DIRECTION ( 'NONE',  ( 0.000000000000000000, 0.000000000000000000, 1.000000000000000000 ) ) ;
#194055 = ORIENTED_EDGE ( 'NONE', *, *, #142777, .F. ) ;
#194056 = TOROIDAL_SURFACE ( 'NONE', #73266, 0.2000000000000000111, 0.1000000000000000056 ) ;
#194057 = AXIS2_PLACEMENT_3D ( 'NONE', #2976, #82496, #202482 ) ;
#194058 = LINE ( 'NONE', #256508, #167814 ) ;
#194059 = EDGE_LOOP ( 'NONE', ( #139055, #215883, #72080, #82478 ) ) ;
#194061 = TOROIDAL_SURFACE ( 'NONE', #32127, 1.900000000000002576, 0.1000000000000000056 ) ;
#194060 = DIRECTION ( 'NONE',  ( 1.000000000000000000, 0.000000000000000000, 0.000000000000000000 ) ) ;
#194062 = LINE ( 'NONE', #97472, #14386 ) ;
#194063 = AXIS2_PLACEMENT_3D ( 'NONE', #44985, #124529, #204046 ) ;
#194064 = EDGE_CURVE ( 'NONE', #214472, #67636, #146086, .T. ) ;
#194065 = CIRCLE ( 'NONE', #189952, 11.75000000000001066 ) ;
#194066 = VERTEX_POINT ( 'NONE', #151345 ) ;
#194067 = FACE_OUTER_BOUND ( 'NONE', #96689, .T. ) ;
#194068 =( BOUNDED_SURFACE ( )  B_SPLINE_SURFACE ( 3, 2, ( 
 ( #203965, #106134, #4475 ),
 ( #65746, #44906, #25361 ),
 ( #222224, #224805, #29235 ),
 ( #223517, #145266, #241810 ),
 ( #246940, #128303, #183140 ),
 ( #166169, #63162, #125714 ) ),
 .UNSPECIFIED., .F., .F., .F. ) 
 B_SPLINE_SURFACE_WITH_KNOTS ( ( 4, 2, 4 ),
 ( 3, 3 ),
 ( 0.0001792624049599400582, 0.0003686986002124377883, 0.0005581347954649355184 ),
 ( 0.000000000000000000, 1.000000000000000000 ),
 .UNSPECIFIED. ) 
 GEOMETRIC_REPRESENTATION_ITEM ( )  RATIONAL_B_SPLINE_SURFACE ( (
 ( 1.000000000000000000, 0.9238795325112714174, 1.000000000000000000),
 ( 1.000000000000000000, 0.9229318695242134662, 1.000000000000000000),
 ( 1.000000000000000000, 0.8926288119225641582, 1.000000000000000000),
 ( 1.000000000000000000, 0.8123777807277360319, 1.000000000000000000),
 ( 1.000000000000000000, 0.7629087100926377207, 1.000000000000000000),
 ( 1.000000000000000000, 0.7071067811865352493, 1.000000000000000000) ) ) 
 REPRESENTATION_ITEM ( '' )  SURFACE ( )  );
#194069 = VERTEX_POINT ( 'NONE', #156497 ) ;
#194071 = VECTOR ( 'NONE', #212816, 1000.000000000000000 ) ;
#194070 = FACE_OUTER_BOUND ( 'NONE', #90127, .T. ) ;
#194072 = CARTESIAN_POINT ( 'NONE',  ( -23.25000000000000000, 1.148907358139439339E-11, -201.0000000000015064 ) ) ;
#194074 = CARTESIAN_POINT ( 'NONE',  ( -18.59999999999999787, 71.93512633425886804, -225.1442869522136334 ) ) ;
#194073 = UNCERTAINTY_MEASURE_WITH_UNIT (LENGTH_MEASURE( 1.000000000000000082E-05 ), #236890, 'distance_accuracy_value', 'NONE');
#194075 = CARTESIAN_POINT ( 'NONE',  ( 21.05000000000000071, 76.00000000001141132, -34.02310748452431710 ) ) ;
#194076 = DIRECTION ( 'NONE',  ( 0.000000000000000000, 1.000000000000000000, 0.000000000000000000 ) ) ;
#194077 = CARTESIAN_POINT ( 'NONE',  ( -13.77178122865953824, 46.49228253827788393, -234.7843890162627645 ) ) ;
#194078 = AXIS2_PLACEMENT_3D ( 'NONE', #124394, #169974, #203910 ) ;
#194079 = DIRECTION ( 'NONE',  ( 1.000000000000000000, -0.000000000000000000, -0.000000000000000000 ) ) ;
#194080 = CARTESIAN_POINT ( 'NONE',  ( -22.45305610364635740, 64.25313205997782973, -247.2214437328673569 ) ) ;
#194082 = EDGE_LOOP ( 'NONE', ( #248613, #249045, #83316 ) ) ;
#194081 = CARTESIAN_POINT ( 'NONE',  ( 21.05000000000000071, -11.64999999998883595, -164.6000000000000227 ) ) ;
#194083 = ORIENTED_EDGE ( 'NONE', *, *, #124177, .T. ) ;
#194085 = CARTESIAN_POINT ( 'NONE',  ( -23.15000000000000213, -4.914013037343267776, -233.1828366659746905 ) ) ;
#194084 = CARTESIAN_POINT ( 'NONE',  ( 13.99999999999999822, 9.849999999999981881, -16.74999999999999645 ) ) ;
#194086 = ORIENTED_EDGE ( 'NONE', *, *, #205652, .T. ) ;
#194088 = ORIENTED_EDGE ( 'NONE', *, *, #170782, .T. ) ;
#194087 = DIRECTION ( 'NONE',  ( 1.000000000000000000, 0.000000000000000000, 0.000000000000000000 ) ) ;
#194089 = ORIENTED_EDGE ( 'NONE', *, *, #213544, .F. ) ;
#194090 = CARTESIAN_POINT ( 'NONE',  ( -18.59999999999999787, 47.92640890138473253, -246.4059919526569900 ) ) ;
#194091 = CARTESIAN_POINT ( 'NONE',  ( 20.30466543256828160, 9.304236939266628426, -175.7536626513919771 ) ) ;
#194092 = DIRECTION ( 'NONE',  ( -0.000000000000000000, 0.1350103645451876666, -0.9908441862701600211 ) ) ;
#194093 = CARTESIAN_POINT ( 'NONE',  ( 20.94999999999999929, 28.08470566095357057, -239.2860081655328770 ) ) ;
#194095 = CARTESIAN_POINT ( 'NONE',  ( -23.15000000000000213, 76.00000000001240608, -174.1731074845243654 ) ) ;
#194094 = AXIS2_PLACEMENT_3D ( 'NONE', #124897, #50455, #184851 ) ;
#194096 = DIRECTION ( 'NONE',  ( 1.000000000000000000, 0.000000000000000000, 0.000000000000000000 ) ) ;
#194097 = CYLINDRICAL_SURFACE ( 'NONE', #198593, 0.1000000000000001443 ) ;
#194098 = ADVANCED_FACE ( 'NONE', ( #211299 ), #251704, .F. ) ;
#194099 = CYLINDRICAL_SURFACE ( 'NONE', #22804, 0.9000000000000014655 ) ;
#194100 = ORIENTED_EDGE ( 'NONE', *, *, #150705, .F. ) ;
#194101 = ORIENTED_EDGE ( 'NONE', *, *, #84634, .F. ) ;
#194102 = CARTESIAN_POINT ( 'NONE',  ( 22.39999999999999503, 7.612336166715857111, -199.3421143478784359 ) ) ;
#194103 = VECTOR ( 'NONE', #88064, 1000.000000000000000 ) ;
#194104 = AXIS2_PLACEMENT_3D ( 'NONE', #187516, #8859, #88362 ) ;
#194105 = ORIENTED_EDGE ( 'NONE', *, *, #74206, .T. ) ;
#194106 = AXIS2_PLACEMENT_3D ( 'NONE', #139532, #40488, #220381 ) ;
#194108 = CARTESIAN_POINT ( 'NONE',  ( 20.95159278453404283, 8.907896337960206523, -142.4847201851092677 ) ) ;
#194107 = AXIS2_PLACEMENT_3D ( 'NONE', #236292, #56355, #156792 ) ;
#194109 = ORIENTED_EDGE ( 'NONE', *, *, #101625, .F. ) ;
#194110 = DIRECTION ( 'NONE',  ( 0.000000000000000000, 0.000000000000000000, 1.000000000000000000 ) ) ;
#194111 = CARTESIAN_POINT ( 'NONE',  ( -20.64999999999999858, 2.000000000011154189, -180.7246219227620543 ) ) ;
#194112 = CARTESIAN_POINT ( 'NONE',  ( -22.50000000000000000, 75.90000000001236913, -170.0231074845243597 ) ) ;
#194113 = ADVANCED_FACE ( 'NONE', ( #230881 ), #4607, .F. ) ;
#194115 = ORIENTED_EDGE ( 'NONE', *, *, #134402, .T. ) ;
#194114 = CARTESIAN_POINT ( 'NONE',  ( -21.59780538579341425, 6.847090529954407145, -33.40102133040201693 ) ) ;
#194116 = DIRECTION ( 'NONE',  ( 1.000000000000000000, 0.000000000000000000, 0.000000000000000000 ) ) ;
#194117 = ORIENTED_EDGE ( 'NONE', *, *, #211156, .F. ) ;
#194118 = CARTESIAN_POINT ( 'NONE',  ( -18.37151313414815945, -9.571014125766627245, -207.8166629092395112 ) ) ;
#194119 = ADVANCED_FACE ( 'NONE', ( #102877 ), #42072, .T. ) ;
#194120 = DIRECTION ( 'NONE',  ( 1.000000000000000000, -0.000000000000000000, -0.000000000000000000 ) ) ;
#194121 = CARTESIAN_POINT ( 'NONE',  ( 18.49999999999996803, 70.15623657602074559, -198.0563205710787713 ) ) ;
#194122 = DIRECTION ( 'NONE',  ( 1.000000000000000000, 0.000000000000000000, 0.000000000000000000 ) ) ;
#194123 = AXIS2_PLACEMENT_3D ( 'NONE', #238841, #201002, #58890 ) ;
#194124 = DIRECTION ( 'NONE',  ( 0.000000000000000000, 1.000000000000000000, 0.000000000000000000 ) ) ;
#194125 = ORIENTED_EDGE ( 'NONE', *, *, #169033, .F. ) ;
#194126 = TOROIDAL_SURFACE ( 'NONE', #2553, 0.2000000000000000111, 0.1000000000000000056 ) ;
#194128 = CARTESIAN_POINT ( 'NONE',  ( -18.43634282235116473, 85.67978719993936920, -29.36245559907037617 ) ) ;
#194127 = DIRECTION ( 'NONE',  ( 0.000000000000000000, 0.2617529984165152257, 0.9651348961777124202 ) ) ;
#194129 = EDGE_CURVE ( 'NONE', #83776, #103483, #50386, .T. ) ;
#194130 = EDGE_LOOP ( 'NONE', ( #72033, #237260, #211207, #195178 ) ) ;
#194133 = ORIENTED_EDGE ( 'NONE', *, *, #16209, .F. ) ;
#194132 = DIRECTION ( 'NONE',  ( 1.000000000000000000, 0.000000000000000000, 0.000000000000000000 ) ) ;
#194131 = DIRECTION ( 'NONE',  ( -1.000000000000000000, 0.000000000000000000, 0.000000000000000000 ) ) ;
#194134 = FACE_OUTER_BOUND ( 'NONE', #161624, .T. ) ;
#194135 = EDGE_CURVE ( 'NONE', #102833, #225971, #83698, .T. ) ;
#194136 = CARTESIAN_POINT ( 'NONE',  ( -22.59999985501179154, 64.25013020700868083, -69.58870615432405771 ) ) ;
#194137 = CIRCLE ( 'NONE', #40020, 0.09999999999998807065 ) ;
#194138 = VERTEX_POINT ( 'NONE', #241150 ) ;
#194139 = EDGE_CURVE ( 'NONE', #206482, #66196, #117063, .T. ) ;
#194140 = DIRECTION ( 'NONE',  ( 1.000000000000000000, 0.000000000000000000, -0.000000000000000000 ) ) ;
#194141 = ADVANCED_FACE ( 'NONE', ( #203288 ), #79471, .T. ) ;
#194142 = CYLINDRICAL_SURFACE ( 'NONE', #146773, 0.1000000000000052097 ) ;
#194144 = ORIENTED_EDGE ( 'NONE', *, *, #224601, .T. ) ;
#194143 = CARTESIAN_POINT ( 'NONE',  ( 20.02499999999999858, 66.25000000001199396, -115.2731074845243597 ) ) ;
#194145 = ADVANCED_FACE ( 'NONE', ( #178619 ), #150398, .T. ) ;
#194146 = ORIENTED_EDGE ( 'NONE', *, *, #226223, .F. ) ;
#194147 = CARTESIAN_POINT ( 'NONE',  ( -16.94107738177415357, 10.01423928514777728, -113.0500000000000256 ) ) ;
#194148 = CARTESIAN_POINT ( 'NONE',  ( -21.05000000000000071, 76.00000000001197975, -107.3231074845242716 ) ) ;
#194149 = CARTESIAN_POINT ( 'NONE',  ( -16.79814274880124358, 44.13799952519313763, -235.2986007742642300 ) ) ;
#194150 = TOROIDAL_SURFACE ( 'NONE', #235809, 12.97499999999999609, 0.1000000000000000056 ) ;
#194151 = CARTESIAN_POINT ( 'NONE',  ( 22.39999999999999503, 64.25000000001165290, -69.42310748452440805 ) ) ;
#194152 = VERTEX_POINT ( 'NONE', #256783 ) ;
#194153 = LINE ( 'NONE', #250252, #72844 ) ;
#194154 = FACE_OUTER_BOUND ( 'NONE', #239359, .T. ) ;
#194155 = DIRECTION ( 'NONE',  ( -1.000000000000000000, -2.952720810173289112E-16, 0.000000000000000000 ) ) ;
#194156 = ORIENTED_EDGE ( 'NONE', *, *, #26293, .F. ) ;
#194157 = CARTESIAN_POINT ( 'NONE',  ( 20.44999100639885015, 59.18650678360199890, -225.6339461820924157 ) ) ;
#194158 = EDGE_CURVE ( 'NONE', #198469, #52116, #238558, .T. ) ;
#194159 = FACE_OUTER_BOUND ( 'NONE', #226610, .T. ) ;
#194160 = ORIENTED_EDGE ( 'NONE', *, *, #206696, .T. ) ;
#194161 = TOROIDAL_SURFACE ( 'NONE', #181679, 1.900000000000002576, 0.1000000000000000056 ) ;
#194162 = SPHERICAL_SURFACE ( 'NONE', #105735, 0.1000000000000000056 ) ;
#194163 = DIRECTION ( 'NONE',  ( 1.000000000000000000, 0.000000000000000000, 0.000000000000000000 ) ) ;
#194164 = FACE_OUTER_BOUND ( 'NONE', #79630, .T. ) ;
#194165 = AXIS2_PLACEMENT_3D ( 'NONE', #26613, #203940, #7021 ) ;
#194166 = CIRCLE ( 'NONE', #115045, 0.09999999999999736877 ) ;
#194167 = ORIENTED_EDGE ( 'NONE', *, *, #218066, .T. ) ;
#194168 = ORIENTED_EDGE ( 'NONE', *, *, #138928, .F. ) ;
#194169 =( BOUNDED_SURFACE ( )  B_SPLINE_SURFACE ( 3, 2, ( 
 ( #122342, #221410, #124917 ),
 ( #123630, #24546, #143165 ),
 ( #241010, #44087, #182329 ),
 ( #102745, #144438, #161486 ) ),
 .UNSPECIFIED., .F., .F., .F. ) 
 B_SPLINE_SURFACE_WITH_KNOTS ( ( 4, 4 ),
 ( 3, 3 ),
 ( 0.04058434257139457990, 0.04256401539001584966 ),
 ( 0.000000000000000000, 1.000000000000000000 ),
 .UNSPECIFIED. ) 
 GEOMETRIC_REPRESENTATION_ITEM ( )  RATIONAL_B_SPLINE_SURFACE ( (
 ( 1.000000000000000000, 0.7103081912008196719, 1.000000000000000000),
 ( 1.000000000000000000, 0.7104998333555380130, 1.000000000000000000),
 ( 1.000000000000000000, 0.7107238315755268765, 1.000000000000000000),
 ( 1.000000000000000000, 0.7110073749539379540, 1.000000000000000000) ) ) 
 REPRESENTATION_ITEM ( '' )  SURFACE ( )  );
#194170 =( GEOMETRIC_REPRESENTATION_CONTEXT ( 3 ) GLOBAL_UNCERTAINTY_ASSIGNED_CONTEXT ( ( #152387 ) ) GLOBAL_UNIT_ASSIGNED_CONTEXT ( ( #172512, #91638, #113757 ) ) REPRESENTATION_CONTEXT ( 'NONE', 'WORKASPACE' ) );
#194171 = EDGE_CURVE ( 'NONE', #47300, #114917, #25485, .T. ) ;
#194172 = DIRECTION ( 'NONE',  ( 1.000000000000000000, 0.000000000000000000, 0.000000000000000000 ) ) ;
#194173 = ORIENTED_EDGE ( 'NONE', *, *, #239502, .T. ) ;
#194175 = ORIENTED_EDGE ( 'NONE', *, *, #179661, .F. ) ;
#194174 = CARTESIAN_POINT ( 'NONE',  ( 22.50927854361885139, 25.97741623539291567, -254.4468631480566501 ) ) ;
#194178 = ORIENTED_EDGE ( 'NONE', *, *, #146602, .F. ) ;
#194177 = EDGE_LOOP ( 'NONE', ( #114451, #158223, #35556, #172808 ) ) ;
#194176 = DIRECTION ( 'NONE',  ( 0.000000000000000000, 0.000000000000000000, -1.000000000000000000 ) ) ;
#194179 = CARTESIAN_POINT ( 'NONE',  ( -21.05000000000000071, -11.74999999998884448, -97.40000000000004832 ) ) ;
#194180 = CARTESIAN_POINT ( 'NONE',  ( 20.89878130938411616, 46.45193731540633308, -243.0811559066744110 ) ) ;
#194181 = CARTESIAN_POINT ( 'NONE',  ( -21.65000000000000213, 52.90028168070691095, -233.8284721206281915 ) ) ;
#194182 = AXIS2_PLACEMENT_3D ( 'NONE', #159664, #55380, #76255 ) ;
#194183 = CARTESIAN_POINT ( 'NONE',  ( 21.05000000000000071, 65.45624872451701037, -195.9667196758603893 ) ) ;
#194184 = EDGE_CURVE ( 'NONE', #133882, #9380, #8724, .T. ) ;
#194185 = CARTESIAN_POINT ( 'NONE',  ( 21.05000000000005400, 83.80000000001119531, -37.18565239344504647 ) ) ;
#194186 = DIRECTION ( 'NONE',  ( 2.952720810173289112E-16, -1.000000000000000000, 0.000000000000000000 ) ) ;
#194188 = ORIENTED_EDGE ( 'NONE', *, *, #51339, .T. ) ;
#194187 = CIRCLE ( 'NONE', #189881, 0.1000000000000087624 ) ;
#194189 = ORIENTED_EDGE ( 'NONE', *, *, #41768, .F. ) ;
#194190 = ORIENTED_EDGE ( 'NONE', *, *, #248501, .T. ) ;
#194191 = PLANE ( 'NONE',  #8259 ) ;
#194193 = ORIENTED_EDGE ( 'NONE', *, *, #11514, .F. ) ;
#194192 = CARTESIAN_POINT ( 'NONE',  ( -16.93658211146644987, 66.00589133767134342, -182.6188124145687652 ) ) ;
#194195 = DIRECTION ( 'NONE',  ( -1.000000000000000000, 0.000000000000000000, 0.000000000000000000 ) ) ;
#194194 = AXIS2_PLACEMENT_3D ( 'NONE', #199530, #239931, #43011 ) ;
#194196 = ORIENTED_EDGE ( 'NONE', *, *, #4336, .T. ) ;
#194197 = CARTESIAN_POINT ( 'NONE',  ( 22.00411653962177638, 7.253442868381098307, -100.4009618941994404 ) ) ;
#194198 = EDGE_CURVE ( 'NONE', #177816, #157290, #112781, .T. ) ;
#194199 = ORIENTED_EDGE ( 'NONE', *, *, #110373, .F. ) ;
#194200 = CARTESIAN_POINT ( 'NONE',  ( -20.64999999999999858, 7.128833340094563376, -233.7327013124401276 ) ) ;
#194201 = CIRCLE ( 'NONE', #248334, 0.2000000000000057288 ) ;
#194202 = AXIS2_PLACEMENT_3D ( 'NONE', #109507, #92513, #73000 ) ;
#194203 = ADVANCED_FACE ( 'NONE', ( #78190 ), #187814, .F. ) ;
#194204 = ADVANCED_FACE ( 'NONE', ( #157793 ), #99021, .T. ) ;
#194205 = EDGE_LOOP ( 'NONE', ( #182330, #247639, #110609, #191188, #23999 ) ) ;
#194206 = CARTESIAN_POINT ( 'NONE',  ( -23.25000000000000000, 76.00000000001170974, -69.52310748452431710 ) ) ;
#194207 = FACE_OUTER_BOUND ( 'NONE', #165996, .T. ) ;
#194208 = EDGE_CURVE ( 'NONE', #108499, #198869, #37976, .T. ) ;
#194211 = ORIENTED_EDGE ( 'NONE', *, *, #225634, .F. ) ;
#194210 = EDGE_LOOP ( 'NONE', ( #150351, #21043, #75502, #121858, #88515 ) ) ;
#194209 = AXIS2_PLACEMENT_3D ( 'NONE', #170177, #11052, #153174 ) ;
#194212 = ORIENTED_EDGE ( 'NONE', *, *, #70438, .F. ) ;
#194213 = DIRECTION ( 'NONE',  ( 0.000000000000000000, -0.4088369013363494231, 0.9126074666063672680 ) ) ;
#194214 = CIRCLE ( 'NONE', #98460, 14.30833333333333890 ) ;
#194215 = EDGE_LOOP ( 'NONE', ( #166657, #20983, #95198, #74324 ) ) ;
#194216 = VECTOR ( 'NONE', #183434, 1000.000000000000227 ) ;
#194217 = EDGE_LOOP ( 'NONE', ( #10621, #48592, #164852, #105691, #107591 ) ) ;
#194218 = EDGE_CURVE ( 'NONE', #170769, #252337, #58766, .T. ) ;
#194219 = DIRECTION ( 'NONE',  ( 1.000000000000000000, 0.000000000000000000, 0.000000000000000000 ) ) ;
#194221 = VERTEX_POINT ( 'NONE', #3806 ) ;
#194220 = CARTESIAN_POINT ( 'NONE',  ( 18.43466021071411731, -9.494190690445389436, -107.1170615601277802 ) ) ;
#194222 = CARTESIAN_POINT ( 'NONE',  ( -20.54999999999999716, -8.999999999988844479, -90.60603087734760663 ) ) ;
#194223 = AXIS2_PLACEMENT_3D ( 'NONE', #127433, #165274, #84398 ) ;
#194225 = DIRECTION ( 'NONE',  ( -0.000000000000000000, 1.000000000000000000, 6.352154140967427193E-15 ) ) ;
#194224 = CARTESIAN_POINT ( 'NONE',  ( -21.14999999999999858, 76.10000000001222986, -148.1726782920690937 ) ) ;
#194226 = CARTESIAN_POINT ( 'NONE',  ( 23.25000000000000000, 64.25000000001253397, -182.1731074845244507 ) ) ;
#194227 = CARTESIAN_POINT ( 'NONE',  ( 18.42555734704284376, -9.497158361925558623, -74.03983049773501079 ) ) ;
#194228 = DIRECTION ( 'NONE',  ( -1.000000000000000000, -0.000000000000000000, -0.000000000000000000 ) ) ;
#194229 = ORIENTED_EDGE ( 'NONE', *, *, #256873, .F. ) ;
#194230 = EDGE_LOOP ( 'NONE', ( #82907, #242873, #112319 ) ) ;
#194231 = CARTESIAN_POINT ( 'NONE',  ( 20.94999999999999574, -11.64999999998883595, -136.9000000000000341 ) ) ;
#194232 = LINE ( 'NONE', #155111, #39338 ) ;
#194233 = DIRECTION ( 'NONE',  ( 0.000000000000000000, 0.9229812358756199764, -0.3848449534832346086 ) ) ;
#194234 = AXIS2_PLACEMENT_3D ( 'NONE', #107580, #142832, #222365 ) ;
#194235 = ORIENTED_EDGE ( 'NONE', *, *, #90470, .F. ) ;
#194237 = MANIFOLD_SOLID_BREP ( 'Stock-MAS-200-1', #3354 ) ;
#194236 = DIRECTION ( 'NONE',  ( 0.000000000000000000, -0.8814952561688437216, 0.4721928772777334582 ) ) ;
#194238 = ADVANCED_FACE ( 'NONE', ( #54149 ), #101581, .T. ) ;
#194239 = CARTESIAN_POINT ( 'NONE',  ( -16.93433913041102912, 51.67388201422455296, -231.8604821533804738 ) ) ;
#194240 = CARTESIAN_POINT ( 'NONE',  ( 18.49999999999998934, 6.550000000011156231, -155.1500000000000057 ) ) ;
#194241 = VERTEX_POINT ( 'NONE', #29500 ) ;
#194242 = ORIENTED_EDGE ( 'NONE', *, *, #58381, .F. ) ;
#194243 = DIRECTION ( 'NONE',  ( 1.000000000000000000, -2.849773892568378313E-16, 7.728835255496647986E-17 ) ) ;
#194244 = DIRECTION ( 'NONE',  ( 0.000000000000000000, 6.982962677686266711E-15, -1.000000000000000000 ) ) ;
#194246 = EDGE_CURVE ( 'NONE', #214743, #142573, #133796, .T. ) ;
#194245 = ORIENTED_EDGE ( 'NONE', *, *, #39743, .F. ) ;
#194247 = FACE_OUTER_BOUND ( 'NONE', #170577, .T. ) ;
#194248 = EDGE_LOOP ( 'NONE', ( #47292, #79107, #2382, #225045, #116516 ) ) ;
#194249 = ADVANCED_FACE ( 'NONE', ( #108985 ), #90708, .T. ) ;
#194250 = DIRECTION ( 'NONE',  ( 0.000000000000000000, 0.000000000000000000, 1.000000000000000000 ) ) ;
#194251 = CARTESIAN_POINT ( 'NONE',  ( -16.79363873026997922, 9.948850229429586634, -154.8461537814455085 ) ) ;
#194253 = CARTESIAN_POINT ( 'NONE',  ( -21.05000000000000071, -1.391858308744749362, -194.6091531227727955 ) ) ;
#194252 = CARTESIAN_POINT ( 'NONE',  ( 18.39999999999999503, 67.17743825834611471, -179.2731074845244166 ) ) ;
#194254 = AXIS2_PLACEMENT_3D ( 'NONE', #153425, #118104, #232943 ) ;
#194255 = CARTESIAN_POINT ( 'NONE',  ( 18.54148534481893407, 65.67467670974468774, -164.4531731826884879 ) ) ;
#194256 = CIRCLE ( 'NONE', #131684, 0.2000000000000003997 ) ;
#194257 = CARTESIAN_POINT ( 'NONE',  ( 23.14999999999998437, 67.23127455305841238, -235.8551265064783991 ) ) ;
#194258 = AXIS2_PLACEMENT_3D ( 'NONE', #25861, #90949, #229194 ) ;
#194259 = VECTOR ( 'NONE', #23332, 1000.000000000000000 ) ;
#194260 = EDGE_CURVE ( 'NONE', #122934, #97226, #230227, .T. ) ;
#194261 = FACE_OUTER_BOUND ( 'NONE', #96235, .T. ) ;
#194263 = VERTEX_POINT ( 'NONE', #8622 ) ;
#194262 = ORIENTED_EDGE ( 'NONE', *, *, #98231, .F. ) ;
#194264 = ORIENTED_EDGE ( 'NONE', *, *, #116414, .F. ) ;
#194265 = DIRECTION ( 'NONE',  ( 0.000000000000000000, -0.1335171055202867274, -0.9910465087640866200 ) ) ;
#194266 = CARTESIAN_POINT ( 'NONE',  ( 22.48508240969612615, 0.04627641451691485996, 11.65001073157356792 ) ) ;
#194267 = DIRECTION ( 'NONE',  ( -0.7071067811865389130, 4.937700262164590641E-15, -0.7071067811865561215 ) ) ;
#194268 = CARTESIAN_POINT ( 'NONE',  ( -18.45068461519105796, -9.486506529077932015, -107.5687771689047452 ) ) ;
#194269 = AXIS2_PLACEMENT_3D ( 'NONE', #71726, #52128, #9169 ) ;
#194271 = CARTESIAN_POINT ( 'NONE',  ( -12.60206096961791999, 66.61031399435616152, -87.35026397817303234 ) ) ;
#194270 = LINE ( 'NONE', #153885, #211844 ) ;
#194272 = PLANE ( 'NONE',  #253788 ) ;
#194273 = ORIENTED_EDGE ( 'NONE', *, *, #67528, .T. ) ;
#194274 = CARTESIAN_POINT ( 'NONE',  ( 21.14999999999999503, -0.1008583690875562017, -88.75043287651064361 ) ) ;
#194275 = CIRCLE ( 'NONE', #98332, 0.1999999999999905742 ) ;
#194276 = ORIENTED_EDGE ( 'NONE', *, *, #8767, .T. ) ;
#194278 = EDGE_CURVE ( 'NONE', #62345, #168131, #38155, .T. ) ;
#194277 = ORIENTED_EDGE ( 'NONE', *, *, #55144, .F. ) ;
#194279 = CARTESIAN_POINT ( 'NONE',  ( 23.25000000000000000, -8.895340756380869962, -215.3721227669300049 ) ) ;
#194280 = CARTESIAN_POINT ( 'NONE',  ( -23.15000000000000213, 75.47649400317826007, -205.4533772768803317 ) ) ;
#194281 = CARTESIAN_POINT ( 'NONE',  ( 21.93340585900753936, 76.00000000001273293, -210.8472545066313160 ) ) ;
#194282 = ADVANCED_FACE ( 'NONE', ( #150696 ), #111571, .F. ) ;
#194283 = CARTESIAN_POINT ( 'NONE',  ( -18.59999999999999787, 46.59314322379660922, -243.1831726892433210 ) ) ;
#194284 = ORIENTED_EDGE ( 'NONE', *, *, #203182, .T. ) ;
#194285 = ORIENTED_EDGE ( 'NONE', *, *, #134483, .T. ) ;
#194286 = CYLINDRICAL_SURFACE ( 'NONE', #97883, 0.1000000000000013933 ) ;
#194287 = VECTOR ( 'NONE', #54027, 1000.000000000000000 ) ;
#194289 = EDGE_CURVE ( 'NONE', #18380, #110751, #171574, .T. ) ;
#194288 = DIRECTION ( 'NONE',  ( 0.000000000000000000, -1.000000000000000000, 0.000000000000000000 ) ) ;
#194290 = FACE_OUTER_BOUND ( 'NONE', #103544, .T. ) ;
#194291 = DIRECTION ( 'NONE',  ( 0.000000000000000000, -0.8660254037844411501, -0.4999999999999956701 ) ) ;
#194292 = LINE ( 'NONE', #15659, #12960 ) ;
#194293 = FACE_OUTER_BOUND ( 'NONE', #235747, .T. ) ;
#194294 = DIRECTION ( 'NONE',  ( 0.000000000000000000, 8.783410004945868831E-15, -1.000000000000000000 ) ) ;
#194295 = EDGE_CURVE ( 'NONE', #231817, #82011, #2128, .T. ) ;
#194297 = DIRECTION ( 'NONE',  ( 1.000000000000000000, 0.000000000000000000, 0.000000000000000000 ) ) ;
#194296 = DIRECTION ( 'NONE',  ( 0.000000000000000000, 0.8814952561688438326, -0.4721928772777332362 ) ) ;
#194298 = CARTESIAN_POINT ( 'NONE',  ( -20.94999999999999929, -11.64999999998884306, -197.8999999999999773 ) ) ;
#194300 = EDGE_CURVE ( 'NONE', #105344, #173747, #250509, .T. ) ;
#194299 = CARTESIAN_POINT ( 'NONE',  ( 21.00000000000000000, -11.65000000000000036, 0.000000000000000000 ) ) ;
#194301 = CARTESIAN_POINT ( 'NONE',  ( -23.15000000000000213, 38.51006445970392633, -250.5427677435266389 ) ) ;
#194302 = CIRCLE ( 'NONE', #11106, 2.000000000000001776 ) ;
#194305 = ORIENTED_EDGE ( 'NONE', *, *, #92215, .F. ) ;
#194304 = CIRCLE ( 'NONE', #123530, 0.09999999999999520384 ) ;
#194303 = DIRECTION ( 'NONE',  ( -0.000000000000000000, 1.000000000000000000, -0.000000000000000000 ) ) ;
#194306 = AXIS2_PLACEMENT_3D ( 'NONE', #175492, #91123, #179344 ) ;
#194307 = AXIS2_PLACEMENT_3D ( 'NONE', #101181, #178233, #159947 ) ;
#194308 = ADVANCED_FACE ( 'NONE', ( #128565 ), #196335, .F. ) ;
#194309 = EDGE_CURVE ( 'NONE', #69570, #22186, #46484, .T. ) ;
#194310 = DIRECTION ( 'NONE',  ( -1.000000000000000000, 0.000000000000000000, 0.000000000000000000 ) ) ;
#194311 = ORIENTED_EDGE ( 'NONE', *, *, #9950, .T. ) ;
#194312 = CARTESIAN_POINT ( 'NONE',  ( -18.59999999999999787, 1.250000000011155299, -41.50000000000000000 ) ) ;
#194313 = FACE_OUTER_BOUND ( 'NONE', #12686, .T. ) ;
#194314 = CIRCLE ( 'NONE', #2732, 0.1000000000000001027 ) ;
#194315 = CARTESIAN_POINT ( 'NONE',  ( 13.88638282980484639, 9.457426452500058645, -85.50004186840010334 ) ) ;
#194316 = CARTESIAN_POINT ( 'NONE',  ( -23.25000000000000000, 6.982009704867601307, -104.1961521182563359 ) ) ;
#194317 = CIRCLE ( 'NONE', #98554, 0.09999999999999939493 ) ;
#194318 = VECTOR ( 'NONE', #126738, 1000.000000000000000 ) ;
#194319 = ADVANCED_FACE ( 'NONE', ( #49019 ), #153300, .T. ) ;
#194320 = DIRECTION ( 'NONE',  ( 0.000000000000000000, 0.000000000000000000, 1.000000000000000000 ) ) ;
#194321 = EDGE_CURVE ( 'NONE', #89168, #239754, #71177, .T. ) ;
#194322 = CARTESIAN_POINT ( 'NONE',  ( 18.59999999999999076, 6.550000000000000711, -10.01702717044001822 ) ) ;
#194323 = DIRECTION ( 'NONE',  ( 1.186688945009010077E-16, 1.000000000000000000, 6.982962677686266711E-15 ) ) ;
#194324 = VECTOR ( 'NONE', #111313, 1000.000000000000000 ) ;
#194325 = ORIENTED_EDGE ( 'NONE', *, *, #58820, .T. ) ;
#194326 = CYLINDRICAL_SURFACE ( 'NONE', #245453, 0.09999999999999939493 ) ;
#194328 = ORIENTED_EDGE ( 'NONE', *, *, #175200, .F. ) ;
#194327 = CARTESIAN_POINT ( 'NONE',  ( -18.59999999999999787, -1.164121893230052995, -74.91484808557160591 ) ) ;
#194329 = DIRECTION ( 'NONE',  ( -0.000000000000000000, -0.000000000000000000, -1.000000000000000000 ) ) ;
#194330 = DIRECTION ( 'NONE',  ( 0.000000000000000000, 1.776356839400250267E-15, -1.000000000000000000 ) ) ;
#194331 = DIRECTION ( 'NONE',  ( 1.000000000000000000, 0.000000000000000000, 0.000000000000000000 ) ) ;
#194332 = ORIENTED_EDGE ( 'NONE', *, *, #196716, .T. ) ;
#194333 = CARTESIAN_POINT ( 'NONE',  ( -20.94999999999999929, -1.835859311432479268, -212.5044391687984842 ) ) ;
#194334 = APPLICATION_PROTOCOL_DEFINITION ( 'draft international standard', 'automotive_design', 1998, #7431 ) ;
#194335 = EDGE_CURVE ( 'NONE', #58001, #190621, #236635, .T. ) ;
#194336 = CARTESIAN_POINT ( 'NONE',  ( -21.14999999999999858, 69.45934304831143891, -203.5231074845243882 ) ) ;
#194337 = CARTESIAN_POINT ( 'NONE',  ( -21.44999999999999929, 7.349999999999998757, -21.15000000000000213 ) ) ;
#194338 = ORIENTED_EDGE ( 'NONE', *, *, #250436, .T. ) ;
#194339 = PLANE ( 'NONE',  #37922 ) ;
#194340 = DIRECTION ( 'NONE',  ( 0.000000000000000000, -1.000000000000000000, 0.000000000000000000 ) ) ;
#194341 = EDGE_CURVE ( 'NONE', #227768, #24438, #254863, .T. ) ;
#194342 = AXIS2_PLACEMENT_3D ( 'NONE', #253520, #149322, #231418 ) ;
#194343 = DIRECTION ( 'NONE',  ( 1.000000000000000000, -0.000000000000000000, -0.000000000000000000 ) ) ;
#194344 = ORIENTED_EDGE ( 'NONE', *, *, #70228, .F. ) ;
#194345 = ORIENTED_EDGE ( 'NONE', *, *, #165608, .T. ) ;
#194346 = ADVANCED_FACE ( 'NONE', ( #194978 ), #97093, .F. ) ;
#194347 = AXIS2_PLACEMENT_3D ( 'NONE', #42263, #100894, #37141 ) ;
#194348 = DIRECTION ( 'NONE',  ( -1.000000000000000000, 0.000000000000000000, 0.000000000000000000 ) ) ;
#194349 = PLANE ( 'NONE',  #2977 ) ;
#194350 = CYLINDRICAL_SURFACE ( 'NONE', #77689, 0.09999999999999939493 ) ;
#194351 = CARTESIAN_POINT ( 'NONE',  ( 20.94999999999999929, 7.021664781911246322, -204.8335654018972605 ) ) ;
#194354 = DIRECTION ( 'NONE',  ( 0.000000000000000000, -1.000000000000000000, 0.000000000000000000 ) ) ;
#194353 = TOROIDAL_SURFACE ( 'NONE', #190238, 0.4000000000000003553, 0.1000000000000000056 ) ;
#194352 = CARTESIAN_POINT ( 'NONE',  ( 21.13435531349809438, -1.381870305043258584, -194.6550139707225355 ) ) ;
#194355 = EDGE_CURVE ( 'NONE', #252063, #48880, #200448, .T. ) ;
#194356 = PLANE ( 'NONE',  #198422 ) ;
#194357 = CARTESIAN_POINT ( 'NONE',  ( -20.15000000000000568, 66.70857864377425983, -57.17310748452438673 ) ) ;
#194358 = CARTESIAN_POINT ( 'NONE',  ( 18.55807992284871588, 65.67101464000451472, -30.44043916224795510 ) ) ;
#194359 = LINE ( 'NONE', #53535, #134808 ) ;
#194360 = VECTOR ( 'NONE', #220500, 1000.000000000000000 ) ;
#194361 = ORIENTED_EDGE ( 'NONE', *, *, #46044, .T. ) ;
#194362 = CIRCLE ( 'NONE', #210894, 0.1000000000000055844 ) ;
#194363 = ORIENTED_EDGE ( 'NONE', *, *, #243309, .T. ) ;
#194364 = CARTESIAN_POINT ( 'NONE',  ( 20.94999999999999929, -1.835341550213257733, -78.55515129256302487 ) ) ;
#194365 = CARTESIAN_POINT ( 'NONE',  ( -17.29838795457901313, 65.62845014207074712, -147.9183662019067640 ) ) ;
#194367 = FACE_OUTER_BOUND ( 'NONE', #109888, .T. ) ;
#194366 = CARTESIAN_POINT ( 'NONE',  ( -18.50000000000000000, 66.65000000001259650, -191.3731074845244393 ) ) ;
#194368 = AXIS2_PLACEMENT_3D ( 'NONE', #19844, #99332, #220598 ) ;
#194369 = CARTESIAN_POINT ( 'NONE',  ( 18.39999999999999147, 8.822561741677553471, -143.2500000000000284 ) ) ;
#194370 = DIRECTION ( 'NONE',  ( 1.000000000000000000, 0.000000000000000000, 0.000000000000000000 ) ) ;
#194371 = EDGE_CURVE ( 'NONE', #44800, #110771, #138786, .T. ) ;
#194372 = DIRECTION ( 'NONE',  ( -1.000000000000000000, 0.000000000000000000, -0.000000000000000000 ) ) ;
#194373 = ORIENTED_EDGE ( 'NONE', *, *, #42974, .F. ) ;
#194374 = EDGE_LOOP ( 'NONE', ( #242018, #136451, #56982, #23972 ) ) ;
#194375 = CARTESIAN_POINT ( 'NONE',  ( -23.25000000000000000, 17.01923898301589944, -224.3994341343041867 ) ) ;
#194376 = VERTEX_POINT ( 'NONE', #256140 ) ;
#194377 = CARTESIAN_POINT ( 'NONE',  ( -23.25000000000000000, -8.999999999988844479, -157.6060308773475924 ) ) ;
#194378 = VECTOR ( 'NONE', #158112, 1000.000000000000000 ) ;
#194379 = PLANE ( 'NONE',  #168651 ) ;
#194380 = AXIS2_PLACEMENT_3D ( 'NONE', #19991, #43388, #1676 ) ;
#194381 = CARTESIAN_POINT ( 'NONE',  ( -21.07971444708686093, 65.48967103324704908, -241.9412416822181058 ) ) ;
#194382 = AXIS2_PLACEMENT_3D ( 'NONE', #114029, #248424, #110183 ) ;
#194384 = ORIENTED_EDGE ( 'NONE', *, *, #40055, .F. ) ;
#194383 = VECTOR ( 'NONE', #96233, 1000.000000000000114 ) ;
#194385 = DIRECTION ( 'NONE',  ( 0.000000000000000000, 0.2558827019433787542, -0.9667078373770204847 ) ) ;
#194386 = AXIS2_PLACEMENT_3D ( 'NONE', #142753, #39849, #119370 ) ;
#194387 = DIRECTION ( 'NONE',  ( -2.827886303505249259E-16, 0.8660254037844412611, 0.4999999999999956701 ) ) ;
#194388 = CARTESIAN_POINT ( 'NONE',  ( 21.05000000000000426, 0.06570161033324307953, -27.24168394266797222 ) ) ;
#194389 = FACE_OUTER_BOUND ( 'NONE', #107124, .T. ) ;
#194390 = DIRECTION ( 'NONE',  ( 0.000000000000000000, 0.000000000000000000, -1.000000000000000000 ) ) ;
#194392 = DIRECTION ( 'NONE',  ( 1.000000000000000000, 0.000000000000000000, 0.000000000000000000 ) ) ;
#194391 = DIRECTION ( 'NONE',  ( 1.000000000000000000, 0.000000000000000000, 0.000000000000000000 ) ) ;
#194393 = CARTESIAN_POINT ( 'NONE',  ( -16.87683809663752044, 66.05000000001224691, -149.9254715027207396 ) ) ;
#194394 = ORIENTED_EDGE ( 'NONE', *, *, #141500, .F. ) ;
#194396 = CARTESIAN_POINT ( 'NONE',  ( -17.11825945287481332, 10.05000000001113847, -87.85000000000003695 ) ) ;
#194395 = FACE_OUTER_BOUND ( 'NONE', #113881, .T. ) ;
#194397 = ORIENTED_EDGE ( 'NONE', *, *, #187853, .F. ) ;
#194399 = ORIENTED_EDGE ( 'NONE', *, *, #86659, .F. ) ;
#194398 = FACE_OUTER_BOUND ( 'NONE', #153578, .T. ) ;
#194400 = AXIS2_PLACEMENT_3D ( 'NONE', #16215, #257306, #198672 ) ;
#194401 = EDGE_LOOP ( 'NONE', ( #158623, #226935, #1001, #167008, #225814 ) ) ;
#194402 = CARTESIAN_POINT ( 'NONE',  ( -18.59999999999999787, 74.73821383144657204, -61.43660852097884373 ) ) ;
#194403 = AXIS2_PLACEMENT_3D ( 'NONE', #128194, #207746, #29139 ) ;
#194404 = CYLINDRICAL_SURFACE ( 'NONE', #146689, 4.049999999999998046 ) ;
#194405 = CIRCLE ( 'NONE', #152720, 0.09999999999998898659 ) ;
#194406 = CARTESIAN_POINT ( 'NONE',  ( 21.05000000000000071, -8.999999999988842703, -157.6060308773475640 ) ) ;
#194407 = DIRECTION ( 'NONE',  ( 1.000000000000000000, 0.000000000000000000, -0.000000000000000000 ) ) ;
#194408 = ORIENTED_EDGE ( 'NONE', *, *, #198071, .F. ) ;
#194409 = CARTESIAN_POINT ( 'NONE',  ( -21.44999999999999929, 68.85000000001228670, -157.6731074845243938 ) ) ;
#194410 = DIRECTION ( 'NONE',  ( 1.000000000000000000, 0.000000000000000000, 0.000000000000000000 ) ) ;
#194411 = ORIENTED_EDGE ( 'NONE', *, *, #166199, .F. ) ;
#194412 = DIRECTION ( 'NONE',  ( 0.000000000000000000, -0.2605042016806647931, -0.9654727137038724427 ) ) ;
#194413 = EDGE_CURVE ( 'NONE', #205356, #228375, #17305, .T. ) ;
#194414 = AXIS2_PLACEMENT_3D ( 'NONE', #21643, #238098, #59432 ) ;
#194415 = CARTESIAN_POINT ( 'NONE',  ( 21.09316766718127667, 6.370153312474412743, 0.03926340231470034497 ) ) ;
#194416 = ORIENTED_EDGE ( 'NONE', *, *, #179759, .T. ) ;
#194417 = VERTEX_POINT ( 'NONE', #34620 ) ;
#194418 = CARTESIAN_POINT ( 'NONE',  ( -16.91256925476569961, 9.985731158139330432, -188.4676424890052431 ) ) ;
#194419 = ORIENTED_EDGE ( 'NONE', *, *, #251342, .T. ) ;
#194420 = DIRECTION ( 'NONE',  ( 0.000000000000000000, -6.982962677686266711E-15, 1.000000000000000000 ) ) ;
#194421 = ORIENTED_EDGE ( 'NONE', *, *, #102232, .F. ) ;
#194422 = CARTESIAN_POINT ( 'NONE',  ( 21.05000000000000426, 75.93429838969034051, -176.2814235418563840 ) ) ;
#194423 = DIRECTION ( 'NONE',  ( 0.000000000000000000, -0.8814952561688444987, 0.4721928772777320149 ) ) ;
#194424 = DIRECTION ( 'NONE',  ( -1.000000000000000000, -0.000000000000000000, 0.000000000000000000 ) ) ;
#194425 = DIRECTION ( 'NONE',  ( 0.000000000000000000, 0.000000000000000000, 1.000000000000000000 ) ) ;
#194426 = AXIS2_PLACEMENT_3D ( 'NONE', #69707, #207934, #72268 ) ;
#194427 = ADVANCED_FACE ( 'NONE', ( #114122 ), #176694, .F. ) ;
#194428 = AXIS2_PLACEMENT_3D ( 'NONE', #228794, #190966, #68428 ) ;
#194429 = AXIS2_PLACEMENT_3D ( 'NONE', #216019, #256380, #55638 ) ;
#194430 = CARTESIAN_POINT ( 'NONE',  ( -21.95218792049438861, 0.09902843981107177507, -26.29849243875332121 ) ) ;
#194431 = CARTESIAN_POINT ( 'NONE',  ( 18.44206774312970865, -9.491027357528929898, -73.62622750469815003 ) ) ;
#194432 = DIRECTION ( 'NONE',  ( 1.000000000000000000, 0.000000000000000000, 0.000000000000000000 ) ) ;
#194433 = VERTEX_POINT ( 'NONE', #39764 ) ;
#194435 = LINE ( 'NONE', #90151, #189751 ) ;
#194434 = CARTESIAN_POINT ( 'NONE',  ( 23.15000000000000213, -11.64999999999999147, -30.50000000000000000 ) ) ;
#194436 = ORIENTED_EDGE ( 'NONE', *, *, #174102, .F. ) ;
#194439 = EDGE_LOOP ( 'NONE', ( #146374, #187212, #35432 ) ) ;
#194438 = DIRECTION ( 'NONE',  ( 0.000000000000000000, 0.2128009952263485993, -0.9770955615653341697 ) ) ;
#194437 = CARTESIAN_POINT ( 'NONE',  ( -20.94999999999999929, 64.35000000001220144, -143.3069731475025321 ) ) ;
#194440 = VECTOR ( 'NONE', #170824, 1000.000000000000000 ) ;
#194441 = ORIENTED_EDGE ( 'NONE', *, *, #74303, .F. ) ;
#194442 = CARTESIAN_POINT ( 'NONE',  ( -23.25000000000000000, 7.783179459866048866, -245.3643104511423019 ) ) ;
#194443 = CARTESIAN_POINT ( 'NONE',  ( 20.04142135623730070, 64.25000000001176659, -78.37310748452439668 ) ) ;
#194444 = CYLINDRICAL_SURFACE ( 'NONE', #115181, 0.1000000000000028644 ) ;
#194445 = EDGE_CURVE ( 'NONE', #195194, #191153, #213218, .T. ) ;
#194446 = LINE ( 'NONE', #198264, #204253 ) ;
#194447 = ORIENTED_EDGE ( 'NONE', *, *, #48335, .F. ) ;
#194449 = ORIENTED_EDGE ( 'NONE', *, *, #250558, .F. ) ;
#194448 = LINE ( 'NONE', #211421, #167903 ) ;
#194450 = EDGE_CURVE ( 'NONE', #232566, #176771, #25663, .T. ) ;
#194451 = TOROIDAL_SURFACE ( 'NONE', #140220, 0.2000000000000000111, 0.1000000000000000056 ) ;
#194452 = EDGE_CURVE ( 'NONE', #40042, #241304, #513, .T. ) ;
#194454 = DIRECTION ( 'NONE',  ( 0.000000000000000000, -6.938893903907222067E-15, -1.000000000000000000 ) ) ;
#194453 = DIRECTION ( 'NONE',  ( 0.000000000000000000, -0.9770955615653315052, -0.2128009952263603954 ) ) ;
#194455 = AXIS2_PLACEMENT_3D ( 'NONE', #88650, #168264, #247752 ) ;
#194457 = ORIENTED_EDGE ( 'NONE', *, *, #139590, .T. ) ;
#194456 = DIRECTION ( 'NONE',  ( 0.000000000000000000, -0.9889818879709272315, -0.1480365673253073999 ) ) ;
#194458 = CIRCLE ( 'NONE', #181951, 0.09999999999999939493 ) ;
#194459 = EDGE_CURVE ( 'NONE', #7521, #2147, #187989, .T. ) ;
#194460 = VERTEX_POINT ( 'NONE', #35903 ) ;
#194461 = ADVANCED_BREP_SHAPE_REPRESENTATION ( '', ( #189505, #2425 ), #119141 ) ;
#194462 = CIRCLE ( 'NONE', #95032, 12.87499999999999822 ) ;
#194463 = DIRECTION ( 'NONE',  ( 0.000000000000000000, -0.9126074666063770380, -0.4088369013363281068 ) ) ;
#194464 = DIRECTION ( 'NONE',  ( 1.000000000000000000, 2.952720810173289112E-16, -0.000000000000000000 ) ) ;
#194465 = EDGE_LOOP ( 'NONE', ( #89623, #53956, #110541, #227046 ) ) ;
#194466 = FACE_OUTER_BOUND ( 'NONE', #164038, .T. ) ;
#194467 = ADVANCED_FACE ( 'NONE', ( #155851 ), #117248, .T. ) ;
#194468 = VERTEX_POINT ( 'NONE', #98371 ) ;
#194469 = DIRECTION ( 'NONE',  ( 0.000000000000000000, -0.8814952561688430555, 0.4721928772777346239 ) ) ;
#194470 = DIRECTION ( 'NONE',  ( -0.000000000000000000, -1.000000000000000000, -7.272083257015735086E-15 ) ) ;
#194471 = ORIENTED_EDGE ( 'NONE', *, *, #121864, .F. ) ;
#194472 = DIRECTION ( 'NONE',  ( 0.000000000000000000, 1.000000000000000000, 6.982962677686266711E-15 ) ) ;
#194473 = EDGE_CURVE ( 'NONE', #248851, #111708, #154579, .T. ) ;
#194474 = CIRCLE ( 'NONE', #206917, 0.09999999999999939493 ) ;
#194475 = LINE ( 'NONE', #73253, #193688 ) ;
#194476 = CIRCLE ( 'NONE', #177899, 0.1999999999999987899 ) ;
#194477 = AXIS2_PLACEMENT_3D ( 'NONE', #109588, #187876, #127890 ) ;
#194478 = ORIENTED_EDGE ( 'NONE', *, *, #121730, .T. ) ;
#194479 = ORIENTED_EDGE ( 'NONE', *, *, #10389, .F. ) ;
#194480 = CARTESIAN_POINT ( 'NONE',  ( 23.14999999999999503, 11.75000000001116263, -88.75000000000004263 ) ) ;
#194481 = ORIENTED_EDGE ( 'NONE', *, *, #108168, .T. ) ;
#194482 = ORIENTED_EDGE ( 'NONE', *, *, #37021, .T. ) ;
#194484 = EDGE_LOOP ( 'NONE', ( #129290, #228176, #191262, #140854 ) ) ;
#194483 = CYLINDRICAL_SURFACE ( 'NONE', #201007, 0.1000000000000118433 ) ;
#194485 = ORIENTED_EDGE ( 'NONE', *, *, #139886, .F. ) ;
#194486 = CARTESIAN_POINT ( 'NONE',  ( 18.49999999999999645, -1.162701749926855266, -108.6000000000000227 ) ) ;
#194487 = VERTEX_POINT ( 'NONE', #59245 ) ;
#194490 = ORIENTED_EDGE ( 'NONE', *, *, #200338, .T. ) ;
#194489 = VERTEX_POINT ( 'NONE', #253622 ) ;
#194488 = CARTESIAN_POINT ( 'NONE',  ( -23.15000000000000213, 64.25000000001246292, -181.7731074845244450 ) ) ;
#194491 = CIRCLE ( 'NONE', #36274, 0.09999999999999939493 ) ;
#194492 = CIRCLE ( 'NONE', #7028, 0.09999999999998898659 ) ;
#194493 = ORIENTED_EDGE ( 'NONE', *, *, #26467, .T. ) ;
#194494 = DIRECTION ( 'NONE',  ( 0.000000000000000000, 1.000000000000000000, 6.938893903907222067E-15 ) ) ;
#194495 = EDGE_CURVE ( 'NONE', #32249, #177703, #183878, .T. ) ;
#194496 = CIRCLE ( 'NONE', #173685, 1.899999999999999023 ) ;
#194497 = DIRECTION ( 'NONE',  ( 0.7071067811865475727, 0.7071067811865475727, 4.937700262164531476E-15 ) ) ;
#194498 = ADVANCED_FACE ( 'NONE', ( #233647 ), #70738, .F. ) ;
#194499 = VERTEX_POINT ( 'NONE', #9447 ) ;
#194500 = PLANE ( 'NONE',  #116415 ) ;
#194502 = VERTEX_POINT ( 'NONE', #171142 ) ;
#194501 = DIRECTION ( 'NONE',  ( -1.000000000000000000, -0.000000000000000000, -0.000000000000000000 ) ) ;
#194503 = CARTESIAN_POINT ( 'NONE',  ( 20.94999999999999929, 1.835341550235569663, -112.0551512925630249 ) ) ;
#194504 = ORIENTED_EDGE ( 'NONE', *, *, #180110, .F. ) ;
#194505 = EDGE_CURVE ( 'NONE', #102030, #25976, #251908, .T. ) ;
#194506 = EDGE_CURVE ( 'NONE', #201773, #244346, #125610, .T. ) ;
#194507 = VERTEX_POINT ( 'NONE', #92826 ) ;
#194508 = CARTESIAN_POINT ( 'NONE',  ( 20.99999999999999645, 13.96358247574307221, -219.2976327551816951 ) ) ;
#194509 = CARTESIAN_POINT ( 'NONE',  ( 20.94999999999999929, 10.29270135741298731, -206.4573618871519045 ) ) ;
#194510 = EDGE_CURVE ( 'NONE', #95294, #86390, #168582, .T. ) ;
#194511 = ORIENTED_EDGE ( 'NONE', *, *, #256833, .T. ) ;
#194512 = VERTEX_POINT ( 'NONE', #189382 ) ;
#194513 = EDGE_CURVE ( 'NONE', #2430, #34898, #131961, .T. ) ;
#194514 = MECHANICAL_DESIGN_GEOMETRIC_PRESENTATION_REPRESENTATION (  '', ( #232112 ), #86309 ) ;
#194516 = EDGE_CURVE ( 'NONE', #29111, #166243, #163055, .T. ) ;
#194515 = EDGE_CURVE ( 'NONE', #114911, #253025, #112414, .T. ) ;
#194518 = ORIENTED_EDGE ( 'NONE', *, *, #86425, .T. ) ;
#194517 = EDGE_LOOP ( 'NONE', ( #56509, #199083, #90945, #221836 ) ) ;
#194519 = ORIENTED_EDGE ( 'NONE', *, *, #109051, .F. ) ;
#194520 = FACE_OUTER_BOUND ( 'NONE', #231313, .T. ) ;
#194521 = VERTEX_POINT ( 'NONE', #151560 ) ;
#194522 = ORIENTED_EDGE ( 'NONE', *, *, #247646, .T. ) ;
#194523 = EDGE_CURVE ( 'NONE', #257538, #225666, #112963, .T. ) ;
#194524 = CARTESIAN_POINT ( 'NONE',  ( -20.54999999999999716, 85.00000000001222134, -146.4170766071767389 ) ) ;
#194525 = EDGE_LOOP ( 'NONE', ( #105181, #96207, #94714, #67758 ) ) ;
#194526 = CARTESIAN_POINT ( 'NONE',  ( 18.59999999999999787, -11.65000000000000036, 30.09999999999999787 ) ) ;
#194527 = AXIS2_PLACEMENT_3D ( 'NONE', #113154, #213525, #174467 ) ;
#194528 = FACE_OUTER_BOUND ( 'NONE', #85884, .T. ) ;
#194529 = VERTEX_POINT ( 'NONE', #53708 ) ;
#194530 = ADVANCED_FACE ( 'NONE', ( #173714 ), #73309, .F. ) ;
#194531 = VERTEX_POINT ( 'NONE', #232375 ) ;
#194532 = AXIS2_PLACEMENT_3D ( 'NONE', #185691, #25353, #186995 ) ;
#194533 = DIRECTION ( 'NONE',  ( 0.000000000000000000, -0.9893560106964500722, 0.1455152366551550613 ) ) ;
#194534 = ADVANCED_FACE ( 'NONE', ( #35472 ), #188093, .T. ) ;
#194535 = EDGE_CURVE ( 'NONE', #99384, #10361, #171443, .T. ) ;
#194536 = VERTEX_POINT ( 'NONE', #113684 ) ;
#194537 = AXIS2_PLACEMENT_3D ( 'NONE', #105189, #4824, #83064 ) ;
#194538 = CIRCLE ( 'NONE', #144406, 0.09999999999999939493 ) ;
#194539 = DIRECTION ( 'NONE',  ( 0.000000000000000000, 0.2617529984165033463, 0.9651348961777157509 ) ) ;
#194540 = EDGE_CURVE ( 'NONE', #173153, #214061, #12042, .T. ) ;
#194541 = FACE_OUTER_BOUND ( 'NONE', #169384, .T. ) ;
#194542 = TOROIDAL_SURFACE ( 'NONE', #82057, 0.6000000000000004219, 0.1000000000000000056 ) ;
#194543 = EDGE_LOOP ( 'NONE', ( #242040, #207340, #14763, #37269 ) ) ;
#194544 = ORIENTED_EDGE ( 'NONE', *, *, #34931, .F. ) ;
#194545 = DIRECTION ( 'NONE',  ( 1.000000000000000000, 0.000000000000000000, 0.000000000000000000 ) ) ;
#194546 = VECTOR ( 'NONE', #104121, 1000.000000000000000 ) ;
#194549 = ADVANCED_FACE ( 'NONE', ( #211508 ), #69444, .T. ) ;
#194548 = ORIENTED_EDGE ( 'NONE', *, *, #172627, .F. ) ;
#194547 = CARTESIAN_POINT ( 'NONE',  ( 18.47073956224741309, 85.47172941248430789, -162.9144217317066250 ) ) ;
#194550 = CARTESIAN_POINT ( 'NONE',  ( 21.14999999999999858, 1.115600667400684642E-11, -127.4593430482987912 ) ) ;
#194551 = DIRECTION ( 'NONE',  ( 0.000000000000000000, -0.000000000000000000, 1.000000000000000000 ) ) ;
#194552 = ORIENTED_EDGE ( 'NONE', *, *, #240316, .T. ) ;
#194553 = EDGE_CURVE ( 'NONE', #147707, #175608, #14614, .T. ) ;
#194554 = CARTESIAN_POINT ( 'NONE',  ( -23.15000000000000213, 11.38316329224760359, -198.5208684056144079 ) ) ;
#194555 = DIRECTION ( 'NONE',  ( 1.000000000000000000, 0.000000000000000000, 0.000000000000000000 ) ) ;
#194556 = DIRECTION ( 'NONE',  ( 1.000000000000000000, 0.000000000000000000, 0.000000000000000000 ) ) ;
#194557 = FACE_OUTER_BOUND ( 'NONE', #207944, .T. ) ;
#194558 = CARTESIAN_POINT ( 'NONE',  ( -20.65000000000000568, 18.70606281991846842, -231.7096448200342138 ) ) ;
#194559 = CARTESIAN_POINT ( 'NONE',  ( 21.05000000000000071, 65.27628289530476025, -157.8619171903969800 ) ) ;
#194560 = CARTESIAN_POINT ( 'NONE',  ( -22.24259225415828567, 68.50806212944624463, -69.62217336797721146 ) ) ;
#194561 = CARTESIAN_POINT ( 'NONE',  ( 22.49999999999999645, 75.91119002362528079, -148.1728704025562138 ) ) ;
#194562 = CARTESIAN_POINT ( 'NONE',  ( -23.25000000000000000, 76.00000000001195133, -103.0231074845243171 ) ) ;
#194563 = AXIS2_PLACEMENT_3D ( 'NONE', #13125, #187909, #31433 ) ;
#194564 = EDGE_LOOP ( 'NONE', ( #232178, #132258, #216564, #194245 ) ) ;
#194565 = CIRCLE ( 'NONE', #148758, 0.1000000000000028644 ) ;
#194568 = EDGE_LOOP ( 'NONE', ( #124321, #217737, #63188, #37402 ) ) ;
#194567 = ORIENTED_EDGE ( 'NONE', *, *, #231595, .F. ) ;
#194566 = CIRCLE ( 'NONE', #198620, 0.1000000000000028644 ) ;
#194569 = ORIENTED_EDGE ( 'NONE', *, *, #157054, .F. ) ;
#194570 = AXIS2_PLACEMENT_3D ( 'NONE', #113897, #154357, #196018 ) ;
#194571 = DIRECTION ( 'NONE',  ( 0.000000000000000000, 0.8096735173027155286, -0.5868805631290315850 ) ) ;
#194572 = DIRECTION ( 'NONE',  ( 0.000000000000000000, 0.9126074666063773710, 0.4088369013363274962 ) ) ;
#194573 = VECTOR ( 'NONE', #117465, 1000.000000000000000 ) ;
#194574 = VECTOR ( 'NONE', #32944, 1000.000000000000000 ) ;
#194576 = DIRECTION ( 'NONE',  ( 0.000000000000000000, 0.000000000000000000, -1.000000000000000000 ) ) ;
#194575 = CARTESIAN_POINT ( 'NONE',  ( 23.15000000000000213, 87.48912529308798014, -106.0231074845242176 ) ) ;
#194577 = ORIENTED_EDGE ( 'NONE', *, *, #141432, .F. ) ;
#194578 = ORIENTED_EDGE ( 'NONE', *, *, #59382, .F. ) ;
#194579 = FACE_OUTER_BOUND ( 'NONE', #28774, .T. ) ;
#194580 = LINE ( 'NONE', #17215, #133340 ) ;
#194581 = CARTESIAN_POINT ( 'NONE',  ( -22.59999999999999787, 64.25012875563544412, -103.0885370755380706 ) ) ;
#194582 = DIRECTION ( 'NONE',  ( 1.000000000000000000, 0.000000000000000000, 0.000000000000000000 ) ) ;
#194583 = EDGE_LOOP ( 'NONE', ( #41913, #241882, #99658, #26250 ) ) ;
#194584 = VERTEX_POINT ( 'NONE', #72007 ) ;
#194585 = AXIS2_PLACEMENT_3D ( 'NONE', #65284, #220519, #101810 ) ;
#194586 = DIRECTION ( 'NONE',  ( -1.000000000000000000, 0.000000000000000000, -0.000000000000000000 ) ) ;
#194587 = TOROIDAL_SURFACE ( 'NONE', #107062, 2.100000000000002309, 0.1000000000000000056 ) ;
#194588 = DIRECTION ( 'NONE',  ( 0.000000000000000000, 0.000000000000000000, -1.000000000000000000 ) ) ;
#194589 = ORIENTED_EDGE ( 'NONE', *, *, #122385, .T. ) ;
#194590 = DIRECTION ( 'NONE',  ( -2.081668171172008469E-13, -0.6413305999522614931, -0.7672646620071019719 ) ) ;
#194591 = CARTESIAN_POINT ( 'NONE',  ( 18.36493879433090370, 77.43242999775311830, -241.6948683660838242 ) ) ;
#194592 = DIRECTION ( 'NONE',  ( 0.000000000000000000, -0.7397360091702802620, 0.6728971962616779878 ) ) ;
#194593 = FACE_OUTER_BOUND ( 'NONE', #224029, .T. ) ;
#194594 = DIRECTION ( 'NONE',  ( 0.000000000000000000, 0.000000000000000000, 1.000000000000000000 ) ) ;
#194595 = ORIENTED_EDGE ( 'NONE', *, *, #85791, .F. ) ;
#194596 = DIRECTION ( 'NONE',  ( 1.000000000000000000, -0.000000000000000000, -0.000000000000000000 ) ) ;
#194597 = DIRECTION ( 'NONE',  ( 1.000000000000000000, 0.000000000000000000, 0.000000000000000000 ) ) ;
#194598 = DIRECTION ( 'NONE',  ( 1.000000000000000000, -0.000000000000000000, -0.000000000000000000 ) ) ;
#194599 = CIRCLE ( 'NONE', #195154, 0.1000000000000045158 ) ;
#194600 = EDGE_CURVE ( 'NONE', #151185, #29926, #254742, .T. ) ;
#194602 = DIRECTION ( 'NONE',  ( 0.000000000000000000, 0.8814952561688437216, -0.4721928772777331806 ) ) ;
#194601 = CYLINDRICAL_SURFACE ( 'NONE', #45211, 0.1000000000000028644 ) ;
#194603 = FACE_OUTER_BOUND ( 'NONE', #52699, .T. ) ;
#194604 = TOROIDAL_SURFACE ( 'NONE', #82111, 11.65000000000000036, 0.1000000000000000056 ) ;
#194605 = DIRECTION ( 'NONE',  ( -1.000000000000000000, -6.754466386607082172E-16, 1.507734853975053202E-15 ) ) ;
#194607 = EDGE_CURVE ( 'NONE', #190048, #80064, #29966, .T. ) ;
#194606 = CARTESIAN_POINT ( 'NONE',  ( 21.05000000000000071, 87.65000000001172964, -72.42310748452422331 ) ) ;
#194608 = CARTESIAN_POINT ( 'NONE',  ( -22.20000000000000284, 6.322468214605804882, 12.11686199900910310 ) ) ;
#194609 = ORIENTED_EDGE ( 'NONE', *, *, #126456, .T. ) ;
#194610 = VECTOR ( 'NONE', #144424, 1000.000000000000000 ) ;
#194611 = EDGE_LOOP ( 'NONE', ( #174323, #43519 ) ) ;
#194612 = EDGE_CURVE ( 'NONE', #97945, #180641, #51874, .T. ) ;
#194613 = CARTESIAN_POINT ( 'NONE',  ( 5.551115123125782702E-14, 76.00000000001119815, -3.023107484524792277 ) ) ;
#194614 = ADVANCED_FACE ( 'NONE', ( #252646 ), #38324, .F. ) ;
#194615 = VERTEX_POINT ( 'NONE', #251374 ) ;
#194616 = DIRECTION ( 'NONE',  ( 1.000000000000000000, 0.000000000000000000, 0.000000000000000000 ) ) ;
#194617 = CIRCLE ( 'NONE', #82126, 0.09999999999999939493 ) ;
#194618 = CIRCLE ( 'NONE', #227908, 0.1000000000000028644 ) ;
#194619 = VERTEX_POINT ( 'NONE', #92298 ) ;
#194620 = VECTOR ( 'NONE', #95456, 1000.000000000000000 ) ;
#194621 = CIRCLE ( 'NONE', #148818, 0.1000000000000028644 ) ;
#194622 = FACE_OUTER_BOUND ( 'NONE', #4484, .T. ) ;
#194623 = VERTEX_POINT ( 'NONE', #210976 ) ;
#194624 = AXIS2_PLACEMENT_3D ( 'NONE', #227859, #113052, #71379 ) ;
#194625 = EDGE_CURVE ( 'NONE', #54224, #179202, #29807, .T. ) ;
#194626 = DIRECTION ( 'NONE',  ( -1.020425574104003999E-15, -0.8814952561688429444, 0.4721928772777345684 ) ) ;
#194627 = EDGE_CURVE ( 'NONE', #257602, #50106, #217356, .T. ) ;
#194628 = CARTESIAN_POINT ( 'NONE',  ( -12.42749937872396515, 9.370689921613768902, -51.02646512666106560 ) ) ;
#194629 = DIRECTION ( 'NONE',  ( -0.000000000000000000, 1.000000000000000000, 6.982962677686267499E-15 ) ) ;
#194630 = DIRECTION ( 'NONE',  ( 0.000000000000000000, 0.000000000000000000, 1.000000000000000000 ) ) ;
#194632 = VERTEX_POINT ( 'NONE', #151006 ) ;
#194631 = CARTESIAN_POINT ( 'NONE',  ( -16.92280123533722147, 30.02947212702651925, -234.7123078551372259 ) ) ;
#194634 = DIRECTION ( 'NONE',  ( 0.000000000000000000, -0.9887567792719341719, -0.1495327102803664099 ) ) ;
#194633 = CARTESIAN_POINT ( 'NONE',  ( 20.94999999999999929, 76.00000000001244871, -170.0231074845243597 ) ) ;
#194635 = DIRECTION ( 'NONE',  ( 0.000000000000000000, 0.000000000000000000, 1.000000000000000000 ) ) ;
#194636 = CARTESIAN_POINT ( 'NONE',  ( -23.15000000000000213, 36.65892442174935439, -249.5511627012433848 ) ) ;
#194637 = CARTESIAN_POINT ( 'NONE',  ( -19.95447128016622784, 5.488301201494659942, 16.50000000000000000 ) ) ;
#194638 = CARTESIAN_POINT ( 'NONE',  ( 23.14999999999999503, 59.16775194334852017, -221.0793150863668473 ) ) ;
#194640 = ORIENTED_EDGE ( 'NONE', *, *, #59499, .F. ) ;
#194639 = AXIS2_PLACEMENT_3D ( 'NONE', #229499, #225604, #245213 ) ;
#194641 = CIRCLE ( 'NONE', #11467, 0.1000000000000001027 ) ;
#194642 =( LENGTH_UNIT ( ) NAMED_UNIT ( * ) SI_UNIT ( .MILLI., .METRE. ) );
#194643 = DIRECTION ( 'NONE',  ( -2.557131231893037478E-16, -0.8660254037844420383, 0.4999999999999941713 ) ) ;
#194644 = EDGE_CURVE ( 'NONE', #144130, #220534, #113324, .T. ) ;
#194645 = VERTEX_POINT ( 'NONE', #133993 ) ;
#194646 = DIRECTION ( 'NONE',  ( -1.000000000000000000, 0.000000000000000000, 0.000000000000000000 ) ) ;
#194647 = EDGE_CURVE ( 'NONE', #116070, #158940, #163232, .T. ) ;
#194648 = ORIENTED_EDGE ( 'NONE', *, *, #5715, .T. ) ;
#194649 = CIRCLE ( 'NONE', #86260, 0.1000000000000028644 ) ;
#194650 = DIRECTION ( 'NONE',  ( 0.000000000000000000, 0.2617529984165031243, 0.9651348961777157509 ) ) ;
#194651 = B_SPLINE_CURVE_WITH_KNOTS ( 'NONE', 3,
 ( #127438, #226510, #29655, #208274, #47885, #28379, #166595, #12649 ),
 .UNSPECIFIED., .F., .F.,
 ( 4, 2, 2, 4 ),
 ( 0.000000000000000000, 0.0002114466876442027635, 0.0003171700314663131984, 0.0004228933752884235790 ),
 .UNSPECIFIED. ) ;
#194652 = CYLINDRICAL_SURFACE ( 'NONE', #11863, 0.09999999999999939493 ) ;
#194653 = DIRECTION ( 'NONE',  ( 1.000000000000000000, 0.000000000000000000, 0.000000000000000000 ) ) ;
#194654 = ORIENTED_EDGE ( 'NONE', *, *, #75131, .F. ) ;
#194655 = ORIENTED_EDGE ( 'NONE', *, *, #241499, .F. ) ;
#194656 = ADVANCED_FACE ( 'NONE', ( #15356 ), #213524, .F. ) ;
#194657 = EDGE_CURVE ( 'NONE', #63272, #90311, #171884, .T. ) ;
#194658 = CARTESIAN_POINT ( 'NONE',  ( 23.24999999999999289, 11.65000000001116298, -112.6500000000000341 ) ) ;
#194659 = CARTESIAN_POINT ( 'NONE',  ( -16.88705144915396517, 63.01218536341742293, -213.3988038337647595 ) ) ;
#194660 = DIRECTION ( 'NONE',  ( 0.000000000000000000, 1.224646799142057732E-16, 1.000000000000000000 ) ) ;
#194662 = CARTESIAN_POINT ( 'NONE',  ( -23.25000000000000000, 69.06610602788505560, -32.23746165015079868 ) ) ;
#194661 = FACE_OUTER_BOUND ( 'NONE', #191201, .T. ) ;
#194663 = EDGE_CURVE ( 'NONE', #213275, #87394, #88162, .T. ) ;
#194664 = CIRCLE ( 'NONE', #227958, 0.1000000000000001305 ) ;
#194665 = VECTOR ( 'NONE', #45454, 1000.000000000000000 ) ;
#194666 = DIRECTION ( 'NONE',  ( 0.000000000000000000, 0.000000000000000000, -1.000000000000000000 ) ) ;
#194668 = VECTOR ( 'NONE', #167196, 1000.000000000000000 ) ;
#194667 = SPHERICAL_SURFACE ( 'NONE', #106423, 0.1000000000000000056 ) ;
#194669 = AXIS2_PLACEMENT_3D ( 'NONE', #141990, #41642, #199431 ) ;
#194670 = CARTESIAN_POINT ( 'NONE',  ( 21.05000000000000071, 30.90801580390627734, -252.0203440857197279 ) ) ;
#194671 = ORIENTED_EDGE ( 'NONE', *, *, #112974, .T. ) ;
#194672 = CARTESIAN_POINT ( 'NONE',  ( 21.00000000000000000, 9.750000000011153745, -121.7500000000000426 ) ) ;
#194674 = ORIENTED_EDGE ( 'NONE', *, *, #252724, .T. ) ;
#194673 = DIRECTION ( 'NONE',  ( 0.000000000000000000, 0.8814952561688428334, -0.4721928772777349570 ) ) ;
#194675 = DIRECTION ( 'NONE',  ( 0.000000000000000000, -0.1332476588733448597, 0.9910827722268067408 ) ) ;
#194676 = CARTESIAN_POINT ( 'NONE',  ( 22.50000000000000000, 0.1000000000111554016, -25.70922040162662014 ) ) ;
#194678 = CARTESIAN_POINT ( 'NONE',  ( 23.14999999999999858, 5.000000000011153745, -155.5947339810869323 ) ) ;
#194677 = DIRECTION ( 'NONE',  ( 1.000000000000000000, -1.207181226542539700E-16, 2.694675058168174199E-16 ) ) ;
#194680 = ORIENTED_EDGE ( 'NONE', *, *, #5285, .T. ) ;
#194679 = DIRECTION ( 'NONE',  ( 0.000000000000000000, 0.000000000000000000, -1.000000000000000000 ) ) ;
#194682 = DIRECTION ( 'NONE',  ( 8.673617379884087537E-15, -0.2128009952263604232, 0.9770955615653316162 ) ) ;
#194681 = FACE_OUTER_BOUND ( 'NONE', #180389, .T. ) ;
#194683 = CARTESIAN_POINT ( 'NONE',  ( 20.94999999999999929, -8.999999999988842703, -158.1060308773475640 ) ) ;
#194684 = ADVANCED_FACE ( 'NONE', ( #110582 ), #91023, .T. ) ;
#194685 = FACE_OUTER_BOUND ( 'NONE', #198386, .T. ) ;
#194686 = FACE_OUTER_BOUND ( 'NONE', #246740, .T. ) ;
#194687 = CARTESIAN_POINT ( 'NONE',  ( -18.59999999999999787, 85.52395432076465909, -96.14109042769693758 ) ) ;
#194688 = ORIENTED_EDGE ( 'NONE', *, *, #94918, .T. ) ;
#194689 = CARTESIAN_POINT ( 'NONE',  ( 18.45036689428330234, -7.780508153564097640, -209.8715945982282278 ) ) ;
#194690 = VERTEX_POINT ( 'NONE', #131428 ) ;
#194691 = EDGE_CURVE ( 'NONE', #209410, #124945, #209006, .T. ) ;
#194692 = CIRCLE ( 'NONE', #28081, 0.09999999999999939493 ) ;
#194694 = AXIS2_PLACEMENT_3D ( 'NONE', #91073, #195335, #256496 ) ;
#194693 = DIRECTION ( 'NONE',  ( -1.000000000000000000, -0.000000000000000000, -0.000000000000000000 ) ) ;
#194695 = ORIENTED_EDGE ( 'NONE', *, *, #207512, .F. ) ;
#194696 = CARTESIAN_POINT ( 'NONE',  ( -23.25000000000000000, 54.92280082623103965, -239.2759596675668092 ) ) ;
#194697 = ORIENTED_EDGE ( 'NONE', *, *, #63824, .T. ) ;
#194698 = CYLINDRICAL_SURFACE ( 'NONE', #89284, 0.1000000000000028644 ) ;
#194699 = DIRECTION ( 'NONE',  ( 0.000000000000000000, 0.000000000000000000, 1.000000000000000000 ) ) ;
#194700 = ORIENTED_EDGE ( 'NONE', *, *, #3763, .F. ) ;
#194701 = CARTESIAN_POINT ( 'NONE',  ( -22.42357213249529480, -1.535990215375571788, -193.4817260165448545 ) ) ;
#194702 = DIRECTION ( 'NONE',  ( 0.000000000000000000, 0.000000000000000000, 1.000000000000000000 ) ) ;
#194703 = CARTESIAN_POINT ( 'NONE',  ( -23.15000000000000213, 1.115600667400684642E-11, -100.5000000000000426 ) ) ;
#194704 = DIRECTION ( 'NONE',  ( -1.000000000000000000, 0.000000000000000000, 0.000000000000000000 ) ) ;
#194705 = LINE ( 'NONE', #175162, #136202 ) ;
#194706 = ORIENTED_EDGE ( 'NONE', *, *, #194445, .F. ) ;
#194707 = CARTESIAN_POINT ( 'NONE',  ( -18.50000000000000000, 85.42129027953477305, -129.6992253054985156 ) ) ;
#194708 = ORIENTED_EDGE ( 'NONE', *, *, #242589, .F. ) ;
#194710 = ORIENTED_EDGE ( 'NONE', *, *, #144151, .F. ) ;
#194709 = CARTESIAN_POINT ( 'NONE',  ( 21.05000000000000071, 67.22371710471938400, -90.87310748452436826 ) ) ;
#194711 = ORIENTED_EDGE ( 'NONE', *, *, #183936, .T. ) ;
#194712 = DIRECTION ( 'NONE',  ( 1.000000000000000000, 2.952720810173289112E-16, -0.000000000000000000 ) ) ;
#194713 = CARTESIAN_POINT ( 'NONE',  ( 13.43443725621851570, 66.55344247694002036, -188.4331655301785133 ) ) ;
#194714 = DIRECTION ( 'NONE',  ( 0.000000000000000000, -0.6728971962616792091, 0.7397360091702790408 ) ) ;
#194715 = CYLINDRICAL_SURFACE ( 'NONE', #224929, 0.5000000000000009992 ) ;
#194716 = ORIENTED_EDGE ( 'NONE', *, *, #102781, .T. ) ;
#194717 = CARTESIAN_POINT ( 'NONE',  ( -16.97683809663752896, 9.950000000011140600, -147.2715247686699627 ) ) ;
#194718 = AXIS2_PLACEMENT_3D ( 'NONE', #217367, #200396, #238226 ) ;
#194719 = DIRECTION ( 'NONE',  ( -1.000000000000000000, 2.986185139342070877E-16, -6.665775143889692774E-16 ) ) ;
#194720 = VERTEX_POINT ( 'NONE', #191445 ) ;
#194722 = ORIENTED_EDGE ( 'NONE', *, *, #145789, .F. ) ;
#194721 = CARTESIAN_POINT ( 'NONE',  ( -16.86445178670701850, 66.03778837089591036, -115.6323300464067643 ) ) ;
#194723 = FACE_OUTER_BOUND ( 'NONE', #56228, .T. ) ;
#194724 = DIRECTION ( 'NONE',  ( 0.000000000000000000, 0.9651348961777158619, -0.2617529984165031243 ) ) ;
#194725 = CIRCLE ( 'NONE', #207362, 11.80000000000000604 ) ;
#194726 = CARTESIAN_POINT ( 'NONE',  ( -16.89155683852514400, 9.950000000011138823, -80.27737184954051486 ) ) ;
#194727 = CIRCLE ( 'NONE', #24022, 0.1000000000000028644 ) ;
#194728 = VERTEX_POINT ( 'NONE', #148442 ) ;
#194729 = CIRCLE ( 'NONE', #140505, 0.09999999999999986677 ) ;
#194730 = EDGE_LOOP ( 'NONE', ( #151744, #125259, #223542, #155677 ) ) ;
#194731 = CARTESIAN_POINT ( 'NONE',  ( -18.40000000000000568, 64.58541674041173053, -48.67310748452441516 ) ) ;
#194732 = ORIENTED_EDGE ( 'NONE', *, *, #56458, .F. ) ;
#194733 = DIRECTION ( 'NONE',  ( 1.000000000000000000, 0.000000000000000000, 0.000000000000000000 ) ) ;
#194734 = AXIS2_PLACEMENT_3D ( 'NONE', #174111, #154537, #12444 ) ;
#194735 = EDGE_CURVE ( 'NONE', #117471, #16854, #75746, .T. ) ;
#194736 = CARTESIAN_POINT ( 'NONE',  ( 12.26145404764308111, 66.64858632091014101, -52.54276391697543147 ) ) ;
#194737 = LINE ( 'NONE', #10951, #84360 ) ;
#194738 = EDGE_CURVE ( 'NONE', #133329, #147377, #84042, .T. ) ;
#194739 = EDGE_CURVE ( 'NONE', #235011, #85365, #229856, .T. ) ;
#194740 = VECTOR ( 'NONE', #85890, 1000.000000000000114 ) ;
#194741 = VECTOR ( 'NONE', #245792, 1000.000000000000000 ) ;
#194742 = ORIENTED_EDGE ( 'NONE', *, *, #221763, .T. ) ;
#194743 = CARTESIAN_POINT ( 'NONE',  ( 21.05000000000000071, 67.18479819544488407, -61.10256998784131355 ) ) ;
#194744 = TOROIDAL_SURFACE ( 'NONE', #236224, 0.2000000000000000111, 0.1000000000000000056 ) ;
#194745 = CIRCLE ( 'NONE', #182260, 2.100000000000002309 ) ;
#194746 = VERTEX_POINT ( 'NONE', #54457 ) ;
#194747 = CIRCLE ( 'NONE', #244594, 0.1000000000000124678 ) ;
#194748 = DIRECTION ( 'NONE',  ( 0.000000000000000000, 0.7397360091702792628, -0.6728971962616790981 ) ) ;
#194749 = ADVANCED_FACE ( 'NONE', ( #34937 ), #143783, .T. ) ;
#194750 = DIRECTION ( 'NONE',  ( 8.673617379884087537E-15, 6.982962677686266711E-15, -1.000000000000000000 ) ) ;
#194752 = ORIENTED_EDGE ( 'NONE', *, *, #257809, .F. ) ;
#194751 = CARTESIAN_POINT ( 'NONE',  ( -23.25000000000000000, 52.91185528119410009, -244.1460391050142960 ) ) ;
#194753 = DIRECTION ( 'NONE',  ( 0.000000000000000000, 0.000000000000000000, -1.000000000000000000 ) ) ;
#194755 = AXIS2_PLACEMENT_3D ( 'NONE', #103969, #124851, #123564 ) ;
#194754 = CARTESIAN_POINT ( 'NONE',  ( -18.59999999999999787, 76.00000000001126921, -203.5231074845248997 ) ) ;
#194756 = DIRECTION ( 'NONE',  ( 0.000000000000000000, -1.387778780781442141E-13, 1.000000000000000000 ) ) ;
#194757 = DIRECTION ( 'NONE',  ( 1.000000000000000000, 0.000000000000000000, 0.000000000000000000 ) ) ;
#194758 = CARTESIAN_POINT ( 'NONE',  ( 16.87683809663749557, 66.05000000001155058, -48.67310748452439384 ) ) ;
#194759 = CARTESIAN_POINT ( 'NONE',  ( -20.94999999999999929, 87.65000000001215597, -139.4231074845242802 ) ) ;
#194760 = CARTESIAN_POINT ( 'NONE',  ( 21.14250536705908345, 6.518172176891879666, -67.00000000000004263 ) ) ;
#194762 = ORIENTED_EDGE ( 'NONE', *, *, #58696, .T. ) ;
#194761 = CARTESIAN_POINT ( 'NONE',  ( -23.15000000000000213, -8.999999999988844479, -57.60603087734755690 ) ) ;
#194763 = AXIS2_PLACEMENT_3D ( 'NONE', #24594, #48927, #61121 ) ;
#194764 = CIRCLE ( 'NONE', #78206, 1.900000000000012790 ) ;
#194765 = DIRECTION ( 'NONE',  ( 1.000000000000000000, 0.000000000000000000, 0.000000000000000000 ) ) ;
#194766 = ADVANCED_FACE ( 'NONE', ( #253930 ), #19187, .F. ) ;
#194767 = EDGE_CURVE ( 'NONE', #70426, #63775, #13385, .T. ) ;
#194768 = DIRECTION ( 'NONE',  ( -0.000000000000000000, 1.000000000000000000, 6.982962677686266711E-15 ) ) ;
#194769 = DIRECTION ( 'NONE',  ( -0.000000000000000000, -0.000000000000000000, -1.000000000000000000 ) ) ;
#194770 = ORIENTED_EDGE ( 'NONE', *, *, #209584, .F. ) ;
#194771 = DIRECTION ( 'NONE',  ( 0.000000000000000000, 0.000000000000000000, 1.000000000000000000 ) ) ;
#194772 = AXIS2_PLACEMENT_3D ( 'NONE', #173450, #36475, #93846 ) ;
#194773 = DIRECTION ( 'NONE',  ( -0.7071067811865388020, 0.6909108974501111389, 0.1504730267679034728 ) ) ;
#194774 = AXIS2_PLACEMENT_3D ( 'NONE', #130389, #189095, #110829 ) ;
#194776 = EDGE_CURVE ( 'NONE', #14807, #6078, #234372, .T. ) ;
#194775 = CARTESIAN_POINT ( 'NONE',  ( -20.93284271247462058, 62.82351852614505106, -207.2177435922979214 ) ) ;
#194778 = VERTEX_POINT ( 'NONE', #256441 ) ;
#194777 = VECTOR ( 'NONE', #61857, 1000.000000000000000 ) ;
#194779 = DIRECTION ( 'NONE',  ( -4.391705002472927119E-16, -1.000000000000000000, -7.026728003956683390E-15 ) ) ;
#194781 = DIRECTION ( 'NONE',  ( 0.000000000000000000, -0.8660254037844411501, -0.4999999999999956701 ) ) ;
#194780 = VECTOR ( 'NONE', #129719, 1000.000000000000227 ) ;
#194782 = ORIENTED_EDGE ( 'NONE', *, *, #42279, .F. ) ;
#194783 = CARTESIAN_POINT ( 'NONE',  ( -18.34374000495059676, 11.47316190337362940, -124.7500000000000426 ) ) ;
#194784 = ORIENTED_EDGE ( 'NONE', *, *, #220856, .T. ) ;
#194785 = FACE_OUTER_BOUND ( 'NONE', #151161, .T. ) ;
#194787 = ORIENTED_EDGE ( 'NONE', *, *, #77577, .T. ) ;
#194786 = FACE_OUTER_BOUND ( 'NONE', #211897, .T. ) ;
#194788 = CIRCLE ( 'NONE', #3209, 0.09999999999999939493 ) ;
#194789 = DIRECTION ( 'NONE',  ( 1.000000000000000000, -7.049440681616512959E-16, 1.911869773728117674E-16 ) ) ;
#194790 = EDGE_CURVE ( 'NONE', #160984, #196419, #76586, .T. ) ;
#194791 = ORIENTED_EDGE ( 'NONE', *, *, #116492, .T. ) ;
#194792 = CARTESIAN_POINT ( 'NONE',  ( -21.05000000000000071, 1.750000000011155743, -179.1695115579016147 ) ) ;
#194793 = TOROIDAL_SURFACE ( 'NONE', #202957, 0.2000000000000000111, 0.1000000000000000056 ) ;
#194794 = VECTOR ( 'NONE', #228601, 1000.000000000000114 ) ;
#194795 = VERTEX_POINT ( 'NONE', #60869 ) ;
#194797 = EDGE_LOOP ( 'NONE', ( #241230, #59696, #149546, #244490 ) ) ;
#194796 = EDGE_LOOP ( 'NONE', ( #117909, #146793, #69588, #76465 ) ) ;
#194798 = LINE ( 'NONE', #95658, #252829 ) ;
#194799 = AXIS2_PLACEMENT_3D ( 'NONE', #193745, #93347, #209445 ) ;
#194800 = ORIENTED_EDGE ( 'NONE', *, *, #108979, .T. ) ;
#194801 = DIRECTION ( 'NONE',  ( 0.000000000000000000, -6.982962677686266711E-15, 1.000000000000000000 ) ) ;
#194802 = ORIENTED_EDGE ( 'NONE', *, *, #120076, .T. ) ;
#194803 = AXIS2_PLACEMENT_3D ( 'NONE', #128456, #191021, #50181 ) ;
#194804 = EDGE_CURVE ( 'NONE', #94515, #250601, #159151, .T. ) ;
#194805 = EDGE_CURVE ( 'NONE', #93167, #85372, #129875, .T. ) ;
#194806 = VERTEX_POINT ( 'NONE', #119591 ) ;
#194807 = DIRECTION ( 'NONE',  ( 0.000000000000000000, 0.8814952561688436106, -0.4721928772777336247 ) ) ;
#194808 = CYLINDRICAL_SURFACE ( 'NONE', #155584, 0.09999999999999939493 ) ;
#194809 = DIRECTION ( 'NONE',  ( 1.000000000000000000, 0.000000000000000000, 0.000000000000000000 ) ) ;
#194810 = EDGE_LOOP ( 'NONE', ( #157385, #129058 ) ) ;
#194811 = EDGE_CURVE ( 'NONE', #252845, #177752, #199107, .T. ) ;
#194813 = EDGE_CURVE ( 'NONE', #4251, #2708, #40068, .T. ) ;
#194812 = CYLINDRICAL_SURFACE ( 'NONE', #57801, 0.09999999999999939493 ) ;
#194814 = CARTESIAN_POINT ( 'NONE',  ( -18.51555513499570083, -9.352657054493093369, -74.19516989569670784 ) ) ;
#194815 = DIRECTION ( 'NONE',  ( 0.000000000000000000, -6.982962677686266711E-15, 1.000000000000000000 ) ) ;
#194816 = AXIS2_PLACEMENT_3D ( 'NONE', #188562, #230252, #9926 ) ;
#194817 = EDGE_LOOP ( 'NONE', ( #252754, #44468, #242671, #159125 ) ) ;
#194818 = CARTESIAN_POINT ( 'NONE',  ( 21.05000000000000071, 64.40000000001145963, -42.95131071479990936 ) ) ;
#194819 = CARTESIAN_POINT ( 'NONE',  ( -18.46154800491024517, 38.05094987613883717, -261.0515204261999997 ) ) ;
#194820 = DIRECTION ( 'NONE',  ( 0.000000000000000000, -0.2617529984165031243, -0.9651348961777157509 ) ) ;
#194821 = ORIENTED_EDGE ( 'NONE', *, *, #87285, .T. ) ;
#194822 = CARTESIAN_POINT ( 'NONE',  ( 23.15000000000000213, 86.43238724539048690, -209.5644480942280836 ) ) ;
#194823 = ORIENTED_EDGE ( 'NONE', *, *, #77629, .T. ) ;
#194825 = VERTEX_POINT ( 'NONE', #59556 ) ;
#194824 = CIRCLE ( 'NONE', #207294, 0.09999999999999939493 ) ;
#194826 = EDGE_CURVE ( 'NONE', #17340, #110197, #146615, .T. ) ;
#194827 = EDGE_CURVE ( 'NONE', #89589, #146074, #150740, .T. ) ;
#194828 = FACE_OUTER_BOUND ( 'NONE', #112670, .T. ) ;
#194829 = EDGE_LOOP ( 'NONE', ( #93996, #42707, #29033 ) ) ;
#194830 = ORIENTED_EDGE ( 'NONE', *, *, #148267, .T. ) ;
#194831 = CARTESIAN_POINT ( 'NONE',  ( -22.49806830649814415, 11.36657099087203093, -198.4452018475131183 ) ) ;
#194832 = CARTESIAN_POINT ( 'NONE',  ( -21.05000000000000071, 76.00000000001192291, -98.72310748452436258 ) ) ;
#194833 = ORIENTED_EDGE ( 'NONE', *, *, #100567, .F. ) ;
#194834 = EDGE_CURVE ( 'NONE', #158368, #189878, #97402, .T. ) ;
#194835 = VERTEX_POINT ( 'NONE', #41345 ) ;
#194836 = LINE ( 'NONE', #215640, #93855 ) ;
#194837 = DIRECTION ( 'NONE',  ( 0.000000000000000000, -0.01562499999999307672, 0.9998779222360100194 ) ) ;
#194838 = ORIENTED_EDGE ( 'NONE', *, *, #83795, .T. ) ;
#194839 = EDGE_CURVE ( 'NONE', #193873, #245180, #120885, .T. ) ;
#194840 = AXIS2_PLACEMENT_3D ( 'NONE', #96117, #135246, #41326 ) ;
#194841 = ADVANCED_FACE ( 'NONE', ( #196532 ), #75344, .F. ) ;
#194842 = CIRCLE ( 'NONE', #136535, 12.87499999999999822 ) ;
#194843 = EDGE_CURVE ( 'NONE', #173155, #121523, #34081, .T. ) ;
#194844 = VERTEX_POINT ( 'NONE', #96136 ) ;
#194845 = FACE_OUTER_BOUND ( 'NONE', #155475, .T. ) ;
#194846 = ADVANCED_FACE ( 'NONE', ( #200395 ), #138252, .T. ) ;
#194847 = CARTESIAN_POINT ( 'NONE',  ( -20.94999999999999929, 11.65000000001115232, -134.0000000000000284 ) ) ;
#194848 = DIRECTION ( 'NONE',  ( -1.000000000000000000, -0.000000000000000000, -0.000000000000000000 ) ) ;
#194849 = DIRECTION ( 'NONE',  ( -1.000000000000000000, -0.000000000000000000, -0.000000000000000000 ) ) ;
#194850 = EDGE_CURVE ( 'NONE', #225971, #81417, #204896, .T. ) ;
#194851 = CARTESIAN_POINT ( 'NONE',  ( 20.94999999999999929, 70.15000000001163016, -59.39061026024639034 ) ) ;
#194852 = CARTESIAN_POINT ( 'NONE',  ( -22.48970261584618058, 11.65000000001115588, -66.94463051178263413 ) ) ;
#194855 = LINE ( 'NONE', #16218, #145190 ) ;
#194854 = AXIS2_PLACEMENT_3D ( 'NONE', #72903, #194124, #152438 ) ;
#194853 = CARTESIAN_POINT ( 'NONE',  ( 21.05000000000000426, 75.94851711812962947, -75.82328730243888515 ) ) ;
#194856 = DIRECTION ( 'NONE',  ( -0.7070776581709311559, 0.000000000000000000, 0.7071359030027479786 ) ) ;
#194858 = EDGE_CURVE ( 'NONE', #213687, #20901, #200636, .T. ) ;
#194857 = CARTESIAN_POINT ( 'NONE',  ( -16.87998658237769334, 23.16638972503378469, -231.0359424933138541 ) ) ;
#194859 = AXIS2_PLACEMENT_3D ( 'NONE', #170026, #31788, #8348 ) ;
#194860 = DIRECTION ( 'NONE',  ( 2.952720810173289605E-16, -0.4721928772777352346, -0.8814952561688427224 ) ) ;
#194861 = ORIENTED_EDGE ( 'NONE', *, *, #95128, .F. ) ;
#194863 = ORIENTED_EDGE ( 'NONE', *, *, #82690, .T. ) ;
#194862 = DIRECTION ( 'NONE',  ( 1.000000000000000000, 0.000000000000000000, 0.000000000000000000 ) ) ;
#194864 = EDGE_CURVE ( 'NONE', #104969, #161165, #21571, .T. ) ;
#194865 =( BOUNDED_CURVE ( )  B_SPLINE_CURVE ( 3, ( #104223, #106797, #243751, #143363 ),
 .UNSPECIFIED., .F., .T. ) 
 B_SPLINE_CURVE_WITH_KNOTS ( ( 4, 4 ),
 ( 3.141592653589791784, 4.712388980384688786 ),
 .UNSPECIFIED. ) 
 CURVE ( )  GEOMETRIC_REPRESENTATION_ITEM ( )  RATIONAL_B_SPLINE_CURVE ( ( 1.000000000000000000, 0.8047378541243649375, 0.8047378541243649375, 1.000000000000000000 ) ) 
 REPRESENTATION_ITEM ( '' )  );
#194866 = FACE_OUTER_BOUND ( 'NONE', #116141, .T. ) ;
#194867 = DIRECTION ( 'NONE',  ( 0.000000000000000000, 0.1350103645451807555, 0.9908441862701609093 ) ) ;
#194868 = EDGE_LOOP ( 'NONE', ( #209841, #166108, #150338, #230657 ) ) ;
#194869 = DIRECTION ( 'NONE',  ( 1.000000000000000000, 0.000000000000000000, 0.000000000000000000 ) ) ;
#194870 = AXIS2_PLACEMENT_3D ( 'NONE', #188790, #67562, #209643 ) ;
#194871 = CARTESIAN_POINT ( 'NONE',  ( 22.50000000000000000, 76.00000000001165290, -69.52310748452431710 ) ) ;
#194872 = ORIENTED_EDGE ( 'NONE', *, *, #218514, .T. ) ;
#194873 = AXIS2_PLACEMENT_3D ( 'NONE', #210205, #147648, #27741 ) ;
#194874 = AXIS2_PLACEMENT_3D ( 'NONE', #180494, #42950, #66363 ) ;
#194875 = CARTESIAN_POINT ( 'NONE',  ( 21.07888907270776002, 60.07907005675570389, -221.2527070780202223 ) ) ;
#194876 = LINE ( 'NONE', #16246, #138058 ) ;
#194877 =( BOUNDED_SURFACE ( )  B_SPLINE_SURFACE ( 3, 2, ( 
 ( #144689, #127718, #26055 ),
 ( #106844, #5158, #228107 ),
 ( #48161, #187702, #104270 ),
 ( #164280, #63884, #27369 ),
 ( #247655, #66451, #9043 ),
 ( #163004, #246375, #147267 ),
 ( #148563, #7772, #207266 ),
 ( #145975, #224230, #225494 ) ),
 .UNSPECIFIED., .F., .F., .F. ) 
 B_SPLINE_SURFACE_WITH_KNOTS ( ( 4, 2, 2, 4 ),
 ( 3, 3 ),
 ( 0.0001704874539069911317, 0.0003809798300636645443, 0.0004862260181420012778, 0.0005914722062203380112 ),
 ( 0.000000000000000000, 1.000000000000000000 ),
 .UNSPECIFIED. ) 
 GEOMETRIC_REPRESENTATION_ITEM ( )  RATIONAL_B_SPLINE_SURFACE ( (
 ( 1.000000000000000000, 0.7071067811864850672, 1.000000000000000000),
 ( 1.000000000000000000, 0.7670648383575194851, 1.000000000000000000),
 ( 1.000000000000000000, 0.8204820770253823392, 1.000000000000000000),
 ( 1.000000000000000000, 0.8877218296113124074, 1.000000000000000000),
 ( 1.000000000000000000, 0.9080815932665092793, 1.000000000000000000),
 ( 1.000000000000000000, 0.9395541505861816356, 1.000000000000000000),
 ( 1.000000000000000000, 0.9506520335379058384, 1.000000000000000000),
 ( 1.000000000000000000, 0.9504532311154573199, 1.000000000000000000) ) ) 
 REPRESENTATION_ITEM ( '' )  SURFACE ( )  );
#194878 = DIRECTION ( 'NONE',  ( -1.000000000000000000, 0.000000000000000000, 0.000000000000000000 ) ) ;
#194880 = ORIENTED_EDGE ( 'NONE', *, *, #101358, .F. ) ;
#194879 = DIRECTION ( 'NONE',  ( -1.000000000000000000, 0.000000000000000000, 0.000000000000000000 ) ) ;
#194881 = AXIS2_PLACEMENT_3D ( 'NONE', #100930, #196225, #159686 ) ;
#194883 = ORIENTED_EDGE ( 'NONE', *, *, #109456, .F. ) ;
#194882 = CARTESIAN_POINT ( 'NONE',  ( -18.50000000000000000, 85.40000000001187175, -96.14106563635156988 ) ) ;
#194884 = FACE_OUTER_BOUND ( 'NONE', #177187, .T. ) ;
#194885 = CARTESIAN_POINT ( 'NONE',  ( -20.64999999999999858, 4.250000000011156409, -155.1500000000000057 ) ) ;
#194886 = CARTESIAN_POINT ( 'NONE',  ( 18.59999999999999787, 74.14897176987119565, -124.8691942151018139 ) ) ;
#194887 = DIRECTION ( 'NONE',  ( 0.000000000000000000, -1.000000000000000000, 0.000000000000000000 ) ) ;
#194888 = EDGE_CURVE ( 'NONE', #215605, #219055, #45164, .T. ) ;
#194890 = CARTESIAN_POINT ( 'NONE',  ( -21.14999999999999858, 69.45934304831041572, -69.42310748452437963 ) ) ;
#194889 = CARTESIAN_POINT ( 'NONE',  ( -16.77431908686106610, 9.945805754529134290, -154.8358392176502605 ) ) ;
#194891 = PLANE ( 'NONE',  #57914 ) ;
#194892 = CARTESIAN_POINT ( 'NONE',  ( -21.12844524849339223, 64.25000000001233502, -163.1186940136820169 ) ) ;
#194893 = DIRECTION ( 'NONE',  ( 1.000000000000000000, 0.000000000000000000, 0.000000000000000000 ) ) ;
#194894 = CIRCLE ( 'NONE', #257348, 0.1000000000000028644 ) ;
#194895 = CIRCLE ( 'NONE', #157501, 14.20833333333335347 ) ;
#194896 = EDGE_CURVE ( 'NONE', #92332, #162858, #79972, .T. ) ;
#194897 = CARTESIAN_POINT ( 'NONE',  ( 21.30000000000002558, 1.115600667400684642E-11, -100.5000000000000284 ) ) ;
#194898 = VECTOR ( 'NONE', #128644, 1000.000000000000000 ) ;
#194899 =( BOUNDED_SURFACE ( )  B_SPLINE_SURFACE ( 3, 2, ( 
 ( #95815, #175408, #254851 ),
 ( #76265, #155837, #197498 ),
 ( #18863, #38434, #196217 ),
 ( #235337, #198783, #136216 ),
 ( #179255, #215769, #177960 ),
 ( #37171, #17571, #257418 ),
 ( #78820, #158417, #237913 ),
 ( #20168, #224761, #87808 ),
 ( #241762, #186965, #166129 ),
 ( #46131, #164810, #203925 ) ),
 .UNSPECIFIED., .F., .F., .F. ) 
 B_SPLINE_SURFACE_WITH_KNOTS ( ( 4, 2, 2, 2, 4 ),
 ( 3, 3 ),
 ( 0.002161241639767785133, 0.002579950749617447234, 0.002789305304542278284, 0.002893982582004694243, 0.002998659859467109768 ),
 ( 0.000000000000000000, 1.000000000000000000 ),
 .UNSPECIFIED. ) 
 GEOMETRIC_REPRESENTATION_ITEM ( )  RATIONAL_B_SPLINE_SURFACE ( (
 ( 1.000000000000000000, 0.7071067811864985009, 1.000000000000000000),
 ( 1.000000000000000000, 0.7632447400663817660, 1.000000000000000000),
 ( 1.000000000000000000, 0.8158073005109720555, 1.000000000000000000),
 ( 1.000000000000000000, 0.8906973462395535446, 1.000000000000000000),
 ( 1.000000000000000000, 0.9149408947797941227, 1.000000000000000000),
 ( 1.000000000000000000, 0.9493368785276861122, 1.000000000000000000),
 ( 1.000000000000000000, 0.9605194247156072507, 1.000000000000000000),
 ( 1.000000000000000000, 0.9803630264781721948, 1.000000000000000000),
 ( 1.000000000000000000, 0.9900844824270734756, 1.000000000000000000),
 ( 1.000000000000000000, 0.9894588281429241849, 1.000000000000000000) ) ) 
 REPRESENTATION_ITEM ( '' )  SURFACE ( )  );
#194900 = EDGE_LOOP ( 'NONE', ( #161214, #13064, #31953, #125655 ) ) ;
#194901 = DIRECTION ( 'NONE',  ( -0.7071067811865475727, 0.7071067811865475727, 4.937700262164531476E-15 ) ) ;
#194902 = AXIS2_PLACEMENT_3D ( 'NONE', #242942, #241668, #223371 ) ;
#194903 = VERTEX_POINT ( 'NONE', #81684 ) ;
#194904 = ORIENTED_EDGE ( 'NONE', *, *, #40055, .T. ) ;
#194905 = EDGE_CURVE ( 'NONE', #166406, #69945, #42601, .T. ) ;
#194906 = DIRECTION ( 'NONE',  ( 0.000000000000000000, 0.2617529984165036239, 0.9651348961777156399 ) ) ;
#194907 = ADVANCED_FACE ( 'NONE', ( #63435 ), #103834, .F. ) ;
#194908 = DIRECTION ( 'NONE',  ( -0.000000000000000000, 0.2617529984165037349, 0.9651348961777156399 ) ) ;
#194909 = ORIENTED_EDGE ( 'NONE', *, *, #60456, .F. ) ;
#194910 = ORIENTED_EDGE ( 'NONE', *, *, #41752, .F. ) ;
#194911 = CARTESIAN_POINT ( 'NONE',  ( 23.24999999999999289, 2.319530388122574394, -217.8268657444419887 ) ) ;
#194912 =( NAMED_UNIT ( * ) SI_UNIT ( $, .STERADIAN. ) SOLID_ANGLE_UNIT ( ) );
#194913 = AXIS2_PLACEMENT_3D ( 'NONE', #24380, #239560, #59599 ) ;
#194914 = ORIENTED_EDGE ( 'NONE', *, *, #255904, .F. ) ;
#194915 = AXIS2_PLACEMENT_3D ( 'NONE', #115265, #18732, #96946 ) ;
#194916 = ORIENTED_EDGE ( 'NONE', *, *, #179273, .F. ) ;
#194918 = CARTESIAN_POINT ( 'NONE',  ( -23.15000000000000213, -11.64999999998884483, -97.40000000000004832 ) ) ;
#194917 = AXIS2_PLACEMENT_3D ( 'NONE', #2387, #25833, #81906 ) ;
#194919 = CARTESIAN_POINT ( 'NONE',  ( -16.77902162784673834, 66.05358074280371738, -56.86111624045504698 ) ) ;
#194920 = VECTOR ( 'NONE', #255837, 1000.000000000000227 ) ;
#194921 = FACE_OUTER_BOUND ( 'NONE', #52689, .T. ) ;
#194922 = CARTESIAN_POINT ( 'NONE',  ( 12.24999999999999822, 9.349999999999983658, -16.52151937182509656 ) ) ;
#194923 = CARTESIAN_POINT ( 'NONE',  ( 21.14999999999999858, 65.51923798433685420, -242.1677427744926092 ) ) ;
#194924 = CARTESIAN_POINT ( 'NONE',  ( 21.04999999999999361, 75.90156250001187743, -142.8223383946165370 ) ) ;
#194925 = ORIENTED_EDGE ( 'NONE', *, *, #163175, .F. ) ;
#194927 = DIRECTION ( 'NONE',  ( 0.000000000000000000, 1.000000000000000000, 0.000000000000000000 ) ) ;
#194926 = CARTESIAN_POINT ( 'NONE',  ( -23.15000000000000213, 76.00000000001126921, -203.5231074845248997 ) ) ;
#194928 = AXIS2_PLACEMENT_3D ( 'NONE', #73887, #76399, #33486 ) ;
#194930 = B_SPLINE_CURVE_WITH_KNOTS ( 'NONE', 3,
 ( #174896, #58714, #238664, #237383, #18330, #1316, #118736, #217791, #37921, #255604 ),
 .UNSPECIFIED., .F., .F.,
 ( 4, 3, 3, 4 ),
 ( 0.000000000000000000, 3.394313611810855516E-05, 6.779740500699835842E-05, 0.0001049857339142647140 ),
 .UNSPECIFIED. ) ;
#194929 = LINE ( 'NONE', #32009, #123984 ) ;
#194931 = ORIENTED_EDGE ( 'NONE', *, *, #163455, .T. ) ;
#194932 = CYLINDRICAL_SURFACE ( 'NONE', #185410, 0.1000000000000028644 ) ;
#194933 = DIRECTION ( 'NONE',  ( 0.000000000000000000, 0.000000000000000000, 1.000000000000000000 ) ) ;
#194934 = EDGE_LOOP ( 'NONE', ( #55550, #10155, #56247, #193222, #118932, #170699, #228345, #32045 ) ) ;
#194935 = CARTESIAN_POINT ( 'NONE',  ( -23.25000000000000000, -8.777002227904194598, -238.5420042644097975 ) ) ;
#194936 = CARTESIAN_POINT ( 'NONE',  ( 22.50000000000000000, 67.23127455305841238, -235.8551265064783991 ) ) ;
#194937 = EDGE_CURVE ( 'NONE', #181381, #26762, #42404, .T. ) ;
#194938 = CARTESIAN_POINT ( 'NONE',  ( -22.59080734064477625, 64.25000000001269029, -203.5538571926214502 ) ) ;
#194939 = AXIS2_PLACEMENT_3D ( 'NONE', #213431, #169219, #93485 ) ;
#194941 = ORIENTED_EDGE ( 'NONE', *, *, #113348, .F. ) ;
#194940 = AXIS2_PLACEMENT_3D ( 'NONE', #47385, #124387, #203906 ) ;
#194942 = ORIENTED_EDGE ( 'NONE', *, *, #42173, .T. ) ;
#194943 = FACE_OUTER_BOUND ( 'NONE', #237947, .T. ) ;
#194944 = DIRECTION ( 'NONE',  ( 1.000000000000000000, 0.000000000000000000, 0.000000000000000000 ) ) ;
#194945 = LINE ( 'NONE', #197479, #7288 ) ;
#194946 = CARTESIAN_POINT ( 'NONE',  ( -15.55912972643741199, 67.50912972645004118, -190.8731074845244109 ) ) ;
#194947 = ORIENTED_EDGE ( 'NONE', *, *, #18965, .T. ) ;
#194948 = EDGE_CURVE ( 'NONE', #146851, #136568, #64727, .T. ) ;
#194949 = CARTESIAN_POINT ( 'NONE',  ( 12.25000000000000178, 47.91396133265956792, -234.2636761031308197 ) ) ;
#194950 = CIRCLE ( 'NONE', #94967, 0.2000000000000111688 ) ;
#194951 = DIRECTION ( 'NONE',  ( 0.000000000000000000, 0.9654727137038715545, -0.2605042016806676242 ) ) ;
#194952 = EDGE_CURVE ( 'NONE', #76927, #194221, #67295, .T. ) ;
#194953 = AXIS2_PLACEMENT_3D ( 'NONE', #76837, #73034, #16889 ) ;
#194954 = CARTESIAN_POINT ( 'NONE',  ( 22.16821283564876666, 7.558973340791918183, -167.4999999999999716 ) ) ;
#194955 = CARTESIAN_POINT ( 'NONE',  ( 23.25000000000000000, 85.60000000001174669, -81.27310748452424605 ) ) ;
#194956 = AXIS2_PLACEMENT_3D ( 'NONE', #202342, #23740, #103219 ) ;
#194957 = CARTESIAN_POINT ( 'NONE',  ( -18.42637059832565427, -9.496945461878542716, -207.6090773097997726 ) ) ;
#194958 = AXIS2_PLACEMENT_3D ( 'NONE', #172440, #91577, #14630 ) ;
#194959 = EDGE_CURVE ( 'NONE', #120793, #216320, #113517, .T. ) ;
#194961 = ORIENTED_EDGE ( 'NONE', *, *, #200044, .F. ) ;
#194960 = CARTESIAN_POINT ( 'NONE',  ( -16.93433913041102912, 65.99402157848787454, -82.08774205712920491 ) ) ;
#194962 = CARTESIAN_POINT ( 'NONE',  ( 18.39999999999999503, 11.75000000001113953, -124.7500000000000426 ) ) ;
#194963 = LINE ( 'NONE', #149421, #24471 ) ;
#194964 = DIRECTION ( 'NONE',  ( -0.000000000000000000, 0.1686199900910312910, -0.9856811345164826488 ) ) ;
#194965 = DIRECTION ( 'NONE',  ( 0.000000000000000000, 0.000000000000000000, -1.000000000000000000 ) ) ;
#194966 = CARTESIAN_POINT ( 'NONE',  ( -23.15000000000000213, 11.65000000001115588, -45.65000000000000568 ) ) ;
#194967 = EDGE_CURVE ( 'NONE', #41483, #208529, #142956, .T. ) ;
#194969 = ORIENTED_EDGE ( 'NONE', *, *, #254264, .F. ) ;
#194968 = LINE ( 'NONE', #16331, #23593 ) ;
#194970 = FACE_OUTER_BOUND ( 'NONE', #14073, .T. ) ;
#194971 = AXIS2_PLACEMENT_3D ( 'NONE', #146244, #223375, #44763 ) ;
#194972 = EDGE_CURVE ( 'NONE', #123343, #56714, #216658, .T. ) ;
#194973 = CARTESIAN_POINT ( 'NONE',  ( -20.00857864376270001, 9.350000000011156942, -155.1500000000000057 ) ) ;
#194974 = CYLINDRICAL_SURFACE ( 'NONE', #211261, 0.09999999999999939493 ) ;
#194975 = ORIENTED_EDGE ( 'NONE', *, *, #34309, .F. ) ;
#194976 = DIRECTION ( 'NONE',  ( 0.000000000000000000, 0.9999631594459058581, 0.008583690987093516023 ) ) ;
#194977 = SPHERICAL_SURFACE ( 'NONE', #252574, 0.1000000000000000056 ) ;
#194978 = FACE_OUTER_BOUND ( 'NONE', #89521, .T. ) ;
#194979 = AXIS2_PLACEMENT_3D ( 'NONE', #77837, #235629, #193962 ) ;
#194980 = FACE_OUTER_BOUND ( 'NONE', #46177, .T. ) ;
#194981 = EDGE_CURVE ( 'NONE', #68824, #248715, #121721, .T. ) ;
#194982 = CIRCLE ( 'NONE', #153303, 0.9000000000000014655 ) ;
#194983 = CARTESIAN_POINT ( 'NONE',  ( -18.47079683080326262, 78.23347366783373502, -231.4733536058482173 ) ) ;
#194984 = CIRCLE ( 'NONE', #220091, 0.5000000000000004441 ) ;
#194985 = DIRECTION ( 'NONE',  ( 1.000000000000000000, 0.000000000000000000, 0.000000000000000000 ) ) ;
#194986 = ORIENTED_EDGE ( 'NONE', *, *, #253019, .T. ) ;
#194987 = ORIENTED_EDGE ( 'NONE', *, *, #236842, .F. ) ;
#194988 = CARTESIAN_POINT ( 'NONE',  ( -18.35663730107557257, 64.52609257350111704, -160.7731074845244450 ) ) ;
#194989 = FACE_OUTER_BOUND ( 'NONE', #244724, .T. ) ;
#194990 = EDGE_CURVE ( 'NONE', #249019, #155941, #167514, .T. ) ;
#194991 = CARTESIAN_POINT ( 'NONE',  ( 18.50000000000000000, -0.5913595841389442942, -242.4574432119242999 ) ) ;
#194992 = DIRECTION ( 'NONE',  ( -0.000000000000000000, -0.000000000000000000, 1.000000000000000000 ) ) ;
#194993 = CARTESIAN_POINT ( 'NONE',  ( 20.94999999999999929, 18.44490481964982465, -236.9051382908829169 ) ) ;
#194994 = AXIS2_PLACEMENT_3D ( 'NONE', #80805, #61271, #121286 ) ;
#194995 = CARTESIAN_POINT ( 'NONE',  ( 20.94999999999999929, 82.48249193998721296, -215.5326005316167084 ) ) ;
#194996 = CARTESIAN_POINT ( 'NONE',  ( -16.93906926870270624, 10.01214687095770906, -113.0534523072268485 ) ) ;
#194997 = B_SPLINE_CURVE_WITH_KNOTS ( 'NONE', 3,
 ( #231428, #31954, #115308, #129741, #133587, #191030, #252245, #194875, #250952, #90598, #214406, #14948, #175322, #91893, #51459, #72359 ),
 .UNSPECIFIED., .F., .F.,
 ( 4, 3, 3, 3, 3, 4 ),
 ( 0.000000000000000000, 3.357088238233777529E-05, 6.714213034887866539E-05, 0.0001007408646121051249, 0.0001343627955914316685, 0.0001573956632896109326 ),
 .UNSPECIFIED. ) ;
#194998 = CIRCLE ( 'NONE', #65799, 0.1000000000000028644 ) ;
#194999 = FACE_OUTER_BOUND ( 'NONE', #148394, .T. ) ;
#195000 = ORIENTED_EDGE ( 'NONE', *, *, #31392, .F. ) ;
#195001 = DIRECTION ( 'NONE',  ( 0.000000000000000000, -1.000000000000000000, -6.982962677686266711E-15 ) ) ;
#195002 = ORIENTED_EDGE ( 'NONE', *, *, #33233, .F. ) ;
#195003 = EDGE_LOOP ( 'NONE', ( #127768, #47946, #66714, #198864 ) ) ;
#195004 = PLANE ( 'NONE',  #29866 ) ;
#195005 = FACE_OUTER_BOUND ( 'NONE', #11314, .T. ) ;
#195006 = PLANE ( 'NONE',  #45701 ) ;
#195008 = ORIENTED_EDGE ( 'NONE', *, *, #19256, .F. ) ;
#195007 = DIRECTION ( 'NONE',  ( 0.000000000000000000, 0.000000000000000000, -1.000000000000000000 ) ) ;
#195009 = DIRECTION ( 'NONE',  ( 3.469446951953635015E-14, 6.982962677686266711E-15, -1.000000000000000000 ) ) ;
#195010 = LINE ( 'NONE', #256174, #156259 ) ;
#195011 = CARTESIAN_POINT ( 'NONE',  ( 20.94999999999999574, 1.835341550235567887, -78.55515129256303908 ) ) ;
#195012 = ORIENTED_EDGE ( 'NONE', *, *, #170777, .F. ) ;
#195013 = CARTESIAN_POINT ( 'NONE',  ( -18.40000000000000213, 64.25000000001230660, -157.3731074845244393 ) ) ;
#195014 = DIRECTION ( 'NONE',  ( 2.952720810173289112E-16, 1.000000000000000000, 6.982962677686266711E-15 ) ) ;
#195015 = CARTESIAN_POINT ( 'NONE',  ( 11.60000000000006004, 67.72071067812984779, -21.02310748452479316 ) ) ;
#195016 = CIRCLE ( 'NONE', #153347, 0.1000000000000124678 ) ;
#195017 = AXIS2_PLACEMENT_3D ( 'NONE', #141071, #241455, #221854 ) ;
#195018 = AXIS2_PLACEMENT_3D ( 'NONE', #82840, #162441, #239397 ) ;
#195019 = CIRCLE ( 'NONE', #232445, 11.80000000000000426 ) ;
#195020 = EDGE_CURVE ( 'NONE', #95981, #168864, #84234, .T. ) ;
#195021 = ORIENTED_EDGE ( 'NONE', *, *, #213948, .T. ) ;
#195022 = DIRECTION ( 'NONE',  ( -1.000000000000000000, 0.000000000000000000, 0.000000000000000000 ) ) ;
#195023 = DIRECTION ( 'NONE',  ( 1.000000000000000000, -0.000000000000000000, -0.000000000000000000 ) ) ;
#195024 = ORIENTED_EDGE ( 'NONE', *, *, #237643, .T. ) ;
#195025 = CARTESIAN_POINT ( 'NONE',  ( 21.08621493067296626, 6.349294291182826733, -133.9438051605239082 ) ) ;
#195026 = EDGE_CURVE ( 'NONE', #207287, #182252, #88355, .T. ) ;
#195027 = CARTESIAN_POINT ( 'NONE',  ( -18.50000000000000000, 1.115600667400684642E-11, -100.5000000000000426 ) ) ;
#195028 = CARTESIAN_POINT ( 'NONE',  ( -22.39999999999999858, 65.09550114356427741, -243.3481044654562879 ) ) ;
#195029 = EDGE_CURVE ( 'NONE', #218226, #20649, #234117, .T. ) ;
#195030 = ORIENTED_EDGE ( 'NONE', *, *, #253638, .T. ) ;
#195031 = AXIS2_PLACEMENT_3D ( 'NONE', #249484, #152976, #150385 ) ;
#195033 = ADVANCED_FACE ( 'NONE', ( #149426 ), #110266, .F. ) ;
#195032 = LINE ( 'NONE', #92051, #129637 ) ;
#195034 = DIRECTION ( 'NONE',  ( 0.000000000000000000, 0.8814952561688430555, -0.4721928772777346239 ) ) ;
#195035 = TOROIDAL_SURFACE ( 'NONE', #20242, 4.100000000000000533, 0.1000000000000000056 ) ;
#195036 = ORIENTED_EDGE ( 'NONE', *, *, #87118, .F. ) ;
#195037 = CIRCLE ( 'NONE', #124299, 12.77500000000000036 ) ;
#195038 = ORIENTED_EDGE ( 'NONE', *, *, #58547, .T. ) ;
#195039 = CARTESIAN_POINT ( 'NONE',  ( -16.86337532320261090, 9.979967204235514089, -87.94892446898285243 ) ) ;
#195040 = EDGE_CURVE ( 'NONE', #152492, #209282, #250860, .T. ) ;
#195041 = DIRECTION ( 'NONE',  ( -1.000000000000000000, -0.000000000000000000, -0.000000000000000000 ) ) ;
#195043 = ORIENTED_EDGE ( 'NONE', *, *, #165912, .T. ) ;
#195042 = DIRECTION ( 'NONE',  ( 1.000000000000000000, 0.000000000000000000, 0.000000000000000000 ) ) ;
#195044 = CARTESIAN_POINT ( 'NONE',  ( -20.94999999999999929, -11.48912529306489994, -63.89999999999999858 ) ) ;
#195045 = CARTESIAN_POINT ( 'NONE',  ( 18.49999999999999289, 10.20857864377385127, -125.1500000000000341 ) ) ;
#195046 = ADVANCED_FACE ( 'NONE', ( #169011 ), #69890, .T. ) ;
#195047 = CARTESIAN_POINT ( 'NONE',  ( -20.93975676684922504, 65.68895814178263493, -131.0026557862138645 ) ) ;
#195048 = DIRECTION ( 'NONE',  ( 0.000000000000000000, 0.2128009952263605342, -0.9770955615653315052 ) ) ;
#195049 = DIRECTION ( 'NONE',  ( 1.000000000000000000, 0.000000000000000000, 0.000000000000000000 ) ) ;
#195050 = LINE ( 'NONE', #153381, #5538 ) ;
#195051 = FACE_OUTER_BOUND ( 'NONE', #93374, .T. ) ;
#195053 = ORIENTED_EDGE ( 'NONE', *, *, #152057, .T. ) ;
#195052 = CARTESIAN_POINT ( 'NONE',  ( 18.79999999999999716, 1.885425182446133885, -11.49641995933507843 ) ) ;
#195056 = ORIENTED_EDGE ( 'NONE', *, *, #101141, .T. ) ;
#195055 = CARTESIAN_POINT ( 'NONE',  ( 20.89999999999999503, 8.000000000000000000, -1.212568896937008089 ) ) ;
#195054 = PRODUCT_DEFINITION ( 'UNKNOWN', '', #236198, #113224 ) ;
#195058 = CARTESIAN_POINT ( 'NONE',  ( 20.84999999999998721, 10.33248238083634440, -72.59484654391314962 ) ) ;
#195057 = DIRECTION ( 'NONE',  ( 0.000000000000000000, 0.5000000000000144329, 0.8660254037844302699 ) ) ;
#195060 = ORIENTED_EDGE ( 'NONE', *, *, #25886, .T. ) ;
#195059 = DIRECTION ( 'NONE',  ( 0.000000000000000000, 0.000000000000000000, 1.000000000000000000 ) ) ;
#195061 = AXIS2_PLACEMENT_3D ( 'NONE', #122411, #84508, #204492 ) ;
#195062 = ORIENTED_EDGE ( 'NONE', *, *, #216663, .F. ) ;
#195063 = DIRECTION ( 'NONE',  ( 2.259780016855445309E-14, 0.9875055080513753802, -0.1575844902526748192 ) ) ;
#195065 = DIRECTION ( 'NONE',  ( 0.000000000000000000, 1.000000000000000000, 0.000000000000000000 ) ) ;
#195064 = CIRCLE ( 'NONE', #128405, 0.09999999999998902822 ) ;
#195066 = VECTOR ( 'NONE', #46777, 1000.000000000000000 ) ;
#195068 = EDGE_CURVE ( 'NONE', #74473, #202477, #34431, .T. ) ;
#195067 = CARTESIAN_POINT ( 'NONE',  ( -18.59999999999999787, 77.86671491006887891, -57.77043223824230722 ) ) ;
#195069 = CARTESIAN_POINT ( 'NONE',  ( 19.90621891164687440, 11.75000000001116263, -58.32844527787765543 ) ) ;
#195070 = EDGE_CURVE ( 'NONE', #247452, #66961, #150930, .T. ) ;
#195071 = EDGE_CURVE ( 'NONE', #244761, #97109, #200822, .T. ) ;
#195073 = DIRECTION ( 'NONE',  ( 0.000000000000000000, 0.9651348961777379554, -0.2617529984164210233 ) ) ;
#195072 = CIRCLE ( 'NONE', #161762, 0.09999999999999939493 ) ;
#195074 = CARTESIAN_POINT ( 'NONE',  ( 20.94999999999999929, 87.19425987394825484, -209.6674621343692024 ) ) ;
#195075 = CARTESIAN_POINT ( 'NONE',  ( -18.50000000000000000, -1.835341550213255957, -78.55515129256302487 ) ) ;
#195076 = VERTEX_POINT ( 'NONE', #153295 ) ;
#195077 = VERTEX_POINT ( 'NONE', #107704 ) ;
#195078 = CARTESIAN_POINT ( 'NONE',  ( 21.07954640115310596, 30.85578282560233987, -252.0785699441653946 ) ) ;
#195079 = EDGE_CURVE ( 'NONE', #161999, #245009, #132415, .T. ) ;
#195080 = AXIS2_PLACEMENT_3D ( 'NONE', #202280, #101863, #2771 ) ;
#195081 = ORIENTED_EDGE ( 'NONE', *, *, #69706, .F. ) ;
#195082 = DIRECTION ( 'NONE',  ( -1.000000000000000000, 0.000000000000000000, 0.000000000000000000 ) ) ;
#195084 = DIRECTION ( 'NONE',  ( -1.000000000000000000, 0.000000000000000000, 0.000000000000000000 ) ) ;
#195083 = VECTOR ( 'NONE', #175214, 1000.000000000000000 ) ;
#195085 = FACE_OUTER_BOUND ( 'NONE', #181299, .T. ) ;
#195086 = AXIS2_PLACEMENT_3D ( 'NONE', #10767, #90278, #169889 ) ;
#195087 = DIRECTION ( 'NONE',  ( -1.000000000000000000, 0.000000000000000000, 0.000000000000000000 ) ) ;
#195088 = ORIENTED_EDGE ( 'NONE', *, *, #208493, .T. ) ;
#195089 = CARTESIAN_POINT ( 'NONE',  ( -12.60829076262179882, 66.61047060254530550, -118.7059995716306702 ) ) ;
#195090 = ORIENTED_EDGE ( 'NONE', *, *, #175702, .T. ) ;
#195091 = CARTESIAN_POINT ( 'NONE',  ( -23.25000000000000000, 1.115600667400684642E-11, -175.4000000000000341 ) ) ;
#195092 = VERTEX_POINT ( 'NONE', #148125 ) ;
#195093 = AXIS2_PLACEMENT_3D ( 'NONE', #14735, #117657, #235048 ) ;
#195094 = CARTESIAN_POINT ( 'NONE',  ( -20.94999999999999929, 76.00000000001170974, -69.52310748452431710 ) ) ;
#195095 = EDGE_CURVE ( 'NONE', #11636, #44715, #205063, .T. ) ;
#195096 = CARTESIAN_POINT ( 'NONE',  ( 21.14999999999999858, 64.35000000001201670, -114.7731074845243882 ) ) ;
#195097 = DIRECTION ( 'NONE',  ( 1.000000000000000000, 0.000000000000000000, 0.000000000000000000 ) ) ;
#195098 = ORIENTED_EDGE ( 'NONE', *, *, #237762, .T. ) ;
#195099 = DIRECTION ( 'NONE',  ( 0.000000000000000000, 0.000000000000000000, 1.000000000000000000 ) ) ;
#195100 = CIRCLE ( 'NONE', #61990, 0.09999999999999938105 ) ;
#195102 = ORIENTED_EDGE ( 'NONE', *, *, #212301, .T. ) ;
#195101 = DIRECTION ( 'NONE',  ( 1.000000000000000000, 0.000000000000000000, 0.000000000000000000 ) ) ;
#195103 = DIRECTION ( 'NONE',  ( -0.000000000000000000, -0.9876197685951290106, 0.1568667991644625281 ) ) ;
#195104 = ORIENTED_EDGE ( 'NONE', *, *, #146375, .T. ) ;
#195105 = TOROIDAL_SURFACE ( 'NONE', #82611, 12.77500000000000036, 0.1000000000000000056 ) ;
#195106 = ORIENTED_EDGE ( 'NONE', *, *, #35893, .T. ) ;
#195107 = AXIS2_PLACEMENT_3D ( 'NONE', #41998, #36877, #39442 ) ;
#195108 = AXIS2_PLACEMENT_3D ( 'NONE', #152874, #54992, #74627 ) ;
#195109 = VECTOR ( 'NONE', #66980, 1000.000000000000000 ) ;
#195110 = EDGE_CURVE ( 'NONE', #59708, #113902, #38504, .T. ) ;
#195111 = CARTESIAN_POINT ( 'NONE',  ( 23.14999999999999858, 36.65892442174935439, -249.5511627012433848 ) ) ;
#195112 = ORIENTED_EDGE ( 'NONE', *, *, #217535, .F. ) ;
#195114 = CIRCLE ( 'NONE', #7667, 0.09999999999998898659 ) ;
#195113 = FACE_OUTER_BOUND ( 'NONE', #11818, .T. ) ;
#195115 = FACE_OUTER_BOUND ( 'NONE', #209509, .T. ) ;
#195116 = CARTESIAN_POINT ( 'NONE',  ( 22.88900146558018989, 67.29609520889876251, -56.87310748452437537 ) ) ;
#195117 = EDGE_CURVE ( 'NONE', #129506, #134706, #30767, .T. ) ;
#195118 = CARTESIAN_POINT ( 'NONE',  ( -21.08621493067320429, 0.05619483948720407906, -60.65070570882810586 ) ) ;
#195119 = ORIENTED_EDGE ( 'NONE', *, *, #206112, .T. ) ;
#195120 = DIRECTION ( 'NONE',  ( 0.000000000000000000, 0.000000000000000000, 1.000000000000000000 ) ) ;
#195121 = CARTESIAN_POINT ( 'NONE',  ( -20.99749315643148151, 64.25000000001195133, -110.0379132532841453 ) ) ;
#195122 = CARTESIAN_POINT ( 'NONE',  ( -20.85000000000000142, -11.64999999998884306, -200.9999999999999432 ) ) ;
#195123 = ORIENTED_EDGE ( 'NONE', *, *, #128020, .T. ) ;
#195124 = CARTESIAN_POINT ( 'NONE',  ( 21.53699400381533380, 6.632243066309477797, -199.5555681750802819 ) ) ;
#195126 = ORIENTED_EDGE ( 'NONE', *, *, #99018, .T. ) ;
#195125 = CIRCLE ( 'NONE', #103500, 0.1000000000000032391 ) ;
#195128 = VECTOR ( 'NONE', #108365, 1000.000000000000000 ) ;
#195127 = CARTESIAN_POINT ( 'NONE',  ( -21.44999999999999929, 68.65000000001180069, -81.77310748452435973 ) ) ;
#195129 = ORIENTED_EDGE ( 'NONE', *, *, #172745, .F. ) ;
#195130 = EDGE_CURVE ( 'NONE', #3673, #57200, #130066, .T. ) ;
#195131 = EDGE_CURVE ( 'NONE', #97821, #202965, #152003, .T. ) ;
#195132 = DIRECTION ( 'NONE',  ( -1.000000000000000000, 0.000000000000000000, -0.000000000000000000 ) ) ;
#195133 = LINE ( 'NONE', #153461, #6327 ) ;
#195135 = VERTEX_POINT ( 'NONE', #89418 ) ;
#195134 = CARTESIAN_POINT ( 'NONE',  ( -23.25000000000000000, 11.65000000000000036, 0.000000000000000000 ) ) ;
#195136 = CARTESIAN_POINT ( 'NONE',  ( -23.25000000000000355, 64.25000000001233502, -160.7731074845244450 ) ) ;
#195137 = EDGE_LOOP ( 'NONE', ( #207028, #42136, #221462, #194284 ) ) ;
#195138 = CYLINDRICAL_SURFACE ( 'NONE', #248363, 0.09999999999999939493 ) ;
#195139 = AXIS2_PLACEMENT_3D ( 'NONE', #136168, #215724, #157070 ) ;
#195140 = CARTESIAN_POINT ( 'NONE',  ( 19.97071067811864609, 64.27928932189333011, -115.1731074845243796 ) ) ;
#195141 = AXIS2_PLACEMENT_3D ( 'NONE', #91620, #229845, #108612 ) ;
#195142 = ORIENTED_EDGE ( 'NONE', *, *, #79475, .F. ) ;
#195143 = CARTESIAN_POINT ( 'NONE',  ( -18.40000000000000213, 64.25000000001179501, -78.77310748452440237 ) ) ;
#195144 = DIRECTION ( 'NONE',  ( 0.000000000000000000, -1.000000000000000000, 0.000000000000000000 ) ) ;
#195145 = CIRCLE ( 'NONE', #224340, 0.1999999999999945155 ) ;
#195146 = ORIENTED_EDGE ( 'NONE', *, *, #22118, .F. ) ;
#195147 = DIRECTION ( 'NONE',  ( 0.000000000000000000, 0.9910465087640866200, 0.1335171055202867274 ) ) ;
#195148 = EDGE_CURVE ( 'NONE', #11036, #126038, #170299, .T. ) ;
#195149 = ORIENTED_EDGE ( 'NONE', *, *, #26837, .F. ) ;
#195150 = CARTESIAN_POINT ( 'NONE',  ( 23.14999999999999503, 23.34004772283015683, -229.2004250369967338 ) ) ;
#195151 = CARTESIAN_POINT ( 'NONE',  ( -23.25000000000000000, 77.73670573947964613, -125.0056848969006182 ) ) ;
#195152 = EDGE_CURVE ( 'NONE', #126808, #78012, #111566, .T. ) ;
#195153 = B_SPLINE_CURVE_WITH_KNOTS ( 'NONE', 3,
 ( #134245, #97675, #139374, #35206, #194268, #135529, #15636, #95138, #234648, #116002 ),
 .UNSPECIFIED., .F., .F.,
 ( 4, 2, 2, 2, 4 ),
 ( 0.000000000000000000, 3.990160268012661246E-05, 7.980320536025322493E-05, 0.0001596064107205033328, 0.0003192128214409992930 ),
 .UNSPECIFIED. ) ;
#195154 = AXIS2_PLACEMENT_3D ( 'NONE', #89000, #66886, #48599 ) ;
#195156 = ORIENTED_EDGE ( 'NONE', *, *, #97449, .T. ) ;
#195155 = CARTESIAN_POINT ( 'NONE',  ( -23.39999999999994529, 76.00000000001119815, -36.02310748452479316 ) ) ;
#195157 = DIRECTION ( 'NONE',  ( 1.000000000000000000, 0.000000000000000000, 0.000000000000000000 ) ) ;
#195158 = TOROIDAL_SURFACE ( 'NONE', #224167, 0.2000000000000000111, 0.1000000000000000056 ) ;
#195159 = CARTESIAN_POINT ( 'NONE',  ( 23.14999999999999858, 76.00000000001190870, -103.0231074845243029 ) ) ;
#195160 = CIRCLE ( 'NONE', #3586, 2.000000000000002665 ) ;
#195161 = EDGE_CURVE ( 'NONE', #204435, #197715, #96730, .T. ) ;
#195162 = CARTESIAN_POINT ( 'NONE',  ( -16.93344882324368683, 9.996588767287876820, -20.91302569480492579 ) ) ;
#195163 = AXIS2_PLACEMENT_3D ( 'NONE', #43713, #218473, #123247 ) ;
#195165 = CARTESIAN_POINT ( 'NONE',  ( -22.49917693094574389, 75.91477003579079508, -181.6729032690550127 ) ) ;
#195164 = CYLINDRICAL_SURFACE ( 'NONE', #202518, 0.09999999999999635569 ) ;
#195166 = LINE ( 'NONE', #131303, #140392 ) ;
#195168 = EDGE_CURVE ( 'NONE', #170534, #13871, #196702, .T. ) ;
#195167 = LINE ( 'NONE', #178164, #123469 ) ;
#195169 = CARTESIAN_POINT ( 'NONE',  ( 18.46905048506370761, 85.47374425739377557, -29.34712119226885108 ) ) ;
#195170 = CARTESIAN_POINT ( 'NONE',  ( 20.94999999999999574, 1.162701749949165642, -108.4000000000000341 ) ) ;
#195171 = ORIENTED_EDGE ( 'NONE', *, *, #73976, .F. ) ;
#195172 = EDGE_LOOP ( 'NONE', ( #44525, #52055, #94795 ) ) ;
#195173 = DIRECTION ( 'NONE',  ( 1.000000000000000000, 0.000000000000000000, 0.000000000000000000 ) ) ;
#195175 = ORIENTED_EDGE ( 'NONE', *, *, #77069, .T. ) ;
#195174 = CARTESIAN_POINT ( 'NONE',  ( -18.39418127959864435, 33.92771173063928103, -235.0603702762365970 ) ) ;
#195176 = ORIENTED_EDGE ( 'NONE', *, *, #127025, .T. ) ;
#195177 = DIRECTION ( 'NONE',  ( -1.000000000000000000, 0.000000000000000000, 0.000000000000000000 ) ) ;
#195178 = ORIENTED_EDGE ( 'NONE', *, *, #223786, .F. ) ;
#195179 = CARTESIAN_POINT ( 'NONE',  ( 17.74533788810829904, 12.76545729867106971, -208.7752074168712397 ) ) ;
#195180 = EDGE_CURVE ( 'NONE', #27421, #38202, #213266, .T. ) ;
#195181 = ADVANCED_FACE ( 'NONE', ( #93273 ), #146807, .T. ) ;
#195182 = CIRCLE ( 'NONE', #12017, 0.5000000000000004441 ) ;
#195183 = ORIENTED_EDGE ( 'NONE', *, *, #178552, .T. ) ;
#195184 = FILL_AREA_STYLE_COLOUR ( '', #256260 ) ;
#195185 = FACE_OUTER_BOUND ( 'NONE', #253925, .T. ) ;
#195187 = ORIENTED_EDGE ( 'NONE', *, *, #92454, .F. ) ;
#195186 = ORIENTED_EDGE ( 'NONE', *, *, #67942, .T. ) ;
#195188 = VERTEX_POINT ( 'NONE', #232816 ) ;
#195189 = ORIENTED_EDGE ( 'NONE', *, *, #32502, .T. ) ;
#195190 = ORIENTED_EDGE ( 'NONE', *, *, #29312, .F. ) ;
#195191 = CARTESIAN_POINT ( 'NONE',  ( -18.69999999999999929, 11.49641995933507843, -1.885425182446134107 ) ) ;
#195192 = DIRECTION ( 'NONE',  ( 0.000000000000000000, 7.086529944415886769E-15, -1.000000000000000000 ) ) ;
#195194 = VERTEX_POINT ( 'NONE', #137523 ) ;
#195193 = CARTESIAN_POINT ( 'NONE',  ( -18.59999999999999787, 66.85000000001180354, -81.87310748452438247 ) ) ;
#195195 = CARTESIAN_POINT ( 'NONE',  ( -20.85000000000000142, 10.33248238082518711, -39.09484654391314962 ) ) ;
#195196 = CARTESIAN_POINT ( 'NONE',  ( 13.12220780326571656, 12.45596502558539065, -213.8760425650930301 ) ) ;
#195198 = VERTEX_POINT ( 'NONE', #157130 ) ;
#195197 = DIRECTION ( 'NONE',  ( 0.000000000000000000, -0.9908441862701791170, 0.1350103645450472789 ) ) ;
#195199 = FACE_OUTER_BOUND ( 'NONE', #231730, .T. ) ;
#195200 = ORIENTED_EDGE ( 'NONE', *, *, #173952, .F. ) ;
#195201 = CARTESIAN_POINT ( 'NONE',  ( -21.65000000000000213, 68.75000000001256240, -182.6731074845244223 ) ) ;
#195203 = VERTEX_POINT ( 'NONE', #57982 ) ;
#195202 = FACE_OUTER_BOUND ( 'NONE', #102818, .T. ) ;
#195204 = LINE ( 'NONE', #34847, #43595 ) ;
#195205 = CARTESIAN_POINT ( 'NONE',  ( -18.50000000000000000, 77.63717271298298783, -191.9409541190523214 ) ) ;
#195206 = DIRECTION ( 'NONE',  ( 0.000000000000000000, 0.2128009952263601456, -0.9770955615653316162 ) ) ;
#195207 = EDGE_LOOP ( 'NONE', ( #146874, #220310, #175776, #185249 ) ) ;
#195208 = CIRCLE ( 'NONE', #3623, 2.100000000000008527 ) ;
#195211 = DIRECTION ( 'NONE',  ( 0.000000000000000000, 0.000000000000000000, -1.000000000000000000 ) ) ;
#195210 = AXIS2_PLACEMENT_3D ( 'NONE', #136099, #133564, #55275 ) ;
#195209 = CARTESIAN_POINT ( 'NONE',  ( -16.84981964351502626, 9.917318234110023667, -46.36960161401952263 ) ) ;
#195212 = AXIS2_PLACEMENT_3D ( 'NONE', #90378, #188209, #211634 ) ;
#195213 = CARTESIAN_POINT ( 'NONE',  ( 22.37643362114956247, 7.625789993969535274, -133.9009186263186564 ) ) ;
#195214 = ADVANCED_FACE ( 'NONE', ( #217055 ), #1045, .T. ) ;
#195215 = CARTESIAN_POINT ( 'NONE',  ( 21.05000000000000071, -9.499999999988848032, -43.39396912265245021 ) ) ;
#195216 = CARTESIAN_POINT ( 'NONE',  ( 21.14999999999999858, 1.115600667400684642E-11, -155.8504291924551808 ) ) ;
#195217 = EDGE_LOOP ( 'NONE', ( #146176, #246969, #197177, #85359, #151285 ) ) ;
#195218 = VERTEX_POINT ( 'NONE', #116690 ) ;
#195219 = DIRECTION ( 'NONE',  ( 0.000000000000000000, 0.000000000000000000, -1.000000000000000000 ) ) ;
#195220 = AXIS2_PLACEMENT_3D ( 'NONE', #120530, #74985, #154532 ) ;
#195221 = DIRECTION ( 'NONE',  ( -2.812466655313719426E-14, 0.1350103645451904977, 0.9908441862701596881 ) ) ;
#195222 = ORIENTED_EDGE ( 'NONE', *, *, #116562, .T. ) ;
#195223 = CARTESIAN_POINT ( 'NONE',  ( -23.15000000000000213, 86.27712145182582049, -209.5223386573213702 ) ) ;
#195224 = VERTEX_POINT ( 'NONE', #239210 ) ;
#195225 = CARTESIAN_POINT ( 'NONE',  ( 6.100000000000062705, 64.25000000001119815, -22.12310748452479103 ) ) ;
#195226 = CARTESIAN_POINT ( 'NONE',  ( -22.47071067811865319, 75.90090754530983475, -177.7431822290224090 ) ) ;
#195227 = VECTOR ( 'NONE', #167249, 1000.000000000000000 ) ;
#195228 = CIRCLE ( 'NONE', #149433, 0.5000000000000007772 ) ;
#195229 = ORIENTED_EDGE ( 'NONE', *, *, #204712, .T. ) ;
#195230 = AXIS2_PLACEMENT_3D ( 'NONE', #224191, #128963, #109370 ) ;
#195231 = DIRECTION ( 'NONE',  ( 1.000000000000000000, 0.000000000000000000, 0.000000000000000000 ) ) ;
#195232 = SURFACE_STYLE_USAGE ( .BOTH. , #74010 ) ;
#195233 = EDGE_CURVE ( 'NONE', #123531, #196984, #179984, .T. ) ;
#195234 = ORIENTED_EDGE ( 'NONE', *, *, #31337, .F. ) ;
#195235 = AXIS2_PLACEMENT_3D ( 'NONE', #101143, #146713, #120789 ) ;
#195236 = ORIENTED_EDGE ( 'NONE', *, *, #206907, .F. ) ;
#195237 = VERTEX_POINT ( 'NONE', #193672 ) ;
#195238 = CARTESIAN_POINT ( 'NONE',  ( -20.54999999999999716, 20.06933876993645782, -235.7297789824848451 ) ) ;
#195239 = CARTESIAN_POINT ( 'NONE',  ( 12.60053434924910221, 66.61046543766484263, -53.84829818013444225 ) ) ;
#195240 = CARTESIAN_POINT ( 'NONE',  ( 21.05000000000000071, 11.75000000001116263, -126.9851942293460922 ) ) ;
#195241 = DIRECTION ( 'NONE',  ( 0.000000000000000000, 0.000000000000000000, -1.000000000000000000 ) ) ;
#195242 = CARTESIAN_POINT ( 'NONE',  ( -21.65000000000000213, 60.93935776605891164, -221.0417277355860790 ) ) ;
#195243 = DIRECTION ( 'NONE',  ( -1.000000000000000000, -2.952720810173289112E-16, 0.000000000000000000 ) ) ;
#195245 = ORIENTED_EDGE ( 'NONE', *, *, #166425, .F. ) ;
#195244 = CARTESIAN_POINT ( 'NONE',  ( -23.25000000000000355, 70.35000000001210196, -127.2731074845243313 ) ) ;
#195246 = DIRECTION ( 'NONE',  ( 0.000000000000000000, 0.8777080977375655291, -0.4791956752370622463 ) ) ;
#195247 = EDGE_LOOP ( 'NONE', ( #43536, #239902, #66544, #160476 ) ) ;
#195248 = CARTESIAN_POINT ( 'NONE',  ( -15.15766958671843945, 9.410538608540022665, -149.4326879971409596 ) ) ;
#195249 = ORIENTED_EDGE ( 'NONE', *, *, #48100, .F. ) ;
#195250 = ORIENTED_EDGE ( 'NONE', *, *, #44465, .F. ) ;
#195251 = FACE_OUTER_BOUND ( 'NONE', #14354, .T. ) ;
#195252 = CARTESIAN_POINT ( 'NONE',  ( -21.05000000000000071, 6.304961112695769643, -134.0213855659371234 ) ) ;
#195253 = CARTESIAN_POINT ( 'NONE',  ( 20.73486653747088582, 42.13647595316533057, -239.1530172309881550 ) ) ;
#195254 = COLOUR_RGB ( '', 0.31764706, 0.68627451, 0.89019608) ;
#195255 = AXIS2_PLACEMENT_3D ( 'NONE', #102741, #121087, #78062 ) ;
#195256 = AXIS2_PLACEMENT_3D ( 'NONE', #43305, #139813, #202371 ) ;
#195257 = CARTESIAN_POINT ( 'NONE',  ( 20.92356734117541706, 18.39335631088232503, -236.9600537807593241 ) ) ;
#195258 = ORIENTED_EDGE ( 'NONE', *, *, #122772, .T. ) ;
#195259 = EDGE_LOOP ( 'NONE', ( #255433, #111087, #187705, #172452 ) ) ;
#195260 = CARTESIAN_POINT ( 'NONE',  ( -20.94999999999999929, -1.162701749926853712, -175.5999999999999659 ) ) ;
#195261 = EDGE_LOOP ( 'NONE', ( #20592, #142004, #197339, #126719 ) ) ;
#195262 = CARTESIAN_POINT ( 'NONE',  ( -16.94180778212363236, 60.88640190408171549, -221.0748371733828606 ) ) ;
#195263 = EDGE_LOOP ( 'NONE', ( #239654, #52219, #105406, #20332 ) ) ;
#195265 = DIRECTION ( 'NONE',  ( 1.000000000000000000, 0.000000000000000000, 0.000000000000000000 ) ) ;
#195264 = VECTOR ( 'NONE', #204902, 1000.000000000000000 ) ;
#195266 = CYLINDRICAL_SURFACE ( 'NONE', #132198, 0.09999999999999939493 ) ;
#195267 = DIRECTION ( 'NONE',  ( 1.000000000000000000, 0.000000000000000000, 0.000000000000000000 ) ) ;
#195268 = ORIENTED_EDGE ( 'NONE', *, *, #64906, .T. ) ;
#195269 = PLANE ( 'NONE',  #220924 ) ;
#195270 = CARTESIAN_POINT ( 'NONE',  ( -21.14999999999999858, -11.74999999998884448, -100.5000000000000284 ) ) ;
#195271 = EDGE_CURVE ( 'NONE', #90102, #156170, #215775, .T. ) ;
#195272 = TOROIDAL_SURFACE ( 'NONE', #74482, 11.70000000000000639, 0.1000000000000000056 ) ;
#195273 = DIRECTION ( 'NONE',  ( 0.000000000000000000, 1.000000000000000000, 1.321694076934707365E-14 ) ) ;
#195274 = AXIS2_PLACEMENT_3D ( 'NONE', #205498, #127260, #107686 ) ;
#195275 = EDGE_LOOP ( 'NONE', ( #206362, #140240, #60918, #257081 ) ) ;
#195276 = AXIS2_PLACEMENT_3D ( 'NONE', #105454, #6388, #220317 ) ;
#195277 = EDGE_CURVE ( 'NONE', #227344, #250075, #254910, .T. ) ;
#195278 = CARTESIAN_POINT ( 'NONE',  ( 21.11344571971284623, 10.61787902351794699, -12.24602089239997227 ) ) ;
#195279 = ORIENTED_EDGE ( 'NONE', *, *, #74557, .T. ) ;
#195280 = CARTESIAN_POINT ( 'NONE',  ( 15.74999999999999289, 66.65000000001225544, -153.5045385271216958 ) ) ;
#195281 = DIRECTION ( 'NONE',  ( 0.000000000000000000, -0.9910465087640866200, 0.1335171055202867274 ) ) ;
#195282 = EDGE_CURVE ( 'NONE', #199182, #89904, #125971, .T. ) ;
#195283 = LINE ( 'NONE', #253928, #250440 ) ;
#195285 = AXIS2_PLACEMENT_3D ( 'NONE', #237846, #213144, #17506 ) ;
#195284 = DIRECTION ( 'NONE',  ( 0.000000000000000000, 0.000000000000000000, 1.000000000000000000 ) ) ;
#195286 = DIRECTION ( 'NONE',  ( 0.000000000000000000, 1.000000000000000000, -0.000000000000000000 ) ) ;
#195287 = DIRECTION ( 'NONE',  ( -3.469446951953515108E-14, 1.000000000000000000, 0.000000000000000000 ) ) ;
#195288 = CIRCLE ( 'NONE', #166245, 0.09999999999999326095 ) ;
#195289 = ORIENTED_EDGE ( 'NONE', *, *, #208238, .F. ) ;
#195290 = SPHERICAL_SURFACE ( 'NONE', #238287, 0.1000000000000000056 ) ;
#195291 = DIRECTION ( 'NONE',  ( -1.000000000000000000, -0.000000000000000000, -0.000000000000000000 ) ) ;
#195292 = CARTESIAN_POINT ( 'NONE',  ( 21.05000000000000071, 87.65000000001215597, -139.6231074845242688 ) ) ;
#195293 = DIRECTION ( 'NONE',  ( -0.000000000000000000, 1.000000000000000000, -1.224646799147352961E-16 ) ) ;
#195295 = ADVANCED_FACE ( 'NONE', ( #38441 ), #117980, .F. ) ;
#195294 = TOROIDAL_SURFACE ( 'NONE', #248872, 4.149999999999999467, 0.1000000000000000056 ) ;
#195296 = DIRECTION ( 'NONE',  ( -6.938893903907209445E-14, -0.9999176327611370985, -0.01283462868040260302 ) ) ;
#195297 = AXIS2_PLACEMENT_3D ( 'NONE', #189108, #155151, #234649 ) ;
#195298 = AXIS2_PLACEMENT_3D ( 'NONE', #57359, #216445, #177364 ) ;
#195300 = ORIENTED_EDGE ( 'NONE', *, *, #157742, .F. ) ;
#195299 = AXIS2_PLACEMENT_3D ( 'NONE', #71729, #225618, #196778 ) ;
#195301 = ORIENTED_EDGE ( 'NONE', *, *, #220698, .T. ) ;
#195302 = DIRECTION ( 'NONE',  ( -1.000000000000000000, 2.952720810173289112E-16, 2.061873921506763405E-30 ) ) ;
#195303 = AXIS2_PLACEMENT_3D ( 'NONE', #203502, #246472, #104369 ) ;
#195304 = LINE ( 'NONE', #178304, #218367 ) ;
#195305 = CARTESIAN_POINT ( 'NONE',  ( -21.05000000000000071, 69.74168394268066606, -203.5888090948464537 ) ) ;
#195306 = DIRECTION ( 'NONE',  ( 0.000000000000000000, 0.2716869542551192951, -0.9623856809447951521 ) ) ;
#195307 = EDGE_CURVE ( 'NONE', #117327, #50256, #171812, .T. ) ;
#195308 = ORIENTED_EDGE ( 'NONE', *, *, #236501, .F. ) ;
#195309 = LINE ( 'NONE', #135285, #205395 ) ;
#195310 = CARTESIAN_POINT ( 'NONE',  ( -18.50000000000000000, -9.399999999988850163, -141.2972597596633193 ) ) ;
#195311 = ORIENTED_EDGE ( 'NONE', *, *, #14382, .F. ) ;
#195312 = CARTESIAN_POINT ( 'NONE',  ( -20.00857864376270001, 66.85000000001222986, -148.7731074845244166 ) ) ;
#195313 = PRODUCT_DEFINITION_SHAPE ( 'NONE', 'NONE',  #258135 ) ;
#195314 = CARTESIAN_POINT ( 'NONE',  ( 23.24999999999999645, 11.31241850904329205, -211.4828089347303433 ) ) ;
#195315 = VECTOR ( 'NONE', #65845, 1000.000000000000000 ) ;
#195316 = AXIS2_PLACEMENT_3D ( 'NONE', #133705, #15061, #115421 ) ;
#195317 = ORIENTED_EDGE ( 'NONE', *, *, #200813, .F. ) ;
#195318 = DIRECTION ( 'NONE',  ( 0.1538461538461484146, -0.9880948137434723000, 0.000000000000000000 ) ) ;
#195319 = ORIENTED_EDGE ( 'NONE', *, *, #254868, .F. ) ;
#195320 = CARTESIAN_POINT ( 'NONE',  ( 20.94999999999999929, 61.00122447389660607, -225.2976766370351527 ) ) ;
#195321 = DIRECTION ( 'NONE',  ( 0.000000000000000000, 6.982962677686266711E-15, -1.000000000000000000 ) ) ;
#195322 = CARTESIAN_POINT ( 'NONE',  ( 23.24999999999999289, 6.550000000011156231, -121.8500000000000369 ) ) ;
#195323 = DIRECTION ( 'NONE',  ( 0.000000000000000000, 1.000000000000000000, 0.000000000000000000 ) ) ;
#195325 = AXIS2_PLACEMENT_3D ( 'NONE', #233430, #173493, #114745 ) ;
#195324 = DIRECTION ( 'NONE',  ( 1.000000000000000000, 0.000000000000000000, 0.000000000000000000 ) ) ;
#195326 = DIRECTION ( 'NONE',  ( 1.000000000000000000, 0.000000000000000000, 0.000000000000000000 ) ) ;
#195327 = CARTESIAN_POINT ( 'NONE',  ( 23.24999999999999289, 64.35000000001201670, -114.7731074845243882 ) ) ;
#195328 = DIRECTION ( 'NONE',  ( -1.000000000000000000, 0.000000000000000000, 0.000000000000000000 ) ) ;
#195329 = CIRCLE ( 'NONE', #82827, 12.77500000000000036 ) ;
#195330 = CARTESIAN_POINT ( 'NONE',  ( 20.85000000000000142, -11.74999999998883560, -64.10000000000000853 ) ) ;
#195331 = CARTESIAN_POINT ( 'NONE',  ( -23.15000000000000213, 47.66483718802935954, -241.7716698398223514 ) ) ;
#195332 = AXIS2_PLACEMENT_3D ( 'NONE', #146858, #111614, #89462 ) ;
#195333 = DIRECTION ( 'NONE',  ( 1.000000000000000000, 0.000000000000000000, 0.000000000000000000 ) ) ;
#195334 = CARTESIAN_POINT ( 'NONE',  ( -17.11825945287481332, 30.11817903451004952, -234.7598257170722889 ) ) ;
#195335 = DIRECTION ( 'NONE',  ( 0.000000000000000000, -0.4948392722769175411, -0.8689845192018386122 ) ) ;
#195336 = ORIENTED_EDGE ( 'NONE', *, *, #61756, .F. ) ;
#195337 = CYLINDRICAL_SURFACE ( 'NONE', #116267, 12.87499999999999822 ) ;
#195338 = CIRCLE ( 'NONE', #20360, 0.1000000000000096922 ) ;
#195339 = ADVANCED_FACE ( 'NONE', ( #158426 ), #46855, .F. ) ;
#195340 = ORIENTED_EDGE ( 'NONE', *, *, #126371, .F. ) ;
#195341 = CARTESIAN_POINT ( 'NONE',  ( -16.87036670365548474, 63.08160062417908165, -212.9922606024214531 ) ) ;
#195342 = CARTESIAN_POINT ( 'NONE',  ( -16.94445028196807002, 66.00793639031378746, -48.63043766294283898 ) ) ;
#195343 = CARTESIAN_POINT ( 'NONE',  ( -18.50000000000000000, 43.08613539620618837, -254.3146655184800409 ) ) ;
#195344 = ADVANCED_FACE ( 'NONE', ( #80094 ), #94553, .T. ) ;
#195345 = VERTEX_POINT ( 'NONE', #75037 ) ;
#195346 = DIRECTION ( 'NONE',  ( 0.000000000000000000, -0.000000000000000000, 1.000000000000000000 ) ) ;
#195347 = CARTESIAN_POINT ( 'NONE',  ( -20.85000000000000142, 68.87972903831482085, -166.3635444426850825 ) ) ;
#195348 = AXIS2_PLACEMENT_3D ( 'NONE', #193511, #254702, #171405 ) ;
#195349 = EDGE_LOOP ( 'NONE', ( #7592, #107149, #190768, #221317 ) ) ;
#195351 = EDGE_CURVE ( 'NONE', #133516, #255891, #214502, .T. ) ;
#195350 = DIRECTION ( 'NONE',  ( 1.000000000000000000, -0.000000000000000000, -0.000000000000000000 ) ) ;
#195352 = LINE ( 'NONE', #233197, #105719 ) ;
#195353 = CIRCLE ( 'NONE', #237025, 0.1000000000000016154 ) ;
#195354 = ORIENTED_EDGE ( 'NONE', *, *, #227017, .T. ) ;
#195355 = CARTESIAN_POINT ( 'NONE',  ( 20.85000000000000142, 68.97833521811159585, -65.68954208262705663 ) ) ;
#195356 = EDGE_CURVE ( 'NONE', #84780, #183877, #159329, .T. ) ;
#195357 = ORIENTED_EDGE ( 'NONE', *, *, #85253, .F. ) ;
#195358 = DIRECTION ( 'NONE',  ( -1.000000000000000000, 0.000000000000000000, 0.000000000000000000 ) ) ;
#195359 = FACE_OUTER_BOUND ( 'NONE', #35733, .T. ) ;
#195360 = DIRECTION ( 'NONE',  ( 1.000000000000000000, -3.265361837132813093E-16, -2.280189983783949500E-30 ) ) ;
#195361 = EDGE_CURVE ( 'NONE', #2705, #105079, #234066, .T. ) ;
#195362 = CARTESIAN_POINT ( 'NONE',  ( 23.14999999999999858, 1.115600667400684642E-11, -67.00000000000000000 ) ) ;
#195363 = DIRECTION ( 'NONE',  ( 1.000000000000000000, 0.000000000000000000, 0.000000000000000000 ) ) ;
#195364 = CARTESIAN_POINT ( 'NONE',  ( -14.87779219673428521, 46.70395665056642542, -234.7173882531051277 ) ) ;
#195365 = DIRECTION ( 'NONE',  ( 1.000000000000000000, 0.000000000000000000, -0.000000000000000000 ) ) ;
#195366 = CARTESIAN_POINT ( 'NONE',  ( -22.10000000000000497, 6.342459739679072506, 12.00000000000000000 ) ) ;
#195368 = ORIENTED_EDGE ( 'NONE', *, *, #41453, .F. ) ;
#195367 = DIRECTION ( 'NONE',  ( 1.000000000000000000, 0.000000000000000000, 0.000000000000000000 ) ) ;
#195369 = ORIENTED_EDGE ( 'NONE', *, *, #143286, .F. ) ;
#195371 = DIRECTION ( 'NONE',  ( -0.000000000000000000, 0.2617529984165031243, 0.9651348961777157509 ) ) ;
#195370 = CARTESIAN_POINT ( 'NONE',  ( 18.39999999999999858, 85.51932773110434027, -96.05013110796491560 ) ) ;
#195373 = ORIENTED_EDGE ( 'NONE', *, *, #60445, .T. ) ;
#195372 = DIRECTION ( 'NONE',  ( 0.000000000000000000, 0.000000000000000000, 1.000000000000000000 ) ) ;
#195374 = ORIENTED_EDGE ( 'NONE', *, *, #68088, .F. ) ;
#195375 = CARTESIAN_POINT ( 'NONE',  ( -18.59999999999999787, 64.25000000001215028, -136.5231074845244166 ) ) ;
#195376 = CARTESIAN_POINT ( 'NONE',  ( 20.58091095332318332, 9.018470153363605135, -175.9186501821585296 ) ) ;
#195377 = EDGE_CURVE ( 'NONE', #167725, #125649, #72010, .T. ) ;
#195378 = DIRECTION ( 'NONE',  ( 1.000000000000000000, 0.000000000000000000, 0.000000000000000000 ) ) ;
#195379 = DIRECTION ( 'NONE',  ( 0.000000000000000000, 0.9274965247785529332, -0.3738317757009255171 ) ) ;
#195380 = CARTESIAN_POINT ( 'NONE',  ( 21.05000000000000071, 76.00000000001216449, -139.4231074845243654 ) ) ;
#195381 = EDGE_CURVE ( 'NONE', #248593, #38453, #47042, .T. ) ;
#195382 = ADVANCED_FACE ( 'NONE', ( #119278 ), #254857, .F. ) ;
#195383 = DIRECTION ( 'NONE',  ( 0.000000000000000000, 0.8814952561688476074, -0.4721928772777262417 ) ) ;
#195384 = CARTESIAN_POINT ( 'NONE',  ( -23.15000000000000213, 2.500000000011154633, -53.77537807723790309 ) ) ;
#195385 = DIRECTION ( 'NONE',  ( 0.000000000000000000, -0.2128009952263604232, 0.9770955615653316162 ) ) ;
#195386 = AXIS2_PLACEMENT_3D ( 'NONE', #119638, #98732, #20541 ) ;
#195387 = VERTEX_POINT ( 'NONE', #159685 ) ;
#195388 = ORIENTED_EDGE ( 'NONE', *, *, #31507, .T. ) ;
#195389 = AXIS2_PLACEMENT_3D ( 'NONE', #31630, #73327, #171157 ) ;
#195390 = DIRECTION ( 'NONE',  ( 0.000000000000000000, -6.982962677686266711E-15, 1.000000000000000000 ) ) ;
#195391 = AXIS2_PLACEMENT_3D ( 'NONE', #86859, #105120, #24368 ) ;
#195392 = AXIS2_PLACEMENT_3D ( 'NONE', #34524, #192301, #178876 ) ;
#195393 = VERTEX_POINT ( 'NONE', #243057 ) ;
#195394 = LINE ( 'NONE', #38875, #159436 ) ;
#195395 = ORIENTED_EDGE ( 'NONE', *, *, #130619, .F. ) ;
#195396 = CARTESIAN_POINT ( 'NONE',  ( 20.94999999999999929, 87.65000000001170122, -69.52310748452424605 ) ) ;
#195397 = CIRCLE ( 'NONE', #112199, 0.09999999999999939493 ) ;
#195398 = EDGE_CURVE ( 'NONE', #187371, #111708, #205256, .T. ) ;
#195399 = DIRECTION ( 'NONE',  ( 0.000000000000000000, 1.000000000000000000, 0.000000000000000000 ) ) ;
#195400 = FACE_OUTER_BOUND ( 'NONE', #76893, .T. ) ;
#195401 = EDGE_CURVE ( 'NONE', #161463, #101099, #217728, .T. ) ;
#195402 = VERTEX_POINT ( 'NONE', #41036 ) ;
#195403 = EDGE_LOOP ( 'NONE', ( #41832, #167373, #144176, #50754 ) ) ;
#195404 = DIRECTION ( 'NONE',  ( 1.000000000000000000, 0.000000000000000000, 0.000000000000000000 ) ) ;
#195406 = DIRECTION ( 'NONE',  ( 0.000000000000000000, -1.000000000000000000, 0.000000000000000000 ) ) ;
#195405 = VECTOR ( 'NONE', #2352, 1000.000000000000000 ) ;
#195407 = CIRCLE ( 'NONE', #174595, 0.9000000000000014655 ) ;
#195408 = DIRECTION ( 'NONE',  ( 1.000000000000000000, 0.000000000000000000, 0.000000000000000000 ) ) ;
#195409 = EDGE_CURVE ( 'NONE', #223804, #236296, #51119, .T. ) ;
#195411 = AXIS2_PLACEMENT_3D ( 'NONE', #166515, #83054, #63519 ) ;
#195410 = CARTESIAN_POINT ( 'NONE',  ( -21.95218792049438861, 75.90097156021282387, -210.7246150457710314 ) ) ;
#195412 = PLANE ( 'NONE',  #11685 ) ;
#195413 = ORIENTED_EDGE ( 'NONE', *, *, #14021, .F. ) ;
#195414 = CARTESIAN_POINT ( 'NONE',  ( -18.31572283045126071, 85.54843783089721398, -29.17248183346574564 ) ) ;
#195415 = ORIENTED_EDGE ( 'NONE', *, *, #25997, .F. ) ;
#195418 = ORIENTED_EDGE ( 'NONE', *, *, #155742, .T. ) ;
#195417 = CYLINDRICAL_SURFACE ( 'NONE', #92122, 0.09999999999999986677 ) ;
#195416 = CARTESIAN_POINT ( 'NONE',  ( 20.94999999999999929, 6.450000000011156587, -110.5170271704400591 ) ) ;
#195419 = VECTOR ( 'NONE', #202268, 1000.000000000000000 ) ;
#195420 = DIRECTION ( 'NONE',  ( 0.000000000000000000, 0.000000000000000000, -1.000000000000000000 ) ) ;
#195421 = ORIENTED_EDGE ( 'NONE', *, *, #6324, .T. ) ;
#195422 = CARTESIAN_POINT ( 'NONE',  ( 18.59999999999999076, 14.51805813080544638, -219.6885945441820809 ) ) ;
#195423 = DIRECTION ( 'NONE',  ( -0.000000000000000000, -0.000000000000000000, -1.000000000000000000 ) ) ;
#195424 = CARTESIAN_POINT ( 'NONE',  ( -16.95709691156388033, 9.949999999999983302, -12.66005756251007774 ) ) ;
#195426 = ORIENTED_EDGE ( 'NONE', *, *, #82554, .T. ) ;
#195425 = DIRECTION ( 'NONE',  ( -0.000000000000000000, -0.000000000000000000, 1.000000000000000000 ) ) ;
#195427 = EDGE_CURVE ( 'NONE', #105460, #33224, #180533, .T. ) ;
#195428 = LINE ( 'NONE', #119732, #126817 ) ;
#195429 = EDGE_LOOP ( 'NONE', ( #103042, #47537, #3835, #229542 ) ) ;
#195430 = ADVANCED_FACE ( 'NONE', ( #43585 ), #242032, .T. ) ;
#195431 = CARTESIAN_POINT ( 'NONE',  ( 23.24999999999999289, 64.35000000001275566, -215.2731074845244450 ) ) ;
#195432 = CARTESIAN_POINT ( 'NONE',  ( 18.59999999999999787, 87.75000000001222134, -148.6731074845242802 ) ) ;
#195433 = DIRECTION ( 'NONE',  ( 0.000000000000000000, 0.6728388485993177515, -0.7397890806274072251 ) ) ;
#195434 = AXIS2_PLACEMENT_3D ( 'NONE', #154005, #134363, #70595 ) ;
#195435 = ORIENTED_EDGE ( 'NONE', *, *, #254008, .F. ) ;
#195436 = DIRECTION ( 'NONE',  ( 0.000000000000000000, 0.2128009952263485993, -0.9770955615653341697 ) ) ;
#195437 = EDGE_LOOP ( 'NONE', ( #120392, #92095, #14871, #168308 ) ) ;
#195438 = DIRECTION ( 'NONE',  ( -1.000000000000000000, 3.265361837132813093E-16, 2.280189983783949500E-30 ) ) ;
#195439 = ADVANCED_FACE ( 'NONE', ( #203936 ), #25325, .T. ) ;
#195440 = EDGE_CURVE ( 'NONE', #184847, #59486, #188518, .T. ) ;
#195441 = DIRECTION ( 'NONE',  ( 1.000000000000000000, -0.000000000000000000, 0.000000000000000000 ) ) ;
#195442 = DIRECTION ( 'NONE',  ( 1.000000000000000000, 0.000000000000000000, 0.000000000000000000 ) ) ;
#195443 = VECTOR ( 'NONE', #33579, 999.9999999999998863 ) ;
#195444 = VERTEX_POINT ( 'NONE', #244337 ) ;
#195445 = DIRECTION ( 'NONE',  ( 0.000000000000000000, 0.000000000000000000, -1.000000000000000000 ) ) ;
#195446 = ADVANCED_FACE ( 'NONE', ( #3147 ), #26608, .T. ) ;
#195447 = DIRECTION ( 'NONE',  ( 0.000000000000000000, -0.8660254037844411501, -0.4999999999999956701 ) ) ;
#195448 = VERTEX_POINT ( 'NONE', #164819 ) ;
#195450 = CIRCLE ( 'NONE', #116338, 0.09999999999999939493 ) ;
#195449 = CARTESIAN_POINT ( 'NONE',  ( -21.64999999999999858, 65.95000000001255103, -182.6731074845244223 ) ) ;
#195451 = DIRECTION ( 'NONE',  ( 0.000000000000000000, -1.000000000000000000, 0.000000000000000000 ) ) ;
#195452 = DIRECTION ( 'NONE',  ( -1.000000000000000000, 0.000000000000000000, 0.000000000000000000 ) ) ;
#195453 = CIRCLE ( 'NONE', #162127, 0.09999999999999939493 ) ;
#195454 = EDGE_CURVE ( 'NONE', #200909, #11610, #246768, .T. ) ;
#195455 = ORIENTED_EDGE ( 'NONE', *, *, #66823, .T. ) ;
#195457 = EDGE_CURVE ( 'NONE', #58178, #166015, #117781, .T. ) ;
#195456 = AXIS2_PLACEMENT_3D ( 'NONE', #100670, #18607, #180254 ) ;
#195458 = FACE_OUTER_BOUND ( 'NONE', #217105, .T. ) ;
#195459 = ORIENTED_EDGE ( 'NONE', *, *, #103804, .F. ) ;
#195461 = ORIENTED_EDGE ( 'NONE', *, *, #81322, .T. ) ;
#195460 = DIRECTION ( 'NONE',  ( 0.000000000000000000, 0.000000000000000000, -1.000000000000000000 ) ) ;
#195462 = ADVANCED_FACE ( 'NONE', ( #222186 ), #219636, .T. ) ;
#195463 = AXIS2_PLACEMENT_3D ( 'NONE', #41941, #22377, #163165 ) ;
#195464 = AXIS2_PLACEMENT_3D ( 'NONE', #122189, #117050, #199150 ) ;
#195467 = ORIENTED_EDGE ( 'NONE', *, *, #193382, .T. ) ;
#195466 = ORIENTED_EDGE ( 'NONE', *, *, #138846, .T. ) ;
#195465 = CARTESIAN_POINT ( 'NONE',  ( -21.09316766718153247, 0.03926340231467564945, 6.370153312474713836 ) ) ;
#195468 = DIRECTION ( 'NONE',  ( 0.000000000000000000, 0.000000000000000000, -1.000000000000000000 ) ) ;
#195469 = CARTESIAN_POINT ( 'NONE',  ( -23.25000000000000000, 1.115600667400684642E-11, -134.0000000000000284 ) ) ;
#195470 = CARTESIAN_POINT ( 'NONE',  ( 20.94999999999999929, 70.50000000001151079, -48.42837350343745584 ) ) ;
#195471 = DIRECTION ( 'NONE',  ( 0.000000000000000000, 0.000000000000000000, -1.000000000000000000 ) ) ;
#195472 = EDGE_CURVE ( 'NONE', #129355, #80209, #109400, .T. ) ;
#195473 = FACE_OUTER_BOUND ( 'NONE', #9555, .T. ) ;
#195474 = CIRCLE ( 'NONE', #95483, 0.09999999999999543976 ) ;
#195475 = CARTESIAN_POINT ( 'NONE',  ( 21.05000000000000071, -1.849084418615859926, -45.15601052144712213 ) ) ;
#195476 = DIRECTION ( 'NONE',  ( -2.840903330521632269E-16, -0.7106264324241465813, 0.7035695228903323661 ) ) ;
#195478 = ORIENTED_EDGE ( 'NONE', *, *, #70103, .T. ) ;
#195477 = CIRCLE ( 'NONE', #195298, 0.2000000000000005107 ) ;
#195479 = VERTEX_POINT ( 'NONE', #120571 ) ;
#195480 = AXIS2_PLACEMENT_3D ( 'NONE', #55951, #156396, #15597 ) ;
#195481 = EDGE_LOOP ( 'NONE', ( #253108, #126245, #224388, #149279 ) ) ;
#195482 = EDGE_CURVE ( 'NONE', #236459, #87211, #213649, .T. ) ;
#195483 = DIRECTION ( 'NONE',  ( 0.000000000000000000, -0.000000000000000000, 1.000000000000000000 ) ) ;
#195485 = ORIENTED_EDGE ( 'NONE', *, *, #163785, .F. ) ;
#195484 = DIRECTION ( 'NONE',  ( -0.000000000000000000, 0.1575546449569769913, 0.9875102702516470599 ) ) ;
#195486 = CARTESIAN_POINT ( 'NONE',  ( 20.95000000000000284, 36.02918351690956200, -236.0543695120161090 ) ) ;
#195487 = ORIENTED_EDGE ( 'NONE', *, *, #193431, .F. ) ;
#195488 = FACE_OUTER_BOUND ( 'NONE', #127803, .T. ) ;
#195489 = ORIENTED_EDGE ( 'NONE', *, *, #59342, .T. ) ;
#195490 = ADVANCED_FACE ( 'NONE', ( #68290 ), #138593, .T. ) ;
#195491 = CARTESIAN_POINT ( 'NONE',  ( -23.25000000000000355, 23.11343627288707481, -230.8941331732335129 ) ) ;
#195492 = ADVANCED_FACE ( 'NONE', ( #248208 ), #33060, .T. ) ;
#195493 = ORIENTED_EDGE ( 'NONE', *, *, #92846, .F. ) ;
#195494 = DIRECTION ( 'NONE',  ( 0.000000000000000000, 0.000000000000000000, 1.000000000000000000 ) ) ;
#195495 = CARTESIAN_POINT ( 'NONE',  ( -23.15000000000000213, -8.999999999988844479, -90.60603087734760663 ) ) ;
#195497 = VERTEX_POINT ( 'NONE', #171290 ) ;
#195496 = VERTEX_POINT ( 'NONE', #50001 ) ;
#195498 = VERTEX_POINT ( 'NONE', #52556 ) ;
#195499 = CARTESIAN_POINT ( 'NONE',  ( -21.44999999999999929, 68.65000000001187175, -90.67310748452436542 ) ) ;
#195500 = ORIENTED_EDGE ( 'NONE', *, *, #228377, .F. ) ;
#195501 = VERTEX_POINT ( 'NONE', #207824 ) ;
#195502 = DIRECTION ( 'NONE',  ( 0.000000000000000000, 0.8814952561688476074, -0.4721928772777262417 ) ) ;
#195503 = ORIENTED_EDGE ( 'NONE', *, *, #193288, .T. ) ;
#195504 = ADVANCED_FACE ( 'NONE', ( #172575 ), #167703, .F. ) ;
#195505 = DIRECTION ( 'NONE',  ( -1.000000000000000000, 0.000000000000000000, 0.000000000000000000 ) ) ;
#195507 = DIRECTION ( 'NONE',  ( 0.000000000000000000, -0.4721928772777346239, -0.8814952561688430555 ) ) ;
#195506 = DIRECTION ( 'NONE',  ( 0.000000000000000000, 1.000000000000000000, 0.000000000000000000 ) ) ;
#195508 = DIRECTION ( 'NONE',  ( 0.000000000000000000, -0.2617529984165152257, -0.9651348961777124202 ) ) ;
#195509 = CYLINDRICAL_SURFACE ( 'NONE', #256731, 0.09999999999999939493 ) ;
#195510 = CARTESIAN_POINT ( 'NONE',  ( -20.54999999999999716, -8.999999999988844479, -90.60603087734760663 ) ) ;
#195511 = ORIENTED_EDGE ( 'NONE', *, *, #56070, .F. ) ;
#195512 = VECTOR ( 'NONE', #121326, 1000.000000000000000 ) ;
#195513 = VERTEX_POINT ( 'NONE', #206505 ) ;
#195514 = CARTESIAN_POINT ( 'NONE',  ( 18.39999999999999858, 77.13860723519891849, -241.8264964602989266 ) ) ;
#195515 = ADVANCED_FACE ( 'NONE', ( #90403 ), #201008, .T. ) ;
#195516 = CARTESIAN_POINT ( 'NONE',  ( -21.05000000000000071, -11.64999999998884483, -69.90000000000004832 ) ) ;
#195517 = CARTESIAN_POINT ( 'NONE',  ( 23.24999999999999645, 71.22429906543263201, -124.6743393804783722 ) ) ;
#195518 = CIRCLE ( 'NONE', #199788, 4.049999999999998934 ) ;
#195519 = ORIENTED_EDGE ( 'NONE', *, *, #251995, .T. ) ;
#195520 = CARTESIAN_POINT ( 'NONE',  ( 18.49999999999999645, 77.83534155023598089, -57.96795619196132776 ) ) ;
#195521 = VECTOR ( 'NONE', #118906, 1000.000000000000000 ) ;
#195522 = DIRECTION ( 'NONE',  ( 0.000000000000000000, 0.9126074666063545004, 0.4088369013363783999 ) ) ;
#195523 = LINE ( 'NONE', #53415, #155198 ) ;
#195524 = VERTEX_POINT ( 'NONE', #29206 ) ;
#195525 = VERTEX_POINT ( 'NONE', #226033 ) ;
#195526 = DIRECTION ( 'NONE',  ( 0.000000000000000000, -1.000000000000000000, 0.000000000000000000 ) ) ;
#195527 = EDGE_CURVE ( 'NONE', #229354, #193751, #108694, .T. ) ;
#195528 = CARTESIAN_POINT ( 'NONE',  ( 20.95000000000005258, 65.35000000001120668, -4.623107484524796362 ) ) ;
#195529 = ORIENTED_EDGE ( 'NONE', *, *, #5590, .T. ) ;
#195530 = PLANE ( 'NONE',  #238932 ) ;
#195531 = ORIENTED_EDGE ( 'NONE', *, *, #43853, .F. ) ;
#195532 = CYLINDRICAL_SURFACE ( 'NONE', #198178, 0.09999999999999939493 ) ;
#195533 = FACE_OUTER_BOUND ( 'NONE', #13579, .T. ) ;
#195535 = FACE_OUTER_BOUND ( 'NONE', #90845, .T. ) ;
#195534 = DIRECTION ( 'NONE',  ( 0.000000000000000000, -0.8490545835447252943, -0.5283051335749948674 ) ) ;
#195536 = AXIS2_PLACEMENT_3D ( 'NONE', #114456, #137847, #16653 ) ;
#195537 = CARTESIAN_POINT ( 'NONE',  ( 18.56579813702274961, 65.66974365629718591, -164.4360145562605169 ) ) ;
#195538 = CARTESIAN_POINT ( 'NONE',  ( 21.14261333020286315, 65.28430735075696134, -90.77310748452416078 ) ) ;
#195539 = AXIS2_PLACEMENT_3D ( 'NONE', #236166, #211474, #53679 ) ;
#195540 = DIRECTION ( 'NONE',  ( 1.000000000000000000, 0.000000000000000000, 0.000000000000000000 ) ) ;
#195541 = EDGE_CURVE ( 'NONE', #132220, #115886, #188230, .T. ) ;
#195542 = VECTOR ( 'NONE', #205403, 1000.000000000000000 ) ;
#195544 = ORIENTED_EDGE ( 'NONE', *, *, #206805, .T. ) ;
#195543 = ORIENTED_EDGE ( 'NONE', *, *, #53244, .T. ) ;
#195545 = VERTEX_POINT ( 'NONE', #31760 ) ;
#195546 = CARTESIAN_POINT ( 'NONE',  ( 22.44352723754029810, 0.009277095043280617764, 11.64972134534870563 ) ) ;
#195547 = LINE ( 'NONE', #15635, #74899 ) ;
#195548 = CARTESIAN_POINT ( 'NONE',  ( -23.15000000000000213, 85.00000000001251976, -179.4170766071767389 ) ) ;
#195550 = FACE_OUTER_BOUND ( 'NONE', #98858, .T. ) ;
#195549 = DIRECTION ( 'NONE',  ( -1.000000000000000000, 1.335000415235278971E-16, -2.979993593738921214E-16 ) ) ;
#195551 = DIRECTION ( 'NONE',  ( 0.000000000000000000, 0.000000000000000000, 1.000000000000000000 ) ) ;
#195552 = ORIENTED_EDGE ( 'NONE', *, *, #100642, .F. ) ;
#195553 = DIRECTION ( 'NONE',  ( 1.000000000000000000, -0.000000000000000000, -0.000000000000000000 ) ) ;
#195554 = ORIENTED_EDGE ( 'NONE', *, *, #169834, .F. ) ;
#195555 = ORIENTED_EDGE ( 'NONE', *, *, #29689, .T. ) ;
#195556 = CARTESIAN_POINT ( 'NONE',  ( -21.11825140030087766, 69.55459243459189622, -69.53031110515726709 ) ) ;
#195557 = CARTESIAN_POINT ( 'NONE',  ( -22.43310005002225438, 0.005636942152031573783, -88.85033787286563722 ) ) ;
#195558 = CARTESIAN_POINT ( 'NONE',  ( -23.15000000000000213, 76.00000000001253397, -182.8981074845243597 ) ) ;
#195559 = CARTESIAN_POINT ( 'NONE',  ( -18.59999999999999787, 64.40000000001188596, -96.09490425424884563 ) ) ;
#195560 = AXIS2_PLACEMENT_3D ( 'NONE', #154959, #117093, #17974 ) ;
#195561 = CARTESIAN_POINT ( 'NONE',  ( -20.64999999999999858, 54.14029358995846053, -238.9803212882090691 ) ) ;
#195562 = VERTEX_POINT ( 'NONE', #9582 ) ;
#195563 = ORIENTED_EDGE ( 'NONE', *, *, #186778, .F. ) ;
#195564 = CARTESIAN_POINT ( 'NONE',  ( -21.00219873199057474, 11.60538868788778721, -40.41264742829478962 ) ) ;
#195565 = CARTESIAN_POINT ( 'NONE',  ( 23.24999999999999645, 1.115600667400684642E-11, -67.00000000000000000 ) ) ;
#195566 = DIRECTION ( 'NONE',  ( 1.000000000000000000, -0.000000000000000000, -3.469446951953635646E-14 ) ) ;
#195567 = CARTESIAN_POINT ( 'NONE',  ( -20.64999999999999858, 1.999999999999998224, -20.27537807723789953 ) ) ;
#195568 = DIRECTION ( 'NONE',  ( -1.000000000000000000, 0.000000000000000000, 0.000000000000000000 ) ) ;
#195569 = CARTESIAN_POINT ( 'NONE',  ( 20.94999999999999929, 69.19063053712525857, -247.5666987377248631 ) ) ;
#195570 = CARTESIAN_POINT ( 'NONE',  ( 20.94999999999999929, 77.16270174994961906, -61.62310748452431142 ) ) ;
#195572 = DIRECTION ( 'NONE',  ( 0.000000000000000000, -1.000000000000000000, -6.982962677686265922E-15 ) ) ;
#195571 = CARTESIAN_POINT ( 'NONE',  ( -22.41119224318417125, 0.000000000000000000, 11.64957080754479968 ) ) ;
#195574 = EDGE_CURVE ( 'NONE', #197779, #115956, #84411, .T. ) ;
#195573 = CARTESIAN_POINT ( 'NONE',  ( -20.54999999999999716, 65.79629777212066699, -213.4483007241822747 ) ) ;
#195575 = CARTESIAN_POINT ( 'NONE',  ( -21.04999999999999716, 85.60000000001190301, -95.99103808782457747 ) ) ;
#195576 = AXIS2_PLACEMENT_3D ( 'NONE', #257464, #136263, #17612 ) ;
#195577 = AXIS2_PLACEMENT_3D ( 'NONE', #32621, #170866, #212521 ) ;
#195578 = DIRECTION ( 'NONE',  ( -0.7071067811865302533, 0.6909108974501196876, 0.1504730267679053324 ) ) ;
#195579 = DIRECTION ( 'NONE',  ( -1.000000000000000000, 0.000000000000000000, 0.000000000000000000 ) ) ;
#195580 = TOROIDAL_SURFACE ( 'NONE', #83071, 0.4000000000000017431, 0.1000000000000000056 ) ;
#195581 = CIRCLE ( 'NONE', #33271, 0.1000000000000013933 ) ;
#195583 = ORIENTED_EDGE ( 'NONE', *, *, #76572, .T. ) ;
#195582 = DIRECTION ( 'NONE',  ( 0.000000000000000000, 0.000000000000000000, -1.000000000000000000 ) ) ;
#195584 = AXIS2_PLACEMENT_3D ( 'NONE', #135586, #198141, #155203 ) ;
#195585 = EDGE_CURVE ( 'NONE', #75869, #101410, #59487, .T. ) ;
#195586 = CARTESIAN_POINT ( 'NONE',  ( -20.54999999999999716, 2.000000000011154189, -146.7246219227621111 ) ) ;
#195587 = EDGE_LOOP ( 'NONE', ( #180071, #78498 ) ) ;
#195588 = APPLICATION_CONTEXT ( 'automotive_design' ) ;
#195589 = ADVANCED_FACE ( 'NONE', ( #167407 ), #91697, .T. ) ;
#195590 = CARTESIAN_POINT ( 'NONE',  ( -21.53551880898957904, 0.09896973458281840830, -93.71520223858368581 ) ) ;
#195591 = DIRECTION ( 'NONE',  ( -1.000000000000000000, -0.000000000000000000, 0.000000000000000000 ) ) ;
#195592 = AXIS2_PLACEMENT_3D ( 'NONE', #180825, #120873, #2157 ) ;
#195593 = ORIENTED_EDGE ( 'NONE', *, *, #148497, .T. ) ;
#195594 = VECTOR ( 'NONE', #113588, 1000.000000000000114 ) ;
#195595 = CARTESIAN_POINT ( 'NONE',  ( 12.93279065517212878, 9.417690691074257714, -85.14160069676461262 ) ) ;
#195596 = CARTESIAN_POINT ( 'NONE',  ( 22.50000000000000000, 0.1000000000111554016, -21.85042919245520210 ) ) ;
#195597 = EDGE_CURVE ( 'NONE', #67859, #41586, #147831, .T. ) ;
#195598 = AXIS2_PLACEMENT_3D ( 'NONE', #24301, #144203, #88069 ) ;
#195599 = CARTESIAN_POINT ( 'NONE',  ( 18.39999999999999503, 70.35000000001151932, -45.27310748452435973 ) ) ;
#195600 = CARTESIAN_POINT ( 'NONE',  ( 18.49999999999998934, 10.28015861705704737, -24.72457207120110922 ) ) ;
#195601 = FACE_OUTER_BOUND ( 'NONE', #164674, .T. ) ;
#195602 = ADVANCED_FACE ( 'NONE', ( #30458 ), #80548, .T. ) ;
#195604 = ORIENTED_EDGE ( 'NONE', *, *, #100567, .T. ) ;
#195603 = EDGE_CURVE ( 'NONE', #119237, #225819, #209360, .T. ) ;
#195605 = DIRECTION ( 'NONE',  ( 0.000000000000000000, -0.2128009952263604232, 0.9770955615653316162 ) ) ;
#195607 = ORIENTED_EDGE ( 'NONE', *, *, #34925, .T. ) ;
#195606 = LINE ( 'NONE', #119932, #171991 ) ;
#195608 = CYLINDRICAL_SURFACE ( 'NONE', #192414, 0.09999999999999939493 ) ;
#195609 =( BOUNDED_SURFACE ( )  B_SPLINE_SURFACE ( 3, 2, ( 
 ( #11605, #10324, #88533 ),
 ( #151107, #226778, #171990 ),
 ( #230646, #51979, #126395 ),
 ( #251472, #72882, #152413 ) ),
 .UNSPECIFIED., .F., .F., .F. ) 
 B_SPLINE_SURFACE_WITH_KNOTS ( ( 4, 4 ),
 ( 3, 3 ),
 ( 5.727910411845712702, 5.983100554402348337 ),
 ( 0.000000000000000000, 1.000000000000000000 ),
 .UNSPECIFIED. ) 
 GEOMETRIC_REPRESENTATION_ITEM ( )  RATIONAL_B_SPLINE_SURFACE ( (
 ( 1.000000000000000000, 0.8946697475932048338, 1.000000000000000000),
 ( 1.000000000000000000, 0.9035312726220381396, 1.000000000000000000),
 ( 1.000000000000000000, 0.9104333467450170803, 1.000000000000000000),
 ( 1.000000000000000000, 0.9152888060719308605, 1.000000000000000000) ) ) 
 REPRESENTATION_ITEM ( '' )  SURFACE ( )  );
#195610 = CARTESIAN_POINT ( 'NONE',  ( -16.80939487329395021, 9.950000000011138823, -188.3500000000008470 ) ) ;
#195611 = EDGE_CURVE ( 'NONE', #93811, #95210, #155559, .T. ) ;
#195612 = DIRECTION ( 'NONE',  ( -1.000000000000000000, -0.000000000000000000, -0.000000000000000000 ) ) ;
#195613 = VERTEX_POINT ( 'NONE', #115114 ) ;
#195614 = CARTESIAN_POINT ( 'NONE',  ( 23.14999999999999858, 69.35000000001186038, -90.67310748452435121 ) ) ;
#195615 = APPLICATION_PROTOCOL_DEFINITION ( 'draft international standard', 'automotive_design', 1998, #95764 ) ;
#195616 = CARTESIAN_POINT ( 'NONE',  ( -16.27683809663751191, 61.49226340392389289, -221.2952930242537377 ) ) ;
#195618 = EDGE_CURVE ( 'NONE', #185762, #150222, #57687, .T. ) ;
#195617 = LINE ( 'NONE', #16973, #42249 ) ;
#195619 = ORIENTED_EDGE ( 'NONE', *, *, #211675, .F. ) ;
#195620 = CARTESIAN_POINT ( 'NONE',  ( -21.05000000000000071, 77.85102823015316176, -158.3691942151018566 ) ) ;
#195621 = FACE_OUTER_BOUND ( 'NONE', #52308, .T. ) ;
#195622 = AXIS2_PLACEMENT_3D ( 'NONE', #255246, #200469, #41413 ) ;
#195623 = DIRECTION ( 'NONE',  ( 0.000000000000000000, 0.8068669527896844551, 0.5907332058517525963 ) ) ;
#195624 = ORIENTED_EDGE ( 'NONE', *, *, #234518, .F. ) ;
#195625 = VECTOR ( 'NONE', #36801, 1000.000000000000000 ) ;
#195626 = ORIENTED_EDGE ( 'NONE', *, *, #225353, .T. ) ;
#195627 = CARTESIAN_POINT ( 'NONE',  ( -22.50047199487955041, 75.95509394809238302, -114.7731549034439524 ) ) ;
#195628 = DIRECTION ( 'NONE',  ( 0.000000000000000000, -0.000000000000000000, 1.000000000000000000 ) ) ;
#195629 = EDGE_CURVE ( 'NONE', #75529, #49319, #255856, .T. ) ;
#195630 = CARTESIAN_POINT ( 'NONE',  ( -20.54999999999999716, 1.115624548013267999E-11, -65.10000000000000853 ) ) ;
#195631 = DIRECTION ( 'NONE',  ( -1.000000000000000000, -0.000000000000000000, -0.000000000000000000 ) ) ;
#195632 = DIRECTION ( 'NONE',  ( 0.000000000000000000, 0.000000000000000000, -1.000000000000000000 ) ) ;
#195633 = CARTESIAN_POINT ( 'NONE',  ( -20.54999999999999716, -11.74999999998884448, -50.25000000000000000 ) ) ;
#195634 = DIRECTION ( 'NONE',  ( 0.000000000000000000, 0.000000000000000000, 1.000000000000000000 ) ) ;
#195635 = DIRECTION ( 'NONE',  ( 1.000000000000000000, 0.000000000000000000, 0.000000000000000000 ) ) ;
#195636 = CARTESIAN_POINT ( 'NONE',  ( -18.59999999999999787, 64.35000000001230092, -157.8731074845244393 ) ) ;
#195637 = CARTESIAN_POINT ( 'NONE',  ( -20.05000000000000426, 30.22839164850006455, -235.6129688350293350 ) ) ;
#195638 = CIRCLE ( 'NONE', #128985, 0.09999999999999939493 ) ;
#195639 = ORIENTED_EDGE ( 'NONE', *, *, #190017, .F. ) ;
#195640 = VERTEX_POINT ( 'NONE', #232518 ) ;
#195641 = DIRECTION ( 'NONE',  ( -1.000000000000000000, 0.000000000000000000, 0.000000000000000000 ) ) ;
#195642 = AXIS2_PLACEMENT_3D ( 'NONE', #90109, #91422, #169712 ) ;
#195643 = LINE ( 'NONE', #215180, #203503 ) ;
#195645 = CARTESIAN_POINT ( 'NONE',  ( -23.15000000000000213, 1.115600667400684642E-11, -100.5000000000000284 ) ) ;
#195644 = CARTESIAN_POINT ( 'NONE',  ( -21.05000000000000071, 74.14897176987071248, -57.86919421510183525 ) ) ;
#195646 = EDGE_CURVE ( 'NONE', #5925, #197139, #9450, .T. ) ;
#195647 = CIRCLE ( 'NONE', #199741, 0.09999999999999939493 ) ;
#195648 = DIRECTION ( 'NONE',  ( 0.000000000000000000, 0.9651348961777156399, -0.2617529984165037349 ) ) ;
#195649 = CARTESIAN_POINT ( 'NONE',  ( 20.99999999999999645, 9.750000000011137757, -46.15000000000000568 ) ) ;
#195650 = CARTESIAN_POINT ( 'NONE',  ( 15.74999999999999645, 12.72489043187540148, -215.4897534858791630 ) ) ;
#195651 = ORIENTED_EDGE ( 'NONE', *, *, #120012, .F. ) ;
#195652 = AXIS2_PLACEMENT_3D ( 'NONE', #109581, #28826, #31385 ) ;
#195653 = CIRCLE ( 'NONE', #174833, 1.899999999999999023 ) ;
#195654 = EDGE_LOOP ( 'NONE', ( #57528, #153850, #159801 ) ) ;
#195655 = DIRECTION ( 'NONE',  ( -0.000000000000000000, -6.982962677686266711E-15, 1.000000000000000000 ) ) ;
#195656 = ORIENTED_EDGE ( 'NONE', *, *, #238438, .T. ) ;
#195657 = EDGE_CURVE ( 'NONE', #80528, #122105, #34320, .T. ) ;
#195658 = CARTESIAN_POINT ( 'NONE',  ( 18.49999999999999645, -1.299733671219632791, -90.52812952286942050 ) ) ;
#195659 = EDGE_CURVE ( 'NONE', #92784, #138590, #80338, .T. ) ;
#195660 = AXIS2_PLACEMENT_3D ( 'NONE', #32001, #151951, #112803 ) ;
#195661 = CARTESIAN_POINT ( 'NONE',  ( -18.59999999999999787, 7.882824859404637508, -245.3558965132535832 ) ) ;
#195662 = TOROIDAL_SURFACE ( 'NONE', #24802, 0.6000000000000009770, 0.1000000000000000056 ) ;
#195663 = LINE ( 'NONE', #177390, #58964 ) ;
#195664 = VECTOR ( 'NONE', #167943, 1000.000000000000000 ) ;
#195665 = AXIS2_PLACEMENT_3D ( 'NONE', #97497, #196623, #16729 ) ;
#195666 = ORIENTED_EDGE ( 'NONE', *, *, #24142, .T. ) ;
#195667 = CARTESIAN_POINT ( 'NONE',  ( -17.01473183483382101, 9.949999999999983302, -12.75000000000000178 ) ) ;
#195668 = AXIS2_PLACEMENT_3D ( 'NONE', #33589, #70130, #171804 ) ;
#195669 = ADVANCED_FACE ( 'NONE', ( #193387 ), #113688, .T. ) ;
#195670 = ORIENTED_EDGE ( 'NONE', *, *, #112161, .F. ) ;
#195671 = DIRECTION ( 'NONE',  ( 0.000000000000000000, 0.000000000000000000, -1.000000000000000000 ) ) ;
#195672 = FACE_OUTER_BOUND ( 'NONE', #94141, .T. ) ;
#195673 = FACE_OUTER_BOUND ( 'NONE', #150911, .T. ) ;
#195674 = ADVANCED_FACE ( 'NONE', ( #194685 ), #99373, .T. ) ;
#195675 = DIRECTION ( 'NONE',  ( 0.000000000000000000, 0.000000000000000000, 1.000000000000000000 ) ) ;
#195676 = EDGE_CURVE ( 'NONE', #243571, #137205, #17312, .T. ) ;
#195677 = DIRECTION ( 'NONE',  ( 0.000000000000000000, 0.2128009952263606175, -0.9770955615653316162 ) ) ;
#195679 = SPHERICAL_SURFACE ( 'NONE', #62549, 0.1000000000000000056 ) ;
#195678 = FACE_OUTER_BOUND ( 'NONE', #32218, .T. ) ;
#195680 = DIRECTION ( 'NONE',  ( 0.000000000000000000, -6.467318590049456648E-15, 1.000000000000000000 ) ) ;
#195681 = ORIENTED_EDGE ( 'NONE', *, *, #12066, .F. ) ;
#195683 = DIRECTION ( 'NONE',  ( 1.000000000000000000, -0.000000000000000000, 0.000000000000000000 ) ) ;
#195682 = DIRECTION ( 'NONE',  ( 0.000000000000000000, 0.000000000000000000, 1.000000000000000000 ) ) ;
#195684 = ORIENTED_EDGE ( 'NONE', *, *, #164508, .F. ) ;
#195686 = ORIENTED_EDGE ( 'NONE', *, *, #223575, .T. ) ;
#195685 = LINE ( 'NONE', #210103, #73401 ) ;
#195687 = ORIENTED_EDGE ( 'NONE', *, *, #230843, .F. ) ;
#195688 = DIRECTION ( 'NONE',  ( 0.000000000000000000, -0.1298341882520022694, -0.9915357197604853789 ) ) ;
#195689 = CARTESIAN_POINT ( 'NONE',  ( -23.25000000000000000, 1.115600667400684642E-11, -167.4999999999999716 ) ) ;
#195690 = CYLINDRICAL_SURFACE ( 'NONE', #164045, 0.09999999999999939493 ) ;
#195691 = EDGE_CURVE ( 'NONE', #8870, #102921, #236340, .T. ) ;
#195692 = DIRECTION ( 'NONE',  ( -0.000000000000000000, -0.7397360091702755991, -0.6728971962616832059 ) ) ;
#195693 = ORIENTED_EDGE ( 'NONE', *, *, #132410, .T. ) ;
#195694 = DIRECTION ( 'NONE',  ( 1.441126678808781316E-14, -0.5469332180710856361, 0.8371762388950170219 ) ) ;
#195695 = CARTESIAN_POINT ( 'NONE',  ( 18.49999999999999289, 10.32573593129922607, -125.3500000000000512 ) ) ;
#195696 = FACE_OUTER_BOUND ( 'NONE', #141428, .T. ) ;
#195697 = ORIENTED_EDGE ( 'NONE', *, *, #215812, .F. ) ;
#195698 = AXIS2_PLACEMENT_3D ( 'NONE', #8727, #176485, #172668 ) ;
#195699 = DIRECTION ( 'NONE',  ( -3.787827842127534447E-15, 0.5795995782408164265, 0.8149014228132551718 ) ) ;
#195700 = AXIS2_PLACEMENT_3D ( 'NONE', #208597, #130307, #165618 ) ;
#195701 = LINE ( 'NONE', #256875, #43257 ) ;
#195702 = ORIENTED_EDGE ( 'NONE', *, *, #64373, .F. ) ;
#195703 = VERTEX_POINT ( 'NONE', #36898 ) ;
#195704 = DIRECTION ( 'NONE',  ( 1.020425574104004196E-15, -6.982962677686266711E-15, 1.000000000000000000 ) ) ;
#195705 = AXIS2_PLACEMENT_3D ( 'NONE', #40371, #117304, #218956 ) ;
#195706 = ORIENTED_EDGE ( 'NONE', *, *, #127277, .F. ) ;
#195707 = DIRECTION ( 'NONE',  ( 0.000000000000000000, 0.9908441862701420355, 0.1350103645453197554 ) ) ;
#195708 = VERTEX_POINT ( 'NONE', #133400 ) ;
#195709 = DIRECTION ( 'NONE',  ( 0.000000000000000000, -0.9770955615653316162, -0.2128009952263604232 ) ) ;
#195710 =( BOUNDED_SURFACE ( )  B_SPLINE_SURFACE ( 3, 2, ( 
 ( #129903, #90772, #170381 ),
 ( #219713, #99750, #161047 ),
 ( #77615, #178050, #176765 ),
 ( #200170, #42373, #121922 ) ),
 .UNSPECIFIED., .F., .F., .F. ) 
 B_SPLINE_SURFACE_WITH_KNOTS ( ( 4, 4 ),
 ( 3, 3 ),
 ( 0.0006461284895273722425, 0.0007503702773986175179 ),
 ( 0.000000000000000000, 1.000000000000000000 ),
 .UNSPECIFIED. ) 
 GEOMETRIC_REPRESENTATION_ITEM ( )  RATIONAL_B_SPLINE_SURFACE ( (
 ( 1.000000000000000000, 0.7071067811865318076, 1.000000000000000000),
 ( 1.000000000000000000, 0.7076476444648260866, 1.000000000000000000),
 ( 1.000000000000000000, 0.7075727925192434320, 1.000000000000000000),
 ( 1.000000000000000000, 0.7071067811865299202, 1.000000000000000000) ) ) 
 REPRESENTATION_ITEM ( '' )  SURFACE ( )  );
#195711 = EDGE_CURVE ( 'NONE', #206485, #36666, #5336, .T. ) ;
#195712 = CARTESIAN_POINT ( 'NONE',  ( -18.40000000000000213, 61.64185094745226934, -212.6324159020321076 ) ) ;
#195713 = CARTESIAN_POINT ( 'NONE',  ( -11.59999999999994458, 64.25000000001119815, -23.72310748452479245 ) ) ;
#195714 = EDGE_CURVE ( 'NONE', #253449, #137759, #151121, .T. ) ;
#195715 = CARTESIAN_POINT ( 'NONE',  ( 23.14999999999999147, 4.150000000011154988, -33.50000000000000000 ) ) ;
#195716 = AXIS2_PLACEMENT_3D ( 'NONE', #95843, #152019, #136243 ) ;
#195717 = VECTOR ( 'NONE', #122338, 1000.000000000000000 ) ;
#195718 = ADVANCED_FACE ( 'NONE', ( #198495 ), #116407, .T. ) ;
#195719 = CARTESIAN_POINT ( 'NONE',  ( 18.54999999999999716, 67.25000000001178080, -82.17310748452437963 ) ) ;
#195720 = DIRECTION ( 'NONE',  ( 4.408576920032447355E-17, -0.1350103645451876666, -0.9908441862701600211 ) ) ;
#195721 = ORIENTED_EDGE ( 'NONE', *, *, #110116, .T. ) ;
#195724 = CARTESIAN_POINT ( 'NONE',  ( 22.49999999999999645, 64.35023708198022518, -136.6119174609113145 ) ) ;
#195723 = CARTESIAN_POINT ( 'NONE',  ( 21.05000000000000071, 17.11694853917244075, -224.3781540347815451 ) ) ;
#195722 = CIRCLE ( 'NONE', #120895, 0.1000000000000001860 ) ;
#195725 = ORIENTED_EDGE ( 'NONE', *, *, #107609, .T. ) ;
#195728 = ORIENTED_EDGE ( 'NONE', *, *, #155037, .T. ) ;
#195727 = CARTESIAN_POINT ( 'NONE',  ( 21.05000000000000071, 44.37956953460552256, -247.4621105139464419 ) ) ;
#195726 = CARTESIAN_POINT ( 'NONE',  ( 11.60000000000000142, -9.650000000000002132, 15.00000000000000355 ) ) ;
#195729 = VERTEX_POINT ( 'NONE', #137238 ) ;
#195730 = DIRECTION ( 'NONE',  ( 0.000000000000000000, 0.01283462868040226822, 0.9999176327611370985 ) ) ;
#195731 = CARTESIAN_POINT ( 'NONE',  ( 13.43443725621852103, 66.55344247693975035, -154.9331655301785133 ) ) ;
#195732 = DIRECTION ( 'NONE',  ( 0.000000000000000000, -7.147358527629766941E-15, 1.000000000000000000 ) ) ;
#195733 = CARTESIAN_POINT ( 'NONE',  ( 15.74999999999999645, 9.350000000011139178, -117.2500000000000284 ) ) ;
#195734 = EDGE_LOOP ( 'NONE', ( #130660, #39931, #52198, #247740 ) ) ;
#195736 = ORIENTED_EDGE ( 'NONE', *, *, #92045, .F. ) ;
#195735 = DIRECTION ( 'NONE',  ( 0.000000000000000000, 0.000000000000000000, -1.000000000000000000 ) ) ;
#195737 = CARTESIAN_POINT ( 'NONE',  ( -18.50000000000000000, 11.75000000001115197, -33.60000000000000142 ) ) ;
#195739 = LINE ( 'NONE', #99153, #254880 ) ;
#195738 = CARTESIAN_POINT ( 'NONE',  ( -21.14999999999999858, 64.35000000001268461, -203.4231074845244507 ) ) ;
#195741 = ORIENTED_EDGE ( 'NONE', *, *, #160379, .F. ) ;
#195740 = DIRECTION ( 'NONE',  ( 1.000000000000000000, -2.986185139342066440E-16, 6.665775143889694746E-16 ) ) ;
#195742 = CIRCLE ( 'NONE', #203897, 0.1999999999999987899 ) ;
#195743 = AXIS2_PLACEMENT_3D ( 'NONE', #93048, #90472, #72223 ) ;
#195744 = ORIENTED_EDGE ( 'NONE', *, *, #28494, .T. ) ;
#195745 = EDGE_CURVE ( 'NONE', #190290, #23758, #142716, .T. ) ;
#195746 = DIRECTION ( 'NONE',  ( 1.000000000000000000, 0.000000000000000000, 0.000000000000000000 ) ) ;
#195747 = EDGE_LOOP ( 'NONE', ( #44000, #37416, #174049 ) ) ;
#195748 = DIRECTION ( 'NONE',  ( 0.000000000000000000, 0.2617529984165152257, 0.9651348961777124202 ) ) ;
#195749 = ORIENTED_EDGE ( 'NONE', *, *, #36511, .F. ) ;
#195750 = EDGE_CURVE ( 'NONE', #242609, #146650, #213838, .T. ) ;
#195751 = CARTESIAN_POINT ( 'NONE',  ( -20.64999999999999858, 1.115600667400684642E-11, -167.4999999999999716 ) ) ;
#195752 = CARTESIAN_POINT ( 'NONE',  ( 23.14999999999999503, 11.65000000001116298, -121.8500000000000369 ) ) ;
#195753 = ORIENTED_EDGE ( 'NONE', *, *, #182, .F. ) ;
#195754 = DIRECTION ( 'NONE',  ( -6.938893903907222856E-15, -0.9651348961777158619, 0.2617529984165028467 ) ) ;
#195755 = EDGE_CURVE ( 'NONE', #22457, #56611, #35611, .T. ) ;
#195756 = VECTOR ( 'NONE', #195991, 1000.000000000000000 ) ;
#195757 = AXIS2_PLACEMENT_3D ( 'NONE', #133599, #93189, #196146 ) ;
#195758 = EDGE_CURVE ( 'NONE', #183157, #205018, #58954, .T. ) ;
#195759 = VECTOR ( 'NONE', #215998, 1000.000000000000000 ) ;
#195760 = AXIS2_PLACEMENT_3D ( 'NONE', #239488, #179525, #204188 ) ;
#195761 = CARTESIAN_POINT ( 'NONE',  ( -16.81931177881022776, 9.936996059515061930, -54.27321787861723834 ) ) ;
#195762 = EDGE_CURVE ( 'NONE', #218186, #41308, #22454, .T. ) ;
#195763 = ORIENTED_EDGE ( 'NONE', *, *, #187524, .F. ) ;
#195764 = CIRCLE ( 'NONE', #45898, 0.1000000000000028644 ) ;
#195765 = ORIENTED_EDGE ( 'NONE', *, *, #161085, .T. ) ;
#195768 = EDGE_CURVE ( 'NONE', #13313, #75395, #204901, .T. ) ;
#195767 = EDGE_CURVE ( 'NONE', #228728, #243879, #178979, .T. ) ;
#195766 = CARTESIAN_POINT ( 'NONE',  ( 20.77526135991734080, 18.81146737447475203, -229.8579754828443811 ) ) ;
#195769 = ORIENTED_EDGE ( 'NONE', *, *, #172412, .F. ) ;
#195770 = EDGE_LOOP ( 'NONE', ( #71909, #13258, #212304, #137634 ) ) ;
#195772 = VERTEX_POINT ( 'NONE', #160693 ) ;
#195771 = CARTESIAN_POINT ( 'NONE',  ( 18.59999999999999432, -1.135018845899022466, -141.7169768834323520 ) ) ;
#195773 = ORIENTED_EDGE ( 'NONE', *, *, #244331, .T. ) ;
#195774 = CARTESIAN_POINT ( 'NONE',  ( 20.73486653747088937, 7.750000000011182166, -154.8500000000000227 ) ) ;
#195775 = CIRCLE ( 'NONE', #79200, 0.8750000000000007772 ) ;
#195778 = ORIENTED_EDGE ( 'NONE', *, *, #220416, .F. ) ;
#195777 = ORIENTED_EDGE ( 'NONE', *, *, #173598, .T. ) ;
#195776 = CARTESIAN_POINT ( 'NONE',  ( -33.72168855820452649, 11.47316190337362585, -76.25000000000004263 ) ) ;
#195779 = AXIS2_PLACEMENT_3D ( 'NONE', #153752, #14208, #209823 ) ;
#195780 = ORIENTED_EDGE ( 'NONE', *, *, #171993, .T. ) ;
#195781 = FACE_OUTER_BOUND ( 'NONE', #66808, .T. ) ;
#195782 = ADVANCED_FACE ( 'NONE', ( #120287 ), #221987, .T. ) ;
#195783 = EDGE_CURVE ( 'NONE', #166894, #23645, #72204, .T. ) ;
#195784 = LINE ( 'NONE', #78361, #113876 ) ;
#195785 = DIRECTION ( 'NONE',  ( 0.000000000000000000, 1.000000000000000000, 0.000000000000000000 ) ) ;
#195786 = ORIENTED_EDGE ( 'NONE', *, *, #145605, .F. ) ;
#195787 = EDGE_CURVE ( 'NONE', #224814, #221149, #32868, .T. ) ;
#195788 = DIRECTION ( 'NONE',  ( 0.000000000000000000, 0.000000000000000000, 1.000000000000000000 ) ) ;
#195790 = VERTEX_POINT ( 'NONE', #164523 ) ;
#195789 = DIRECTION ( 'NONE',  ( 1.000000000000000000, 0.000000000000000000, 0.000000000000000000 ) ) ;
#195791 = DIRECTION ( 'NONE',  ( 1.000000000000000000, 0.000000000000000000, 0.000000000000000000 ) ) ;
#195792 = ORIENTED_EDGE ( 'NONE', *, *, #238538, .T. ) ;
#195793 = EDGE_LOOP ( 'NONE', ( #74277, #169198, #196158, #217157 ) ) ;
#195795 = ADVANCED_FACE ( 'NONE', ( #244033 ), #43284, .F. ) ;
#195794 = CARTESIAN_POINT ( 'NONE',  ( 18.42555734704284731, 85.49715836194830842, -62.48327698678934183 ) ) ;
#195796 = FACE_OUTER_BOUND ( 'NONE', #16133, .T. ) ;
#195797 = ORIENTED_EDGE ( 'NONE', *, *, #103447, .T. ) ;
#195798 = ADVANCED_FACE ( 'NONE', ( #238916 ), #255284, .T. ) ;
#195799 = ORIENTED_EDGE ( 'NONE', *, *, #107671, .F. ) ;
#195801 = AXIS2_PLACEMENT_3D ( 'NONE', #52934, #172937, #251119 ) ;
#195800 = PLANE ( 'NONE',  #226743 ) ;
#195802 = FACE_OUTER_BOUND ( 'NONE', #30306, .T. ) ;
#195804 = EDGE_LOOP ( 'NONE', ( #5276, #234934, #231067, #74987 ) ) ;
#195803 = VERTEX_POINT ( 'NONE', #199806 ) ;
#195805 = ORIENTED_EDGE ( 'NONE', *, *, #214497, .T. ) ;
#195806 = DIRECTION ( 'NONE',  ( 1.000000000000000000, 0.000000000000000000, 0.000000000000000000 ) ) ;
#195807 = ORIENTED_EDGE ( 'NONE', *, *, #207806, .T. ) ;
#195808 = ORIENTED_EDGE ( 'NONE', *, *, #12581, .T. ) ;
#195809 = DIRECTION ( 'NONE',  ( 0.000000000000000000, 1.000000000000000000, 0.000000000000000000 ) ) ;
#195810 = CIRCLE ( 'NONE', #41678, 0.09999999999999939493 ) ;
#195811 = ORIENTED_EDGE ( 'NONE', *, *, #3357, .F. ) ;
#195812 = EDGE_CURVE ( 'NONE', #215983, #90102, #163237, .T. ) ;
#195813 = FACE_OUTER_BOUND ( 'NONE', #214925, .T. ) ;
#195815 = CARTESIAN_POINT ( 'NONE',  ( -22.48970261584618058, 64.35000000001268461, -203.5784769727418393 ) ) ;
#195814 = CYLINDRICAL_SURFACE ( 'NONE', #136241, 1.500000000000001332 ) ;
#195816 = VERTEX_POINT ( 'NONE', #62838 ) ;
#195817 = ORIENTED_EDGE ( 'NONE', *, *, #40915, .F. ) ;
#195818 = EDGE_CURVE ( 'NONE', #176136, #121787, #217901, .T. ) ;
#195819 = DIRECTION ( 'NONE',  ( 1.000000000000000000, 0.000000000000000000, 0.000000000000000000 ) ) ;
#195821 = ORIENTED_EDGE ( 'NONE', *, *, #40804, .T. ) ;
#195820 = VECTOR ( 'NONE', #61249, 1000.000000000000000 ) ;
#195822 = AXIS2_PLACEMENT_3D ( 'NONE', #114825, #24746, #26006 ) ;
#195823 = DIRECTION ( 'NONE',  ( -0.000000000000000000, -0.8660254037844420383, 0.4999999999999943379 ) ) ;
#195824 = ORIENTED_EDGE ( 'NONE', *, *, #104963, .F. ) ;
#195825 = ORIENTED_EDGE ( 'NONE', *, *, #77062, .F. ) ;
#195826 = VECTOR ( 'NONE', #46098, 1000.000000000000000 ) ;
#195827 = DIRECTION ( 'NONE',  ( -1.000000000000000000, 0.000000000000000000, -0.000000000000000000 ) ) ;
#195828 = ADVANCED_FACE ( 'NONE', ( #122833 ), #151321, .F. ) ;
#195830 = ORIENTED_EDGE ( 'NONE', *, *, #174806, .F. ) ;
#195829 = CARTESIAN_POINT ( 'NONE',  ( 18.40000000000000213, 85.50000000001233502, -162.9910380878246485 ) ) ;
#195831 = CARTESIAN_POINT ( 'NONE',  ( 20.94999999999999929, -1.835341550213257733, -45.05515129256298223 ) ) ;
#195832 = DIRECTION ( 'NONE',  ( 1.000000000000000000, 0.000000000000000000, 0.000000000000000000 ) ) ;
#195833 = EDGE_LOOP ( 'NONE', ( #150096, #204813, #224365, #63351 ) ) ;
#195834 = AXIS2_PLACEMENT_3D ( 'NONE', #49310, #187567, #88412 ) ;
#195835 = CYLINDRICAL_SURFACE ( 'NONE', #49623, 0.1000000000000124678 ) ;
#195836 = DIRECTION ( 'NONE',  ( 0.000000000000000000, -6.982962677686266711E-15, 1.000000000000000000 ) ) ;
#195837 = FACE_OUTER_BOUND ( 'NONE', #248532, .T. ) ;
#195838 = CARTESIAN_POINT ( 'NONE',  ( -20.85000000000000142, 70.29876110920605470, -198.0544810472949564 ) ) ;
#195839 = CARTESIAN_POINT ( 'NONE',  ( -16.92989507731676824, 63.02487450102639599, -213.3520164823955838 ) ) ;
#195840 = DIRECTION ( 'NONE',  ( 0.000000000000000000, 0.000000000000000000, 1.000000000000000000 ) ) ;
#195841 = DIRECTION ( 'NONE',  ( 0.000000000000000000, -6.982962677686266711E-15, 1.000000000000000000 ) ) ;
#195842 = DIRECTION ( 'NONE',  ( -3.265361837132813093E-16, 1.000000000000000000, 0.000000000000000000 ) ) ;
#195843 = ORIENTED_EDGE ( 'NONE', *, *, #122167, .T. ) ;
#195844 = CIRCLE ( 'NONE', #75046, 0.1000000000000053069 ) ;
#195845 = AXIS2_PLACEMENT_3D ( 'NONE', #118018, #95874, #94595 ) ;
#195846 = VECTOR ( 'NONE', #104131, 1000.000000000000000 ) ;
#195847 = VECTOR ( 'NONE', #119873, 1000.000000000000227 ) ;
#195848 = TOROIDAL_SURFACE ( 'NONE', #175027, 0.6000000000000009770, 0.1000000000000000056 ) ;
#195850 = ORIENTED_EDGE ( 'NONE', *, *, #18487, .T. ) ;
#195849 = EDGE_LOOP ( 'NONE', ( #243902, #21618, #210184, #8779 ) ) ;
#195851 = ORIENTED_EDGE ( 'NONE', *, *, #75402, .F. ) ;
#195852 = DIRECTION ( 'NONE',  ( 0.000000000000000000, -6.982962677686266711E-15, 1.000000000000000000 ) ) ;
#195853 = DIRECTION ( 'NONE',  ( -1.000000000000000000, 0.000000000000000000, 0.000000000000000000 ) ) ;
#195855 = CARTESIAN_POINT ( 'NONE',  ( -20.54999999999999716, 85.40000000001207070, -126.6291383618717816 ) ) ;
#195854 = DIRECTION ( 'NONE',  ( -0.4999999999999799050, 0.000000000000000000, -0.8660254037844502539 ) ) ;
#195856 = EDGE_LOOP ( 'NONE', ( #167025, #212444, #231724, #62384 ) ) ;
#195857 = LINE ( 'NONE', #129749, #46525 ) ;
#195858 = AXIS2_PLACEMENT_3D ( 'NONE', #150842, #173027, #231684 ) ;
#195859 = CARTESIAN_POINT ( 'NONE',  ( -23.15000000000000213, 74.00000000001180922, -82.74772940728641402 ) ) ;
#195860 = PLANE ( 'NONE',  #59739 ) ;
#195861 = CARTESIAN_POINT ( 'NONE',  ( -18.40000000000000213, 11.75000000001113953, -158.2500000000000284 ) ) ;
#195862 = VERTEX_POINT ( 'NONE', #60263 ) ;
#195863 = EDGE_LOOP ( 'NONE', ( #155413, #67678, #151253, #75426 ) ) ;
#195864 = CARTESIAN_POINT ( 'NONE',  ( -20.54999999999999716, 85.00000000001149658, -45.91707660717669626 ) ) ;
#195865 = VERTEX_POINT ( 'NONE', #40748 ) ;
#195866 = DIRECTION ( 'NONE',  ( 0.000000000000000000, -0.5859227990963362664, -0.8103668758649469339 ) ) ;
#195867 = DIRECTION ( 'NONE',  ( 1.000000000000000000, 0.000000000000000000, -0.000000000000000000 ) ) ;
#195868 = DIRECTION ( 'NONE',  ( -0.000000000000000000, 1.000000000000000000, 6.982962677686266711E-15 ) ) ;
#195869 = CARTESIAN_POINT ( 'NONE',  ( 21.14999999999999858, -11.64999999998883595, -67.00000000000004263 ) ) ;
#195870 = CARTESIAN_POINT ( 'NONE',  ( 18.49999999999998934, 19.88098775990103562, -199.0038892813511779 ) ) ;
#195871 = ORIENTED_EDGE ( 'NONE', *, *, #246538, .F. ) ;
#195872 = DIRECTION ( 'NONE',  ( -0.000000000000000000, -0.9594490217226112616, -0.2818822000686178608 ) ) ;
#195873 = CARTESIAN_POINT ( 'NONE',  ( 20.04142135623730070, 11.65000000001115943, -88.35000000000003695 ) ) ;
#195874 = AXIS2_PLACEMENT_3D ( 'NONE', #197301, #103328, #99467 ) ;
#195875 = CARTESIAN_POINT ( 'NONE',  ( -23.15000000000000213, 1.115600667400684642E-11, -138.1500000000000057 ) ) ;
#195877 = CYLINDRICAL_SURFACE ( 'NONE', #91207, 0.1000000000000001443 ) ;
#195876 = CARTESIAN_POINT ( 'NONE',  ( -20.94999999999999929, 7.021664781911246322, -171.1335654018973003 ) ) ;
#195879 = EDGE_CURVE ( 'NONE', #229929, #52, #100647, .T. ) ;
#195878 = CARTESIAN_POINT ( 'NONE',  ( -23.25000000000000000, -11.74999999998884448, -63.89999999999999858 ) ) ;
#195880 = TOROIDAL_SURFACE ( 'NONE', #83391, 11.65000000000000036, 0.1000000000000000056 ) ;
#195881 = CARTESIAN_POINT ( 'NONE',  ( -23.15000000000000213, 11.75000000001115907, -194.1583993101029364 ) ) ;
#195882 = CARTESIAN_POINT ( 'NONE',  ( -20.64999999999999858, 74.05981308412400210, -90.19398827347099257 ) ) ;
#195884 = ORIENTED_EDGE ( 'NONE', *, *, #39966, .F. ) ;
#195883 = AXIS2_PLACEMENT_3D ( 'NONE', #7625, #224086, #203250 ) ;
#195885 = ORIENTED_EDGE ( 'NONE', *, *, #167132, .T. ) ;
#195886 = VERTEX_POINT ( 'NONE', #184065 ) ;
#195887 = ADVANCED_FACE ( 'NONE', ( #180234 ), #97073, .T. ) ;
#195888 = DIRECTION ( 'NONE',  ( 0.000000000000000000, 0.1298341882519953583, 0.9915357197604862671 ) ) ;
#195889 = CIRCLE ( 'NONE', #254108, 0.3999999999999975797 ) ;
#195890 = EDGE_CURVE ( 'NONE', #92094, #170589, #1566, .T. ) ;
#195891 = AXIS2_PLACEMENT_3D ( 'NONE', #87692, #69454, #146376 ) ;
#195892 = PRESENTATION_STYLE_ASSIGNMENT (( #231174 ) ) ;
#195893 = DIRECTION ( 'NONE',  ( -1.000000000000000000, 8.623019343401632876E-17, 8.389849937938899189E-16 ) ) ;
#195894 = VECTOR ( 'NONE', #180426, 1000.000000000000000 ) ;
#195895 = EDGE_LOOP ( 'NONE', ( #192358, #178515, #72081, #23003 ) ) ;
#195896 = VECTOR ( 'NONE', #83585, 1000.000000000000000 ) ;
#195897 = CARTESIAN_POINT ( 'NONE',  ( 20.46382478191414833, 67.09862044131001824, -194.9773793896413281 ) ) ;
#195898 = FACE_OUTER_BOUND ( 'NONE', #7722, .T. ) ;
#195899 = DIRECTION ( 'NONE',  ( 1.000000000000000000, 0.000000000000000000, 0.000000000000000000 ) ) ;
#195900 = ADVANCED_FACE ( 'NONE', ( #84930 ), #121567, .T. ) ;
#195901 = EDGE_CURVE ( 'NONE', #19454, #158664, #122073, .T. ) ;
#195902 = DIRECTION ( 'NONE',  ( 0.000000000000000000, -1.000000000000000000, -0.000000000000000000 ) ) ;
#195904 = EDGE_LOOP ( 'NONE', ( #160930, #143810, #174360, #10437 ) ) ;
#195903 = CARTESIAN_POINT ( 'NONE',  ( 20.94999999999999574, 74.83729825007462466, -195.5231074845243597 ) ) ;
#195906 = DIRECTION ( 'NONE',  ( 0.000000000000000000, -0.9656312546561486299, -0.2599159095384356855 ) ) ;
#195905 = CARTESIAN_POINT ( 'NONE',  ( 21.11833042828174456, 6.296499826410054013, -199.6214225183865665 ) ) ;
#195907 = CARTESIAN_POINT ( 'NONE',  ( -18.50000000000000000, 1.115600667400684642E-11, -134.0000000000000284 ) ) ;
#195908 = CARTESIAN_POINT ( 'NONE',  ( 23.14999999999999858, 0.000000000000000000, -33.50000000000000000 ) ) ;
#195910 = ADVANCED_FACE ( 'NONE', ( #245336 ), #6713, .F. ) ;
#195909 = CARTESIAN_POINT ( 'NONE',  ( -19.96434256916585070, 5.572646937746800866, 16.50000000334722117 ) ) ;
#195911 = CARTESIAN_POINT ( 'NONE',  ( 23.14999999999999503, 11.75000000001116263, -126.9851942293460922 ) ) ;
#195912 = ORIENTED_EDGE ( 'NONE', *, *, #201402, .F. ) ;
#195913 = DIRECTION ( 'NONE',  ( 0.000000000000000000, 0.000000000000000000, -1.000000000000000000 ) ) ;
#195914 = CIRCLE ( 'NONE', #212475, 4.300000000000025580 ) ;
#195915 = EDGE_CURVE ( 'NONE', #38481, #246420, #197063, .T. ) ;
#195916 = AXIS2_PLACEMENT_3D ( 'NONE', #140873, #125167, #200846 ) ;
#195917 = ORIENTED_EDGE ( 'NONE', *, *, #161872, .F. ) ;
#195918 = CARTESIAN_POINT ( 'NONE',  ( 18.49999999999998934, 66.47189219944506533, -213.6315278230738102 ) ) ;
#195920 = ORIENTED_EDGE ( 'NONE', *, *, #136189, .F. ) ;
#195919 = B_SPLINE_CURVE_WITH_KNOTS ( 'NONE', 3,
 ( #89400, #166416, #145523, #64712, #144229, #227626, #188509, #48995, #223771, #245927, #85523, #244624, #107685, #168991, #149410, #128541, #45148, #165101, #67278, #225047, #228929, #46419, #146795, #205496, #26905, #226326, #47703, #127257, #206795, #56663 ),
 .UNSPECIFIED., .F., .F.,
 ( 4, 2, 2, 2, 2, 2, 2, 2, 2, 2, 2, 2, 2, 2, 4 ),
 ( 0.000000000000000000, 0.0003422764154113355664, 0.0006845528308226711328, 0.001026829246234006862, 0.001369105661645342266, 0.002053658492468009387, 0.002738211323290676725, 0.003080487738702010828, 0.003422764154113344063, 0.003765040569524678166, 0.004107316984936011835, 0.004449593400347345504, 0.004791869815758679173, 0.005134146231170016311, 0.005476422646581353450 ),
 .UNSPECIFIED. ) ;
#195921 = CARTESIAN_POINT ( 'NONE',  ( 18.49999999999999289, 55.02897297050080994, -230.1354412432072536 ) ) ;
#195922 = EDGE_CURVE ( 'NONE', #200926, #180867, #126663, .T. ) ;
#195923 = CARTESIAN_POINT ( 'NONE',  ( 22.39999999999999503, 75.90000000001273861, -209.7731074845243597 ) ) ;
#195924 = CARTESIAN_POINT ( 'NONE',  ( -20.94999999999999929, 70.15854073567089699, -198.1993227616376885 ) ) ;
#195925 = ORIENTED_EDGE ( 'NONE', *, *, #53744, .T. ) ;
#195926 = ORIENTED_EDGE ( 'NONE', *, *, #90457, .F. ) ;
#195927 = EDGE_CURVE ( 'NONE', #251583, #80091, #55385, .T. ) ;
#195928 = CARTESIAN_POINT ( 'NONE',  ( 21.08489247129320887, 8.877675190881227252, -112.8500000000000654 ) ) ;
#195929 = CARTESIAN_POINT ( 'NONE',  ( 20.95443524775735611, 10.49118055759163504, -207.4488969755982737 ) ) ;
#195930 = TOROIDAL_SURFACE ( 'NONE', #158516, 4.099999999999999645, 0.1000000000000000056 ) ;
#195931 = DIRECTION ( 'NONE',  ( -0.000000000000000000, -0.000000000000000000, 1.000000000000000000 ) ) ;
#195933 = FACE_OUTER_BOUND ( 'NONE', #12972, .T. ) ;
#195932 = AXIS2_PLACEMENT_3D ( 'NONE', #28821, #67894, #209986 ) ;
#195936 = DIRECTION ( 'NONE',  ( 1.000000000000000000, 0.000000000000000000, 0.000000000000000000 ) ) ;
#195935 = CIRCLE ( 'NONE', #25244, 0.1000000000000028644 ) ;
#195934 = CARTESIAN_POINT ( 'NONE',  ( -21.07094088545368749, 75.90110629745997528, -142.8432747064414343 ) ) ;
#195937 = DIRECTION ( 'NONE',  ( 0.000000000000000000, 0.000000000000000000, 1.000000000000000000 ) ) ;
#195938 = CARTESIAN_POINT ( 'NONE',  ( -21.14999999999994174, 74.16448838626247664, -47.52760213295649550 ) ) ;
#195939 = CARTESIAN_POINT ( 'NONE',  ( -17.29158576265543346, 31.48883999867549477, -235.0235465672944031 ) ) ;
#195940 = ORIENTED_EDGE ( 'NONE', *, *, #127605, .T. ) ;
#195941 = DIRECTION ( 'NONE',  ( 0.000000000000000000, 1.000000000000000000, -6.308085367188393199E-16 ) ) ;
#195943 = EDGE_LOOP ( 'NONE', ( #15848, #176984, #41336, #26791 ) ) ;
#195942 = CARTESIAN_POINT ( 'NONE',  ( -23.15000000000000213, 64.35000000001222986, -148.6731074845244507 ) ) ;
#195944 = TOROIDAL_SURFACE ( 'NONE', #237625, 0.4000000000000012990, 0.1000000000000000056 ) ;
#195945 = DIRECTION ( 'NONE',  ( 1.000000000000000000, 0.000000000000000000, 0.000000000000000000 ) ) ;
#195946 = LINE ( 'NONE', #17302, #186586 ) ;
#195948 = DIRECTION ( 'NONE',  ( 0.000000000000000000, 0.000000000000000000, 1.000000000000000000 ) ) ;
#195947 = DIRECTION ( 'NONE',  ( -0.000000000000000000, -1.000000000000000000, -0.000000000000000000 ) ) ;
#195949 = VERTEX_POINT ( 'NONE', #15393 ) ;
#195951 = CARTESIAN_POINT ( 'NONE',  ( -18.59999999999999787, 38.29773864426884700, -236.0513742605307925 ) ) ;
#195950 = CARTESIAN_POINT ( 'NONE',  ( 20.94999999999999929, 49.36776662947724503, -253.7196102226803021 ) ) ;
#195952 = CARTESIAN_POINT ( 'NONE',  ( -20.05000000000000426, 61.53642629385834795, -221.5144953033309321 ) ) ;
#195953 = CARTESIAN_POINT ( 'NONE',  ( -18.50000000000000000, 85.40000000001209912, -129.6084491415546154 ) ) ;
#195954 = DIRECTION ( 'NONE',  ( 0.000000000000000000, 0.9654727137038726648, -0.2605042016806632943 ) ) ;
#195955 = CARTESIAN_POINT ( 'NONE',  ( 21.05000000000000071, 65.57661458509942065, -162.5310555606543232 ) ) ;
#195956 = EDGE_LOOP ( 'NONE', ( #190740, #34053, #52988 ) ) ;
#195957 = CARTESIAN_POINT ( 'NONE',  ( 23.14999999999999503, 69.55000000001223270, -148.2731074845243597 ) ) ;
#195959 = ORIENTED_EDGE ( 'NONE', *, *, #172170, .T. ) ;
#195958 = TOROIDAL_SURFACE ( 'NONE', #54459, 0.6000000000000013101, 0.1000000000000000056 ) ;
#195960 = LINE ( 'NONE', #79817, #184160 ) ;
#195961 = EDGE_LOOP ( 'NONE', ( #99734, #204628, #93694, #20804 ) ) ;
#195962 = CARTESIAN_POINT ( 'NONE',  ( -18.59999999999999787, -9.849999999999996092, 31.39999999999999858 ) ) ;
#195963 = ORIENTED_EDGE ( 'NONE', *, *, #100465, .T. ) ;
#195964 = EDGE_CURVE ( 'NONE', #142228, #113101, #30513, .T. ) ;
#195965 = SPHERICAL_SURFACE ( 'NONE', #60066, 0.1000000000000000056 ) ;
#195966 = PLANE ( 'NONE',  #247079 ) ;
#195967 = VERTEX_POINT ( 'NONE', #88796 ) ;
#195968 = EDGE_CURVE ( 'NONE', #16790, #5236, #42972, .T. ) ;
#195969 = AXIS2_PLACEMENT_3D ( 'NONE', #183410, #59564, #202961 ) ;
#195970 = EDGE_CURVE ( 'NONE', #220454, #82222, #80517, .T. ) ;
#195971 = CARTESIAN_POINT ( 'NONE',  ( -21.30740335185486600, -1.298594845133715259, -194.5724652801384309 ) ) ;
#195972 = CARTESIAN_POINT ( 'NONE',  ( 21.14999999999999503, 87.75000000001222134, -148.2731074845242176 ) ) ;
#195973 = ADVANCED_FACE ( 'NONE', ( #247892 ), #207506, .T. ) ;
#195974 = DIRECTION ( 'NONE',  ( 0.000000000000000000, 0.000000000000000000, -1.000000000000000000 ) ) ;
#195975 = EDGE_CURVE ( 'NONE', #195703, #100848, #251222, .T. ) ;
#195976 = CARTESIAN_POINT ( 'NONE',  ( -17.11825945287482753, 60.96553306590055854, -220.9452142459683159 ) ) ;
#195978 = LINE ( 'NONE', #233813, #19736 ) ;
#195977 = AXIS2_PLACEMENT_3D ( 'NONE', #1934, #21535, #223553 ) ;
#195979 = ADVANCED_FACE ( 'NONE', ( #135304 ), #176257, .F. ) ;
#195980 = ORIENTED_EDGE ( 'NONE', *, *, #144939, .T. ) ;
#195982 = EDGE_CURVE ( 'NONE', #72990, #200797, #63817, .T. ) ;
#195981 = CARTESIAN_POINT ( 'NONE',  ( -23.15000000000000213, 15.92646454033039660, -219.3818586450342707 ) ) ;
#195983 = ORIENTED_EDGE ( 'NONE', *, *, #132511, .T. ) ;
#195985 = ORIENTED_EDGE ( 'NONE', *, *, #165170, .F. ) ;
#195984 = DIRECTION ( 'NONE',  ( 0.000000000000000000, 0.4721928772777346239, 0.8814952561688430555 ) ) ;
#195986 = ORIENTED_EDGE ( 'NONE', *, *, #238557, .F. ) ;
#195987 = CARTESIAN_POINT ( 'NONE',  ( -0.8999999999999994671, -8.250000000000005329, 21.95857864376268864 ) ) ;
#195988 = CARTESIAN_POINT ( 'NONE',  ( 23.24999999999999645, 1.148907358139439339E-11, -201.0000000000015064 ) ) ;
#195989 = LINE ( 'NONE', #218078, #122173 ) ;
#195990 = EDGE_CURVE ( 'NONE', #53585, #52602, #113882, .T. ) ;
#195991 = DIRECTION ( 'NONE',  ( -1.000000000000000000, -0.000000000000000000, -0.000000000000000000 ) ) ;
#195992 = ORIENTED_EDGE ( 'NONE', *, *, #243645, .T. ) ;
#195993 = CYLINDRICAL_SURFACE ( 'NONE', #18833, 0.1000000000000028644 ) ;
#195994 = EDGE_LOOP ( 'NONE', ( #190333, #58286, #52751, #95030 ) ) ;
#195996 = VERTEX_POINT ( 'NONE', #233166 ) ;
#195995 = DIRECTION ( 'NONE',  ( -1.000000000000000000, -0.000000000000000000, -0.000000000000000000 ) ) ;
#195997 = DIRECTION ( 'NONE',  ( 0.000000000000000000, 0.000000000000000000, -1.000000000000000000 ) ) ;
#195998 = CARTESIAN_POINT ( 'NONE',  ( -16.85697194749131711, 9.908543714134740554, -79.93500426761436017 ) ) ;
#195999 = AXIS2_PLACEMENT_3D ( 'NONE', #237013, #137882, #156216 ) ;
#196000 = VECTOR ( 'NONE', #73829, 1000.000000000000000 ) ;
#196001 = ADVANCED_FACE ( 'NONE', ( #108392 ), #209551, .F. ) ;
#196002 = DIRECTION ( 'NONE',  ( 1.000000000000000000, 0.000000000000000000, 0.000000000000000000 ) ) ;
#196003 = ORIENTED_EDGE ( 'NONE', *, *, #195818, .F. ) ;
#196004 = CIRCLE ( 'NONE', #12848, 0.09999999999999939493 ) ;
#196005 = EDGE_CURVE ( 'NONE', #212748, #30860, #75378, .T. ) ;
#196006 = LINE ( 'NONE', #30833, #168740 ) ;
#196007 = CARTESIAN_POINT ( 'NONE',  ( 13.12229106158772929, 66.56936289831479314, -51.25484686646344556 ) ) ;
#196008 = ADVANCED_FACE ( 'NONE', ( #214854 ), #53927, .F. ) ;
#196009 = AXIS2_PLACEMENT_3D ( 'NONE', #17271, #154249, #173823 ) ;
#196010 = CIRCLE ( 'NONE', #42077, 0.09999999999999971412 ) ;
#196011 = CARTESIAN_POINT ( 'NONE',  ( -18.59999999999999787, 59.07123845373075710, -221.0531397865252075 ) ) ;
#196012 = B_SPLINE_CURVE_WITH_KNOTS ( 'NONE', 3,
 ( #29921, #229393, #67738, #66454, #148566, #106847, #187706, #168168, #145980, #147270, #183832, #246379, #70342, #207269, #226805, #169448, #228110, #208552, #48165 ),
 .UNSPECIFIED., .F., .F.,
 ( 4, 3, 3, 3, 3, 3, 4 ),
 ( 0.000000000000000000, 7.110282409889993145E-05, 0.0001508797727291377874, 0.0002027344179858592635, 0.0002343294522349093773, 0.0002454816334821335877, 0.0002619873080085596676 ),
 .UNSPECIFIED. ) ;
#196013 = AXIS2_PLACEMENT_3D ( 'NONE', #119589, #96133, #17886 ) ;
#196014 = AXIS2_PLACEMENT_3D ( 'NONE', #245410, #103298, #26361 ) ;
#196015 = VECTOR ( 'NONE', #234359, 1000.000000000000000 ) ;
#196016 = VERTEX_POINT ( 'NONE', #240848 ) ;
#196018 = DIRECTION ( 'NONE',  ( 0.000000000000000000, -6.982962677686266711E-15, 1.000000000000000000 ) ) ;
#196017 = VECTOR ( 'NONE', #98964, 1000.000000000000000 ) ;
#196019 = AXIS2_PLACEMENT_3D ( 'NONE', #83271, #145830, #27217 ) ;
#196020 = VERTEX_POINT ( 'NONE', #141729 ) ;
#196021 = CARTESIAN_POINT ( 'NONE',  ( 20.94999999999999929, 85.00000000001149658, -45.91707660717670336 ) ) ;
#196022 = CYLINDRICAL_SURFACE ( 'NONE', #108232, 0.1000000000000024342 ) ;
#196024 = EDGE_LOOP ( 'NONE', ( #207658, #81106, #211538, #55839 ) ) ;
#196023 = DIRECTION ( 'NONE',  ( 0.000000000000000000, 0.000000000000000000, 1.000000000000000000 ) ) ;
#196025 = FACE_OUTER_BOUND ( 'NONE', #168249, .T. ) ;
#196026 = DIRECTION ( 'NONE',  ( -1.000000000000000000, -0.000000000000000000, 0.000000000000000000 ) ) ;
#196027 = CARTESIAN_POINT ( 'NONE',  ( 21.05000000000000071, 28.60154115857409352, -258.4512230915049713 ) ) ;
#196028 = CARTESIAN_POINT ( 'NONE',  ( 23.14999999999999503, 6.550000000000000711, -21.15000000000000213 ) ) ;
#196029 = CARTESIAN_POINT ( 'NONE',  ( -20.94999999999999929, 77.85102823015316176, -158.3691942151018566 ) ) ;
#196030 = CARTESIAN_POINT ( 'NONE',  ( -20.94999999999999929, 76.00000000001190870, -103.0231074845243029 ) ) ;
#196031 = CARTESIAN_POINT ( 'NONE',  ( -18.40000000000000213, 85.51932773110452501, -129.5501311079649156 ) ) ;
#196032 = AXIS2_PLACEMENT_3D ( 'NONE', #190982, #231377, #29354 ) ;
#196033 = ORIENTED_EDGE ( 'NONE', *, *, #118359, .F. ) ;
#196034 = B_SPLINE_CURVE_WITH_KNOTS ( 'NONE', 3,
 ( #252307, #232781, #213185, #129805, #151971, #54114, #209339, #231494, #9859, #133660, #11151, #248479, #30740, #34582, #253591, #94520, #75001, #249761, #230191, #69860, #214470, #110238, #170272, #35865, #192356, #188498 ),
 .UNSPECIFIED., .F., .F.,
 ( 4, 2, 2, 2, 2, 2, 2, 2, 2, 2, 2, 2, 4 ),
 ( 0.005476422646581347378, 0.006160811967703556588, 0.006845201288825765798, 0.007187395949386870403, 0.007529590609947975008, 0.007871785270509079613, 0.008213979931070184218, 0.008556174591631288823, 0.008898369252192393428, 0.009240563912753498033, 0.009582758573314602638, 0.01026714789443681185, 0.01095153721555902106 ),
 .UNSPECIFIED. ) ;
#196035 = DIRECTION ( 'NONE',  ( 1.000000000000000000, 0.000000000000000000, 0.000000000000000000 ) ) ;
#196036 = FACE_OUTER_BOUND ( 'NONE', #65142, .T. ) ;
#196037 = ORIENTED_EDGE ( 'NONE', *, *, #139499, .F. ) ;
#196038 = LINE ( 'NONE', #96886, #253917 ) ;
#196039 = AXIS2_PLACEMENT_3D ( 'NONE', #86015, #183870, #166908 ) ;
#196040 = EDGE_CURVE ( 'NONE', #101698, #198432, #34796, .T. ) ;
#196041 = CARTESIAN_POINT ( 'NONE',  ( -18.41799967126723914, 85.50000000001161027, -62.49103767126882758 ) ) ;
#196042 = EDGE_CURVE ( 'NONE', #97847, #241878, #160046, .T. ) ;
#196043 = VERTEX_POINT ( 'NONE', #17930 ) ;
#196044 = AXIS2_PLACEMENT_3D ( 'NONE', #199946, #236478, #78674 ) ;
#196045 = CYLINDRICAL_SURFACE ( 'NONE', #143777, 0.09999999999999939493 ) ;
#196046 = DIRECTION ( 'NONE',  ( -0.000000000000000000, -0.9770955615653316162, -0.2128009952263597848 ) ) ;
#196047 = EDGE_CURVE ( 'NONE', #251571, #48720, #126348, .T. ) ;
#196049 = ORIENTED_EDGE ( 'NONE', *, *, #231296, .T. ) ;
#196048 = VECTOR ( 'NONE', #169266, 1000.000000000000114 ) ;
#196051 = EDGE_CURVE ( 'NONE', #175937, #207750, #79178, .T. ) ;
#196050 = CARTESIAN_POINT ( 'NONE',  ( 18.49999999999999645, 74.26374286841446803, -91.45445515550682103 ) ) ;
#196052 = ORIENTED_EDGE ( 'NONE', *, *, #224739, .T. ) ;
#196053 = CARTESIAN_POINT ( 'NONE',  ( -22.94999999999999929, -1.885425182446134107, -11.49641995933507843 ) ) ;
#196055 = VERTEX_POINT ( 'NONE', #235697 ) ;
#196054 = FACE_OUTER_BOUND ( 'NONE', #222116, .T. ) ;
#196056 = DIRECTION ( 'NONE',  ( 2.978066053179066765E-16, 0.9651348961777157509, -0.2617529984165031243 ) ) ;
#196057 = ORIENTED_EDGE ( 'NONE', *, *, #230996, .F. ) ;
#196058 = AXIS2_PLACEMENT_3D ( 'NONE', #75853, #155433, #34193 ) ;
#196059 = CARTESIAN_POINT ( 'NONE',  ( -20.90000000000000213, -1.885425182446133885, -11.49641995933507843 ) ) ;
#196060 = EDGE_LOOP ( 'NONE', ( #119865, #49442 ) ) ;
#196062 = VERTEX_POINT ( 'NONE', #77902 ) ;
#196061 = ORIENTED_EDGE ( 'NONE', *, *, #75383, .T. ) ;
#196063 = CARTESIAN_POINT ( 'NONE',  ( 18.43579564894469414, 85.51932753530462605, -129.5501308406639112 ) ) ;
#196064 = ORIENTED_EDGE ( 'NONE', *, *, #3310, .F. ) ;
#196065 = DIRECTION ( 'NONE',  ( -1.000000000000000000, 0.000000000000000000, 0.000000000000000000 ) ) ;
#196066 = CIRCLE ( 'NONE', #133515, 0.5000000000000004441 ) ;
#196067 = EDGE_LOOP ( 'NONE', ( #2119, #149625, #46762, #238912 ) ) ;
#196068 = AXIS2_PLACEMENT_3D ( 'NONE', #150940, #72710, #149674 ) ;
#196069 = EDGE_CURVE ( 'NONE', #19219, #212713, #1431, .T. ) ;
#196070 = EDGE_CURVE ( 'NONE', #42435, #80243, #48040, .T. ) ;
#196071 = AXIS2_PLACEMENT_3D ( 'NONE', #173061, #89610, #214698 ) ;
#196072 = VERTEX_POINT ( 'NONE', #178328 ) ;
#196073 = LINE ( 'NONE', #96923, #99440 ) ;
#196074 = CARTESIAN_POINT ( 'NONE',  ( 23.14999999999999858, 72.00000000001170974, -69.52310748452433131 ) ) ;
#196075 = CARTESIAN_POINT ( 'NONE',  ( 21.30000000000002558, 1.115650265596050101E-11, -138.0500000000000114 ) ) ;
#196076 = ORIENTED_EDGE ( 'NONE', *, *, #164698, .F. ) ;
#196077 = CARTESIAN_POINT ( 'NONE',  ( -20.64999999999999858, 74.07476635515223506, -123.7928639513981892 ) ) ;
#196078 = DIRECTION ( 'NONE',  ( 0.000000000000000000, -0.6728971962616412394, 0.7397360091703134577 ) ) ;
#196079 = ORIENTED_EDGE ( 'NONE', *, *, #178054, .F. ) ;
#196080 = CARTESIAN_POINT ( 'NONE',  ( 23.14999999999999858, 5.500000000011153745, -155.0947339810869323 ) ) ;
#196082 = EDGE_CURVE ( 'NONE', #74339, #72992, #147867, .T. ) ;
#196081 = CARTESIAN_POINT ( 'NONE',  ( -18.52309608778585570, 38.02470060592907686, -261.2215444011879981 ) ) ;
#196083 = DIRECTION ( 'NONE',  ( 1.000000000000000000, 0.000000000000000000, 0.000000000000000000 ) ) ;
#196084 = AXIS2_PLACEMENT_3D ( 'NONE', #103965, #225199, #179695 ) ;
#196085 = ORIENTED_EDGE ( 'NONE', *, *, #93336, .T. ) ;
#196086 = ADVANCED_FACE ( 'NONE', ( #59602 ), #151976, .F. ) ;
#196087 = CARTESIAN_POINT ( 'NONE',  ( -16.89268316805466341, 66.04827818676967865, -90.37885996306994230 ) ) ;
#196088 = EDGE_LOOP ( 'NONE', ( #163054, #97030, #209186, #123445 ) ) ;
#196089 = EDGE_LOOP ( 'NONE', ( #71656, #255970, #31461, #137112 ) ) ;
#196090 = DIRECTION ( 'NONE',  ( 0.000000000000000000, -1.000000000000000000, 0.000000000000000000 ) ) ;
#196091 = ORIENTED_EDGE ( 'NONE', *, *, #180845, .F. ) ;
#196092 = ORIENTED_EDGE ( 'NONE', *, *, #26721, .T. ) ;
#196093 = CARTESIAN_POINT ( 'NONE',  ( -21.05000000000000071, -11.48912529306489994, -164.6000000000000227 ) ) ;
#196094 = CARTESIAN_POINT ( 'NONE',  ( -16.93433913041102912, 10.00597842153509376, -188.4353654273951406 ) ) ;
#196095 = EDGE_LOOP ( 'NONE', ( #223716, #4129, #171277, #218194 ) ) ;
#196096 = ORIENTED_EDGE ( 'NONE', *, *, #41457, .F. ) ;
#196097 = ADVANCED_FACE ( 'NONE', ( #219987 ), #96177, .F. ) ;
#196098 = CARTESIAN_POINT ( 'NONE',  ( 20.84999999999999787, 62.84855743180811771, -207.1254202119976640 ) ) ;
#196099 = CARTESIAN_POINT ( 'NONE',  ( -21.65000000000000213, 28.93140779147704933, -237.1870821964559184 ) ) ;
#196100 = EDGE_CURVE ( 'NONE', #62075, #147404, #176911, .T. ) ;
#196101 = VERTEX_POINT ( 'NONE', #41383 ) ;
#196102 = VECTOR ( 'NONE', #172935, 1000.000000000000000 ) ;
#196103 = CIRCLE ( 'NONE', #87744, 0.1000000000000000472 ) ;
#196104 = AXIS2_PLACEMENT_3D ( 'NONE', #12206, #90419, #72171 ) ;
#196105 = VERTEX_POINT ( 'NONE', #101271 ) ;
#196106 = AXIS2_PLACEMENT_3D ( 'NONE', #151657, #116364, #92920 ) ;
#196107 = EDGE_CURVE ( 'NONE', #15038, #210038, #120923, .T. ) ;
#196108 = ORIENTED_EDGE ( 'NONE', *, *, #68139, .T. ) ;
#196109 = AXIS2_PLACEMENT_3D ( 'NONE', #243050, #181801, #164811 ) ;
#196110 = LINE ( 'NONE', #44425, #155781 ) ;
#196111 = DIRECTION ( 'NONE',  ( -0.000000000000000000, 0.8660254037844383745, -0.5000000000000003331 ) ) ;
#196112 = EDGE_CURVE ( 'NONE', #138993, #429, #28858, .T. ) ;
#196113 = CARTESIAN_POINT ( 'NONE',  ( 5.999999999999997335, -11.25000000000000000, 13.90000000000000213 ) ) ;
#196114 = LINE ( 'NONE', #138661, #18226 ) ;
#196115 = DIRECTION ( 'NONE',  ( 0.000000000000000000, 1.000000000000000000, 2.891205793294679805E-16 ) ) ;
#196116 = VECTOR ( 'NONE', #212603, 1000.000000000000000 ) ;
#196117 = DIRECTION ( 'NONE',  ( 0.000000000000000000, -0.000000000000000000, 1.000000000000000000 ) ) ;
#196118 = FACE_OUTER_BOUND ( 'NONE', #250112, .T. ) ;
#196119 = EDGE_CURVE ( 'NONE', #96547, #69378, #27075, .T. ) ;
#196121 = LINE ( 'NONE', #232690, #149500 ) ;
#196120 = CARTESIAN_POINT ( 'NONE',  ( 21.05000000000000071, 76.01759718701968893, -75.96387837818673461 ) ) ;
#196122 = DIRECTION ( 'NONE',  ( 1.000000000000000000, 0.000000000000000000, 0.000000000000000000 ) ) ;
#196123 = DIRECTION ( 'NONE',  ( -1.000000000000000000, -2.952720810173289112E-16, 0.000000000000000000 ) ) ;
#196124 = DIRECTION ( 'NONE',  ( -1.000000000000000000, -0.000000000000000000, -0.000000000000000000 ) ) ;
#196125 = LINE ( 'NONE', #199983, #151031 ) ;
#196126 = VERTEX_POINT ( 'NONE', #205543 ) ;
#196128 = ORIENTED_EDGE ( 'NONE', *, *, #194321, .T. ) ;
#196127 = CYLINDRICAL_SURFACE ( 'NONE', #132165, 0.09999999999999781286 ) ;
#196129 = AXIS2_PLACEMENT_3D ( 'NONE', #227354, #48712, #251734 ) ;
#196130 = LINE ( 'NONE', #199991, #23533 ) ;
#196131 = DIRECTION ( 'NONE',  ( -0.000000000000000000, 0.000000000000000000, 1.000000000000000000 ) ) ;
#196132 = EDGE_LOOP ( 'NONE', ( #244229, #24995, #25174, #66935, #55618 ) ) ;
#196133 = CIRCLE ( 'NONE', #116838, 0.1000000000000067224 ) ;
#196134 = CARTESIAN_POINT ( 'NONE',  ( 18.39999999999999858, 85.60000000001240039, -163.4229180933022576 ) ) ;
#196135 = VECTOR ( 'NONE', #107822, 1000.000000000000000 ) ;
#196136 = CARTESIAN_POINT ( 'NONE',  ( -16.92778301347243897, 65.99905508317739589, -157.4516255924938832 ) ) ;
#196137 = ORIENTED_EDGE ( 'NONE', *, *, #203888, .F. ) ;
#196138 = DIRECTION ( 'NONE',  ( 0.000000000000000000, -0.8660254037844377084, -0.5000000000000016653 ) ) ;
#196139 = CYLINDRICAL_SURFACE ( 'NONE', #4765, 11.74999999999999822 ) ;
#196140 = VECTOR ( 'NONE', #195893, 1000.000000000000000 ) ;
#196141 = CARTESIAN_POINT ( 'NONE',  ( -21.07928932188134041, 10.02993822722303818, -228.1074463178677263 ) ) ;
#196143 = VERTEX_POINT ( 'NONE', #42635 ) ;
#196142 = CARTESIAN_POINT ( 'NONE',  ( 20.94999999999999574, 76.00000000001267608, -203.5231074845243597 ) ) ;
#196145 = ORIENTED_EDGE ( 'NONE', *, *, #143760, .T. ) ;
#196144 = FACE_OUTER_BOUND ( 'NONE', #40413, .T. ) ;
#196146 = DIRECTION ( 'NONE',  ( 0.000000000000000000, -0.1335171055202867274, 0.9910465087640866200 ) ) ;
#196147 = CYLINDRICAL_SURFACE ( 'NONE', #153260, 0.09999999999999939493 ) ;
#196148 = DIRECTION ( 'NONE',  ( -0.000000000000000000, -0.000000000000000000, -1.000000000000000000 ) ) ;
#196150 = CARTESIAN_POINT ( 'NONE',  ( -23.15000000000000213, 11.75000000001115552, -54.85000000000000142 ) ) ;
#196149 = CARTESIAN_POINT ( 'NONE',  ( -16.80891096016325292, 9.950000000011137047, -154.8676628072681751 ) ) ;
#196152 = EDGE_CURVE ( 'NONE', #19663, #3284, #22974, .T. ) ;
#196151 = DIRECTION ( 'NONE',  ( -1.000000000000000000, -7.304098846218135653E-16, -4.639676173203994055E-30 ) ) ;
#196154 = CYLINDRICAL_SURFACE ( 'NONE', #120471, 2.000000000000013323 ) ;
#196153 = AXIS2_PLACEMENT_3D ( 'NONE', #46192, #24100, #141442 ) ;
#196155 = CARTESIAN_POINT ( 'NONE',  ( -18.40904629823843663, 85.50000000001242029, -163.4229179220422736 ) ) ;
#196156 = CARTESIAN_POINT ( 'NONE',  ( 21.12757541349815682, 10.18096795049375025, -228.0240099581621109 ) ) ;
#196157 = CIRCLE ( 'NONE', #200256, 0.09999999999999939493 ) ;
#196158 = ORIENTED_EDGE ( 'NONE', *, *, #124166, .F. ) ;
#196160 = CARTESIAN_POINT ( 'NONE',  ( 21.13435531349810148, 1.115513965377477154E-11, -94.00627893640816524 ) ) ;
#196159 = AXIS2_PLACEMENT_3D ( 'NONE', #176449, #192161, #173910 ) ;
#196161 = ORIENTED_EDGE ( 'NONE', *, *, #147724, .F. ) ;
#196162 = CIRCLE ( 'NONE', #162879, 4.099999999999992539 ) ;
#196163 = VERTEX_POINT ( 'NONE', #162598 ) ;
#196164 = CARTESIAN_POINT ( 'NONE',  ( -21.05000000000000071, 74.83729825007408465, -128.4231074845243086 ) ) ;
#196165 = EDGE_CURVE ( 'NONE', #100350, #216920, #247241, .T. ) ;
#196166 = CARTESIAN_POINT ( 'NONE',  ( 20.94999999999999929, 76.00000000001267608, -203.5231074845243597 ) ) ;
#196167 = VERTEX_POINT ( 'NONE', #202990 ) ;
#196168 = AXIS2_PLACEMENT_3D ( 'NONE', #180195, #120248, #161925 ) ;
#196169 = AXIS2_PLACEMENT_3D ( 'NONE', #644, #239293, #56760 ) ;
#196170 = ADVANCED_FACE ( 'NONE', ( #8647 ), #201709, .F. ) ;
#196171 = EDGE_CURVE ( 'NONE', #167923, #147541, #222537, .T. ) ;
#196172 = ORIENTED_EDGE ( 'NONE', *, *, #6824, .F. ) ;
#196173 = CARTESIAN_POINT ( 'NONE',  ( -16.94107738177415357, 10.01423928514777728, -146.5500000000000114 ) ) ;
#196175 = ORIENTED_EDGE ( 'NONE', *, *, #224221, .T. ) ;
#196174 = CIRCLE ( 'NONE', #46318, 0.1000000000000028644 ) ;
#196176 = AXIS2_PLACEMENT_3D ( 'NONE', #174910, #177451, #219094 ) ;
#196177 = CIRCLE ( 'NONE', #254416, 0.09999999999999036049 ) ;
#196178 = EDGE_LOOP ( 'NONE', ( #163819, #164929, #153402 ) ) ;
#196179 = TOROIDAL_SURFACE ( 'NONE', #8748, 7.800000000000000711, 0.1000000000000000056 ) ;
#196180 = CARTESIAN_POINT ( 'NONE',  ( 21.15000000000005542, 87.50449464844290048, -37.85861909827351468 ) ) ;
#196181 = CYLINDRICAL_SURFACE ( 'NONE', #57733, 0.09999999999999939493 ) ;
#196182 = CARTESIAN_POINT ( 'NONE',  ( -18.59999999999999787, 66.85000000001259934, -191.1731074845244223 ) ) ;
#196183 = FACE_OUTER_BOUND ( 'NONE', #54925, .T. ) ;
#196184 = CARTESIAN_POINT ( 'NONE',  ( 14.11444803880196552, 9.457431528848912805, -14.99991693789965730 ) ) ;
#196185 = EDGE_CURVE ( 'NONE', #226600, #11036, #23099, .T. ) ;
#196186 = CARTESIAN_POINT ( 'NONE',  ( 20.94999999999999929, 76.00000000001126921, -203.5231074845248997 ) ) ;
#196187 = DIRECTION ( 'NONE',  ( -1.000000000000000000, -1.836970198721029934E-16, 0.000000000000000000 ) ) ;
#196189 = ORIENTED_EDGE ( 'NONE', *, *, #166501, .F. ) ;
#196188 = DIRECTION ( 'NONE',  ( 1.000000000000000000, 0.000000000000000000, 0.000000000000000000 ) ) ;
#196191 = FACE_OUTER_BOUND ( 'NONE', #190886, .T. ) ;
#196190 = CARTESIAN_POINT ( 'NONE',  ( 0.000000000000000000, -11.65000000000000036, 33.00000000000000000 ) ) ;
#196192 = CARTESIAN_POINT ( 'NONE',  ( 20.94999999999999929, 11.65000000000000391, -26.71613433702190932 ) ) ;
#196193 = ORIENTED_EDGE ( 'NONE', *, *, #132070, .F. ) ;
#196194 = CARTESIAN_POINT ( 'NONE',  ( -16.92563707711778420, 63.07545484833583771, -213.0929648075107536 ) ) ;
#196195 = CARTESIAN_POINT ( 'NONE',  ( -20.54999999999999716, 1.925233644870967487, -87.76975646687391475 ) ) ;
#196196 = ORIENTED_EDGE ( 'NONE', *, *, #67790, .T. ) ;
#196198 = CARTESIAN_POINT ( 'NONE',  ( 22.39999999999999503, 76.10085836911045476, -81.27267460801371612 ) ) ;
#196197 = CARTESIAN_POINT ( 'NONE',  ( 23.24999999999999645, 76.00000000001244871, -170.0231074845243597 ) ) ;
#196199 = LINE ( 'NONE', #111531, #177747 ) ;
#196200 = CARTESIAN_POINT ( 'NONE',  ( -20.85000000000000142, -11.74999999998884448, -67.00000000000000000 ) ) ;
#196201 = ORIENTED_EDGE ( 'NONE', *, *, #157752, .F. ) ;
#196202 = ORIENTED_EDGE ( 'NONE', *, *, #135893, .T. ) ;
#196203 = DIRECTION ( 'NONE',  ( 0.000000000000000000, -0.2128009952263651694, 0.9770955615653305060 ) ) ;
#196204 = EDGE_CURVE ( 'NONE', #96705, #152028, #239433, .T. ) ;
#196205 = FACE_OUTER_BOUND ( 'NONE', #146471, .T. ) ;
#196206 = DIRECTION ( 'NONE',  ( -3.890533409366484652E-14, 0.3848449534832963370, 0.9229812358755945523 ) ) ;
#196207 = DIRECTION ( 'NONE',  ( -1.020425574104004196E-15, -0.000000000000000000, -1.000000000000000000 ) ) ;
#196208 = ORIENTED_EDGE ( 'NONE', *, *, #118898, .F. ) ;
#196209 = AXIS2_PLACEMENT_3D ( 'NONE', #196688, #121047, #18057 ) ;
#196210 = DIRECTION ( 'NONE',  ( 1.000000000000000000, 0.000000000000000000, 0.000000000000000000 ) ) ;
#196211 = EDGE_CURVE ( 'NONE', #239723, #34485, #72875, .T. ) ;
#196212 = FACE_OUTER_BOUND ( 'NONE', #179977, .T. ) ;
#196213 = CIRCLE ( 'NONE', #158661, 0.1000000000000028644 ) ;
#196215 = ORIENTED_EDGE ( 'NONE', *, *, #111760, .T. ) ;
#196214 = FACE_OUTER_BOUND ( 'NONE', #109119, .T. ) ;
#196216 = CARTESIAN_POINT ( 'NONE',  ( 18.59999999999999787, 1.866714910068465239, -45.25267524628200988 ) ) ;
#196217 = CARTESIAN_POINT ( 'NONE',  ( -16.87333278164142669, 66.11739021543297667, -89.88993967837170374 ) ) ;
#196218 = CARTESIAN_POINT ( 'NONE',  ( 18.59999999999999432, 77.44184265367997000, -241.6694879557322508 ) ) ;
#196219 = DIRECTION ( 'NONE',  ( 2.952720810173289112E-16, -1.000000000000000000, 0.000000000000000000 ) ) ;
#196220 = DIRECTION ( 'NONE',  ( -0.000000000000000000, 0.9770955615653313941, 0.2128009952263606730 ) ) ;
#196222 = ORIENTED_EDGE ( 'NONE', *, *, #17679, .T. ) ;
#196221 = DIRECTION ( 'NONE',  ( 2.879366945564059217E-14, 0.9118278131605125347, -0.4105728183244932161 ) ) ;
#196223 = CARTESIAN_POINT ( 'NONE',  ( 22.50000000000000000, 64.35042919246758686, -170.1231074845244393 ) ) ;
#196224 = CARTESIAN_POINT ( 'NONE',  ( -20.00857864376270001, 66.85000000001180354, -81.87310748452438247 ) ) ;
#196225 = DIRECTION ( 'NONE',  ( 0.000000000000000000, 0.000000000000000000, 1.000000000000000000 ) ) ;
#196226 = ORIENTED_EDGE ( 'NONE', *, *, #71271, .F. ) ;
#196227 = DIRECTION ( 'NONE',  ( 0.000000000000000000, 0.8034013718071717491, -0.5954378521544919645 ) ) ;
#196228 = DIRECTION ( 'NONE',  ( 0.000000000000000000, 1.000000000000000000, 0.000000000000000000 ) ) ;
#196229 = DIRECTION ( 'NONE',  ( 1.000000000000000000, 0.000000000000000000, -0.000000000000000000 ) ) ;
#196230 = CARTESIAN_POINT ( 'NONE',  ( -23.15000000000000213, 0.000000000000000000, 0.000000000000000000 ) ) ;
#196232 = AXIS2_PLACEMENT_3D ( 'NONE', #106677, #227933, #49287 ) ;
#196231 = CARTESIAN_POINT ( 'NONE',  ( -18.46946985241241279, 78.23782832475592386, -231.6011469542054897 ) ) ;
#196234 = TOROIDAL_SURFACE ( 'NONE', #158856, 0.2000000000000000111, 0.1000000000000000056 ) ;
#196233 = DIRECTION ( 'NONE',  ( -1.000000000000000000, 0.000000000000000000, 0.000000000000000000 ) ) ;
#196235 = ORIENTED_EDGE ( 'NONE', *, *, #49995, .T. ) ;
#196236 = ORIENTED_EDGE ( 'NONE', *, *, #138707, .T. ) ;
#196237 = AXIS2_PLACEMENT_3D ( 'NONE', #27345, #69016, #229365 ) ;
#196238 = EDGE_CURVE ( 'NONE', #48902, #91508, #43920, .T. ) ;
#196239 = CARTESIAN_POINT ( 'NONE',  ( 23.14999999999999503, 69.55000000001173532, -81.27310748452437394 ) ) ;
#196241 = EDGE_CURVE ( 'NONE', #208794, #253814, #91928, .T. ) ;
#196240 = FACE_OUTER_BOUND ( 'NONE', #34261, .T. ) ;
#196242 = DIRECTION ( 'NONE',  ( -0.000000000000000000, -0.000000000000000000, 1.000000000000000000 ) ) ;
#196243 = DIRECTION ( 'NONE',  ( -1.000000000000000000, -0.000000000000000000, -0.000000000000000000 ) ) ;
#196244 = VERTEX_POINT ( 'NONE', #83010 ) ;
#196245 = ADVANCED_FACE ( 'NONE', ( #126014 ), #123463, .T. ) ;
#196246 = ADVANCED_FACE ( 'NONE', ( #221255, #184706 ), #84271, .F. ) ;
#196247 = DIRECTION ( 'NONE',  ( 0.000000000000000000, 0.9550021345545507412, -0.2965989261549202838 ) ) ;
#196248 = CARTESIAN_POINT ( 'NONE',  ( 20.44999100639885725, 11.85173402866923986, -206.3597776261780155 ) ) ;
#196249 = TOROIDAL_SURFACE ( 'NONE', #225457, 0.2000000000000000111, 0.1000000000000000056 ) ;
#196250 = EDGE_CURVE ( 'NONE', #77215, #14013, #144274, .T. ) ;
#196251 = DIRECTION ( 'NONE',  ( 0.000000000000000000, 0.9910827722268042983, 0.1332476588733639278 ) ) ;
#196252 = DIRECTION ( 'NONE',  ( -1.000000000000000000, -0.000000000000000000, -0.000000000000000000 ) ) ;
#196253 = EDGE_CURVE ( 'NONE', #195803, #51994, #243399, .T. ) ;
#196255 = EDGE_CURVE ( 'NONE', #67785, #20946, #193648, .T. ) ;
#196254 = EDGE_CURVE ( 'NONE', #53303, #113518, #218553, .T. ) ;
#196256 = ORIENTED_EDGE ( 'NONE', *, *, #120672, .T. ) ;
#196257 = CARTESIAN_POINT ( 'NONE',  ( -18.59999999999999787, 64.25000000001151079, -48.27310748452440237 ) ) ;
#196258 = VERTEX_POINT ( 'NONE', #187300 ) ;
#196259 = ORIENTED_EDGE ( 'NONE', *, *, #205928, .T. ) ;
#196260 = CARTESIAN_POINT ( 'NONE',  ( 21.13614978966381486, 76.00000000001239187, -176.5222121863581322 ) ) ;
#196261 = DIRECTION ( 'NONE',  ( 0.000000000000000000, -6.688090509790120484E-15, 1.000000000000000000 ) ) ;
#196262 = DIRECTION ( 'NONE',  ( 1.000000000000000000, 0.000000000000000000, 0.000000000000000000 ) ) ;
#196263 = ORIENTED_EDGE ( 'NONE', *, *, #143766, .F. ) ;
#196264 = CARTESIAN_POINT ( 'NONE',  ( 20.94999999999999574, 77.25000000001189449, -95.02310748452430289 ) ) ;
#196265 = DIRECTION ( 'NONE',  ( 0.000000000000000000, -0.8814952561688476074, 0.4721928772777262417 ) ) ;
#196266 = DIRECTION ( 'NONE',  ( -2.827886303505248766E-16, -0.03181660087583048496, 0.9994937237965570986 ) ) ;
#196267 = VERTEX_POINT ( 'NONE', #169043 ) ;
#196268 = DIRECTION ( 'NONE',  ( -1.000000000000000000, 0.000000000000000000, -0.000000000000000000 ) ) ;
#196269 = EDGE_CURVE ( 'NONE', #206711, #217493, #52899, .T. ) ;
#196271 = EDGE_LOOP ( 'NONE', ( #50862, #140245, #124148, #250608 ) ) ;
#196270 = CARTESIAN_POINT ( 'NONE',  ( -20.94999999999999929, 76.00000000001242029, -165.9231074845243654 ) ) ;
#196272 = TOROIDAL_SURFACE ( 'NONE', #254513, 11.65000000000000036, 0.1000000000000000056 ) ;
#196273 = CIRCLE ( 'NONE', #229604, 0.1000000000000046685 ) ;
#196274 = DIRECTION ( 'NONE',  ( 1.000000000000000000, 0.000000000000000000, 0.000000000000000000 ) ) ;
#196275 = LINE ( 'NONE', #214549, #206195 ) ;
#196276 = AXIS2_PLACEMENT_3D ( 'NONE', #9883, #230221, #149425 ) ;
#196277 = EDGE_CURVE ( 'NONE', #256947, #42982, #202020, .T. ) ;
#196278 = ADVANCED_FACE ( 'NONE', ( #29526 ), #133721, .T. ) ;
#196279 = ORIENTED_EDGE ( 'NONE', *, *, #29813, .T. ) ;
#196280 = DIRECTION ( 'NONE',  ( -0.000000000000000000, 1.000000000000000000, -0.000000000000000000 ) ) ;
#196282 = EDGE_CURVE ( 'NONE', #92552, #30609, #31192, .T. ) ;
#196281 = DIRECTION ( 'NONE',  ( 0.000000000000000000, 0.9893560106964510714, -0.1455152366551481502 ) ) ;
#196283 = CARTESIAN_POINT ( 'NONE',  ( 18.59999999999999432, 70.30054753569064019, -149.0653814410941607 ) ) ;
#196284 = ORIENTED_EDGE ( 'NONE', *, *, #80591, .T. ) ;
#196285 = CARTESIAN_POINT ( 'NONE',  ( 21.07971444708685738, 6.329792081637700463, -133.9121765636821237 ) ) ;
#196286 = CARTESIAN_POINT ( 'NONE',  ( 22.59066674512239814, 55.88295497714577920, -232.8089693692780600 ) ) ;
#196287 = DIRECTION ( 'NONE',  ( -1.000000000000000000, 0.000000000000000000, 0.000000000000000000 ) ) ;
#196288 = EDGE_CURVE ( 'NONE', #195996, #152615, #56250, .T. ) ;
#196289 = AXIS2_PLACEMENT_3D ( 'NONE', #79165, #161309, #120908 ) ;
#196290 = VERTEX_POINT ( 'NONE', #90733 ) ;
#196291 = EDGE_CURVE ( 'NONE', #15834, #125839, #147837, .T. ) ;
#196292 = ORIENTED_EDGE ( 'NONE', *, *, #157322, .F. ) ;
#196293 = VERTEX_POINT ( 'NONE', #32086 ) ;
#196294 = CARTESIAN_POINT ( 'NONE',  ( -18.40000000000000213, 70.35000000001261355, -190.8731074845244109 ) ) ;
#196295 = DIRECTION ( 'NONE',  ( -1.000000000000000000, 0.000000000000000000, 0.000000000000000000 ) ) ;
#196296 = ORIENTED_EDGE ( 'NONE', *, *, #221568, .F. ) ;
#196297 = DIRECTION ( 'NONE',  ( 0.000000000000000000, -0.2128009952263678062, 0.9770955615653298398 ) ) ;
#196298 = CARTESIAN_POINT ( 'NONE',  ( -20.15000000000000568, 66.70857864377450142, -81.77310748452437394 ) ) ;
#196299 = DIRECTION ( 'NONE',  ( 0.000000000000000000, 1.734723475976807292E-15, -1.000000000000000000 ) ) ;
#196300 = DIRECTION ( 'NONE',  ( 0.000000000000000000, 0.4088369013363281068, -0.9126074666063770380 ) ) ;
#196301 = CARTESIAN_POINT ( 'NONE',  ( -18.50000000000000000, 1.637172712981535883, -112.0821533654720525 ) ) ;
#196302 = DIRECTION ( 'NONE',  ( 0.000000000000000000, -7.086529944415894657E-15, 1.000000000000000000 ) ) ;
#196303 = FACE_OUTER_BOUND ( 'NONE', #214112, .T. ) ;
#196305 = VERTEX_POINT ( 'NONE', #170338 ) ;
#196304 = DIRECTION ( 'NONE',  ( 1.000000000000000000, 0.000000000000000000, 0.000000000000000000 ) ) ;
#196307 = VERTEX_POINT ( 'NONE', #128598 ) ;
#196306 = DIRECTION ( 'NONE',  ( 0.000000000000000000, -1.000000000000000000, 0.000000000000000000 ) ) ;
#196309 = CARTESIAN_POINT ( 'NONE',  ( -16.96982749440682170, 51.18557661132589232, -232.1405759491296976 ) ) ;
#196308 = CARTESIAN_POINT ( 'NONE',  ( -16.77683809663752257, 48.78215419113038109, -213.4964773079645681 ) ) ;
#196311 = EDGE_LOOP ( 'NONE', ( #240300, #200240, #166342, #78247 ) ) ;
#196310 = CARTESIAN_POINT ( 'NONE',  ( 23.24999999999999645, 11.75000000001113953, -180.1499999999999773 ) ) ;
#196312 = CIRCLE ( 'NONE', #38124, 0.09999999999998898659 ) ;
#196313 = ORIENTED_EDGE ( 'NONE', *, *, #10382, .T. ) ;
#196314 = DIRECTION ( 'NONE',  ( 0.000000000000000000, 0.000000000000000000, 1.000000000000000000 ) ) ;
#196315 = CARTESIAN_POINT ( 'NONE',  ( -21.05000000000000426, 12.80863705670246411, -205.3010250813005655 ) ) ;
#196316 = TOROIDAL_SURFACE ( 'NONE', #129685, 0.2000000000000000111, 0.1000000000000000056 ) ;
#196317 = FACE_OUTER_BOUND ( 'NONE', #130150, .T. ) ;
#196318 = AXIS2_PLACEMENT_3D ( 'NONE', #105417, #83297, #44215 ) ;
#196319 = CARTESIAN_POINT ( 'NONE',  ( 18.49999999999999645, 4.158309866074138661, -211.9342015984041439 ) ) ;
#196320 = FACE_OUTER_BOUND ( 'NONE', #97373, .T. ) ;
#196321 = AXIS2_PLACEMENT_3D ( 'NONE', #63033, #23946, #181715 ) ;
#196322 = CYLINDRICAL_SURFACE ( 'NONE', #110431, 0.1000000000000052097 ) ;
#196324 = ORIENTED_EDGE ( 'NONE', *, *, #100253, .T. ) ;
#196323 = EDGE_CURVE ( 'NONE', #37627, #10839, #153338, .T. ) ;
#196325 = ORIENTED_EDGE ( 'NONE', *, *, #145239, .F. ) ;
#196326 = DIRECTION ( 'NONE',  ( 1.000000000000000000, 0.000000000000000000, 0.000000000000000000 ) ) ;
#196327 = CIRCLE ( 'NONE', #50578, 12.87499999999999822 ) ;
#196328 = MANIFOLD_SOLID_BREP ( 'Stock-MAS-200-1', #215926 ) ;
#196329 = EDGE_CURVE ( 'NONE', #257458, #17700, #172845, .T. ) ;
#196330 = ORIENTED_EDGE ( 'NONE', *, *, #189550, .T. ) ;
#196331 = CARTESIAN_POINT ( 'NONE',  ( 18.69999999999999929, -1.467286812112899463, 28.00000000000000000 ) ) ;
#196332 = AXIS2_PLACEMENT_3D ( 'NONE', #199570, #20932, #121330 ) ;
#196333 = CARTESIAN_POINT ( 'NONE',  ( 18.49999999999998934, 68.00417547777205129, -224.2303273613012209 ) ) ;
#196334 = DIRECTION ( 'NONE',  ( 0.000000000000000000, 0.2617529984164955192, 0.9651348961777177493 ) ) ;
#196335 = TOROIDAL_SURFACE ( 'NONE', #83873, 0.4000000000000003553, 0.1000000000000000056 ) ;
#196336 = CARTESIAN_POINT ( 'NONE',  ( 23.25000000000000000, 87.75000000001202238, -114.7731074845242318 ) ) ;
#196337 = EDGE_CURVE ( 'NONE', #92509, #1130, #31372, .T. ) ;
#196338 = ORIENTED_EDGE ( 'NONE', *, *, #250921, .T. ) ;
#196340 = EDGE_CURVE ( 'NONE', #209959, #233793, #197724, .T. ) ;
#196339 = CARTESIAN_POINT ( 'NONE',  ( -12.24999999999999822, 66.65000000001205649, -119.6573643172504688 ) ) ;
#196341 = ORIENTED_EDGE ( 'NONE', *, *, #123775, .T. ) ;
#196343 = VECTOR ( 'NONE', #223265, 1000.000000000000000 ) ;
#196342 = DIRECTION ( 'NONE',  ( -1.000000000000000000, -3.265361837132813093E-16, 0.000000000000000000 ) ) ;
#196344 = EDGE_LOOP ( 'NONE', ( #36925, #59906, #209537, #132034 ) ) ;
#196345 = CARTESIAN_POINT ( 'NONE',  ( -14.00000000000000178, 66.15000000001155911, -52.77310748452439526 ) ) ;
#196346 = CARTESIAN_POINT ( 'NONE',  ( -23.15000000000000213, 2.718532714028243369, -213.4823957989985956 ) ) ;
#196347 = CARTESIAN_POINT ( 'NONE',  ( 21.30000000000002558, 1.115600667400684642E-11, -167.4999999999999716 ) ) ;
#196348 = EDGE_LOOP ( 'NONE', ( #133498, #27620, #46957, #154717 ) ) ;
#196349 = DIRECTION ( 'NONE',  ( -0.000000000000000000, 1.000000000000000000, 6.982962677686266711E-15 ) ) ;
#196351 = ORIENTED_EDGE ( 'NONE', *, *, #55190, .T. ) ;
#196350 = LINE ( 'NONE', #36018, #84624 ) ;
#196352 = AXIS2_PLACEMENT_3D ( 'NONE', #27304, #88494, #246319 ) ;
#196353 = PLANE ( 'NONE',  #252111 ) ;
#196355 = EDGE_LOOP ( 'NONE', ( #106330, #140959, #116266, #53953 ) ) ;
#196354 = CIRCLE ( 'NONE', #158985, 0.09999999999999939493 ) ;
#196356 = AXIS2_PLACEMENT_3D ( 'NONE', #60911, #222543, #140446 ) ;
#196357 = EDGE_CURVE ( 'NONE', #71652, #97513, #247811, .T. ) ;
#196358 = PLANE ( 'NONE',  #132364 ) ;
#196359 = ORIENTED_EDGE ( 'NONE', *, *, #166566, .F. ) ;
#196360 = DIRECTION ( 'NONE',  ( -1.000000000000000000, -3.265361837132813093E-16, 0.000000000000000000 ) ) ;
#196361 = CARTESIAN_POINT ( 'NONE',  ( 22.45301702632625762, 64.16722595661912010, -247.0947660219591739 ) ) ;
#196362 =( BOUNDED_CURVE ( )  B_SPLINE_CURVE ( 3, ( #95954, #94674, #136342, #213332 ),
 .UNSPECIFIED., .F., .F. ) 
 B_SPLINE_CURVE_WITH_KNOTS ( ( 4, 4 ),
 ( 2.589852378279006828, 2.850972632318389710 ),
 .UNSPECIFIED. ) 
 CURVE ( )  GEOMETRIC_REPRESENTATION_ITEM ( )  RATIONAL_B_SPLINE_CURVE ( ( 1.000000000000000000, 0.9943260843901262636, 0.9943260843901262636, 1.000000000000000000 ) ) 
 REPRESENTATION_ITEM ( '' )  );
#196363 = CARTESIAN_POINT ( 'NONE',  ( -18.50000000000000000, 9.350000000011156942, -45.85000000000000142 ) ) ;
#196364 = CARTESIAN_POINT ( 'NONE',  ( -23.15000000000000213, 2.500000000011154633, -87.27537807723794572 ) ) ;
#196365 = CYLINDRICAL_SURFACE ( 'NONE', #114535, 0.5000000000000004441 ) ;
#196366 = ORIENTED_EDGE ( 'NONE', *, *, #233858, .F. ) ;
#196367 = DIRECTION ( 'NONE',  ( 1.000000000000000000, 0.000000000000000000, 0.000000000000000000 ) ) ;
#196368 = FACE_OUTER_BOUND ( 'NONE', #22487, .T. ) ;
#196369 = CARTESIAN_POINT ( 'NONE',  ( -20.99749315643149217, 11.75000000001115197, -160.4851942312420761 ) ) ;
#196370 = ORIENTED_EDGE ( 'NONE', *, *, #156037, .F. ) ;
#196371 = ADVANCED_FACE ( 'NONE', ( #200131 ), #122921, .T. ) ;
#196372 = CARTESIAN_POINT ( 'NONE',  ( 13.40000000000000036, -8.279289321881348584, 18.97071067811865674 ) ) ;
#196373 = ORIENTED_EDGE ( 'NONE', *, *, #253602, .T. ) ;
#196374 = LINE ( 'NONE', #58127, #102355 ) ;
#196375 = ORIENTED_EDGE ( 'NONE', *, *, #45085, .T. ) ;
#196376 = CARTESIAN_POINT ( 'NONE',  ( -20.64999999999999858, 71.65000000001151648, -48.37310748452435405 ) ) ;
#196377 = DIRECTION ( 'NONE',  ( 0.000000000000000000, -6.982962677686266711E-15, 1.000000000000000000 ) ) ;
#196379 = ORIENTED_EDGE ( 'NONE', *, *, #223630, .T. ) ;
#196378 = DIRECTION ( 'NONE',  ( 0.7071067811865487940, 0.7071067811865462405, -7.215498431451186046E-16 ) ) ;
#196380 = VERTEX_POINT ( 'NONE', #178014 ) ;
#196381 = EDGE_CURVE ( 'NONE', #165593, #113902, #195010, .T. ) ;
#196382 = AXIS2_PLACEMENT_3D ( 'NONE', #252193, #73606, #227499 ) ;
#196383 = CARTESIAN_POINT ( 'NONE',  ( -20.54999999999999716, 4.350000000011156054, -146.3500000000000227 ) ) ;
#196384 = LINE ( 'NONE', #17735, #81288 ) ;
#196385 = EDGE_CURVE ( 'NONE', #132466, #73568, #43796, .T. ) ;
#196386 = ORIENTED_EDGE ( 'NONE', *, *, #108846, .F. ) ;
#196387 = EDGE_LOOP ( 'NONE', ( #214908, #196145, #117928, #54291 ) ) ;
#196388 = CARTESIAN_POINT ( 'NONE',  ( -21.07094088545368393, 0.09889370256337755294, -127.6798327780828686 ) ) ;
#196389 = CARTESIAN_POINT ( 'NONE',  ( -21.05000000000000071, 11.75000000001115197, -193.9851942293460070 ) ) ;
#196390 = ORIENTED_EDGE ( 'NONE', *, *, #215345, .T. ) ;
#196391 = CARTESIAN_POINT ( 'NONE',  ( 21.14999999999999858, 10.21728496540352893, -227.9671432372868765 ) ) ;
#196392 = ORIENTED_EDGE ( 'NONE', *, *, #114734, .F. ) ;
#196393 =( BOUNDED_SURFACE ( )  B_SPLINE_SURFACE ( 3, 2, ( 
 ( #13634, #33235, #193560 ),
 ( #211841, #250936, #168893 ),
 ( #12371, #30649, #94442 ),
 ( #233957, #210549, #112732 ),
 ( #232694, #192283, #248391 ),
 ( #170185, #93157, #174033 ) ),
 .UNSPECIFIED., .F., .F., .F. ) 
 B_SPLINE_SURFACE_WITH_KNOTS ( ( 4, 2, 4 ),
 ( 3, 3 ),
 ( 0.0001792624049599621759, 0.0003686986002124818611, 0.0005581347954650015463 ),
 ( 0.000000000000000000, 1.000000000000000000 ),
 .UNSPECIFIED. ) 
 GEOMETRIC_REPRESENTATION_ITEM ( )  RATIONAL_B_SPLINE_SURFACE ( (
 ( 1.000000000000000000, 0.9238795325113097201, 1.000000000000000000),
 ( 1.000000000000000000, 0.9229318695240524839, 1.000000000000000000),
 ( 1.000000000000000000, 0.8926288119227774320, 1.000000000000000000),
 ( 1.000000000000000000, 0.8123777807274952245, 1.000000000000000000),
 ( 1.000000000000000000, 0.7629087100928820808, 1.000000000000000000),
 ( 1.000000000000000000, 0.7071067811865597852, 1.000000000000000000) ) ) 
 REPRESENTATION_ITEM ( '' )  SURFACE ( )  );
#196394 = ADVANCED_FACE ( 'NONE', ( #95869 ), #115441, .T. ) ;
#196396 = CARTESIAN_POINT ( 'NONE',  ( -21.14999999999994174, 76.00000000001119815, -3.123107484524795474 ) ) ;
#196395 = AXIS2_PLACEMENT_3D ( 'NONE', #132349, #112798, #210607 ) ;
#196397 = CARTESIAN_POINT ( 'NONE',  ( -22.50000000000000000, 11.64957080755595520, -133.9000000000000057 ) ) ;
#196398 = ADVANCED_FACE ( 'NONE', ( #175449 ), #100970, .T. ) ;
#196399 = EDGE_CURVE ( 'NONE', #232502, #205893, #254896, .T. ) ;
#196401 = VERTEX_POINT ( 'NONE', #116731 ) ;
#196400 = DIRECTION ( 'NONE',  ( -0.000000000000000000, -0.8660254037844420383, 0.4999999999999943379 ) ) ;
#196402 = DIRECTION ( 'NONE',  ( -1.000000000000000000, -0.000000000000000000, -0.000000000000000000 ) ) ;
#196403 = DIRECTION ( 'NONE',  ( -1.000000000000000000, 2.952720810173289112E-16, 2.061873921506763405E-30 ) ) ;
#196404 = DIRECTION ( 'NONE',  ( 2.952720810173289112E-16, -1.000000000000000000, 0.000000000000000000 ) ) ;
#196405 = EDGE_CURVE ( 'NONE', #4010, #73777, #246997, .T. ) ;
#196407 = CARTESIAN_POINT ( 'NONE',  ( -20.54999999999999716, 54.18117728009210055, -239.0715820348696923 ) ) ;
#196406 = CARTESIAN_POINT ( 'NONE',  ( 20.12500000000000355, 59.40384239514754938, -225.5881082859534956 ) ) ;
#196408 = CARTESIAN_POINT ( 'NONE',  ( -21.05000000000000071, 76.01465611852459858, -143.0197940702917094 ) ) ;
#196409 = LINE ( 'NONE', #214689, #23557 ) ;
#196410 = AXIS2_PLACEMENT_3D ( 'NONE', #142307, #86164, #44514 ) ;
#196411 = CARTESIAN_POINT ( 'NONE',  ( 23.40000000000005542, 77.36076146337680370, -43.99645795275012006 ) ) ;
#196412 = AXIS2_PLACEMENT_3D ( 'NONE', #36474, #118569, #235915 ) ;
#196413 = DIRECTION ( 'NONE',  ( 1.000000000000000000, 0.000000000000000000, 0.000000000000000000 ) ) ;
#196415 = EDGE_LOOP ( 'NONE', ( #170124, #145444, #94876 ) ) ;
#196414 = AXIS2_PLACEMENT_3D ( 'NONE', #8971, #168094, #106776 ) ;
#196416 = VERTEX_POINT ( 'NONE', #157173 ) ;
#196417 = DIRECTION ( 'NONE',  ( 1.000000000000000000, 0.000000000000000000, 0.000000000000000000 ) ) ;
#196419 = VERTEX_POINT ( 'NONE', #118015 ) ;
#196418 = CYLINDRICAL_SURFACE ( 'NONE', #66882, 0.09999999999999939493 ) ;
#196420 = ORIENTED_EDGE ( 'NONE', *, *, #99728, .T. ) ;
#196421 = EDGE_CURVE ( 'NONE', #239691, #156870, #117825, .T. ) ;
#196422 = CARTESIAN_POINT ( 'NONE',  ( 18.54999999999999716, 67.25000000001185185, -90.37310748452436826 ) ) ;
#196423 = VERTEX_POINT ( 'NONE', #60598 ) ;
#196424 = CARTESIAN_POINT ( 'NONE',  ( -20.64999999999999858, 18.47808476326694915, -239.8121846073901224 ) ) ;
#196425 = ORIENTED_EDGE ( 'NONE', *, *, #198662, .F. ) ;
#196426 = AXIS2_PLACEMENT_3D ( 'NONE', #148472, #46776, #228003 ) ;
#196427 = DIRECTION ( 'NONE',  ( 0.000000000000000000, 0.000000000000000000, 1.000000000000000000 ) ) ;
#196429 = ORIENTED_EDGE ( 'NONE', *, *, #154407, .F. ) ;
#196428 = ORIENTED_EDGE ( 'NONE', *, *, #53549, .F. ) ;
#196430 = VERTEX_POINT ( 'NONE', #155890 ) ;
#196431 = ORIENTED_EDGE ( 'NONE', *, *, #163670, .F. ) ;
#196432 = ORIENTED_EDGE ( 'NONE', *, *, #67679, .T. ) ;
#196433 = DIRECTION ( 'NONE',  ( 0.000000000000000000, 0.000000000000000000, 1.000000000000000000 ) ) ;
#196434 = DIRECTION ( 'NONE',  ( 1.000000000000000000, -0.000000000000000000, 0.000000000000000000 ) ) ;
#196436 = VERTEX_POINT ( 'NONE', #179305 ) ;
#196435 = FACE_OUTER_BOUND ( 'NONE', #135386, .T. ) ;
#196437 = CARTESIAN_POINT ( 'NONE',  ( -22.47071067811865674, 33.41224047107334627, -242.5462774987836383 ) ) ;
#196438 = CARTESIAN_POINT ( 'NONE',  ( 15.39793903038207112, 12.50981721680830105, -214.3157313002988928 ) ) ;
#196440 = ORIENTED_EDGE ( 'NONE', *, *, #53510, .T. ) ;
#196439 = CARTESIAN_POINT ( 'NONE',  ( -16.92925196614876882, 60.90909993422622648, -221.0679780288619156 ) ) ;
#196441 = DIRECTION ( 'NONE',  ( 1.000000000000000000, -0.000000000000000000, -0.000000000000000000 ) ) ;
#196442 = EDGE_LOOP ( 'NONE', ( #165721, #243615, #65535, #172540 ) ) ;
#196443 = CARTESIAN_POINT ( 'NONE',  ( 20.94999999999999929, 1.115600667400684642E-11, -100.5000000000000284 ) ) ;
#196445 = ORIENTED_EDGE ( 'NONE', *, *, #188319, .F. ) ;
#196444 = CARTESIAN_POINT ( 'NONE',  ( -21.05000000000000071, 13.99999999999999822, -28.07290746961752603 ) ) ;
#196446 = DIRECTION ( 'NONE',  ( 0.000000000000000000, 0.4088369013363281068, -0.9126074666063770380 ) ) ;
#196447 = LINE ( 'NONE', #213448, #187282 ) ;
#196448 = CIRCLE ( 'NONE', #200548, 7.791421356237310469 ) ;
#196449 = AXIS2_PLACEMENT_3D ( 'NONE', #202962, #148132, #163846 ) ;
#196450 = CARTESIAN_POINT ( 'NONE',  ( -17.11825945287481687, 9.950000000011138823, -87.75000000000004263 ) ) ;
#196451 = CIRCLE ( 'NONE', #154979, 0.09999999999999939493 ) ;
#196452 = ORIENTED_EDGE ( 'NONE', *, *, #157491, .F. ) ;
#196454 = DIRECTION ( 'NONE',  ( 1.000000000000000000, 0.000000000000000000, 0.000000000000000000 ) ) ;
#196453 = CARTESIAN_POINT ( 'NONE',  ( -20.94999999999999929, 79.03126467873600802, -235.8703919547671717 ) ) ;
#196455 = CARTESIAN_POINT ( 'NONE',  ( -21.64999999999999858, 68.75000000001152500, -48.37310748452436826 ) ) ;
#196456 = CARTESIAN_POINT ( 'NONE',  ( -22.59999999999999787, 11.74956712350054744, -33.39914163090129762 ) ) ;
#196457 = CARTESIAN_POINT ( 'NONE',  ( 20.94999999999999929, 85.00000000001179501, -79.41707660717668205 ) ) ;
#196458 = ORIENTED_EDGE ( 'NONE', *, *, #170606, .T. ) ;
#196459 = ORIENTED_EDGE ( 'NONE', *, *, #72576, .F. ) ;
#196460 = CARTESIAN_POINT ( 'NONE',  ( -20.54999999999999716, 85.00000000001207923, -126.6291383618717816 ) ) ;
#196461 = DIRECTION ( 'NONE',  ( 1.000000000000000000, -0.000000000000000000, -0.000000000000000000 ) ) ;
#196462 = ORIENTED_EDGE ( 'NONE', *, *, #67467, .T. ) ;
#196463 = CARTESIAN_POINT ( 'NONE',  ( -18.50000000000000000, 9.250000000011157297, -121.8500000000000369 ) ) ;
#196464 = VERTEX_POINT ( 'NONE', #77579 ) ;
#196465 = CARTESIAN_POINT ( 'NONE',  ( -18.59999999999999787, -1.835341550224411922, -11.55515129256297868 ) ) ;
#196466 = EDGE_CURVE ( 'NONE', #247436, #120372, #5371, .T. ) ;
#196467 = CARTESIAN_POINT ( 'NONE',  ( -23.15000000000000213, -11.48912529306489816, -130.9000000000000341 ) ) ;
#196468 = CIRCLE ( 'NONE', #108981, 0.2000000000000057288 ) ;
#196469 = ADVANCED_FACE ( 'NONE', ( #176727 ), #140130, .T. ) ;
#196470 = EDGE_CURVE ( 'NONE', #223804, #101672, #20217, .T. ) ;
#196471 = ORIENTED_EDGE ( 'NONE', *, *, #240121, .F. ) ;
#196472 = CARTESIAN_POINT ( 'NONE',  ( -21.04142135623731136, 6.223900101154156594, 12.00000000000000000 ) ) ;
#196473 = ORIENTED_EDGE ( 'NONE', *, *, #148183, .F. ) ;
#196474 = ORIENTED_EDGE ( 'NONE', *, *, #239153, .T. ) ;
#196475 = ORIENTED_EDGE ( 'NONE', *, *, #213771, .T. ) ;
#196476 = CARTESIAN_POINT ( 'NONE',  ( -22.39999999999999503, 68.20922040163897293, -170.1231074845244109 ) ) ;
#196477 = DIRECTION ( 'NONE',  ( 0.000000000000000000, 0.8700118002898322711, -0.4930308989875231696 ) ) ;
#196478 = DIRECTION ( 'NONE',  ( 1.186688945009010077E-16, -1.000000000000000000, -0.000000000000000000 ) ) ;
#196479 = LINE ( 'NONE', #218601, #157200 ) ;
#196480 = CARTESIAN_POINT ( 'NONE',  ( 21.87500000000000355, 66.25000000001253397, -182.2731074845244450 ) ) ;
#196481 = EDGE_CURVE ( 'NONE', #63725, #181753, #609, .T. ) ;
#196482 = TOROIDAL_SURFACE ( 'NONE', #133942, 7.791421356237335338, 0.1000000000000000056 ) ;
#196484 = DIRECTION ( 'NONE',  ( 0.000000000000000000, -0.9651348961777157509, 0.2617529984165031243 ) ) ;
#196483 = CARTESIAN_POINT ( 'NONE',  ( 21.05000000000000071, -9.399999999988844834, -124.1060308773475924 ) ) ;
#196485 = CYLINDRICAL_SURFACE ( 'NONE', #133217, 0.1000000000000124678 ) ;
#196487 = ORIENTED_EDGE ( 'NONE', *, *, #196381, .T. ) ;
#196486 = PLANE ( 'NONE',  #106365 ) ;
#196488 = CARTESIAN_POINT ( 'NONE',  ( 23.14999999999999503, 64.25000000001156764, -57.37310748452440379 ) ) ;
#196489 = ORIENTED_EDGE ( 'NONE', *, *, #240035, .F. ) ;
#196490 = CARTESIAN_POINT ( 'NONE',  ( -18.39999999999999858, 11.47316190336247388, -9.325946066807970780 ) ) ;
#196491 = ORIENTED_EDGE ( 'NONE', *, *, #253647, .T. ) ;
#196492 = ORIENTED_EDGE ( 'NONE', *, *, #187274, .F. ) ;
#196493 = CARTESIAN_POINT ( 'NONE',  ( -16.93211319090181632, 66.00001321885403627, -48.60060198525133046 ) ) ;
#196494 = CIRCLE ( 'NONE', #84014, 0.1999999999999997335 ) ;
#196495 = DIRECTION ( 'NONE',  ( 0.000000000000000000, 0.4999999999999956701, -0.8660254037844411501 ) ) ;
#196496 = CARTESIAN_POINT ( 'NONE',  ( 18.59999999999999787, 86.35479209693714608, -75.76656650145046967 ) ) ;
#196497 = ORIENTED_EDGE ( 'NONE', *, *, #238869, .F. ) ;
#196498 = AXIS2_PLACEMENT_3D ( 'NONE', #223157, #227016, #105763 ) ;
#196499 = CARTESIAN_POINT ( 'NONE',  ( -23.25000000000000000, 77.83585931145546510, -91.41866831572575336 ) ) ;
#196500 = AXIS2_PLACEMENT_3D ( 'NONE', #83601, #240157, #182759 ) ;
#196501 = ORIENTED_EDGE ( 'NONE', *, *, #51478, .F. ) ;
#196502 = ORIENTED_EDGE ( 'NONE', *, *, #74771, .T. ) ;
#196503 = AXIS2_PLACEMENT_3D ( 'NONE', #96144, #196538, #178297 ) ;
#196505 = VERTEX_POINT ( 'NONE', #65751 ) ;
#196504 = ADVANCED_FACE ( 'NONE', ( #55439 ), #219676, .T. ) ;
#196506 = DIRECTION ( 'NONE',  ( 1.000000000000000000, 0.000000000000000000, 0.000000000000000000 ) ) ;
#196507 = DIRECTION ( 'NONE',  ( 0.000000000000000000, -1.000000000000000000, -6.982962677686265922E-15 ) ) ;
#196508 = ORIENTED_EDGE ( 'NONE', *, *, #222541, .T. ) ;
#196509 = ADVANCED_FACE ( 'NONE', ( #103567 ), #142703, .F. ) ;
#196510 = CARTESIAN_POINT ( 'NONE',  ( 20.94999999999999929, -1.835341550213257733, -112.0551512925630249 ) ) ;
#196511 = FACE_OUTER_BOUND ( 'NONE', #221593, .T. ) ;
#196512 = CARTESIAN_POINT ( 'NONE',  ( -22.94999999999999929, 11.59510167572422112, 1.901609089591594692 ) ) ;
#196513 = VERTEX_POINT ( 'NONE', #202688 ) ;
#196514 = CIRCLE ( 'NONE', #225712, 4.000000000000003553 ) ;
#196516 = CIRCLE ( 'NONE', #109019, 0.1000000000000021427 ) ;
#196515 = DIRECTION ( 'NONE',  ( 0.000000000000000000, 0.5000000000000078826, -0.8660254037844340447 ) ) ;
#196517 = DIRECTION ( 'NONE',  ( 0.5932847527679310229, -0.8049926720990042694, 0.000000000000000000 ) ) ;
#196518 = B_SPLINE_CURVE_WITH_KNOTS ( 'NONE', 3,
 ( #127176, #243250, #206709, #25517, #103722, #43786, #22966, #145438 ),
 .UNSPECIFIED., .F., .F.,
 ( 4, 2, 2, 4 ),
 ( 0.000000000000000000, 6.534141206312327069E-05, 0.0001306828241262465414, 0.0002613656482524937333 ),
 .UNSPECIFIED. ) ;
#196519 = ADVANCED_FACE ( 'NONE', ( #220959 ), #184405, .T. ) ;
#196520 = CIRCLE ( 'NONE', #42400, 0.09999999999999939493 ) ;
#196521 = DIRECTION ( 'NONE',  ( 0.000000000000000000, -0.5000000000000016653, 0.8660254037844377084 ) ) ;
#196522 = AXIS2_PLACEMENT_3D ( 'NONE', #196346, #17697, #178093 ) ;
#196523 = ORIENTED_EDGE ( 'NONE', *, *, #202262, .F. ) ;
#196524 = AXIS2_PLACEMENT_3D ( 'NONE', #117005, #36206, #219953 ) ;
#196525 = CARTESIAN_POINT ( 'NONE',  ( -21.14999999999999858, 31.89597452117651244, -238.9192857152811769 ) ) ;
#196526 = ORIENTED_EDGE ( 'NONE', *, *, #48018, .T. ) ;
#196527 = CARTESIAN_POINT ( 'NONE',  ( -17.11825945287481332, 10.05000000001113847, -54.25000000000000000 ) ) ;
#196528 = AXIS2_PLACEMENT_3D ( 'NONE', #220078, #3584, #199241 ) ;
#196529 = CARTESIAN_POINT ( 'NONE',  ( -22.48970261584618058, 12.58107241917856456, -223.4371365001174752 ) ) ;
#196530 = DIRECTION ( 'NONE',  ( 0.000000000000000000, -1.000000000000000000, 0.000000000000000000 ) ) ;
#196531 = DIRECTION ( 'NONE',  ( -1.000000000000000000, 0.000000000000000000, 0.000000000000000000 ) ) ;
#196532 = FACE_OUTER_BOUND ( 'NONE', #226222, .T. ) ;
#196533 = CARTESIAN_POINT ( 'NONE',  ( -18.59999999999999787, -1.164121893230052995, -108.2148480855716457 ) ) ;
#196534 = ORIENTED_EDGE ( 'NONE', *, *, #84274, .F. ) ;
#196535 = ADVANCED_FACE ( 'NONE', ( #124454 ), #51159, .T. ) ;
#196536 = DIRECTION ( 'NONE',  ( 0.000000000000000000, -0.4558084472153119959, 0.8900778951570285091 ) ) ;
#196537 = DIRECTION ( 'NONE',  ( 1.000000000000000000, -0.000000000000000000, -0.000000000000000000 ) ) ;
#196538 = DIRECTION ( 'NONE',  ( 1.000000000000000000, -0.000000000000000000, -0.000000000000000000 ) ) ;
#196539 = VECTOR ( 'NONE', #170058, 1000.000000000000000 ) ;
#196540 = CIRCLE ( 'NONE', #117450, 0.1000000000000002554 ) ;
#196541 = CARTESIAN_POINT ( 'NONE',  ( 20.59588692710267921, 65.63127657884294308, -61.88402639001368044 ) ) ;
#196542 = AXIS2_PLACEMENT_3D ( 'NONE', #213498, #193959, #253902 ) ;
#196543 = ORIENTED_EDGE ( 'NONE', *, *, #89467, .T. ) ;
#196544 = ORIENTED_EDGE ( 'NONE', *, *, #170422, .T. ) ;
#196545 = CARTESIAN_POINT ( 'NONE',  ( 18.39999999999999858, 85.60000000001186038, -96.42291809330220076 ) ) ;
#196546 = DIRECTION ( 'NONE',  ( -0.5932847527679298016, 0.7865547670005540448, 0.1713032417725961210 ) ) ;
#196548 = ADVANCED_FACE ( 'NONE', ( #203971 ), #127012, .F. ) ;
#196547 = LINE ( 'NONE', #96150, #26889 ) ;
#196549 = LINE ( 'NONE', #17907, #201356 ) ;
#196550 = CARTESIAN_POINT ( 'NONE',  ( -23.25000000000000000, 46.05992536685982230, -240.5730681801377102 ) ) ;
#196551 = ORIENTED_EDGE ( 'NONE', *, *, #176363, .F. ) ;
#196552 = CARTESIAN_POINT ( 'NONE',  ( -20.94999999999999929, -1.835859311432479268, -112.0044391687985694 ) ) ;
#196553 = ADVANCED_FACE ( 'NONE', ( #222229 ), #167931, .F. ) ;
#196554 = EDGE_CURVE ( 'NONE', #28425, #79078, #130478, .T. ) ;
#196555 = LINE ( 'NONE', #17912, #200837 ) ;
#196556 = ORIENTED_EDGE ( 'NONE', *, *, #175922, .T. ) ;
#196557 = CARTESIAN_POINT ( 'NONE',  ( -20.94999999999999929, 87.48912529308871910, -200.4231074845242802 ) ) ;
#196558 = DIRECTION ( 'NONE',  ( 0.000000000000000000, 0.9651348961777148627, -0.2617529984165062329 ) ) ;
#196559 = AXIS2_PLACEMENT_3D ( 'NONE', #57587, #38065, #237535 ) ;
#196560 = ADVANCED_FACE ( 'NONE', ( #104835 ), #107444, .F. ) ;
#196561 = EDGE_CURVE ( 'NONE', #13684, #139774, #47077, .T. ) ;
#196562 = ORIENTED_EDGE ( 'NONE', *, *, #248684, .T. ) ;
#196563 = CARTESIAN_POINT ( 'NONE',  ( 21.14999999999999858, 1.115600667400684642E-11, -60.45934304829879835 ) ) ;
#196564 = VERTEX_POINT ( 'NONE', #24084 ) ;
#196565 = DIRECTION ( 'NONE',  ( 0.000000000000000000, -1.616829647512364004E-14, 1.000000000000000000 ) ) ;
#196566 = CARTESIAN_POINT ( 'NONE',  ( 21.05000000000000071, 4.850467289730772791, -45.53426740900168568 ) ) ;
#196568 = EDGE_CURVE ( 'NONE', #117253, #128029, #162302, .T. ) ;
#196567 = FACE_OUTER_BOUND ( 'NONE', #232063, .T. ) ;
#196569 = DIRECTION ( 'NONE',  ( 1.000000000000000000, -0.000000000000000000, -0.000000000000000000 ) ) ;
#196570 = CARTESIAN_POINT ( 'NONE',  ( -23.25000000000000000, 18.38993523765007154, -239.7649653196623376 ) ) ;
#196571 = DIRECTION ( 'NONE',  ( 0.000000000000000000, -7.545205021724366615E-15, 1.000000000000000000 ) ) ;
#196572 = CARTESIAN_POINT ( 'NONE',  ( -23.25000000000000000, 85.00000000001188027, -93.12913836187181005 ) ) ;
#196573 = CARTESIAN_POINT ( 'NONE',  ( 23.14999999999999858, 1.115625160336667635E-11, -98.50000000000004263 ) ) ;
#196574 = EDGE_CURVE ( 'NONE', #76744, #257895, #217768, .T. ) ;
#196575 = CARTESIAN_POINT ( 'NONE',  ( 18.45068634130097962, -7.764979893827074875, -209.9256099644128994 ) ) ;
#196576 = FACE_OUTER_BOUND ( 'NONE', #24770, .T. ) ;
#196577 = DIRECTION ( 'NONE',  ( 0.000000000000000000, 1.000000000000000000, 6.982962677686266711E-15 ) ) ;
#196578 = CARTESIAN_POINT ( 'NONE',  ( 18.49999999999999289, 10.29270135741298731, -206.4573618871519045 ) ) ;
#196579 = ADVANCED_FACE ( 'NONE', ( #5751 ), #42340, .F. ) ;
#196580 = ADVANCED_FACE ( 'NONE', ( #223521, #161008 ), #164862, .F. ) ;
#196581 = FACE_OUTER_BOUND ( 'NONE', #231569, .T. ) ;
#196582 = DIRECTION ( 'NONE',  ( 1.000000000000000000, 0.000000000000000000, 0.000000000000000000 ) ) ;
#196583 = ORIENTED_EDGE ( 'NONE', *, *, #638, .T. ) ;
#196584 = DIRECTION ( 'NONE',  ( 0.000000000000000000, -0.5868805631290353597, -0.8096735173027127530 ) ) ;
#196586 = EDGE_CURVE ( 'NONE', #211036, #146445, #92008, .T. ) ;
#196585 = CARTESIAN_POINT ( 'NONE',  ( 23.14999999999999858, 4.999999999999997335, -21.09473398108690390 ) ) ;
#196587 = CARTESIAN_POINT ( 'NONE',  ( 20.22516295850462598, 9.899364295460458152, -41.41006571209138798 ) ) ;
#196588 = ORIENTED_EDGE ( 'NONE', *, *, #244459, .F. ) ;
#196589 = DIRECTION ( 'NONE',  ( 1.000000000000000000, -0.000000000000000000, -0.000000000000000000 ) ) ;
#196590 = EDGE_CURVE ( 'NONE', #133244, #55828, #138642, .T. ) ;
#196591 = ADVANCED_FACE ( 'NONE', ( #110008 ), #93016, .F. ) ;
#196592 = CARTESIAN_POINT ( 'NONE',  ( -15.55912972643740488, 8.490870273562565629, -20.94999999999999929 ) ) ;
#196593 = ORIENTED_EDGE ( 'NONE', *, *, #107069, .T. ) ;
#196594 = DIRECTION ( 'NONE',  ( 0.5932847527679310229, 0.3291107096594082515, -0.7346423231209699978 ) ) ;
#196595 = CARTESIAN_POINT ( 'NONE',  ( 23.25000000000000000, -9.599999999988842347, -157.6060308773475640 ) ) ;
#196596 = ADVANCED_FACE ( 'NONE', ( #211706 ), #188266, .T. ) ;
#196597 = AXIS2_PLACEMENT_3D ( 'NONE', #79453, #182441, #220286 ) ;
#196598 = VERTEX_POINT ( 'NONE', #207862 ) ;
#196599 = AXIS2_PLACEMENT_3D ( 'NONE', #180264, #99415, #117710 ) ;
#196600 = ORIENTED_EDGE ( 'NONE', *, *, #46739, .F. ) ;
#196601 = FACE_OUTER_BOUND ( 'NONE', #127286, .T. ) ;
#196602 = ORIENTED_EDGE ( 'NONE', *, *, #140216, .F. ) ;
#196603 = EDGE_CURVE ( 'NONE', #14611, #243577, #125619, .T. ) ;
#196604 = DIRECTION ( 'NONE',  ( 1.000000000000000000, -3.265361837132813093E-16, -2.280189983783949500E-30 ) ) ;
#196605 = EDGE_CURVE ( 'NONE', #186477, #81287, #1293, .T. ) ;
#196606 = CARTESIAN_POINT ( 'NONE',  ( -18.59999999999999787, 12.87592094156238609, -205.3750039893633073 ) ) ;
#196608 = CARTESIAN_POINT ( 'NONE',  ( -21.05000000000000071, 13.66123737402873495, -238.6633470470287648 ) ) ;
#196607 = UNCERTAINTY_MEASURE_WITH_UNIT (LENGTH_MEASURE( 1.000000000000000082E-05 ), #185899, 'distance_accuracy_value', 'NONE');
#196609 = CARTESIAN_POINT ( 'NONE',  ( -20.85000000000000142, 77.16412189325360771, -162.2082593989527197 ) ) ;
#196610 = DIRECTION ( 'NONE',  ( -1.000000000000000000, 0.000000000000000000, 0.000000000000000000 ) ) ;
#196611 = CARTESIAN_POINT ( 'NONE',  ( -12.84409460144754078, 46.89406695649162060, -234.6540829047535510 ) ) ;
#196612 = CIRCLE ( 'NONE', #121812, 0.09999999999999939493 ) ;
#196613 = PLANE ( 'NONE',  #1263 ) ;
#196614 = CARTESIAN_POINT ( 'NONE',  ( 22.47071067811864964, 0.3704148268517156728, -229.9999874772931037 ) ) ;
#196616 = ORIENTED_EDGE ( 'NONE', *, *, #140100, .T. ) ;
#196615 = CARTESIAN_POINT ( 'NONE',  ( 21.07954763557401634, 69.67070900997461536, -103.0889834031428620 ) ) ;
#196617 = ORIENTED_EDGE ( 'NONE', *, *, #75829, .T. ) ;
#196619 = DIRECTION ( 'NONE',  ( 0.000000000000000000, 0.2128009952263485993, -0.9770955615653341697 ) ) ;
#196618 = CARTESIAN_POINT ( 'NONE',  ( -20.94999999999999929, 11.65000000001115232, -160.7161343370219129 ) ) ;
#196621 = ORIENTED_EDGE ( 'NONE', *, *, #143546, .F. ) ;
#196620 = CARTESIAN_POINT ( 'NONE',  ( -23.25000000000000000, 74.08971962617978591, -56.89173962932539297 ) ) ;
#196622 = ORIENTED_EDGE ( 'NONE', *, *, #110318, .F. ) ;
#196623 = DIRECTION ( 'NONE',  ( 1.186688945009010077E-16, -1.000000000000000000, -0.000000000000000000 ) ) ;
#196624 = CARTESIAN_POINT ( 'NONE',  ( -21.65000000000000213, 68.25000000001230660, -157.6731074845243938 ) ) ;
#196625 = CARTESIAN_POINT ( 'NONE',  ( 20.94999999999999929, 62.98048128140158752, -207.0210305352945568 ) ) ;
#196626 = LINE ( 'NONE', #17988, #93245 ) ;
#196627 = CARTESIAN_POINT ( 'NONE',  ( -23.49999999999994316, 77.16254490893143725, -44.02310748452479316 ) ) ;
#196628 = CARTESIAN_POINT ( 'NONE',  ( -21.65000000000000213, 9.950000000011140600, -46.15000000000000568 ) ) ;
#196629 = DIRECTION ( 'NONE',  ( 0.000000000000000000, 0.2617529984165055668, 0.9651348961777149738 ) ) ;
#196630 = CIRCLE ( 'NONE', #142464, 0.1000000000000010186 ) ;
#196631 = CIRCLE ( 'NONE', #50877, 0.2000000000000057288 ) ;
#196633 = CIRCLE ( 'NONE', #5074, 0.6000000000000064171 ) ;
#196632 = DIRECTION ( 'NONE',  ( -1.000000000000000000, 0.000000000000000000, 0.000000000000000000 ) ) ;
#196635 = ORIENTED_EDGE ( 'NONE', *, *, #2504, .F. ) ;
#196634 = EDGE_CURVE ( 'NONE', #24890, #26416, #53897, .T. ) ;
#196636 = VERTEX_POINT ( 'NONE', #130859 ) ;
#196637 = DIRECTION ( 'NONE',  ( 0.000000000000000000, -1.734723475976997999E-14, 1.000000000000000000 ) ) ;
#196638 = ADVANCED_FACE ( 'NONE', ( #10931 ), #189567, .F. ) ;
#196639 = ORIENTED_EDGE ( 'NONE', *, *, #76212, .T. ) ;
#196640 = DIRECTION ( 'NONE',  ( 0.000000000000000000, -0.1350103645451807555, -0.9908441862701610203 ) ) ;
#196641 = EDGE_LOOP ( 'NONE', ( #179756, #75166, #42301, #35425 ) ) ;
#196642 = CARTESIAN_POINT ( 'NONE',  ( -22.49806830649814415, 64.35011034517307849, -136.6005718008498775 ) ) ;
#196643 = CARTESIAN_POINT ( 'NONE',  ( -15.75000000000000355, 48.12247445990688988, -234.1702647910923361 ) ) ;
#196644 = DIRECTION ( 'NONE',  ( -1.000000000000000000, -0.000000000000000000, -0.000000000000000000 ) ) ;
#196646 = ORIENTED_EDGE ( 'NONE', *, *, #15626, .F. ) ;
#196645 = DIRECTION ( 'NONE',  ( 0.000000000000000000, -7.056502275159890043E-15, 1.000000000000000000 ) ) ;
#196647 = CARTESIAN_POINT ( 'NONE',  ( 19.88284271247461632, 34.46644681994002468, -235.1135425616689076 ) ) ;
#196648 = ORIENTED_EDGE ( 'NONE', *, *, #153557, .F. ) ;
#196649 = DIRECTION ( 'NONE',  ( -1.000000000000000000, -3.265361837132813093E-16, 0.000000000000000000 ) ) ;
#196650 = VECTOR ( 'NONE', #126686, 1000.000000000000000 ) ;
#196651 = CARTESIAN_POINT ( 'NONE',  ( 24.30000000000000071, -12.79999999999999716, 33.00000000000000000 ) ) ;
#196652 = CARTESIAN_POINT ( 'NONE',  ( 22.88900146558018989, 8.703904791123973084, -54.34999999999999432 ) ) ;
#196653 = DIRECTION ( 'NONE',  ( -1.000000000000000000, -0.000000000000000000, 0.000000000000000000 ) ) ;
#196654 = CARTESIAN_POINT ( 'NONE',  ( -20.54999999999999716, 82.09643798151613225, -215.4278993322501208 ) ) ;
#196655 = ADVANCED_FACE ( 'NONE', ( #250802 ), #188738, .T. ) ;
#196656 = EDGE_LOOP ( 'NONE', ( #144751, #172547, #68646, #180125 ) ) ;
#196657 = DIRECTION ( 'NONE',  ( 0.000000000000000000, -0.8660254037844384856, 0.5000000000000003331 ) ) ;
#196658 = ORIENTED_EDGE ( 'NONE', *, *, #121852, .T. ) ;
#196661 = EDGE_LOOP ( 'NONE', ( #219534, #116910, #164561, #218910 ) ) ;
#196660 = DIRECTION ( 'NONE',  ( -2.602085213965226419E-14, -0.000000000000000000, 1.000000000000000000 ) ) ;
#196659 = CARTESIAN_POINT ( 'NONE',  ( -22.50000000000000000, 64.35042919246788529, -203.6231074845244393 ) ) ;
#196662 = AXIS2_PLACEMENT_3D ( 'NONE', #140976, #41884, #121431 ) ;
#196663 = CARTESIAN_POINT ( 'NONE',  ( -16.77683809663752257, 66.05000000001255955, -182.6731074845244223 ) ) ;
#196664 = LINE ( 'NONE', #218788, #137799 ) ;
#196665 = ORIENTED_EDGE ( 'NONE', *, *, #83875, .F. ) ;
#196666 = CARTESIAN_POINT ( 'NONE',  ( 18.39999999999999858, 85.68240343348848853, -129.8662641071115047 ) ) ;
#196667 = DIRECTION ( 'NONE',  ( 0.000000000000000000, -0.8660254037844377084, -0.5000000000000016653 ) ) ;
#196668 = DIRECTION ( 'NONE',  ( 1.000000000000000000, 0.000000000000000000, 0.000000000000000000 ) ) ;
#196670 = ORIENTED_EDGE ( 'NONE', *, *, #85404, .F. ) ;
#196669 = SPHERICAL_SURFACE ( 'NONE', #218380, 0.1000000000000000056 ) ;
#196671 = VECTOR ( 'NONE', #248807, 1000.000000000000000 ) ;
#196672 = FACE_OUTER_BOUND ( 'NONE', #247994, .T. ) ;
#196673 = AXIS2_PLACEMENT_3D ( 'NONE', #164300, #145998, #204678 ) ;
#196674 = ORIENTED_EDGE ( 'NONE', *, *, #36266, .F. ) ;
#196675 = VECTOR ( 'NONE', #154113, 1000.000000000000000 ) ;
#196676 = AXIS2_PLACEMENT_3D ( 'NONE', #210230, #112407, #49846 ) ;
#196677 = CARTESIAN_POINT ( 'NONE',  ( 19.97071067811864609, 62.39759438041176765, -208.9001066625100123 ) ) ;
#196678 = DIRECTION ( 'NONE',  ( 0.000000000000000000, 0.000000000000000000, -1.000000000000000000 ) ) ;
#196679 = DIRECTION ( 'NONE',  ( 0.000000000000000000, 0.008583690987128059571, -0.9999631594459056361 ) ) ;
#196680 = VERTEX_POINT ( 'NONE', #170040 ) ;
#196681 = CARTESIAN_POINT ( 'NONE',  ( -16.87845715379269507, 66.04214188611527447, -157.3993068334655447 ) ) ;
#196683 = ORIENTED_EDGE ( 'NONE', *, *, #9019, .F. ) ;
#196682 = CIRCLE ( 'NONE', #67503, 0.09999999999999939493 ) ;
#196684 = DIRECTION ( 'NONE',  ( 0.000000000000000000, -0.2617529984165032908, -0.9651348961777156399 ) ) ;
#196685 = DIRECTION ( 'NONE',  ( -0.000000000000000000, 1.000000000000000000, -0.000000000000000000 ) ) ;
#196686 = CARTESIAN_POINT ( 'NONE',  ( -16.97092634996683813, 10.00088896635997315, -46.13014276629746746 ) ) ;
#196687 = ORIENTED_EDGE ( 'NONE', *, *, #32369, .F. ) ;
#196688 = CARTESIAN_POINT ( 'NONE',  ( 20.94999999999999929, -8.999999999988842703, -57.10603087734755690 ) ) ;
#196689 = AXIS2_PLACEMENT_3D ( 'NONE', #176961, #243304, #180788 ) ;
#196690 = ADVANCED_FACE ( 'NONE', ( #248246 ), #147031, .T. ) ;
#196691 = PLANE ( 'NONE',  #234573 ) ;
#196692 = AXIS2_PLACEMENT_3D ( 'NONE', #126927, #115064, #52504 ) ;
#196693 = ADVANCED_FACE ( 'NONE', ( #90437 ), #52600, .T. ) ;
#196694 = VERTEX_POINT ( 'NONE', #149166 ) ;
#196695 = CIRCLE ( 'NONE', #5138, 0.1000000000000028644 ) ;
#196696 = AXIS2_PLACEMENT_3D ( 'NONE', #118552, #179800, #62411 ) ;
#196697 = DIRECTION ( 'NONE',  ( 1.000000000000000000, 0.000000000000000000, 0.000000000000000000 ) ) ;
#196698 = CARTESIAN_POINT ( 'NONE',  ( -21.65000000000000213, 7.249999999999983125, -9.250000000000001776 ) ) ;
#196700 = CARTESIAN_POINT ( 'NONE',  ( 21.05000000000000071, 76.00000000001237765, -170.0231074845243597 ) ) ;
#196699 = AXIS2_PLACEMENT_3D ( 'NONE', #253743, #34302, #53838 ) ;
#196701 = ORIENTED_EDGE ( 'NONE', *, *, #125729, .F. ) ;
#196702 = CIRCLE ( 'NONE', #26044, 0.1000000000000013933 ) ;
#196703 = EDGE_CURVE ( 'NONE', #220164, #136504, #234535, .T. ) ;
#196704 = CARTESIAN_POINT ( 'NONE',  ( 23.40000000000005187, 77.83551161375991967, -47.62760213295649692 ) ) ;
#196705 = ORIENTED_EDGE ( 'NONE', *, *, #169348, .F. ) ;
#196707 = EDGE_LOOP ( 'NONE', ( #49527, #83750, #99819, #146580, #177677 ) ) ;
#196706 = CARTESIAN_POINT ( 'NONE',  ( -18.39999999999999858, 77.26488334054519669, -241.9697969554615611 ) ) ;
#196708 = CIRCLE ( 'NONE', #217542, 0.1000000000000041550 ) ;
#196709 = EDGE_CURVE ( 'NONE', #214744, #100973, #9676, .T. ) ;
#196712 = VERTEX_POINT ( 'NONE', #129586 ) ;
#196711 = ORIENTED_EDGE ( 'NONE', *, *, #210720, .T. ) ;
#196710 = DIRECTION ( 'NONE',  ( -1.000000000000000000, 0.000000000000000000, -0.000000000000000000 ) ) ;
#196713 = CARTESIAN_POINT ( 'NONE',  ( 23.40000000000005542, 77.83551161375991967, -47.52760213295649550 ) ) ;
#196714 = CARTESIAN_POINT ( 'NONE',  ( -21.09813707148783735, 0.03135149954058748939, -161.1149378942632779 ) ) ;
#196715 = DIRECTION ( 'NONE',  ( -1.000000000000000000, 0.000000000000000000, -0.000000000000000000 ) ) ;
#196716 = EDGE_CURVE ( 'NONE', #202898, #107904, #109628, .T. ) ;
#196717 = CARTESIAN_POINT ( 'NONE',  ( -16.87683809663750623, 12.57413723904470082, -211.9780204941619104 ) ) ;
#196718 = DIRECTION ( 'NONE',  ( 0.000000000000000000, -0.9908441862701610203, 0.1350103645451807555 ) ) ;
#196719 = CIRCLE ( 'NONE', #88564, 0.1000000000000043771 ) ;
#196720 = CARTESIAN_POINT ( 'NONE',  ( -23.15000000000000213, 74.07476635515219243, -115.7533510176504450 ) ) ;
#196721 = CARTESIAN_POINT ( 'NONE',  ( -20.85000000000000142, 67.23127455305835554, -235.8551265064784559 ) ) ;
#196724 = CYLINDRICAL_SURFACE ( 'NONE', #180608, 0.1000000000000013933 ) ;
#196723 = CARTESIAN_POINT ( 'NONE',  ( -18.50000000000000000, 14.80545736607782814, -235.9842437978701639 ) ) ;
#196722 = AXIS2_PLACEMENT_3D ( 'NONE', #178263, #56969, #257706 ) ;
#196725 = VERTEX_POINT ( 'NONE', #89157 ) ;
#196726 = ORIENTED_EDGE ( 'NONE', *, *, #153064, .F. ) ;
#196727 = ORIENTED_EDGE ( 'NONE', *, *, #52260, .T. ) ;
#196728 = CARTESIAN_POINT ( 'NONE',  ( -21.44999999999999929, 68.65000000001199965, -115.3731074845243540 ) ) ;
#196730 = ORIENTED_EDGE ( 'NONE', *, *, #251274, .F. ) ;
#196729 = CYLINDRICAL_SURFACE ( 'NONE', #207710, 0.09999999999999939493 ) ;
#196731 = LINE ( 'NONE', #160209, #142493 ) ;
#196732 = EDGE_LOOP ( 'NONE', ( #256194, #13833, #77825, #80203 ) ) ;
#196733 = EDGE_CURVE ( 'NONE', #212838, #211733, #142932, .T. ) ;
#196734 = LINE ( 'NONE', #75534, #247525 ) ;
#196735 = VERTEX_POINT ( 'NONE', #74784 ) ;
#196736 = CARTESIAN_POINT ( 'NONE',  ( -16.81744102076748959, 66.05000000001224691, -149.1731074845244223 ) ) ;
#196737 = VERTEX_POINT ( 'NONE', #154331 ) ;
#196738 = LINE ( 'NONE', #97617, #77085 ) ;
#196739 = DIRECTION ( 'NONE',  ( 0.000000000000000000, 0.000000000000000000, 1.000000000000000000 ) ) ;
#196740 = VECTOR ( 'NONE', #130100, 1000.000000000000000 ) ;
#196742 = ORIENTED_EDGE ( 'NONE', *, *, #211255, .F. ) ;
#196741 = ORIENTED_EDGE ( 'NONE', *, *, #142926, .T. ) ;
#196743 = ORIENTED_EDGE ( 'NONE', *, *, #65728, .F. ) ;
#196744 = CARTESIAN_POINT ( 'NONE',  ( -21.64999999999999858, 7.350000000011155166, -79.25000000000004263 ) ) ;
#196745 = ORIENTED_EDGE ( 'NONE', *, *, #27473, .T. ) ;
#196746 = ORIENTED_EDGE ( 'NONE', *, *, #154179, .T. ) ;
#196747 = PLANE ( 'NONE',  #117762 ) ;
#196748 = TOROIDAL_SURFACE ( 'NONE', #176126, 11.65000000000000036, 0.1000000000000000056 ) ;
#196750 = ORIENTED_EDGE ( 'NONE', *, *, #13535, .T. ) ;
#196749 = CARTESIAN_POINT ( 'NONE',  ( -18.59999999999999787, 1.835341550235567887, -179.0551512925629538 ) ) ;
#196752 = CARTESIAN_POINT ( 'NONE',  ( 20.95132126680579887, 65.51005012986553311, -162.4527829460899113 ) ) ;
#196751 = CARTESIAN_POINT ( 'NONE',  ( 19.58285714285715073, 59.20544293262641133, -225.7731470885128715 ) ) ;
#196753 = DIRECTION ( 'NONE',  ( 0.000000000000000000, -0.2128009952263604232, 0.9770955615653316162 ) ) ;
#196754 = CARTESIAN_POINT ( 'NONE',  ( -22.45305610364635385, 76.10085836911147794, -215.2726746080137161 ) ) ;
#196755 = ORIENTED_EDGE ( 'NONE', *, *, #135287, .T. ) ;
#196756 = ORIENTED_EDGE ( 'NONE', *, *, #124144, .F. ) ;
#196757 = FACE_OUTER_BOUND ( 'NONE', #159855, .T. ) ;
#196758 = DIRECTION ( 'NONE',  ( 0.000000000000000000, 0.9126074666063660468, 0.4088369013363524762 ) ) ;
#196759 = ORIENTED_EDGE ( 'NONE', *, *, #157174, .T. ) ;
#196760 = DIRECTION ( 'NONE',  ( 0.000000000000000000, -0.1298341882520022694, -0.9915357197604853789 ) ) ;
#196761 = EDGE_CURVE ( 'NONE', #127382, #188971, #176302, .T. ) ;
#196762 = CARTESIAN_POINT ( 'NONE',  ( -16.93262454970419384, 51.66793538483853609, -231.8674831426984042 ) ) ;
#196763 = DIRECTION ( 'NONE',  ( 0.000000000000000000, -6.982962677686266711E-15, 1.000000000000000000 ) ) ;
#196764 = ORIENTED_EDGE ( 'NONE', *, *, #192225, .F. ) ;
#196765 = ORIENTED_EDGE ( 'NONE', *, *, #88771, .F. ) ;
#196766 = LINE ( 'NONE', #182365, #121717 ) ;
#196767 = CARTESIAN_POINT ( 'NONE',  ( 20.85000000000000142, 7.021664781911246322, -137.8335654018973457 ) ) ;
#196768 = ORIENTED_EDGE ( 'NONE', *, *, #141381, .F. ) ;
#196769 = CARTESIAN_POINT ( 'NONE',  ( 18.59999999999999076, 69.35000000001151932, -48.17310748452437252 ) ) ;
#196770 = ORIENTED_EDGE ( 'NONE', *, *, #169046, .T. ) ;
#196771 = CYLINDRICAL_SURFACE ( 'NONE', #193913, 0.1000000000000026007 ) ;
#196774 = ADVANCED_FACE ( 'NONE', ( #177729 ), #159431, .F. ) ;
#196773 = DIRECTION ( 'NONE',  ( 1.000000000000000000, 0.000000000000000000, 0.000000000000000000 ) ) ;
#196772 = SHAPE_REPRESENTATION ( 'Injection Molded Chain Links 6', ( #2425 ), #252581 ) ;
#196776 = CARTESIAN_POINT ( 'NONE',  ( -22.59066674512246209, 55.88295497714577920, -232.8089693692780600 ) ) ;
#196775 = CARTESIAN_POINT ( 'NONE',  ( -20.12071067811865888, 66.67928932189363422, -157.6731074845244223 ) ) ;
#196777 = CARTESIAN_POINT ( 'NONE',  ( -18.39999999999999858, 13.18938849241619593, -207.6453216105643946 ) ) ;
#196778 = DIRECTION ( 'NONE',  ( 0.000000000000000000, -3.469446951953515108E-14, 1.000000000000000000 ) ) ;
#196779 = EDGE_CURVE ( 'NONE', #56802, #170560, #242906, .T. ) ;
#196780 = ADVANCED_FACE ( 'NONE', ( #16084 ), #26447, .T. ) ;
#196781 = VECTOR ( 'NONE', #190141, 1000.000000000000000 ) ;
#196782 = CARTESIAN_POINT ( 'NONE',  ( -18.34374000495059676, 54.09900352584866567, -229.1663746252470446 ) ) ;
#196783 = CIRCLE ( 'NONE', #84294, 0.09999999999999939493 ) ;
#196785 = ORIENTED_EDGE ( 'NONE', *, *, #62653, .T. ) ;
#196784 = ORIENTED_EDGE ( 'NONE', *, *, #127465, .T. ) ;
#196786 = ORIENTED_EDGE ( 'NONE', *, *, #55339, .T. ) ;
#196787 = AXIS2_PLACEMENT_3D ( 'NONE', #255126, #214766, #40023 ) ;
#196788 = DIRECTION ( 'NONE',  ( -2.316152573905153269E-15, -0.9910465087640865089, 0.1335171055202867274 ) ) ;
#196789 = CYLINDRICAL_SURFACE ( 'NONE', #53288, 0.09999999999999892308 ) ;
#196790 = CARTESIAN_POINT ( 'NONE',  ( 20.94999999999999929, 85.00000000001222134, -146.4170766071767389 ) ) ;
#196791 = CARTESIAN_POINT ( 'NONE',  ( 22.59999999999999432, 75.90000000001172964, -81.17267829206912211 ) ) ;
#196793 = ADVANCED_FACE ( 'NONE', ( #233824 ), #99419, .T. ) ;
#196792 = B_SPLINE_CURVE_WITH_KNOTS ( 'NONE', 3,
 ( #30558, #69684, #85341, #104896 ),
 .UNSPECIFIED., .F., .F.,
 ( 4, 4 ),
 ( 0.000000000000000000, 0.0001048066582182452479 ),
 .UNSPECIFIED. ) ;
#196795 = CARTESIAN_POINT ( 'NONE',  ( -23.25000000000000000, 7.783179459866048866, -245.3643104511423019 ) ) ;
#196794 = FACE_OUTER_BOUND ( 'NONE', #220903, .T. ) ;
#196796 = VERTEX_POINT ( 'NONE', #138537 ) ;
#196797 = EDGE_CURVE ( 'NONE', #102643, #161835, #117716, .T. ) ;
#196798 = CARTESIAN_POINT ( 'NONE',  ( -20.64999999999999858, 85.00000000001197975, -112.9170766071766820 ) ) ;
#196799 = EDGE_LOOP ( 'NONE', ( #173507, #245613, #211770, #11932 ) ) ;
#196800 = ORIENTED_EDGE ( 'NONE', *, *, #143408, .T. ) ;
#196801 = LINE ( 'NONE', #13068, #79325 ) ;
#196803 = VECTOR ( 'NONE', #197391, 1000.000000000000114 ) ;
#196802 = DIRECTION ( 'NONE',  ( 0.000000000000000000, -1.000000000000000000, -0.000000000000000000 ) ) ;
#196804 = DIRECTION ( 'NONE',  ( -1.000000000000000000, -0.000000000000000000, -0.000000000000000000 ) ) ;
#196805 = CIRCLE ( 'NONE', #5239, 0.09999999999999939493 ) ;
#196806 = DIRECTION ( 'NONE',  ( 0.000000000000000000, 0.1575546449569757979, -0.9875102702516471709 ) ) ;
#196807 = ORIENTED_EDGE ( 'NONE', *, *, #165273, .T. ) ;
#196808 = ORIENTED_EDGE ( 'NONE', *, *, #228526, .F. ) ;
#196809 = CARTESIAN_POINT ( 'NONE',  ( 23.15000000000000213, 87.65000000001172964, -72.62310748452422615 ) ) ;
#196810 = ADVANCED_FACE ( 'NONE', ( #219375 ), #35654, .T. ) ;
#196811 = VECTOR ( 'NONE', #225485, 1000.000000000000114 ) ;
#196812 = FACE_OUTER_BOUND ( 'NONE', #8282, .T. ) ;
#196814 = ORIENTED_EDGE ( 'NONE', *, *, #136604, .T. ) ;
#196813 = EDGE_CURVE ( 'NONE', #252467, #59289, #256250, .T. ) ;
#196815 = CARTESIAN_POINT ( 'NONE',  ( -16.87242674293850797, 22.97710641253713959, -230.9345486045511109 ) ) ;
#196816 = DIRECTION ( 'NONE',  ( 0.000000000000000000, -1.000000000000000000, 0.000000000000000000 ) ) ;
#196817 = ADVANCED_FACE ( 'NONE', ( #237672 ), #172231, .T. ) ;
#196818 = CARTESIAN_POINT ( 'NONE',  ( -23.25000000000000000, 74.00000000001223555, -149.7477294072864709 ) ) ;
#196819 = CARTESIAN_POINT ( 'NONE',  ( -21.05000000000000071, 1.261786168576181755, -108.5864989635455089 ) ) ;
#196820 = DIRECTION ( 'NONE',  ( 0.000000000000000000, -0.8700118002898321601, 0.4930308989875230030 ) ) ;
#196821 = AXIS2_PLACEMENT_3D ( 'NONE', #154746, #80282, #174339 ) ;
#196824 = CYLINDRICAL_SURFACE ( 'NONE', #58041, 0.09999999999999939493 ) ;
#196823 = CIRCLE ( 'NONE', #200924, 0.2000000000000000944 ) ;
#196822 = DIRECTION ( 'NONE',  ( 1.000000000000000000, -0.000000000000000000, 0.000000000000000000 ) ) ;
#196826 = PLANE ( 'NONE',  #91626 ) ;
#196825 = AXIS2_PLACEMENT_3D ( 'NONE', #16049, #57694, #116416 ) ;
#196827 = AXIS2_PLACEMENT_3D ( 'NONE', #3689, #62392, #45389 ) ;
#196828 = DIRECTION ( 'NONE',  ( 0.000000000000000000, 1.000000000000000000, 6.982962677686266711E-15 ) ) ;
#196829 = FACE_OUTER_BOUND ( 'NONE', #162225, .T. ) ;
#196830 = DIRECTION ( 'NONE',  ( 0.000000000000000000, 0.9999631594459056361, -0.008583690987128059571 ) ) ;
#196832 = VERTEX_POINT ( 'NONE', #176433 ) ;
#196831 = FACE_OUTER_BOUND ( 'NONE', #236080, .T. ) ;
#196833 = CARTESIAN_POINT ( 'NONE',  ( 18.79999999999999716, 1.149999999999999911, -15.00000000000000000 ) ) ;
#196834 = ORIENTED_EDGE ( 'NONE', *, *, #227532, .F. ) ;
#196835 = SPHERICAL_SURFACE ( 'NONE', #228478, 0.1000000000000000056 ) ;
#196836 = EDGE_LOOP ( 'NONE', ( #43216, #96348, #209756, #21967 ) ) ;
#196837 = ADVANCED_FACE ( 'NONE', ( #60301 ), #255892, .F. ) ;
#196838 = FACE_OUTER_BOUND ( 'NONE', #209088, .T. ) ;
#196839 = DIRECTION ( 'NONE',  ( -1.000000000000000000, 0.000000000000000000, 0.000000000000000000 ) ) ;
#196841 = AXIS2_PLACEMENT_3D ( 'NONE', #216830, #156899, #60322 ) ;
#196840 = FACE_OUTER_BOUND ( 'NONE', #74893, .T. ) ;
#196842 = VECTOR ( 'NONE', #39004, 1000.000000000000000 ) ;
#196843 = CYLINDRICAL_SURFACE ( 'NONE', #14111, 0.1000000000000000472 ) ;
#196844 = CARTESIAN_POINT ( 'NONE',  ( 18.54286124688534088, 85.62391757880946841, -62.78190515266153682 ) ) ;
#196845 = CARTESIAN_POINT ( 'NONE',  ( -20.54999999999999716, 68.76258920191057200, -222.5680764032308048 ) ) ;
#196846 = ORIENTED_EDGE ( 'NONE', *, *, #190993, .F. ) ;
#196847 = CARTESIAN_POINT ( 'NONE',  ( -18.59999999999999787, 1.851028230152016674, -112.1539132694225316 ) ) ;
#196849 = VERTEX_POINT ( 'NONE', #94294 ) ;
#196848 = DIRECTION ( 'NONE',  ( 0.000000000000000000, 0.4088369013363281623, -0.9126074666063771490 ) ) ;
#196850 = DIRECTION ( 'NONE',  ( 0.000000000000000000, 0.000000000000000000, -1.000000000000000000 ) ) ;
#196851 = EDGE_CURVE ( 'NONE', #82762, #184062, #76483, .T. ) ;
#196852 = AXIS2_PLACEMENT_3D ( 'NONE', #7175, #104967, #110143 ) ;
#196853 = CARTESIAN_POINT ( 'NONE',  ( -18.59999999999999787, 72.02722222756958104, -225.1832529173024398 ) ) ;
#196854 = CARTESIAN_POINT ( 'NONE',  ( -20.94999999999999929, 1.115600667400684642E-11, -167.5000000000000284 ) ) ;
#196855 = ORIENTED_EDGE ( 'NONE', *, *, #111805, .F. ) ;
#196856 = LINE ( 'NONE', #100312, #30477 ) ;
#196857 = AXIS2_PLACEMENT_3D ( 'NONE', #119573, #240788, #141672 ) ;
#196858 = ADVANCED_FACE ( 'NONE', ( #19923, #113867 ), #193424, .F. ) ;
#196859 = APPLICATION_PROTOCOL_DEFINITION ( 'draft international standard', 'automotive_design', 1998, #247326 ) ;
#196861 = CIRCLE ( 'NONE', #234264, 0.2000000000000057288 ) ;
#196860 = DIRECTION ( 'NONE',  ( 0.000000000000000000, -0.2617529984164856383, -0.9651348961777204138 ) ) ;
#196862 = ORIENTED_EDGE ( 'NONE', *, *, #101413, .T. ) ;
#196863 = AXIS2_PLACEMENT_3D ( 'NONE', #106913, #166937, #226866 ) ;
#196865 = EDGE_CURVE ( 'NONE', #2197, #243331, #83684, .T. ) ;
#196864 = DIRECTION ( 'NONE',  ( 0.000000000000000000, -6.938893903907222067E-15, 1.000000000000000000 ) ) ;
#196866 = DIRECTION ( 'NONE',  ( 1.000000000000000000, 0.000000000000000000, 0.000000000000000000 ) ) ;
#196867 = CIRCLE ( 'NONE', #251018, 0.09999999999999939493 ) ;
#196868 = AXIS2_PLACEMENT_3D ( 'NONE', #125995, #243376, #146831 ) ;
#196869 = CIRCLE ( 'NONE', #213428, 11.89999999999999325 ) ;
#196870 = EDGE_CURVE ( 'NONE', #201070, #87569, #251269, .T. ) ;
#196871 = EDGE_CURVE ( 'NONE', #230513, #32681, #109808, .T. ) ;
#196872 = CARTESIAN_POINT ( 'NONE',  ( -16.77828822459933633, 9.946229375067616729, -121.3373717490810861 ) ) ;
#196873 = ORIENTED_EDGE ( 'NONE', *, *, #234639, .F. ) ;
#196874 = ORIENTED_EDGE ( 'NONE', *, *, #142678, .T. ) ;
#196875 = LINE ( 'NONE', #241160, #5625 ) ;
#196877 = AXIS2_PLACEMENT_3D ( 'NONE', #249446, #129491, #190777 ) ;
#196876 = CARTESIAN_POINT ( 'NONE',  ( 21.04999999999908411, 8.776282895301829257, -45.65790900265250229 ) ) ;
#196879 = AXIS2_PLACEMENT_3D ( 'NONE', #117329, #196848, #97729 ) ;
#196878 = CARTESIAN_POINT ( 'NONE',  ( -23.39999999999994529, 87.50449464844290048, -34.18759587077607165 ) ) ;
#196880 = DIRECTION ( 'NONE',  ( 0.000000000000000000, -0.8814952561688444987, 0.4721928772777320149 ) ) ;
#196881 = CARTESIAN_POINT ( 'NONE',  ( 18.49999999999999289, 10.23906162413259402, -125.2543974345976778 ) ) ;
#196883 = FACE_OUTER_BOUND ( 'NONE', #134500, .T. ) ;
#196882 = DIRECTION ( 'NONE',  ( 0.000000000000000000, 8.673617379884087537E-15, -1.000000000000000000 ) ) ;
#196884 = AXIS2_PLACEMENT_3D ( 'NONE', #145381, #82808, #42434 ) ;
#196885 = CARTESIAN_POINT ( 'NONE',  ( -18.40000000000000213, 5.650000000011139001, -121.3500000000000369 ) ) ;
#196886 = CARTESIAN_POINT ( 'NONE',  ( -20.94999999999999929, 87.65000000001144542, -39.02310748452423894 ) ) ;
#196887 = SPHERICAL_SURFACE ( 'NONE', #87944, 0.1000000000000000056 ) ;
#196888 = CARTESIAN_POINT ( 'NONE',  ( -16.86422026484316916, 9.970447360871808939, -146.5822132256730299 ) ) ;
#196889 = VERTEX_POINT ( 'NONE', #21221 ) ;
#196890 = EDGE_CURVE ( 'NONE', #62787, #89611, #105508, .T. ) ;
#196891 = VERTEX_POINT ( 'NONE', #4180 ) ;
#196892 = CARTESIAN_POINT ( 'NONE',  ( 18.59999999999998366, 1.115600667400684642E-11, -100.5000000000000426 ) ) ;
#196893 = EDGE_CURVE ( 'NONE', #63429, #67858, #184644, .T. ) ;
#196895 = DIRECTION ( 'NONE',  ( -1.000000000000000000, 0.000000000000000000, 0.000000000000000000 ) ) ;
#196894 = CARTESIAN_POINT ( 'NONE',  ( 21.07928932188134397, 69.67148334361836248, -69.62200263017875557 ) ) ;
#196896 = AXIS2_PLACEMENT_3D ( 'NONE', #94255, #257135, #56402 ) ;
#196897 = AXIS2_PLACEMENT_3D ( 'NONE', #255633, #156626, #236117 ) ;
#196898 =( GEOMETRIC_REPRESENTATION_CONTEXT ( 3 ) GLOBAL_UNCERTAINTY_ASSIGNED_CONTEXT ( ( #257884 ) ) GLOBAL_UNIT_ASSIGNED_CONTEXT ( ( #223454, #164787, #44835 ) ) REPRESENTATION_CONTEXT ( 'NONE', 'WORKASPACE' ) );
#196899 = LINE ( 'NONE', #75693, #160145 ) ;
#196901 = ADVANCED_FACE ( 'NONE', ( #181568 ), #146257, .T. ) ;
#196900 = DIRECTION ( 'NONE',  ( 1.000000000000000000, -0.000000000000000000, 0.000000000000000000 ) ) ;
#196902 = CARTESIAN_POINT ( 'NONE',  ( 21.05000000000000071, 74.83729825007408465, -128.6231074845242972 ) ) ;
#196903 = ORIENTED_EDGE ( 'NONE', *, *, #127389, .T. ) ;
#196904 = ORIENTED_EDGE ( 'NONE', *, *, #115962, .F. ) ;
#196905 = ADVANCED_FACE ( 'NONE', ( #1612 ), #105833, .F. ) ;
#196906 = CARTESIAN_POINT ( 'NONE',  ( -20.94999999999999929, 64.35000000001160458, -62.50830171387039513 ) ) ;
#196907 = VERTEX_POINT ( 'NONE', #26333 ) ;
#196908 = CARTESIAN_POINT ( 'NONE',  ( 20.94999999999999929, 5.000000000011153745, -88.09473398108696074 ) ) ;
#196909 = EDGE_CURVE ( 'NONE', #118509, #27654, #203678, .T. ) ;
#196910 = VECTOR ( 'NONE', #182583, 1000.000000000000000 ) ;
#196911 = AXIS2_PLACEMENT_3D ( 'NONE', #79217, #117092, #158807 ) ;
#196912 = VECTOR ( 'NONE', #57180, 1000.000000000000000 ) ;
#196913 = CARTESIAN_POINT ( 'NONE',  ( 18.48413544395649666, 85.66430403363912660, -29.34000249148596140 ) ) ;
#196914 = EDGE_CURVE ( 'NONE', #2577, #22950, #40785, .T. ) ;
#196915 = VERTEX_POINT ( 'NONE', #2889 ) ;
#196916 = CARTESIAN_POINT ( 'NONE',  ( -18.59999999999999787, 11.65000000001115232, -45.65000000000000568 ) ) ;
#196917 = EDGE_LOOP ( 'NONE', ( #200237, #12479, #1225, #231826, #187318 ) ) ;
#196918 = CARTESIAN_POINT ( 'NONE',  ( -15.55912972643741199, 8.490870273573719373, -180.1499999999999773 ) ) ;
#196919 = ADVANCED_FACE ( 'NONE', ( #143694 ), #88955, .F. ) ;
#196920 = CARTESIAN_POINT ( 'NONE',  ( -23.15000000000000213, -11.48912529306489994, -130.9000000000000341 ) ) ;
#196921 = DIRECTION ( 'NONE',  ( 1.000000000000000000, 0.000000000000000000, 0.000000000000000000 ) ) ;
#196922 = FACE_OUTER_BOUND ( 'NONE', #204857, .T. ) ;
#196923 = CARTESIAN_POINT ( 'NONE',  ( 21.05000000000000071, 65.63213158188987961, -242.1335211407336772 ) ) ;
#196924 = CARTESIAN_POINT ( 'NONE',  ( 18.51024323315077069, 65.68895814178262071, -131.0026557862138361 ) ) ;
#196925 = DIRECTION ( 'NONE',  ( 0.000000000000000000, 0.000000000000000000, 1.000000000000000000 ) ) ;
#196926 = ORIENTED_EDGE ( 'NONE', *, *, #145877, .F. ) ;
#196928 = LINE ( 'NONE', #256852, #172684 ) ;
#196927 = DIRECTION ( 'NONE',  ( 1.000000000000000000, 0.000000000000000000, 0.000000000000000000 ) ) ;
#196929 = VERTEX_POINT ( 'NONE', #82412 ) ;
#196931 = ORIENTED_EDGE ( 'NONE', *, *, #94860, .T. ) ;
#196930 = DIRECTION ( 'NONE',  ( 0.000000000000000000, -0.5273008465188072647, 0.8496786552930167824 ) ) ;
#196932 = ORIENTED_EDGE ( 'NONE', *, *, #47618, .T. ) ;
#196933 = DIRECTION ( 'NONE',  ( 1.000000000000000000, 0.000000000000000000, -0.000000000000000000 ) ) ;
#196934 = CARTESIAN_POINT ( 'NONE',  ( -21.93340585898929973, 1.115541036281197940E-11, -26.17585297787465137 ) ) ;
#196935 = CARTESIAN_POINT ( 'NONE',  ( -20.65000000000000568, 68.75000000001261924, -190.8731074845244109 ) ) ;
#196936 = CARTESIAN_POINT ( 'NONE',  ( -20.94999999999999929, 87.39257802171739797, -72.59705706435616435 ) ) ;
#196937 = AXIS2_PLACEMENT_3D ( 'NONE', #243099, #43628, #163576 ) ;
#196938 = ORIENTED_EDGE ( 'NONE', *, *, #4902, .F. ) ;
#196939 = DIRECTION ( 'NONE',  ( 0.5932847527679299127, -0.8049926720990051576, 6.366092712777055223E-16 ) ) ;
#196940 = DIRECTION ( 'NONE',  ( 0.000000000000000000, 1.000000000000000000, 6.982962677686266711E-15 ) ) ;
#196941 = CARTESIAN_POINT ( 'NONE',  ( 16.27683809663749770, 66.65000000001234071, -160.7731074845244166 ) ) ;
#196942 = ORIENTED_EDGE ( 'NONE', *, *, #38507, .T. ) ;
#196943 = PLANE ( 'NONE',  #173491 ) ;
#196944 = CARTESIAN_POINT ( 'NONE',  ( 21.14999999999999858, 11.65000000001115943, -45.65000000000000568 ) ) ;
#196945 = ORIENTED_EDGE ( 'NONE', *, *, #172087, .T. ) ;
#196946 = ORIENTED_EDGE ( 'NONE', *, *, #226546, .F. ) ;
#196947 = CIRCLE ( 'NONE', #209417, 0.09999999999998898659 ) ;
#196948 = ORIENTED_EDGE ( 'NONE', *, *, #84117, .F. ) ;
#196949 = CARTESIAN_POINT ( 'NONE',  ( -20.64999999999999858, 74.00000000001151079, -48.84772940728643675 ) ) ;
#196950 = ORIENTED_EDGE ( 'NONE', *, *, #14166, .T. ) ;
#196951 = DIRECTION ( 'NONE',  ( 0.000000000000000000, 0.000000000000000000, 1.000000000000000000 ) ) ;
#196952 = EDGE_CURVE ( 'NONE', #11085, #68838, #162006, .T. ) ;
#196953 = LINE ( 'NONE', #118733, #81522 ) ;
#196954 = DIRECTION ( 'NONE',  ( 0.000000000000000000, 0.000000000000000000, -1.000000000000000000 ) ) ;
#196955 = CARTESIAN_POINT ( 'NONE',  ( -23.15000000000000213, 1.115600667400684642E-11, -132.0000000000000284 ) ) ;
#196957 = CIRCLE ( 'NONE', #184481, 0.09999999999999939493 ) ;
#196956 = CARTESIAN_POINT ( 'NONE',  ( -21.44999999999999929, 68.85000000001259934, -191.1731074845243938 ) ) ;
#196958 = DIRECTION ( 'NONE',  ( -1.000000000000000000, 0.000000000000000000, 0.000000000000000000 ) ) ;
#196960 = ADVANCED_FACE ( 'NONE', ( #221924 ), #241519, .F. ) ;
#196959 = CARTESIAN_POINT ( 'NONE',  ( -20.64999999999999858, 74.07476635515219243, -115.7533510176504450 ) ) ;
#196961 = ORIENTED_EDGE ( 'NONE', *, *, #87305, .F. ) ;
#196963 = DIRECTION ( 'NONE',  ( 0.000000000000000000, -0.9126074666063769270, -0.4088369013363280513 ) ) ;
#196962 = CARTESIAN_POINT ( 'NONE',  ( 20.85000000000000142, 17.16609282392354174, -224.6038045889790453 ) ) ;
#196965 = ORIENTED_EDGE ( 'NONE', *, *, #138912, .T. ) ;
#196964 = CIRCLE ( 'NONE', #55461, 1.749999999999999778 ) ;
#196968 = ORIENTED_EDGE ( 'NONE', *, *, #247165, .T. ) ;
#196967 = CARTESIAN_POINT ( 'NONE',  ( -18.50000000000000000, 77.16270174995010223, -128.4231074845242802 ) ) ;
#196966 = CARTESIAN_POINT ( 'NONE',  ( -21.14999999999994174, 64.25000000001119815, -51.02310748452479316 ) ) ;
#196969 = ORIENTED_EDGE ( 'NONE', *, *, #95881, .F. ) ;
#196970 = CARTESIAN_POINT ( 'NONE',  ( 13.40000000000000036, -8.279289321881350361, 15.00000000000000355 ) ) ;
#196971 = DIRECTION ( 'NONE',  ( -1.000000000000000000, 0.000000000000000000, -0.000000000000000000 ) ) ;
#196973 = CARTESIAN_POINT ( 'NONE',  ( 0.000000000000000000, -11.65000000000000036, 32.89999999999999858 ) ) ;
#196972 = CIRCLE ( 'NONE', #84501, 0.1000000000000028644 ) ;
#196974 = CARTESIAN_POINT ( 'NONE',  ( -18.35668295345803713, 64.52683809664974035, -145.7731074845244450 ) ) ;
#196975 = EDGE_LOOP ( 'NONE', ( #148931, #7463, #7377, #200284 ) ) ;
#196976 = CARTESIAN_POINT ( 'NONE',  ( 19.75857864376269291, 16.76897757977919667, -222.7804130109903156 ) ) ;
#196977 = FACE_OUTER_BOUND ( 'NONE', #153375, .T. ) ;
#196979 = DIRECTION ( 'NONE',  ( -0.7071067811865474617, -0.3338907855510734324, -0.6233112732207618523 ) ) ;
#196978 = DIRECTION ( 'NONE',  ( 0.000000000000000000, 0.9908441862701596881, -0.1350103645451904977 ) ) ;
#196981 = ORIENTED_EDGE ( 'NONE', *, *, #123843, .T. ) ;
#196980 = CARTESIAN_POINT ( 'NONE',  ( -20.85000000000000142, 79.19526988099229925, -196.1889237952725296 ) ) ;
#196982 = CIRCLE ( 'NONE', #251127, 0.1000000000000028644 ) ;
#196983 = AXIS2_PLACEMENT_3D ( 'NONE', #76420, #16482, #78966 ) ;
#196984 = VERTEX_POINT ( 'NONE', #84976 ) ;
#196985 = LINE ( 'NONE', #117475, #122188 ) ;
#196986 = VERTEX_POINT ( 'NONE', #202395 ) ;
#196987 = DIRECTION ( 'NONE',  ( -0.000000000000000000, 0.8660254037844424824, 0.4999999999999934497 ) ) ;
#196988 = ORIENTED_EDGE ( 'NONE', *, *, #28915, .F. ) ;
#196990 = CIRCLE ( 'NONE', #84526, 12.87499999999999822 ) ;
#196989 = FACE_OUTER_BOUND ( 'NONE', #110392, .T. ) ;
#196991 = LINE ( 'NONE', #18371, #124334 ) ;
#196992 = DIRECTION ( 'NONE',  ( 1.000000000000000000, 0.000000000000000000, 0.000000000000000000 ) ) ;
#196993 = ORIENTED_EDGE ( 'NONE', *, *, #94440, .T. ) ;
#196994 = DIRECTION ( 'NONE',  ( 0.000000000000000000, 0.000000000000000000, -1.000000000000000000 ) ) ;
#196995 = VECTOR ( 'NONE', #44851, 1000.000000000000000 ) ;
#196996 = TOROIDAL_SURFACE ( 'NONE', #121996, 0.2000000000000000111, 0.1000000000000000056 ) ;
#196998 = EDGE_CURVE ( 'NONE', #234281, #212214, #165852, .T. ) ;
#196997 = CIRCLE ( 'NONE', #5452, 0.09999999999998712696 ) ;
#196999 = AXIS2_PLACEMENT_3D ( 'NONE', #38436, #94546, #114111 ) ;
#197000 = EDGE_CURVE ( 'NONE', #7959, #10735, #230439, .T. ) ;
#197001 = CYLINDRICAL_SURFACE ( 'NONE', #2303, 0.09999999999999781286 ) ;
#197002 = ORIENTED_EDGE ( 'NONE', *, *, #24475, .T. ) ;
#197003 = ORIENTED_EDGE ( 'NONE', *, *, #87299, .T. ) ;
#197004 = DIRECTION ( 'NONE',  ( -1.000000000000000000, 0.000000000000000000, -0.000000000000000000 ) ) ;
#197005 = ORIENTED_EDGE ( 'NONE', *, *, #96368, .T. ) ;
#197006 = ADVANCED_FACE ( 'NONE', ( #144967 ), #224517, .F. ) ;
#197007 = ORIENTED_EDGE ( 'NONE', *, *, #198946, .F. ) ;
#197009 = ORIENTED_EDGE ( 'NONE', *, *, #222460, .F. ) ;
#197008 = DIRECTION ( 'NONE',  ( 0.000000000000000000, 0.4999999999999689138, -0.8660254037844565822 ) ) ;
#197010 = EDGE_CURVE ( 'NONE', #218009, #217695, #118007, .T. ) ;
#197011 = ORIENTED_EDGE ( 'NONE', *, *, #236515, .T. ) ;
#197014 = ORIENTED_EDGE ( 'NONE', *, *, #192530, .T. ) ;
#197013 = ORIENTED_EDGE ( 'NONE', *, *, #241188, .T. ) ;
#197012 = CARTESIAN_POINT ( 'NONE',  ( 18.54999999999999716, 52.34166666667822199, -52.77310748452448763 ) ) ;
#197015 = CIRCLE ( 'NONE', #251169, 0.1000000000000094008 ) ;
#197016 = CIRCLE ( 'NONE', #230339, 0.09999999999998898659 ) ;
#197018 = ADVANCED_FACE ( 'NONE', ( #186696 ), #126390, .T. ) ;
#197017 = VERTEX_POINT ( 'NONE', #129277 ) ;
#197019 = DIRECTION ( 'NONE',  ( -3.265361837132813093E-16, -1.000000000000000000, 7.445645354460596589E-46 ) ) ;
#197020 = CARTESIAN_POINT ( 'NONE',  ( -20.94999999999999929, 76.00000000001207923, -128.6231074845242972 ) ) ;
#197021 = DIRECTION ( 'NONE',  ( 0.000000000000000000, -0.9274965247785504907, -0.3738317757009320674 ) ) ;
#197022 = ORIENTED_EDGE ( 'NONE', *, *, #62469, .T. ) ;
#197023 = AXIS2_PLACEMENT_3D ( 'NONE', #29346, #163685, #245788 ) ;
#197024 = DIRECTION ( 'NONE',  ( -0.000000000000000000, -0.4088369013363281068, 0.9126074666063770380 ) ) ;
#197026 = ORIENTED_EDGE ( 'NONE', *, *, #244362, .T. ) ;
#197025 = CARTESIAN_POINT ( 'NONE',  ( -20.94999999999999929, -11.48912529307605546, -30.50000000000000000 ) ) ;
#197027 = DIRECTION ( 'NONE',  ( 0.000000000000000000, -1.000000000000000000, -8.717686153663073805E-15 ) ) ;
#197029 = ORIENTED_EDGE ( 'NONE', *, *, #242143, .F. ) ;
#197028 = DIRECTION ( 'NONE',  ( 1.000000000000000000, 0.000000000000000000, 0.000000000000000000 ) ) ;
#197030 = ADVANCED_FACE ( 'NONE', ( #108431 ), #70617, .F. ) ;
#197031 = ORIENTED_EDGE ( 'NONE', *, *, #189526, .F. ) ;
#197032 = LINE ( 'NONE', #73288, #32301 ) ;
#197033 = DIRECTION ( 'NONE',  ( 1.000000000000000000, 0.000000000000000000, 0.000000000000000000 ) ) ;
#197034 = AXIS2_PLACEMENT_3D ( 'NONE', #193810, #33489, #72594 ) ;
#197035 = AXIS2_PLACEMENT_3D ( 'NONE', #240374, #20050, #179138 ) ;
#197037 = VERTEX_POINT ( 'NONE', #90125 ) ;
#197036 = AXIS2_PLACEMENT_3D ( 'NONE', #207029, #28430, #167929 ) ;
#197038 = VERTEX_POINT ( 'NONE', #167154 ) ;
#197039 = DIRECTION ( 'NONE',  ( 0.000000000000000000, 0.000000000000000000, 1.000000000000000000 ) ) ;
#197040 = CARTESIAN_POINT ( 'NONE',  ( -21.07928932188134397, 0.09889514566555075714, -161.1714833436066385 ) ) ;
#197041 = AXIS2_PLACEMENT_3D ( 'NONE', #55508, #52972, #193781 ) ;
#197043 = ORIENTED_EDGE ( 'NONE', *, *, #222621, .T. ) ;
#197042 = ORIENTED_EDGE ( 'NONE', *, *, #32828, .F. ) ;
#197044 = ORIENTED_EDGE ( 'NONE', *, *, #242558, .T. ) ;
#197045 = CARTESIAN_POINT ( 'NONE',  ( -22.39999999999999858, 64.18196446391819165, -247.0985338183330668 ) ) ;
#197046 = ORIENTED_EDGE ( 'NONE', *, *, #239573, .T. ) ;
#197047 = VERTEX_POINT ( 'NONE', #206249 ) ;
#197048 = CARTESIAN_POINT ( 'NONE',  ( 23.24999999999999289, 29.08883969319483498, -237.9520757887960940 ) ) ;
#197049 = EDGE_LOOP ( 'NONE', ( #224006, #110071, #194211, #175072 ) ) ;
#197050 = DIRECTION ( 'NONE',  ( 0.000000000000000000, 0.000000000000000000, 1.000000000000000000 ) ) ;
#197051 = AXIS2_PLACEMENT_3D ( 'NONE', #126610, #91352, #169639 ) ;
#197053 = DIRECTION ( 'NONE',  ( 0.000000000000000000, 7.147358527629766941E-15, -1.000000000000000000 ) ) ;
#197052 = CARTESIAN_POINT ( 'NONE',  ( -23.25000000000000355, 64.25000000001264766, -194.2731074845244450 ) ) ;
#197054 = EDGE_CURVE ( 'NONE', #113973, #220002, #28940, .T. ) ;
#197056 = ORIENTED_EDGE ( 'NONE', *, *, #151169, .T. ) ;
#197055 = AXIS2_PLACEMENT_3D ( 'NONE', #77639, #172960, #212058 ) ;
#197058 = EDGE_LOOP ( 'NONE', ( #156528, #190355, #141501, #41708, #64670 ) ) ;
#197057 = ORIENTED_EDGE ( 'NONE', *, *, #185296, .T. ) ;
#197059 = AXIS2_PLACEMENT_3D ( 'NONE', #200884, #40573, #137064 ) ;
#197060 = DIRECTION ( 'NONE',  ( 0.000000000000000000, 0.8660254037844309360, -0.5000000000000134337 ) ) ;
#197061 = EDGE_LOOP ( 'NONE', ( #191329, #81756, #161120, #231573 ) ) ;
#197062 = AXIS2_PLACEMENT_3D ( 'NONE', #103999, #10065, #129990 ) ;
#197063 = CIRCLE ( 'NONE', #159671, 0.09999999999999939493 ) ;
#197064 = CIRCLE ( 'NONE', #193005, 0.1000000000000054040 ) ;
#197065 = EDGE_CURVE ( 'NONE', #234543, #97016, #13971, .T. ) ;
#197066 = AXIS2_PLACEMENT_3D ( 'NONE', #226000, #147798, #30422 ) ;
#197067 = CARTESIAN_POINT ( 'NONE',  ( -21.65000000000000213, 12.43531352672262003, -211.3405985074572300 ) ) ;
#197068 = VERTEX_POINT ( 'NONE', #249233 ) ;
#197069 = VERTEX_POINT ( 'NONE', #187974 ) ;
#197070 = CARTESIAN_POINT ( 'NONE',  ( 20.95000000000005258, 67.65000000001118963, -25.49719488170504533 ) ) ;
#197071 = ORIENTED_EDGE ( 'NONE', *, *, #126242, .F. ) ;
#197072 = CARTESIAN_POINT ( 'NONE',  ( 21.05000000000000071, 87.65000000001192859, -106.1231074845242262 ) ) ;
#197073 = DIRECTION ( 'NONE',  ( 0.000000000000000000, -1.000000000000000000, 0.000000000000000000 ) ) ;
#197074 = ORIENTED_EDGE ( 'NONE', *, *, #98701, .T. ) ;
#197075 = DIRECTION ( 'NONE',  ( 0.000000000000000000, 0.000000000000000000, -1.000000000000000000 ) ) ;
#197077 = EDGE_CURVE ( 'NONE', #117921, #86585, #172301, .T. ) ;
#197076 = DIRECTION ( 'NONE',  ( -1.000000000000000000, 0.000000000000000000, 0.000000000000000000 ) ) ;
#197079 = CARTESIAN_POINT ( 'NONE',  ( -20.54999999999999716, 1.999999999999998224, -13.22462192276210224 ) ) ;
#197078 = DIRECTION ( 'NONE',  ( 1.000000000000000000, 0.000000000000000000, 0.000000000000000000 ) ) ;
#197080 = DIRECTION ( 'NONE',  ( 0.000000000000000000, -6.530723674265620862E-15, 1.000000000000000000 ) ) ;
#197081 = FACE_OUTER_BOUND ( 'NONE', #23397, .T. ) ;
#197082 = CYLINDRICAL_SURFACE ( 'NONE', #3383, 0.1000000000000028644 ) ;
#197083 = DIRECTION ( 'NONE',  ( -1.000000000000000000, 0.000000000000000000, 0.000000000000000000 ) ) ;
#197084 = CARTESIAN_POINT ( 'NONE',  ( 11.60000000000000320, -9.650000000000002132, 17.60000000000000497 ) ) ;
#197085 = CARTESIAN_POINT ( 'NONE',  ( -23.39999999999994529, 76.00000000001119815, -36.02310748452479316 ) ) ;
#197086 = EDGE_CURVE ( 'NONE', #75446, #58850, #215243, .T. ) ;
#197087 = CIRCLE ( 'NONE', #163784, 2.000000000000001776 ) ;
#197089 = VERTEX_POINT ( 'NONE', #47141 ) ;
#197088 = AXIS2_PLACEMENT_3D ( 'NONE', #16414, #94635, #158500 ) ;
#197090 = AXIS2_PLACEMENT_3D ( 'NONE', #3596, #222625, #80539 ) ;
#197091 = AXIS2_PLACEMENT_3D ( 'NONE', #205690, #213391, #212134 ) ;
#197093 = ORIENTED_EDGE ( 'NONE', *, *, #205577, .T. ) ;
#197092 = ORIENTED_EDGE ( 'NONE', *, *, #178933, .F. ) ;
#197094 = EDGE_LOOP ( 'NONE', ( #79045, #113050, #40778, #83732 ) ) ;
#197095 = ORIENTED_EDGE ( 'NONE', *, *, #170213, .F. ) ;
#197096 = CARTESIAN_POINT ( 'NONE',  ( -21.11927991906891577, 0.009083679485028806067, -94.05150688150853000 ) ) ;
#197098 = EDGE_CURVE ( 'NONE', #57195, #108495, #193043, .T. ) ;
#197097 =( BOUNDED_CURVE ( )  B_SPLINE_CURVE ( 3, ( #35596, #255842, #52543, #132098 ),
 .UNSPECIFIED., .F., .F. ) 
 B_SPLINE_CURVE_WITH_KNOTS ( ( 4, 4 ),
 ( 0.3000847527772385614, 0.5517402753107881752 ),
 .UNSPECIFIED. ) 
 CURVE ( )  GEOMETRIC_REPRESENTATION_ITEM ( )  RATIONAL_B_SPLINE_CURVE ( ( 1.000000000000000000, 0.9947294176030464508, 0.9947294176030464508, 1.000000000000000000 ) ) 
 REPRESENTATION_ITEM ( '' )  );
#197099 = CARTESIAN_POINT ( 'NONE',  ( -20.64999999999999858, 4.350000000011156054, -112.7500000000000284 ) ) ;
#197101 = DIRECTION ( 'NONE',  ( 1.000000000000000000, 0.000000000000000000, -0.000000000000000000 ) ) ;
#197100 = DIRECTION ( 'NONE',  ( 0.000000000000000000, -6.982962677686266711E-15, 1.000000000000000000 ) ) ;
#197102 = ORIENTED_EDGE ( 'NONE', *, *, #24050, .F. ) ;
#197103 = EDGE_CURVE ( 'NONE', #70015, #109498, #87559, .T. ) ;
#197104 = LINE ( 'NONE', #156739, #30004 ) ;
#197105 = EDGE_CURVE ( 'NONE', #144474, #151867, #59724, .T. ) ;
#197106 = B_SPLINE_CURVE_WITH_KNOTS ( 'NONE', 3,
 ( #10313, #85944, #143380, #104235 ),
 .UNSPECIFIED., .F., .F.,
 ( 4, 4 ),
 ( 0.000000000000000000, 0.0002118541922231925311 ),
 .UNSPECIFIED. ) ;
#197107 = FACE_OUTER_BOUND ( 'NONE', #25809, .T. ) ;
#197108 = FACE_OUTER_BOUND ( 'NONE', #109187, .T. ) ;
#197109 = ORIENTED_EDGE ( 'NONE', *, *, #99089, .F. ) ;
#197110 = CARTESIAN_POINT ( 'NONE',  ( -23.25000000000000000, 1.115600667400684642E-11, -134.0000000000000284 ) ) ;
#197111 = ADVANCED_FACE ( 'NONE', ( #71884 ), #226318, .T. ) ;
#197112 = AXIS2_PLACEMENT_3D ( 'NONE', #64170, #201105, #101975 ) ;
#197113 = ORIENTED_EDGE ( 'NONE', *, *, #230207, .F. ) ;
#197114 = LINE ( 'NONE', #35524, #33122 ) ;
#197115 = CARTESIAN_POINT ( 'NONE',  ( -21.05000000000000071, -11.65000000000000036, -3.000000000000002665 ) ) ;
#197116 = EDGE_CURVE ( 'NONE', #201392, #192382, #27647, .T. ) ;
#197117 = CARTESIAN_POINT ( 'NONE',  ( -17.11825945287481332, 10.05000000001113847, -121.3500000000000369 ) ) ;
#197118 = FACE_OUTER_BOUND ( 'NONE', #135969, .T. ) ;
#197119 = ADVANCED_FACE ( 'NONE', ( #189257 ), #34834, .F. ) ;
#197120 = CARTESIAN_POINT ( 'NONE',  ( -23.25000000000000000, 1.115600667400684642E-11, -200.9999999999999432 ) ) ;
#197121 = ORIENTED_EDGE ( 'NONE', *, *, #112105, .T. ) ;
#197122 = DIRECTION ( 'NONE',  ( 0.000000000000000000, 0.2617529984165031243, 0.9651348961777157509 ) ) ;
#197123 = DIRECTION ( 'NONE',  ( -0.000000000000000000, 1.000000000000000000, -0.000000000000000000 ) ) ;
#197124 = FACE_OUTER_BOUND ( 'NONE', #107257, .T. ) ;
#197125 = B_SPLINE_CURVE_WITH_KNOTS ( 'NONE', 3,
 ( #201974, #62464, #139402, #221507, #119889, #199420, #100271, #122438, #160302, #182422 ),
 .UNSPECIFIED., .F., .F.,
 ( 4, 3, 3, 4 ),
 ( 0.000000000000000000, 0.0002000000000008536833, 0.001000000000082972495, 0.001967863649483314603 ),
 .UNSPECIFIED. ) ;
#197127 = CARTESIAN_POINT ( 'NONE',  ( 23.25000000000000000, -11.74999999998883560, -88.75000000000004263 ) ) ;
#197126 = CARTESIAN_POINT ( 'NONE',  ( 20.85000000000000142, 77.26327546522891510, -61.62124281777789037 ) ) ;
#197128 = CARTESIAN_POINT ( 'NONE',  ( 18.59999999999998721, 70.29876110920605470, -198.0544810472949564 ) ) ;
#197129 = CARTESIAN_POINT ( 'NONE',  ( 21.07928932188134397, 0.09889514566555242248, -27.17148334360669537 ) ) ;
#197130 = CARTESIAN_POINT ( 'NONE',  ( -18.39999999999999858, 64.52683809664983983, -160.7232782360584338 ) ) ;
#197131 = CARTESIAN_POINT ( 'NONE',  ( 22.50000000000000000, 75.90000000001202807, -114.6726782920691221 ) ) ;
#197132 = VECTOR ( 'NONE', #134743, 1000.000000000000000 ) ;
#197133 = ORIENTED_EDGE ( 'NONE', *, *, #62636, .T. ) ;
#197134 = CIRCLE ( 'NONE', #138835, 0.1000000000000064587 ) ;
#197135 = TOROIDAL_SURFACE ( 'NONE', #147640, 0.2000000000000000111, 0.1000000000000000056 ) ;
#197136 = ORIENTED_EDGE ( 'NONE', *, *, #139807, .T. ) ;
#197137 = LINE ( 'NONE', #13387, #169555 ) ;
#197138 = EDGE_CURVE ( 'NONE', #67782, #94150, #22363, .T. ) ;
#197139 = VERTEX_POINT ( 'NONE', #191850 ) ;
#197140 = EDGE_CURVE ( 'NONE', #233724, #159477, #221691, .T. ) ;
#197141 = CARTESIAN_POINT ( 'NONE',  ( -23.25000000000000000, -9.599999999988838795, -124.1060308773475924 ) ) ;
#197142 = EDGE_CURVE ( 'NONE', #138601, #7989, #201393, .T. ) ;
#197144 = DIRECTION ( 'NONE',  ( 0.000000000000000000, -0.4999999999999649170, 0.8660254037844589137 ) ) ;
#197143 = CIRCLE ( 'NONE', #172065, 0.2000000000000057288 ) ;
#197145 = DIRECTION ( 'NONE',  ( 0.000000000000000000, 0.000000000000000000, -1.000000000000000000 ) ) ;
#197146 = EDGE_LOOP ( 'NONE', ( #162616, #211252, #56511, #82092 ) ) ;
#197147 = CIRCLE ( 'NONE', #26484, 0.09999999999999939493 ) ;
#197148 = CARTESIAN_POINT ( 'NONE',  ( -16.93860193097148326, 30.27088047374820334, -234.7927206923158963 ) ) ;
#197149 = CIRCLE ( 'NONE', #113946, 0.09999999999999939493 ) ;
#197150 = CARTESIAN_POINT ( 'NONE',  ( -15.73854595235691178, 9.351413679112543065, -50.48034356754896379 ) ) ;
#197151 = CARTESIAN_POINT ( 'NONE',  ( -18.50596464788227635, 65.69367753730655579, -97.51892380663478832 ) ) ;
#197152 = AXIS2_PLACEMENT_3D ( 'NONE', #255336, #170776, #57163 ) ;
#197153 = DIRECTION ( 'NONE',  ( 0.000000000000000000, 0.2617529984165031243, 0.9651348961777157509 ) ) ;
#197155 = ORIENTED_EDGE ( 'NONE', *, *, #31581, .T. ) ;
#197154 = DIRECTION ( 'NONE',  ( 0.000000000000000000, -7.109473446599835262E-15, 1.000000000000000000 ) ) ;
#197157 = CYLINDRICAL_SURFACE ( 'NONE', #67099, 0.09999999999999520384 ) ;
#197156 = CARTESIAN_POINT ( 'NONE',  ( -20.54999999999999716, 11.60058429089262333, -246.3380203656811887 ) ) ;
#197158 = FACE_OUTER_BOUND ( 'NONE', #90116, .T. ) ;
#197159 = DIRECTION ( 'NONE',  ( -0.7071067811865475727, -0.7071067811865475727, 0.000000000000000000 ) ) ;
#197160 = FACE_OUTER_BOUND ( 'NONE', #176543, .T. ) ;
#197161 = DIRECTION ( 'NONE',  ( 1.000000000000000000, 0.000000000000000000, -0.000000000000000000 ) ) ;
#197162 = ORIENTED_EDGE ( 'NONE', *, *, #240855, .T. ) ;
#197163 = CIRCLE ( 'NONE', #247228, 0.1000000000000002554 ) ;
#197164 = EDGE_CURVE ( 'NONE', #123954, #174920, #9862, .T. ) ;
#197165 = DIRECTION ( 'NONE',  ( 0.000000000000000000, 0.000000000000000000, 1.000000000000000000 ) ) ;
#197166 = DIRECTION ( 'NONE',  ( -3.265361837132813093E-16, -1.000000000000000000, -6.938893903907229955E-15 ) ) ;
#197167 = AXIS2_PLACEMENT_3D ( 'NONE', #94290, #99416, #193421 ) ;
#197168 = ORIENTED_EDGE ( 'NONE', *, *, #67837, .T. ) ;
#197169 = EDGE_CURVE ( 'NONE', #11088, #191619, #163995, .T. ) ;
#197170 = DIRECTION ( 'NONE',  ( 0.000000000000000000, -1.000000000000000000, -6.982962677686266711E-15 ) ) ;
#197171 = EDGE_LOOP ( 'NONE', ( #7529, #68212, #215494 ) ) ;
#197172 = DIRECTION ( 'NONE',  ( -1.836970198721029934E-16, -0.4088369013363280513, 0.9126074666063769270 ) ) ;
#197173 = CARTESIAN_POINT ( 'NONE',  ( -16.94389599337535657, 9.991197989756724240, -20.89235519820161358 ) ) ;
#197174 = ADVANCED_FACE ( 'NONE', ( #174873 ), #93984, .T. ) ;
#197175 = LINE ( 'NONE', #176362, #207594 ) ;
#197176 = ORIENTED_EDGE ( 'NONE', *, *, #112424, .T. ) ;
#197177 = ORIENTED_EDGE ( 'NONE', *, *, #161339, .F. ) ;
#197178 = CIRCLE ( 'NONE', #34923, 0.1000000000000054040 ) ;
#197179 = EDGE_CURVE ( 'NONE', #249334, #222623, #133885, .T. ) ;
#197180 = CIRCLE ( 'NONE', #184707, 3.999999999999999112 ) ;
#197181 = AXIS2_PLACEMENT_3D ( 'NONE', #88170, #193432, #233833 ) ;
#197182 = VECTOR ( 'NONE', #256797, 1000.000000000000000 ) ;
#197183 = CARTESIAN_POINT ( 'NONE',  ( 23.24999999999999645, 76.00000000001142553, -36.02310748452432421 ) ) ;
#197184 = DIRECTION ( 'NONE',  ( 0.000000000000000000, 0.000000000000000000, -1.000000000000000000 ) ) ;
#197185 = CARTESIAN_POINT ( 'NONE',  ( -16.77180007708461318, 63.08949790057268103, -213.1137372711198452 ) ) ;
#197186 = CARTESIAN_POINT ( 'NONE',  ( -18.39999999999999858, -9.519327731081281385, -140.9729763765593589 ) ) ;
#197187 = EDGE_CURVE ( 'NONE', #12756, #106580, #176129, .T. ) ;
#197189 = CARTESIAN_POINT ( 'NONE',  ( -20.65000000000000568, 70.35000000001210196, -127.2731074845243313 ) ) ;
#197188 = DIRECTION ( 'NONE',  ( -1.073024830501117923E-15, -0.9126074666063771490, -0.4088369013363281623 ) ) ;
#197191 = MANIFOLD_SOLID_BREP ( 'Stock-MAS-200-1', #157355 ) ;
#197190 = DIRECTION ( 'NONE',  ( -0.000000000000000000, -0.9651348961777157509, 0.2617529984165031243 ) ) ;
#197192 = CARTESIAN_POINT ( 'NONE',  ( 21.11344571971268635, 65.38212097649370946, -90.77708659212511577 ) ) ;
#197193 = CARTESIAN_POINT ( 'NONE',  ( 22.59999954896768770, 76.00882823225471441, -148.2736161585922616 ) ) ;
#197194 = ORIENTED_EDGE ( 'NONE', *, *, #254605, .F. ) ;
#197195 = CARTESIAN_POINT ( 'NONE',  ( -21.05000000000000071, -0.2561057920922211739, 0.03489644167229202787 ) ) ;
#197196 = EDGE_CURVE ( 'NONE', #56225, #82405, #173594, .T. ) ;
#197198 = ORIENTED_EDGE ( 'NONE', *, *, #170133, .T. ) ;
#197197 = CARTESIAN_POINT ( 'NONE',  ( 21.05000000000000071, 76.00000000001244871, -170.0231074845243597 ) ) ;
#197199 = CARTESIAN_POINT ( 'NONE',  ( 22.39999999999999503, -0.09999999998884338825, -88.85042919245522341 ) ) ;
#197201 = ADVANCED_FACE ( 'NONE', ( #34065 ), #160582, .F. ) ;
#197200 = EDGE_CURVE ( 'NONE', #219843, #127058, #68321, .T. ) ;
#197202 = CARTESIAN_POINT ( 'NONE',  ( 23.14999999999999858, 3.900000000011155432, -167.5000000000000284 ) ) ;
#197204 = CARTESIAN_POINT ( 'NONE',  ( 18.54999999999999716, 22.41143600680915782, -231.9928577185252152 ) ) ;
#197203 = DIRECTION ( 'NONE',  ( 0.000000000000000000, 0.2128009952263403282, -0.9770955615653358350 ) ) ;
#197205 =( BOUNDED_CURVE ( )  B_SPLINE_CURVE ( 3, ( #60260, #142367, #141101, #100645 ),
 .UNSPECIFIED., .F., .F. ) 
 B_SPLINE_CURVE_WITH_KNOTS ( ( 4, 4 ),
 ( 4.712388980384687898, 5.672655318024669491 ),
 .UNSPECIFIED. ) 
 CURVE ( )  GEOMETRIC_REPRESENTATION_ITEM ( )  RATIONAL_B_SPLINE_CURVE ( ( 1.000000000000000000, 0.9246222802177384015, 0.9246222802177384015, 1.000000000000000000 ) ) 
 REPRESENTATION_ITEM ( '' )  );
#197206 = VERTEX_POINT ( 'NONE', #105512 ) ;
#197208 = DIRECTION ( 'NONE',  ( 0.000000000000000000, 0.9126074666063660468, 0.4088369013363524762 ) ) ;
#197207 = DIRECTION ( 'NONE',  ( 1.000000000000000000, 1.646408749285562691E-14, 1.073024830501117725E-15 ) ) ;
#197209 = CARTESIAN_POINT ( 'NONE',  ( -21.05000000000000071, -0.09999999998884338825, -55.35042919245524473 ) ) ;
#197210 = DIRECTION ( 'NONE',  ( -0.000000000000000000, -6.982962677686266711E-15, 1.000000000000000000 ) ) ;
#197211 = DIRECTION ( 'NONE',  ( 1.000000000000000000, 0.000000000000000000, 0.000000000000000000 ) ) ;
#197212 = CARTESIAN_POINT ( 'NONE',  ( 18.49999999999998934, 19.85039924724470950, -136.2803030578013761 ) ) ;
#197213 = VERTEX_POINT ( 'NONE', #202090 ) ;
#197214 = FACE_BOUND ( 'NONE', #129031, .T. ) ;
#197215 = ORIENTED_EDGE ( 'NONE', *, *, #188905, .T. ) ;
#197216 = AXIS2_PLACEMENT_3D ( 'NONE', #213273, #13802, #94609 ) ;
#197217 = CIRCLE ( 'NONE', #201305, 0.1000000000000028783 ) ;
#197218 = CARTESIAN_POINT ( 'NONE',  ( -18.45140287520617761, -9.486077739529564568, -40.14052312668610512 ) ) ;
#197219 = ORIENTED_EDGE ( 'NONE', *, *, #112142, .F. ) ;
#197220 = CARTESIAN_POINT ( 'NONE',  ( -20.94983749550516450, 46.34703458179515678, -243.0587802416264651 ) ) ;
#197221 = CIRCLE ( 'NONE', #81058, 0.1000000000000028644 ) ;
#197222 = ADVANCED_FACE ( 'NONE', ( #160422 ), #22184, .T. ) ;
#197223 = EDGE_CURVE ( 'NONE', #252869, #61629, #76676, .T. ) ;
#197224 = ORIENTED_EDGE ( 'NONE', *, *, #38212, .T. ) ;
#197225 = CARTESIAN_POINT ( 'NONE',  ( -21.22070241538126112, 6.469946272880768845, -167.4010809694649424 ) ) ;
#197226 = AXIS2_PLACEMENT_3D ( 'NONE', #74449, #154001, #135649 ) ;
#197227 = EDGE_CURVE ( 'NONE', #83940, #237434, #126578, .T. ) ;
#197228 = VECTOR ( 'NONE', #97656, 1000.000000000000000 ) ;
#197229 = FACE_OUTER_BOUND ( 'NONE', #168725, .T. ) ;
#197230 = EDGE_LOOP ( 'NONE', ( #76297, #96551, #182352, #182944 ) ) ;
#197231 = ADVANCED_FACE ( 'NONE', ( #84659 ), #125129, .T. ) ;
#197232 = CIRCLE ( 'NONE', #13890, 0.1999999999999987899 ) ;
#197233 = LINE ( 'NONE', #19900, #30099 ) ;
#197234 = EDGE_CURVE ( 'NONE', #221002, #10713, #234914, .T. ) ;
#197236 = CIRCLE ( 'NONE', #134674, 0.1000000000000024342 ) ;
#197235 = CARTESIAN_POINT ( 'NONE',  ( -20.64999999999999858, 34.89593390941166007, -248.6067769466879156 ) ) ;
#197237 = DIRECTION ( 'NONE',  ( -1.000000000000000000, 0.000000000000000000, -0.000000000000000000 ) ) ;
#197239 = AXIS2_PLACEMENT_3D ( 'NONE', #121080, #221400, #58476 ) ;
#197238 = CARTESIAN_POINT ( 'NONE',  ( -20.94999999999999929, 1.835341550235569663, -112.0551512925630249 ) ) ;
#197240 = DIRECTION ( 'NONE',  ( -1.000000000000000000, 0.000000000000000000, 0.000000000000000000 ) ) ;
#197241 = AXIS2_PLACEMENT_3D ( 'NONE', #116297, #195842, #53735 ) ;
#197242 = CARTESIAN_POINT ( 'NONE',  ( 19.75857864376269646, 62.46583972339645641, -208.9186153945276487 ) ) ;
#197243 = EDGE_LOOP ( 'NONE', ( #76400, #19180 ) ) ;
#197244 = DIRECTION ( 'NONE',  ( -1.073024830501117725E-15, -6.982962677686266711E-15, 1.000000000000000000 ) ) ;
#197245 = ORIENTED_EDGE ( 'NONE', *, *, #219553, .F. ) ;
#197247 = VERTEX_POINT ( 'NONE', #3882 ) ;
#197246 = DIRECTION ( 'NONE',  ( -1.000000000000000000, 0.000000000000000000, -0.000000000000000000 ) ) ;
#197248 = AXIS2_PLACEMENT_3D ( 'NONE', #4546, #84043, #206613 ) ;
#197249 = ORIENTED_EDGE ( 'NONE', *, *, #136681, .T. ) ;
#197250 = DIRECTION ( 'NONE',  ( 0.000000000000000000, -0.1575844902526687130, -0.9875055080513762684 ) ) ;
#197251 = DIRECTION ( 'NONE',  ( 0.000000000000000000, -1.000000000000000000, -6.982962677686265922E-15 ) ) ;
#197252 = CARTESIAN_POINT ( 'NONE',  ( 20.94999999999999929, 77.83534155023599510, -57.96795619196132776 ) ) ;
#197253 = ORIENTED_EDGE ( 'NONE', *, *, #78514, .F. ) ;
#197254 = EDGE_CURVE ( 'NONE', #70167, #176282, #101662, .T. ) ;
#197255 = CARTESIAN_POINT ( 'NONE',  ( -16.89020380669786547, 9.950000000011137047, -146.7574111481105774 ) ) ;
#197257 = DIRECTION ( 'NONE',  ( 1.000000000000000000, 0.000000000000000000, 0.000000000000000000 ) ) ;
#197256 = AXIS2_PLACEMENT_3D ( 'NONE', #142009, #22088, #83298 ) ;
#197258 = ORIENTED_EDGE ( 'NONE', *, *, #49664, .T. ) ;
#197260 = VERTEX_POINT ( 'NONE', #162979 ) ;
#197259 = LINE ( 'NONE', #126379, #100997 ) ;
#197261 = CARTESIAN_POINT ( 'NONE',  ( 18.59999999999999076, 21.13195309841794867, -243.6318585593224100 ) ) ;
#197262 = EDGE_CURVE ( 'NONE', #39695, #144636, #222387, .T. ) ;
#197263 = VECTOR ( 'NONE', #136739, 1000.000000000000000 ) ;
#197264 = CARTESIAN_POINT ( 'NONE',  ( -16.77431908686106610, 9.945805754529134290, -79.66416078234981057 ) ) ;
#197265 = ORIENTED_EDGE ( 'NONE', *, *, #67586, .T. ) ;
#197266 = CIRCLE ( 'NONE', #84796, 0.1000000000000028644 ) ;
#197267 = VECTOR ( 'NONE', #20000, 1000.000000000000114 ) ;
#197268 = VECTOR ( 'NONE', #165135, 1000.000000000000114 ) ;
#197269 = CARTESIAN_POINT ( 'NONE',  ( 20.96428641294180650, 64.25000000001195133, -109.8482143065826051 ) ) ;
#197270 = ORIENTED_EDGE ( 'NONE', *, *, #76177, .F. ) ;
#197271 = CARTESIAN_POINT ( 'NONE',  ( -21.45000000000000284, 68.29142135624888965, -57.27310748452437394 ) ) ;
#197272 = ADVANCED_FACE ( 'NONE', ( #199542 ), #20908, .F. ) ;
#197273 = CARTESIAN_POINT ( 'NONE',  ( 20.94999999999999929, 74.16465844978765176, -124.9679561919613207 ) ) ;
#197274 = CARTESIAN_POINT ( 'NONE',  ( 15.73863059295127798, 66.64859682586990175, -52.54357704768591475 ) ) ;
#197275 = FACE_OUTER_BOUND ( 'NONE', #184639, .T. ) ;
#197276 = VECTOR ( 'NONE', #70689, 1000.000000000000114 ) ;
#197277 = AXIS2_PLACEMENT_3D ( 'NONE', #122911, #184145, #39546 ) ;
#197278 = EDGE_CURVE ( 'NONE', #24103, #159940, #18421, .T. ) ;
#197279 = AXIS2_PLACEMENT_3D ( 'NONE', #18991, #239339, #163655 ) ;
#197280 = CIRCLE ( 'NONE', #247343, 0.1000000000000028644 ) ;
#197281 = ORIENTED_EDGE ( 'NONE', *, *, #104142, .F. ) ;
#197282 = DIRECTION ( 'NONE',  ( 0.000000000000000000, 0.000000000000000000, -1.000000000000000000 ) ) ;
#197283 = EDGE_LOOP ( 'NONE', ( #91627, #198227, #219498, #223683 ) ) ;
#197284 = DIRECTION ( 'NONE',  ( -1.000000000000000000, 0.000000000000000000, 0.000000000000000000 ) ) ;
#197285 = DIRECTION ( 'NONE',  ( 0.000000000000000000, 0.2617529984165059553, 0.9651348961777148627 ) ) ;
#197287 = EDGE_LOOP ( 'NONE', ( #11465, #152115, #2739 ) ) ;
#197286 = CARTESIAN_POINT ( 'NONE',  ( 21.04116576186311605, 10.62466307876251292, -146.3285817686277994 ) ) ;
#197288 = CARTESIAN_POINT ( 'NONE',  ( -18.59999999999999787, 66.65000000001253966, -182.3731074845244393 ) ) ;
#197289 = DIRECTION ( 'NONE',  ( 0.000000000000000000, 6.982962677686266711E-15, -1.000000000000000000 ) ) ;
#197290 = CARTESIAN_POINT ( 'NONE',  ( -5.999999999999938716, 64.35000000001120668, -22.12310748452479103 ) ) ;
#197291 = LINE ( 'NONE', #18660, #222887 ) ;
#197292 = DIRECTION ( 'NONE',  ( 7.304098846218134667E-16, 1.000000000000000000, -0.000000000000000000 ) ) ;
#197293 = CARTESIAN_POINT ( 'NONE',  ( -18.49999999999999289, 85.32100840337339775, -129.2871692354463562 ) ) ;
#197295 = VERTEX_POINT ( 'NONE', #164256 ) ;
#197294 = DIRECTION ( 'NONE',  ( 0.000000000000000000, 0.9893560106964510714, -0.1455152366551481502 ) ) ;
#197296 = CARTESIAN_POINT ( 'NONE',  ( -20.94999999999999929, 36.65892442174935439, -249.5511627012433848 ) ) ;
#197297 = ORIENTED_EDGE ( 'NONE', *, *, #241626, .F. ) ;
#197298 = CARTESIAN_POINT ( 'NONE',  ( -18.44204374631833687, 85.49103638961001650, -62.89690621430324313 ) ) ;
#197299 = DIRECTION ( 'NONE',  ( -1.836970198721029934E-16, 1.000000000000000000, 0.000000000000000000 ) ) ;
#197300 = VERTEX_POINT ( 'NONE', #243777 ) ;
#197301 = CARTESIAN_POINT ( 'NONE',  ( -23.15000000000000213, 4.150000000000001243, -21.14999999999999858 ) ) ;
#197302 = ADVANCED_FACE ( 'NONE', ( #140831 ), #161697, .F. ) ;
#197303 =( NAMED_UNIT ( * ) PLANE_ANGLE_UNIT ( ) SI_UNIT ( $, .RADIAN. ) );
#197304 = ORIENTED_EDGE ( 'NONE', *, *, #99752, .T. ) ;
#197305 = AXIS2_PLACEMENT_3D ( 'NONE', #40179, #87910, #244437 ) ;
#197306 = VECTOR ( 'NONE', #66397, 1000.000000000000000 ) ;
#197307 = CARTESIAN_POINT ( 'NONE',  ( -16.93230518875208190, 65.99924963859275806, -190.9473291364229226 ) ) ;
#197308 = ORIENTED_EDGE ( 'NONE', *, *, #190236, .F. ) ;
#197309 = DIRECTION ( 'NONE',  ( 1.000000000000000000, 0.000000000000000000, 0.000000000000000000 ) ) ;
#197310 = ORIENTED_EDGE ( 'NONE', *, *, #77872, .T. ) ;
#197311 = EDGE_CURVE ( 'NONE', #176, #192558, #1296, .T. ) ;
#197312 = CARTESIAN_POINT ( 'NONE',  ( -16.97683809663752186, 9.950000000011138823, -46.90236401819648648 ) ) ;
#197314 = ORIENTED_EDGE ( 'NONE', *, *, #188771, .F. ) ;
#197313 = DIRECTION ( 'NONE',  ( 0.000000000000000000, 0.000000000000000000, 1.000000000000000000 ) ) ;
#197316 = EDGE_CURVE ( 'NONE', #218130, #161032, #255702, .T. ) ;
#197315 = FACE_OUTER_BOUND ( 'NONE', #93927, .T. ) ;
#197317 = ORIENTED_EDGE ( 'NONE', *, *, #146802, .T. ) ;
#197318 = CARTESIAN_POINT ( 'NONE',  ( -23.15000000000000213, 2.000000000011154189, -46.72462192276210402 ) ) ;
#197319 = VERTEX_POINT ( 'NONE', #239940 ) ;
#197321 = ORIENTED_EDGE ( 'NONE', *, *, #112028, .F. ) ;
#197320 = ORIENTED_EDGE ( 'NONE', *, *, #14867, .T. ) ;
#197322 = CARTESIAN_POINT ( 'NONE',  ( 20.94999999999999929, 71.00000000001180922, -81.92837350343744163 ) ) ;
#197323 = ORIENTED_EDGE ( 'NONE', *, *, #85939, .T. ) ;
#197324 = CARTESIAN_POINT ( 'NONE',  ( 21.05000000000000071, 76.00000000001168132, -73.82310748452435689 ) ) ;
#197326 = ADVANCED_FACE ( 'NONE', ( #79546 ), #159135, .T. ) ;
#197325 = ORIENTED_EDGE ( 'NONE', *, *, #58183, .T. ) ;
#197327 = AXIS2_PLACEMENT_3D ( 'NONE', #76581, #257732, #19182 ) ;
#197328 = CIRCLE ( 'NONE', #118233, 0.1000000000000028644 ) ;
#197329 = AXIS2_PLACEMENT_3D ( 'NONE', #201838, #59732, #102708 ) ;
#197330 = EDGE_CURVE ( 'NONE', #104319, #155390, #89149, .T. ) ;
#197331 = ADVANCED_FACE ( 'NONE', ( #10319 ), #226497, .T. ) ;
#197332 = ORIENTED_EDGE ( 'NONE', *, *, #143636, .F. ) ;
#197333 = B_SPLINE_CURVE_WITH_KNOTS ( 'NONE', 3,
 ( #103635, #181919, #147933, #85347, #223585, #183208, #146616, #28008, #25424, #144051 ),
 .UNSPECIFIED., .F., .F.,
 ( 4, 2, 2, 2, 4 ),
 ( 0.000000000000000000, 0.0003916577441626488279, 0.0005874866162439766571, 0.0006854010522846775430, 0.0007833154883253782121 ),
 .UNSPECIFIED. ) ;
#197334 = DIRECTION ( 'NONE',  ( 0.000000000000000000, 0.2128009952263603677, -0.9770955615653313941 ) ) ;
#197335 = CARTESIAN_POINT ( 'NONE',  ( -18.59999999999999787, 77.63717271298195044, -57.94095411905229298 ) ) ;
#197337 = ORIENTED_EDGE ( 'NONE', *, *, #194295, .F. ) ;
#197336 = DIRECTION ( 'NONE',  ( 0.000000000000000000, -0.2128009952263603677, 0.9770955615653313941 ) ) ;
#197338 = FACE_OUTER_BOUND ( 'NONE', #118849, .T. ) ;
#197339 = ORIENTED_EDGE ( 'NONE', *, *, #196323, .T. ) ;
#197340 = EDGE_CURVE ( 'NONE', #133593, #64097, #91119, .T. ) ;
#197341 = CARTESIAN_POINT ( 'NONE',  ( 21.14999999999999503, 64.25313205997782973, -247.2214437328673853 ) ) ;
#197342 = DIRECTION ( 'NONE',  ( 0.000000000000000000, -6.982962677686266711E-15, 1.000000000000000000 ) ) ;
#197343 = DIRECTION ( 'NONE',  ( -1.000000000000000000, -0.000000000000000000, -0.000000000000000000 ) ) ;
#197344 = CIRCLE ( 'NONE', #126622, 12.77499999999999503 ) ;
#197345 = ORIENTED_EDGE ( 'NONE', *, *, #6525, .T. ) ;
#197346 = AXIS2_PLACEMENT_3D ( 'NONE', #37683, #97595, #232354 ) ;
#197347 = CARTESIAN_POINT ( 'NONE',  ( -20.64999999999999858, 4.768403829798271154, -213.4961173936592331 ) ) ;
#197348 = CARTESIAN_POINT ( 'NONE',  ( -18.37151313414626586, 38.14841574062842966, -261.2067459223885635 ) ) ;
#197349 = CARTESIAN_POINT ( 'NONE',  ( -18.59999999999999787, 21.17283678855158513, -243.7231193059830332 ) ) ;
#197350 = CIRCLE ( 'NONE', #89011, 7.800000000000001599 ) ;
#197351 = EDGE_CURVE ( 'NONE', #127795, #198825, #211071, .T. ) ;
#197352 = ORIENTED_EDGE ( 'NONE', *, *, #37865, .T. ) ;
#197353 = B_SPLINE_CURVE_WITH_KNOTS ( 'NONE', 3,
 ( #189769, #91947, #149386, #128516, #132360, #11137, #33304, #112804, #192340, #168969, #167662, #172820, #12439, #171523, #211917, #231479, #108937, #51508, #251001, #252290, #69845, #89366, #93226, #34566, #228901, #191079 ),
 .UNSPECIFIED., .F., .F.,
 ( 4, 2, 2, 2, 2, 2, 2, 2, 2, 2, 2, 2, 4 ),
 ( 0.005476422646581353450, 0.006160811967703566129, 0.006845201288825777074, 0.007187395949386882546, 0.007529590609947988886, 0.007871785270509093491, 0.008213979931070199830, 0.008556174591631306170, 0.008898369252192410775, 0.009240563912753517115, 0.009582758573314621720, 0.01026714789443683440, 0.01095153721555904534 ),
 .UNSPECIFIED. ) ;
#197354 = CARTESIAN_POINT ( 'NONE',  ( -16.92132318717937522, 66.03392997600593617, -90.40070085417231383 ) ) ;
#197355 = ORIENTED_EDGE ( 'NONE', *, *, #190788, .T. ) ;
#197356 = AXIS2_PLACEMENT_3D ( 'NONE', #34413, #253418, #74830 ) ;
#197357 = EDGE_LOOP ( 'NONE', ( #226130, #129831, #213384, #254226 ) ) ;
#197358 = CARTESIAN_POINT ( 'NONE',  ( -18.59999999999999787, 74.16465844978819177, -191.9679561919613775 ) ) ;
#197360 = ORIENTED_EDGE ( 'NONE', *, *, #112274, .F. ) ;
#197359 = AXIS2_PLACEMENT_3D ( 'NONE', #220435, #181316, #142164 ) ;
#197361 = ORIENTED_EDGE ( 'NONE', *, *, #232295, .F. ) ;
#197362 = DIRECTION ( 'NONE',  ( -0.000000000000000000, 0.4791956752371485107, 0.8777080977375185666 ) ) ;
#197363 = CARTESIAN_POINT ( 'NONE',  ( -16.93589915522259304, 10.00862525870701347, -188.4405601019602727 ) ) ;
#197364 = EDGE_LOOP ( 'NONE', ( #134300, #30607, #95725, #107457 ) ) ;
#197365 = EDGE_CURVE ( 'NONE', #80895, #18621, #72429, .T. ) ;
#197366 = ORIENTED_EDGE ( 'NONE', *, *, #89503, .T. ) ;
#197367 = CARTESIAN_POINT ( 'NONE',  ( -21.05000000000000071, 0.2561057921033771945, -100.4651035583277405 ) ) ;
#197368 = AXIS2_PLACEMENT_3D ( 'NONE', #86000, #69061, #106868 ) ;
#197369 = AXIS2_PLACEMENT_3D ( 'NONE', #70624, #229670, #92707 ) ;
#197370 = DIRECTION ( 'NONE',  ( 0.000000000000000000, -7.056502275159890832E-15, 1.000000000000000000 ) ) ;
#197371 = EDGE_CURVE ( 'NONE', #63249, #68443, #22536, .T. ) ;
#197372 = AXIS2_PLACEMENT_3D ( 'NONE', #20525, #37515, #118334 ) ;
#197373 = ORIENTED_EDGE ( 'NONE', *, *, #128136, .F. ) ;
#197374 = ORIENTED_EDGE ( 'NONE', *, *, #14243, .F. ) ;
#197375 = ORIENTED_EDGE ( 'NONE', *, *, #226547, .T. ) ;
#197376 = ADVANCED_FACE ( 'NONE', ( #131528 ), #109382, .T. ) ;
#197377 = DIRECTION ( 'NONE',  ( -0.000000000000000000, 1.000000000000000000, 0.000000000000000000 ) ) ;
#197378 = CARTESIAN_POINT ( 'NONE',  ( -23.15000000000000213, 87.48912529308822172, -139.5231074845243029 ) ) ;
#197379 = DIRECTION ( 'NONE',  ( 1.000000000000000000, 0.000000000000000000, 0.000000000000000000 ) ) ;
#197380 = DIRECTION ( 'NONE',  ( -1.000000000000000000, 0.000000000000000000, 0.000000000000000000 ) ) ;
#197381 = CARTESIAN_POINT ( 'NONE',  ( 20.94999999999999574, -11.64999999998883595, -36.39999999999999858 ) ) ;
#197382 = DIRECTION ( 'NONE',  ( -1.000000000000000000, 0.000000000000000000, 0.000000000000000000 ) ) ;
#197383 = AXIS2_PLACEMENT_3D ( 'NONE', #35338, #217759, #58685 ) ;
#197385 = DIRECTION ( 'NONE',  ( 0.000000000000000000, 0.9651348961777157509, -0.2617529984165031243 ) ) ;
#197384 = FACE_OUTER_BOUND ( 'NONE', #197447, .T. ) ;
#197386 = DIRECTION ( 'NONE',  ( -1.000000000000000000, -0.000000000000000000, 0.000000000000000000 ) ) ;
#197387 = DIRECTION ( 'NONE',  ( 0.000000000000000000, -1.000000000000000000, -6.982962677686266711E-15 ) ) ;
#197388 = CIRCLE ( 'NONE', #147518, 0.4999999999999902855 ) ;
#197389 = CARTESIAN_POINT ( 'NONE',  ( -18.59999999999999787, 45.53758419368699606, -241.2860287061636768 ) ) ;
#197391 = DIRECTION ( 'NONE',  ( 0.7071067811865456854, -0.3338907855510742650, -0.6233112732207634066 ) ) ;
#197390 = AXIS2_PLACEMENT_3D ( 'NONE', #82087, #100366, #5109 ) ;
#197392 = ORIENTED_EDGE ( 'NONE', *, *, #101632, .T. ) ;
#197393 = EDGE_CURVE ( 'NONE', #77718, #92509, #30928, .T. ) ;
#197394 = AXIS2_PLACEMENT_3D ( 'NONE', #40512, #236097, #178734 ) ;
#197395 = AXIS2_PLACEMENT_3D ( 'NONE', #124957, #123673, #166676 ) ;
#197397 = ORIENTED_EDGE ( 'NONE', *, *, #145650, .T. ) ;
#197396 = FACE_OUTER_BOUND ( 'NONE', #175921, .T. ) ;
#197398 = EDGE_CURVE ( 'NONE', #121258, #98885, #151548, .T. ) ;
#197399 = DIRECTION ( 'NONE',  ( 1.000000000000000000, -3.265361837132813093E-16, -2.280189983783949500E-30 ) ) ;
#197400 = AXIS2_PLACEMENT_3D ( 'NONE', #227665, #208137, #46454 ) ;
#197401 = CARTESIAN_POINT ( 'NONE',  ( -22.50000000000000000, 64.08545097430041437, -247.0723585184913986 ) ) ;
#197402 = EDGE_LOOP ( 'NONE', ( #187985, #4524, #20642, #243652, #143446 ) ) ;
#197403 = AXIS2_PLACEMENT_3D ( 'NONE', #100349, #127496, #90925 ) ;
#197404 = EDGE_CURVE ( 'NONE', #59486, #154024, #914, .T. ) ;
#197405 = EDGE_CURVE ( 'NONE', #75834, #145735, #130850, .T. ) ;
#197406 = VECTOR ( 'NONE', #11426, 1000.000000000000000 ) ;
#197407 = PRODUCT_DEFINITION_SHAPE ( 'NONE', 'NONE',  #258120 ) ;
#197408 = CARTESIAN_POINT ( 'NONE',  ( -16.89081410710458542, 9.951318529847110739, -20.85440591983636693 ) ) ;
#197409 = EDGE_CURVE ( 'NONE', #205612, #3192, #114089, .T. ) ;
#197410 = ORIENTED_EDGE ( 'NONE', *, *, #142824, .F. ) ;
#197411 = AXIS2_PLACEMENT_3D ( 'NONE', #216244, #37646, #117168 ) ;
#197412 = CARTESIAN_POINT ( 'NONE',  ( -20.97625342178436725, 11.60000000083177696, -140.9282032298017953 ) ) ;
#197413 = FACE_OUTER_BOUND ( 'NONE', #118006, .T. ) ;
#197414 = FACE_OUTER_BOUND ( 'NONE', #235496, .T. ) ;
#197415 = EDGE_CURVE ( 'NONE', #81210, #52494, #205664, .T. ) ;
#197416 = CARTESIAN_POINT ( 'NONE',  ( -21.07946286933444568, 10.04976323809818162, -228.1174753750304660 ) ) ;
#197418 = VERTEX_POINT ( 'NONE', #127691 ) ;
#197417 = DIRECTION ( 'NONE',  ( -0.000000000000000000, -6.982962677686266711E-15, 1.000000000000000000 ) ) ;
#197419 = AXIS2_PLACEMENT_3D ( 'NONE', #171559, #210653, #45486 ) ;
#197421 = VERTEX_POINT ( 'NONE', #209791 ) ;
#197420 = CARTESIAN_POINT ( 'NONE',  ( -18.59999999999999787, 1.115600667400684642E-11, -100.5000000000000284 ) ) ;
#197422 = CARTESIAN_POINT ( 'NONE',  ( 21.13507111622890022, 10.71768338699838807, -12.24916858636078842 ) ) ;
#197423 = PLANE ( 'NONE',  #227661 ) ;
#197424 = FACE_OUTER_BOUND ( 'NONE', #55619, .T. ) ;
#197425 = CIRCLE ( 'NONE', #39253, 0.1000000000000046685 ) ;
#197427 = DIRECTION ( 'NONE',  ( -1.000000000000000000, 0.000000000000000000, 0.000000000000000000 ) ) ;
#197426 = CARTESIAN_POINT ( 'NONE',  ( -16.84793658983431897, 9.950000000011140600, -154.7663533221900423 ) ) ;
#197428 = LINE ( 'NONE', #179191, #157941 ) ;
#197429 = CARTESIAN_POINT ( 'NONE',  ( -20.94999999999999929, 11.60000000001115161, -40.42820323027555673 ) ) ;
#197430 = PLANE ( 'NONE',  #166258 ) ;
#197431 = CARTESIAN_POINT ( 'NONE',  ( -20.00857864376270001, 22.33586458086958615, -231.4986017528744071 ) ) ;
#197432 = CIRCLE ( 'NONE', #84989, 0.1000000000000028644 ) ;
#197434 = ORIENTED_EDGE ( 'NONE', *, *, #143237, .T. ) ;
#197433 = AXIS2_PLACEMENT_3D ( 'NONE', #207625, #185477, #10695 ) ;
#197435 = EDGE_CURVE ( 'NONE', #7468, #201052, #89819, .T. ) ;
#197436 = DIRECTION ( 'NONE',  ( 0.000000000000000000, 0.2128009952263603122, -0.9770955615653315052 ) ) ;
#197437 = AXIS2_PLACEMENT_3D ( 'NONE', #1872, #46158, #184377 ) ;
#197438 = ORIENTED_EDGE ( 'NONE', *, *, #19922, .F. ) ;
#197439 = ORIENTED_EDGE ( 'NONE', *, *, #102791, .F. ) ;
#197440 = DIRECTION ( 'NONE',  ( 0.000000000000000000, 3.543264972207943384E-15, -1.000000000000000000 ) ) ;
#197441 = DIRECTION ( 'NONE',  ( 1.000000000000000000, -0.000000000000000000, -0.000000000000000000 ) ) ;
#197442 = ADVANCED_FACE ( 'NONE', ( #11602 ), #170712, .T. ) ;
#197443 = VERTEX_POINT ( 'NONE', #9016 ) ;
#197444 = APPLICATION_CONTEXT ( 'automotive_design' ) ;
#197445 = ADVANCED_FACE ( 'NONE', ( #168139 ), #247362, .T. ) ;
#197446 = B_SPLINE_CURVE_WITH_KNOTS ( 'NONE', 3,
 ( #235333, #134927, #194957, #231512, #234054, #151990, #213199, #55383, #94537, #254846 ),
 .UNSPECIFIED., .F., .F.,
 ( 4, 2, 2, 2, 4 ),
 ( 0.000000000000000000, 4.221631689683615497E-05, 8.443263379367230994E-05, 0.0001688652675874169633, 0.0003377305351749844138 ),
 .UNSPECIFIED. ) ;
#197447 = EDGE_LOOP ( 'NONE', ( #62445, #76037, #158756, #163923 ) ) ;
#197448 = SHAPE_REPRESENTATION_RELATIONSHIP ( 'NONE' , 'NONE' ,  #10216, #26318 ) ;
#197449 = EDGE_CURVE ( 'NONE', #223936, #100463, #106817, .T. ) ;
#197450 = CIRCLE ( 'NONE', #130250, 0.09999999999999939493 ) ;
#197451 = ORIENTED_EDGE ( 'NONE', *, *, #50581, .T. ) ;
#197452 = CIRCLE ( 'NONE', #239158, 0.1000000000000024342 ) ;
#197453 = ORIENTED_EDGE ( 'NONE', *, *, #22397, .F. ) ;
#197454 = CARTESIAN_POINT ( 'NONE',  ( -21.05000000000000071, -11.39257802169451139, -63.92605042016806749 ) ) ;
#197455 = CARTESIAN_POINT ( 'NONE',  ( 20.94999999999999929, 10.47338541492405817, -41.07865446424855094 ) ) ;
#197456 = DIRECTION ( 'NONE',  ( 0.000000000000000000, 6.982962677686266711E-15, -1.000000000000000000 ) ) ;
#197457 = DIRECTION ( 'NONE',  ( -1.000000000000000000, 0.000000000000000000, 0.000000000000000000 ) ) ;
#197458 = CARTESIAN_POINT ( 'NONE',  ( 15.75000000000000711, 9.349999999999985434, -16.51856895740264619 ) ) ;
#197459 = CYLINDRICAL_SURFACE ( 'NONE', #150046, 1.749999999999998002 ) ;
#197460 = DIRECTION ( 'NONE',  ( -0.000000000000000000, -1.000000000000000000, -6.982962677686266711E-15 ) ) ;
#197462 = ORIENTED_EDGE ( 'NONE', *, *, #163659, .F. ) ;
#197461 = CARTESIAN_POINT ( 'NONE',  ( 20.27550659511088682, 19.63441466210375808, -229.9765866052221099 ) ) ;
#197464 = CARTESIAN_POINT ( 'NONE',  ( -22.42357213249529480, 65.12722920756738176, -243.2346049986351204 ) ) ;
#197463 = CARTESIAN_POINT ( 'NONE',  ( -22.50000000000000000, 0.000000000000000000, 11.64957080754479968 ) ) ;
#197465 = DIRECTION ( 'NONE',  ( 1.000000000000000000, 0.000000000000000000, 0.000000000000000000 ) ) ;
#197466 = VERTEX_POINT ( 'NONE', #186386 ) ;
#197467 = CARTESIAN_POINT ( 'NONE',  ( 21.05000000000005400, 65.35000000001120668, -4.623107484524796362 ) ) ;
#197468 = DIRECTION ( 'NONE',  ( -2.602085213965226419E-14, 6.982962677686266711E-15, -1.000000000000000000 ) ) ;
#197469 = ORIENTED_EDGE ( 'NONE', *, *, #247949, .F. ) ;
#197470 = EDGE_CURVE ( 'NONE', #221237, #202146, #7743, .T. ) ;
#197472 = CARTESIAN_POINT ( 'NONE',  ( -20.94999999999999929, -11.48912529306489994, -131.0000000000000284 ) ) ;
#197471 = LINE ( 'NONE', #34580, #66251 ) ;
#197473 = CARTESIAN_POINT ( 'NONE',  ( -21.30740335185486245, 75.90106547423613392, -109.5797654065523119 ) ) ;
#197474 = DIRECTION ( 'NONE',  ( 0.000000000000000000, -0.9651348961777379554, 0.2617529984164210233 ) ) ;
#197475 = EDGE_LOOP ( 'NONE', ( #117017, #93019, #48773, #169275 ) ) ;
#197476 = STYLED_ITEM ( 'NONE', ( #37900 ), #197191 ) ;
#197477 = LINE ( 'NONE', #177940, #128498 ) ;
#197478 = LINE ( 'NONE', #99641, #78277 ) ;
#197479 = CARTESIAN_POINT ( 'NONE',  ( -20.94999999999999929, 87.75000000001143974, -39.12310748452424747 ) ) ;
#197480 = CARTESIAN_POINT ( 'NONE',  ( -21.14999999999999858, 64.25000000001161027, -62.73924182154625129 ) ) ;
#197481 = VERTEX_POINT ( 'NONE', #113250 ) ;
#197482 = DIRECTION ( 'NONE',  ( 0.000000000000000000, 0.8034013718071717491, -0.5954378521544919645 ) ) ;
#197483 = EDGE_CURVE ( 'NONE', #32589, #32249, #74162, .T. ) ;
#197484 = CARTESIAN_POINT ( 'NONE',  ( 22.39999999999999858, 1.115600667400684642E-11, -33.50000000000000000 ) ) ;
#197485 = DIRECTION ( 'NONE',  ( 1.000000000000000000, 0.000000000000000000, 0.000000000000000000 ) ) ;
#197486 = EDGE_CURVE ( 'NONE', #88490, #222045, #196626, .T. ) ;
#197487 = TOROIDAL_SURFACE ( 'NONE', #222408, 2.100000000000002309, 0.1000000000000000056 ) ;
#197488 = CARTESIAN_POINT ( 'NONE',  ( 22.39999999999999503, 64.25000000001193712, -103.1231074845243825 ) ) ;
#197489 = VECTOR ( 'NONE', #111626, 1000.000000000000000 ) ;
#197490 = CARTESIAN_POINT ( 'NONE',  ( -21.55000000000000071, 68.65000000001157332, -57.17310748452437252 ) ) ;
#197491 = AXIS2_PLACEMENT_3D ( 'NONE', #30067, #50855, #11789 ) ;
#197492 = AXIS2_PLACEMENT_3D ( 'NONE', #18139, #97649, #177247 ) ;
#197493 = EDGE_CURVE ( 'NONE', #159212, #155020, #22729, .T. ) ;
#197495 = ORIENTED_EDGE ( 'NONE', *, *, #56548, .T. ) ;
#197494 = DIRECTION ( 'NONE',  ( 1.000000000000000000, 0.000000000000000000, 0.000000000000000000 ) ) ;
#197496 = DIRECTION ( 'NONE',  ( -1.000000000000000000, 0.000000000000000000, 0.000000000000000000 ) ) ;
#197497 = EDGE_CURVE ( 'NONE', #49158, #106325, #174567, .T. ) ;
#197498 = CARTESIAN_POINT ( 'NONE',  ( -16.87683809663752754, 66.13411015068085419, -89.75568067745427925 ) ) ;
#197499 = DIRECTION ( 'NONE',  ( 1.000000000000000000, 0.000000000000000000, -0.000000000000000000 ) ) ;
#197500 = DIRECTION ( 'NONE',  ( 1.000000000000000000, -0.000000000000000000, -0.000000000000000000 ) ) ;
#197501 = CARTESIAN_POINT ( 'NONE',  ( 18.52928932188133970, 10.27928932188134858, -24.65000000000000213 ) ) ;
#197503 = VERTEX_POINT ( 'NONE', #134082 ) ;
#197502 = CARTESIAN_POINT ( 'NONE',  ( 21.14999999999999858, 67.21339244341145047, -57.27310748452438105 ) ) ;
#197504 = CARTESIAN_POINT ( 'NONE',  ( -21.05000000000000071, 56.01362831242967388, -232.7091905853083347 ) ) ;
#197505 = DIRECTION ( 'NONE',  ( 0.000000000000000000, -0.8660254037844377084, -0.5000000000000016653 ) ) ;
#197506 = ORIENTED_EDGE ( 'NONE', *, *, #80925, .T. ) ;
#197507 = CARTESIAN_POINT ( 'NONE',  ( -18.59999999999999787, 74.83729825007388570, -95.02310748452431710 ) ) ;
#197508 = CARTESIAN_POINT ( 'NONE',  ( 21.05000000000000071, 76.10000000001241460, -176.5637644362255969 ) ) ;
#197509 = DIRECTION ( 'NONE',  ( 0.7071067811865474617, -0.7071067811865474617, -4.937700262164531476E-15 ) ) ;
#197510 = CARTESIAN_POINT ( 'NONE',  ( -23.15000000000000213, -11.74999999998884448, -21.75000000000000355 ) ) ;
#197511 = VECTOR ( 'NONE', #1314, 1000.000000000000000 ) ;
#197512 = CARTESIAN_POINT ( 'NONE',  ( -18.41799967126741677, 78.24072142544075348, -231.5548840223034972 ) ) ;
#197513 = TOROIDAL_SURFACE ( 'NONE', #51748, 7.791421356237335338, 0.1000000000000000056 ) ;
#197514 = FACE_OUTER_BOUND ( 'NONE', #18949, .T. ) ;
#197515 = EDGE_CURVE ( 'NONE', #65513, #115551, #58376, .T. ) ;
#197516 = EDGE_CURVE ( 'NONE', #72090, #194645, #47614, .T. ) ;
#197517 = ORIENTED_EDGE ( 'NONE', *, *, #76449, .F. ) ;
#197518 = ORIENTED_EDGE ( 'NONE', *, *, #82606, .T. ) ;
#197519 = AXIS2_PLACEMENT_3D ( 'NONE', #47884, #28378, #106566 ) ;
#197520 = CARTESIAN_POINT ( 'NONE',  ( -21.05000000000000071, 68.48451787451661232, -224.2224406095231757 ) ) ;
#197522 = DIRECTION ( 'NONE',  ( 0.000000000000000000, -0.9126074666063771490, -0.4088369013363278293 ) ) ;
#197521 = VECTOR ( 'NONE', #108389, 1000.000000000000114 ) ;
#197523 = DIRECTION ( 'NONE',  ( -0.000000000000000000, -0.1686199900910294591, 0.9856811345164832039 ) ) ;
#197524 = DIRECTION ( 'NONE',  ( 4.336808689942128177E-15, 0.9525900758537759749, -0.3042567129660372904 ) ) ;
#197525 = ORIENTED_EDGE ( 'NONE', *, *, #152050, .F. ) ;
#197526 = CARTESIAN_POINT ( 'NONE',  ( 20.95545211741311320, 10.58641331155510379, -175.0861468595882684 ) ) ;
#197527 = VECTOR ( 'NONE', #181738, 1000.000000000000000 ) ;
#197528 = AXIS2_PLACEMENT_3D ( 'NONE', #65765, #67058, #64490 ) ;
#197529 = CARTESIAN_POINT ( 'NONE',  ( 20.13684514580420526, 11.01120340441282153, -206.9357926396625089 ) ) ;
#197530 = EDGE_CURVE ( 'NONE', #231071, #85621, #72609, .T. ) ;
#197531 = VECTOR ( 'NONE', #115473, 1000.000000000000000 ) ;
#197532 = CARTESIAN_POINT ( 'NONE',  ( -16.77732147278574715, 9.945966932573432118, -12.66350875687580846 ) ) ;
#197533 = EDGE_CURVE ( 'NONE', #227067, #223699, #5919, .T. ) ;
#197534 = CYLINDRICAL_SURFACE ( 'NONE', #157108, 0.09999999999999939493 ) ;
#197535 = ORIENTED_EDGE ( 'NONE', *, *, #246377, .T. ) ;
#197536 = DIRECTION ( 'NONE',  ( 0.000000000000000000, 2.891205793294679805E-16, -1.000000000000000000 ) ) ;
#197537 = VERTEX_POINT ( 'NONE', #136647 ) ;
#197538 = CARTESIAN_POINT ( 'NONE',  ( -16.83199318825828783, 9.930646127981159310, -20.72758518820919704 ) ) ;
#197539 = ORIENTED_EDGE ( 'NONE', *, *, #257998, .T. ) ;
#197540 = DIRECTION ( 'NONE',  ( 0.000000000000000000, 0.000000000000000000, -1.000000000000000000 ) ) ;
#197541 = CARTESIAN_POINT ( 'NONE',  ( -16.94445028196808778, 66.00793639031412852, -90.41577730610593733 ) ) ;
#197542 = CARTESIAN_POINT ( 'NONE',  ( -20.94999999999999929, 87.29603075034721371, -99.97520832486037534 ) ) ;
#197543 = VERTEX_POINT ( 'NONE', #255269 ) ;
#197544 = ADVANCED_FACE ( 'NONE', ( #132828 ), #190282, .T. ) ;
#197546 = VECTOR ( 'NONE', #235485, 1000.000000000000000 ) ;
#197545 = LINE ( 'NONE', #198834, #215621 ) ;
#197547 = CARTESIAN_POINT ( 'NONE',  ( -18.59999999999999787, 57.82359945636609666, -226.0354702357591350 ) ) ;
#197548 = DIRECTION ( 'NONE',  ( 0.000000000000000000, 0.000000000000000000, 1.000000000000000000 ) ) ;
#197549 = AXIS2_PLACEMENT_3D ( 'NONE', #151111, #89827, #48143 ) ;
#197550 = ORIENTED_EDGE ( 'NONE', *, *, #25043, .F. ) ;
#197552 = CARTESIAN_POINT ( 'NONE',  ( 20.12500000000000000, 9.750000000011153745, -121.6500000000000341 ) ) ;
#197551 = VECTOR ( 'NONE', #206543, 1000.000000000000000 ) ;
#197554 = ORIENTED_EDGE ( 'NONE', *, *, #252999, .T. ) ;
#197553 = LINE ( 'NONE', #118020, #29987 ) ;
#197555 = DIRECTION ( 'NONE',  ( 0.000000000000000000, 3.341447938192219320E-14, 1.000000000000000000 ) ) ;
#197556 = CARTESIAN_POINT ( 'NONE',  ( -18.49719636458545935, 85.44636535924018972, -162.9514936146412651 ) ) ;
#197557 = EDGE_CURVE ( 'NONE', #160578, #52356, #51898, .T. ) ;
#197558 = ORIENTED_EDGE ( 'NONE', *, *, #177641, .T. ) ;
#197559 = DIRECTION ( 'NONE',  ( 0.000000000000000000, 0.000000000000000000, -1.000000000000000000 ) ) ;
#197560 = DIRECTION ( 'NONE',  ( -0.000000000000000000, 0.01283462868039629209, -0.9999176327611372095 ) ) ;
#197561 = DIRECTION ( 'NONE',  ( 1.000000000000000000, -0.000000000000000000, -0.000000000000000000 ) ) ;
#197562 = ORIENTED_EDGE ( 'NONE', *, *, #142319, .F. ) ;
#197563 = DIRECTION ( 'NONE',  ( -1.000000000000000000, 0.000000000000000000, 0.000000000000000000 ) ) ;
#197564 = ADVANCED_FACE ( 'NONE', ( #213630 ), #94961, .F. ) ;
#197565 = CARTESIAN_POINT ( 'NONE',  ( 14.88075390448864432, 49.48471825922439393, -233.4704840993163941 ) ) ;
#197566 = DIRECTION ( 'NONE',  ( -4.391705002472929091E-16, 1.000000000000000000, 0.000000000000000000 ) ) ;
#197567 = AXIS2_PLACEMENT_3D ( 'NONE', #130537, #232237, #193099 ) ;
#197568 = ORIENTED_EDGE ( 'NONE', *, *, #125439, .T. ) ;
#197569 = CIRCLE ( 'NONE', #110087, 0.09999999999998898659 ) ;
#197571 = ORIENTED_EDGE ( 'NONE', *, *, #20263, .F. ) ;
#197570 = CIRCLE ( 'NONE', #39213, 4.100000000000000533 ) ;
#197572 = AXIS2_PLACEMENT_3D ( 'NONE', #3255, #118089, #142762 ) ;
#197573 = CIRCLE ( 'NONE', #151825, 0.09999999999999990841 ) ;
#197574 = VERTEX_POINT ( 'NONE', #46215 ) ;
#197575 = DIRECTION ( 'NONE',  ( 0.000000000000000000, 0.000000000000000000, 1.000000000000000000 ) ) ;
#197576 = CARTESIAN_POINT ( 'NONE',  ( 21.13461538461538325, 8.885417037985614996, -45.74999999999999289 ) ) ;
#197578 = VERTEX_POINT ( 'NONE', #65787 ) ;
#197577 = CYLINDRICAL_SURFACE ( 'NONE', #37769, 0.09999999999998898659 ) ;
#197579 = DIRECTION ( 'NONE',  ( -1.000000000000000000, -0.000000000000000000, 1.073024830501117725E-15 ) ) ;
#197581 = AXIS2_PLACEMENT_3D ( 'NONE', #123144, #64452, #24057 ) ;
#197580 = DIRECTION ( 'NONE',  ( 0.000000000000000000, -0.8660254037844247188, 0.5000000000000245359 ) ) ;
#197582 = PLANE ( 'NONE',  #104561 ) ;
#197583 = DIRECTION ( 'NONE',  ( 1.000000000000000000, 1.541880601228652843E-16, 2.878400969107353907E-16 ) ) ;
#197584 = DIRECTION ( 'NONE',  ( 1.000000000000000000, 0.000000000000000000, 0.000000000000000000 ) ) ;
#197585 = AXIS2_PLACEMENT_3D ( 'NONE', #170215, #235257, #154486 ) ;
#197586 = DIRECTION ( 'NONE',  ( 0.000000000000000000, -6.982962677686266711E-15, 1.000000000000000000 ) ) ;
#197587 = CIRCLE ( 'NONE', #139315, 0.5000000000000004441 ) ;
#197589 = VERTEX_POINT ( 'NONE', #245714 ) ;
#197588 = FACE_OUTER_BOUND ( 'NONE', #116811, .T. ) ;
#197591 = ORIENTED_EDGE ( 'NONE', *, *, #215535, .F. ) ;
#197590 = DIRECTION ( 'NONE',  ( 1.000000000000000000, 0.000000000000000000, 0.000000000000000000 ) ) ;
#197593 = CARTESIAN_POINT ( 'NONE',  ( -16.80621392010915827, 51.58591888298440864, -231.9697716580949702 ) ) ;
#197592 = CARTESIAN_POINT ( 'NONE',  ( -23.25000000000000000, 71.85000000001224407, -148.8731074845244109 ) ) ;
#197594 = AXIS2_PLACEMENT_3D ( 'NONE', #175340, #253549, #213147 ) ;
#197595 = VERTEX_POINT ( 'NONE', #106176 ) ;
#197596 = VERTEX_POINT ( 'NONE', #59663 ) ;
#197597 = CARTESIAN_POINT ( 'NONE',  ( -18.50016250449483479, 10.29766095125287073, -105.9743663933276139 ) ) ;
#197598 = PLANE ( 'NONE',  #63889 ) ;
#197599 = LINE ( 'NONE', #77636, #246764 ) ;
#197600 = DIRECTION ( 'NONE',  ( 0.000000000000000000, -0.9770955615653315052, -0.2128009952263603954 ) ) ;
#197601 = DIRECTION ( 'NONE',  ( 0.000000000000000000, 0.000000000000000000, -1.000000000000000000 ) ) ;
#197602 = DIRECTION ( 'NONE',  ( 0.7071067811865463515, 0.7071067811865487940, 4.937700262164540154E-15 ) ) ;
#197603 = CARTESIAN_POINT ( 'NONE',  ( 23.40000000000005542, 83.90000000001120384, -34.86056257560453986 ) ) ;
#197604 = AXIS2_PLACEMENT_3D ( 'NONE', #189699, #128442, #249678 ) ;
#197605 = ORIENTED_EDGE ( 'NONE', *, *, #199231, .T. ) ;
#197606 = EDGE_LOOP ( 'NONE', ( #36371, #175465 ) ) ;
#197607 = EDGE_CURVE ( 'NONE', #63849, #20437, #60100, .T. ) ;
#197608 = DIRECTION ( 'NONE',  ( 0.000000000000000000, 0.000000000000000000, 1.000000000000000000 ) ) ;
#197609 = MANIFOLD_SOLID_BREP ( 'Stock-MAS-200-1', #99032 ) ;
#197610 = ORIENTED_EDGE ( 'NONE', *, *, #52569, .T. ) ;
#197611 = DIRECTION ( 'NONE',  ( 0.000000000000000000, -0.3343365196859449662, 0.9424537609900497381 ) ) ;
#197613 = AXIS2_PLACEMENT_3D ( 'NONE', #23285, #41561, #200611 ) ;
#197612 = CARTESIAN_POINT ( 'NONE',  ( 18.51697539158856642, 68.06642993404716435, -224.1774859612004036 ) ) ;
#197614 = VECTOR ( 'NONE', #150882, 1000.000000000000000 ) ;
#197615 = CARTESIAN_POINT ( 'NONE',  ( -14.87779219673429054, 66.56936653093875123, -54.29134168970030316 ) ) ;
#197616 = CIRCLE ( 'NONE', #118548, 4.299999999999952749 ) ;
#197617 = DIRECTION ( 'NONE',  ( 0.000000000000000000, 0.000000000000000000, 1.000000000000000000 ) ) ;
#197618 = ORIENTED_EDGE ( 'NONE', *, *, #167733, .T. ) ;
#197619 = ADVANCED_FACE ( 'NONE', ( #961 ), #160102, .T. ) ;
#197620 = CARTESIAN_POINT ( 'NONE',  ( -14.56336952470180357, 66.55335465531678096, -118.1123010284241985 ) ) ;
#197621 = ORIENTED_EDGE ( 'NONE', *, *, #80902, .T. ) ;
#197622 = CARTESIAN_POINT ( 'NONE',  ( -18.44085059012131822, 11.51401249349495970, -91.24030531912158892 ) ) ;
#197623 = ORIENTED_EDGE ( 'NONE', *, *, #162021, .T. ) ;
#197624 = ADVANCED_FACE ( 'NONE', ( #146583 ), #67077, .F. ) ;
#197625 = DIRECTION ( 'NONE',  ( 0.000000000000000000, -1.000000000000000000, -0.000000000000000000 ) ) ;
#197626 = CARTESIAN_POINT ( 'NONE',  ( 23.30000000000000426, -11.79999999999999538, 33.00000000000000000 ) ) ;
#197627 = CARTESIAN_POINT ( 'NONE',  ( 18.49999999999999645, 77.16412189325258453, -28.10825939895270764 ) ) ;
#197628 = ORIENTED_EDGE ( 'NONE', *, *, #189275, .T. ) ;
#197629 = CYLINDRICAL_SURFACE ( 'NONE', #135945, 1.749999999999998002 ) ;
#197631 = ORIENTED_EDGE ( 'NONE', *, *, #14647, .T. ) ;
#197630 = DIRECTION ( 'NONE',  ( 0.000000000000000000, 0.000000000000000000, -1.000000000000000000 ) ) ;
#197632 = DIRECTION ( 'NONE',  ( 0.000000000000000000, -0.1298341882519953583, -0.9915357197604862671 ) ) ;
#197633 = TOROIDAL_SURFACE ( 'NONE', #43708, 11.65000000000000036, 0.1000000000000000056 ) ;
#197634 = ORIENTED_EDGE ( 'NONE', *, *, #85910, .F. ) ;
#197635 = ADVANCED_FACE ( 'NONE', ( #226116 ), #214252, .F. ) ;
#197636 = CIRCLE ( 'NONE', #85183, 0.1000000000000001860 ) ;
#197637 = CARTESIAN_POINT ( 'NONE',  ( -21.14999999999999858, 69.74218538953603286, -136.6208977758331287 ) ) ;
#197638 = ADVANCED_FACE ( 'NONE', ( #184445 ), #199214, .F. ) ;
#197639 = ORIENTED_EDGE ( 'NONE', *, *, #148901, .T. ) ;
#197640 = CARTESIAN_POINT ( 'NONE',  ( -18.59999999999999787, 7.021664781911246322, -104.3335654018973315 ) ) ;
#197641 = FACE_OUTER_BOUND ( 'NONE', #163085, .T. ) ;
#197642 = CARTESIAN_POINT ( 'NONE',  ( -18.59999999999999787, 66.85000000001205933, -124.1731074845243512 ) ) ;
#197643 = CARTESIAN_POINT ( 'NONE',  ( 18.59117750673696534, 67.49222854868494892, -195.4187676019683693 ) ) ;
#197644 = EDGE_CURVE ( 'NONE', #118817, #30421, #164894, .T. ) ;
#197645 = DIRECTION ( 'NONE',  ( -7.304098846218201720E-16, 1.000000000000000000, 0.000000000000000000 ) ) ;
#197646 = VERTEX_POINT ( 'NONE', #60965 ) ;
#197647 = DIRECTION ( 'NONE',  ( 0.000000000000000000, 1.000000000000000000, 6.853228547068871147E-15 ) ) ;
#197648 = CARTESIAN_POINT ( 'NONE',  ( -21.04386569057595580, 11.75000000001099210, -160.6428373517797752 ) ) ;
#197649 = B_SPLINE_CURVE_WITH_KNOTS ( 'NONE', 3,
 ( #214615, #196339, #58092, #18982, #115516, #217171, #94669, #195089, #93386, #175525, #174266, #76378, #38560, #75146, #213325, #155964, #197620, #234174, #235460, #97195, #176804, #256243, #77658, #157250, #236740, #98477, #251162, #72567, #219749, #163645 ),
 .UNSPECIFIED., .F., .F.,
 ( 4, 2, 2, 2, 2, 2, 2, 2, 2, 2, 2, 2, 2, 2, 4 ),
 ( 0.000000000000000000, 0.0003422764154113370843, 0.0006845528308226741685, 0.001026829246234011199, 0.001369105661645348337, 0.002053658492468020229, 0.002738211323290691904, 0.003080487738702025139, 0.003422764154113358808, 0.003765040569524692043, 0.004107316984936025712, 0.004449593400347358514, 0.004791869815758693051, 0.005134146231170025852, 0.005476422646581359521 ),
 .UNSPECIFIED. ) ;
#197650 = ORIENTED_EDGE ( 'NONE', *, *, #117776, .F. ) ;
#197651 = FACE_OUTER_BOUND ( 'NONE', #10678, .T. ) ;
#197652 = VERTEX_POINT ( 'NONE', #5787 ) ;
#197653 = DIRECTION ( 'NONE',  ( -5.603264701231742896E-32, 0.8814952561688431665, -0.4721928772777344574 ) ) ;
#197654 = ORIENTED_EDGE ( 'NONE', *, *, #70378, .F. ) ;
#197655 = CIRCLE ( 'NONE', #219072, 0.5000000000000004441 ) ;
#197656 = CIRCLE ( 'NONE', #147601, 0.1000000000000024342 ) ;
#197657 = ADVANCED_FACE ( 'NONE', ( #27986 ), #140495, .F. ) ;
#197658 = CARTESIAN_POINT ( 'NONE',  ( -22.50000000000000000, 64.35000000001240039, -170.0231074845244166 ) ) ;
#197659 = DIRECTION ( 'NONE',  ( 0.000000000000000000, 1.734723475976807292E-15, -1.000000000000000000 ) ) ;
#197661 = ORIENTED_EDGE ( 'NONE', *, *, #1651, .F. ) ;
#197660 = LINE ( 'NONE', #19030, #56939 ) ;
#197662 = CARTESIAN_POINT ( 'NONE',  ( -20.64999999999999858, 70.12557831835937350, -215.6322690948981915 ) ) ;
#197663 = ORIENTED_EDGE ( 'NONE', *, *, #111197, .T. ) ;
#197664 = DIRECTION ( 'NONE',  ( 0.000000000000000000, -0.8814952561688423893, 0.4721928772777359007 ) ) ;
#197665 = CARTESIAN_POINT ( 'NONE',  ( -23.25000000000000000, 1.115600667400684642E-11, -100.5000000000000284 ) ) ;
#197667 = EDGE_CURVE ( 'NONE', #50215, #211121, #107481, .T. ) ;
#197666 = ORIENTED_EDGE ( 'NONE', *, *, #81576, .T. ) ;
#197668 = ORIENTED_EDGE ( 'NONE', *, *, #39855, .T. ) ;
#197669 = FACE_OUTER_BOUND ( 'NONE', #213088, .T. ) ;
#197670 = DIRECTION ( 'NONE',  ( 1.000000000000000000, -0.000000000000000000, -0.000000000000000000 ) ) ;
#197671 = ORIENTED_EDGE ( 'NONE', *, *, #11284, .F. ) ;
#197673 = CARTESIAN_POINT ( 'NONE',  ( 21.05000000000000071, 10.30543449102041187, -228.0143625250146329 ) ) ;
#197672 = AXIS2_PLACEMENT_3D ( 'NONE', #186118, #32203, #46584 ) ;
#197674 = CIRCLE ( 'NONE', #93639, 0.1000000000000028644 ) ;
#197675 = ORIENTED_EDGE ( 'NONE', *, *, #232309, .T. ) ;
#197676 = ORIENTED_EDGE ( 'NONE', *, *, #149917, .F. ) ;
#197677 = AXIS2_PLACEMENT_3D ( 'NONE', #4491, #241826, #142717 ) ;
#197678 = CARTESIAN_POINT ( 'NONE',  ( -23.25000000000000000, 40.35498466150055918, -247.8953732508333587 ) ) ;
#197680 = ORIENTED_EDGE ( 'NONE', *, *, #84971, .F. ) ;
#197679 = CARTESIAN_POINT ( 'NONE',  ( -21.05000000000000071, 1.115600667400684642E-11, -134.0000000000000284 ) ) ;
#197681 = DIRECTION ( 'NONE',  ( 0.000000000000000000, -6.982962677686266711E-15, 1.000000000000000000 ) ) ;
#197682 = FACE_OUTER_BOUND ( 'NONE', #97298, .T. ) ;
#197683 = DIRECTION ( 'NONE',  ( 0.000000000000000000, 0.000000000000000000, 1.000000000000000000 ) ) ;
#197685 = CARTESIAN_POINT ( 'NONE',  ( -1.739115166359751801E-14, 64.35000000001197407, -111.6731074845243796 ) ) ;
#197684 = CARTESIAN_POINT ( 'NONE',  ( 20.95083306685154056, 8.916842641901356004, -41.97732485325835938 ) ) ;
#197686 = DIRECTION ( 'NONE',  ( -0.000000000000000000, -0.000000000000000000, 1.000000000000000000 ) ) ;
#197687 = DIRECTION ( 'NONE',  ( -1.000000000000000000, -0.000000000000000000, -0.000000000000000000 ) ) ;
#197688 = CARTESIAN_POINT ( 'NONE',  ( 18.44444291854882323, 85.49010118095463895, -29.39420351963329026 ) ) ;
#197689 = TOROIDAL_SURFACE ( 'NONE', #27048, 0.2000000000000000111, 0.1000000000000000056 ) ;
#197690 = DIRECTION ( 'NONE',  ( 0.000000000000000000, -1.387778780781406043E-13, 1.000000000000000000 ) ) ;
#197691 = CIRCLE ( 'NONE', #106105, 0.1000000000000028644 ) ;
#197692 = ORIENTED_EDGE ( 'NONE', *, *, #213592, .F. ) ;
#197693 = VERTEX_POINT ( 'NONE', #68366 ) ;
#197694 = AXIS2_PLACEMENT_3D ( 'NONE', #5242, #240044, #24868 ) ;
#197695 = EDGE_CURVE ( 'NONE', #122992, #10605, #143497, .T. ) ;
#197697 = EDGE_CURVE ( 'NONE', #7048, #257242, #164363, .T. ) ;
#197696 = AXIS2_PLACEMENT_3D ( 'NONE', #220333, #123796, #41701 ) ;
#197699 = ORIENTED_EDGE ( 'NONE', *, *, #34503, .F. ) ;
#197698 = CARTESIAN_POINT ( 'NONE',  ( -21.05000000000000071, 87.75000000001216449, -139.4231074845242802 ) ) ;
#197700 = ORIENTED_EDGE ( 'NONE', *, *, #115129, .F. ) ;
#197701 = CARTESIAN_POINT ( 'NONE',  ( -21.14999999999999858, 41.46275801244657799, -260.2743004338703940 ) ) ;
#197702 = ORIENTED_EDGE ( 'NONE', *, *, #124477, .T. ) ;
#197703 = EDGE_CURVE ( 'NONE', #25924, #973, #197656, .T. ) ;
#197704 = ADVANCED_FACE ( 'NONE', ( #248283 ), #150480, .F. ) ;
#197705 = VECTOR ( 'NONE', #197870, 1000.000000000000000 ) ;
#197706 = AXIS2_PLACEMENT_3D ( 'NONE', #217432, #16706, #237027 ) ;
#197707 = VERTEX_POINT ( 'NONE', #170077 ) ;
#197708 = AXIS2_PLACEMENT_3D ( 'NONE', #29275, #192173, #209136 ) ;
#197709 = EDGE_CURVE ( 'NONE', #216286, #217224, #129622, .T. ) ;
#197710 =( LENGTH_UNIT ( ) NAMED_UNIT ( * ) SI_UNIT ( .MILLI., .METRE. ) );
#197711 = FACE_OUTER_BOUND ( 'NONE', #45226, .T. ) ;
#197712 = CIRCLE ( 'NONE', #147279, 0.09999999999999939493 ) ;
#197713 = EDGE_CURVE ( 'NONE', #148669, #131851, #122682, .T. ) ;
#197715 = VERTEX_POINT ( 'NONE', #69663 ) ;
#197714 = ORIENTED_EDGE ( 'NONE', *, *, #6954, .T. ) ;
#197716 = EDGE_LOOP ( 'NONE', ( #164641, #173119, #255387, #11526 ) ) ;
#197718 = ADVANCED_FACE ( 'NONE', ( #188298 ), #176843, .F. ) ;
#197717 = ADVANCED_FACE ( 'NONE', ( #132188 ), #222587, .T. ) ;
#197719 = EDGE_LOOP ( 'NONE', ( #21725, #255312, #124660, #73353 ) ) ;
#197720 = PLANE ( 'NONE',  #38054 ) ;
#197721 = CARTESIAN_POINT ( 'NONE',  ( -23.25000000000000000, 43.27008861172207332, -245.2265230569236110 ) ) ;
#197723 = EDGE_LOOP ( 'NONE', ( #108541, #136193, #8167, #214226 ) ) ;
#197722 = LINE ( 'NONE', #42495, #224908 ) ;
#197724 = CIRCLE ( 'NONE', #102031, 0.09999999999999939493 ) ;
#197725 = DIRECTION ( 'NONE',  ( -0.000000000000000000, -6.982962677686266711E-15, 1.000000000000000000 ) ) ;
#197726 = DIRECTION ( 'NONE',  ( 1.000000000000000000, 0.000000000000000000, -0.000000000000000000 ) ) ;
#197727 = VERTEX_POINT ( 'NONE', #113906 ) ;
#197728 = DIRECTION ( 'NONE',  ( 0.000000000000000000, -1.000000000000000000, 0.000000000000000000 ) ) ;
#197729 = ORIENTED_EDGE ( 'NONE', *, *, #15256, .F. ) ;
#197730 = AXIS2_PLACEMENT_3D ( 'NONE', #197012, #254408, #14571 ) ;
#197731 = CARTESIAN_POINT ( 'NONE',  ( -18.40000000000000213, 64.25000000001188027, -90.37310748452439668 ) ) ;
#197732 = CIRCLE ( 'NONE', #22983, 0.09999999999999574507 ) ;
#197734 = ORIENTED_EDGE ( 'NONE', *, *, #244331, .F. ) ;
#197733 = DIRECTION ( 'NONE',  ( 0.000000000000000000, 0.8660254037844384856, -0.5000000000000003331 ) ) ;
#197735 = CARTESIAN_POINT ( 'NONE',  ( 21.10000000000000142, 0.000000000000000000, 4.000000000000000000 ) ) ;
#197737 = EDGE_CURVE ( 'NONE', #129083, #166628, #73528, .T. ) ;
#197736 = CYLINDRICAL_SURFACE ( 'NONE', #166450, 0.09999999999998898659 ) ;
#197738 = CARTESIAN_POINT ( 'NONE',  ( 20.94560253601876809, 11.75000000001115907, -60.01008351251527984 ) ) ;
#197739 = ORIENTED_EDGE ( 'NONE', *, *, #163323, .F. ) ;
#197740 = LINE ( 'NONE', #60786, #66469 ) ;
#197741 = FACE_OUTER_BOUND ( 'NONE', #112106, .T. ) ;
#197742 = ADVANCED_FACE ( 'NONE', ( #130894, #70964, #31834 ), #253410, .F. ) ;
#197743 = EDGE_CURVE ( 'NONE', #252270, #151938, #14363, .T. ) ;
#197744 = FACE_OUTER_BOUND ( 'NONE', #116839, .T. ) ;
#197745 = CARTESIAN_POINT ( 'NONE',  ( 16.87683809663749557, 9.950000000011131718, -188.3499999999999659 ) ) ;
#197746 = CARTESIAN_POINT ( 'NONE',  ( -20.94999999999999574, 36.09166453643263850, -236.0643439437599511 ) ) ;
#197747 = EDGE_LOOP ( 'NONE', ( #22260, #9177 ) ) ;
#197748 = ORIENTED_EDGE ( 'NONE', *, *, #118285, .F. ) ;
#197749 = VERTEX_POINT ( 'NONE', #153080 ) ;
#197750 = EDGE_CURVE ( 'NONE', #142564, #70430, #230836, .T. ) ;
#197751 = LINE ( 'NONE', #42523, #238700 ) ;
#197752 = ORIENTED_EDGE ( 'NONE', *, *, #215893, .T. ) ;
#197753 = DIRECTION ( 'NONE',  ( 0.000000000000000000, -0.1298341882520022694, -0.9915357197604853789 ) ) ;
#197754 = ORIENTED_EDGE ( 'NONE', *, *, #123186, .T. ) ;
#197755 = FACE_OUTER_BOUND ( 'NONE', #216921, .T. ) ;
#197756 = ADVANCED_FACE ( 'NONE', ( #48789 ), #250832, .T. ) ;
#197757 = AXIS2_PLACEMENT_3D ( 'NONE', #243768, #204624, #26015 ) ;
#197758 = CIRCLE ( 'NONE', #68770, 0.1000000000000028644 ) ;
#197759 = EDGE_LOOP ( 'NONE', ( #14572, #73200, #92865, #36637, #106914, #92505, #80305, #143683, #51189, #3099, #169835, #199615, #161561, #59791, #24523, #88964 ) ) ;
#197760 = FACE_OUTER_BOUND ( 'NONE', #62947, .T. ) ;
#197761 = SURFACE_STYLE_USAGE ( .BOTH. , #157396 ) ;
#197762 = AXIS2_PLACEMENT_3D ( 'NONE', #227427, #207900, #189607 ) ;
#197763 = ORIENTED_EDGE ( 'NONE', *, *, #31328, .T. ) ;
#197764 = ORIENTED_EDGE ( 'NONE', *, *, #33315, .F. ) ;
#197765 = ORIENTED_EDGE ( 'NONE', *, *, #52499, .F. ) ;
#197766 = VECTOR ( 'NONE', #214018, 1000.000000000000000 ) ;
#197767 = FACE_OUTER_BOUND ( 'NONE', #70825, .T. ) ;
#197768 = DIRECTION ( 'NONE',  ( 1.000000000000000000, 0.000000000000000000, 0.000000000000000000 ) ) ;
#197769 = CIRCLE ( 'NONE', #201870, 0.09999999999999771572 ) ;
#197770 = CARTESIAN_POINT ( 'NONE',  ( 21.72449340488910252, 23.13575923509592513, -230.6406825367463966 ) ) ;
#197771 = DIRECTION ( 'NONE',  ( 0.000000000000000000, 0.000000000000000000, -1.000000000000000000 ) ) ;
#197773 = LINE ( 'NONE', #19139, #161751 ) ;
#197772 = DIRECTION ( 'NONE',  ( 0.000000000000000000, 1.000000000000000000, 0.000000000000000000 ) ) ;
#197774 = DIRECTION ( 'NONE',  ( 0.000000000000000000, 0.000000000000000000, -1.000000000000000000 ) ) ;
#197775 = ORIENTED_EDGE ( 'NONE', *, *, #127198, .F. ) ;
#197776 = DIRECTION ( 'NONE',  ( 0.000000000000000000, -0.4088369013363281068, 0.9126074666063770380 ) ) ;
#197777 = VERTEX_POINT ( 'NONE', #192179 ) ;
#197778 = CARTESIAN_POINT ( 'NONE',  ( 20.12500000000000000, 66.25000000001232081, -161.9113362024101548 ) ) ;
#197779 = VERTEX_POINT ( 'NONE', #172651 ) ;
#197780 = ORIENTED_EDGE ( 'NONE', *, *, #141279, .T. ) ;
#197781 = DIRECTION ( 'NONE',  ( 0.000000000000000000, -1.000000000000000000, 0.000000000000000000 ) ) ;
#197782 = VECTOR ( 'NONE', #48618, 1000.000000000000000 ) ;
#197783 = CARTESIAN_POINT ( 'NONE',  ( -21.12230431290519661, 69.54243334671865284, -69.52831733621336241 ) ) ;
#197784 = DIRECTION ( 'NONE',  ( 1.000000000000000000, 0.000000000000000000, -0.000000000000000000 ) ) ;
#197785 = ORIENTED_EDGE ( 'NONE', *, *, #42319, .T. ) ;
#197786 = VECTOR ( 'NONE', #48632, 1000.000000000000000 ) ;
#197787 = VERTEX_POINT ( 'NONE', #29282 ) ;
#197788 = ORIENTED_EDGE ( 'NONE', *, *, #222483, .T. ) ;
#197789 = ORIENTED_EDGE ( 'NONE', *, *, #151832, .F. ) ;
#197790 = CARTESIAN_POINT ( 'NONE',  ( -16.93226657140833069, 60.87288173690708248, -221.0975609556742540 ) ) ;
#197791 = DIRECTION ( 'NONE',  ( 1.000000000000000000, 0.000000000000000000, 0.000000000000000000 ) ) ;
#197792 = ORIENTED_EDGE ( 'NONE', *, *, #126126, .F. ) ;
#197793 = FACE_OUTER_BOUND ( 'NONE', #189080, .T. ) ;
#197794 = CIRCLE ( 'NONE', #181260, 0.1000000000000028644 ) ;
#197795 = DIRECTION ( 'NONE',  ( -0.7070776581708965169, 0.7071359030027827286, 4.937903618720407826E-15 ) ) ;
#197796 = CARTESIAN_POINT ( 'NONE',  ( 22.50014994444007499, 11.74971973190328178, -133.9169198432811072 ) ) ;
#197797 = ORIENTED_EDGE ( 'NONE', *, *, #82387, .F. ) ;
#197798 = CARTESIAN_POINT ( 'NONE',  ( 23.14999999999999858, 65.40605961984560679, -236.6728003091511425 ) ) ;
#197799 = EDGE_CURVE ( 'NONE', #252677, #147021, #149203, .T. ) ;
#197800 = CARTESIAN_POINT ( 'NONE',  ( -18.59999999999999787, 11.65000000001115232, -107.5148057706540357 ) ) ;
#197801 = CARTESIAN_POINT ( 'NONE',  ( -21.14999999999999858, 31.89597452117651244, -238.9192857152811769 ) ) ;
#197802 = ADVANCED_FACE ( 'NONE', ( #53932 ), #160099, .T. ) ;
#197803 = VECTOR ( 'NONE', #151576, 1000.000000000000000 ) ;
#197804 = ORIENTED_EDGE ( 'NONE', *, *, #139903, .T. ) ;
#197805 = AXIS2_PLACEMENT_3D ( 'NONE', #11892, #167122, #70586 ) ;
#197806 = EDGE_CURVE ( 'NONE', #211751, #137090, #193418, .T. ) ;
#197808 = ORIENTED_EDGE ( 'NONE', *, *, #208401, .F. ) ;
#197807 = CARTESIAN_POINT ( 'NONE',  ( 13.40000000000005898, 67.75000000001118394, -18.42310748452479530 ) ) ;
#197809 = EDGE_CURVE ( 'NONE', #196796, #72101, #152917, .T. ) ;
#197810 = VERTEX_POINT ( 'NONE', #95618 ) ;
#197811 = DIRECTION ( 'NONE',  ( 0.000000000000000000, 0.000000000000000000, -1.000000000000000000 ) ) ;
#197812 = CARTESIAN_POINT ( 'NONE',  ( 18.39999999999999858, 78.24390740893980478, -231.6169762517609172 ) ) ;
#197813 = CARTESIAN_POINT ( 'NONE',  ( 21.08489247129321953, 67.12232480914252619, -191.1731074845244507 ) ) ;
#197814 = CARTESIAN_POINT ( 'NONE',  ( -16.87036670365549895, 9.989418819312803066, -46.02043988269794283 ) ) ;
#197815 = CARTESIAN_POINT ( 'NONE',  ( -16.89060415895971090, 66.04877923720985677, -123.8771872602539190 ) ) ;
#197816 = ORIENTED_EDGE ( 'NONE', *, *, #126356, .T. ) ;
#197817 = LINE ( 'NONE', #160008, #146686 ) ;
#197818 = CARTESIAN_POINT ( 'NONE',  ( 21.14999999999999858, 11.65000000001115943, -45.65000000000000568 ) ) ;
#197819 = CARTESIAN_POINT ( 'NONE',  ( -18.46919391072067995, 77.27558647942372261, -241.9522046346448292 ) ) ;
#197820 = DIRECTION ( 'NONE',  ( -1.000000000000000000, 0.000000000000000000, 0.000000000000000000 ) ) ;
#197821 = TOROIDAL_SURFACE ( 'NONE', #235241, 0.2000000000000000111, 0.1000000000000000056 ) ;
#197822 = DIRECTION ( 'NONE',  ( 1.000000000000000000, 0.000000000000000000, 0.000000000000000000 ) ) ;
#197823 = EDGE_CURVE ( 'NONE', #174664, #14211, #39541, .T. ) ;
#197824 = EDGE_CURVE ( 'NONE', #58156, #10047, #52087, .T. ) ;
#197825 = ORIENTED_EDGE ( 'NONE', *, *, #39648, .T. ) ;
#197826 = ORIENTED_EDGE ( 'NONE', *, *, #36179, .T. ) ;
#197827 = CARTESIAN_POINT ( 'NONE',  ( -20.85000000000001208, 64.25000000001196554, -109.9422547304830999 ) ) ;
#197828 = CARTESIAN_POINT ( 'NONE',  ( -18.59999999999999787, 57.72708596674832648, -226.0092949359174952 ) ) ;
#197829 = LINE ( 'NONE', #233148, #118043 ) ;
#197831 = CARTESIAN_POINT ( 'NONE',  ( -18.59999999999999787, 9.250000000011157297, -155.1500000000000057 ) ) ;
#197830 = AXIS2_PLACEMENT_3D ( 'NONE', #243725, #50636, #130180 ) ;
#197832 =( BOUNDED_SURFACE ( )  B_SPLINE_SURFACE ( 3, 2, ( 
 ( #63968, #142211, #62688 ),
 ( #82205, #83490, #61395 ),
 ( #140947, #26135, #220485 ),
 ( #121411, #200906, #101768 ),
 ( #2691, #112097, #91240 ),
 ( #10419, #49538, #170823 ),
 ( #32580, #131636, #92502 ),
 ( #232044, #226882, #129080 ),
 ( #187778, #250301, #110786 ),
 ( #48248, #206044, #9131 ) ),
 .UNSPECIFIED., .F., .F., .F. ) 
 B_SPLINE_SURFACE_WITH_KNOTS ( ( 4, 2, 2, 2, 4 ),
 ( 3, 3 ),
 ( 0.002161241639767785133, 0.002579950749617447234, 0.002789305304542278284, 0.002893982582004694243, 0.002998659859467109768 ),
 ( 0.000000000000000000, 1.000000000000000000 ),
 .UNSPECIFIED. ) 
 GEOMETRIC_REPRESENTATION_ITEM ( )  RATIONAL_B_SPLINE_SURFACE ( (
 ( 1.000000000000000000, 0.7071067811864923947, 1.000000000000000000),
 ( 1.000000000000000000, 0.7632447400664396087, 1.000000000000000000),
 ( 1.000000000000000000, 0.8158073005108742448, 1.000000000000000000),
 ( 1.000000000000000000, 0.8906973462396178265, 1.000000000000000000),
 ( 1.000000000000000000, 0.9149408947802133429, 1.000000000000000000),
 ( 1.000000000000000000, 0.9493368785274678423, 1.000000000000000000),
 ( 1.000000000000000000, 0.9605194247157190501, 1.000000000000000000),
 ( 1.000000000000000000, 0.9803630264780686110, 1.000000000000000000),
 ( 1.000000000000000000, 0.9900844824271547440, 1.000000000000000000),
 ( 1.000000000000000000, 0.9894588281429235188, 1.000000000000000000) ) ) 
 REPRESENTATION_ITEM ( '' )  SURFACE ( )  );
#197833 = DIRECTION ( 'NONE',  ( -1.000000000000000000, -0.000000000000000000, 0.000000000000000000 ) ) ;
#197834 = ORIENTED_EDGE ( 'NONE', *, *, #42559, .F. ) ;
#197835 = DIRECTION ( 'NONE',  ( -6.938893903907222067E-15, 1.000000000000000000, 0.000000000000000000 ) ) ;
#197836 = CARTESIAN_POINT ( 'NONE',  ( 18.79999999999999716, -2.105948478070175156, -13.13328020565119125 ) ) ;
#197837 = ORIENTED_EDGE ( 'NONE', *, *, #235357, .F. ) ;
#197838 = SPHERICAL_SURFACE ( 'NONE', #196289, 0.1000000000000000056 ) ;
#197839 = EDGE_CURVE ( 'NONE', #194690, #7738, #39498, .T. ) ;
#197840 = DIRECTION ( 'NONE',  ( -1.000000000000000000, -0.000000000000000000, -0.000000000000000000 ) ) ;
#197841 = EDGE_CURVE ( 'NONE', #149877, #248438, #156916, .T. ) ;
#197842 = AXIS2_PLACEMENT_3D ( 'NONE', #16493, #133850, #111725 ) ;
#197843 = CIRCLE ( 'NONE', #151903, 0.4000000000000114575 ) ;
#197844 = ORIENTED_EDGE ( 'NONE', *, *, #145040, .F. ) ;
#197845 = DIRECTION ( 'NONE',  ( -1.000000000000000000, -0.000000000000000000, -0.000000000000000000 ) ) ;
#197846 = EDGE_LOOP ( 'NONE', ( #172621, #119553, #162546, #243452 ) ) ;
#197847 = DIRECTION ( 'NONE',  ( 0.000000000000000000, 1.000000000000000000, 7.116814260417668513E-15 ) ) ;
#197848 = CARTESIAN_POINT ( 'NONE',  ( 21.05000000000000071, 69.74218538953624602, -170.1208977758331855 ) ) ;
#197849 = DIRECTION ( 'NONE',  ( 1.000000000000000000, 0.000000000000000000, 0.000000000000000000 ) ) ;
#197850 = ADVANCED_FACE ( 'NONE', ( #219406 ), #35401, .T. ) ;
#197851 = CARTESIAN_POINT ( 'NONE',  ( -23.15000000000000213, 76.00000000001126921, -203.5231074845248997 ) ) ;
#197852 = CARTESIAN_POINT ( 'NONE',  ( -23.25000000000000000, 8.980461154494397746, -187.0187154576991304 ) ) ;
#197853 = CARTESIAN_POINT ( 'NONE',  ( 20.94999999999999929, 18.75483929237739389, -228.0790484105328630 ) ) ;
#197854 = DIRECTION ( 'NONE',  ( -1.000000000000000000, 0.000000000000000000, -0.000000000000000000 ) ) ;
#197855 = DIRECTION ( 'NONE',  ( 1.186688945009009831E-16, -1.000000000000000000, 0.000000000000000000 ) ) ;
#197856 = EDGE_CURVE ( 'NONE', #241591, #134704, #56187, .T. ) ;
#197857 = DIRECTION ( 'NONE',  ( -1.000000000000000000, -2.283407518332345398E-16, 1.048447799332034305E-15 ) ) ;
#197858 = CARTESIAN_POINT ( 'NONE',  ( 18.41356215285962605, -7.785976468740678946, -209.8926132507865532 ) ) ;
#197859 = LINE ( 'NONE', #19231, #18935 ) ;
#197860 = CARTESIAN_POINT ( 'NONE',  ( -20.54999999999999716, 9.350000000011156942, -121.7500000000000426 ) ) ;
#197861 = ADVANCED_FACE ( 'NONE', ( #236418 ), #233859, .F. ) ;
#197862 = VECTOR ( 'NONE', #105520, 1000.000000000000000 ) ;
#197863 = CYLINDRICAL_SURFACE ( 'NONE', #257785, 1.749999999999999778 ) ;
#197864 = DIRECTION ( 'NONE',  ( 0.000000000000000000, 0.000000000000000000, -1.000000000000000000 ) ) ;
#197865 = AXIS2_PLACEMENT_3D ( 'NONE', #129155, #24935, #206120 ) ;
#197866 = EDGE_LOOP ( 'NONE', ( #208595, #226071, #54980 ) ) ;
#197868 = CARTESIAN_POINT ( 'NONE',  ( -23.49999999999994316, 64.25000000001119815, -36.02310748452479316 ) ) ;
#197867 =( GEOMETRIC_REPRESENTATION_CONTEXT ( 3 ) GLOBAL_UNCERTAINTY_ASSIGNED_CONTEXT ( ( #107780 ) ) GLOBAL_UNIT_ASSIGNED_CONTEXT ( ( #44766, #188127, #169900 ) ) REPRESENTATION_CONTEXT ( 'NONE', 'WORKASPACE' ) );
#197869 = CARTESIAN_POINT ( 'NONE',  ( -15.75000000000000355, 62.59162599727320497, -217.2417264603073477 ) ) ;
#197870 = DIRECTION ( 'NONE',  ( 1.000000000000000000, -0.000000000000000000, -0.000000000000000000 ) ) ;
#197871 = ADVANCED_FACE ( 'NONE', ( #119052 ), #201963, .T. ) ;
#197872 = ORIENTED_EDGE ( 'NONE', *, *, #101390, .T. ) ;
#197873 = DIRECTION ( 'NONE',  ( 0.000000000000000000, -6.982962677686266711E-15, 1.000000000000000000 ) ) ;
#197874 = LINE ( 'NONE', #161342, #226384 ) ;
#197875 = ADVANCED_FACE ( 'NONE', ( #155639 ), #117752, .F. ) ;
#197876 = EDGE_LOOP ( 'NONE', ( #10578, #178916, #132914, #17345 ) ) ;
#197877 = DIRECTION ( 'NONE',  ( 0.000000000000000000, -1.000000000000000000, 0.000000000000000000 ) ) ;
#197878 = DIRECTION ( 'NONE',  ( 0.000000000000000000, -1.000000000000000000, 0.000000000000000000 ) ) ;
#197879 = VERTEX_POINT ( 'NONE', #138567 ) ;
#197880 = VECTOR ( 'NONE', #243516, 1000.000000000000000 ) ;
#197881 = AXIS2_PLACEMENT_3D ( 'NONE', #79348, #136759, #200598 ) ;
#197882 = CIRCLE ( 'NONE', #189541, 0.1000000000000072220 ) ;
#197883 = ORIENTED_EDGE ( 'NONE', *, *, #28737, .T. ) ;
#197884 = DIRECTION ( 'NONE',  ( 0.000000000000000000, 0.9126074666063844765, 0.4088369013363114535 ) ) ;
#197885 = ORIENTED_EDGE ( 'NONE', *, *, #230278, .T. ) ;
#197886 =( BOUNDED_CURVE ( )  B_SPLINE_CURVE ( 3, ( #45904, #108447, #111011, #8073 ),
 .UNSPECIFIED., .F., .F. ) 
 B_SPLINE_CURVE_WITH_KNOTS ( ( 4, 4 ),
 ( 0.3000847527772382839, 0.5497968875596824789 ),
 .UNSPECIFIED. ) 
 CURVE ( )  GEOMETRIC_REPRESENTATION_ITEM ( )  RATIONAL_B_SPLINE_CURVE ( ( 1.000000000000000000, 0.9948104011409419911, 0.9948104011409419911, 1.000000000000000000 ) ) 
 REPRESENTATION_ITEM ( '' )  );
#197887 = FACE_OUTER_BOUND ( 'NONE', #155713, .T. ) ;
#197889 = AXIS2_PLACEMENT_3D ( 'NONE', #96838, #232561, #216811 ) ;
#197888 = DIRECTION ( 'NONE',  ( -0.000000000000000000, -0.000000000000000000, 1.000000000000000000 ) ) ;
#197891 = FACE_OUTER_BOUND ( 'NONE', #98960, .T. ) ;
#197890 = CIRCLE ( 'NONE', #110606, 0.1999999999999987899 ) ;
#197892 = DIRECTION ( 'NONE',  ( 0.000000000000000000, -1.265107689135680095E-16, 1.000000000000000000 ) ) ;
#197893 = DIRECTION ( 'NONE',  ( 1.000000000000000000, 0.000000000000000000, 0.000000000000000000 ) ) ;
#197894 = LINE ( 'NONE', #38845, #76105 ) ;
#197895 = FACE_OUTER_BOUND ( 'NONE', #76285, .T. ) ;
#197897 = ORIENTED_EDGE ( 'NONE', *, *, #212652, .F. ) ;
#197896 = CARTESIAN_POINT ( 'NONE',  ( 18.40916198585727059, 86.89640093994682957, -199.6396876344186637 ) ) ;
#197898 = ORIENTED_EDGE ( 'NONE', *, *, #65669, .F. ) ;
#197900 = CARTESIAN_POINT ( 'NONE',  ( -21.12844524849339223, 64.25000000001161027, -62.61869401368159771 ) ) ;
#197899 = FACE_OUTER_BOUND ( 'NONE', #104342, .T. ) ;
#197903 = ORIENTED_EDGE ( 'NONE', *, *, #149436, .T. ) ;
#197902 = CARTESIAN_POINT ( 'NONE',  ( 21.14261333020286671, 10.71569264926606202, -146.2500000000002274 ) ) ;
#197901 = DIRECTION ( 'NONE',  ( 1.000000000000000000, 0.000000000000000000, 0.000000000000000000 ) ) ;
#197904 = ORIENTED_EDGE ( 'NONE', *, *, #47150, .T. ) ;
#197905 = CARTESIAN_POINT ( 'NONE',  ( -16.93935632781549572, 66.01526950028714680, -149.1334467358141467 ) ) ;
#197906 = DIRECTION ( 'NONE',  ( 0.000000000000000000, 0.000000000000000000, 1.000000000000000000 ) ) ;
#197907 = AXIS2_PLACEMENT_3D ( 'NONE', #194672, #215477, #33046 ) ;
#197908 = CARTESIAN_POINT ( 'NONE',  ( 20.85000000000000142, -1.164121893230052995, -208.9148480855715775 ) ) ;
#197909 = CARTESIAN_POINT ( 'NONE',  ( 18.59999999999999076, 6.450000000011156587, -121.7500000000000426 ) ) ;
#197910 = CARTESIAN_POINT ( 'NONE',  ( 20.12500000000000000, 9.750000000011153745, -108.6117712821143186 ) ) ;
#197911 = DIRECTION ( 'NONE',  ( -5.603264701231743991E-32, -7.172728831056617961E-15, 1.000000000000000000 ) ) ;
#197912 = CIRCLE ( 'NONE', #189569, 0.09999999999998898659 ) ;
#197913 = LINE ( 'NONE', #74165, #211273 ) ;
#197914 = CARTESIAN_POINT ( 'NONE',  ( 20.94999999999999929, -1.362429037182151470, -175.3888812479212334 ) ) ;
#197915 = ORIENTED_EDGE ( 'NONE', *, *, #177808, .T. ) ;
#197916 = ORIENTED_EDGE ( 'NONE', *, *, #141267, .F. ) ;
#197917 = CARTESIAN_POINT ( 'NONE',  ( -21.05000000000000071, 47.95459712139159336, -246.5019368548292675 ) ) ;
#197918 = VERTEX_POINT ( 'NONE', #137307 ) ;
#197919 = CARTESIAN_POINT ( 'NONE',  ( 23.14999999999999858, 9.374458193048763377, -220.5475659691911119 ) ) ;
#197920 = ORIENTED_EDGE ( 'NONE', *, *, #79017, .F. ) ;
#197921 = DIRECTION ( 'NONE',  ( 0.000000000000000000, 0.2617529984164955192, 0.9651348961777178603 ) ) ;
#197922 =( BOUNDED_SURFACE ( )  B_SPLINE_SURFACE ( 3, 2, ( 
 ( #76431, #95987, #257582 ),
 ( #77705, #157289, #236785 ),
 ( #154725, #119434, #178133 ),
 ( #115563, #78974, #724 ),
 ( #16490, #175564, #215933 ),
 ( #60710, #140244, #193832 ),
 ( #37335, #19032, #158574 ),
 ( #238073, #75186, #255011 ) ),
 .UNSPECIFIED., .F., .F., .F. ) 
 B_SPLINE_SURFACE_WITH_KNOTS ( ( 4, 2, 2, 4 ),
 ( 3, 3 ),
 ( 0.0001723339234021435316, 0.0002782939632049939412, 0.0003842540030078444050, 0.0005961740826135453327 ),
 ( 0.000000000000000000, 1.000000000000000000 ),
 .UNSPECIFIED. ) 
 GEOMETRIC_REPRESENTATION_ITEM ( )  RATIONAL_B_SPLINE_SURFACE ( (
 ( 1.000000000000000000, 0.9504532311154613167, 1.000000000000000000),
 ( 1.000000000000000000, 0.9506023220703098131, 1.000000000000000000),
 ( 1.000000000000000000, 0.9395774818190307798, 1.000000000000000000),
 ( 1.000000000000000000, 0.9079328464638727336, 1.000000000000000000),
 ( 1.000000000000000000, 0.8875702416201843858, 1.000000000000000000),
 ( 1.000000000000000000, 0.8205919608046280400, 1.000000000000000000),
 ( 1.000000000000000000, 0.7666842783593341704, 1.000000000000000000),
 ( 1.000000000000000000, 0.7071067811864559793, 1.000000000000000000) ) ) 
 REPRESENTATION_ITEM ( '' )  SURFACE ( )  );
#197923 = DIRECTION ( 'NONE',  ( 0.000000000000000000, 0.000000000000000000, -1.000000000000000000 ) ) ;
#197924 = LINE ( 'NONE', #231956, #156029 ) ;
#197925 = ADVANCED_FACE ( 'NONE', ( #99452 ), #235142, .T. ) ;
#197926 = CARTESIAN_POINT ( 'NONE',  ( 18.47149038651512143, -9.671457157995547504, -207.6727863347383618 ) ) ;
#197927 = FACE_OUTER_BOUND ( 'NONE', #135444, .T. ) ;
#197928 = ORIENTED_EDGE ( 'NONE', *, *, #121257, .T. ) ;
#197929 = FACE_OUTER_BOUND ( 'NONE', #102041, .T. ) ;
#197930 = VECTOR ( 'NONE', #97168, 1000.000000000000000 ) ;
#197931 = EDGE_CURVE ( 'NONE', #228584, #168498, #216898, .T. ) ;
#197932 = DIRECTION ( 'NONE',  ( 0.000000000000000000, 0.000000000000000000, -1.000000000000000000 ) ) ;
#197933 = ADVANCED_FACE ( 'NONE', ( #367 ), #56477, .F. ) ;
#197934 = PLANE ( 'NONE',  #206148 ) ;
#197935 = AXIS2_PLACEMENT_3D ( 'NONE', #4854, #182253, #27053 ) ;
#197936 = DIRECTION ( 'NONE',  ( 0.000000000000000000, -0.9910465087640866200, 0.1335171055202867274 ) ) ;
#197937 = DIRECTION ( 'NONE',  ( -2.978066053179067751E-16, 1.000000000000000000, 0.000000000000000000 ) ) ;
#197938 = VECTOR ( 'NONE', #211096, 1000.000000000000000 ) ;
#197939 = ORIENTED_EDGE ( 'NONE', *, *, #73247, .F. ) ;
#197940 = CARTESIAN_POINT ( 'NONE',  ( -18.40000000000000213, 85.50000000001139711, -29.10095763519389322 ) ) ;
#197941 = ORIENTED_EDGE ( 'NONE', *, *, #115334, .T. ) ;
#197944 = VERTEX_POINT ( 'NONE', #139868 ) ;
#197943 = DIRECTION ( 'NONE',  ( 1.000000000000000000, 0.000000000000000000, 0.000000000000000000 ) ) ;
#197942 = CARTESIAN_POINT ( 'NONE',  ( -22.59999985501179154, 64.25013020700970401, -203.5887061543241714 ) ) ;
#197945 = CARTESIAN_POINT ( 'NONE',  ( -22.32929514600008503, 0.09907567812507747651, -159.9213524346234578 ) ) ;
#197946 = CIRCLE ( 'NONE', #6413, 11.70000000000001172 ) ;
#197947 = LINE ( 'NONE', #177142, #204431 ) ;
#197948 = AXIS2_PLACEMENT_3D ( 'NONE', #150022, #110872, #71767 ) ;
#197949 = ORIENTED_EDGE ( 'NONE', *, *, #139361, .T. ) ;
#197950 = DIRECTION ( 'NONE',  ( 0.000000000000000000, -0.1298341882520022694, -0.9915357197604852679 ) ) ;
#197951 = EDGE_CURVE ( 'NONE', #103565, #201031, #21258, .T. ) ;
#197952 = DIRECTION ( 'NONE',  ( -0.000000000000000000, -0.000000000000000000, -1.000000000000000000 ) ) ;
#197953 = CARTESIAN_POINT ( 'NONE',  ( 20.85000000000000142, 11.75000000001115907, -60.21613433702191287 ) ) ;
#197954 = VECTOR ( 'NONE', #43456, 1000.000000000000227 ) ;
#197955 = UNCERTAINTY_MEASURE_WITH_UNIT (LENGTH_MEASURE( 1.000000000000000082E-05 ), #1399, 'distance_accuracy_value', 'NONE');
#197957 = EDGE_LOOP ( 'NONE', ( #70718, #36697, #67118, #73959 ) ) ;
#197956 = DIRECTION ( 'NONE',  ( -1.000000000000000000, -0.000000000000000000, 0.000000000000000000 ) ) ;
#197958 = CIRCLE ( 'NONE', #164660, 0.5000000000000004441 ) ;
#197959 = CARTESIAN_POINT ( 'NONE',  ( -20.54999999999999716, 85.00000000001179501, -79.01707660717669057 ) ) ;
#197960 = VECTOR ( 'NONE', #24662, 1000.000000000000000 ) ;
#197961 = ORIENTED_EDGE ( 'NONE', *, *, #96031, .F. ) ;
#197962 = DIRECTION ( 'NONE',  ( 0.000000000000000000, 0.9654727137038715545, -0.2605042016806676242 ) ) ;
#197963 = DIRECTION ( 'NONE',  ( 0.000000000000000000, 0.000000000000000000, 1.000000000000000000 ) ) ;
#197964 = DIRECTION ( 'NONE',  ( 0.000000000000000000, -0.7397890806274222131, -0.6728388485993012091 ) ) ;
#197965 = VERTEX_POINT ( 'NONE', #223263 ) ;
#197966 = CARTESIAN_POINT ( 'NONE',  ( -33.72168855820452649, 64.52683809664929981, -78.77310748452438816 ) ) ;
#197967 = ORIENTED_EDGE ( 'NONE', *, *, #255113, .F. ) ;
#197968 = CARTESIAN_POINT ( 'NONE',  ( 6.100000000000049383, 64.35000000001120668, -51.02310748452480738 ) ) ;
#197969 = EDGE_CURVE ( 'NONE', #2377, #221167, #221960, .T. ) ;
#197970 = CYLINDRICAL_SURFACE ( 'NONE', #68254, 0.09999999999999939493 ) ;
#197971 = CARTESIAN_POINT ( 'NONE',  ( -21.05000000000000071, 1.148907358139439339E-11, -201.0000000000015064 ) ) ;
#197972 = ADVANCED_FACE ( 'NONE', ( #160769 ), #245421, .T. ) ;
#197973 = CIRCLE ( 'NONE', #93926, 0.09999999999999543976 ) ;
#197974 = ORIENTED_EDGE ( 'NONE', *, *, #97323, .F. ) ;
#197975 = CARTESIAN_POINT ( 'NONE',  ( 21.05000000000000071, 22.90266353732884497, -230.0169390150674076 ) ) ;
#197976 = DIRECTION ( 'NONE',  ( 0.000000000000000000, -0.9797463026583741463, -0.2002428086779788896 ) ) ;
#197977 = CARTESIAN_POINT ( 'NONE',  ( 21.05000000000000071, -9.000000000000000000, -24.00603087734755547 ) ) ;
#197979 = EDGE_CURVE ( 'NONE', #104336, #61955, #47805, .T. ) ;
#197978 = ORIENTED_EDGE ( 'NONE', *, *, #57803, .F. ) ;
#197980 = CARTESIAN_POINT ( 'NONE',  ( 22.39999999999999503, 11.75000000000000000, 0.09999999999999592548 ) ) ;
#197981 = FACE_OUTER_BOUND ( 'NONE', #96194, .T. ) ;
#197982 = CIRCLE ( 'NONE', #81439, 4.049999999999998046 ) ;
#197983 = CIRCLE ( 'NONE', #10573, 7.900000000000002132 ) ;
#197984 = ORIENTED_EDGE ( 'NONE', *, *, #152519, .F. ) ;
#197985 = DIRECTION ( 'NONE',  ( 0.000000000000000000, 0.000000000000000000, -1.000000000000000000 ) ) ;
#197986 = VERTEX_POINT ( 'NONE', #201142 ) ;
#197988 = ORIENTED_EDGE ( 'NONE', *, *, #226132, .F. ) ;
#197987 = CARTESIAN_POINT ( 'NONE',  ( -21.14999999999999858, 12.62988036037870465, -223.4632815780722694 ) ) ;
#197992 = EDGE_CURVE ( 'NONE', #7914, #193723, #147797, .T. ) ;
#197991 = ORIENTED_EDGE ( 'NONE', *, *, #194896, .F. ) ;
#197990 = EDGE_LOOP ( 'NONE', ( #17187, #145074, #66219, #94077, #147064 ) ) ;
#197989 = CARTESIAN_POINT ( 'NONE',  ( -21.08134388332232589, 0.07581891750697818122, 6.334680580517975557 ) ) ;
#197993 = PLANE ( 'NONE',  #112202 ) ;
#197994 = CARTESIAN_POINT ( 'NONE',  ( -20.89192007715127986, 65.67101464000451472, -30.44043916224795510 ) ) ;
#197995 = CARTESIAN_POINT ( 'NONE',  ( -18.59999999999999787, 9.350000000011156942, -54.65000000000000568 ) ) ;
#197996 = DIRECTION ( 'NONE',  ( -0.7071067811865475727, 0.7071067811865475727, 4.937700262164531476E-15 ) ) ;
#197997 = CARTESIAN_POINT ( 'NONE',  ( 23.14999999999999503, 11.65000000001116298, -93.48519422934610645 ) ) ;
#197998 = CIRCLE ( 'NONE', #247901, 0.1000000000000124678 ) ;
#197999 = DIRECTION ( 'NONE',  ( 0.000000000000000000, 0.000000000000000000, -1.000000000000000000 ) ) ;
#198000 = CARTESIAN_POINT ( 'NONE',  ( 21.87500000000000355, 30.37633856152204359, -235.1250019192171408 ) ) ;
#198002 = DIRECTION ( 'NONE',  ( 0.000000000000000000, 0.000000000000000000, -1.000000000000000000 ) ) ;
#198001 = CARTESIAN_POINT ( 'NONE',  ( -20.93284271247462058, 17.11694853917243719, -224.3781540347815451 ) ) ;
#198003 = VERTEX_POINT ( 'NONE', #125472 ) ;
#198004 = ORIENTED_EDGE ( 'NONE', *, *, #175897, .F. ) ;
#198005 = EDGE_CURVE ( 'NONE', #102227, #68445, #447, .T. ) ;
#198006 = CARTESIAN_POINT ( 'NONE',  ( -23.15000000000000213, 56.06656052939784729, -228.0911609752645290 ) ) ;
#198007 = AXIS2_PLACEMENT_3D ( 'NONE', #141737, #81732, #3503 ) ;
#198009 = ORIENTED_EDGE ( 'NONE', *, *, #27587, .F. ) ;
#198008 = CARTESIAN_POINT ( 'NONE',  ( 21.14999999999999858, 0.000000000000000000, -0.09999999999999592548 ) ) ;
#198010 = LINE ( 'NONE', #80614, #59078 ) ;
#198011 = ORIENTED_EDGE ( 'NONE', *, *, #81845, .T. ) ;
#198012 = DIRECTION ( 'NONE',  ( 0.000000000000000000, 0.000000000000000000, 1.000000000000000000 ) ) ;
#198013 = ORIENTED_EDGE ( 'NONE', *, *, #169033, .T. ) ;
#198014 = FACE_OUTER_BOUND ( 'NONE', #223223, .T. ) ;
#198015 = EDGE_CURVE ( 'NONE', #117567, #174834, #184141, .T. ) ;
#198016 = EDGE_CURVE ( 'NONE', #201957, #240784, #182891, .T. ) ;
#198017 = EDGE_LOOP ( 'NONE', ( #110981, #148756, #97296, #123549 ) ) ;
#198018 = CARTESIAN_POINT ( 'NONE',  ( 23.14999999999998437, 1.148907358139439339E-11, -201.0000000000015064 ) ) ;
#198019 = LINE ( 'NONE', #79349, #152756 ) ;
#198020 = EDGE_CURVE ( 'NONE', #100043, #116896, #224551, .T. ) ;
#198023 = ORIENTED_EDGE ( 'NONE', *, *, #48316, .F. ) ;
#198022 = ORIENTED_EDGE ( 'NONE', *, *, #134603, .F. ) ;
#198021 = AXIS2_PLACEMENT_3D ( 'NONE', #58139, #42450, #201523 ) ;
#198024 = VECTOR ( 'NONE', #178606, 1000.000000000000000 ) ;
#198025 = VERTEX_POINT ( 'NONE', #65480 ) ;
#198027 = ADVANCED_FACE ( 'NONE', ( #103311 ), #139389, .T. ) ;
#198026 = LINE ( 'NONE', #257958, #227823 ) ;
#198028 = ORIENTED_EDGE ( 'NONE', *, *, #135079, .F. ) ;
#198029 = ORIENTED_EDGE ( 'NONE', *, *, #22510, .F. ) ;
#198030 = DIRECTION ( 'NONE',  ( 1.000000000000000000, 0.000000000000000000, 0.000000000000000000 ) ) ;
#198031 = ORIENTED_EDGE ( 'NONE', *, *, #159592, .T. ) ;
#198032 = EDGE_CURVE ( 'NONE', #24563, #42426, #163315, .T. ) ;
#198034 = CARTESIAN_POINT ( 'NONE',  ( 20.95420533658165141, 65.45413552525275236, -162.4556014638312149 ) ) ;
#198033 = CARTESIAN_POINT ( 'NONE',  ( -23.25000000000000355, 70.35000000001190301, -93.77310748452434552 ) ) ;
#198035 = DIRECTION ( 'NONE',  ( 1.000000000000000000, -0.000000000000000000, -0.000000000000000000 ) ) ;
#198036 = DIRECTION ( 'NONE',  ( 1.000000000000000000, 0.000000000000000000, 0.000000000000000000 ) ) ;
#198037 = FACE_OUTER_BOUND ( 'NONE', #130192, .T. ) ;
#198038 = ORIENTED_EDGE ( 'NONE', *, *, #237310, .T. ) ;
#198039 = ORIENTED_EDGE ( 'NONE', *, *, #221272, .T. ) ;
#198040 = CARTESIAN_POINT ( 'NONE',  ( 23.14999999999999858, 71.00000000001151079, -48.42837350343745584 ) ) ;
#198041 = CARTESIAN_POINT ( 'NONE',  ( 18.49999999999999289, 65.50857864377491069, -145.1731074845244507 ) ) ;
#198043 = EDGE_CURVE ( 'NONE', #86618, #20356, #6116, .T. ) ;
#198042 = PLANE ( 'NONE',  #212222 ) ;
#198044 = CIRCLE ( 'NONE', #252201, 11.65000000000000036 ) ;
#198045 = ORIENTED_EDGE ( 'NONE', *, *, #85001, .F. ) ;
#198047 = MANIFOLD_SOLID_BREP ( 'Stock-MAS-200-1', #203301 ) ;
#198046 = CARTESIAN_POINT ( 'NONE',  ( 18.49999999999999645, 67.23127455305841238, -235.8551265064783991 ) ) ;
#198048 = CIRCLE ( 'NONE', #256234, 0.09999999999999999167 ) ;
#198049 = EDGE_CURVE ( 'NONE', #176580, #180347, #176029, .T. ) ;
#198050 = ADVANCED_FACE ( 'NONE', ( #62920 ), #220283, .F. ) ;
#198051 = AXIS2_PLACEMENT_3D ( 'NONE', #151661, #228615, #231190 ) ;
#198052 = CIRCLE ( 'NONE', #56390, 0.09999999999999976963 ) ;
#198053 = FACE_OUTER_BOUND ( 'NONE', #72797, .T. ) ;
#198054 = CARTESIAN_POINT ( 'NONE',  ( 23.24999999999999289, 11.65000000001116298, -54.85000000000000142 ) ) ;
#198055 = ORIENTED_EDGE ( 'NONE', *, *, #87734, .F. ) ;
#198056 = ORIENTED_EDGE ( 'NONE', *, *, #174018, .F. ) ;
#198057 = EDGE_CURVE ( 'NONE', #226700, #61549, #106061, .T. ) ;
#198058 = CARTESIAN_POINT ( 'NONE',  ( -20.94999999999999929, -1.835341550213257733, -112.0551512925630249 ) ) ;
#198059 = DIRECTION ( 'NONE',  ( -0.000000000000000000, -0.000000000000000000, -1.000000000000000000 ) ) ;
#198060 = ORIENTED_EDGE ( 'NONE', *, *, #208286, .T. ) ;
#198061 = CARTESIAN_POINT ( 'NONE',  ( 16.27683809663749770, 66.65000000001191438, -93.77310748452437394 ) ) ;
#198062 = ORIENTED_EDGE ( 'NONE', *, *, #211565, .F. ) ;
#198063 = DIRECTION ( 'NONE',  ( -0.000000000000000000, -6.982962677686266711E-15, 1.000000000000000000 ) ) ;
#198064 = LINE ( 'NONE', #57251, #149784 ) ;
#198066 = CYLINDRICAL_SURFACE ( 'NONE', #79328, 0.09999999999999543976 ) ;
#198065 = FACE_OUTER_BOUND ( 'NONE', #5096, .T. ) ;
#198067 = EDGE_CURVE ( 'NONE', #72101, #246385, #97866, .T. ) ;
#198069 = EDGE_CURVE ( 'NONE', #24262, #176398, #40387, .T. ) ;
#198068 = CARTESIAN_POINT ( 'NONE',  ( 22.49066049874202022, 0.05634325154338429287, -55.34998776248293950 ) ) ;
#198070 = CARTESIAN_POINT ( 'NONE',  ( -20.85000000000000142, 78.57213941646344324, -232.7862224702232652 ) ) ;
#198071 = EDGE_CURVE ( 'NONE', #43706, #188542, #140693, .T. ) ;
#198072 = CARTESIAN_POINT ( 'NONE',  ( -20.94999999999999929, 0.000000000000000000, -33.50000000000000000 ) ) ;
#198073 = CIRCLE ( 'NONE', #56570, 0.09999999999998898659 ) ;
#198074 = PRESENTATION_LAYER_ASSIGNMENT (  '', '', ( #23128 ) ) ;
#198076 = ORIENTED_EDGE ( 'NONE', *, *, #81759, .F. ) ;
#198075 = VERTEX_POINT ( 'NONE', #199439 ) ;
#198077 = EDGE_LOOP ( 'NONE', ( #160545, #35993, #36857 ) ) ;
#198078 = VECTOR ( 'NONE', #121325, 1000.000000000000114 ) ;
#198079 = CARTESIAN_POINT ( 'NONE',  ( -23.25000000000000000, 67.23127455305841238, -235.8551265064783991 ) ) ;
#198080 = DIRECTION ( 'NONE',  ( 0.000000000000000000, 0.9126074666064696306, 0.4088369013361213278 ) ) ;
#198081 = DIRECTION ( 'NONE',  ( -1.000000000000000000, -0.000000000000000000, -0.000000000000000000 ) ) ;
#198082 = VECTOR ( 'NONE', #78574, 1000.000000000000000 ) ;
#198083 = LINE ( 'NONE', #215081, #245084 ) ;
#198084 = EDGE_CURVE ( 'NONE', #82189, #20391, #60293, .T. ) ;
#198086 = CARTESIAN_POINT ( 'NONE',  ( 20.94999999999999929, 87.24382154048164750, -206.5725299160771726 ) ) ;
#198085 = CARTESIAN_POINT ( 'NONE',  ( 20.30531438145591139, 10.09690106109084695, -7.796017807273384115 ) ) ;
#198087 = VERTEX_POINT ( 'NONE', #239838 ) ;
#198088 = CARTESIAN_POINT ( 'NONE',  ( -16.87683809663752399, 66.15000000001153069, -49.42547150272069700 ) ) ;
#198089 = ORIENTED_EDGE ( 'NONE', *, *, #237014, .T. ) ;
#198090 = CIRCLE ( 'NONE', #114890, 0.1000000000000091649 ) ;
#198091 = DIRECTION ( 'NONE',  ( 1.000000000000000000, 0.000000000000000000, 0.000000000000000000 ) ) ;
#198092 = TOROIDAL_SURFACE ( 'NONE', #210558, 0.6000000000000013101, 0.1000000000000000056 ) ;
#198093 = VECTOR ( 'NONE', #125240, 1000.000000000000000 ) ;
#198094 = VERTEX_POINT ( 'NONE', #100291 ) ;
#198095 = ORIENTED_EDGE ( 'NONE', *, *, #45031, .T. ) ;
#198096 = CARTESIAN_POINT ( 'NONE',  ( 18.59999999999999432, 77.44184265367997000, -241.6694879557322508 ) ) ;
#198097 = DIRECTION ( 'NONE',  ( 0.000000000000000000, 1.000000000000000000, 0.000000000000000000 ) ) ;
#198098 = LINE ( 'NONE', #32968, #254243 ) ;
#198099 = CARTESIAN_POINT ( 'NONE',  ( -22.39999999999999858, 7.591056067193246548, -199.2444047917219052 ) ) ;
#198100 = LINE ( 'NONE', #122428, #154891 ) ;
#198101 = ORIENTED_EDGE ( 'NONE', *, *, #77916, .T. ) ;
#198102 = EDGE_LOOP ( 'NONE', ( #121030, #224135, #257921, #135222, #99863, #121676, #7535, #160286, #192272, #7421 ) ) ;
#198103 = VECTOR ( 'NONE', #195941, 1000.000000000000000 ) ;
#198104 = DIRECTION ( 'NONE',  ( 1.000000000000000000, 0.000000000000000000, 0.000000000000000000 ) ) ;
#198105 = DIRECTION ( 'NONE',  ( 1.000000000000000000, 0.000000000000000000, 0.000000000000000000 ) ) ;
#198106 = ORIENTED_EDGE ( 'NONE', *, *, #146902, .T. ) ;
#198107 = CARTESIAN_POINT ( 'NONE',  ( -23.25000000000000000, 87.75000000001172396, -69.52310748452423184 ) ) ;
#198108 = CARTESIAN_POINT ( 'NONE',  ( -22.39999999999999858, 76.10085836911045476, -81.27267460801371612 ) ) ;
#198109 = CIRCLE ( 'NONE', #85634, 1.749999999999998002 ) ;
#198110 = DIRECTION ( 'NONE',  ( 1.000000000000000000, 0.000000000000000000, 0.000000000000000000 ) ) ;
#198111 = AXIS2_PLACEMENT_3D ( 'NONE', #5815, #224866, #164911 ) ;
#198112 = DIRECTION ( 'NONE',  ( 1.000000000000000000, 2.952720810173289112E-16, -0.000000000000000000 ) ) ;
#198113 = LINE ( 'NONE', #196819, #17599 ) ;
#198114 = CARTESIAN_POINT ( 'NONE',  ( 21.05000000000000071, -8.999999999988842703, -191.5060308773475128 ) ) ;
#198116 = DIRECTION ( 'NONE',  ( 0.000000000000000000, 1.000000000000000000, 0.000000000000000000 ) ) ;
#198115 = FACE_OUTER_BOUND ( 'NONE', #110478, .T. ) ;
#198117 = CARTESIAN_POINT ( 'NONE',  ( -20.64999999999999858, 19.93396995659180249, -235.7707092203739307 ) ) ;
#198118 = CARTESIAN_POINT ( 'NONE',  ( 21.05000000000000426, 65.43724016256057041, -62.06629352660576870 ) ) ;
#198119 = EDGE_CURVE ( 'NONE', #36105, #72109, #197843, .T. ) ;
#198120 = CARTESIAN_POINT ( 'NONE',  ( 18.59999999999999432, 1.736257131608553550, -78.56865232901755292 ) ) ;
#198122 = VERTEX_POINT ( 'NONE', #116046 ) ;
#198121 = CARTESIAN_POINT ( 'NONE',  ( -18.59999999999999787, 14.73746888278882494, -235.8584165281851028 ) ) ;
#198123 = EDGE_CURVE ( 'NONE', #188383, #204007, #85383, .T. ) ;
#198124 = ORIENTED_EDGE ( 'NONE', *, *, #77062, .T. ) ;
#198125 = CARTESIAN_POINT ( 'NONE',  ( -18.40000000000000213, 23.60914413563410008, -229.5451841312037402 ) ) ;
#198126 = EDGE_CURVE ( 'NONE', #155597, #42984, #161601, .T. ) ;
#198127 = ORIENTED_EDGE ( 'NONE', *, *, #77126, .F. ) ;
#198128 = CARTESIAN_POINT ( 'NONE',  ( -22.39999999999999858, 75.90000000001170122, -77.31388708289772183 ) ) ;
#198129 = AXIS2_PLACEMENT_3D ( 'NONE', #134409, #69344, #172331 ) ;
#198131 = VERTEX_POINT ( 'NONE', #57317 ) ;
#198130 = AXIS2_PLACEMENT_3D ( 'NONE', #56517, #136052, #155682 ) ;
#198132 = DIRECTION ( 'NONE',  ( 0.000000000000000000, -0.1298341882519953860, -0.9915357197604862671 ) ) ;
#198133 = AXIS2_PLACEMENT_3D ( 'NONE', #152116, #234178, #251167 ) ;
#198134 = CARTESIAN_POINT ( 'NONE',  ( -18.59999999999999787, 64.25000000001229239, -157.8731074845244393 ) ) ;
#198135 = CARTESIAN_POINT ( 'NONE',  ( 22.41477678272288188, 0.0008238657741001866345, -21.85041471548460379 ) ) ;
#198136 = SPHERICAL_SURFACE ( 'NONE', #101543, 0.1000000000000000056 ) ;
#198137 = CARTESIAN_POINT ( 'NONE',  ( 20.10000000000000853, 5.552655413246003313, 16.61686199900910310 ) ) ;
#198138 = CARTESIAN_POINT ( 'NONE',  ( -22.50000000000000000, 11.75000000001115552, -100.5000000000000284 ) ) ;
#198139 = CIRCLE ( 'NONE', #148249, 12.97499999999999964 ) ;
#198140 = ORIENTED_EDGE ( 'NONE', *, *, #92716, .F. ) ;
#198141 = DIRECTION ( 'NONE',  ( 1.000000000000000000, 0.000000000000000000, 0.000000000000000000 ) ) ;
#198143 = ORIENTED_EDGE ( 'NONE', *, *, #158388, .F. ) ;
#198142 = DIRECTION ( 'NONE',  ( -1.000000000000000000, 0.000000000000000000, 0.000000000000000000 ) ) ;
#198144 = DIRECTION ( 'NONE',  ( -1.000000000000000000, 0.000000000000000000, -0.000000000000000000 ) ) ;
#198145 = CARTESIAN_POINT ( 'NONE',  ( -16.80117486205003630, 9.949657268323468529, -188.3488548729254717 ) ) ;
#198146 = DIRECTION ( 'NONE',  ( 0.000000000000000000, 0.000000000000000000, -1.000000000000000000 ) ) ;
#198147 = AXIS2_PLACEMENT_3D ( 'NONE', #41900, #5281, #165699 ) ;
#198148 = VERTEX_POINT ( 'NONE', #41650 ) ;
#198149 = FACE_OUTER_BOUND ( 'NONE', #189099, .T. ) ;
#198150 = VECTOR ( 'NONE', #239486, 1000.000000000000000 ) ;
#198151 = PRODUCT_CONTEXT ( 'NONE', #212334, 'mechanical' ) ;
#198152 = CARTESIAN_POINT ( 'NONE',  ( -20.15000000000000568, 9.291421356248463326, -146.2500000000000284 ) ) ;
#198153 = VECTOR ( 'NONE', #66972, 1000.000000000000227 ) ;
#198154 = ORIENTED_EDGE ( 'NONE', *, *, #58298, .T. ) ;
#198155 = FACE_OUTER_BOUND ( 'NONE', #119715, .T. ) ;
#198156 = LINE ( 'NONE', #19538, #21630 ) ;
#198157 = EDGE_CURVE ( 'NONE', #246455, #97895, #231198, .T. ) ;
#198158 =( LENGTH_UNIT ( ) NAMED_UNIT ( * ) SI_UNIT ( .MILLI., .METRE. ) );
#198159 = ORIENTED_EDGE ( 'NONE', *, *, #6385, .T. ) ;
#198160 = AXIS2_PLACEMENT_3D ( 'NONE', #183584, #84425, #152184 ) ;
#198161 = ORIENTED_EDGE ( 'NONE', *, *, #78120, .T. ) ;
#198162 = DIRECTION ( 'NONE',  ( 1.000000000000000000, 0.000000000000000000, 0.000000000000000000 ) ) ;
#198163 = DIRECTION ( 'NONE',  ( 0.000000000000000000, 0.2617529984165031798, 0.9651348961777156399 ) ) ;
#198164 = EDGE_CURVE ( 'NONE', #5222, #148838, #93619, .T. ) ;
#198165 = PLANE ( 'NONE',  #98620 ) ;
#198166 = DIRECTION ( 'NONE',  ( 2.840903330521631775E-16, -0.8700118002898321601, 0.4930308989875230585 ) ) ;
#198167 = CARTESIAN_POINT ( 'NONE',  ( -21.14999999999994174, 74.16448838626247664, -47.52760213295649550 ) ) ;
#198168 = CARTESIAN_POINT ( 'NONE',  ( -23.15000000000000213, 0.000000000000000000, -33.50000000000000000 ) ) ;
#198169 = EDGE_CURVE ( 'NONE', #16840, #178804, #239366, .T. ) ;
#198171 = PLANE ( 'NONE',  #162151 ) ;
#198170 = DIRECTION ( 'NONE',  ( 0.5932847527679310229, -0.3801118060259202069, -0.7095972217059536291 ) ) ;
#198172 = DIRECTION ( 'NONE',  ( -1.000000000000000000, -0.000000000000000000, -0.000000000000000000 ) ) ;
#198173 = CARTESIAN_POINT ( 'NONE',  ( 20.94999999999999574, -1.835341550224411922, -11.55515129256298046 ) ) ;
#198174 = CARTESIAN_POINT ( 'NONE',  ( 18.50000000000000000, -9.499999999988842703, -74.03206939669971121 ) ) ;
#198175 = CARTESIAN_POINT ( 'NONE',  ( -16.87368910959167678, 9.961273816702552963, -146.6124930966406339 ) ) ;
#198176 = CIRCLE ( 'NONE', #169170, 4.049999999999998046 ) ;
#198177 = ORIENTED_EDGE ( 'NONE', *, *, #84449, .T. ) ;
#198178 = AXIS2_PLACEMENT_3D ( 'NONE', #16883, #96379, #124959 ) ;
#198179 = ORIENTED_EDGE ( 'NONE', *, *, #175942, .T. ) ;
#198180 = CIRCLE ( 'NONE', #69224, 4.299999999999956302 ) ;
#198181 = DIRECTION ( 'NONE',  ( 1.000000000000000000, 0.000000000000000000, 0.000000000000000000 ) ) ;
#198183 = CARTESIAN_POINT ( 'NONE',  ( 21.07199075132372101, 67.22505500089651775, -191.3095753229115701 ) ) ;
#198182 = CARTESIAN_POINT ( 'NONE',  ( 21.08134388332232234, 69.66531941949371287, -69.59892640203138114 ) ) ;
#198184 = ADVANCED_FACE ( 'NONE', ( #256766 ), #78169, .F. ) ;
#198185 = LINE ( 'NONE', #217733, #68541 ) ;
#198186 = CARTESIAN_POINT ( 'NONE',  ( -23.25000000000000000, 1.115650265596050101E-11, -29.45000000000000284 ) ) ;
#198187 = FACE_OUTER_BOUND ( 'NONE', #252709, .T. ) ;
#198188 = ADVANCED_FACE ( 'NONE', ( #187582 ), #108027, .F. ) ;
#198189 = ORIENTED_EDGE ( 'NONE', *, *, #118525, .F. ) ;
#198190 = EDGE_CURVE ( 'NONE', #95993, #240051, #214594, .T. ) ;
#198191 = CYLINDRICAL_SURFACE ( 'NONE', #93351, 0.9000000000000014655 ) ;
#198192 = ORIENTED_EDGE ( 'NONE', *, *, #82167, .F. ) ;
#198193 = DIRECTION ( 'NONE',  ( 1.000000000000000000, 0.000000000000000000, 0.000000000000000000 ) ) ;
#198194 = ADVANCED_FACE ( 'NONE', ( #104149 ), #150643, .F. ) ;
#198195 = AXIS2_PLACEMENT_3D ( 'NONE', #62772, #107016, #143589 ) ;
#198196 = ORIENTED_EDGE ( 'NONE', *, *, #248772, .F. ) ;
#198197 = CARTESIAN_POINT ( 'NONE',  ( -20.94999999999999929, 87.65000000001246860, -173.0231074845243029 ) ) ;
#198198 = VECTOR ( 'NONE', #96711, 1000.000000000000000 ) ;
#198199 = DIRECTION ( 'NONE',  ( 0.000000000000000000, 0.1350103645451904977, 0.9908441862701596881 ) ) ;
#198200 = ORIENTED_EDGE ( 'NONE', *, *, #117338, .F. ) ;
#198201 = DIRECTION ( 'NONE',  ( -0.000000000000000000, -1.000000000000000000, -6.982962677686266711E-15 ) ) ;
#198202 = ADVANCED_FACE ( 'NONE', ( #66332 ), #60461, .F. ) ;
#198203 = VERTEX_POINT ( 'NONE', #44207 ) ;
#198204 = FACE_OUTER_BOUND ( 'NONE', #161917, .T. ) ;
#198205 = DIRECTION ( 'NONE',  ( 0.000000000000000000, 1.000000000000000000, 0.000000000000000000 ) ) ;
#198206 = DIRECTION ( 'NONE',  ( 0.000000000000000000, 1.000000000000000000, 0.000000000000000000 ) ) ;
#198207 = FACE_OUTER_BOUND ( 'NONE', #14745, .T. ) ;
#198208 = CARTESIAN_POINT ( 'NONE',  ( -16.84421487269768392, 9.949999999999981526, -12.66950212244496043 ) ) ;
#198210 = CARTESIAN_POINT ( 'NONE',  ( -20.94999999999999929, 5.899999999999947065, -10.21909976465641456 ) ) ;
#198209 = DIRECTION ( 'NONE',  ( 0.000000000000000000, 0.000000000000000000, -1.000000000000000000 ) ) ;
#198211 = DIRECTION ( 'NONE',  ( 0.7071067811865474617, 0.3338907855510734324, 0.6233112732207618523 ) ) ;
#198212 = EDGE_LOOP ( 'NONE', ( #70697, #175252, #91299, #66593 ) ) ;
#198214 = CARTESIAN_POINT ( 'NONE',  ( -23.15000000000000213, 0.000000000000000000, -12.77499999999999858 ) ) ;
#198213 = DIRECTION ( 'NONE',  ( -1.000000000000000000, 0.000000000000000000, 0.000000000000000000 ) ) ;
#198215 = ORIENTED_EDGE ( 'NONE', *, *, #166934, .F. ) ;
#198217 = ORIENTED_EDGE ( 'NONE', *, *, #104764, .F. ) ;
#198216 = DIRECTION ( 'NONE',  ( -0.000000000000000000, -6.982962677686266711E-15, 1.000000000000000000 ) ) ;
#198218 = TOROIDAL_SURFACE ( 'NONE', #210685, 7.800000000000000711, 0.1000000000000000056 ) ;
#198219 = ORIENTED_EDGE ( 'NONE', *, *, #132167, .F. ) ;
#198220 = DIRECTION ( 'NONE',  ( 0.000000000000000000, -1.000000000000000000, -6.982962677686266711E-15 ) ) ;
#198221 = CARTESIAN_POINT ( 'NONE',  ( -21.00023020733502932, 1.115542391533913547E-11, -27.10913075473164824 ) ) ;
#198222 = DIRECTION ( 'NONE',  ( 0.000000000000000000, 0.1335171055202901413, 0.9910465087640860649 ) ) ;
#198223 = FACE_OUTER_BOUND ( 'NONE', #115665, .T. ) ;
#198224 = ORIENTED_EDGE ( 'NONE', *, *, #125975, .F. ) ;
#198225 = CARTESIAN_POINT ( 'NONE',  ( -23.25000000000000000, -0.1008583690875562017, -55.25043287651065782 ) ) ;
#198226 = DIRECTION ( 'NONE',  ( 0.000000000000000000, 0.000000000000000000, 1.000000000000000000 ) ) ;
#198227 = ORIENTED_EDGE ( 'NONE', *, *, #174921, .F. ) ;
#198228 = DIRECTION ( 'NONE',  ( 2.840903330521632762E-16, -0.9550021345545507412, 0.2965989261549202838 ) ) ;
#198230 = VECTOR ( 'NONE', #209901, 1000.000000000000000 ) ;
#198229 = CARTESIAN_POINT ( 'NONE',  ( 21.08134388332232234, 6.334680580517956905, 0.07581891750702302035 ) ) ;
#198231 = ORIENTED_EDGE ( 'NONE', *, *, #812, .F. ) ;
#198232 = ORIENTED_EDGE ( 'NONE', *, *, #23743, .F. ) ;
#198234 = CARTESIAN_POINT ( 'NONE',  ( 21.13461538461538325, 10.61458296203669249, -179.8499999999999943 ) ) ;
#198233 = AXIS2_PLACEMENT_3D ( 'NONE', #4541, #84037, #140189 ) ;
#198235 = AXIS2_PLACEMENT_3D ( 'NONE', #185967, #184673, #243365 ) ;
#198236 = AXIS2_PLACEMENT_3D ( 'NONE', #30958, #90892, #11365 ) ;
#198237 = EDGE_CURVE ( 'NONE', #247867, #117217, #10613, .T. ) ;
#198238 = VERTEX_POINT ( 'NONE', #144563 ) ;
#198239 = ORIENTED_EDGE ( 'NONE', *, *, #244378, .F. ) ;
#198240 = CARTESIAN_POINT ( 'NONE',  ( 16.27683809663750125, 9.350000000011137402, -176.7499999999999716 ) ) ;
#198241 = LINE ( 'NONE', #256886, #10662 ) ;
#198242 = DIRECTION ( 'NONE',  ( 0.000000000000000000, 0.9634813093406718876, 0.2677755899091333047 ) ) ;
#198243 = EDGE_CURVE ( 'NONE', #91227, #2383, #43911, .T. ) ;
#198244 = DIRECTION ( 'NONE',  ( 1.186688945009009831E-16, 1.000000000000000000, 6.982962677686266711E-15 ) ) ;
#198245 = EDGE_CURVE ( 'NONE', #73802, #149398, #189666, .T. ) ;
#198246 = EDGE_CURVE ( 'NONE', #190938, #68335, #122461, .T. ) ;
#198247 = FACE_OUTER_BOUND ( 'NONE', #163136, .T. ) ;
#198248 = CARTESIAN_POINT ( 'NONE',  ( -22.45354308602489013, 2.198879698723710744E-07, -88.74956710954123196 ) ) ;
#198249 = FACE_BOUND ( 'NONE', #44914, .T. ) ;
#198250 = ORIENTED_EDGE ( 'NONE', *, *, #209159, .F. ) ;
#198252 = CARTESIAN_POINT ( 'NONE',  ( -21.33487959338958362, 6.725558151922345296, -33.50000000000000000 ) ) ;
#198251 = LINE ( 'NONE', #178736, #45727 ) ;
#198253 = AXIS2_PLACEMENT_3D ( 'NONE', #192246, #108827, #207961 ) ;
#198254 = ORIENTED_EDGE ( 'NONE', *, *, #126329, .F. ) ;
#198258 = EDGE_LOOP ( 'NONE', ( #83118, #32081, #156685, #224914, #249999, #15883, #126134, #29716, #119567 ) ) ;
#198257 = DIRECTION ( 'NONE',  ( 1.000000000000000000, 0.000000000000000000, 0.000000000000000000 ) ) ;
#198256 =( BOUNDED_CURVE ( )  B_SPLINE_CURVE ( 3, ( #209828, #166880, #27377, #248960 ),
 .UNSPECIFIED., .F., .T. ) 
 B_SPLINE_CURVE_WITH_KNOTS ( ( 4, 4 ),
 ( 5.733388419619901200, 5.983100554402348337 ),
 .UNSPECIFIED. ) 
 CURVE ( )  GEOMETRIC_REPRESENTATION_ITEM ( )  RATIONAL_B_SPLINE_CURVE ( ( 1.000000000000000000, 0.9948104011409416580, 0.9948104011409416580, 1.000000000000000000 ) ) 
 REPRESENTATION_ITEM ( '' )  );
#198255 = FACE_OUTER_BOUND ( 'NONE', #178579, .T. ) ;
#198259 = ORIENTED_EDGE ( 'NONE', *, *, #190877, .T. ) ;
#198260 = CARTESIAN_POINT ( 'NONE',  ( 20.05000000000002913, 18.70606281991848263, -231.7096448200342138 ) ) ;
#198261 = VECTOR ( 'NONE', #119702, 1000.000000000000000 ) ;
#198262 = CARTESIAN_POINT ( 'NONE',  ( 21.05000000000000071, -0.09999993529482767429, -60.52192177890540847 ) ) ;
#198263 = DIRECTION ( 'NONE',  ( -1.000000000000000000, 0.000000000000000000, 0.000000000000000000 ) ) ;
#198264 = CARTESIAN_POINT ( 'NONE',  ( -23.15000000000000213, 4.250000000011156409, -45.75000000000000000 ) ) ;
#198265 = ORIENTED_EDGE ( 'NONE', *, *, #124144, .T. ) ;
#198266 = FACE_OUTER_BOUND ( 'NONE', #215297, .T. ) ;
#198267 = AXIS2_PLACEMENT_3D ( 'NONE', #238637, #18301, #59973 ) ;
#198268 = EDGE_CURVE ( 'NONE', #64409, #129910, #39847, .T. ) ;
#198269 = CARTESIAN_POINT ( 'NONE',  ( -22.39999999999999858, 76.10085836911147794, -215.2726746080137445 ) ) ;
#198270 = VECTOR ( 'NONE', #24446, 1000.000000000000114 ) ;
#198271 = ADVANCED_FACE ( 'NONE', ( #24663 ), #226671, .T. ) ;
#198273 = DIRECTION ( 'NONE',  ( 0.000000000000000000, 0.2128009952263242854, -0.9770955615653393878 ) ) ;
#198272 = DIRECTION ( 'NONE',  ( 0.000000000000000000, 0.000000000000000000, 1.000000000000000000 ) ) ;
#198274 = AXIS2_PLACEMENT_3D ( 'NONE', #101781, #82216, #83505 ) ;
#198276 = ORIENTED_EDGE ( 'NONE', *, *, #167983, .F. ) ;
#198275 = CARTESIAN_POINT ( 'NONE',  ( 22.47071067811865319, 0.09909245470260570621, 7.720074744498046648 ) ) ;
#198277 = PRODUCT_DEFINITION ( 'UNKNOWN', '', #123793, #183477 ) ;
#198278 = ORIENTED_EDGE ( 'NONE', *, *, #158573, .F. ) ;
#198279 = AXIS2_PLACEMENT_3D ( 'NONE', #63307, #103702, #142828 ) ;
#198280 = CARTESIAN_POINT ( 'NONE',  ( -16.94107738177415712, 44.01795756907898749, -235.2811900454759382 ) ) ;
#198281 = ORIENTED_EDGE ( 'NONE', *, *, #25183, .T. ) ;
#198282 = LINE ( 'NONE', #63916, #193613 ) ;
#198283 = EDGE_LOOP ( 'NONE', ( #188193, #126473, #25732, #41138 ) ) ;
#198284 = CIRCLE ( 'NONE', #6752, 0.1999999999999996503 ) ;
#198285 = EDGE_CURVE ( 'NONE', #115127, #252901, #242383, .T. ) ;
#198286 = PLANE ( 'NONE',  #193282 ) ;
#198288 = EDGE_CURVE ( 'NONE', #184295, #237894, #207131, .T. ) ;
#198287 = CARTESIAN_POINT ( 'NONE',  ( 22.49999999999999645, 75.89914163091330579, -114.7726746080137161 ) ) ;
#198289 = CARTESIAN_POINT ( 'NONE',  ( -23.15000000000000213, 55.39363411790988323, -234.6384634766556303 ) ) ;
#198290 = EDGE_CURVE ( 'NONE', #95570, #136069, #14725, .T. ) ;
#198292 = VERTEX_POINT ( 'NONE', #143293 ) ;
#198291 = AXIS2_PLACEMENT_3D ( 'NONE', #146663, #163694, #8476 ) ;
#198293 = DIRECTION ( 'NONE',  ( 1.000000000000000000, 0.000000000000000000, 0.000000000000000000 ) ) ;
#198294 = AXIS2_PLACEMENT_3D ( 'NONE', #92177, #73937, #133872 ) ;
#198295 = CARTESIAN_POINT ( 'NONE',  ( -16.83199318825828428, 9.930646127992318384, -54.22758518820919704 ) ) ;
#198296 = VERTEX_POINT ( 'NONE', #78172 ) ;
#198297 = ORIENTED_EDGE ( 'NONE', *, *, #218095, .F. ) ;
#198298 = VERTEX_POINT ( 'NONE', #222820 ) ;
#198299 = DIRECTION ( 'NONE',  ( 1.000000000000000000, 6.834672213024256725E-16, -4.941700349840508052E-16 ) ) ;
#198300 = EDGE_LOOP ( 'NONE', ( #192724, #222351, #254079, #59465 ) ) ;
#198302 = ORIENTED_EDGE ( 'NONE', *, *, #25183, .F. ) ;
#198301 = DIRECTION ( 'NONE',  ( -0.000000000000000000, -6.982962677686266711E-15, 1.000000000000000000 ) ) ;
#198303 = SHAPE_REPRESENTATION ( 'Snap Open Cable Crossbars 10', ( #2425 ), #210534 ) ;
#198304 = ORIENTED_EDGE ( 'NONE', *, *, #39440, .F. ) ;
#198305 = CIRCLE ( 'NONE', #156657, 0.09999999999998898659 ) ;
#198306 = AXIS2_PLACEMENT_3D ( 'NONE', #145682, #126115, #183549 ) ;
#198310 = ADVANCED_FACE ( 'NONE', ( #157782 ), #59883, .T. ) ;
#198309 = ORIENTED_EDGE ( 'NONE', *, *, #237579, .F. ) ;
#198308 = ORIENTED_EDGE ( 'NONE', *, *, #36981, .T. ) ;
#198307 = CARTESIAN_POINT ( 'NONE',  ( 23.14999999999999858, 71.18691588786198565, -47.96462524104817504 ) ) ;
#198311 = VECTOR ( 'NONE', #128810, 1000.000000000000000 ) ;
#198312 = AXIS2_PLACEMENT_3D ( 'NONE', #74853, #72259, #13570 ) ;
#198313 = ORIENTED_EDGE ( 'NONE', *, *, #29908, .T. ) ;
#198314 = DIRECTION ( 'NONE',  ( 1.000000000000000000, 2.986185139342066440E-16, -6.665775143889693760E-16 ) ) ;
#198315 = CARTESIAN_POINT ( 'NONE',  ( 21.05000000000000071, 74.83729825007388570, -95.12310748452432563 ) ) ;
#198316 = CIRCLE ( 'NONE', #73276, 0.09999999999999939493 ) ;
#198317 = CARTESIAN_POINT ( 'NONE',  ( 21.05000000000000071, 71.14953271029195037, -57.48884007552268116 ) ) ;
#198318 = VERTEX_POINT ( 'NONE', #238543 ) ;
#198319 = EDGE_CURVE ( 'NONE', #245768, #162687, #247921, .T. ) ;
#198320 = CARTESIAN_POINT ( 'NONE',  ( 20.94999999999999929, 87.48912529308798014, -105.9231074845242091 ) ) ;
#198322 = ORIENTED_EDGE ( 'NONE', *, *, #100494, .T. ) ;
#198321 = CARTESIAN_POINT ( 'NONE',  ( -21.05000000000000071, 1.115600667400684642E-11, -138.2999999999999829 ) ) ;
#198324 = ORIENTED_EDGE ( 'NONE', *, *, #72837, .F. ) ;
#198323 = CARTESIAN_POINT ( 'NONE',  ( -22.39999999999999858, 76.10000000001276987, -215.1726782920691505 ) ) ;
#198325 = CIRCLE ( 'NONE', #127608, 0.1999999999999987899 ) ;
#198326 = ORIENTED_EDGE ( 'NONE', *, *, #173643, .T. ) ;
#198327 = EDGE_CURVE ( 'NONE', #25668, #158504, #185562, .T. ) ;
#198328 = VECTOR ( 'NONE', #219633, 1000.000000000000227 ) ;
#198329 = DIRECTION ( 'NONE',  ( 1.000000000000000000, 0.000000000000000000, -0.000000000000000000 ) ) ;
#198330 = DIRECTION ( 'NONE',  ( -0.7071067811865475727, -0.7071067811865475727, 0.000000000000000000 ) ) ;
#198331 = AXIS2_PLACEMENT_3D ( 'NONE', #28877, #107068, #227019 ) ;
#198332 = EDGE_CURVE ( 'NONE', #213681, #239657, #241139, .T. ) ;
#198333 = ORIENTED_EDGE ( 'NONE', *, *, #170819, .F. ) ;
#198334 = ORIENTED_EDGE ( 'NONE', *, *, #70609, .T. ) ;
#198335 = CARTESIAN_POINT ( 'NONE',  ( 18.39999999999998082, 11.47316190337362585, -76.25000000000004263 ) ) ;
#198336 = CARTESIAN_POINT ( 'NONE',  ( 20.85000000000000142, 64.25000000001249134, -176.8069731475025321 ) ) ;
#198337 = EDGE_CURVE ( 'NONE', #157290, #53632, #140727, .T. ) ;
#198339 = ORIENTED_EDGE ( 'NONE', *, *, #118034, .T. ) ;
#198338 = VERTEX_POINT ( 'NONE', #40391 ) ;
#198340 = VERTEX_POINT ( 'NONE', #218975 ) ;
#198342 = EDGE_CURVE ( 'NONE', #215461, #21223, #1195, .T. ) ;
#198341 = CARTESIAN_POINT ( 'NONE',  ( -22.45437739390952103, 64.18196446285904244, -247.0985338222384087 ) ) ;
#198343 = ORIENTED_EDGE ( 'NONE', *, *, #168329, .F. ) ;
#198344 = ORIENTED_EDGE ( 'NONE', *, *, #211549, .F. ) ;
#198345 = DIRECTION ( 'NONE',  ( -1.000000000000000000, 1.652117596168391700E-15, 0.000000000000000000 ) ) ;
#198346 = AXIS2_PLACEMENT_3D ( 'NONE', #102411, #116877, #97268 ) ;
#198347 = ORIENTED_EDGE ( 'NONE', *, *, #166492, .T. ) ;
#198348 = DIRECTION ( 'NONE',  ( 1.000000000000000000, -3.265361837132813093E-16, -2.280189983783949500E-30 ) ) ;
#198349 = CARTESIAN_POINT ( 'NONE',  ( -21.65000000000000213, 68.75000000001232081, -157.3731074845244109 ) ) ;
#198350 = ORIENTED_EDGE ( 'NONE', *, *, #117352, .T. ) ;
#198352 = ORIENTED_EDGE ( 'NONE', *, *, #201004, .F. ) ;
#198351 = ORIENTED_EDGE ( 'NONE', *, *, #207604, .F. ) ;
#198353 = CARTESIAN_POINT ( 'NONE',  ( -18.50000000000000000, 7.128833340094563376, -233.7327013124401276 ) ) ;
#198354 = CARTESIAN_POINT ( 'NONE',  ( 19.75857864376268935, 54.57427006634497957, -228.7596887170734306 ) ) ;
#198355 = ORIENTED_EDGE ( 'NONE', *, *, #60868, .F. ) ;
#198356 = AXIS2_PLACEMENT_3D ( 'NONE', #63082, #142607, #180479 ) ;
#198357 = VECTOR ( 'NONE', #11118, 1000.000000000000000 ) ;
#198358 = ADVANCED_FACE ( 'NONE', ( #62491 ), #68882, .F. ) ;
#198359 = AXIS2_PLACEMENT_3D ( 'NONE', #154030, #195699, #34069 ) ;
#198360 = CIRCLE ( 'NONE', #185883, 0.1000000000000013933 ) ;
#198361 = EDGE_CURVE ( 'NONE', #219131, #55413, #119919, .T. ) ;
#198362 = CARTESIAN_POINT ( 'NONE',  ( -20.64999999999999858, 2.000000000011154189, -53.77537807723790309 ) ) ;
#198363 = ORIENTED_EDGE ( 'NONE', *, *, #230682, .T. ) ;
#198364 = ORIENTED_EDGE ( 'NONE', *, *, #115588, .T. ) ;
#198365 = EDGE_CURVE ( 'NONE', #73802, #168523, #23090, .T. ) ;
#198366 = DIRECTION ( 'NONE',  ( 1.000000000000000000, 0.000000000000000000, 0.000000000000000000 ) ) ;
#198367 = VERTEX_POINT ( 'NONE', #198134 ) ;
#198368 = FACE_OUTER_BOUND ( 'NONE', #36689, .T. ) ;
#198369 = DIRECTION ( 'NONE',  ( -1.000000000000000000, 0.000000000000000000, 0.000000000000000000 ) ) ;
#198370 = EDGE_LOOP ( 'NONE', ( #88752, #221202, #175155, #57885 ) ) ;
#198371 = DIRECTION ( 'NONE',  ( -0.7071067811865388020, 0.7071067811865561215, 0.000000000000000000 ) ) ;
#198372 = CARTESIAN_POINT ( 'NONE',  ( 23.15000000000000213, 85.50000000001197975, -112.9170766071766820 ) ) ;
#198374 = CARTESIAN_POINT ( 'NONE',  ( -16.82542659449980604, 9.934499891438555608, -121.2553643999738142 ) ) ;
#198373 = DIRECTION ( 'NONE',  ( -0.000000000000000000, -0.000000000000000000, -1.000000000000000000 ) ) ;
#198375 = CARTESIAN_POINT ( 'NONE',  ( 18.49999999999999645, 0.5876173420563333138, -209.1618981382189588 ) ) ;
#198376 = DIRECTION ( 'NONE',  ( 0.000000000000000000, 0.000000000000000000, -1.000000000000000000 ) ) ;
#198377 = FACE_OUTER_BOUND ( 'NONE', #249730, .T. ) ;
#198379 = EDGE_CURVE ( 'NONE', #239723, #224903, #258066, .T. ) ;
#198378 = CARTESIAN_POINT ( 'NONE',  ( -16.85939681242905763, 66.09477481408694644, -149.4831855293329284 ) ) ;
#198380 = DIRECTION ( 'NONE',  ( 3.469446951953728416E-14, -0.8660254037844309360, 0.5000000000000134337 ) ) ;
#198381 = CARTESIAN_POINT ( 'NONE',  ( -21.05000000000000071, 67.23127455305841238, -235.8551265064783991 ) ) ;
#198382 = AXIS2_PLACEMENT_3D ( 'NONE', #52823, #211929, #154544 ) ;
#198383 = EDGE_CURVE ( 'NONE', #182323, #146255, #139570, .T. ) ;
#198384 = CIRCLE ( 'NONE', #152626, 0.5999999999999968692 ) ;
#198385 = VECTOR ( 'NONE', #88573, 1000.000000000000000 ) ;
#198386 = EDGE_LOOP ( 'NONE', ( #42734, #45875, #165061 ) ) ;
#198388 = VERTEX_POINT ( 'NONE', #160325 ) ;
#198387 = ORIENTED_EDGE ( 'NONE', *, *, #119560, .T. ) ;
#198389 = AXIS2_PLACEMENT_3D ( 'NONE', #120965, #182204, #217448 ) ;
#198390 = ORIENTED_EDGE ( 'NONE', *, *, #138006, .T. ) ;
#198391 = ORIENTED_EDGE ( 'NONE', *, *, #68943, .F. ) ;
#198392 = CARTESIAN_POINT ( 'NONE',  ( 20.94999999999999929, 76.52350599684427834, -201.5928376921694678 ) ) ;
#198393 = FACE_OUTER_BOUND ( 'NONE', #241552, .T. ) ;
#198394 = EDGE_CURVE ( 'NONE', #161516, #248655, #31484, .T. ) ;
#198396 = DIRECTION ( 'NONE',  ( 0.000000000000000000, 0.000000000000000000, -1.000000000000000000 ) ) ;
#198395 = CYLINDRICAL_SURFACE ( 'NONE', #220019, 0.09999999999998002154 ) ;
#198397 = EDGE_CURVE ( 'NONE', #77018, #121003, #20807, .T. ) ;
#198398 = CARTESIAN_POINT ( 'NONE',  ( -21.08134388332232589, 75.92418108250521414, -142.8577880650422571 ) ) ;
#198399 = ORIENTED_EDGE ( 'NONE', *, *, #7862, .F. ) ;
#198400 = CARTESIAN_POINT ( 'NONE',  ( -20.93975676684922504, 10.31104185824063180, -106.0204516983106231 ) ) ;
#198401 =( LENGTH_UNIT ( ) NAMED_UNIT ( * ) SI_UNIT ( .MILLI., .METRE. ) );
#198402 = CARTESIAN_POINT ( 'NONE',  ( -23.25000000000000000, 4.350000000011156054, -112.7500000000000284 ) ) ;
#198403 = DIRECTION ( 'NONE',  ( 0.000000000000000000, 8.881784197000696176E-16, -1.000000000000000000 ) ) ;
#198404 = LINE ( 'NONE', #193, #8171 ) ;
#198405 = ORIENTED_EDGE ( 'NONE', *, *, #138827, .F. ) ;
#198406 = VECTOR ( 'NONE', #94108, 1000.000000000000000 ) ;
#198407 = CARTESIAN_POINT ( 'NONE',  ( 18.59999999999998366, 7.021664781911246322, -204.8335654018972605 ) ) ;
#198408 = DIRECTION ( 'NONE',  ( 0.000000000000000000, -0.9915357197604804940, 0.1298341882520397950 ) ) ;
#198409 = ORIENTED_EDGE ( 'NONE', *, *, #96693, .T. ) ;
#198410 = CARTESIAN_POINT ( 'NONE',  ( -18.59999999999999787, 11.65000000001115232, -40.51480577065400013 ) ) ;
#198411 = DIRECTION ( 'NONE',  ( -1.000000000000000000, 0.000000000000000000, 0.000000000000000000 ) ) ;
#198412 = DIRECTION ( 'NONE',  ( -1.000000000000000000, -6.649824375826082804E-14, -1.991473509853015959E-14 ) ) ;
#198413 = LINE ( 'NONE', #138410, #102481 ) ;
#198414 = CARTESIAN_POINT ( 'NONE',  ( -17.22767730082269466, 10.34924421246736692, -22.14242869057048324 ) ) ;
#198415 = VERTEX_POINT ( 'NONE', #122464 ) ;
#198416 = CARTESIAN_POINT ( 'NONE',  ( 23.14999999999999858, 76.00000000001165290, -69.52310748452431710 ) ) ;
#198417 = LINE ( 'NONE', #4066, #146404 ) ;
#198418 = CARTESIAN_POINT ( 'NONE',  ( -23.15000000000000213, 87.65000000001144542, -39.02310748452423894 ) ) ;
#198420 = DIRECTION ( 'NONE',  ( -0.000000000000000000, 1.000000000000000000, 6.982962677686266711E-15 ) ) ;
#198419 = CARTESIAN_POINT ( 'NONE',  ( -18.50000000000000000, 77.86671491006960366, -158.2704322382423356 ) ) ;
#198421 = DIRECTION ( 'NONE',  ( 0.000000000000000000, 1.224646799142015331E-16, 1.000000000000000000 ) ) ;
#198422 = AXIS2_PLACEMENT_3D ( 'NONE', #191790, #153967, #190502 ) ;
#198423 = DIRECTION ( 'NONE',  ( 0.000000000000000000, -0.6728971962616412394, -0.7397360091703134577 ) ) ;
#198424 = DIRECTION ( 'NONE',  ( 1.000000000000000000, -0.000000000000000000, -0.000000000000000000 ) ) ;
#198425 = CARTESIAN_POINT ( 'NONE',  ( 22.39999999999999503, 76.00000000001203659, -114.6726782920691221 ) ) ;
#198426 = AXIS2_PLACEMENT_3D ( 'NONE', #198797, #128267, #224773 ) ;
#198427 = ORIENTED_EDGE ( 'NONE', *, *, #39966, .T. ) ;
#198428 = TOROIDAL_SURFACE ( 'NONE', #219267, 11.65000000000000036, 0.1000000000000000056 ) ;
#198429 = ADVANCED_FACE ( 'NONE', ( #121205 ), #172957, .T. ) ;
#198430 = ORIENTED_EDGE ( 'NONE', *, *, #237142, .F. ) ;
#198431 = DIRECTION ( 'NONE',  ( 1.000000000000000000, 0.000000000000000000, 0.000000000000000000 ) ) ;
#198432 = VERTEX_POINT ( 'NONE', #201992 ) ;
#198433 = DIRECTION ( 'NONE',  ( -0.000000000000000000, 1.265107689135680095E-16, -1.000000000000000000 ) ) ;
#198434 = DIRECTION ( 'NONE',  ( 0.000000000000000000, -0.8700118002898359348, 0.4930308989875165082 ) ) ;
#198435 = ADVANCED_FACE ( 'NONE', ( #162891 ), #2196, .T. ) ;
#198436 = FACE_OUTER_BOUND ( 'NONE', #169222, .T. ) ;
#198437 = VECTOR ( 'NONE', #249477, 1000.000000000000000 ) ;
#198438 = ORIENTED_EDGE ( 'NONE', *, *, #113796, .T. ) ;
#198439 = DIRECTION ( 'NONE',  ( -1.000000000000000000, 0.000000000000000000, 0.000000000000000000 ) ) ;
#198440 = CIRCLE ( 'NONE', #65167, 0.6000000000000033085 ) ;
#198441 = CARTESIAN_POINT ( 'NONE',  ( -12.48127053791144903, 9.376580978055098825, -51.12694624701194357 ) ) ;
#198442 = CARTESIAN_POINT ( 'NONE',  ( -18.50211644919735576, 65.69792220476320210, -97.53355541284614105 ) ) ;
#198443 = CIRCLE ( 'NONE', #19969, 0.1000000000000000749 ) ;
#198444 = DIRECTION ( 'NONE',  ( 0.000000000000000000, 0.000000000000000000, 1.000000000000000000 ) ) ;
#198447 = EDGE_LOOP ( 'NONE', ( #200657, #123330, #100149, #112526, #248358, #55360, #16566, #212590, #84886, #52985 ) ) ;
#198446 = CARTESIAN_POINT ( 'NONE',  ( -16.87333278164157946, 9.882609784590092872, -187.8668321938465056 ) ) ;
#198445 = CIRCLE ( 'NONE', #181881, 0.3999999999999975797 ) ;
#198449 = CARTESIAN_POINT ( 'NONE',  ( -17.27223548802645325, 10.34539739140118542, -156.1336061792111991 ) ) ;
#198448 = DIRECTION ( 'NONE',  ( 0.000000000000000000, -0.8814952561688429444, 0.4721928772777349570 ) ) ;
#198450 = DIRECTION ( 'NONE',  ( 0.000000000000000000, -0.6728971962616412394, 0.7397360091703134577 ) ) ;
#198451 = CARTESIAN_POINT ( 'NONE',  ( -18.50000000000000000, 9.150000000011157653, -121.6500000000000341 ) ) ;
#198452 = VECTOR ( 'NONE', #152093, 999.9999999999998863 ) ;
#198453 = DIRECTION ( 'NONE',  ( 0.000000000000000000, -0.4930308989875324399, -0.8700118002898268310 ) ) ;
#198454 = SURFACE_STYLE_FILL_AREA ( #138455 ) ;
#198456 = VERTEX_POINT ( 'NONE', #63757 ) ;
#198455 = CIRCLE ( 'NONE', #252612, 0.1000000000000028644 ) ;
#198457 = DIRECTION ( 'NONE',  ( 1.000000000000000000, 0.000000000000000000, 0.000000000000000000 ) ) ;
#198458 = CARTESIAN_POINT ( 'NONE',  ( 23.24999999999997513, 36.02367271998545561, -235.8812521208699309 ) ) ;
#198459 = ORIENTED_EDGE ( 'NONE', *, *, #196914, .T. ) ;
#198460 = DIRECTION ( 'NONE',  ( 6.484947573744956454E-15, -0.03803313543129139412, 0.9992764785629977276 ) ) ;
#198461 = ORIENTED_EDGE ( 'NONE', *, *, #115475, .T. ) ;
#198462 = AXIS2_PLACEMENT_3D ( 'NONE', #230096, #51427, #130999 ) ;
#198463 = DIRECTION ( 'NONE',  ( 1.186688945009010077E-16, -1.000000000000000000, -0.000000000000000000 ) ) ;
#198464 = AXIS2_PLACEMENT_3D ( 'NONE', #100869, #157059, #166062 ) ;
#198465 = CIRCLE ( 'NONE', #86010, 0.1000000000000024342 ) ;
#198466 = LINE ( 'NONE', #104473, #161706 ) ;
#198467 = FACE_OUTER_BOUND ( 'NONE', #51299, .T. ) ;
#198468 = VERTEX_POINT ( 'NONE', #70213 ) ;
#198469 = VERTEX_POINT ( 'NONE', #28539 ) ;
#198470 = CARTESIAN_POINT ( 'NONE',  ( 23.14999999999999503, 14.10000000001115694, -161.8997023888606748 ) ) ;
#198471 = DIRECTION ( 'NONE',  ( 1.000000000000000000, 7.304098846218134667E-16, 0.000000000000000000 ) ) ;
#198472 = CYLINDRICAL_SURFACE ( 'NONE', #20412, 0.09999999999999939493 ) ;
#198473 = CARTESIAN_POINT ( 'NONE',  ( -18.40000000000000213, 11.47316190337362762, -79.55000000000005400 ) ) ;
#198474 = EDGE_CURVE ( 'NONE', #137392, #47866, #127594, .T. ) ;
#198475 = CIRCLE ( 'NONE', #194414, 0.09999999999999939493 ) ;
#198477 = DIRECTION ( 'NONE',  ( 0.000000000000000000, 0.000000000000000000, -1.000000000000000000 ) ) ;
#198476 = CARTESIAN_POINT ( 'NONE',  ( -18.59999999999999787, 74.83729825007360148, -61.52310748452433131 ) ) ;
#198479 = MANIFOLD_SOLID_BREP ( 'Stock-MAS-200-1', #207597 ) ;
#198478 = CARTESIAN_POINT ( 'NONE',  ( -18.52328366898031931, -9.642321089041253401, -40.21481933757005578 ) ) ;
#198480 = CARTESIAN_POINT ( 'NONE',  ( 20.09999999999999787, 9.750000000011137757, -87.85000000000003695 ) ) ;
#198481 = DIRECTION ( 'NONE',  ( 0.000000000000000000, -1.000000000000000000, 0.000000000000000000 ) ) ;
#198482 = EDGE_LOOP ( 'NONE', ( #184960, #22195, #210766, #147759 ) ) ;
#198483 = CARTESIAN_POINT ( 'NONE',  ( 20.04142135623730070, 34.40595771266846725, -235.0146864773515176 ) ) ;
#198485 = ORIENTED_EDGE ( 'NONE', *, *, #147667, .T. ) ;
#198484 = DIRECTION ( 'NONE',  ( 0.000000000000000000, 0.000000000000000000, -1.000000000000000000 ) ) ;
#198486 = SPHERICAL_SURFACE ( 'NONE', #147735, 0.1000000000000000056 ) ;
#198487 = DIRECTION ( 'NONE',  ( 0.000000000000000000, -0.4088369013363281623, 0.9126074666063771490 ) ) ;
#198489 = FACE_OUTER_BOUND ( 'NONE', #241474, .T. ) ;
#198488 = DIRECTION ( 'NONE',  ( 1.000000000000000000, 0.000000000000000000, 0.000000000000000000 ) ) ;
#198490 = EDGE_CURVE ( 'NONE', #215970, #247446, #25931, .T. ) ;
#198491 = VERTEX_POINT ( 'NONE', #186292 ) ;
#198493 = DIRECTION ( 'NONE',  ( 1.000000000000000000, -0.000000000000000000, 0.000000000000000000 ) ) ;
#198492 = CARTESIAN_POINT ( 'NONE',  ( -16.87683809663752399, 66.15000000001160174, -56.12074346632791588 ) ) ;
#198494 = CARTESIAN_POINT ( 'NONE',  ( 20.85000000000000142, -1.149570369564537842, -175.3159124845019790 ) ) ;
#198495 = FACE_OUTER_BOUND ( 'NONE', #176948, .T. ) ;
#198496 = CARTESIAN_POINT ( 'NONE',  ( 18.49999999999999645, 7.128833340094563376, -233.7327013124401276 ) ) ;
#198497 = CARTESIAN_POINT ( 'NONE',  ( -15.73854595235690468, 66.64858632091116419, -186.5427639169753888 ) ) ;
#198498 = EDGE_CURVE ( 'NONE', #52160, #217616, #118947, .T. ) ;
#198499 = ORIENTED_EDGE ( 'NONE', *, *, #93278, .F. ) ;
#198500 = CARTESIAN_POINT ( 'NONE',  ( -21.05000000000000071, 1.115600667400684642E-11, -167.4999999999999716 ) ) ;
#198501 = CIRCLE ( 'NONE', #148441, 0.09999999999999999167 ) ;
#198502 = ORIENTED_EDGE ( 'NONE', *, *, #119340, .F. ) ;
#198503 = VECTOR ( 'NONE', #174299, 1000.000000000000000 ) ;
#198504 = VECTOR ( 'NONE', #4346, 1000.000000000000000 ) ;
#198505 = CARTESIAN_POINT ( 'NONE',  ( 22.39999999999999503, 64.25000000001237765, -170.0231074845244166 ) ) ;
#198506 = ADVANCED_FACE ( 'NONE', ( #184997 ), #160474, .T. ) ;
#198507 = ORIENTED_EDGE ( 'NONE', *, *, #253126, .T. ) ;
#198508 = DIRECTION ( 'NONE',  ( 0.000000000000000000, 0.000000000000000000, -1.000000000000000000 ) ) ;
#198509 = ORIENTED_EDGE ( 'NONE', *, *, #105144, .F. ) ;
#198510 = AXIS2_PLACEMENT_3D ( 'NONE', #95390, #13293, #169838 ) ;
#198511 = DIRECTION ( 'NONE',  ( 0.000000000000000000, 1.000000000000000000, 0.000000000000000000 ) ) ;
#198512 = CARTESIAN_POINT ( 'NONE',  ( -23.25000000000000000, 1.115649040949250830E-11, -197.0999999999999659 ) ) ;
#198513 = EDGE_LOOP ( 'NONE', ( #37373, #50483, #62387 ) ) ;
#198514 = EDGE_CURVE ( 'NONE', #176027, #135423, #106247, .T. ) ;
#198515 = AXIS2_PLACEMENT_3D ( 'NONE', #31673, #194598, #192022 ) ;
#198517 = AXIS2_PLACEMENT_3D ( 'NONE', #252878, #256684, #235878 ) ;
#198516 = CARTESIAN_POINT ( 'NONE',  ( -18.50000000000000000, -9.399999999988850163, -174.3820418481726904 ) ) ;
#198518 = CARTESIAN_POINT ( 'NONE',  ( 22.60000000000000142, 0.1008583690987122083, 11.74956712348939192 ) ) ;
#198519 = AXIS2_PLACEMENT_3D ( 'NONE', #11857, #133071, #109635 ) ;
#198520 = DIRECTION ( 'NONE',  ( -1.000000000000000000, 0.000000000000000000, 0.000000000000000000 ) ) ;
#198521 = DIRECTION ( 'NONE',  ( 0.000000000000000000, 6.769652589177795712E-15, -1.000000000000000000 ) ) ;
#198522 = DIRECTION ( 'NONE',  ( 2.952720810173289605E-16, -0.9770955615653318382, -0.2128009952263588411 ) ) ;
#198523 = VERTEX_POINT ( 'NONE', #87160 ) ;
#198524 = CARTESIAN_POINT ( 'NONE',  ( 18.54999999999999716, 29.63969710739366903, -235.8648393122026334 ) ) ;
#198525 = ORIENTED_EDGE ( 'NONE', *, *, #97703, .F. ) ;
#198527 = ORIENTED_EDGE ( 'NONE', *, *, #247748, .T. ) ;
#198526 = DIRECTION ( 'NONE',  ( -1.000000000000000000, -0.000000000000000000, -0.000000000000000000 ) ) ;
#198528 = VERTEX_POINT ( 'NONE', #88430 ) ;
#198529 = DIRECTION ( 'NONE',  ( 1.000000000000000000, 0.000000000000000000, 0.000000000000000000 ) ) ;
#198530 = CARTESIAN_POINT ( 'NONE',  ( 20.94999999999999574, 1.250000000011155299, -142.0000000000000284 ) ) ;
#198531 = CARTESIAN_POINT ( 'NONE',  ( 12.24999999999999822, 66.65000000001258229, -187.0015881126993520 ) ) ;
#198532 = LINE ( 'NONE', #77293, #209657 ) ;
#198533 = FACE_OUTER_BOUND ( 'NONE', #230031, .T. ) ;
#198535 = VERTEX_POINT ( 'NONE', #165444 ) ;
#198534 = AXIS2_PLACEMENT_3D ( 'NONE', #94133, #189392, #249376 ) ;
#198536 = DIRECTION ( 'NONE',  ( 0.000000000000000000, -0.8777080977375132376, 0.4791956752371582251 ) ) ;
#198537 = CYLINDRICAL_SURFACE ( 'NONE', #56233, 0.09999999999999939493 ) ;
#198538 = VERTEX_POINT ( 'NONE', #246259 ) ;
#198539 = EDGE_CURVE ( 'NONE', #249019, #172315, #48005, .T. ) ;
#198541 = ORIENTED_EDGE ( 'NONE', *, *, #171338, .T. ) ;
#198540 = CARTESIAN_POINT ( 'NONE',  ( -22.50000000000000000, 7.128833340093095217, -233.7327013124392749 ) ) ;
#198542 = CARTESIAN_POINT ( 'NONE',  ( -23.15000000000000213, 66.26558728512915764, -222.7970849955717938 ) ) ;
#198543 = DIRECTION ( 'NONE',  ( -1.000000000000000000, 2.849773892568378313E-16, -7.728835255496647986E-17 ) ) ;
#198544 = VECTOR ( 'NONE', #34274, 1000.000000000000000 ) ;
#198545 = ORIENTED_EDGE ( 'NONE', *, *, #175901, .F. ) ;
#198546 = AXIS2_PLACEMENT_3D ( 'NONE', #73384, #53783, #176328 ) ;
#198547 = AXIS2_PLACEMENT_3D ( 'NONE', #58064, #137601, #217135 ) ;
#198548 = VECTOR ( 'NONE', #90636, 1000.000000000000000 ) ;
#198549 = EDGE_CURVE ( 'NONE', #147959, #87546, #56538, .T. ) ;
#198550 = ORIENTED_EDGE ( 'NONE', *, *, #211240, .F. ) ;
#198551 = DIRECTION ( 'NONE',  ( 0.000000000000000000, -6.938893903907222067E-15, 1.000000000000000000 ) ) ;
#198552 = LINE ( 'NONE', #19942, #180590 ) ;
#198553 = EDGE_CURVE ( 'NONE', #121939, #176943, #80927, .T. ) ;
#198554 = DIRECTION ( 'NONE',  ( 0.000000000000000000, 0.000000000000000000, 1.000000000000000000 ) ) ;
#198555 = AXIS2_PLACEMENT_3D ( 'NONE', #35864, #116661, #171537 ) ;
#198556 = EDGE_CURVE ( 'NONE', #143156, #44391, #203271, .T. ) ;
#198557 = AXIS2_PLACEMENT_3D ( 'NONE', #51847, #66308, #28508 ) ;
#198558 = AXIS2_PLACEMENT_3D ( 'NONE', #182580, #129017, #48173 ) ;
#198559 = ORIENTED_EDGE ( 'NONE', *, *, #23779, .T. ) ;
#198560 = AXIS2_PLACEMENT_3D ( 'NONE', #170388, #184751, #107787 ) ;
#198561 = VERTEX_POINT ( 'NONE', #128885 ) ;
#198562 = FACE_OUTER_BOUND ( 'NONE', #179982, .T. ) ;
#198563 = CARTESIAN_POINT ( 'NONE',  ( 18.59999999999999076, 69.55000000001187743, -93.00608031408432907 ) ) ;
#198566 = ADVANCED_FACE ( 'NONE', ( #208434 ), #135667, .T. ) ;
#198565 = ORIENTED_EDGE ( 'NONE', *, *, #118391, .T. ) ;
#198564 = DIRECTION ( 'NONE',  ( 0.000000000000000000, 0.9126074666063660468, 0.4088369013363524762 ) ) ;
#198567 = DIRECTION ( 'NONE',  ( 0.000000000000000000, 0.000000000000000000, -1.000000000000000000 ) ) ;
#198568 = DIRECTION ( 'NONE',  ( 1.000000000000000000, 3.190570557967288949E-16, 6.948722487160392945E-17 ) ) ;
#198569 = DIRECTION ( 'NONE',  ( 0.000000000000000000, -0.9999631594459056361, -0.008583690987124413183 ) ) ;
#198570 = FACE_OUTER_BOUND ( 'NONE', #42709, .T. ) ;
#198571 = CARTESIAN_POINT ( 'NONE',  ( -16.85939591225059075, 9.905226478399002943, -79.96006824646910616 ) ) ;
#198572 = EDGE_CURVE ( 'NONE', #154016, #205739, #188844, .T. ) ;
#198573 = CARTESIAN_POINT ( 'NONE',  ( -21.14999999999999858, 6.540656951701240729, 0.000000000000000000 ) ) ;
#198574 = EDGE_CURVE ( 'NONE', #14308, #90904, #250108, .T. ) ;
#198575 = CARTESIAN_POINT ( 'NONE',  ( -20.85000000000000142, -1.736705739456431807, -78.51742258762372728 ) ) ;
#198577 = ORIENTED_EDGE ( 'NONE', *, *, #244692, .T. ) ;
#198576 = DIRECTION ( 'NONE',  ( 1.000000000000000000, 0.000000000000000000, 0.000000000000000000 ) ) ;
#198578 = CIRCLE ( 'NONE', #44484, 0.1000000000000028644 ) ;
#198580 = EDGE_CURVE ( 'NONE', #99784, #129969, #127300, .T. ) ;
#198579 = CARTESIAN_POINT ( 'NONE',  ( -11.59999999999994458, 67.75000000001118394, -25.06452884076210452 ) ) ;
#198581 = ORIENTED_EDGE ( 'NONE', *, *, #94732, .F. ) ;
#198582 = ORIENTED_EDGE ( 'NONE', *, *, #128585, .F. ) ;
#198584 = ADVANCED_FACE ( 'NONE', ( #170627 ), #8990, .F. ) ;
#198583 = CARTESIAN_POINT ( 'NONE',  ( -18.40000000000000213, 85.50000000001168132, -62.60095763519382928 ) ) ;
#198585 = CARTESIAN_POINT ( 'NONE',  ( 22.47071067811864609, 68.27992525551390202, -103.1221999392269595 ) ) ;
#198586 = EDGE_CURVE ( 'NONE', #223695, #229697, #247550, .T. ) ;
#198587 = CIRCLE ( 'NONE', #236003, 11.90000000000000213 ) ;
#198588 = ORIENTED_EDGE ( 'NONE', *, *, #59422, .F. ) ;
#198589 = DIRECTION ( 'NONE',  ( 0.000000000000000000, -0.2128009952263601734, 0.9770955615653315052 ) ) ;
#198590 = CARTESIAN_POINT ( 'NONE',  ( -18.47079683080344026, 85.47166410525650804, -62.41424694353178637 ) ) ;
#198591 = AXIS2_PLACEMENT_3D ( 'NONE', #45523, #69920, #162926 ) ;
#198592 = ORIENTED_EDGE ( 'NONE', *, *, #221033, .F. ) ;
#198593 = AXIS2_PLACEMENT_3D ( 'NONE', #57101, #234472, #54557 ) ;
#198594 = CIRCLE ( 'NONE', #23847, 0.5000000000000013323 ) ;
#198595 = CARTESIAN_POINT ( 'NONE',  ( 18.49999999999999289, 65.75000000001151079, -48.17310748452439384 ) ) ;
#198596 = CARTESIAN_POINT ( 'NONE',  ( -16.93255653858138388, 66.00154854603545118, -190.9414641165347462 ) ) ;
#198597 = EDGE_LOOP ( 'NONE', ( #122063, #184871, #238743, #202290 ) ) ;
#198599 = CARTESIAN_POINT ( 'NONE',  ( -17.73285935861037288, 65.14201819622032019, -46.26454567474291935 ) ) ;
#198598 = AXIS2_PLACEMENT_3D ( 'NONE', #217883, #241338, #80945 ) ;
#198600 = EDGE_CURVE ( 'NONE', #28459, #215370, #173150, .T. ) ;
#198601 = ORIENTED_EDGE ( 'NONE', *, *, #141777, .F. ) ;
#198602 = EDGE_CURVE ( 'NONE', #189647, #20661, #74070, .T. ) ;
#198603 = FACE_OUTER_BOUND ( 'NONE', #256628, .T. ) ;
#198604 = VECTOR ( 'NONE', #63411, 1000.000000000000000 ) ;
#198606 = ORIENTED_EDGE ( 'NONE', *, *, #201806, .F. ) ;
#198605 = DIRECTION ( 'NONE',  ( 0.000000000000000000, 0.000000000000000000, 1.000000000000000000 ) ) ;
#198607 = CARTESIAN_POINT ( 'NONE',  ( -21.05000000000000071, 87.41227409416161720, -100.0231074845242318 ) ) ;
#198608 = VERTEX_POINT ( 'NONE', #15364 ) ;
#198609 = CARTESIAN_POINT ( 'NONE',  ( 23.14999999999999503, 51.24799949642838470, -230.1402408152235637 ) ) ;
#198610 = VERTEX_POINT ( 'NONE', #75350 ) ;
#198613 = EDGE_CURVE ( 'NONE', #162352, #122635, #72785, .T. ) ;
#198612 = VERTEX_POINT ( 'NONE', #255173 ) ;
#198611 = EDGE_LOOP ( 'NONE', ( #73043, #223032, #246105, #215406, #86303, #151205, #177527 ) ) ;
#198614 = CARTESIAN_POINT ( 'NONE',  ( 21.05000000000000426, 69.69981666374590645, -136.5744349168656697 ) ) ;
#198615 = ORIENTED_EDGE ( 'NONE', *, *, #38713, .T. ) ;
#198616 = FACE_OUTER_BOUND ( 'NONE', #3703, .T. ) ;
#198618 = ORIENTED_EDGE ( 'NONE', *, *, #192182, .T. ) ;
#198617 = CIRCLE ( 'NONE', #111331, 0.09999999999999939493 ) ;
#198619 = CIRCLE ( 'NONE', #219456, 0.1999999999999987899 ) ;
#198620 = AXIS2_PLACEMENT_3D ( 'NONE', #120205, #21096, #116330 ) ;
#198621 = ORIENTED_EDGE ( 'NONE', *, *, #49259, .T. ) ;
#198622 = AXIS2_PLACEMENT_3D ( 'NONE', #171052, #27678, #186726 ) ;
#198623 = DIRECTION ( 'NONE',  ( -1.000000000000000000, 0.000000000000000000, 0.000000000000000000 ) ) ;
#198624 = DIRECTION ( 'NONE',  ( 1.000000000000000000, 0.000000000000000000, 0.000000000000000000 ) ) ;
#198625 =( BOUNDED_CURVE ( )  B_SPLINE_CURVE ( 3, ( #157743, #79415, #216373, #53458 ),
 .UNSPECIFIED., .F., .F. ) 
 B_SPLINE_CURVE_WITH_KNOTS ( ( 4, 4 ),
 ( 0.3000847527772385614, 0.5517402753107881752 ),
 .UNSPECIFIED. ) 
 CURVE ( )  GEOMETRIC_REPRESENTATION_ITEM ( )  RATIONAL_B_SPLINE_CURVE ( ( 1.000000000000000000, 0.9947294176030464508, 0.9947294176030464508, 1.000000000000000000 ) ) 
 REPRESENTATION_ITEM ( '' )  );
#198627 = ORIENTED_EDGE ( 'NONE', *, *, #193369, .F. ) ;
#198626 = CARTESIAN_POINT ( 'NONE',  ( 22.39999999999999858, 67.23127455305841238, -235.8551265064783991 ) ) ;
#198628 = DIRECTION ( 'NONE',  ( -0.000000000000000000, 0.9126074666063770380, 0.4088369013363281068 ) ) ;
#198629 = ORIENTED_EDGE ( 'NONE', *, *, #132217, .F. ) ;
#198630 = VECTOR ( 'NONE', #210463, 1000.000000000000000 ) ;
#198631 = CARTESIAN_POINT ( 'NONE',  ( -18.53317502108577131, 65.67736539654967487, -130.9625116876572406 ) ) ;
#198632 = AXIS2_PLACEMENT_3D ( 'NONE', #156735, #199706, #234961 ) ;
#198633 = LINE ( 'NONE', #39603, #14792 ) ;
#198634 = DIRECTION ( 'NONE',  ( 0.7071067811865493491, -0.7071067811865456854, -4.937700262164518065E-15 ) ) ;
#198636 = ORIENTED_EDGE ( 'NONE', *, *, #115178, .F. ) ;
#198635 = EDGE_CURVE ( 'NONE', #194825, #90961, #101756, .T. ) ;
#198637 = CARTESIAN_POINT ( 'NONE',  ( -22.94999999999999929, 0.000000000000000000, 0.000000000000000000 ) ) ;
#198638 = CARTESIAN_POINT ( 'NONE',  ( -18.40904629823862848, 37.99112787675455394, -261.0419301349346028 ) ) ;
#198639 = DIRECTION ( 'NONE',  ( -1.000000000000000000, 0.000000000000000000, -0.000000000000000000 ) ) ;
#198640 = EDGE_CURVE ( 'NONE', #58809, #236908, #131434, .T. ) ;
#198641 = ORIENTED_EDGE ( 'NONE', *, *, #44587, .F. ) ;
#198642 = CARTESIAN_POINT ( 'NONE',  ( -21.05000000000000071, 87.48912529308779540, -72.52310748452423184 ) ) ;
#198643 = ORIENTED_EDGE ( 'NONE', *, *, #97982, .T. ) ;
#198644 = ORIENTED_EDGE ( 'NONE', *, *, #201677, .T. ) ;
#198645 = VECTOR ( 'NONE', #112140, 1000.000000000000000 ) ;
#198646 = CIRCLE ( 'NONE', #244615, 0.09999999999999939493 ) ;
#198647 = FACE_OUTER_BOUND ( 'NONE', #113425, .T. ) ;
#198648 = EDGE_CURVE ( 'NONE', #104317, #217495, #190145, .T. ) ;
#198649 = ORIENTED_EDGE ( 'NONE', *, *, #21518, .T. ) ;
#198650 = ORIENTED_EDGE ( 'NONE', *, *, #13943, .T. ) ;
#198651 = EDGE_CURVE ( 'NONE', #126149, #243059, #154883, .T. ) ;
#198652 = CARTESIAN_POINT ( 'NONE',  ( 23.24999999999999289, 64.35000000001249987, -177.0379132551783812 ) ) ;
#198653 = EDGE_LOOP ( 'NONE', ( #98452, #133888, #6950, #216895, #221305 ) ) ;
#198654 = EDGE_LOOP ( 'NONE', ( #249077, #156952, #225962, #151475 ) ) ;
#198655 = CARTESIAN_POINT ( 'NONE',  ( 20.04999999999999716, 8.750000000011173285, -121.3500000000000227 ) ) ;
#198656 = EDGE_CURVE ( 'NONE', #50473, #229612, #230550, .T. ) ;
#198657 = DIRECTION ( 'NONE',  ( 0.000000000000000000, 0.9770955615653313941, 0.2128009952263603677 ) ) ;
#198658 = ORIENTED_EDGE ( 'NONE', *, *, #156283, .T. ) ;
#198659 = VECTOR ( 'NONE', #95716, 1000.000000000000000 ) ;
#198660 = ORIENTED_EDGE ( 'NONE', *, *, #51549, .F. ) ;
#198661 = ORIENTED_EDGE ( 'NONE', *, *, #141803, .F. ) ;
#198662 = EDGE_CURVE ( 'NONE', #122358, #105820, #206410, .T. ) ;
#198663 = ADVANCED_FACE ( 'NONE', ( #135270 ), #89304, .T. ) ;
#198664 = TOROIDAL_SURFACE ( 'NONE', #32291, 0.2000000000000000111, 0.1000000000000000056 ) ;
#198665 = LINE ( 'NONE', #99535, #67877 ) ;
#198666 = CARTESIAN_POINT ( 'NONE',  ( 18.49351773456780634, 85.44302569515771495, -196.3377819584974588 ) ) ;
#198667 = EDGE_CURVE ( 'NONE', #255891, #151389, #68479, .T. ) ;
#198668 = DIRECTION ( 'NONE',  ( 0.000000000000000000, 0.000000000000000000, -1.000000000000000000 ) ) ;
#198669 = CARTESIAN_POINT ( 'NONE',  ( 23.14999999999999503, 11.65000000001116298, -59.98519422934606382 ) ) ;
#198670 = CIRCLE ( 'NONE', #240213, 0.1000000000000028644 ) ;
#198671 = DIRECTION ( 'NONE',  ( 1.000000000000000000, 0.000000000000000000, 0.000000000000000000 ) ) ;
#198672 = DIRECTION ( 'NONE',  ( 0.000000000000000000, 0.000000000000000000, -1.000000000000000000 ) ) ;
#198673 = AXIS2_PLACEMENT_3D ( 'NONE', #206649, #189657, #231364 ) ;
#198674 = DIRECTION ( 'NONE',  ( -1.000000000000000000, 0.000000000000000000, -6.938893903907270030E-14 ) ) ;
#198676 = CARTESIAN_POINT ( 'NONE',  ( 21.13422380239047271, 34.00421293006652235, -243.6253044407205550 ) ) ;
#198675 = DIRECTION ( 'NONE',  ( 1.000000000000000000, 0.000000000000000000, 0.000000000000000000 ) ) ;
#198678 = TOROIDAL_SURFACE ( 'NONE', #7124, 0.2000000000000000111, 0.1000000000000000056 ) ;
#198677 = FACE_OUTER_BOUND ( 'NONE', #52305, .T. ) ;
#198679 = TOROIDAL_SURFACE ( 'NONE', #215254, 11.65000000000000036, 0.1000000000000000056 ) ;
#198680 = DIRECTION ( 'NONE',  ( 4.408576920032447355E-17, -0.1350103645451876666, -0.9908441862701600211 ) ) ;
#198681 = DIRECTION ( 'NONE',  ( 2.952720810173288619E-16, 0.4088369013363239990, -0.9126074666063788143 ) ) ;
#198682 = DIRECTION ( 'NONE',  ( 1.000000000000000000, 0.000000000000000000, 0.000000000000000000 ) ) ;
#198683 = EDGE_CURVE ( 'NONE', #61341, #156062, #31098, .T. ) ;
#198684 = EDGE_CURVE ( 'NONE', #118720, #219738, #79145, .T. ) ;
#198686 = ORIENTED_EDGE ( 'NONE', *, *, #112625, .T. ) ;
#198685 = VECTOR ( 'NONE', #33873, 1000.000000000000000 ) ;
#198687 = EDGE_CURVE ( 'NONE', #52103, #172976, #22711, .T. ) ;
#198689 = ORIENTED_EDGE ( 'NONE', *, *, #150667, .T. ) ;
#198688 = DIRECTION ( 'NONE',  ( 1.000000000000000000, 2.952720810173289112E-16, -0.000000000000000000 ) ) ;
#198690 = CARTESIAN_POINT ( 'NONE',  ( 22.39999999999999858, 7.790779598384538929, -100.4000000000000341 ) ) ;
#198691 = ADVANCED_FACE ( 'NONE', ( #218659 ), #177341, .T. ) ;
#198692 = DIRECTION ( 'NONE',  ( 0.000000000000000000, 0.8660254037844419273, -0.4999999999999942824 ) ) ;
#198693 = AXIS2_PLACEMENT_3D ( 'NONE', #178513, #257968, #181071 ) ;
#198694 = CARTESIAN_POINT ( 'NONE',  ( 20.27550659511088682, 41.33268472976309482, -237.3587910501520071 ) ) ;
#198695 = EDGE_CURVE ( 'NONE', #255042, #185478, #73179, .T. ) ;
#198696 = ORIENTED_EDGE ( 'NONE', *, *, #64035, .T. ) ;
#198697 = TOROIDAL_SURFACE ( 'NONE', #86247, 12.77499999999999858, 0.1000000000000000056 ) ;
#198698 = CARTESIAN_POINT ( 'NONE',  ( -20.94999999999999929, 76.00000000001142553, -36.02310748452432421 ) ) ;
#198699 = CARTESIAN_POINT ( 'NONE',  ( -16.89318236219977010, 66.04846474213715624, -157.3782371166302880 ) ) ;
#198700 = VERTEX_POINT ( 'NONE', #98686 ) ;
#198701 = AXIS2_PLACEMENT_3D ( 'NONE', #9618, #189560, #10922 ) ;
#198702 = CARTESIAN_POINT ( 'NONE',  ( -18.50211644919735576, 10.30207779525983192, -206.4895520716782187 ) ) ;
#198703 = CARTESIAN_POINT ( 'NONE',  ( 20.94999999999999929, 72.02722222756959525, -225.1832529173024398 ) ) ;
#198704 = CARTESIAN_POINT ( 'NONE',  ( 21.14999999999999858, 47.74710514101221293, -244.5837943500090716 ) ) ;
#198705 = ADVANCED_FACE ( 'NONE', ( #101240 ), #156165, .F. ) ;
#198706 = DIRECTION ( 'NONE',  ( 0.000000000000000000, 1.000000000000000000, 0.000000000000000000 ) ) ;
#198708 = ORIENTED_EDGE ( 'NONE', *, *, #133257, .F. ) ;
#198707 = CARTESIAN_POINT ( 'NONE',  ( -23.15000000000000213, 1.115600667400684642E-11, -67.00000000000000000 ) ) ;
#198710 = ORIENTED_EDGE ( 'NONE', *, *, #245256, .F. ) ;
#198709 = CARTESIAN_POINT ( 'NONE',  ( 18.50000000000000000, -9.399999999988843058, -73.88204184817267617 ) ) ;
#198711 = CARTESIAN_POINT ( 'NONE',  ( -21.05000000000000071, 87.48912529308817909, -133.5231074845242176 ) ) ;
#198712 = DIRECTION ( 'NONE',  ( -1.000000000000000000, 0.000000000000000000, 0.000000000000000000 ) ) ;
#198713 = DIRECTION ( 'NONE',  ( 1.000000000000000000, -7.304098846218135653E-16, -5.100424963727256530E-30 ) ) ;
#198714 = EDGE_CURVE ( 'NONE', #88928, #238533, #238230, .T. ) ;
#198716 = DIRECTION ( 'NONE',  ( 0.000000000000000000, 0.000000000000000000, 1.000000000000000000 ) ) ;
#198715 = CARTESIAN_POINT ( 'NONE',  ( -16.93344882324368683, 63.05726507258725633, -213.0545985399865856 ) ) ;
#198717 = DIRECTION ( 'NONE',  ( -1.000000000000000000, -0.000000000000000000, -0.000000000000000000 ) ) ;
#198718 = CARTESIAN_POINT ( 'NONE',  ( -23.25000000000000000, 86.43238724539048690, -209.5644480942280836 ) ) ;
#198719 = DIRECTION ( 'NONE',  ( 1.000000000000000000, 8.995003028460479049E-16, -4.818376878839538654E-16 ) ) ;
#198720 = FACE_OUTER_BOUND ( 'NONE', #43711, .T. ) ;
#198721 = CIRCLE ( 'NONE', #61353, 0.09999999999999939493 ) ;
#198722 = VECTOR ( 'NONE', #171864, 999.9999999999998863 ) ;
#198723 = DIRECTION ( 'NONE',  ( -0.000000000000000000, -1.000000000000000000, 0.000000000000000000 ) ) ;
#198724 = CIRCLE ( 'NONE', #194669, 0.1000000000000013933 ) ;
#198725 = ORIENTED_EDGE ( 'NONE', *, *, #123903, .T. ) ;
#198726 = DIRECTION ( 'NONE',  ( 0.000000000000000000, 0.000000000000000000, -1.000000000000000000 ) ) ;
#198727 = VERTEX_POINT ( 'NONE', #81690 ) ;
#198728 =( BOUNDED_SURFACE ( )  B_SPLINE_SURFACE ( 3, 2, ( 
 ( #78270, #215232, #233527 ),
 ( #15781, #95282, #174874 ),
 ( #177421, #156579, #254334 ),
 ( #75732, #116146, #37901 ) ),
 .UNSPECIFIED., .F., .F., .T. ) 
 B_SPLINE_SURFACE_WITH_KNOTS ( ( 4, 4 ),
 ( 3, 3 ),
 ( 0.0006461284895273780972, 0.0007503702773985888950 ),
 ( 0.000000000000000000, 1.000000000000000000 ),
 .UNSPECIFIED. ) 
 GEOMETRIC_REPRESENTATION_ITEM ( )  RATIONAL_B_SPLINE_SURFACE ( (
 ( 1.000000000000000000, 0.7071067811865483499, 1.000000000000000000),
 ( 1.000000000000000000, 0.7076476444648895914, 1.000000000000000000),
 ( 1.000000000000000000, 0.7075727925191884760, 1.000000000000000000),
 ( 1.000000000000000000, 0.7071067811865966446, 1.000000000000000000) ) ) 
 REPRESENTATION_ITEM ( '' )  SURFACE ( )  );
#198729 = EDGE_LOOP ( 'NONE', ( #89407, #39538, #98127, #8808 ) ) ;
#198730 = ADVANCED_FACE ( 'NONE', ( #221224 ), #230619, .T. ) ;
#198731 = CARTESIAN_POINT ( 'NONE',  ( 20.94999999999999929, 1.835341550235569663, -78.55515129256303908 ) ) ;
#198732 = CARTESIAN_POINT ( 'NONE',  ( -21.14999999999994174, 76.00000000001119815, -40.17310748452479174 ) ) ;
#198733 = ORIENTED_EDGE ( 'NONE', *, *, #207197, .F. ) ;
#198734 = ORIENTED_EDGE ( 'NONE', *, *, #174582, .F. ) ;
#198735 = CIRCLE ( 'NONE', #86288, 0.1999999999999981515 ) ;
#198736 = AXIS2_PLACEMENT_3D ( 'NONE', #68267, #125660, #86504 ) ;
#198737 = EDGE_CURVE ( 'NONE', #87561, #183680, #81476, .T. ) ;
#198738 = ORIENTED_EDGE ( 'NONE', *, *, #35705, .T. ) ;
#198739 = ORIENTED_EDGE ( 'NONE', *, *, #199471, .F. ) ;
#198740 = CYLINDRICAL_SURFACE ( 'NONE', #237909, 0.1000000000000124678 ) ;
#198741 = DIRECTION ( 'NONE',  ( 1.000000000000000000, 0.000000000000000000, -0.000000000000000000 ) ) ;
#198742 = AXIS2_PLACEMENT_3D ( 'NONE', #216411, #37805, #33976 ) ;
#198743 = DIRECTION ( 'NONE',  ( 0.000000000000000000, 0.000000000000000000, -1.000000000000000000 ) ) ;
#198744 = CARTESIAN_POINT ( 'NONE',  ( 20.94999999999999929, 68.96522873961046685, -235.0783363939394235 ) ) ;
#198745 = FACE_OUTER_BOUND ( 'NONE', #123915, .T. ) ;
#198746 = CARTESIAN_POINT ( 'NONE',  ( 21.05000000000000071, 76.00000000001213607, -136.5231074845242745 ) ) ;
#198748 = ORIENTED_EDGE ( 'NONE', *, *, #129573, .T. ) ;
#198747 = DIRECTION ( 'NONE',  ( -0.000000000000000000, -1.000000000000000000, -6.982962677686266711E-15 ) ) ;
#198750 = CARTESIAN_POINT ( 'NONE',  ( 23.15000000000000213, -11.74999999998883560, -179.6499999999999773 ) ) ;
#198749 = CARTESIAN_POINT ( 'NONE',  ( -16.94107738177415712, 65.98576071487597972, -190.9731074845244336 ) ) ;
#198751 = DIRECTION ( 'NONE',  ( 0.000000000000000000, 0.9740678456249560746, -0.2262561206234139088 ) ) ;
#198752 = ORIENTED_EDGE ( 'NONE', *, *, #203372, .T. ) ;
#198753 = CARTESIAN_POINT ( 'NONE',  ( 18.59999999999999076, 18.90448995781211750, -232.7802074516171444 ) ) ;
#198754 = CARTESIAN_POINT ( 'NONE',  ( -18.59999999999999787, 64.35000000001157616, -57.37310748452439668 ) ) ;
#198755 = ORIENTED_EDGE ( 'NONE', *, *, #21398, .F. ) ;
#198757 = CARTESIAN_POINT ( 'NONE',  ( -16.93353400591626112, 65.99538760383906322, -115.5904230143189579 ) ) ;
#198756 = CARTESIAN_POINT ( 'NONE',  ( 23.14999999999999858, -8.777002227904191045, -238.5420042644097975 ) ) ;
#198758 = AXIS2_PLACEMENT_3D ( 'NONE', #160874, #42200, #121749 ) ;
#198759 = CARTESIAN_POINT ( 'NONE',  ( -22.42357213249529124, 75.90091303601045070, -110.6960398708842490 ) ) ;
#198760 = CARTESIAN_POINT ( 'NONE',  ( 20.85000000000000142, 87.75000000001215028, -139.4231074845242802 ) ) ;
#198761 = ORIENTED_EDGE ( 'NONE', *, *, #130745, .T. ) ;
#198762 = DIRECTION ( 'NONE',  ( 1.000000000000000000, 0.000000000000000000, 0.000000000000000000 ) ) ;
#198763 = DIRECTION ( 'NONE',  ( -0.000000000000000000, -0.9126074666063770380, -0.4088369013363281068 ) ) ;
#198764 = DIRECTION ( 'NONE',  ( -0.000000000000000000, 0.8660254037844383745, -0.5000000000000003331 ) ) ;
#198765 = DIRECTION ( 'NONE',  ( 1.000000000000000000, -0.000000000000000000, -0.000000000000000000 ) ) ;
#198766 = ORIENTED_EDGE ( 'NONE', *, *, #216858, .T. ) ;
#198767 = VECTOR ( 'NONE', #13748, 999.9999999999998863 ) ;
#198768 = CARTESIAN_POINT ( 'NONE',  ( 20.94999999999999574, 87.41227409416235616, -200.6231074845242688 ) ) ;
#198769 = ADVANCED_FACE ( 'NONE', ( #72136 ), #150386, .F. ) ;
#198770 = VECTOR ( 'NONE', #61890, 1000.000000000000000 ) ;
#198771 = CARTESIAN_POINT ( 'NONE',  ( -17.22767730082750504, 10.34924421247735182, -122.6424286905667458 ) ) ;
#198772 = DIRECTION ( 'NONE',  ( -0.000000000000000000, -6.982962677686266711E-15, 1.000000000000000000 ) ) ;
#198773 = SPHERICAL_SURFACE ( 'NONE', #42598, 0.1000000000000000056 ) ;
#198774 = VECTOR ( 'NONE', #132831, 1000.000000000000114 ) ;
#198776 = CARTESIAN_POINT ( 'NONE',  ( 22.57320508075688537, 11.65000000001115588, -67.00000000000004263 ) ) ;
#198775 = VECTOR ( 'NONE', #66252, 1000.000000000000000 ) ;
#198777 = CARTESIAN_POINT ( 'NONE',  ( -20.65000000000000568, 52.72272256579932304, -234.4105091754867942 ) ) ;
#198778 = AXIS2_PLACEMENT_3D ( 'NONE', #157086, #38407, #39719 ) ;
#198780 = ORIENTED_EDGE ( 'NONE', *, *, #3402, .T. ) ;
#198779 = CARTESIAN_POINT ( 'NONE',  ( 20.94999999999999574, 87.48912529308871910, -200.5231074845242745 ) ) ;
#198781 = DIRECTION ( 'NONE',  ( -2.578261006436900068E-14, 0.1350103645451904977, -0.9908441862701597991 ) ) ;
#198782 = CIRCLE ( 'NONE', #232140, 0.09999999999999939493 ) ;
#198783 = CARTESIAN_POINT ( 'NONE',  ( -16.88705144915409662, 66.05000000001187743, -90.09212888981180356 ) ) ;
#198784 = DIRECTION ( 'NONE',  ( 1.000000000000000000, 0.000000000000000000, 0.000000000000000000 ) ) ;
#198785 = CARTESIAN_POINT ( 'NONE',  ( 21.05000000000000426, 0.03486800302426329434, -94.22991413631089586 ) ) ;
#198786 = ADVANCED_FACE ( 'NONE', ( #249485 ), #33043, .F. ) ;
#198787 = VECTOR ( 'NONE', #150962, 1000.000000000000227 ) ;
#198788 = DIRECTION ( 'NONE',  ( 0.000000000000000000, -1.000000000000000000, 0.000000000000000000 ) ) ;
#198790 = ORIENTED_EDGE ( 'NONE', *, *, #53468, .T. ) ;
#198789 = CARTESIAN_POINT ( 'NONE',  ( -18.39999999999999858, -9.599999999988845900, -140.7001893912220680 ) ) ;
#198791 = FACE_OUTER_BOUND ( 'NONE', #171868, .T. ) ;
#198792 = DIRECTION ( 'NONE',  ( 0.000000000000000000, 0.000000000000000000, -1.000000000000000000 ) ) ;
#198793 = CARTESIAN_POINT ( 'NONE',  ( 23.15000000000000213, -8.663551401858002876, -177.0241011180672785 ) ) ;
#198794 = EDGE_CURVE ( 'NONE', #34074, #48521, #2379, .T. ) ;
#198795 = ORIENTED_EDGE ( 'NONE', *, *, #89592, .T. ) ;
#198796 = CARTESIAN_POINT ( 'NONE',  ( -16.97683809663752186, 9.850000000011137402, -80.40236401819653622 ) ) ;
#198797 = CARTESIAN_POINT ( 'NONE',  ( 20.94999999999999929, 9.083217576421224848, -211.4565844547649931 ) ) ;
#198798 = B_SPLINE_CURVE_WITH_KNOTS ( 'NONE', 3,
 ( #115655, #53103, #230469, #235586, #174395, #251297, #16569 ),
 .UNSPECIFIED., .F., .F.,
 ( 4, 3, 4 ),
 ( 0.000000000000000000, 3.882884552234286342E-05, 5.798605692158378976E-05 ),
 .UNSPECIFIED. ) ;
#198799 = DIRECTION ( 'NONE',  ( 0.000000000000000000, 0.1455152366551700771, 0.9893560106964479628 ) ) ;
#198800 = CARTESIAN_POINT ( 'NONE',  ( -21.04999999999994387, 64.25000000001119815, -6.123107484524794586 ) ) ;
#198802 = EDGE_CURVE ( 'NONE', #57244, #133691, #147813, .T. ) ;
#198801 = AXIS2_PLACEMENT_3D ( 'NONE', #222859, #143322, #44242 ) ;
#198803 = FACE_OUTER_BOUND ( 'NONE', #163610, .T. ) ;
#198804 = AXIS2_PLACEMENT_3D ( 'NONE', #219791, #140242, #202803 ) ;
#198805 = ORIENTED_EDGE ( 'NONE', *, *, #11707, .T. ) ;
#198806 = ORIENTED_EDGE ( 'NONE', *, *, #40418, .T. ) ;
#198807 = ADVANCED_FACE ( 'NONE', ( #24349 ), #108675, .F. ) ;
#198808 = AXIS2_PLACEMENT_3D ( 'NONE', #18432, #97938, #236190 ) ;
#198809 = DIRECTION ( 'NONE',  ( 0.000000000000000000, 0.9770955615653313941, 0.2128009952263603677 ) ) ;
#198810 = FACE_OUTER_BOUND ( 'NONE', #139848, .T. ) ;
#198811 = EDGE_CURVE ( 'NONE', #34631, #243100, #181489, .T. ) ;
#198812 = VECTOR ( 'NONE', #220407, 1000.000000000000114 ) ;
#198813 = DIRECTION ( 'NONE',  ( 0.000000000000000000, 0.000000000000000000, 1.000000000000000000 ) ) ;
#198814 = ORIENTED_EDGE ( 'NONE', *, *, #32998, .F. ) ;
#198815 = EDGE_CURVE ( 'NONE', #188235, #166644, #168704, .T. ) ;
#198816 = CARTESIAN_POINT ( 'NONE',  ( -18.40000000000000213, 64.52132590001262713, -179.2978007008650536 ) ) ;
#198817 = CARTESIAN_POINT ( 'NONE',  ( -22.59999999999999787, 75.90000000001172964, -81.17267829206912211 ) ) ;
#198818 = ADVANCED_FACE ( 'NONE', ( #48688 ), #130800, .T. ) ;
#198819 = LINE ( 'NONE', #235374, #237257 ) ;
#198820 = CARTESIAN_POINT ( 'NONE',  ( 20.95265033839679347, 10.51225083247831371, -108.0657637560299946 ) ) ;
#198821 = FACE_OUTER_BOUND ( 'NONE', #13575, .T. ) ;
#198822 = VECTOR ( 'NONE', #40319, 1000.000000000000000 ) ;
#198823 = CIRCLE ( 'NONE', #23895, 0.09999999999999441280 ) ;
#198824 = TOROIDAL_SURFACE ( 'NONE', #148968, 11.89999999999999858, 0.1000000000000000056 ) ;
#198825 = VERTEX_POINT ( 'NONE', #190818 ) ;
#198826 = CARTESIAN_POINT ( 'NONE',  ( 23.14999999999999503, 45.11960049378627247, -238.4740710069430349 ) ) ;
#198827 = ORIENTED_EDGE ( 'NONE', *, *, #178455, .T. ) ;
#198828 = CARTESIAN_POINT ( 'NONE',  ( -16.87683809663752399, 9.849999999999988987, -20.09763598180369826 ) ) ;
#198829 = EDGE_LOOP ( 'NONE', ( #169068, #95858, #37733, #104704 ) ) ;
#198830 = FACE_OUTER_BOUND ( 'NONE', #138164, .T. ) ;
#198831 = LINE ( 'NONE', #237952, #96989 ) ;
#198832 = DIRECTION ( 'NONE',  ( 0.000000000000000000, 0.9915357197604973694, -0.1298341882519105928 ) ) ;
#198833 = ORIENTED_EDGE ( 'NONE', *, *, #137034, .T. ) ;
#198834 = CARTESIAN_POINT ( 'NONE',  ( -23.25000000000000000, 70.29876110920605470, -198.0544810472949564 ) ) ;
#198835 = CARTESIAN_POINT ( 'NONE',  ( -37.88850191057539973, -8.350000000000004974, 10.52591260281975138 ) ) ;
#198836 = ORIENTED_EDGE ( 'NONE', *, *, #241478, .F. ) ;
#198837 = ADVANCED_FACE ( 'NONE', ( #189507 ), #123430, .F. ) ;
#198838 = CARTESIAN_POINT ( 'NONE',  ( -15.39126916658602795, 9.389571634557565716, -151.8176407123691547 ) ) ;
#198839 = AXIS2_PLACEMENT_3D ( 'NONE', #169267, #27186, #85797 ) ;
#198841 = ORIENTED_EDGE ( 'NONE', *, *, #79021, .F. ) ;
#198840 = DIRECTION ( 'NONE',  ( -1.000000000000000000, 0.000000000000000000, -0.000000000000000000 ) ) ;
#198842 = CIRCLE ( 'NONE', #86382, 0.1000000000000024342 ) ;
#198843 = CARTESIAN_POINT ( 'NONE',  ( -18.59999996769639097, 85.36327376984262116, -162.8416135690584667 ) ) ;
#198844 = VECTOR ( 'NONE', #119924, 1000.000000000000000 ) ;
#198845 = ORIENTED_EDGE ( 'NONE', *, *, #137099, .F. ) ;
#198846 = VECTOR ( 'NONE', #60439, 1000.000000000000114 ) ;
#198847 = CARTESIAN_POINT ( 'NONE',  ( -18.59999999999999787, -1.736705739456431807, -179.0174225876237415 ) ) ;
#198849 = EDGE_CURVE ( 'NONE', #59419, #120448, #171271, .T. ) ;
#198848 = CARTESIAN_POINT ( 'NONE',  ( 21.14999999999999858, 10.71339244341104013, -79.25000000000004263 ) ) ;
#198850 = LINE ( 'NONE', #20231, #159974 ) ;
#198851 = ORIENTED_EDGE ( 'NONE', *, *, #168166, .T. ) ;
#198852 = LINE ( 'NONE', #162317, #25874 ) ;
#198853 = CARTESIAN_POINT ( 'NONE',  ( 12.30626653967341433, 48.53477651487869338, -233.9781183031097669 ) ) ;
#198854 = CARTESIAN_POINT ( 'NONE',  ( -18.50000000000000000, 47.95459712139159336, -246.5019368548292675 ) ) ;
#198855 = CIRCLE ( 'NONE', #98862, 2.000000000000013323 ) ;
#198856 = ORIENTED_EDGE ( 'NONE', *, *, #203723, .T. ) ;
#198857 = CIRCLE ( 'NONE', #3211, 0.1000000000000028644 ) ;
#198858 = AXIS2_PLACEMENT_3D ( 'NONE', #107654, #7263, #88063 ) ;
#198859 = VECTOR ( 'NONE', #30842, 1000.000000000000114 ) ;
#198860 = EDGE_CURVE ( 'NONE', #146449, #92812, #68270, .T. ) ;
#198861 = ORIENTED_EDGE ( 'NONE', *, *, #11499, .T. ) ;
#198862 = AXIS2_PLACEMENT_3D ( 'NONE', #29693, #171775, #128773 ) ;
#198863 = EDGE_CURVE ( 'NONE', #201931, #227367, #149946, .T. ) ;
#198864 = ORIENTED_EDGE ( 'NONE', *, *, #197497, .F. ) ;
#198865 = ORIENTED_EDGE ( 'NONE', *, *, #215007, .T. ) ;
#198866 = CARTESIAN_POINT ( 'NONE',  ( -16.87304349924914604, 9.961745077968330975, -87.88906667504529935 ) ) ;
#198867 = CARTESIAN_POINT ( 'NONE',  ( 20.97462148592277131, 8.874737576461731337, -45.75464433173102918 ) ) ;
#198870 = EDGE_CURVE ( 'NONE', #17591, #39875, #133385, .T. ) ;
#198869 = VERTEX_POINT ( 'NONE', #53841 ) ;
#198868 = CARTESIAN_POINT ( 'NONE',  ( 21.05000000000000071, 64.23744694032046709, -224.5446448091673233 ) ) ;
#198871 = DIRECTION ( 'NONE',  ( 1.000000000000000000, 0.000000000000000000, 0.000000000000000000 ) ) ;
#198872 = DIRECTION ( 'NONE',  ( 0.7070776581709139474, -0.7071359030027652981, -2.453168425935592377E-14 ) ) ;
#198873 = CARTESIAN_POINT ( 'NONE',  ( -20.94999999999999929, -1.249999999988843369, -142.0000000000000284 ) ) ;
#198874 = DIRECTION ( 'NONE',  ( 0.000000000000000000, 0.000000000000000000, 1.000000000000000000 ) ) ;
#198875 = CARTESIAN_POINT ( 'NONE',  ( 22.59080734064467677, 31.82702841783752845, -238.8405965839959606 ) ) ;
#198876 = CIRCLE ( 'NONE', #32330, 0.5999999999999998668 ) ;
#198877 = ADVANCED_FACE ( 'NONE', ( #38144 ), #134632, .T. ) ;
#198878 = FACE_OUTER_BOUND ( 'NONE', #1078, .T. ) ;
#198879 = EDGE_CURVE ( 'NONE', #159940, #115264, #122662, .T. ) ;
#198881 = ORIENTED_EDGE ( 'NONE', *, *, #211335, .F. ) ;
#198880 = DIRECTION ( 'NONE',  ( 1.000000000000000000, 0.000000000000000000, -0.000000000000000000 ) ) ;
#198883 = ORIENTED_EDGE ( 'NONE', *, *, #153929, .T. ) ;
#198882 = DIRECTION ( 'NONE',  ( -1.000000000000000000, -2.885090398161910246E-16, -6.283419270304610340E-17 ) ) ;
#198884 = FACE_OUTER_BOUND ( 'NONE', #60444, .T. ) ;
#198885 = EDGE_LOOP ( 'NONE', ( #92359, #117041, #140537, #109730, #99870 ) ) ;
#198886 = ORIENTED_EDGE ( 'NONE', *, *, #108866, .T. ) ;
#198887 = CARTESIAN_POINT ( 'NONE',  ( -21.05000000000000071, 6.258316057343182415, -167.4342983896778776 ) ) ;
#198888 = CARTESIAN_POINT ( 'NONE',  ( -16.98495255085919098, 10.00556436600592924, -46.13461720622050422 ) ) ;
#198889 = VECTOR ( 'NONE', #1605, 1000.000000000000000 ) ;
#198891 = EDGE_CURVE ( 'NONE', #107789, #73651, #10234, .T. ) ;
#198890 = CARTESIAN_POINT ( 'NONE',  ( -20.64999999999999858, 2.000000000011154189, -79.72462192276213955 ) ) ;
#198892 = CARTESIAN_POINT ( 'NONE',  ( 23.25000000000000000, -11.74999999998883560, -97.40000000000004832 ) ) ;
#198893 = DIRECTION ( 'NONE',  ( -1.000000000000000000, 0.000000000000000000, 0.000000000000000000 ) ) ;
#198894 = FACE_OUTER_BOUND ( 'NONE', #226825, .T. ) ;
#198895 = CARTESIAN_POINT ( 'NONE',  ( 21.14999999999999858, 11.50215294792677767, -198.5972978622482970 ) ) ;
#198896 = ORIENTED_EDGE ( 'NONE', *, *, #16202, .T. ) ;
#198897 = ORIENTED_EDGE ( 'NONE', *, *, #79017, .T. ) ;
#198898 = CARTESIAN_POINT ( 'NONE',  ( 23.15000000000000213, 87.16808457410660083, -209.7639756239869939 ) ) ;
#198899 = AXIS2_PLACEMENT_3D ( 'NONE', #252044, #94249, #232510 ) ;
#198900 = VECTOR ( 'NONE', #63412, 1000.000000000000000 ) ;
#198901 = ORIENTED_EDGE ( 'NONE', *, *, #141005, .T. ) ;
#198903 = DIRECTION ( 'NONE',  ( -1.000000000000000000, 2.952720810173289112E-16, 2.061873921506763405E-30 ) ) ;
#198902 = CIRCLE ( 'NONE', #128188, 0.1000000000000024342 ) ;
#198904 = CARTESIAN_POINT ( 'NONE',  ( -17.11825945287481687, 51.57797924205760864, -231.8552082689889460 ) ) ;
#198905 = CARTESIAN_POINT ( 'NONE',  ( -20.64999999999999858, 71.65000000001228386, -157.6731074845243938 ) ) ;
#198906 = ORIENTED_EDGE ( 'NONE', *, *, #9693, .F. ) ;
#198907 = DIRECTION ( 'NONE',  ( 1.000000000000000000, 2.885090398161910739E-16, 6.283419270304611573E-17 ) ) ;
#198908 = ADVANCED_FACE ( 'NONE', ( #34305 ), #194667, .T. ) ;
#198909 = ORIENTED_EDGE ( 'NONE', *, *, #89846, .T. ) ;
#198910 = ADVANCED_FACE ( 'NONE', ( #113809 ), #24233, .F. ) ;
#198911 = DIRECTION ( 'NONE',  ( 1.000000000000000000, 0.000000000000000000, 0.000000000000000000 ) ) ;
#198912 = ORIENTED_EDGE ( 'NONE', *, *, #203998, .F. ) ;
#198913 = DIRECTION ( 'NONE',  ( -1.000000000000000000, 0.000000000000000000, 0.000000000000000000 ) ) ;
#198914 = CARTESIAN_POINT ( 'NONE',  ( -16.87368910959167678, 9.961273816702552963, -113.1124930966406197 ) ) ;
#198915 = AXIS2_PLACEMENT_3D ( 'NONE', #179248, #200074, #102212 ) ;
#198916 = ORIENTED_EDGE ( 'NONE', *, *, #203695, .T. ) ;
#198917 = EDGE_CURVE ( 'NONE', #241842, #169539, #218021, .T. ) ;
#198918 = DIRECTION ( 'NONE',  ( 0.000000000000000000, -1.000000000000000000, 0.000000000000000000 ) ) ;
#198920 = EDGE_LOOP ( 'NONE', ( #44545, #152920, #39235, #103072 ) ) ;
#198919 = DIRECTION ( 'NONE',  ( -1.000000000000000000, 0.000000000000000000, 0.000000000000000000 ) ) ;
#198921 = DIRECTION ( 'NONE',  ( 0.000000000000000000, -0.1332476588733448597, -0.9910827722268067408 ) ) ;
#198922 = ORIENTED_EDGE ( 'NONE', *, *, #44962, .F. ) ;
#198923 = VECTOR ( 'NONE', #156484, 1000.000000000000114 ) ;
#198924 = DIRECTION ( 'NONE',  ( 1.040834085586049673E-13, 0.7899159663865300551, 0.6132151058540831201 ) ) ;
#198925 = ORIENTED_EDGE ( 'NONE', *, *, #222121, .T. ) ;
#198926 = DIRECTION ( 'NONE',  ( 0.000000000000000000, -0.4999999999999689138, 0.8660254037844565822 ) ) ;
#198927 = DIRECTION ( 'NONE',  ( 0.000000000000000000, -1.000000000000000000, -6.982962677686266711E-15 ) ) ;
#198928 = CARTESIAN_POINT ( 'NONE',  ( 23.14999999999999147, -4.149999999999999467, 0.000000000000000000 ) ) ;
#198929 = CARTESIAN_POINT ( 'NONE',  ( -18.59999999999999787, 64.35000000001208775, -129.5083017138703667 ) ) ;
#198930 = DIRECTION ( 'NONE',  ( 1.000000000000000000, 7.304098846218134667E-16, 0.000000000000000000 ) ) ;
#198931 = ORIENTED_EDGE ( 'NONE', *, *, #230436, .F. ) ;
#198932 = DIRECTION ( 'NONE',  ( 0.000000000000000000, 0.8068669527896844551, 0.5907332058517525963 ) ) ;
#198933 = CARTESIAN_POINT ( 'NONE',  ( 21.07954763557417621, 6.329290990048651366, -100.4341240813815261 ) ) ;
#198934 = CYLINDRICAL_SURFACE ( 'NONE', #196884, 0.5000000000000004441 ) ;
#198935 = EDGE_CURVE ( 'NONE', #128091, #256608, #158122, .T. ) ;
#198936 = AXIS2_PLACEMENT_3D ( 'NONE', #65302, #185255, #2747 ) ;
#198937 = ORIENTED_EDGE ( 'NONE', *, *, #181868, .F. ) ;
#198938 = CARTESIAN_POINT ( 'NONE',  ( 21.07016717456945898, 6.176163237836302500, -199.6548974988868679 ) ) ;
#198939 = ORIENTED_EDGE ( 'NONE', *, *, #149078, .T. ) ;
#198940 = DIRECTION ( 'NONE',  ( 0.000000000000000000, 0.4088369013363345461, -0.9126074666063741514 ) ) ;
#198941 = VERTEX_POINT ( 'NONE', #73433 ) ;
#198942 = DIRECTION ( 'NONE',  ( 0.000000000000000000, 0.000000000000000000, 1.000000000000000000 ) ) ;
#198943 = DIRECTION ( 'NONE',  ( 1.000000000000000000, 0.000000000000000000, 0.000000000000000000 ) ) ;
#198944 = ORIENTED_EDGE ( 'NONE', *, *, #233630, .T. ) ;
#198947 = VERTEX_POINT ( 'NONE', #23733 ) ;
#198946 = EDGE_CURVE ( 'NONE', #22410, #193505, #152977, .T. ) ;
#198945 = DIRECTION ( 'NONE',  ( 1.000000000000000000, 7.304098846218134667E-16, 0.000000000000000000 ) ) ;
#198948 = LINE ( 'NONE', #179413, #100502 ) ;
#198949 = ORIENTED_EDGE ( 'NONE', *, *, #246657, .T. ) ;
#198950 = VECTOR ( 'NONE', #64435, 1000.000000000000000 ) ;
#198951 = CARTESIAN_POINT ( 'NONE',  ( 15.48841904831874849, 8.561580951692381092, -54.35000000000000853 ) ) ;
#198952 = ADVANCED_FACE ( 'NONE', ( #121549 ), #203618, .F. ) ;
#198953 = CARTESIAN_POINT ( 'NONE',  ( -22.50000000000000000, 7.040683814476209612, -233.6854820247115185 ) ) ;
#198954 = EDGE_LOOP ( 'NONE', ( #189270, #23866, #175601, #71812 ) ) ;
#198955 = ORIENTED_EDGE ( 'NONE', *, *, #218296, .T. ) ;
#198956 = DIRECTION ( 'NONE',  ( 1.000000000000000000, -3.265361837132813093E-16, -2.280189983783949500E-30 ) ) ;
#198958 = EDGE_CURVE ( 'NONE', #17438, #74968, #231002, .T. ) ;
#198957 = CARTESIAN_POINT ( 'NONE',  ( -18.59999999999999787, 77.16270174994990327, -95.02310748452430289 ) ) ;
#198959 = ORIENTED_EDGE ( 'NONE', *, *, #238546, .T. ) ;
#198960 = CARTESIAN_POINT ( 'NONE',  ( -23.15000000000000213, 11.65000000001115588, -54.85000000000000142 ) ) ;
#198962 = B_SPLINE_CURVE_WITH_KNOTS ( 'NONE', 3,
 ( #145493, #123379, #24295, #103780, #183358, #4686, #84180, #163796, #243306, #223737, #204179, #25569, #184625, #85486, #12435, #170255, #110217, #112801, #9841, #14997, #192337, #48962, #172816, #150640, #128511, #52805, #30722, #132354, #90648, #91943 ),
 .UNSPECIFIED., .F., .F.,
 ( 4, 2, 2, 2, 2, 2, 2, 2, 2, 2, 2, 2, 2, 2, 4 ),
 ( 0.000000000000000000, 0.0003422764154113199539, 0.0006845528308226399078, 0.001026829246233963927, 0.001369105661645287839, 0.002053658492467965585, 0.002738211323290642898, 0.003080487738701979603, 0.003422764154113315874, 0.003765040569524652145, 0.004107316984935988416, 0.004449593400347324687, 0.004791869815758660958, 0.005134146231169998097, 0.005476422646581333500 ),
 .UNSPECIFIED. ) ;
#198961 = TOROIDAL_SURFACE ( 'NONE', #15669, 1.900000000000002576, 0.1000000000000000056 ) ;
#198963 = AXIS2_PLACEMENT_3D ( 'NONE', #65938, #142876, #42513 ) ;
#198965 = ORIENTED_EDGE ( 'NONE', *, *, #96331, .T. ) ;
#198964 = CIRCLE ( 'NONE', #119903, 0.09999999999999939493 ) ;
#198966 = ORIENTED_EDGE ( 'NONE', *, *, #107064, .F. ) ;
#198967 = EDGE_CURVE ( 'NONE', #99410, #100756, #215028, .T. ) ;
#198971 = ADVANCED_FACE ( 'NONE', ( #160673 ), #114455, .T. ) ;
#198970 = EDGE_CURVE ( 'NONE', #25147, #194241, #178961, .T. ) ;
#198969 = FACE_OUTER_BOUND ( 'NONE', #97313, .T. ) ;
#198968 = VECTOR ( 'NONE', #82556, 1000.000000000000227 ) ;
#198972 = AXIS2_PLACEMENT_3D ( 'NONE', #245597, #3103, #66949 ) ;
#198973 = APPLICATION_CONTEXT ( 'automotive_design' ) ;
#198975 = ORIENTED_EDGE ( 'NONE', *, *, #30786, .F. ) ;
#198974 = DIRECTION ( 'NONE',  ( 0.000000000000000000, -0.8068669527896844551, -0.5907332058517525963 ) ) ;
#198976 = FACE_OUTER_BOUND ( 'NONE', #135781, .T. ) ;
#198977 = CARTESIAN_POINT ( 'NONE',  ( -23.15000000000000213, 67.23127455305841238, -235.8551265064783991 ) ) ;
#198978 = DIRECTION ( 'NONE',  ( -2.978066053179066272E-16, -1.000000000000000000, -8.338584948901384773E-15 ) ) ;
#198980 = CARTESIAN_POINT ( 'NONE',  ( -22.43310005002225438, 75.99436305787158119, -181.6727696116587651 ) ) ;
#198979 = CARTESIAN_POINT ( 'NONE',  ( -17.78241384945340187, 65.14442424721026725, -126.2740698120452549 ) ) ;
#198981 = CARTESIAN_POINT ( 'NONE',  ( -20.64999999999999858, 68.75000000001253397, -182.3731074845244109 ) ) ;
#198982 = DIRECTION ( 'NONE',  ( 0.000000000000000000, 0.000000000000000000, 1.000000000000000000 ) ) ;
#198983 = CIRCLE ( 'NONE', #57502, 0.09999999999999971412 ) ;
#198984 = CARTESIAN_POINT ( 'NONE',  ( 18.50000000000000355, -9.419209763398097124, -40.74776946275895284 ) ) ;
#198985 = CARTESIAN_POINT ( 'NONE',  ( 22.39999999999999503, 75.90000000001170122, -77.31388708289770761 ) ) ;
#198986 = EDGE_CURVE ( 'NONE', #161497, #123658, #2830, .T. ) ;
#198988 = EDGE_CURVE ( 'NONE', #231806, #43771, #97673, .T. ) ;
#198987 = CIRCLE ( 'NONE', #203275, 0.1000000000000028644 ) ;
#198989 = EDGE_LOOP ( 'NONE', ( #110986, #30343, #158828, #94059 ) ) ;
#198990 = AXIS2_PLACEMENT_3D ( 'NONE', #194224, #237179, #61096 ) ;
#198991 = VECTOR ( 'NONE', #239059, 1000.000000000000000 ) ;
#198993 = ORIENTED_EDGE ( 'NONE', *, *, #95635, .T. ) ;
#198992 = LINE ( 'NONE', #137716, #250045 ) ;
#198994 = CIRCLE ( 'NONE', #182452, 0.09999999999998898659 ) ;
#198995 = EDGE_LOOP ( 'NONE', ( #175530, #235076, #175750, #147129 ) ) ;
#198996 = EDGE_CURVE ( 'NONE', #97044, #254141, #75126, .T. ) ;
#198997 = CARTESIAN_POINT ( 'NONE',  ( -23.15000000000000213, 39.47455543563931002, -237.7297955216985201 ) ) ;
#198998 = ORIENTED_EDGE ( 'NONE', *, *, #129772, .T. ) ;
#198999 = LINE ( 'NONE', #79019, #221768 ) ;
#199000 = AXIS2_PLACEMENT_3D ( 'NONE', #197637, #3276, #142782 ) ;
#199001 = EDGE_CURVE ( 'NONE', #44761, #253610, #26985, .T. ) ;
#199002 = VERTEX_POINT ( 'NONE', #104488 ) ;
#199003 = CARTESIAN_POINT ( 'NONE',  ( 20.94999999999999929, 11.65000000001115943, -127.1583993101029790 ) ) ;
#199004 = EDGE_CURVE ( 'NONE', #237745, #6498, #106043, .T. ) ;
#199006 = ORIENTED_EDGE ( 'NONE', *, *, #223879, .T. ) ;
#199005 = VERTEX_POINT ( 'NONE', #244017 ) ;
#199007 = ORIENTED_EDGE ( 'NONE', *, *, #34327, .T. ) ;
#199008 = AXIS2_PLACEMENT_3D ( 'NONE', #250002, #71386, #231735 ) ;
#199009 = CIRCLE ( 'NONE', #40665, 2.000000000000000000 ) ;
#199010 = ORIENTED_EDGE ( 'NONE', *, *, #172685, .T. ) ;
#199011 = CYLINDRICAL_SURFACE ( 'NONE', #237932, 0.1000000000000028644 ) ;
#199013 = CLOSED_SHELL ( 'NONE', ( #187726, #125692, #3577, #136865, #136844, #133980, #105232, #196905, #190612, #74810, #7766, #132294, #66493, #64405, #5521, #9362, #107220, #57595, #155383, #257218, #60054, #110868, #247173, #26921, #212508, #104320, #214567, #188876, #8635, #104870, #92136, #91086, #173873, #138804, #68724, #202208, #215233, #237617, #21367, #75018, #160318, #237386, #102404, #95012, #250016, #173607, #68179, #120732, #106281, #43878, #25, #206531, #181012 ) ) ;
#199012 = CARTESIAN_POINT ( 'NONE',  ( -18.59999999999999787, -9.849999999999996092, 31.39999999999999858 ) ) ;
#199015 = EDGE_LOOP ( 'NONE', ( #207370, #211422, #130344, #23013 ) ) ;
#199014 = SPHERICAL_SURFACE ( 'NONE', #69, 0.1000000000000000056 ) ;
#199016 = CARTESIAN_POINT ( 'NONE',  ( -20.94999999999999929, 74.16465844978715438, -57.86795619196135476 ) ) ;
#199017 = EDGE_CURVE ( 'NONE', #3690, #141829, #120270, .T. ) ;
#199018 = LINE ( 'NONE', #20396, #211783 ) ;
#199020 = EDGE_LOOP ( 'NONE', ( #202819, #69151, #37886, #8856 ) ) ;
#199019 = DIRECTION ( 'NONE',  ( 0.000000000000000000, 0.2617529984165027912, 0.9651348961777158619 ) ) ;
#199021 = DIRECTION ( 'NONE',  ( 1.000000000000000000, 0.000000000000000000, 0.000000000000000000 ) ) ;
#199022 = ORIENTED_EDGE ( 'NONE', *, *, #61335, .T. ) ;
#199023 = DIRECTION ( 'NONE',  ( -3.035766082959430717E-14, -6.982962677686266711E-15, 1.000000000000000000 ) ) ;
#199025 = ORIENTED_EDGE ( 'NONE', *, *, #239227, .T. ) ;
#199024 = CARTESIAN_POINT ( 'NONE',  ( 22.39999999999999503, 1.115600667400684642E-11, -59.20922040162666633 ) ) ;
#199026 = CIRCLE ( 'NONE', #215580, 11.65000000000000036 ) ;
#199027 = CARTESIAN_POINT ( 'NONE',  ( -23.25000000000000000, 11.75000000001115552, -67.00000000000004263 ) ) ;
#199028 = CARTESIAN_POINT ( 'NONE',  ( -15.15564720441980562, 27.50042447306176285, -233.9693577020172199 ) ) ;
#199029 = CIRCLE ( 'NONE', #257234, 0.1000000000000028644 ) ;
#199030 = DIRECTION ( 'NONE',  ( -0.000000000000000000, -0.000000000000000000, -1.000000000000000000 ) ) ;
#199032 = EDGE_CURVE ( 'NONE', #220374, #55259, #161947, .T. ) ;
#199031 = ORIENTED_EDGE ( 'NONE', *, *, #105721, .T. ) ;
#199034 = CARTESIAN_POINT ( 'NONE',  ( -16.88560720703333473, 44.13352770193326080, -235.2991880424075646 ) ) ;
#199033 = DIRECTION ( 'NONE',  ( 4.408576920032447355E-17, -0.1350103645451876666, -0.9908441862701600211 ) ) ;
#199035 = CARTESIAN_POINT ( 'NONE',  ( -15.15564720441980739, 66.58929125296474183, -84.95389907868026569 ) ) ;
#199036 = AXIS2_PLACEMENT_3D ( 'NONE', #189517, #89116, #10878 ) ;
#199037 = CARTESIAN_POINT ( 'NONE',  ( 18.39999999999999858, 85.68240343348878696, -163.3662641071115047 ) ) ;
#199038 = CARTESIAN_POINT ( 'NONE',  ( -22.50000000000000000, 29.50811709945089945, -252.6450601445781103 ) ) ;
#199039 = LINE ( 'NONE', #116932, #192671 ) ;
#199040 = VERTEX_POINT ( 'NONE', #198480 ) ;
#199041 = ORIENTED_EDGE ( 'NONE', *, *, #189941, .T. ) ;
#199043 = ORIENTED_EDGE ( 'NONE', *, *, #107963, .T. ) ;
#199042 = CIRCLE ( 'NONE', #36761, 0.09999999999999108213 ) ;
#199044 = DIRECTION ( 'NONE',  ( 0.000000000000000000, 0.000000000000000000, -1.000000000000000000 ) ) ;
#199045 = VERTEX_POINT ( 'NONE', #19864 ) ;
#199046 = CARTESIAN_POINT ( 'NONE',  ( 21.14999999999999858, 76.00000000001267608, -203.5231074845243597 ) ) ;
#199047 = VERTEX_POINT ( 'NONE', #141086 ) ;
#199048 = EDGE_CURVE ( 'NONE', #61384, #90961, #220620, .T. ) ;
#199049 = DIRECTION ( 'NONE',  ( 0.000000000000000000, -0.9126074666063660468, -0.4088369013363524762 ) ) ;
#199050 = CYLINDRICAL_SURFACE ( 'NONE', #248352, 0.09999999999999609201 ) ;
#199051 = AXIS2_PLACEMENT_3D ( 'NONE', #124580, #25480, #48875 ) ;
#199052 = CIRCLE ( 'NONE', #11628, 0.1000000000000013933 ) ;
#199053 = AXIS2_PLACEMENT_3D ( 'NONE', #57935, #234017, #179215 ) ;
#199054 = EDGE_LOOP ( 'NONE', ( #107998, #48975, #75449, #18186 ) ) ;
#199055 = CARTESIAN_POINT ( 'NONE',  ( -23.15000000000000213, 1.115600667400684642E-11, -67.00000000000000000 ) ) ;
#199056 =( LENGTH_UNIT ( ) NAMED_UNIT ( * ) SI_UNIT ( .MILLI., .METRE. ) );
#199057 = ORIENTED_EDGE ( 'NONE', *, *, #247944, .T. ) ;
#199058 = ORIENTED_EDGE ( 'NONE', *, *, #139271, .F. ) ;
#199059 = ORIENTED_EDGE ( 'NONE', *, *, #5642, .T. ) ;
#199060 = CARTESIAN_POINT ( 'NONE',  ( -21.64999999999999858, 68.65000000001253966, -182.3731074845244109 ) ) ;
#199061 = LINE ( 'NONE', #20440, #236608 ) ;
#199062 = DIRECTION ( 'NONE',  ( 1.000000000000000000, 0.000000000000000000, 0.000000000000000000 ) ) ;
#199063 = CARTESIAN_POINT ( 'NONE',  ( -21.05000000000000071, 14.90151243843701856, -203.3975529985363551 ) ) ;
#199064 = CARTESIAN_POINT ( 'NONE',  ( -18.59999999999999787, 64.25000000001246292, -181.7731074845244450 ) ) ;
#199066 = DIRECTION ( 'NONE',  ( 0.000000000000000000, 0.000000000000000000, -1.000000000000000000 ) ) ;
#199065 = DIRECTION ( 'NONE',  ( 0.000000000000000000, -6.454785026890406770E-15, 1.000000000000000000 ) ) ;
#199067 = DIRECTION ( 'NONE',  ( 0.000000000000000000, 2.891205793294679805E-16, -1.000000000000000000 ) ) ;
#199069 = ORIENTED_EDGE ( 'NONE', *, *, #57577, .T. ) ;
#199068 = LINE ( 'NONE', #119547, #106542 ) ;
#199070 = CARTESIAN_POINT ( 'NONE',  ( -16.92132318717937522, 12.42386347980771077, -211.2125078751872707 ) ) ;
#199071 = ORIENTED_EDGE ( 'NONE', *, *, #12597, .T. ) ;
#199072 = DIRECTION ( 'NONE',  ( -0.7071067811865388020, 0.7071067811865561215, 0.000000000000000000 ) ) ;
#199073 = ORIENTED_EDGE ( 'NONE', *, *, #35413, .T. ) ;
#199074 = EDGE_LOOP ( 'NONE', ( #60711, #229676, #81459, #93762 ) ) ;
#199075 = CARTESIAN_POINT ( 'NONE',  ( -23.39999999999994529, 74.94272479589878344, -8.023107484524793165 ) ) ;
#199076 = AXIS2_PLACEMENT_3D ( 'NONE', #245041, #165519, #87230 ) ;
#199077 = DIRECTION ( 'NONE',  ( -2.342056488767301376E-15, -0.1350103645451904977, 0.9908441862701596881 ) ) ;
#199078 = DIRECTION ( 'NONE',  ( 0.000000000000000000, -0.9126074666062392593, -0.4088369013366354165 ) ) ;
#199079 = EDGE_LOOP ( 'NONE', ( #230088, #248012, #52545, #32857 ) ) ;
#199080 = CIRCLE ( 'NONE', #20033, 0.1000000000000012546 ) ;
#199081 = DIRECTION ( 'NONE',  ( -0.000000000000000000, -0.000000000000000000, 1.000000000000000000 ) ) ;
#199082 = ORIENTED_EDGE ( 'NONE', *, *, #21597, .F. ) ;
#199083 = ORIENTED_EDGE ( 'NONE', *, *, #107671, .T. ) ;
#199084 = CARTESIAN_POINT ( 'NONE',  ( 18.59999999999999076, 70.53171716061257257, -228.4612385850772682 ) ) ;
#199085 = EDGE_LOOP ( 'NONE', ( #114603, #900, #71649, #190028 ) ) ;
#199086 = DIRECTION ( 'NONE',  ( 1.000000000000000000, -0.000000000000000000, 0.000000000000000000 ) ) ;
#199087 = FACE_OUTER_BOUND ( 'NONE', #164635, .T. ) ;
#199088 = ORIENTED_EDGE ( 'NONE', *, *, #159089, .T. ) ;
#199089 = CARTESIAN_POINT ( 'NONE',  ( 18.49999999999999645, 76.00000000001170974, -69.52310748452431710 ) ) ;
#199090 = DIRECTION ( 'NONE',  ( 1.000000000000000000, -0.000000000000000000, -0.000000000000000000 ) ) ;
#199091 = CARTESIAN_POINT ( 'NONE',  ( 22.49999999999999645, 11.64957080755595520, -133.9000000000000057 ) ) ;
#199092 = VERTEX_POINT ( 'NONE', #79793 ) ;
#199093 = CARTESIAN_POINT ( 'NONE',  ( -23.15000000000000213, -8.999999999988846255, -76.39396912265249284 ) ) ;
#199095 = EDGE_CURVE ( 'NONE', #1409, #226915, #226871, .T. ) ;
#199094 = CARTESIAN_POINT ( 'NONE',  ( -23.15000000000000213, 2.600000000011156054, -147.2246219227621111 ) ) ;
#199096 = AXIS2_PLACEMENT_3D ( 'NONE', #135933, #53854, #134642 ) ;
#199098 = AXIS2_PLACEMENT_3D ( 'NONE', #229896, #207790, #31731 ) ;
#199097 = DIRECTION ( 'NONE',  ( -0.000000000000000000, -0.000000000000000000, 1.000000000000000000 ) ) ;
#199099 = CIRCLE ( 'NONE', #140841, 0.09999999999999063804 ) ;
#199100 = VERTEX_POINT ( 'NONE', #247878 ) ;
#199102 = VERTEX_POINT ( 'NONE', #246587 ) ;
#199101 = DIRECTION ( 'NONE',  ( -0.000000000000000000, 0.9876197685951276783, 0.1568667991644721316 ) ) ;
#199103 = ORIENTED_EDGE ( 'NONE', *, *, #90504, .T. ) ;
#199104 = CARTESIAN_POINT ( 'NONE',  ( 21.03675099975491136, 67.12481996722722499, -124.1975653477462913 ) ) ;
#199105 = CARTESIAN_POINT ( 'NONE',  ( -23.25000000000000000, 0.000000000000000000, -12.77499999999999858 ) ) ;
#199106 = CARTESIAN_POINT ( 'NONE',  ( -20.54999999999999361, 11.65000000001115232, -188.8499999999999659 ) ) ;
#199107 = LINE ( 'NONE', #174466, #4963 ) ;
#199108 = DIRECTION ( 'NONE',  ( 0.000000000000000000, 6.982962677686266711E-15, -1.000000000000000000 ) ) ;
#199109 = EDGE_CURVE ( 'NONE', #102935, #245138, #164348, .T. ) ;
#199110 = ADVANCED_FACE ( 'NONE', ( #90072 ), #105773, .T. ) ;
#199111 = ORIENTED_EDGE ( 'NONE', *, *, #121948, .F. ) ;
#199112 = CARTESIAN_POINT ( 'NONE',  ( -16.92570016628985385, 63.08493209837725146, -213.0969949883626100 ) ) ;
#199113 = DIRECTION ( 'NONE',  ( -0.7071067811865463515, 0.7071067811865487940, -0.000000000000000000 ) ) ;
#199114 = AXIS2_PLACEMENT_3D ( 'NONE', #224753, #129527, #29185 ) ;
#199115 = CARTESIAN_POINT ( 'NONE',  ( -18.43634282235113275, 77.26728940060307593, -241.9658523025645707 ) ) ;
#199116 = DIRECTION ( 'NONE',  ( 1.000000000000000000, -0.000000000000000000, -0.000000000000000000 ) ) ;
#199117 = AXIS2_PLACEMENT_3D ( 'NONE', #150436, #188254, #109993 ) ;
#199118 = FACE_OUTER_BOUND ( 'NONE', #257110, .T. ) ;
#199119 = AXIS2_PLACEMENT_3D ( 'NONE', #220183, #97633, #195508 ) ;
#199120 = ORIENTED_EDGE ( 'NONE', *, *, #219245, .F. ) ;
#199121 = EDGE_LOOP ( 'NONE', ( #202065, #67241 ) ) ;
#199122 = CARTESIAN_POINT ( 'NONE',  ( 20.94999999999999929, 67.22371710471902873, -48.27310748452438105 ) ) ;
#199123 = CARTESIAN_POINT ( 'NONE',  ( -18.50000000000000000, 47.93499546395150190, -254.9093547331817717 ) ) ;
#199125 = EDGE_CURVE ( 'NONE', #86736, #1482, #147778, .T. ) ;
#199124 = DIRECTION ( 'NONE',  ( -0.000000000000000000, 1.000000000000000000, 6.982962677686267499E-15 ) ) ;
#199126 = CARTESIAN_POINT ( 'NONE',  ( -23.39999999999994529, 64.35000000001120668, -3.023107484524792277 ) ) ;
#199127 = DIRECTION ( 'NONE',  ( 0.000000000000000000, 0.000000000000000000, 1.000000000000000000 ) ) ;
#199128 = EDGE_CURVE ( 'NONE', #95790, #49183, #67956, .T. ) ;
#199129 = ORIENTED_EDGE ( 'NONE', *, *, #231093, .T. ) ;
#199130 = DIRECTION ( 'NONE',  ( -3.265361837132813093E-16, 1.000000000000000000, 0.000000000000000000 ) ) ;
#199131 = ADVANCED_FACE ( 'NONE', ( #245322 ), #50937, .T. ) ;
#199132 = FACE_OUTER_BOUND ( 'NONE', #224325, .T. ) ;
#199133 = CARTESIAN_POINT ( 'NONE',  ( -23.15000000000000213, 2.000000000011154189, -79.72462192276213955 ) ) ;
#199134 = EDGE_CURVE ( 'NONE', #88637, #55402, #47088, .T. ) ;
#199135 = CARTESIAN_POINT ( 'NONE',  ( 21.15000000000005542, 64.35000000001120668, -3.123107484524795474 ) ) ;
#199136 = CIRCLE ( 'NONE', #169961, 0.09999999999999062417 ) ;
#199137 = VECTOR ( 'NONE', #59080, 1000.000000000000000 ) ;
#199138 = AXIS2_PLACEMENT_3D ( 'NONE', #174508, #97441, #257775 ) ;
#199139 = ADVANCED_FACE ( 'NONE', ( #127941 ), #208770, .F. ) ;
#199140 = ORIENTED_EDGE ( 'NONE', *, *, #1754, .T. ) ;
#199141 = CARTESIAN_POINT ( 'NONE',  ( 18.49999999999999289, 7.021664781900089913, -37.33356540189728889 ) ) ;
#199142 = ORIENTED_EDGE ( 'NONE', *, *, #31124, .T. ) ;
#199143 = CARTESIAN_POINT ( 'NONE',  ( -18.50000000000000000, 77.83534155023700407, -191.9679561919613491 ) ) ;
#199144 = CARTESIAN_POINT ( 'NONE',  ( 21.14999999999999858, 69.45934304831114048, -170.0231074845243882 ) ) ;
#199145 = AXIS2_PLACEMENT_3D ( 'NONE', #225740, #87518, #62839 ) ;
#199146 = CARTESIAN_POINT ( 'NONE',  ( 18.49999999999998934, 64.04577702392042227, -222.1950530992138226 ) ) ;
#199147 = CARTESIAN_POINT ( 'NONE',  ( 18.50016250449482413, 65.70233904877102304, -64.04874109119650427 ) ) ;
#199148 = DIRECTION ( 'NONE',  ( 0.000000000000000000, -0.000000000000000000, -1.000000000000000000 ) ) ;
#199149 = DIRECTION ( 'NONE',  ( 0.000000000000000000, 0.000000000000000000, -1.000000000000000000 ) ) ;
#199150 = DIRECTION ( 'NONE',  ( 0.000000000000000000, -0.9998779222360104635, -0.01562499999996343723 ) ) ;
#199151 = ADVANCED_FACE ( 'NONE', ( #28886 ), #149140, .T. ) ;
#199152 = CYLINDRICAL_SURFACE ( 'NONE', #224659, 0.1000000000000001443 ) ;
#199153 = CARTESIAN_POINT ( 'NONE',  ( 21.14999999999999858, 1.115600667400684642E-11, -112.6500000000000341 ) ) ;
#199154 = DIRECTION ( 'NONE',  ( 0.000000000000000000, 0.000000000000000000, -1.000000000000000000 ) ) ;
#199155 = CARTESIAN_POINT ( 'NONE',  ( -18.50000000000000000, 65.70729864261058140, -164.5657455973725121 ) ) ;
#199156 = VECTOR ( 'NONE', #20970, 1000.000000000000000 ) ;
#199157 = AXIS2_PLACEMENT_3D ( 'NONE', #149041, #68205, #69507 ) ;
#199158 = AXIS2_PLACEMENT_3D ( 'NONE', #228736, #246983, #127047 ) ;
#199159 = FACE_OUTER_BOUND ( 'NONE', #124607, .T. ) ;
#199160 = CARTESIAN_POINT ( 'NONE',  ( 20.94999999999999929, 9.863005973831429074, -220.4411654715779321 ) ) ;
#199161 = AXIS2_PLACEMENT_3D ( 'NONE', #28881, #31436, #227023 ) ;
#199162 = VERTEX_POINT ( 'NONE', #9269 ) ;
#199163 = CARTESIAN_POINT ( 'NONE',  ( 21.05000000000000071, 6.540656951701244282, -0.1000000000000009354 ) ) ;
#199164 = CARTESIAN_POINT ( 'NONE',  ( 23.24999999999999289, 69.45000000001222418, -148.6731074845243938 ) ) ;
#199165 = CARTESIAN_POINT ( 'NONE',  ( 20.59588692710267921, 10.36872342118021528, -41.13908109451047324 ) ) ;
#199166 = ORIENTED_EDGE ( 'NONE', *, *, #132277, .F. ) ;
#199167 = FACE_OUTER_BOUND ( 'NONE', #40521, .T. ) ;
#199168 = AXIS2_PLACEMENT_3D ( 'NONE', #60240, #138475, #61540 ) ;
#199169 = DIRECTION ( 'NONE',  ( 0.000000000000000000, -0.8814952561688476074, 0.4721928772777262417 ) ) ;
#199170 = EDGE_LOOP ( 'NONE', ( #134474, #228686, #40345, #95381 ) ) ;
#199171 = CARTESIAN_POINT ( 'NONE',  ( -23.25000000000000355, 9.950000000011138823, -76.25000000000004263 ) ) ;
#199172 = FACE_OUTER_BOUND ( 'NONE', #63554, .T. ) ;
#199173 = CIRCLE ( 'NONE', #128440, 0.5999999999999894307 ) ;
#199174 = ORIENTED_EDGE ( 'NONE', *, *, #198667, .T. ) ;
#199175 = CIRCLE ( 'NONE', #186723, 0.09999999999998898659 ) ;
#199176 = EDGE_CURVE ( 'NONE', #163070, #248091, #239346, .T. ) ;
#199177 = VECTOR ( 'NONE', #171177, 1000.000000000000000 ) ;
#199179 = EDGE_CURVE ( 'NONE', #146352, #89391, #71832, .T. ) ;
#199178 = AXIS2_PLACEMENT_3D ( 'NONE', #74580, #231070, #53688 ) ;
#199180 = AXIS2_PLACEMENT_3D ( 'NONE', #99261, #164402, #24909 ) ;
#199182 = VERTEX_POINT ( 'NONE', #87503 ) ;
#199181 = AXIS2_PLACEMENT_3D ( 'NONE', #86512, #227335, #145221 ) ;
#199183 = DIRECTION ( 'NONE',  ( 0.000000000000000000, 1.000000000000000000, 0.000000000000000000 ) ) ;
#199184 = VERTEX_POINT ( 'NONE', #228329 ) ;
#199185 = EDGE_CURVE ( 'NONE', #202583, #239004, #1995, .T. ) ;
#199187 = EDGE_CURVE ( 'NONE', #169719, #148485, #101948, .T. ) ;
#199186 = CARTESIAN_POINT ( 'NONE',  ( 22.57320508075687115, 64.25000000001237765, -170.0231074845244166 ) ) ;
#199188 = CARTESIAN_POINT ( 'NONE',  ( 13.99999999999999822, 9.850000000011137402, -50.24999999999999289 ) ) ;
#199190 = LINE ( 'NONE', #196608, #249339 ) ;
#199189 = PRODUCT_DEFINITION_CONTEXT ( 'detailed design', #229068, 'design' ) ;
#199191 = LINE ( 'NONE', #120959, #246063 ) ;
#199192 = CARTESIAN_POINT ( 'NONE',  ( 20.94999999999999929, 0.6656436123793473270, -212.6810495496487476 ) ) ;
#199193 = FACE_OUTER_BOUND ( 'NONE', #210311, .T. ) ;
#199194 = EDGE_CURVE ( 'NONE', #33727, #14870, #137428, .T. ) ;
#199195 = DIRECTION ( 'NONE',  ( 2.827886303505248766E-16, 0.9667078373770112698, 0.2558827019434132821 ) ) ;
#199196 = CYLINDRICAL_SURFACE ( 'NONE', #95567, 0.09999999999999543976 ) ;
#199198 = ORIENTED_EDGE ( 'NONE', *, *, #57117, .F. ) ;
#199197 = CARTESIAN_POINT ( 'NONE',  ( 18.36493879433392706, 86.98067545911243315, -199.3289539518750644 ) ) ;
#199199 = ORIENTED_EDGE ( 'NONE', *, *, #183415, .T. ) ;
#199201 = DIRECTION ( 'NONE',  ( 0.000000000000000000, 0.000000000000000000, -1.000000000000000000 ) ) ;
#199200 = CARTESIAN_POINT ( 'NONE',  ( 18.54286124688535153, 38.05691696594434603, -261.2177481181072949 ) ) ;
#199204 = ORIENTED_EDGE ( 'NONE', *, *, #183299, .T. ) ;
#199203 = CARTESIAN_POINT ( 'NONE',  ( -16.96982749440685367, 61.06363243814870145, -220.5835025252905268 ) ) ;
#199202 = CARTESIAN_POINT ( 'NONE',  ( 21.05000000000000071, 65.27628289530507288, -191.3731074845244393 ) ) ;
#199205 = EDGE_CURVE ( 'NONE', #38071, #4663, #35296, .T. ) ;
#199206 = ORIENTED_EDGE ( 'NONE', *, *, #47715, .T. ) ;
#199207 = CARTESIAN_POINT ( 'NONE',  ( -16.89268316805465986, 66.04827818677006235, -149.1673550059788909 ) ) ;
#199209 = EDGE_CURVE ( 'NONE', #257284, #41279, #143481, .T. ) ;
#199208 = VECTOR ( 'NONE', #155028, 1000.000000000000000 ) ;
#199210 = CARTESIAN_POINT ( 'NONE',  ( 20.87631937322887410, 10.47149503677486138, -175.0797458745818176 ) ) ;
#199211 = CIRCLE ( 'NONE', #207787, 0.1000000000000028644 ) ;
#199213 = ADVANCED_FACE ( 'NONE', ( #155238 ), #14436, .T. ) ;
#199212 = LINE ( 'NONE', #36299, #171439 ) ;
#199214 = CYLINDRICAL_SURFACE ( 'NONE', #155999, 11.79999999999999538 ) ;
#199215 = CARTESIAN_POINT ( 'NONE',  ( -6.100000000000012079, -11.75000000000000000, -15.00000000000000355 ) ) ;
#199216 = DIRECTION ( 'NONE',  ( 1.000000000000000000, -0.000000000000000000, -0.000000000000000000 ) ) ;
#199217 = CARTESIAN_POINT ( 'NONE',  ( -18.59999999999999787, -1.736257131586239844, -145.5686523290175387 ) ) ;
#199218 = AXIS2_PLACEMENT_3D ( 'NONE', #56943, #136492, #239476 ) ;
#199219 = EDGE_CURVE ( 'NONE', #218429, #9515, #254278, .T. ) ;
#199220 = AXIS2_PLACEMENT_3D ( 'NONE', #104718, #245566, #126897 ) ;
#199221 = CARTESIAN_POINT ( 'NONE',  ( -22.50000000000000000, 55.98745301258804119, -232.8057040749261262 ) ) ;
#199222 = ORIENTED_EDGE ( 'NONE', *, *, #164989, .T. ) ;
#199223 = ORIENTED_EDGE ( 'NONE', *, *, #89503, .F. ) ;
#199224 = DIRECTION ( 'NONE',  ( 0.000000000000000000, -0.2617529984165036239, -0.9651348961777156399 ) ) ;
#199225 = EDGE_CURVE ( 'NONE', #231640, #116304, #81115, .T. ) ;
#199226 = ORIENTED_EDGE ( 'NONE', *, *, #159601, .T. ) ;
#199227 = FACE_OUTER_BOUND ( 'NONE', #148296, .T. ) ;
#199228 = EDGE_LOOP ( 'NONE', ( #3622, #157171, #253619, #33068 ) ) ;
#199229 = CARTESIAN_POINT ( 'NONE',  ( -20.54999999999999716, 7.150000000011155876, -79.35000000000005116 ) ) ;
#199230 = AXIS2_PLACEMENT_3D ( 'NONE', #172137, #50834, #147395 ) ;
#199231 = EDGE_CURVE ( 'NONE', #37076, #34877, #15724, .T. ) ;
#199232 = DIRECTION ( 'NONE',  ( 0.000000000000000000, -0.000000000000000000, -1.000000000000000000 ) ) ;
#199233 = DIRECTION ( 'NONE',  ( 0.000000000000000000, -0.4721928772776434191, -0.8814952561688919053 ) ) ;
#199234 = CARTESIAN_POINT ( 'NONE',  ( 23.24999999999999645, 67.23127455305841238, -235.8551265064783991 ) ) ;
#199235 = EDGE_CURVE ( 'NONE', #180226, #28001, #135620, .T. ) ;
#199236 = CARTESIAN_POINT ( 'NONE',  ( 22.39999999999999503, 11.65000000001116298, -66.90000000000004832 ) ) ;
#199237 = EDGE_LOOP ( 'NONE', ( #174972, #59656, #137632 ) ) ;
#199238 = EDGE_CURVE ( 'NONE', #173345, #182680, #256037, .T. ) ;
#199239 = VECTOR ( 'NONE', #79997, 1000.000000000000114 ) ;
#199240 = DIRECTION ( 'NONE',  ( 0.000000000000000000, -0.9908441862701420355, -0.1350103645453197554 ) ) ;
#199241 = DIRECTION ( 'NONE',  ( 1.000000000000000000, 0.000000000000000000, 0.000000000000000000 ) ) ;
#199242 = AXIS2_PLACEMENT_3D ( 'NONE', #29471, #110242, #145515 ) ;
#199244 = CARTESIAN_POINT ( 'NONE',  ( -20.94999999999999929, 68.48451787451661232, -224.2224406095231757 ) ) ;
#199243 = AXIS2_PLACEMENT_3D ( 'NONE', #17256, #57634, #95487 ) ;
#199245 = CARTESIAN_POINT ( 'NONE',  ( -21.14999999999999858, -0.1008583690875562017, -55.25043287651065782 ) ) ;
#199246 = CIRCLE ( 'NONE', #153493, 0.6000000000000187406 ) ;
#199247 = CARTESIAN_POINT ( 'NONE',  ( -23.15000000000000213, 47.91013932883114990, -242.3192343197862044 ) ) ;
#199248 = ORIENTED_EDGE ( 'NONE', *, *, #147647, .F. ) ;
#199249 = DIRECTION ( 'NONE',  ( -1.000000000000000000, -0.000000000000000000, 0.000000000000000000 ) ) ;
#199250 = ORIENTED_EDGE ( 'NONE', *, *, #175765, .T. ) ;
#199253 = ORIENTED_EDGE ( 'NONE', *, *, #119450, .T. ) ;
#199252 = CARTESIAN_POINT ( 'NONE',  ( -18.59999999999999787, 74.83729825007431202, -161.9231074845243654 ) ) ;
#199251 = CARTESIAN_POINT ( 'NONE',  ( -18.59999999999999787, -26.43935341558978891, -152.1415086075074896 ) ) ;
#199254 = VECTOR ( 'NONE', #136738, 1000.000000000000000 ) ;
#199255 = DIRECTION ( 'NONE',  ( 0.000000000000000000, -0.9908441862701600211, -0.1350103645451876666 ) ) ;
#199256 = CARTESIAN_POINT ( 'NONE',  ( -23.15000000000000213, 36.65892442174472876, -249.5511627012454596 ) ) ;
#199257 = EDGE_LOOP ( 'NONE', ( #27087, #250795, #254480, #4400 ) ) ;
#199258 = CARTESIAN_POINT ( 'NONE',  ( 18.50000000000000355, 85.42107434499909857, -129.6986354250934710 ) ) ;
#199259 = CARTESIAN_POINT ( 'NONE',  ( -16.93262454970419384, 10.00202046794151478, -54.42707622623731112 ) ) ;
#199260 = CARTESIAN_POINT ( 'NONE',  ( -22.42253884134832020, -3.139326375914578193, -228.2301371206982026 ) ) ;
#199262 = EDGE_LOOP ( 'NONE', ( #142585, #199444 ) ) ;
#199261 = CARTESIAN_POINT ( 'NONE',  ( -21.14999999999994174, 64.25000000001119815, -51.02310748452479316 ) ) ;
#199263 = DIRECTION ( 'NONE',  ( 1.000000000000000000, -0.000000000000000000, 0.000000000000000000 ) ) ;
#199264 = VERTEX_POINT ( 'NONE', #74420 ) ;
#199265 = FACE_OUTER_BOUND ( 'NONE', #231142, .T. ) ;
#199266 = CARTESIAN_POINT ( 'NONE',  ( 22.00411653962174796, 60.20480020221229012, -234.0521012187997769 ) ) ;
#199267 = DIRECTION ( 'NONE',  ( -2.081668171172242982E-13, -0.7092521942343974484, -0.7049548389604062271 ) ) ;
#199268 = ORIENTED_EDGE ( 'NONE', *, *, #20852, .T. ) ;
#199269 = LINE ( 'NONE', #197966, #125869 ) ;
#199270 = ORIENTED_EDGE ( 'NONE', *, *, #123303, .F. ) ;
#199271 = CARTESIAN_POINT ( 'NONE',  ( -20.94999999999999929, 1.115600667400684642E-11, -100.5000000000000426 ) ) ;
#199272 = DIRECTION ( 'NONE',  ( 0.000000000000000000, -1.000000000000000000, 0.000000000000000000 ) ) ;
#199273 = CARTESIAN_POINT ( 'NONE',  ( 20.99780126800925473, 36.04544038259444250, -236.0569647481119091 ) ) ;
#199274 = ORIENTED_EDGE ( 'NONE', *, *, #183145, .F. ) ;
#199275 = CARTESIAN_POINT ( 'NONE',  ( 21.05000000000000071, 22.91252772851732189, -230.0222229922490271 ) ) ;
#199276 = CARTESIAN_POINT ( 'NONE',  ( 20.94999999999999574, 62.00000000001190870, -97.59601495414186445 ) ) ;
#199277 = EDGE_CURVE ( 'NONE', #102375, #134983, #201943, .T. ) ;
#199278 = DIRECTION ( 'NONE',  ( 0.7071067811865474617, 0.7071067811865474617, 2.044391222244499837E-16 ) ) ;
#199279 = EDGE_LOOP ( 'NONE', ( #27485, #168417, #41234, #86221 ) ) ;
#199280 = TOROIDAL_SURFACE ( 'NONE', #240971, 0.2000000000000000111, 0.1000000000000000056 ) ;
#199282 = CIRCLE ( 'NONE', #95223, 0.09999999999999749367 ) ;
#199281 = CARTESIAN_POINT ( 'NONE',  ( -20.94999999999999929, 87.65000000001171543, -69.52310748452423184 ) ) ;
#199284 = EDGE_CURVE ( 'NONE', #250075, #126194, #18258, .T. ) ;
#199283 = DIRECTION ( 'NONE',  ( -0.000000000000000000, -1.897661533703519897E-16, 1.000000000000000000 ) ) ;
#199285 = ORIENTED_EDGE ( 'NONE', *, *, #147757, .T. ) ;
#199286 = AXIS2_PLACEMENT_3D ( 'NONE', #48380, #154905, #246582 ) ;
#199287 = CARTESIAN_POINT ( 'NONE',  ( 21.05000000000000071, 69.74218538953552127, -69.62089777583315708 ) ) ;
#199288 = EDGE_LOOP ( 'NONE', ( #167409, #4478, #204404, #58963 ) ) ;
#199289 = EDGE_CURVE ( 'NONE', #115921, #206232, #96486, .T. ) ;
#199290 = DIRECTION ( 'NONE',  ( 1.000000000000000000, 0.000000000000000000, 0.000000000000000000 ) ) ;
#199291 = AXIS2_PLACEMENT_3D ( 'NONE', #188187, #228605, #249453 ) ;
#199292 = ORIENTED_EDGE ( 'NONE', *, *, #52774, .T. ) ;
#199295 = ADVANCED_FACE ( 'NONE', ( #153968 ), #134332, .F. ) ;
#199294 = EDGE_LOOP ( 'NONE', ( #156214, #28631, #175764 ) ) ;
#199293 = DIRECTION ( 'NONE',  ( -1.000000000000000000, 1.207181226542539700E-16, -2.694675058168174199E-16 ) ) ;
#199298 = ORIENTED_EDGE ( 'NONE', *, *, #82853, .T. ) ;
#199297 = ORIENTED_EDGE ( 'NONE', *, *, #230488, .T. ) ;
#199296 = CARTESIAN_POINT ( 'NONE',  ( -18.50000000000000000, 11.76393579169289083, -211.0774408799668720 ) ) ;
#199300 = VECTOR ( 'NONE', #65538, 1000.000000000000000 ) ;
#199299 = DIRECTION ( 'NONE',  ( -3.469446951953515108E-14, 4.163336342344217877E-13, -1.000000000000000000 ) ) ;
#199301 = AXIS2_PLACEMENT_3D ( 'NONE', #197099, #215380, #116306 ) ;
#199302 = CARTESIAN_POINT ( 'NONE',  ( -20.94999675878240808, 65.70692517833182933, -30.56446533783036656 ) ) ;
#199303 = CARTESIAN_POINT ( 'NONE',  ( 23.14999999999999858, 5.000000000011153745, -45.90526601891310321 ) ) ;
#199304 = CIRCLE ( 'NONE', #61742, 0.09999999999999939493 ) ;
#199305 = CARTESIAN_POINT ( 'NONE',  ( -16.87401514999228169, 12.42892566803711318, -211.3112680601871318 ) ) ;
#199306 = FACE_OUTER_BOUND ( 'NONE', #125039, .T. ) ;
#199307 = CARTESIAN_POINT ( 'NONE',  ( 21.04999999999999716, 65.37049252075502181, -195.8951280845284373 ) ) ;
#199308 = CARTESIAN_POINT ( 'NONE',  ( -20.94999999999999929, -1.162701749926853712, -41.40000000000000568 ) ) ;
#199309 = CIRCLE ( 'NONE', #232644, 11.80000000000000426 ) ;
#199311 = DIRECTION ( 'NONE',  ( -0.000000000000000000, -6.982962677686266711E-15, 1.000000000000000000 ) ) ;
#199310 = CARTESIAN_POINT ( 'NONE',  ( 21.00000000000000000, 66.25000000001179501, -81.87310748452438247 ) ) ;
#199312 = ADVANCED_FACE ( 'NONE', ( #133076 ), #136918, .F. ) ;
#199313 = ORIENTED_EDGE ( 'NONE', *, *, #96836, .F. ) ;
#199314 = ORIENTED_EDGE ( 'NONE', *, *, #208091, .F. ) ;
#199315 = DIRECTION ( 'NONE',  ( 0.000000000000000000, 1.000000000000000000, -0.000000000000000000 ) ) ;
#199317 = ORIENTED_EDGE ( 'NONE', *, *, #202750, .F. ) ;
#199316 = DIRECTION ( 'NONE',  ( 0.000000000000000000, 0.000000000000000000, 1.000000000000000000 ) ) ;
#199318 = FACE_OUTER_BOUND ( 'NONE', #121382, .T. ) ;
#199319 = ORIENTED_EDGE ( 'NONE', *, *, #223415, .F. ) ;
#199320 = CARTESIAN_POINT ( 'NONE',  ( 22.47071067811865319, 7.720074744509197728, -100.4009075452974429 ) ) ;
#199321 = ORIENTED_EDGE ( 'NONE', *, *, #191408, .F. ) ;
#199322 = CARTESIAN_POINT ( 'NONE',  ( -21.64999999999999858, 7.250000000011148416, -121.6500000000000341 ) ) ;
#199323 = ADVANCED_FACE ( 'NONE', ( #92648 ), #177366, .F. ) ;
#199324 = ORIENTED_EDGE ( 'NONE', *, *, #13041, .T. ) ;
#199325 = CARTESIAN_POINT ( 'NONE',  ( -16.94052228080551714, 66.01372026691295503, -82.13273198185495971 ) ) ;
#199326 = DIRECTION ( 'NONE',  ( 0.000000000000000000, 0.8814952561688437216, -0.4721928772777334582 ) ) ;
#199327 = TOROIDAL_SURFACE ( 'NONE', #95265, 0.2000000000000000111, 0.1000000000000000056 ) ;
#199328 = ADVANCED_FACE ( 'NONE', ( #131781 ), #189469, .T. ) ;
#199329 = AXIS2_PLACEMENT_3D ( 'NONE', #174968, #194501, #74573 ) ;
#199330 = CIRCLE ( 'NONE', #228555, 0.1999999999999987899 ) ;
#199332 = VERTEX_POINT ( 'NONE', #112241 ) ;
#199331 = ORIENTED_EDGE ( 'NONE', *, *, #213883, .T. ) ;
#199333 = VERTEX_POINT ( 'NONE', #219013 ) ;
#199334 = DIRECTION ( 'NONE',  ( 1.000000000000000000, 0.000000000000000000, 0.000000000000000000 ) ) ;
#199335 = VERTEX_POINT ( 'NONE', #40427 ) ;
#199336 = EDGE_LOOP ( 'NONE', ( #221993, #225200, #122261, #173905 ) ) ;
#199337 = DIRECTION ( 'NONE',  ( 1.000000000000000000, 0.000000000000000000, 0.000000000000000000 ) ) ;
#199339 = ORIENTED_EDGE ( 'NONE', *, *, #9320, .T. ) ;
#199338 = CARTESIAN_POINT ( 'NONE',  ( 18.60000000000000142, -9.480686695267818820, -107.4411151687579036 ) ) ;
#199340 = AXIS2_PLACEMENT_3D ( 'NONE', #246164, #6249, #67517 ) ;
#199342 = CARTESIAN_POINT ( 'NONE',  ( -23.25000000000000000, -11.75000000000000000, -33.50000000000000000 ) ) ;
#199341 = DIRECTION ( 'NONE',  ( 0.000000000000000000, 0.000000000000000000, 1.000000000000000000 ) ) ;
#199343 = ADVANCED_FACE ( 'NONE', ( #220322 ), #159080, .T. ) ;
#199344 = CARTESIAN_POINT ( 'NONE',  ( -15.55912972643741199, 67.50912972644901799, -56.87310748452438247 ) ) ;
#199345 = CARTESIAN_POINT ( 'NONE',  ( -23.25000000000000000, 77.73670573947995877, -158.5056848969006182 ) ) ;
#199346 = CARTESIAN_POINT ( 'NONE',  ( -18.41431012584569871, 11.48747202921931709, -176.7267639868983338 ) ) ;
#199347 = ORIENTED_EDGE ( 'NONE', *, *, #138717, .F. ) ;
#199348 = EDGE_CURVE ( 'NONE', #180003, #253474, #197636, .T. ) ;
#199349 = ORIENTED_EDGE ( 'NONE', *, *, #34489, .T. ) ;
#199350 = DIRECTION ( 'NONE',  ( -1.000000000000000000, 2.952720810173289112E-16, 2.061873921506763405E-30 ) ) ;
#199351 = CARTESIAN_POINT ( 'NONE',  ( 20.94999999999999929, 10.29970289650803572, -222.9162226222096308 ) ) ;
#199352 = DIRECTION ( 'NONE',  ( 0.000000000000000000, 0.000000000000000000, 1.000000000000000000 ) ) ;
#199354 = EDGE_CURVE ( 'NONE', #177806, #201109, #41690, .T. ) ;
#199353 = ORIENTED_EDGE ( 'NONE', *, *, #19244, .T. ) ;
#199355 = AXIS2_PLACEMENT_3D ( 'NONE', #142786, #62006, #21599 ) ;
#199357 = LINE ( 'NONE', #55954, #157112 ) ;
#199356 = AXIS2_PLACEMENT_3D ( 'NONE', #13708, #232778, #11148 ) ;
#199358 = CIRCLE ( 'NONE', #128610, 0.09999999999999939493 ) ;
#199359 = CARTESIAN_POINT ( 'NONE',  ( 22.39999999999999503, 65.09550114356429162, -243.3481044654562879 ) ) ;
#199360 = CARTESIAN_POINT ( 'NONE',  ( -13.54795643572457919, 12.43804190223351114, -213.6995959073539666 ) ) ;
#199361 = AXIS2_PLACEMENT_3D ( 'NONE', #252688, #194040, #82693 ) ;
#199362 = EDGE_LOOP ( 'NONE', ( #55952, #163182, #224178, #7369, #75361 ) ) ;
#199363 = ORIENTED_EDGE ( 'NONE', *, *, #200247, .F. ) ;
#199364 = CARTESIAN_POINT ( 'NONE',  ( -20.94999999999999929, -11.74999999998884448, -70.10000000000005116 ) ) ;
#199365 = DIRECTION ( 'NONE',  ( 0.000000000000000000, 0.000000000000000000, -1.000000000000000000 ) ) ;
#199366 = ORIENTED_EDGE ( 'NONE', *, *, #213656, .F. ) ;
#199367 = DIRECTION ( 'NONE',  ( -1.000000000000000000, -0.000000000000000000, -0.000000000000000000 ) ) ;
#199368 = VERTEX_POINT ( 'NONE', #241173 ) ;
#199369 = ADVANCED_FACE ( 'NONE', ( #104193 ), #214568, .F. ) ;
#199370 = DIRECTION ( 'NONE',  ( 1.000000000000000000, -1.156482317317869556E-14, -3.083952846180985271E-14 ) ) ;
#199371 = LINE ( 'NONE', #179808, #220504 ) ;
#199373 = LINE ( 'NONE', #138082, #37680 ) ;
#199372 = DIRECTION ( 'NONE',  ( -0.5932847527679299127, -0.8049926720990051576, -6.257843056355997642E-15 ) ) ;
#199374 = CIRCLE ( 'NONE', #82776, 0.1000000000000134115 ) ;
#199375 = AXIS2_PLACEMENT_3D ( 'NONE', #101914, #181501, #2826 ) ;
#199376 = DIRECTION ( 'NONE',  ( 0.000000000000000000, 1.000000000000000000, 0.000000000000000000 ) ) ;
#199378 = EDGE_CURVE ( 'NONE', #123166, #156295, #83330, .T. ) ;
#199377 = CARTESIAN_POINT ( 'NONE',  ( -16.88815647973234135, 66.04916738069613302, -90.37589042119837757 ) ) ;
#199379 = EDGE_LOOP ( 'NONE', ( #50271, #247965, #19854, #157265 ) ) ;
#199380 = VECTOR ( 'NONE', #168120, 1000.000000000000000 ) ;
#199381 = DIRECTION ( 'NONE',  ( 0.000000000000000000, 0.000000000000000000, 1.000000000000000000 ) ) ;
#199382 = B_SPLINE_CURVE_WITH_KNOTS ( 'NONE', 3,
 ( #160400, #237347, #79525, #138213, #3864, #61272, #83368, #222898, #44287, #217751 ),
 .UNSPECIFIED., .F., .F.,
 ( 4, 2, 2, 2, 4 ),
 ( 0.000000000000000000, 4.221631689688066147E-05, 8.443263379376132294E-05, 0.0001688652675874656168, 0.0003377305351749607782 ),
 .UNSPECIFIED. ) ;
#199385 = VERTEX_POINT ( 'NONE', #62523 ) ;
#199384 = VERTEX_POINT ( 'NONE', #22132 ) ;
#199383 = AXIS2_PLACEMENT_3D ( 'NONE', #245237, #163139, #84829 ) ;
#199386 = EDGE_LOOP ( 'NONE', ( #67327, #67924, #205459, #135785 ) ) ;
#199387 = CIRCLE ( 'NONE', #224299, 0.1000000000000013933 ) ;
#199388 = CIRCLE ( 'NONE', #182829, 4.000000000000003553 ) ;
#199389 = CIRCLE ( 'NONE', #86903, 0.09999999999999939493 ) ;
#199390 = CARTESIAN_POINT ( 'NONE',  ( -23.25000000000000000, 76.00000000001264766, -199.3731074845243540 ) ) ;
#199391 = DIRECTION ( 'NONE',  ( 0.000000000000000000, -1.000000000000000000, 0.000000000000000000 ) ) ;
#199393 = CARTESIAN_POINT ( 'NONE',  ( 18.50000000000000000, 85.40000000001232650, -163.0238218066854472 ) ) ;
#199392 =( BOUNDED_CURVE ( )  B_SPLINE_CURVE ( 3, ( #7589, #221480, #145803, #42870 ),
 .UNSPECIFIED., .F., .F. ) 
 B_SPLINE_CURVE_WITH_KNOTS ( ( 4, 4 ),
 ( 1.570796326794885012, 3.141592653589794448 ),
 .UNSPECIFIED. ) 
 CURVE ( )  GEOMETRIC_REPRESENTATION_ITEM ( )  RATIONAL_B_SPLINE_CURVE ( ( 1.000000000000000000, 0.8047378541243619399, 0.8047378541243619399, 1.000000000000000000 ) ) 
 REPRESENTATION_ITEM ( '' )  );
#199394 = DIRECTION ( 'NONE',  ( 0.000000000000000000, 0.1350103645451904977, -0.9908441862701596881 ) ) ;
#199395 = LINE ( 'NONE', #96400, #41101 ) ;
#199396 = VECTOR ( 'NONE', #186838, 999.9999999999998863 ) ;
#199398 = CARTESIAN_POINT ( 'NONE',  ( -13.43673303185029333, 66.55335100938299320, -87.93394418860120254 ) ) ;
#199397 = CARTESIAN_POINT ( 'NONE',  ( -20.64999999999999858, 76.00000000001142553, -36.02310748452432421 ) ) ;
#199399 = EDGE_LOOP ( 'NONE', ( #142136, #27116, #208061, #251351, #54566 ) ) ;
#199400 = DIRECTION ( 'NONE',  ( 0.000000000000000000, 1.000000000000000000, 0.000000000000000000 ) ) ;
#199401 = ORIENTED_EDGE ( 'NONE', *, *, #108806, .T. ) ;
#199402 = CARTESIAN_POINT ( 'NONE',  ( 22.47071067811865319, 33.41224047107334627, -242.5462774987836667 ) ) ;
#199403 = ORIENTED_EDGE ( 'NONE', *, *, #100280, .T. ) ;
#199404 = ORIENTED_EDGE ( 'NONE', *, *, #168149, .F. ) ;
#199405 = CYLINDRICAL_SURFACE ( 'NONE', #212645, 0.09999999999998898659 ) ;
#199406 = CARTESIAN_POINT ( 'NONE',  ( 21.14999999999999858, 2.585532092011767702, -212.8717110730202933 ) ) ;
#199407 = DIRECTION ( 'NONE',  ( 1.000000000000000000, -0.000000000000000000, 0.000000000000000000 ) ) ;
#199408 = CARTESIAN_POINT ( 'NONE',  ( 13.43443725621852458, 9.446557523083688679, -82.08994195434591745 ) ) ;
#199409 = AXIS2_PLACEMENT_3D ( 'NONE', #94396, #115254, #30604 ) ;
#199411 = CIRCLE ( 'NONE', #86927, 0.5000000000000004441 ) ;
#199410 = DIRECTION ( 'NONE',  ( 0.000000000000000000, 0.09425075112713271475, 0.9955484899852801162 ) ) ;
#199412 = ORIENTED_EDGE ( 'NONE', *, *, #256145, .F. ) ;
#199413 = ORIENTED_EDGE ( 'NONE', *, *, #20345, .F. ) ;
#199414 = CYLINDRICAL_SURFACE ( 'NONE', #78047, 0.09999999999999939493 ) ;
#199415 = EDGE_LOOP ( 'NONE', ( #83787, #199992, #71375, #104961 ) ) ;
#199416 = CARTESIAN_POINT ( 'NONE',  ( -23.15000000000000213, 11.65000000001115588, -55.25000000000004974 ) ) ;
#199417 = DIRECTION ( 'NONE',  ( 1.000000000000000000, 0.000000000000000000, 0.000000000000000000 ) ) ;
#199418 = DIRECTION ( 'NONE',  ( 0.000000000000000000, 0.000000000000000000, -1.000000000000000000 ) ) ;
#199419 = CARTESIAN_POINT ( 'NONE',  ( 20.94999999999999929, 8.776282895303628706, -42.05862899514094977 ) ) ;
#199420 = CARTESIAN_POINT ( 'NONE',  ( 21.59780538579342135, 0.09897866960914131207, -60.15290947005679101 ) ) ;
#199421 = CARTESIAN_POINT ( 'NONE',  ( 6.099999999999987210, -11.65000000000000036, -15.00000000000001243 ) ) ;
#199422 = AXIS2_PLACEMENT_3D ( 'NONE', #110892, #151326, #46082 ) ;
#199424 = DIRECTION ( 'NONE',  ( 0.000000000000000000, 0.000000000000000000, -1.000000000000000000 ) ) ;
#199423 = CARTESIAN_POINT ( 'NONE',  ( -22.94999999999999929, 11.59510167572422112, 1.901609089591594692 ) ) ;
#199425 = CARTESIAN_POINT ( 'NONE',  ( -18.59999999999999787, 63.83985267992358104, -213.0213082169670145 ) ) ;
#199426 = VECTOR ( 'NONE', #142431, 1000.000000000000227 ) ;
#199427 = CARTESIAN_POINT ( 'NONE',  ( 18.50000000000002132, 65.50857864377520912, -178.7731074845244166 ) ) ;
#199429 = EDGE_CURVE ( 'NONE', #200753, #213781, #47986, .T. ) ;
#199428 = DIRECTION ( 'NONE',  ( 0.000000000000000000, 0.000000000000000000, -1.000000000000000000 ) ) ;
#199430 = TOROIDAL_SURFACE ( 'NONE', #157767, 6.258578643762700899, 0.1000000000000000056 ) ;
#199431 = DIRECTION ( 'NONE',  ( 0.000000000000000000, 0.8814952561688476074, -0.4721928772777262417 ) ) ;
#199432 = VECTOR ( 'NONE', #174068, 1000.000000000000000 ) ;
#199433 = ORIENTED_EDGE ( 'NONE', *, *, #56260, .T. ) ;
#199434 = CARTESIAN_POINT ( 'NONE',  ( 22.39999999999999503, -1.649207712992805996, -193.4275093978701818 ) ) ;
#199435 = EDGE_CURVE ( 'NONE', #157237, #148346, #172932, .T. ) ;
#199436 = ORIENTED_EDGE ( 'NONE', *, *, #40110, .F. ) ;
#199437 = CARTESIAN_POINT ( 'NONE',  ( 21.07928932188134397, 30.84304088367083097, -252.0482413927653340 ) ) ;
#199438 = CARTESIAN_POINT ( 'NONE',  ( 20.94999999999999929, 67.70174932746996888, -211.7710791003628401 ) ) ;
#199440 = ADVANCED_FACE ( 'NONE', ( #122506 ), #121253, .T. ) ;
#199439 = CARTESIAN_POINT ( 'NONE',  ( 23.14999999999999858, 1.115649653272650466E-11, -96.50000000000004263 ) ) ;
#199442 = ADVANCED_FACE ( 'NONE', ( #100333 ), #161646, .T. ) ;
#199441 = CIRCLE ( 'NONE', #86950, 0.09999999999998464284 ) ;
#199443 = AXIS2_PLACEMENT_3D ( 'NONE', #142012, #122472, #247204 ) ;
#199444 = ORIENTED_EDGE ( 'NONE', *, *, #116054, .T. ) ;
#199445 = LINE ( 'NONE', #20805, #50837 ) ;
#199446 = CIRCLE ( 'NONE', #74568, 0.1999999999999987899 ) ;
#199447 = DIRECTION ( 'NONE',  ( -1.000000000000000000, 0.000000000000000000, -0.000000000000000000 ) ) ;
#199448 = DIRECTION ( 'NONE',  ( 1.000000000000000000, 2.952720810173289112E-16, -0.000000000000000000 ) ) ;
#199449 = DIRECTION ( 'NONE',  ( 0.000000000000000000, 5.551115123126393596E-13, -1.000000000000000000 ) ) ;
#199450 = CARTESIAN_POINT ( 'NONE',  ( -23.15000000000000213, 71.65000000001155911, -57.17310748452435121 ) ) ;
#199451 = ORIENTED_EDGE ( 'NONE', *, *, #245343, .T. ) ;
#199452 = DIRECTION ( 'NONE',  ( 0.000000000000000000, 0.000000000000000000, 1.000000000000000000 ) ) ;
#199454 = VERTEX_POINT ( 'NONE', #199485 ) ;
#199453 = DIRECTION ( 'NONE',  ( 0.000000000000000000, 0.000000000000000000, -1.000000000000000000 ) ) ;
#199455 = DIRECTION ( 'NONE',  ( -0.7071067811865389130, 4.937700262164590641E-15, -0.7071067811865561215 ) ) ;
#199456 = EDGE_CURVE ( 'NONE', #234078, #97897, #110528, .T. ) ;
#199457 = CARTESIAN_POINT ( 'NONE',  ( -16.77779411440718249, 9.946101447118758543, -188.3369425829954480 ) ) ;
#199458 = DIRECTION ( 'NONE',  ( 0.000000000000000000, -0.8814952561688431665, 0.4721928772777346794 ) ) ;
#199459 =( BOUNDED_SURFACE ( )  B_SPLINE_SURFACE ( 3, 2, ( 
 ( #150024, #144849, #187865 ),
 ( #146139, #105703, #48327 ),
 ( #169614, #185279, #9201 ),
 ( #229549, #6629, #50869 ),
 ( #31378, #110875, #88715 ),
 ( #86140, #27529, #245259 ) ),
 .UNSPECIFIED., .F., .F., .F. ) 
 B_SPLINE_SURFACE_WITH_KNOTS ( ( 4, 2, 4 ),
 ( 3, 3 ),
 ( 0.0001300404313046711721, 0.0003183318589266732066, 0.0005066232865486751868 ),
 ( 0.000000000000000000, 1.000000000000000000 ),
 .UNSPECIFIED. ) 
 GEOMETRIC_REPRESENTATION_ITEM ( )  RATIONAL_B_SPLINE_SURFACE ( (
 ( 1.000000000000000000, 0.7071067811865352493, 1.000000000000000000),
 ( 1.000000000000000000, 0.7625113560539715785, 1.000000000000000000),
 ( 1.000000000000000000, 0.8126073484689285698, 1.000000000000000000),
 ( 1.000000000000000000, 0.8923049332731626260, 1.000000000000000000),
 ( 1.000000000000000000, 0.9231914937770224761, 1.000000000000000000),
 ( 1.000000000000000000, 0.9238795325112909573, 1.000000000000000000) ) ) 
 REPRESENTATION_ITEM ( '' )  SURFACE ( )  );
#199460 = ORIENTED_EDGE ( 'NONE', *, *, #78836, .T. ) ;
#199461 = CARTESIAN_POINT ( 'NONE',  ( 23.15000000000000213, 87.39257802171739797, -72.59705706435616435 ) ) ;
#199462 = CIRCLE ( 'NONE', #182314, 0.09999999999999910349 ) ;
#199463 = SHAPE_DEFINITION_REPRESENTATION ( #251405, #106899 ) ;
#199464 = DIRECTION ( 'NONE',  ( 1.000000000000000000, 0.000000000000000000, 0.000000000000000000 ) ) ;
#199465 = ORIENTED_EDGE ( 'NONE', *, *, #102304, .T. ) ;
#199466 = FACE_OUTER_BOUND ( 'NONE', #1799, .T. ) ;
#199467 = CARTESIAN_POINT ( 'NONE',  ( -23.25000000000000000, 87.75000000001247713, -173.1231074845242688 ) ) ;
#199468 = CARTESIAN_POINT ( 'NONE',  ( 21.05000000000000071, 9.480858690661944976, -221.0361137499737936 ) ) ;
#199469 = ADVANCED_FACE ( 'NONE', ( #238587 ), #63805, .T. ) ;
#199470 = ORIENTED_EDGE ( 'NONE', *, *, #105086, .T. ) ;
#199471 = EDGE_CURVE ( 'NONE', #185811, #20386, #123783, .T. ) ;
#199472 = ORIENTED_EDGE ( 'NONE', *, *, #103695, .F. ) ;
#199473 = LINE ( 'NONE', #140761, #63928 ) ;
#199474 = DIRECTION ( 'NONE',  ( 0.000000000000000000, 0.9126074666063772600, 0.4088369013363274407 ) ) ;
#199475 = CARTESIAN_POINT ( 'NONE',  ( 20.95000000000005258, 65.15000000001120384, -3.123107484524795474 ) ) ;
#199476 = CARTESIAN_POINT ( 'NONE',  ( 23.24999999999999289, 53.46521213003792639, -234.8449159514430846 ) ) ;
#199477 = FACE_OUTER_BOUND ( 'NONE', #32809, .T. ) ;
#199478 = DIRECTION ( 'NONE',  ( 0.000000000000000000, 6.982962677686267499E-15, -1.000000000000000000 ) ) ;
#199479 = EDGE_CURVE ( 'NONE', #48405, #227579, #84600, .T. ) ;
#199481 = CARTESIAN_POINT ( 'NONE',  ( 21.05000000000000071, 77.73625713160897988, -57.95445515550681392 ) ) ;
#199480 = DIRECTION ( 'NONE',  ( 0.000000000000000000, -0.5000000000000275335, -0.8660254037844228314 ) ) ;
#199482 = AXIS2_PLACEMENT_3D ( 'NONE', #179613, #38812, #58334 ) ;
#199484 = DIRECTION ( 'NONE',  ( 1.186688945009010077E-16, -1.000000000000000000, -0.000000000000000000 ) ) ;
#199483 = AXIS2_PLACEMENT_3D ( 'NONE', #210250, #26473, #109833 ) ;
#199485 = CARTESIAN_POINT ( 'NONE',  ( -20.54999999999999716, 53.03738849591485405, -234.3791188517465400 ) ) ;
#199486 = CARTESIAN_POINT ( 'NONE',  ( 18.59999999999996945, 65.66751761918722252, -164.4282609406112670 ) ) ;
#199487 = AXIS2_PLACEMENT_3D ( 'NONE', #112531, #192078, #113803 ) ;
#199489 = CARTESIAN_POINT ( 'NONE',  ( 23.14999999999999503, 61.57587952878035509, -212.2000740415318774 ) ) ;
#199488 = CIRCLE ( 'NONE', #87000, 0.09999999999999939493 ) ;
#199490 = VERTEX_POINT ( 'NONE', #58642 ) ;
#199491 = ORIENTED_EDGE ( 'NONE', *, *, #244147, .F. ) ;
#199492 = DIRECTION ( 'NONE',  ( 0.000000000000000000, 0.000000000000000000, -1.000000000000000000 ) ) ;
#199494 = DIRECTION ( 'NONE',  ( 1.000000000000000000, 0.000000000000000000, 0.000000000000000000 ) ) ;
#199493 = CARTESIAN_POINT ( 'NONE',  ( 18.69999999999999929, 10.88519226655716565, -15.14794223642649840 ) ) ;
#199495 =( BOUNDED_CURVE ( )  B_SPLINE_CURVE ( 3, ( #123751, #104159, #227978, #243688 ),
 .UNSPECIFIED., .F., .F. ) 
 B_SPLINE_CURVE_WITH_KNOTS ( ( 4, 4 ),
 ( 4.712388980384689674, 6.283185307179586232 ),
 .UNSPECIFIED. ) 
 CURVE ( )  GEOMETRIC_REPRESENTATION_ITEM ( )  RATIONAL_B_SPLINE_CURVE ( ( 1.000000000000000000, 0.8047378541243649375, 0.8047378541243649375, 1.000000000000000000 ) ) 
 REPRESENTATION_ITEM ( '' )  );
#199496 = CIRCLE ( 'NONE', #128739, 0.2000000000000057288 ) ;
#199497 = CARTESIAN_POINT ( 'NONE',  ( -23.15000000000000213, 64.35000000001254250, -182.1731074845244507 ) ) ;
#199498 = CARTESIAN_POINT ( 'NONE',  ( 20.27550659511089037, 9.216043722519994930, -154.8500000000000227 ) ) ;
#199499 = ORIENTED_EDGE ( 'NONE', *, *, #192254, .T. ) ;
#199500 = DIRECTION ( 'NONE',  ( 0.000000000000000000, 0.000000000000000000, -1.000000000000000000 ) ) ;
#199501 = EDGE_LOOP ( 'NONE', ( #178231, #195250, #148344, #160411 ) ) ;
#199502 = AXIS2_PLACEMENT_3D ( 'NONE', #210844, #92171, #146997 ) ;
#199504 = VECTOR ( 'NONE', #93674, 1000.000000000000114 ) ;
#199503 = CARTESIAN_POINT ( 'NONE',  ( -13.11924609551135390, 9.431689550524099630, -18.27929003223606585 ) ) ;
#199505 = ORIENTED_EDGE ( 'NONE', *, *, #51991, .F. ) ;
#199506 = CARTESIAN_POINT ( 'NONE',  ( 23.14999999999999858, 76.00000000001170974, -69.52310748452431710 ) ) ;
#199507 = AXIS2_PLACEMENT_3D ( 'NONE', #125588, #63037, #43494 ) ;
#199508 = CARTESIAN_POINT ( 'NONE',  ( 20.94999999999999929, -8.999999999988842703, -124.5060308773475839 ) ) ;
#199509 = EDGE_CURVE ( 'NONE', #21996, #36999, #93774, .T. ) ;
#199510 = ADVANCED_FACE ( 'NONE', ( #1239 ), #80772, .T. ) ;
#199511 = ORIENTED_EDGE ( 'NONE', *, *, #174534, .F. ) ;
#199512 = CARTESIAN_POINT ( 'NONE',  ( -23.25000000000000000, 80.82423061532404063, -192.8091306798888525 ) ) ;
#199513 = ORIENTED_EDGE ( 'NONE', *, *, #106766, .T. ) ;
#199514 = ADVANCED_FACE ( 'NONE', ( #89770 ), #204585, .F. ) ;
#199516 = EDGE_CURVE ( 'NONE', #199385, #103641, #89671, .T. ) ;
#199515 = CARTESIAN_POINT ( 'NONE',  ( -23.15000000000000213, 74.00000000001186606, -89.79848556176222019 ) ) ;
#199517 = FACE_OUTER_BOUND ( 'NONE', #251153, .T. ) ;
#199518 = DIRECTION ( 'NONE',  ( 0.000000000000000000, 0.000000000000000000, 1.000000000000000000 ) ) ;
#199519 = FACE_OUTER_BOUND ( 'NONE', #79316, .T. ) ;
#199520 = CARTESIAN_POINT ( 'NONE',  ( 23.04999999999999716, 67.17743825834565996, -123.8731074845243683 ) ) ;
#199522 = DIRECTION ( 'NONE',  ( 1.000000000000000000, 0.000000000000000000, 0.000000000000000000 ) ) ;
#199521 = CARTESIAN_POINT ( 'NONE',  ( 21.10000000000000142, 4.898587196589412829E-16, -4.000000000000000000 ) ) ;
#199523 = EDGE_CURVE ( 'NONE', #33727, #37705, #90296, .T. ) ;
#199524 = CARTESIAN_POINT ( 'NONE',  ( -20.94999999999999929, 67.23127455305841238, -235.8551265064783991 ) ) ;
#199526 = ORIENTED_EDGE ( 'NONE', *, *, #84218, .T. ) ;
#199525 = CARTESIAN_POINT ( 'NONE',  ( 20.30466543256828160, 66.69576306075789773, -128.2694448331316153 ) ) ;
#199528 = LINE ( 'NONE', #40473, #243364 ) ;
#199527 = DIRECTION ( 'NONE',  ( 0.000000000000000000, 6.982962677686266711E-15, -1.000000000000000000 ) ) ;
#199529 = EDGE_LOOP ( 'NONE', ( #249503, #254978, #155956, #2620 ) ) ;
#199531 = ORIENTED_EDGE ( 'NONE', *, *, #102325, .F. ) ;
#199530 = CARTESIAN_POINT ( 'NONE',  ( 21.05000000000000071, 76.00000000001195133, -103.0231074845243171 ) ) ;
#199532 = AXIS2_PLACEMENT_3D ( 'NONE', #210088, #56106, #193087 ) ;
#199533 = EDGE_CURVE ( 'NONE', #139324, #169843, #188888, .T. ) ;
#199534 = EDGE_LOOP ( 'NONE', ( #63137, #38597, #230050, #7086 ) ) ;
#199535 = CARTESIAN_POINT ( 'NONE',  ( 20.95000000000005258, 64.25000000001119815, -29.92310748452479174 ) ) ;
#199537 = ADVANCED_FACE ( 'NONE', ( #224149 ), #246297, .F. ) ;
#199536 = EDGE_CURVE ( 'NONE', #252276, #196725, #8964, .T. ) ;
#199538 = DIRECTION ( 'NONE',  ( 1.000000000000000000, -1.145314911736513911E-16, 3.106193895438251633E-17 ) ) ;
#199539 = DIRECTION ( 'NONE',  ( 0.000000000000000000, 0.000000000000000000, 1.000000000000000000 ) ) ;
#199540 = VERTEX_POINT ( 'NONE', #49380 ) ;
#199541 = DIRECTION ( 'NONE',  ( -1.000000000000000000, 0.000000000000000000, 0.000000000000000000 ) ) ;
#199542 = FACE_OUTER_BOUND ( 'NONE', #27607, .T. ) ;
#199543 = AXIS2_PLACEMENT_3D ( 'NONE', #112748, #52754, #94456 ) ;
#199545 = EDGE_CURVE ( 'NONE', #137609, #128950, #152062, .T. ) ;
#199544 = DIRECTION ( 'NONE',  ( 0.000000000000000000, 0.2617529984165031243, 0.9651348961777157509 ) ) ;
#199546 = CARTESIAN_POINT ( 'NONE',  ( -16.89318236219977365, 9.951535257886286345, -154.8551296321058715 ) ) ;
#199547 = DIRECTION ( 'NONE',  ( 2.952720810173289112E-16, 1.000000000000000000, 6.938893903907222067E-15 ) ) ;
#199548 = EDGE_CURVE ( 'NONE', #71417, #108268, #164537, .T. ) ;
#199549 = DIRECTION ( 'NONE',  ( 0.000000000000000000, 0.000000000000000000, -1.000000000000000000 ) ) ;
#199550 = ORIENTED_EDGE ( 'NONE', *, *, #17385, .T. ) ;
#199551 = ORIENTED_EDGE ( 'NONE', *, *, #211626, .F. ) ;
#199552 = CIRCLE ( 'NONE', #7999, 0.1000000000000028644 ) ;
#199553 = DIRECTION ( 'NONE',  ( -4.336808689941752679E-15, 0.8660254037844482555, 0.4999999999999837907 ) ) ;
#199554 = ADVANCED_FACE ( 'NONE', ( #225420 ), #52071, .T. ) ;
#199555 = EDGE_CURVE ( 'NONE', #67614, #58239, #2185, .T. ) ;
#199556 = VECTOR ( 'NONE', #21179, 1000.000000000000000 ) ;
#199557 = ORIENTED_EDGE ( 'NONE', *, *, #123115, .F. ) ;
#199558 = CARTESIAN_POINT ( 'NONE',  ( 18.59999999999999076, 69.35000000001180354, -81.77310748452435973 ) ) ;
#199560 = EDGE_LOOP ( 'NONE', ( #169679, #126258, #154546, #213492 ) ) ;
#199559 = AXIS2_PLACEMENT_3D ( 'NONE', #227374, #203956, #205229 ) ;
#199561 = CARTESIAN_POINT ( 'NONE',  ( 20.93975676684922504, 10.31104185824063535, -173.0204516983106089 ) ) ;
#199562 = EDGE_CURVE ( 'NONE', #252869, #3898, #110630, .T. ) ;
#199563 = CARTESIAN_POINT ( 'NONE',  ( 23.50000000000005684, 87.50449464844290048, -34.18759587077607165 ) ) ;
#199564 = CARTESIAN_POINT ( 'NONE',  ( 23.24999999999999289, 2.272311100394802885, -217.9150152700588592 ) ) ;
#199565 = CARTESIAN_POINT ( 'NONE',  ( -16.89268316805465986, 63.08557629953710943, -213.1216189793661329 ) ) ;
#199566 = EDGE_CURVE ( 'NONE', #164668, #212715, #208472, .T. ) ;
#199567 = AXIS2_PLACEMENT_3D ( 'NONE', #164447, #2772, #103155 ) ;
#199568 = CIRCLE ( 'NONE', #87088, 0.1000000000000028644 ) ;
#199569 = ADVANCED_FACE ( 'NONE', ( #85897 ), #70257, .F. ) ;
#199570 = CARTESIAN_POINT ( 'NONE',  ( -23.15000000000000213, 85.00000000001179501, -79.41707660717668205 ) ) ;
#199571 = DIRECTION ( 'NONE',  ( -0.000000000000000000, -0.2128009952263603677, 0.9770955615653313941 ) ) ;
#199572 = CARTESIAN_POINT ( 'NONE',  ( 20.85000000000000142, 56.23643450586807546, -227.9054833905874204 ) ) ;
#199573 = EDGE_LOOP ( 'NONE', ( #77873, #193357, #172683, #119554 ) ) ;
#199575 = DIRECTION ( 'NONE',  ( 0.000000000000000000, -1.000000000000000000, 6.308085367188393199E-16 ) ) ;
#199574 = DIRECTION ( 'NONE',  ( -1.000000000000000000, 1.836970198721029934E-16, 1.601412966608202925E-30 ) ) ;
#199576 = EDGE_LOOP ( 'NONE', ( #33851, #57487, #8492, #80679 ) ) ;
#199579 = ORIENTED_EDGE ( 'NONE', *, *, #20342, .T. ) ;
#199578 = CARTESIAN_POINT ( 'NONE',  ( -21.14999999999999858, 11.48087284840413425, -198.4995883060917947 ) ) ;
#199577 = CARTESIAN_POINT ( 'NONE',  ( -18.59999999999999787, 11.74999999999999645, -21.35000000000000142 ) ) ;
#199580 = AXIS2_PLACEMENT_3D ( 'NONE', #196483, #235608, #197772 ) ;
#199581 = VERTEX_POINT ( 'NONE', #209738 ) ;
#199582 = SPHERICAL_SURFACE ( 'NONE', #76769, 0.1000000000000000056 ) ;
#199583 = AXIS2_PLACEMENT_3D ( 'NONE', #140772, #117361, #79493 ) ;
#199584 = CARTESIAN_POINT ( 'NONE',  ( 18.59999999999999076, 6.400000000011158541, -76.93042463006162279 ) ) ;
#199585 = AXIS2_PLACEMENT_3D ( 'NONE', #155112, #98918, #95103 ) ;
#199586 = CARTESIAN_POINT ( 'NONE',  ( -18.59999999999999787, 80.78317333349157536, -192.9003134612048882 ) ) ;
#199587 = CARTESIAN_POINT ( 'NONE',  ( -16.80100426158789872, 9.943150520407291637, -113.1829457528341010 ) ) ;
#199588 = ORIENTED_EDGE ( 'NONE', *, *, #142671, .F. ) ;
#199589 = DIRECTION ( 'NONE',  ( -0.5932847527679310229, -0.8049926720990042694, -4.984624513800578906E-15 ) ) ;
#199590 = EDGE_CURVE ( 'NONE', #200909, #7750, #245005, .T. ) ;
#199591 = VECTOR ( 'NONE', #93506, 1000.000000000000000 ) ;
#199592 = DIRECTION ( 'NONE',  ( 0.000000000000000000, 0.000000000000000000, 1.000000000000000000 ) ) ;
#199594 = LINE ( 'NONE', #100431, #230006 ) ;
#199593 = CARTESIAN_POINT ( 'NONE',  ( 18.59999999999999076, 54.57427006634497957, -228.7596887170734306 ) ) ;
#199596 = EDGE_LOOP ( 'NONE', ( #83591, #242131 ) ) ;
#199595 = DIRECTION ( 'NONE',  ( 0.000000000000000000, -0.9553114395362780620, -0.2956011730205483912 ) ) ;
#199597 = ORIENTED_EDGE ( 'NONE', *, *, #71165, .F. ) ;
#199598 = LINE ( 'NONE', #216563, #84726 ) ;
#199599 = ORIENTED_EDGE ( 'NONE', *, *, #90479, .T. ) ;
#199600 = DIRECTION ( 'NONE',  ( 1.186688945009009831E-16, 0.9651348961777157509, -0.2617529984165031243 ) ) ;
#199601 = VERTEX_POINT ( 'NONE', #11548 ) ;
#199602 = DIRECTION ( 'NONE',  ( 1.000000000000000000, 0.000000000000000000, 0.000000000000000000 ) ) ;
#199603 = DIRECTION ( 'NONE',  ( -1.000000000000000000, 0.000000000000000000, 0.000000000000000000 ) ) ;
#199604 = CARTESIAN_POINT ( 'NONE',  ( -21.05000000000000071, 1.116121084443477685E-11, -136.9000000000000057 ) ) ;
#199605 = ORIENTED_EDGE ( 'NONE', *, *, #142114, .F. ) ;
#199606 = CYLINDRICAL_SURFACE ( 'NONE', #166850, 0.09999999999999789613 ) ;
#199607 = VECTOR ( 'NONE', #187577, 1000.000000000000000 ) ;
#199608 = VECTOR ( 'NONE', #241246, 999.9999999999998863 ) ;
#199609 = EDGE_CURVE ( 'NONE', #111962, #26247, #46788, .T. ) ;
#199610 = AXIS2_PLACEMENT_3D ( 'NONE', #184715, #42644, #85581 ) ;
#199612 = EDGE_CURVE ( 'NONE', #37627, #22332, #68862, .T. ) ;
#199611 = CARTESIAN_POINT ( 'NONE',  ( -16.78493211734302903, 9.945835743215324598, -54.33605098089597618 ) ) ;
#199613 = AXIS2_PLACEMENT_3D ( 'NONE', #152911, #210294, #15967 ) ;
#199614 = EDGE_LOOP ( 'NONE', ( #215353, #76800, #209014, #92125 ) ) ;
#199615 = ORIENTED_EDGE ( 'NONE', *, *, #256615, .T. ) ;
#199616 = ORIENTED_EDGE ( 'NONE', *, *, #50493, .F. ) ;
#199617 = ADVANCED_FACE ( 'NONE', ( #93635 ), #153673, .F. ) ;
#199618 = PLANE ( 'NONE',  #20914 ) ;
#199619 = ORIENTED_EDGE ( 'NONE', *, *, #182810, .F. ) ;
#199622 = EDGE_CURVE ( 'NONE', #46891, #493, #16684, .T. ) ;
#199621 = EDGE_LOOP ( 'NONE', ( #36731, #178715, #43824, #182975 ) ) ;
#199620 = CARTESIAN_POINT ( 'NONE',  ( 15.66039659514496130, 66.63925083009746686, -186.2085373439172145 ) ) ;
#199623 = ORIENTED_EDGE ( 'NONE', *, *, #218707, .T. ) ;
#199624 = VECTOR ( 'NONE', #199127, 1000.000000000000000 ) ;
#199627 = ORIENTED_EDGE ( 'NONE', *, *, #192163, .T. ) ;
#199626 = VERTEX_POINT ( 'NONE', #136592 ) ;
#199625 = CARTESIAN_POINT ( 'NONE',  ( 21.05000000000000071, 85.00000000001251976, -179.9170766071767389 ) ) ;
#199628 = CIRCLE ( 'NONE', #212084, 4.049999999999998046 ) ;
#199629 = VERTEX_POINT ( 'NONE', #174520 ) ;
#199630 = CARTESIAN_POINT ( 'NONE',  ( -21.52071067811865746, 7.779289321892505882, -146.3500000000000227 ) ) ;
#199631 = TOROIDAL_SURFACE ( 'NONE', #203872, 0.9750000000000019762, 0.1000000000000000056 ) ;
#199632 = CARTESIAN_POINT ( 'NONE',  ( 20.95000000000005258, 66.15000000001120384, -5.923107484524795296 ) ) ;
#199633 = EDGE_CURVE ( 'NONE', #111449, #102386, #235410, .T. ) ;
#199634 = CARTESIAN_POINT ( 'NONE',  ( -20.64999999999999858, 76.00000000001222134, -149.3981074845243313 ) ) ;
#199635 = ORIENTED_EDGE ( 'NONE', *, *, #10872, .T. ) ;
#199636 = B_SPLINE_CURVE_WITH_KNOTS ( 'NONE', 3,
 ( #169676, #133075, #210055, #131780, #212618, #152664, #14434, #71830, #92647, #253007, #91382, #151369, #70561, #10566, #228328, #50936, #129222, #113505, #109639 ),
 .UNSPECIFIED., .F., .F.,
 ( 4, 3, 3, 3, 3, 3, 4 ),
 ( 0.000000000000000000, 1.655171619025938174E-05, 2.773500582849094026E-05, 5.941817267379380797E-05, 0.0001114174635873529072, 0.0001914169455916513380, 0.0002627181070750865912 ),
 .UNSPECIFIED. ) ;
#199637 = CARTESIAN_POINT ( 'NONE',  ( 23.14999999999999503, 11.75000000001116263, -155.7499999999999716 ) ) ;
#199639 = ORIENTED_EDGE ( 'NONE', *, *, #23856, .F. ) ;
#199638 = DIRECTION ( 'NONE',  ( 1.000000000000000000, 0.000000000000000000, 0.000000000000000000 ) ) ;
#199640 = CARTESIAN_POINT ( 'NONE',  ( -18.40000000000000213, 5.650000000011139001, -180.1499999999999773 ) ) ;
#199642 = EDGE_LOOP ( 'NONE', ( #193310, #226851, #109153, #35261, #175245, #107161, #180222, #34517, #120068, #219190 ) ) ;
#199641 = DIRECTION ( 'NONE',  ( 0.000000000000000000, 6.982962677686266711E-15, -1.000000000000000000 ) ) ;
#199643 = ORIENTED_EDGE ( 'NONE', *, *, #3827, .F. ) ;
#199644 = DIRECTION ( 'NONE',  ( 0.000000000000000000, 0.000000000000000000, 1.000000000000000000 ) ) ;
#199645 = ORIENTED_EDGE ( 'NONE', *, *, #98346, .T. ) ;
#199646 = ORIENTED_EDGE ( 'NONE', *, *, #212999, .F. ) ;
#199647 = AXIS2_PLACEMENT_3D ( 'NONE', #32453, #113232, #53269 ) ;
#199648 = CARTESIAN_POINT ( 'NONE',  ( 20.94999999999999929, 5.000000000011153745, -121.9947339810869380 ) ) ;
#199649 = DIRECTION ( 'NONE',  ( 0.000000000000000000, 0.000000000000000000, -1.000000000000000000 ) ) ;
#199650 = ADVANCED_FACE ( 'NONE', ( #114481 ), #123015, .T. ) ;
#199652 = VERTEX_POINT ( 'NONE', #12839 ) ;
#199651 = ORIENTED_EDGE ( 'NONE', *, *, #154041, .F. ) ;
#199653 = ORIENTED_EDGE ( 'NONE', *, *, #155348, .T. ) ;
#199654 = CARTESIAN_POINT ( 'NONE',  ( 21.09706851349341861, 61.96409884441155214, -221.7490514850052534 ) ) ;
#199655 = ORIENTED_EDGE ( 'NONE', *, *, #135513, .T. ) ;
#199656 = ORIENTED_EDGE ( 'NONE', *, *, #200825, .T. ) ;
#199657 = CARTESIAN_POINT ( 'NONE',  ( 18.41416235934318735, 85.50000000001242029, -163.4229180933022576 ) ) ;
#199658 = ORIENTED_EDGE ( 'NONE', *, *, #146910, .F. ) ;
#199660 = CARTESIAN_POINT ( 'NONE',  ( -16.77683809663752257, 9.945835743215301505, -46.16394901910421567 ) ) ;
#199659 = DIRECTION ( 'NONE',  ( -1.000000000000000000, 0.000000000000000000, 0.000000000000000000 ) ) ;
#199661 = EDGE_CURVE ( 'NONE', #87546, #221522, #171933, .T. ) ;
#199662 = VERTEX_POINT ( 'NONE', #233175 ) ;
#199663 = EDGE_CURVE ( 'NONE', #64319, #72979, #39649, .T. ) ;
#199665 = ORIENTED_EDGE ( 'NONE', *, *, #33516, .T. ) ;
#199664 = VERTEX_POINT ( 'NONE', #55753 ) ;
#199667 = CIRCLE ( 'NONE', #83065, 0.2000000000000000944 ) ;
#199666 = LINE ( 'NONE', #241351, #90252 ) ;
#199668 = FACE_OUTER_BOUND ( 'NONE', #29349, .T. ) ;
#199669 = AXIS2_PLACEMENT_3D ( 'NONE', #122390, #117256, #221455 ) ;
#199670 = AXIS2_PLACEMENT_3D ( 'NONE', #199135, #242100, #37510 ) ;
#199671 = AXIS2_PLACEMENT_3D ( 'NONE', #110849, #192967, #191709 ) ;
#199672 = EDGE_LOOP ( 'NONE', ( #197451, #18736, #71735 ) ) ;
#199673 = EDGE_CURVE ( 'NONE', #187409, #219130, #156361, .T. ) ;
#199674 = CIRCLE ( 'NONE', #83077, 0.1000000000000028644 ) ;
#199675 = CARTESIAN_POINT ( 'NONE',  ( -18.45068461519106506, 85.48650652910100689, -95.95433031561951509 ) ) ;
#199676 = ORIENTED_EDGE ( 'NONE', *, *, #93729, .T. ) ;
#199677 = ORIENTED_EDGE ( 'NONE', *, *, #167257, .T. ) ;
#199678 = FACE_OUTER_BOUND ( 'NONE', #148937, .T. ) ;
#199680 = EDGE_CURVE ( 'NONE', #111107, #220201, #113199, .T. ) ;
#199679 = ORIENTED_EDGE ( 'NONE', *, *, #139375, .F. ) ;
#199681 = CARTESIAN_POINT ( 'NONE',  ( 21.00000000000000000, 22.61918030723622408, -230.9697045991730988 ) ) ;
#199682 = ORIENTED_EDGE ( 'NONE', *, *, #140659, .T. ) ;
#199683 = EDGE_CURVE ( 'NONE', #155114, #249345, #213576, .T. ) ;
#199684 = CARTESIAN_POINT ( 'NONE',  ( 18.59999999999997655, 1.115600667400684642E-11, -200.9999999999999432 ) ) ;
#199685 = CARTESIAN_POINT ( 'NONE',  ( -18.44085059012131822, 11.51401249349495437, -42.75969468087846792 ) ) ;
#199687 = LINE ( 'NONE', #21052, #45637 ) ;
#199686 = LINE ( 'NONE', #185236, #227861 ) ;
#199688 = CARTESIAN_POINT ( 'NONE',  ( -18.59999999999999787, 79.58035499750722863, -226.6153910028758958 ) ) ;
#199690 = CARTESIAN_POINT ( 'NONE',  ( 23.14999999999999858, 76.00000000001126921, -203.5231074845248997 ) ) ;
#199689 = CIRCLE ( 'NONE', #141392, 0.1000000000000124678 ) ;
#199692 = CARTESIAN_POINT ( 'NONE',  ( -20.64999999999999858, 2.400000000011155432, -53.77537807723790309 ) ) ;
#199691 = CIRCLE ( 'NONE', #216407, 0.09999999999999939493 ) ;
#199693 = DIRECTION ( 'NONE',  ( 0.000000000000000000, 0.4930308989875324399, 0.8700118002898268310 ) ) ;
#199694 = VECTOR ( 'NONE', #189902, 1000.000000000000000 ) ;
#199696 = EDGE_CURVE ( 'NONE', #42010, #159384, #143835, .T. ) ;
#199695 = DIRECTION ( 'NONE',  ( -1.000000000000000000, 0.000000000000000000, 0.000000000000000000 ) ) ;
#199697 = CARTESIAN_POINT ( 'NONE',  ( -23.25000000000000000, 1.115600667400684642E-11, -171.5499999999999829 ) ) ;
#199698 = VERTEX_POINT ( 'NONE', #54501 ) ;
#199699 = AXIS2_PLACEMENT_3D ( 'NONE', #149031, #70787, #147732 ) ;
#199701 = ORIENTED_EDGE ( 'NONE', *, *, #78336, .T. ) ;
#199700 = ORIENTED_EDGE ( 'NONE', *, *, #197979, .T. ) ;
#199702 = ORIENTED_EDGE ( 'NONE', *, *, #8782, .F. ) ;
#199703 = ORIENTED_EDGE ( 'NONE', *, *, #5102, .T. ) ;
#199705 = ADVANCED_FACE ( 'NONE', ( #196576 ), #247348, .F. ) ;
#199704 = DIRECTION ( 'NONE',  ( 1.000000000000000000, 0.000000000000000000, 0.000000000000000000 ) ) ;
#199706 = DIRECTION ( 'NONE',  ( -1.000000000000000000, -0.000000000000000000, 0.000000000000000000 ) ) ;
#199708 = DIRECTION ( 'NONE',  ( 0.000000000000000000, 0.9126074666063772600, 0.4088369013363277182 ) ) ;
#199707 = CARTESIAN_POINT ( 'NONE',  ( -22.39999999999999858, 29.50811709945089945, -252.6450601445781103 ) ) ;
#199709 = CARTESIAN_POINT ( 'NONE',  ( -21.05000000000000071, -0.2561057920810652089, -167.4651035583276553 ) ) ;
#199710 = ORIENTED_EDGE ( 'NONE', *, *, #50853, .T. ) ;
#199711 = CARTESIAN_POINT ( 'NONE',  ( -20.54999999999999361, 11.65000000001115232, -54.85000000000000142 ) ) ;
#199712 = CARTESIAN_POINT ( 'NONE',  ( 22.39999999999999858, 68.20922040163875977, -136.6231074845243540 ) ) ;
#199713 = LINE ( 'NONE', #181431, #34859 ) ;
#199714 = CARTESIAN_POINT ( 'NONE',  ( -23.25000000000000000, 5.950000000011167245, -157.1942976949652007 ) ) ;
#199715 = ORIENTED_EDGE ( 'NONE', *, *, #219274, .F. ) ;
#199716 = AXIS2_PLACEMENT_3D ( 'NONE', #153699, #15430, #229339 ) ;
#199717 = DIRECTION ( 'NONE',  ( -0.000000000000000000, -0.1350103645451876666, -0.9908441862701600211 ) ) ;
#199718 = CARTESIAN_POINT ( 'NONE',  ( -21.05000000000000071, -0.09999996528893663472, -94.02244781750655989 ) ) ;
#199719 = ORIENTED_EDGE ( 'NONE', *, *, #85801, .T. ) ;
#199720 = CARTESIAN_POINT ( 'NONE',  ( -18.34374000495060386, 64.52683809665015247, -194.2731074845244450 ) ) ;
#199721 = AXIS2_PLACEMENT_3D ( 'NONE', #70781, #72047, #149023 ) ;
#199722 = FACE_OUTER_BOUND ( 'NONE', #249289, .T. ) ;
#199723 = DIRECTION ( 'NONE',  ( 0.000000000000000000, 0.000000000000000000, -1.000000000000000000 ) ) ;
#199724 = CARTESIAN_POINT ( 'NONE',  ( 21.05000000000000071, -11.64999999998883595, -197.9999999999999432 ) ) ;
#199725 = CARTESIAN_POINT ( 'NONE',  ( -21.55000000000000071, 7.350000000011155166, -112.8500000000000369 ) ) ;
#199726 = EDGE_LOOP ( 'NONE', ( #210554, #227380, #176905, #193768 ) ) ;
#199727 = CARTESIAN_POINT ( 'NONE',  ( 23.24999999999999289, 11.65000000001116298, -100.6000000000000369 ) ) ;
#199728 = CARTESIAN_POINT ( 'NONE',  ( 21.30000000000002558, 76.00000000001213607, -136.5231074845242745 ) ) ;
#199729 = CYLINDRICAL_SURFACE ( 'NONE', #141645, 0.5000000000000004441 ) ;
#199731 = CARTESIAN_POINT ( 'NONE',  ( 23.15000000000000213, 52.64219947837469959, -255.2660483925003803 ) ) ;
#199730 = CYLINDRICAL_SURFACE ( 'NONE', #128422, 0.1000000000000026007 ) ;
#199732 = CARTESIAN_POINT ( 'NONE',  ( -20.85000000000000142, -1.736705739456431807, -145.5174225876237699 ) ) ;
#199733 = CARTESIAN_POINT ( 'NONE',  ( -21.14999999999999858, 11.75000000001115552, -167.5999999999999659 ) ) ;
#199734 = DIRECTION ( 'NONE',  ( 0.000000000000000000, 0.000000000000000000, 1.000000000000000000 ) ) ;
#199735 = DIRECTION ( 'NONE',  ( 1.000000000000000000, 0.000000000000000000, 0.000000000000000000 ) ) ;
#199736 = CIRCLE ( 'NONE', #24953, 0.1000000000000013933 ) ;
#199737 = ORIENTED_EDGE ( 'NONE', *, *, #229842, .F. ) ;
#199738 = EDGE_CURVE ( 'NONE', #162005, #21871, #219993, .T. ) ;
#199739 = AXIS2_PLACEMENT_3D ( 'NONE', #134367, #213927, #108415 ) ;
#199740 = VERTEX_POINT ( 'NONE', #2214 ) ;
#199742 = EDGE_LOOP ( 'NONE', ( #108477, #72886, #153433, #33206 ) ) ;
#199741 = AXIS2_PLACEMENT_3D ( 'NONE', #105059, #163810, #64692 ) ;
#199743 = EDGE_CURVE ( 'NONE', #166838, #198612, #238267, .T. ) ;
#199744 = LINE ( 'NONE', #240141, #230487 ) ;
#199745 = CIRCLE ( 'NONE', #91401, 0.1000000000000028644 ) ;
#199746 = AXIS2_PLACEMENT_3D ( 'NONE', #140442, #216131, #62209 ) ;
#199747 = EDGE_CURVE ( 'NONE', #248047, #183490, #43925, .T. ) ;
#199748 = EDGE_CURVE ( 'NONE', #139130, #82762, #27187, .T. ) ;
#199749 = LINE ( 'NONE', #101877, #217065 ) ;
#199750 = CARTESIAN_POINT ( 'NONE',  ( 21.93340585899577988, 65.31415710917552531, -242.9239163822612682 ) ) ;
#199751 = ORIENTED_EDGE ( 'NONE', *, *, #66782, .F. ) ;
#199752 = AXIS2_PLACEMENT_3D ( 'NONE', #24299, #62128, #144201 ) ;
#199753 = FACE_OUTER_BOUND ( 'NONE', #133140, .T. ) ;
#199754 = AXIS2_PLACEMENT_3D ( 'NONE', #250144, #191483, #117052 ) ;
#199755 = AXIS2_PLACEMENT_3D ( 'NONE', #203563, #224396, #45767 ) ;
#199756 = FACE_OUTER_BOUND ( 'NONE', #34055, .T. ) ;
#199757 = FACE_OUTER_BOUND ( 'NONE', #186051, .T. ) ;
#199758 = AXIS2_PLACEMENT_3D ( 'NONE', #29582, #33442, #192476 ) ;
#199759 = DIRECTION ( 'NONE',  ( 1.000000000000000000, 0.000000000000000000, 0.000000000000000000 ) ) ;
#199761 = ORIENTED_EDGE ( 'NONE', *, *, #210642, .F. ) ;
#199760 = CARTESIAN_POINT ( 'NONE',  ( -20.64999999999999858, 85.40000000001198543, -112.9170766071766820 ) ) ;
#199763 = CARTESIAN_POINT ( 'NONE',  ( -16.94107738177414291, 10.01423928514777728, -154.9500000000000455 ) ) ;
#199762 = DIRECTION ( 'NONE',  ( -1.186688945009010077E-16, -1.000000000000000000, -6.789366196018717631E-15 ) ) ;
#199764 = EDGE_CURVE ( 'NONE', #191355, #102134, #102295, .T. ) ;
#199765 = AXIS2_PLACEMENT_3D ( 'NONE', #214736, #115645, #195211 ) ;
#199766 = CARTESIAN_POINT ( 'NONE',  ( -20.54999999999999716, 67.23127455305841238, -235.8551265064783991 ) ) ;
#199767 = PRESENTATION_STYLE_ASSIGNMENT (( #160645 ) ) ;
#199768 = ORIENTED_EDGE ( 'NONE', *, *, #9228, .F. ) ;
#199769 = CARTESIAN_POINT ( 'NONE',  ( 0.000000000000000000, 0.000000000000000000, 0.000000000000000000 ) ) ;
#199770 = CARTESIAN_POINT ( 'NONE',  ( -21.07928932188134041, -1.250084634896336366, -194.7953894783290423 ) ) ;
#199771 = ORIENTED_EDGE ( 'NONE', *, *, #53249, .F. ) ;
#199772 = CARTESIAN_POINT ( 'NONE',  ( 12.25000000000000000, 47.91805600923871822, -233.7139610577891631 ) ) ;
#199773 = LINE ( 'NONE', #220603, #27911 ) ;
#199775 = ORIENTED_EDGE ( 'NONE', *, *, #63809, .T. ) ;
#199774 = AXIS2_PLACEMENT_3D ( 'NONE', #33919, #14332, #251631 ) ;
#199776 = DIRECTION ( 'NONE',  ( -1.000000000000000000, -0.000000000000000000, -0.000000000000000000 ) ) ;
#199777 = DIRECTION ( 'NONE',  ( -1.000000000000000000, -0.000000000000000000, -0.000000000000000000 ) ) ;
#199778 = CARTESIAN_POINT ( 'NONE',  ( -18.50000000000000000, 77.83585931145600512, -158.5186683157258187 ) ) ;
#199779 = EDGE_CURVE ( 'NONE', #208687, #93015, #200439, .T. ) ;
#199780 = EDGE_LOOP ( 'NONE', ( #213333, #254458, #61745, #255051, #82739 ) ) ;
#199781 = ADVANCED_FACE ( 'NONE', ( #79186 ), #227234, .F. ) ;
#199782 = EDGE_LOOP ( 'NONE', ( #121336, #12159, #154820, #168281 ) ) ;
#199783 = TOROIDAL_SURFACE ( 'NONE', #112296, 0.4000000000000005773, 0.1000000000000000056 ) ;
#199784 = DIRECTION ( 'NONE',  ( 0.000000000000000000, 0.000000000000000000, -1.000000000000000000 ) ) ;
#199785 = LINE ( 'NONE', #181499, #206705 ) ;
#199786 = DIRECTION ( 'NONE',  ( 0.000000000000000000, -1.000000000000000000, -6.982962677686266711E-15 ) ) ;
#199787 = DIRECTION ( 'NONE',  ( 0.000000000000000000, -6.982962677686266711E-15, 1.000000000000000000 ) ) ;
#199788 = AXIS2_PLACEMENT_3D ( 'NONE', #179013, #192435, #114171 ) ;
#199789 = EDGE_CURVE ( 'NONE', #216103, #255384, #2366, .T. ) ;
#199791 = DIRECTION ( 'NONE',  ( -1.000000000000000000, -0.000000000000000000, -0.000000000000000000 ) ) ;
#199790 = DIRECTION ( 'NONE',  ( 1.000000000000000000, -0.000000000000000000, -0.000000000000000000 ) ) ;
#199792 = DIRECTION ( 'NONE',  ( 0.000000000000000000, 0.4088369013362170290, -0.9126074666064267760 ) ) ;
#199793 = CARTESIAN_POINT ( 'NONE',  ( 22.49999999999999645, 75.90000000001222702, -148.1726782920690937 ) ) ;
#199794 = ORIENTED_EDGE ( 'NONE', *, *, #110435, .F. ) ;
#199795 = DIRECTION ( 'NONE',  ( -1.020425574104004196E-15, -0.000000000000000000, -1.000000000000000000 ) ) ;
#199796 = CIRCLE ( 'NONE', #145588, 0.1000000000000028644 ) ;
#199798 = VERTEX_POINT ( 'NONE', #21811 ) ;
#199797 = DIRECTION ( 'NONE',  ( -1.000000000000000000, 0.000000000000000000, 0.000000000000000000 ) ) ;
#199799 = CARTESIAN_POINT ( 'NONE',  ( 20.95561247346651967, 65.40499263480907643, -195.9293247175427837 ) ) ;
#199801 = CARTESIAN_POINT ( 'NONE',  ( -21.55000000000000071, 68.75000000001205080, -124.1731074845243370 ) ) ;
#199800 = CYLINDRICAL_SURFACE ( 'NONE', #241880, 0.5000000000000007772 ) ;
#199802 = VERTEX_POINT ( 'NONE', #77907 ) ;
#199804 = DIRECTION ( 'NONE',  ( 0.000000000000000000, 0.2128009952263582305, -0.9770955615653319493 ) ) ;
#199803 = DIRECTION ( 'NONE',  ( 1.000000000000000000, -7.304098846218134667E-16, -4.217023435051625732E-16 ) ) ;
#199805 = CARTESIAN_POINT ( 'NONE',  ( 18.59999999999999787, -8.250000000000005329, 10.50000000000000178 ) ) ;
#199806 = CARTESIAN_POINT ( 'NONE',  ( -5.999999999999938716, 64.65000000001120384, -22.12310748452479103 ) ) ;
#199807 = FACE_OUTER_BOUND ( 'NONE', #42489, .T. ) ;
#199808 = CARTESIAN_POINT ( 'NONE',  ( 18.59999999999997655, 1.115600667400684642E-11, -134.0000000000000284 ) ) ;
#199809 = ORIENTED_EDGE ( 'NONE', *, *, #227585, .T. ) ;
#199810 = CARTESIAN_POINT ( 'NONE',  ( -22.50000000000000000, 31.81502280147385164, -238.9558108736092095 ) ) ;
#199812 = ORIENTED_EDGE ( 'NONE', *, *, #77922, .T. ) ;
#199811 = AXIS2_PLACEMENT_3D ( 'NONE', #187286, #188545, #9903 ) ;
#199813 = ADVANCED_FACE ( 'NONE', ( #221261 ), #161326, .T. ) ;
#199814 = VECTOR ( 'NONE', #199315, 1000.000000000000000 ) ;
#199815 = CARTESIAN_POINT ( 'NONE',  ( -16.77683809663752257, 9.945835743215303282, -54.33605098089579855 ) ) ;
#199816 = ORIENTED_EDGE ( 'NONE', *, *, #196204, .T. ) ;
#199817 = DIRECTION ( 'NONE',  ( 1.000000000000000000, 0.000000000000000000, 0.000000000000000000 ) ) ;
#199818 = AXIS2_PLACEMENT_3D ( 'NONE', #149325, #33243, #230119 ) ;
#199819 = ORIENTED_EDGE ( 'NONE', *, *, #58559, .T. ) ;
#199820 =( BOUNDED_SURFACE ( )  B_SPLINE_SURFACE ( 3, 2, ( 
 ( #186304, #48058, #7666 ),
 ( #70227, #91043, #50611 ),
 ( #231855, #130156, #170636 ),
 ( #27255, #32388, #209709 ) ),
 .UNSPECIFIED., .F., .F., .T. ) 
 B_SPLINE_SURFACE_WITH_KNOTS ( ( 4, 4 ),
 ( 3, 3 ),
 ( 0.04058434257139457990, 0.04256401539001584966 ),
 ( 0.000000000000000000, 1.000000000000000000 ),
 .UNSPECIFIED. ) 
 GEOMETRIC_REPRESENTATION_ITEM ( )  RATIONAL_B_SPLINE_SURFACE ( (
 ( 1.000000000000000000, 0.7103081912007894738, 1.000000000000000000),
 ( 1.000000000000000000, 0.7104998333556562518, 1.000000000000000000),
 ( 1.000000000000000000, 0.7107238315754180746, 1.000000000000000000),
 ( 1.000000000000000000, 0.7110073749539692622, 1.000000000000000000) ) ) 
 REPRESENTATION_ITEM ( '' )  SURFACE ( )  );
#199821 = CARTESIAN_POINT ( 'NONE',  ( 20.95512820512820440, 8.876151316299271343, -176.0586289951409071 ) ) ;
#199822 = ADVANCED_FACE ( 'NONE', ( #100018 ), #60622, .T. ) ;
#199823 = FACE_OUTER_BOUND ( 'NONE', #168794, .T. ) ;
#199824 = ORIENTED_EDGE ( 'NONE', *, *, #232783, .T. ) ;
#199825 = EDGE_CURVE ( 'NONE', #104663, #130320, #118929, .T. ) ;
#199826 = ADVANCED_FACE ( 'NONE', ( #122196 ), #164704, .F. ) ;
#199827 = CARTESIAN_POINT ( 'NONE',  ( -21.05000000000000071, 1.162701749949165642, -75.10000000000003695 ) ) ;
#199828 = DIRECTION ( 'NONE',  ( 0.000000000000000000, 0.9126074666063767049, 0.4088369013363286619 ) ) ;
#199829 = CARTESIAN_POINT ( 'NONE',  ( -18.59999999999999787, 11.65000000001115232, -188.8499999999999659 ) ) ;
#199831 = CIRCLE ( 'NONE', #45681, 0.09999999999999530098 ) ;
#199830 = DIRECTION ( 'NONE',  ( -1.836970198721029934E-16, 1.000000000000000000, 0.000000000000000000 ) ) ;
#199832 = VECTOR ( 'NONE', #215559, 1000.000000000000000 ) ;
#199833 = CARTESIAN_POINT ( 'NONE',  ( 22.48970261584622321, 12.58107241917856634, -223.4371365001174752 ) ) ;
#199834 = ORIENTED_EDGE ( 'NONE', *, *, #218642, .T. ) ;
#199835 = CARTESIAN_POINT ( 'NONE',  ( -23.25000000000000000, 69.16514130714681130, -247.7543978865853660 ) ) ;
#199836 = ORIENTED_EDGE ( 'NONE', *, *, #107678, .T. ) ;
#199838 = ORIENTED_EDGE ( 'NONE', *, *, #111226, .F. ) ;
#199837 = SPHERICAL_SURFACE ( 'NONE', #19001, 0.1000000000000000056 ) ;
#199839 = EDGE_CURVE ( 'NONE', #239496, #35839, #80446, .T. ) ;
#199840 = ORIENTED_EDGE ( 'NONE', *, *, #92120, .F. ) ;
#199841 = CARTESIAN_POINT ( 'NONE',  ( 23.25000000000000000, 30.73962027982165424, -265.0781340245722504 ) ) ;
#199842 = ADVANCED_FACE ( 'NONE', ( #237005 ), #23104, .T. ) ;
#199843 = CARTESIAN_POINT ( 'NONE',  ( 23.14999999999999858, 67.92720994251783395, -214.1870976236629929 ) ) ;
#199844 = CARTESIAN_POINT ( 'NONE',  ( 15.75000000000000355, 66.65000000001258229, -187.0045385271217526 ) ) ;
#199845 = CARTESIAN_POINT ( 'NONE',  ( 20.94999999999999929, 1.115600667400684642E-11, -67.00000000000000000 ) ) ;
#199846 = DIRECTION ( 'NONE',  ( -0.000000000000000000, -0.1350103645451904977, 0.9908441862701596881 ) ) ;
#199847 = ORIENTED_EDGE ( 'NONE', *, *, #102568, .T. ) ;
#199848 = CARTESIAN_POINT ( 'NONE',  ( -20.64999999999999858, 48.98768910550766975, -253.5949463715719787 ) ) ;
#199849 = CARTESIAN_POINT ( 'NONE',  ( -16.85939591225058010, 66.09477352162440411, -157.0630392380553531 ) ) ;
#199850 = ORIENTED_EDGE ( 'NONE', *, *, #254307, .T. ) ;
#199851 = CARTESIAN_POINT ( 'NONE',  ( -23.15000000000000213, 87.65000000001195701, -103.0231074845242318 ) ) ;
#199852 = AXIS2_PLACEMENT_3D ( 'NONE', #42052, #163279, #221922 ) ;
#199853 = EDGE_CURVE ( 'NONE', #139155, #194632, #242119, .T. ) ;
#199854 = CIRCLE ( 'NONE', #233174, 0.3999999999999994671 ) ;
#199855 = TOROIDAL_SURFACE ( 'NONE', #87385, 0.4000000000000005773, 0.1000000000000000056 ) ;
#199856 = FACE_OUTER_BOUND ( 'NONE', #110814, .T. ) ;
#199857 = ORIENTED_EDGE ( 'NONE', *, *, #189790, .F. ) ;
#199858 = CARTESIAN_POINT ( 'NONE',  ( 21.05000000000000071, 61.00620644593068675, -234.0632213031365438 ) ) ;
#199859 = EDGE_CURVE ( 'NONE', #178238, #56894, #177391, .T. ) ;
#199860 = CIRCLE ( 'NONE', #141742, 0.1000000000000028644 ) ;
#199861 = CARTESIAN_POINT ( 'NONE',  ( 20.99551997958429794, 64.25000000001158185, -109.8714483468354928 ) ) ;
#199862 = ORIENTED_EDGE ( 'NONE', *, *, #33504, .F. ) ;
#199863 = DIRECTION ( 'NONE',  ( 1.000000000000000000, 0.000000000000000000, 0.000000000000000000 ) ) ;
#199864 = EDGE_CURVE ( 'NONE', #82161, #85729, #197859, .T. ) ;
#199865 = FACE_OUTER_BOUND ( 'NONE', #238197, .T. ) ;
#199866 =( BOUNDED_SURFACE ( )  B_SPLINE_SURFACE ( 3, 2, ( 
 ( #34595, #232794, #228930 ),
 ( #54124, #193655, #174130 ),
 ( #15027, #72436, #29478 ),
 ( #192368, #13726, #253601 ) ),
 .UNSPECIFIED., .F., .F., .F. ) 
 B_SPLINE_SURFACE_WITH_KNOTS ( ( 4, 4 ),
 ( 3, 3 ),
 ( 0.0006461284895273765793, 0.0007503702773986202284 ),
 ( 0.000000000000000000, 1.000000000000000000 ),
 .UNSPECIFIED. ) 
 GEOMETRIC_REPRESENTATION_ITEM ( )  RATIONAL_B_SPLINE_SURFACE ( (
 ( 1.000000000000000000, 0.7071067811865475727, 1.000000000000000000),
 ( 1.000000000000000000, 0.7076476444649162367, 1.000000000000000000),
 ( 1.000000000000000000, 0.7075727925191654943, 1.000000000000000000),
 ( 1.000000000000000000, 0.7071067811865581199, 1.000000000000000000) ) ) 
 REPRESENTATION_ITEM ( '' )  SURFACE ( )  );
#199867 = CYLINDRICAL_SURFACE ( 'NONE', #21885, 0.1000000000000028644 ) ;
#199868 = ADVANCED_FACE ( 'NONE', ( #25654 ), #85577, .F. ) ;
#199869 = TOROIDAL_SURFACE ( 'NONE', #112725, 4.099999999999999645, 0.1000000000000000056 ) ;
#199870 = EDGE_CURVE ( 'NONE', #153115, #16503, #169025, .T. ) ;
#199871 = VECTOR ( 'NONE', #28666, 1000.000000000000000 ) ;
#199872 = EDGE_CURVE ( 'NONE', #70203, #8870, #26964, .T. ) ;
#199873 = VECTOR ( 'NONE', #62130, 1000.000000000000114 ) ;
#199874 = ORIENTED_EDGE ( 'NONE', *, *, #116606, .F. ) ;
#199875 = FILL_AREA_STYLE_COLOUR ( '', #215377 ) ;
#199876 = VERTEX_POINT ( 'NONE', #46476 ) ;
#199877 = CARTESIAN_POINT ( 'NONE',  ( 20.27550659511088682, 19.63441466210375808, -229.9765866052221099 ) ) ;
#199878 = CARTESIAN_POINT ( 'NONE',  ( 23.15000000000000213, 87.75000000001173817, -72.62310748452422615 ) ) ;
#199880 = ORIENTED_EDGE ( 'NONE', *, *, #204784, .T. ) ;
#199879 = DIRECTION ( 'NONE',  ( -1.000000000000000000, 0.000000000000000000, 0.000000000000000000 ) ) ;
#199881 = FACE_OUTER_BOUND ( 'NONE', #147670, .T. ) ;
#199882 = EDGE_CURVE ( 'NONE', #104351, #21018, #106412, .T. ) ;
#199883 = DIRECTION ( 'NONE',  ( 0.000000000000000000, 0.000000000000000000, -1.000000000000000000 ) ) ;
#199884 = CARTESIAN_POINT ( 'NONE',  ( 21.14999999999999858, 76.00000000001200817, -109.5637644362255685 ) ) ;
#199885 = CARTESIAN_POINT ( 'NONE',  ( -23.15000000000000213, 74.00000000001205080, -123.2984855617622060 ) ) ;
#199886 = EDGE_CURVE ( 'NONE', #107706, #78910, #126020, .T. ) ;
#199887 = CARTESIAN_POINT ( 'NONE',  ( -18.59999999999999787, 66.75000000001205080, -124.1731074845243654 ) ) ;
#199888 = DIRECTION ( 'NONE',  ( 1.000000000000000000, 0.000000000000000000, 0.000000000000000000 ) ) ;
#199890 = ORIENTED_EDGE ( 'NONE', *, *, #228911, .F. ) ;
#199889 = CARTESIAN_POINT ( 'NONE',  ( -23.15000000000000213, 71.85000000001224407, -148.8731074845244109 ) ) ;
#199891 = AXIS2_PLACEMENT_3D ( 'NONE', #119344, #80171, #60626 ) ;
#199892 = DIRECTION ( 'NONE',  ( -1.000000000000000000, -1.836970198721029934E-16, 0.000000000000000000 ) ) ;
#199893 = ORIENTED_EDGE ( 'NONE', *, *, #90581, .T. ) ;
#199894 = ORIENTED_EDGE ( 'NONE', *, *, #50415, .F. ) ;
#199895 = VECTOR ( 'NONE', #174739, 1000.000000000000000 ) ;
#199896 = CARTESIAN_POINT ( 'NONE',  ( -18.33981767444248945, 85.56957578981656809, -62.70394564079953881 ) ) ;
#199897 = CARTESIAN_POINT ( 'NONE',  ( 21.00023020733438273, 69.60913075474422840, -103.0231074845243597 ) ) ;
#199898 = VECTOR ( 'NONE', #79234, 1000.000000000000000 ) ;
#199899 = ORIENTED_EDGE ( 'NONE', *, *, #111600, .T. ) ;
#199900 = CYLINDRICAL_SURFACE ( 'NONE', #104246, 0.1000000000000000472 ) ;
#199901 = CARTESIAN_POINT ( 'NONE',  ( -18.54159361262948735, 85.46313213550472199, -62.47398526823135967 ) ) ;
#199902 = ADVANCED_FACE ( 'NONE', ( #86877 ), #8654, .F. ) ;
#199903 = EDGE_LOOP ( 'NONE', ( #126786, #68259, #185182, #107507 ) ) ;
#199904 = AXIS2_PLACEMENT_3D ( 'NONE', #66387, #162939, #121267 ) ;
#199906 = ADVANCED_FACE ( 'NONE', ( #105136 ), #186007, .T. ) ;
#199905 = CARTESIAN_POINT ( 'NONE',  ( -20.94999999999999929, 65.70729864260985664, -64.06574559737245522 ) ) ;
#199907 = AXIS2_PLACEMENT_3D ( 'NONE', #233208, #136630, #234450 ) ;
#199908 = CARTESIAN_POINT ( 'NONE',  ( -16.93302609847409457, 66.00331747920938597, -190.9367189891619034 ) ) ;
#199909 = VERTEX_POINT ( 'NONE', #29534 ) ;
#199910 = ORIENTED_EDGE ( 'NONE', *, *, #192441, .F. ) ;
#199911 = DIRECTION ( 'NONE',  ( 0.000000000000000000, -0.9908441862701600211, -0.1350103645451876666 ) ) ;
#199912 = AXIS2_PLACEMENT_3D ( 'NONE', #164778, #81348, #240458 ) ;
#199913 = VERTEX_POINT ( 'NONE', #127317 ) ;
#199914 = CARTESIAN_POINT ( 'NONE',  ( -20.54999999999999716, -8.663551401858001100, -90.97589888193274987 ) ) ;
#199915 = EDGE_LOOP ( 'NONE', ( #178340, #163461, #170851, #195374 ) ) ;
#199917 = ORIENTED_EDGE ( 'NONE', *, *, #126510, .T. ) ;
#199916 = DIRECTION ( 'NONE',  ( 0.000000000000000000, -0.4930308989874653269, -0.8700118002898649117 ) ) ;
#199918 = AXIS2_PLACEMENT_3D ( 'NONE', #168022, #148427, #11486 ) ;
#199919 = CIRCLE ( 'NONE', #170739, 0.09999999999999939493 ) ;
#199920 = CARTESIAN_POINT ( 'NONE',  ( 23.25000000000000000, 24.26958830762006514, -252.6664436919618879 ) ) ;
#199921 = VERTEX_POINT ( 'NONE', #6071 ) ;
#199922 = CARTESIAN_POINT ( 'NONE',  ( -21.53699400384214968, 1.542889524662434004E-12, -93.71228820675507620 ) ) ;
#199923 = ORIENTED_EDGE ( 'NONE', *, *, #21518, .F. ) ;
#199925 = ORIENTED_EDGE ( 'NONE', *, *, #90199, .F. ) ;
#199924 = VERTEX_POINT ( 'NONE', #166476 ) ;
#199926 = DIRECTION ( 'NONE',  ( -0.000000000000000000, -1.000000000000000000, -0.000000000000000000 ) ) ;
#199927 = ADVANCED_FACE ( 'NONE', ( #67342 ), #56520, .F. ) ;
#199928 = CARTESIAN_POINT ( 'NONE',  ( -20.64999999999999858, 71.65000000001228386, -157.7731074845243882 ) ) ;
#199929 = ORIENTED_EDGE ( 'NONE', *, *, #176981, .T. ) ;
#199930 = CIRCLE ( 'NONE', #170929, 0.1000000000000028783 ) ;
#199931 = VECTOR ( 'NONE', #152708, 1000.000000000000000 ) ;
#199932 = CIRCLE ( 'NONE', #54156, 0.09999999999999939493 ) ;
#199933 = AXIS2_PLACEMENT_3D ( 'NONE', #3061, #159596, #142574 ) ;
#199934 = VECTOR ( 'NONE', #247821, 999.9999999999998863 ) ;
#199935 = ORIENTED_EDGE ( 'NONE', *, *, #246388, .F. ) ;
#199937 = AXIS2_PLACEMENT_3D ( 'NONE', #220843, #202575, #183027 ) ;
#199936 = CARTESIAN_POINT ( 'NONE',  ( 20.95512820512820440, 67.12384868372345181, -57.37310748452438247 ) ) ;
#199938 = CYLINDRICAL_SURFACE ( 'NONE', #1401, 11.74999999999999112 ) ;
#199940 = ORIENTED_EDGE ( 'NONE', *, *, #256561, .F. ) ;
#199939 = CYLINDRICAL_SURFACE ( 'NONE', #20079, 0.09999999999998898659 ) ;
#199941 = CYLINDRICAL_SURFACE ( 'NONE', #64630, 0.09999999999999939493 ) ;
#199942 = ORIENTED_EDGE ( 'NONE', *, *, #159394, .F. ) ;
#199943 = DIRECTION ( 'NONE',  ( 0.000000000000000000, 0.8814952561688444987, -0.4721928772777320149 ) ) ;
#199944 = CYLINDRICAL_SURFACE ( 'NONE', #177100, 0.1000000000000050432 ) ;
#199945 = VERTEX_POINT ( 'NONE', #188569 ) ;
#199946 = CARTESIAN_POINT ( 'NONE',  ( -23.15000000000000213, 4.350000000011156054, -88.15000000000004832 ) ) ;
#199947 = FACE_OUTER_BOUND ( 'NONE', #142071, .T. ) ;
#199948 = DIRECTION ( 'NONE',  ( 0.000000000000000000, -6.853228547068871147E-15, 1.000000000000000000 ) ) ;
#199949 = ORIENTED_EDGE ( 'NONE', *, *, #223539, .F. ) ;
#199950 = FACE_OUTER_BOUND ( 'NONE', #220123, .T. ) ;
#199951 = VERTEX_POINT ( 'NONE', #47758 ) ;
#199952 = ORIENTED_EDGE ( 'NONE', *, *, #142900, .T. ) ;
#199953 = DIRECTION ( 'NONE',  ( 0.000000000000000000, 0.000000000000000000, -1.000000000000000000 ) ) ;
#199954 = ORIENTED_EDGE ( 'NONE', *, *, #32682, .F. ) ;
#199955 = ORIENTED_EDGE ( 'NONE', *, *, #218446, .T. ) ;
#199956 = DIRECTION ( 'NONE',  ( 1.000000000000000000, 1.186688945009010077E-16, 0.000000000000000000 ) ) ;
#199957 = CARTESIAN_POINT ( 'NONE',  ( -21.05000000000000071, 1.162701749938009677, -7.900000000000000355 ) ) ;
#199958 = ORIENTED_EDGE ( 'NONE', *, *, #101345, .T. ) ;
#199959 = EDGE_LOOP ( 'NONE', ( #244348, #178470, #211101 ) ) ;
#199960 = CARTESIAN_POINT ( 'NONE',  ( 21.05000000000000071, 62.82351852614503684, -207.2177435922979214 ) ) ;
#199961 = FACE_OUTER_BOUND ( 'NONE', #67268, .T. ) ;
#199962 = ORIENTED_EDGE ( 'NONE', *, *, #29048, .T. ) ;
#199963 = CIRCLE ( 'NONE', #45823, 4.149999999999999467 ) ;
#199964 = EDGE_CURVE ( 'NONE', #257664, #129332, #202303, .T. ) ;
#199965 = ORIENTED_EDGE ( 'NONE', *, *, #113571, .F. ) ;
#199966 = ORIENTED_EDGE ( 'NONE', *, *, #185596, .T. ) ;
#199967 = AXIS2_PLACEMENT_3D ( 'NONE', #39068, #155180, #179858 ) ;
#199968 = EDGE_CURVE ( 'NONE', #4930, #173330, #85550, .T. ) ;
#199969 = CYLINDRICAL_SURFACE ( 'NONE', #90760, 0.5000000000000004441 ) ;
#199970 = EDGE_CURVE ( 'NONE', #225394, #80895, #131377, .T. ) ;
#199971 = LINE ( 'NONE', #63004, #251182 ) ;
#199972 = CARTESIAN_POINT ( 'NONE',  ( -20.99780126800919078, 11.60538868788780498, -127.0873525717055657 ) ) ;
#199973 = DIRECTION ( 'NONE',  ( 0.000000000000000000, 0.000000000000000000, -1.000000000000000000 ) ) ;
#199974 = AXIS2_PLACEMENT_3D ( 'NONE', #160609, #200992, #202277 ) ;
#199975 = CARTESIAN_POINT ( 'NONE',  ( -22.50000000000000000, 0.000000000000000000, 0.000000000000000000 ) ) ;
#199976 = DIRECTION ( 'NONE',  ( 1.000000000000000000, 3.265361837132813093E-16, -0.000000000000000000 ) ) ;
#199977 = TOROIDAL_SURFACE ( 'NONE', #183408, 4.099999999999999645, 0.1000000000000000056 ) ;
#199978 = CARTESIAN_POINT ( 'NONE',  ( -20.64999999999999858, 26.18196512540240661, -241.1028522842020152 ) ) ;
#199979 = DIRECTION ( 'NONE',  ( 0.000000000000000000, -0.2128009952263403282, 0.9770955615653358350 ) ) ;
#199980 = CYLINDRICAL_SURFACE ( 'NONE', #161267, 0.1000000000000028644 ) ;
#199981 = EDGE_CURVE ( 'NONE', #228509, #121064, #152259, .T. ) ;
#199982 = DIRECTION ( 'NONE',  ( 1.000000000000000000, 0.000000000000000000, 0.000000000000000000 ) ) ;
#199983 = CARTESIAN_POINT ( 'NONE',  ( -23.25000000000000000, 65.66751761918668251, -97.42826094061121012 ) ) ;
#199984 = AXIS2_PLACEMENT_3D ( 'NONE', #251950, #65306, #143558 ) ;
#199985 = VERTEX_POINT ( 'NONE', #169050 ) ;
#199986 = CIRCLE ( 'NONE', #112503, 0.3999999999999952482 ) ;
#199988 = EDGE_LOOP ( 'NONE', ( #229070, #184213, #133159, #38147 ) ) ;
#199987 = LINE ( 'NONE', #467, #115773 ) ;
#199990 = EDGE_CURVE ( 'NONE', #88287, #40232, #248544, .T. ) ;
#199989 = DIRECTION ( 'NONE',  ( -0.7071067811865474617, -0.7071067811865474617, -0.000000000000000000 ) ) ;
#199991 = CARTESIAN_POINT ( 'NONE',  ( -20.94999999999999929, 87.41227409416113403, -38.92310748452424463 ) ) ;
#199992 = ORIENTED_EDGE ( 'NONE', *, *, #40442, .F. ) ;
#199994 = AXIS2_PLACEMENT_3D ( 'NONE', #75242, #154781, #234276 ) ;
#199993 = DIRECTION ( 'NONE',  ( 0.5000000000001141309, -6.047423072554455661E-15, 0.8660254037843729824 ) ) ;
#199995 = AXIS2_PLACEMENT_3D ( 'NONE', #90160, #128035, #148887 ) ;
#199996 = DIRECTION ( 'NONE',  ( -0.000000000000000000, 6.982962677686266711E-15, -1.000000000000000000 ) ) ;
#199997 = EDGE_LOOP ( 'NONE', ( #71930, #244438, #236149, #166018 ) ) ;
#199998 = CARTESIAN_POINT ( 'NONE',  ( -20.54999999999999716, 76.00000000001244871, -170.0231074845243597 ) ) ;
#199999 = CARTESIAN_POINT ( 'NONE',  ( -21.05000000000000071, 0.5876173420563349792, -209.1618981382189588 ) ) ;
#200000 = DIRECTION ( 'NONE',  ( 0.000000000000000000, -1.000000000000000000, -7.109473446599835262E-15 ) ) ;
#200001 = DIRECTION ( 'NONE',  ( -1.000000000000000000, -1.836970198721029934E-16, 0.000000000000000000 ) ) ;
#200003 = ORIENTED_EDGE ( 'NONE', *, *, #64526, .T. ) ;
#200002 = CARTESIAN_POINT ( 'NONE',  ( -21.05000000000000071, 76.00000000001126921, -203.5231074845248997 ) ) ;
#200005 = ORIENTED_EDGE ( 'NONE', *, *, #207778, .F. ) ;
#200004 = CARTESIAN_POINT ( 'NONE',  ( 22.39999999999999503, 64.35000000001267040, -203.4231074845244507 ) ) ;
#200006 = CARTESIAN_POINT ( 'NONE',  ( -18.50000000000000000, 76.00000000001190870, -103.0231074845243029 ) ) ;
#200007 = DIRECTION ( 'NONE',  ( 0.000000000000000000, -0.2617529984165152257, -0.9651348961777124202 ) ) ;
#200008 = DIRECTION ( 'NONE',  ( -1.000000000000000000, -2.952720810173289112E-16, 0.000000000000000000 ) ) ;
#200009 = LINE ( 'NONE', #38367, #23763 ) ;
#200010 = VECTOR ( 'NONE', #203020, 1000.000000000000000 ) ;
#200013 = CARTESIAN_POINT ( 'NONE',  ( -21.05000000000000071, 1.148907358139439339E-11, -201.0000000000015064 ) ) ;
#200012 = AXIS2_PLACEMENT_3D ( 'NONE', #151615, #215405, #137156 ) ;
#200011 = CARTESIAN_POINT ( 'NONE',  ( -16.93860193097148326, 63.05725141050672278, -213.0679477116501062 ) ) ;
#200014 = CARTESIAN_POINT ( 'NONE',  ( -21.05000000000000426, 34.10212959586274195, -243.5992781215346099 ) ) ;
#200015 = DIRECTION ( 'NONE',  ( 0.000000000000000000, -0.4088369013362965210, 0.9126074666063913599 ) ) ;
#200016 = AXIS2_PLACEMENT_3D ( 'NONE', #2084, #218562, #137742 ) ;
#200017 = CIRCLE ( 'NONE', #162429, 0.09999999999999938105 ) ;
#200018 = CARTESIAN_POINT ( 'NONE',  ( -20.95613430942426092, 64.25000000001233502, -163.1659448363049876 ) ) ;
#200019 = FACE_OUTER_BOUND ( 'NONE', #137458, .T. ) ;
#200020 = CARTESIAN_POINT ( 'NONE',  ( 18.59999999999997655, 76.00000000001239187, -162.1231074845243825 ) ) ;
#200021 = ORIENTED_EDGE ( 'NONE', *, *, #189146, .T. ) ;
#200022 = EDGE_CURVE ( 'NONE', #47766, #209877, #225107, .T. ) ;
#200023 = CARTESIAN_POINT ( 'NONE',  ( -21.05000000000000071, 7.128833340093095217, -233.7327013124392749 ) ) ;
#200024 = CIRCLE ( 'NONE', #62656, 0.5000000000000051070 ) ;
#200025 = ORIENTED_EDGE ( 'NONE', *, *, #47657, .T. ) ;
#200026 = EDGE_LOOP ( 'NONE', ( #154766, #218560, #28822, #144065 ) ) ;
#200027 = CARTESIAN_POINT ( 'NONE',  ( 20.58091095332318332, 66.98152984665945553, -94.60445730236581596 ) ) ;
#200028 = FACE_OUTER_BOUND ( 'NONE', #63522, .T. ) ;
#200029 = EDGE_LOOP ( 'NONE', ( #198550, #238882, #31157, #16393 ) ) ;
#200030 = EDGE_CURVE ( 'NONE', #220609, #82047, #231354, .T. ) ;
#200031 = ORIENTED_EDGE ( 'NONE', *, *, #181647, .T. ) ;
#200032 = AXIS2_PLACEMENT_3D ( 'NONE', #91150, #52005, #213666 ) ;
#200033 = EDGE_CURVE ( 'NONE', #242376, #56828, #84277, .T. ) ;
#200034 =( NAMED_UNIT ( * ) SI_UNIT ( $, .STERADIAN. ) SOLID_ANGLE_UNIT ( ) );
#200035 = EDGE_CURVE ( 'NONE', #74293, #51580, #45207, .T. ) ;
#200036 = ORIENTED_EDGE ( 'NONE', *, *, #103644, .F. ) ;
#200037 = CARTESIAN_POINT ( 'NONE',  ( -21.05000000000000071, 87.75000000001192291, -105.9231074845242091 ) ) ;
#200038 = VERTEX_POINT ( 'NONE', #133729 ) ;
#200039 = CARTESIAN_POINT ( 'NONE',  ( 20.85000000000000142, -1.835859311432481045, -112.0044391687985694 ) ) ;
#200040 = CARTESIAN_POINT ( 'NONE',  ( 18.59999999999999076, 67.75954444190071513, -227.8703747234148693 ) ) ;
#200041 = CARTESIAN_POINT ( 'NONE',  ( 20.85000000000000142, 76.00000000001170974, -69.52310748452431710 ) ) ;
#200042 = CARTESIAN_POINT ( 'NONE',  ( -23.15000000000000213, 85.00000000001159606, -59.62913836187181715 ) ) ;
#200043 = CARTESIAN_POINT ( 'NONE',  ( -18.40000000000000213, 64.52683809665003878, -179.3490535513324176 ) ) ;
#200044 = EDGE_CURVE ( 'NONE', #243903, #3898, #234111, .T. ) ;
#200045 = FACE_OUTER_BOUND ( 'NONE', #153475, .T. ) ;
#200046 = DIRECTION ( 'NONE',  ( 0.000000000000000000, 0.8814952561688437216, -0.4721928772777334582 ) ) ;
#200048 = ORIENTED_EDGE ( 'NONE', *, *, #179235, .T. ) ;
#200047 = CARTESIAN_POINT ( 'NONE',  ( -22.42357213249529124, 75.90091303601015227, -77.19603987088426322 ) ) ;
#200049 = CARTESIAN_POINT ( 'NONE',  ( -20.94999999999999929, 11.65000000001115588, -107.5148057706540357 ) ) ;
#200050 = EDGE_CURVE ( 'NONE', #147041, #256686, #235394, .T. ) ;
#200051 = DIRECTION ( 'NONE',  ( 0.000000000000000000, 0.000000000000000000, -1.000000000000000000 ) ) ;
#200052 = ORIENTED_EDGE ( 'NONE', *, *, #57281, .F. ) ;
#200053 = DIRECTION ( 'NONE',  ( 1.000000000000000000, 0.000000000000000000, 0.000000000000000000 ) ) ;
#200054 = EDGE_CURVE ( 'NONE', #235865, #188797, #223136, .T. ) ;
#200055 = VERTEX_POINT ( 'NONE', #12530 ) ;
#200057 = CARTESIAN_POINT ( 'NONE',  ( 23.24999999999999645, 5.600000000011153389, -122.2500000000000284 ) ) ;
#200056 = PLANE ( 'NONE',  #194874 ) ;
#200058 = VECTOR ( 'NONE', #164890, 1000.000000000000000 ) ;
#200059 = CARTESIAN_POINT ( 'NONE',  ( -22.14074124539699895, 75.90094710416794044, -110.4131853355680875 ) ) ;
#200060 = CARTESIAN_POINT ( 'NONE',  ( 21.14999999999999503, 76.10085836911075319, -114.7726746080137019 ) ) ;
#200061 = ORIENTED_EDGE ( 'NONE', *, *, #92103, .T. ) ;
#200062 = CYLINDRICAL_SURFACE ( 'NONE', #132596, 0.09999999999999939493 ) ;
#200063 = EDGE_CURVE ( 'NONE', #52101, #227362, #110724, .T. ) ;
#200065 = CYLINDRICAL_SURFACE ( 'NONE', #61724, 0.09999999999999939493 ) ;
#200064 = AXIS2_PLACEMENT_3D ( 'NONE', #174431, #72747, #153583 ) ;
#200066 = CARTESIAN_POINT ( 'NONE',  ( 23.15000000000000213, -11.74999999998883737, -112.7500000000000284 ) ) ;
#200067 = EDGE_CURVE ( 'NONE', #172693, #121283, #39825, .T. ) ;
#200068 = EDGE_LOOP ( 'NONE', ( #162431, #61351, #166380, #233565 ) ) ;
#200069 = EDGE_CURVE ( 'NONE', #66389, #71706, #94597, .T. ) ;
#200070 = CARTESIAN_POINT ( 'NONE',  ( -16.91049119928362643, 66.05000000001255955, -182.6413870913335700 ) ) ;
#200071 = CARTESIAN_POINT ( 'NONE',  ( 20.05000000000002913, 68.75000000001260503, -194.2731074845244166 ) ) ;
#200072 = CARTESIAN_POINT ( 'NONE',  ( 17.74533788810830259, 65.18150020854118054, -113.3367301594719407 ) ) ;
#200073 = VECTOR ( 'NONE', #122201, 1000.000000000000000 ) ;
#200074 = DIRECTION ( 'NONE',  ( 1.000000000000000000, 0.000000000000000000, 0.000000000000000000 ) ) ;
#200076 = DIRECTION ( 'NONE',  ( 0.000000000000000000, 0.000000000000000000, 1.000000000000000000 ) ) ;
#200075 = AXIS2_PLACEMENT_3D ( 'NONE', #249866, #68670, #149509 ) ;
#200078 = EDGE_LOOP ( 'NONE', ( #102589, #101350, #75817 ) ) ;
#200077 = DIRECTION ( 'NONE',  ( 0.000000000000000000, 1.000000000000000000, 0.000000000000000000 ) ) ;
#200079 = CARTESIAN_POINT ( 'NONE',  ( -21.14999999999999858, 36.65892442174472876, -249.5511627012454596 ) ) ;
#200081 = EDGE_CURVE ( 'NONE', #173524, #75404, #252167, .T. ) ;
#200080 = CARTESIAN_POINT ( 'NONE',  ( -21.44999999999999929, 68.65000000001253966, -182.3731074845244109 ) ) ;
#200082 = DIRECTION ( 'NONE',  ( 0.000000000000000000, -0.000000000000000000, -1.000000000000000000 ) ) ;
#200083 = CIRCLE ( 'NONE', #141800, 0.1000000000000028644 ) ;
#200084 = DIRECTION ( 'NONE',  ( 0.000000000000000000, 0.9908441862701596881, -0.1350103645451904977 ) ) ;
#200085 = ADVANCED_FACE ( 'NONE', ( #32093 ), #27383, .T. ) ;
#200086 = DIRECTION ( 'NONE',  ( -1.000000000000000000, 0.000000000000000000, 0.000000000000000000 ) ) ;
#200088 = ORIENTED_EDGE ( 'NONE', *, *, #103803, .F. ) ;
#200087 = DIRECTION ( 'NONE',  ( 0.000000000000000000, 0.9126074666063764829, 0.4088369013363294391 ) ) ;
#200089 = DIRECTION ( 'NONE',  ( 0.000000000000000000, 0.000000000000000000, 1.000000000000000000 ) ) ;
#200090 = VECTOR ( 'NONE', #231194, 1000.000000000000114 ) ;
#200091 = DIRECTION ( 'NONE',  ( 0.000000000000000000, -1.000000000000000000, 0.000000000000000000 ) ) ;
#200092 = CARTESIAN_POINT ( 'NONE',  ( 20.94999027547553894, 67.49459761544871128, -195.5598716110968951 ) ) ;
#200093 = ORIENTED_EDGE ( 'NONE', *, *, #215253, .F. ) ;
#200094 = DIRECTION ( 'NONE',  ( 1.000000000000000000, 0.000000000000000000, 0.000000000000000000 ) ) ;
#200095 = CARTESIAN_POINT ( 'NONE',  ( -20.90000000000000213, 1.885425182446133885, -11.49641995933507843 ) ) ;
#200096 = CARTESIAN_POINT ( 'NONE',  ( -21.04999999999994387, 74.94272479589878344, -8.023107484524793165 ) ) ;
#200097 = EDGE_CURVE ( 'NONE', #225545, #47226, #219037, .T. ) ;
#200098 = CARTESIAN_POINT ( 'NONE',  ( -18.79999999999999716, 8.000000000000000000, 1.212568896937007867 ) ) ;
#200099 = CIRCLE ( 'NONE', #87649, 0.09999999999999990841 ) ;
#200100 = CIRCLE ( 'NONE', #87650, 0.1000000000000060424 ) ;
#200102 = EDGE_LOOP ( 'NONE', ( #2146, #217498, #149088, #101115 ) ) ;
#200101 = CIRCLE ( 'NONE', #112794, 0.2000000000000057288 ) ;
#200103 = ORIENTED_EDGE ( 'NONE', *, *, #35358, .T. ) ;
#200104 = TOROIDAL_SURFACE ( 'NONE', #33737, 0.2000000000000000111, 0.1000000000000000056 ) ;
#200105 = CARTESIAN_POINT ( 'NONE',  ( -23.25000000000000000, -1.835859311432481045, -112.0044391687985694 ) ) ;
#200106 = CARTESIAN_POINT ( 'NONE',  ( -20.90000000000000213, -11.75000000000000000, 11.89999999999999858 ) ) ;
#200107 = DIRECTION ( 'NONE',  ( -1.000000000000000000, -0.000000000000000000, -0.000000000000000000 ) ) ;
#200108 = CARTESIAN_POINT ( 'NONE',  ( -23.15000000000000213, 7.128833340094563376, -233.7327013124401276 ) ) ;
#200109 = ORIENTED_EDGE ( 'NONE', *, *, #103968, .F. ) ;
#200110 = CARTESIAN_POINT ( 'NONE',  ( 20.95566103547454517, 10.61824765095822087, -175.1318401929805475 ) ) ;
#200111 = EDGE_CURVE ( 'NONE', #224306, #68117, #194137, .T. ) ;
#200112 = CARTESIAN_POINT ( 'NONE',  ( 20.94999999999999929, -9.399999999988844834, -90.60603087734760663 ) ) ;
#200113 = AXIS2_PLACEMENT_3D ( 'NONE', #144756, #87353, #65236 ) ;
#200114 = FACE_OUTER_BOUND ( 'NONE', #242252, .T. ) ;
#200115 = EDGE_CURVE ( 'NONE', #178346, #252694, #173320, .T. ) ;
#200116 = CARTESIAN_POINT ( 'NONE',  ( 20.95203847575071521, 10.50106053928516303, -108.0670713486235996 ) ) ;
#200117 = DIRECTION ( 'NONE',  ( 0.000000000000000000, 1.000000000000000000, 0.000000000000000000 ) ) ;
#200118 = EDGE_LOOP ( 'NONE', ( #47834, #239995, #45699 ) ) ;
#200120 = ORIENTED_EDGE ( 'NONE', *, *, #31213, .F. ) ;
#200119 = DIRECTION ( 'NONE',  ( 2.952720810173289112E-16, -1.000000000000000000, 0.000000000000000000 ) ) ;
#200121 = ADVANCED_FACE ( 'NONE', ( #252377 ), #231561, .F. ) ;
#200122 = ORIENTED_EDGE ( 'NONE', *, *, #47769, .T. ) ;
#200123 = DIRECTION ( 'NONE',  ( -0.000000000000000000, -0.000000000000000000, -1.000000000000000000 ) ) ;
#200124 = EDGE_CURVE ( 'NONE', #222419, #144818, #134994, .T. ) ;
#200125 = ORIENTED_EDGE ( 'NONE', *, *, #208654, .T. ) ;
#200126 = CARTESIAN_POINT ( 'NONE',  ( -18.50000000000000000, 68.97833521811159585, -65.68954208262705663 ) ) ;
#200127 = CARTESIAN_POINT ( 'NONE',  ( -21.05000000000000071, 6.304961112695925074, -100.5213855659375639 ) ) ;
#200128 = CARTESIAN_POINT ( 'NONE',  ( 19.75857864376268935, 11.75000000001115907, -58.35000000000000142 ) ) ;
#200129 = EDGE_LOOP ( 'NONE', ( #56550, #50582, #189722, #114525 ) ) ;
#200130 = CARTESIAN_POINT ( 'NONE',  ( 21.05000000000000071, 6.650000000011155876, -43.51702717044002355 ) ) ;
#200132 = EDGE_CURVE ( 'NONE', #106580, #59743, #95878, .T. ) ;
#200131 = FACE_OUTER_BOUND ( 'NONE', #28103, .T. ) ;
#200134 = ORIENTED_EDGE ( 'NONE', *, *, #67657, .T. ) ;
#200133 = AXIS2_PLACEMENT_3D ( 'NONE', #75788, #34127, #113621 ) ;
#200135 = CARTESIAN_POINT ( 'NONE',  ( -15.57281606413133090, 9.370655051134637148, -151.5258232559808675 ) ) ;
#200137 = ORIENTED_EDGE ( 'NONE', *, *, #113908, .T. ) ;
#200136 = FACE_OUTER_BOUND ( 'NONE', #65069, .T. ) ;
#200138 = CARTESIAN_POINT ( 'NONE',  ( -23.25000000000000000, 64.35000000001238618, -170.0231074845244166 ) ) ;
#200139 = CARTESIAN_POINT ( 'NONE',  ( -18.40000000000000213, 23.82801463864234037, -229.3483719500187306 ) ) ;
#200140 = CIRCLE ( 'NONE', #87687, 0.2000000000000057288 ) ;
#200141 = EDGE_CURVE ( 'NONE', #14757, #117904, #11228, .T. ) ;
#200142 = EDGE_CURVE ( 'NONE', #42422, #233341, #35939, .T. ) ;
#200143 = ORIENTED_EDGE ( 'NONE', *, *, #133221, .T. ) ;
#200144 = DIRECTION ( 'NONE',  ( 1.000000000000000000, 0.000000000000000000, 0.000000000000000000 ) ) ;
#200145 = LINE ( 'NONE', #201415, #112956 ) ;
#200146 = CIRCLE ( 'NONE', #145965, 1.900000000000012790 ) ;
#200147 = CARTESIAN_POINT ( 'NONE',  ( -18.40000000000000213, 64.25000000001188027, -90.37310748452439668 ) ) ;
#200148 = ORIENTED_EDGE ( 'NONE', *, *, #225381, .T. ) ;
#200149 = CYLINDRICAL_SURFACE ( 'NONE', #882, 0.09999999999999939493 ) ;
#200150 = EDGE_CURVE ( 'NONE', #139671, #224622, #114066, .T. ) ;
#200151 = CARTESIAN_POINT ( 'NONE',  ( 15.31784899511110076, 49.15934945732309558, -233.6546618023460553 ) ) ;
#200152 = DIRECTION ( 'NONE',  ( 1.000000000000000000, 0.000000000000000000, 0.000000000000000000 ) ) ;
#200153 = AXIS2_PLACEMENT_3D ( 'NONE', #77130, #216643, #154151 ) ;
#200154 = EDGE_LOOP ( 'NONE', ( #66354, #254284, #114746, #221957 ) ) ;
#200155 = EDGE_CURVE ( 'NONE', #49762, #208340, #155899, .T. ) ;
#200156 = AXIS2_PLACEMENT_3D ( 'NONE', #141013, #5301, #181429 ) ;
#200157 = AXIS2_PLACEMENT_3D ( 'NONE', #111818, #53109, #113095 ) ;
#200159 = ORIENTED_EDGE ( 'NONE', *, *, #73458, .F. ) ;
#200158 = CIRCLE ( 'NONE', #37685, 0.5000000000000008882 ) ;
#200160 = EDGE_CURVE ( 'NONE', #229941, #157888, #23453, .T. ) ;
#200161 = VERTEX_POINT ( 'NONE', #119317 ) ;
#200162 = LINE ( 'NONE', #154638, #122546 ) ;
#200163 = LINE ( 'NONE', #201433, #233530 ) ;
#200166 = ORIENTED_EDGE ( 'NONE', *, *, #249286, .T. ) ;
#200165 = DIRECTION ( 'NONE',  ( 0.000000000000000000, -0.9999631594459053030, -0.008583690987162452199 ) ) ;
#200164 =( BOUNDED_CURVE ( )  B_SPLINE_CURVE ( 3, ( #172196, #114742, #15670, #71785 ),
 .UNSPECIFIED., .F., .F. ) 
 B_SPLINE_CURVE_WITH_KNOTS ( ( 4, 4 ),
 ( 6.664455228996977694E-14, 1.570796326794907438 ),
 .UNSPECIFIED. ) 
 CURVE ( )  GEOMETRIC_REPRESENTATION_ITEM ( )  RATIONAL_B_SPLINE_CURVE ( ( 1.000000000000000000, 0.8047378541243781491, 0.8047378541243781491, 1.000000000000000000 ) ) 
 REPRESENTATION_ITEM ( '' )  );
#200167 = EDGE_CURVE ( 'NONE', #163243, #80026, #52439, .T. ) ;
#200168 = CARTESIAN_POINT ( 'NONE',  ( 21.02374657821589921, 11.60000000083178406, -127.0717967701983326 ) ) ;
#200169 = DIRECTION ( 'NONE',  ( 0.7071359030027680737, 0.7070776581709111719, 0.000000000000000000 ) ) ;
#200170 = CARTESIAN_POINT ( 'NONE',  ( -22.48660254037842776, 11.37252324248628987, -198.4720136275361710 ) ) ;
#200171 = CARTESIAN_POINT ( 'NONE',  ( -21.55000000000000426, 7.708578643773852157, -54.65000000000000568 ) ) ;
#200172 = ADVANCED_FACE ( 'NONE', ( #236673 ), #81434, .F. ) ;
#200173 = LINE ( 'NONE', #21541, #66977 ) ;
#200174 = CARTESIAN_POINT ( 'NONE',  ( -18.59999999999999787, 11.65000000001115232, -141.0148057706540214 ) ) ;
#200176 = ORIENTED_EDGE ( 'NONE', *, *, #191514, .F. ) ;
#200175 = CARTESIAN_POINT ( 'NONE',  ( 23.14999999999998437, 76.00000000001213607, -136.5231074845242745 ) ) ;
#200178 = ORIENTED_EDGE ( 'NONE', *, *, #101645, .F. ) ;
#200177 = DIRECTION ( 'NONE',  ( -1.000000000000000000, 0.000000000000000000, 0.000000000000000000 ) ) ;
#200179 = DIRECTION ( 'NONE',  ( 0.8049926720990051576, -0.5932847527679298016, -4.142885285818778274E-15 ) ) ;
#200180 = TOROIDAL_SURFACE ( 'NONE', #87722, 1.900000000000002576, 0.1000000000000000056 ) ;
#200181 = ORIENTED_EDGE ( 'NONE', *, *, #64855, .F. ) ;
#200182 = VERTEX_POINT ( 'NONE', #200138 ) ;
#200183 = CARTESIAN_POINT ( 'NONE',  ( -18.50211644919735576, 10.30207779525982836, -105.9895520716782897 ) ) ;
#200184 = DIRECTION ( 'NONE',  ( 4.504528286903032433E-15, 0.9579639084728162057, 0.2868887416115976086 ) ) ;
#200185 = DIRECTION ( 'NONE',  ( 0.000000000000000000, 0.1332476588733448597, 0.9910827722268067408 ) ) ;
#200186 = CARTESIAN_POINT ( 'NONE',  ( -18.40000000000000213, 61.75216633358002127, -212.7659468556851436 ) ) ;
#200187 = ADVANCED_FACE ( 'NONE', ( #161015 ), #202485, .F. ) ;
#200188 = CARTESIAN_POINT ( 'NONE',  ( 20.94999999999999574, 10.62357026049396680, -174.9919452032305287 ) ) ;
#200189 = DIRECTION ( 'NONE',  ( 0.000000000000000000, 1.000000000000000000, 0.000000000000000000 ) ) ;
#200190 = CARTESIAN_POINT ( 'NONE',  ( -21.05000000000000071, 77.16270174995064224, -195.4231074845243370 ) ) ;
#200191 = CIRCLE ( 'NONE', #87742, 0.5000000000000004441 ) ;
#200192 = EDGE_LOOP ( 'NONE', ( #173099, #143726, #4777, #207536 ) ) ;
#200193 = ORIENTED_EDGE ( 'NONE', *, *, #111425, .T. ) ;
#200194 = AXIS2_PLACEMENT_3D ( 'NONE', #222792, #159019, #101542 ) ;
#200195 = CARTESIAN_POINT ( 'NONE',  ( -20.07928932188135107, 13.51025652711681069, -219.7033947181103031 ) ) ;
#200196 = VECTOR ( 'NONE', #126930, 1000.000000000000000 ) ;
#200197 = ORIENTED_EDGE ( 'NONE', *, *, #73520, .T. ) ;
#200198 = DIRECTION ( 'NONE',  ( 0.000000000000000000, 0.9908441862701596881, 0.1350103645451904977 ) ) ;
#200199 = LINE ( 'NONE', #115511, #101822 ) ;
#200200 = CARTESIAN_POINT ( 'NONE',  ( -13.77178122865954357, 66.54397173950366096, -54.51190944945868466 ) ) ;
#200201 = AXIS2_PLACEMENT_3D ( 'NONE', #115398, #254852, #200082 ) ;
#200202 = FACE_OUTER_BOUND ( 'NONE', #227494, .T. ) ;
#200203 = ORIENTED_EDGE ( 'NONE', *, *, #243897, .T. ) ;
#200204 = ADVANCED_FACE ( 'NONE', ( #41084 ), #42347, .T. ) ;
#200205 = FACE_OUTER_BOUND ( 'NONE', #60798, .T. ) ;
#200206 = ORIENTED_EDGE ( 'NONE', *, *, #123749, .F. ) ;
#200207 = LINE ( 'NONE', #195091, #208802 ) ;
#200208 = ORIENTED_EDGE ( 'NONE', *, *, #188960, .F. ) ;
#200209 = AXIS2_PLACEMENT_3D ( 'NONE', #125354, #7980, #26261 ) ;
#200210 = DIRECTION ( 'NONE',  ( 1.000000000000000000, 0.000000000000000000, 0.000000000000000000 ) ) ;
#200211 = FACE_OUTER_BOUND ( 'NONE', #133200, .T. ) ;
#200212 = ORIENTED_EDGE ( 'NONE', *, *, #210495, .T. ) ;
#200213 = CARTESIAN_POINT ( 'NONE',  ( -23.25000000000000000, 1.115600667400684642E-11, -200.9999999999999432 ) ) ;
#200215 = ORIENTED_EDGE ( 'NONE', *, *, #66475, .T. ) ;
#200214 = DIRECTION ( 'NONE',  ( 0.000000000000000000, -0.9126074666063795915, -0.4088369013363224447 ) ) ;
#200216 = EDGE_CURVE ( 'NONE', #229996, #143721, #177584, .T. ) ;
#200217 = DIRECTION ( 'NONE',  ( -1.020425574104004196E-15, 0.000000000000000000, 1.000000000000000000 ) ) ;
#200218 = ORIENTED_EDGE ( 'NONE', *, *, #127661, .F. ) ;
#200219 = CARTESIAN_POINT ( 'NONE',  ( -23.15000000000000213, 2.000000000011154189, -187.7753780772378889 ) ) ;
#200220 = ORIENTED_EDGE ( 'NONE', *, *, #238048, .F. ) ;
#200221 = DIRECTION ( 'NONE',  ( -1.000000000000000000, 0.000000000000000000, 0.000000000000000000 ) ) ;
#200223 = CARTESIAN_POINT ( 'NONE',  ( 22.49436431346199683, 25.99973956953803622, -254.2530358866374343 ) ) ;
#200222 = CIRCLE ( 'NONE', #87776, 0.9750000000000036415 ) ;
#200224 = DIRECTION ( 'NONE',  ( 0.000000000000000000, -0.2617529984164994050, -0.9651348961777166391 ) ) ;
#200225 = DIRECTION ( 'NONE',  ( 0.000000000000000000, 8.881784197001252323E-16, -1.000000000000000000 ) ) ;
#200226 = FACE_OUTER_BOUND ( 'NONE', #172015, .T. ) ;
#200227 = VECTOR ( 'NONE', #66006, 1000.000000000000114 ) ;
#200228 = ORIENTED_EDGE ( 'NONE', *, *, #171306, .F. ) ;
#200229 = CARTESIAN_POINT ( 'NONE',  ( 22.59999999999999076, 64.25012875563618309, -203.5885370755381132 ) ) ;
#200230 = DIRECTION ( 'NONE',  ( 5.603264701231743991E-32, -0.8814952561688430555, 0.4721928772777344019 ) ) ;
#200231 = AXIS2_PLACEMENT_3D ( 'NONE', #2926, #201139, #184135 ) ;
#200232 = ORIENTED_EDGE ( 'NONE', *, *, #466, .F. ) ;
#200234 = CARTESIAN_POINT ( 'NONE',  ( 18.50000972452444969, 10.29326151435342851, -105.9592822510414862 ) ) ;
#200233 = B_SPLINE_CURVE_WITH_KNOTS ( 'NONE', 3,
 ( #42247, #212241, #56967, #33636, #135234, #34904, #115693, #121792, #93553, #214782 ),
 .UNSPECIFIED., .F., .F.,
 ( 4, 3, 3, 4 ),
 ( 0.000000000000000000, 3.394313611811197040E-05, 6.779740500700327799E-05, 0.0001049857339142765996 ),
 .UNSPECIFIED. ) ;
#200235 = ORIENTED_EDGE ( 'NONE', *, *, #163903, .T. ) ;
#200236 = DIRECTION ( 'NONE',  ( -1.000000000000000000, -0.000000000000000000, -0.000000000000000000 ) ) ;
#200237 = ORIENTED_EDGE ( 'NONE', *, *, #154379, .T. ) ;
#200238 = CARTESIAN_POINT ( 'NONE',  ( -21.59780538579341069, 69.15290947006943156, -203.6220861541223996 ) ) ;
#200239 = CARTESIAN_POINT ( 'NONE',  ( -20.94788355080264353, 10.30207779525983014, -72.48955207167824710 ) ) ;
#200240 = ORIENTED_EDGE ( 'NONE', *, *, #201764, .F. ) ;
#200241 = CIRCLE ( 'NONE', #241922, 0.1000000000000028644 ) ;
#200243 = VERTEX_POINT ( 'NONE', #120619 ) ;
#200242 = CARTESIAN_POINT ( 'NONE',  ( -21.14999999999999858, 76.10000000001174669, -81.17267829206912211 ) ) ;
#200244 = CYLINDRICAL_SURFACE ( 'NONE', #79669, 2.000000000000001776 ) ;
#200245 = ORIENTED_EDGE ( 'NONE', *, *, #179542, .T. ) ;
#200246 = DIRECTION ( 'NONE',  ( -1.000000000000000000, 0.000000000000000000, 0.000000000000000000 ) ) ;
#200247 = EDGE_CURVE ( 'NONE', #191840, #101698, #135830, .T. ) ;
#200248 = FACE_OUTER_BOUND ( 'NONE', #151931, .T. ) ;
#200249 = VERTEX_POINT ( 'NONE', #99716 ) ;
#200250 = ORIENTED_EDGE ( 'NONE', *, *, #204974, .F. ) ;
#200251 = FACE_OUTER_BOUND ( 'NONE', #49742, .T. ) ;
#200252 = CARTESIAN_POINT ( 'NONE',  ( -21.00000000000000000, 1.885425182446133885, -11.49641995933507843 ) ) ;
#200253 = ORIENTED_EDGE ( 'NONE', *, *, #117734, .F. ) ;
#200254 = CARTESIAN_POINT ( 'NONE',  ( -16.88495309932523014, 66.04537294153921323, -123.8885588107124676 ) ) ;
#200255 = AXIS2_PLACEMENT_3D ( 'NONE', #207878, #29254, #110024 ) ;
#200256 = AXIS2_PLACEMENT_3D ( 'NONE', #212697, #73204, #34087 ) ;
#200257 = VERTEX_POINT ( 'NONE', #21515 ) ;
#200258 = ORIENTED_EDGE ( 'NONE', *, *, #53915, .F. ) ;
#200259 = CARTESIAN_POINT ( 'NONE',  ( -33.72168855820451938, 9.950000000011156587, -180.1499999999999204 ) ) ;
#200261 =( BOUNDED_CURVE ( )  B_SPLINE_CURVE ( 3, ( #3240, #59344, #181906, #200186 ),
 .UNSPECIFIED., .F., .T. ) 
 B_SPLINE_CURVE_WITH_KNOTS ( ( 4, 4 ),
 ( -1.172395514004165307E-13, 1.570796326794935194 ),
 .UNSPECIFIED. ) 
 CURVE ( )  GEOMETRIC_REPRESENTATION_ITEM ( )  RATIONAL_B_SPLINE_CURVE ( ( 1.000000000000000000, 0.8047378541243281891, 0.8047378541243281891, 1.000000000000000000 ) ) 
 REPRESENTATION_ITEM ( '' )  );
#200260 = CIRCLE ( 'NONE', #33720, 1.749999999999999778 ) ;
#200262 = EDGE_CURVE ( 'NONE', #108947, #155129, #139917, .T. ) ;
#200263 = CIRCLE ( 'NONE', #254402, 0.09999999999999864553 ) ;
#200264 = AXIS2_PLACEMENT_3D ( 'NONE', #152073, #213291, #114202 ) ;
#200265 = EDGE_CURVE ( 'NONE', #243492, #178434, #100978, .T. ) ;
#200267 = ORIENTED_EDGE ( 'NONE', *, *, #125615, .T. ) ;
#200266 = CARTESIAN_POINT ( 'NONE',  ( -23.25000000000000000, 74.00000000001180922, -82.74772940728641402 ) ) ;
#200268 = FACE_BOUND ( 'NONE', #170261, .T. ) ;
#200269 = CARTESIAN_POINT ( 'NONE',  ( -23.15000000000000213, 45.96866462019919197, -240.6139518702713360 ) ) ;
#200270 = DIRECTION ( 'NONE',  ( 1.000000000000000000, -0.000000000000000000, -0.000000000000000000 ) ) ;
#200272 = DIRECTION ( 'NONE',  ( 0.000000000000000000, 0.8814952561688430555, -0.4721928772777344574 ) ) ;
#200271 = CARTESIAN_POINT ( 'NONE',  ( -16.93440969289731157, 66.00481482419790780, -90.43187329951359743 ) ) ;
#200273 = DIRECTION ( 'NONE',  ( 0.000000000000000000, -0.7397360091702802620, 0.6728971962616779878 ) ) ;
#200274 = CARTESIAN_POINT ( 'NONE',  ( -20.64999999999999858, 6.294532028225942710, -220.7845521659012888 ) ) ;
#200275 = EDGE_CURVE ( 'NONE', #239256, #159674, #59290, .T. ) ;
#200276 = LINE ( 'NONE', #185842, #255832 ) ;
#200277 = AXIS2_PLACEMENT_3D ( 'NONE', #125979, #107702, #144242 ) ;
#200278 = DIRECTION ( 'NONE',  ( -1.000000000000000000, -0.000000000000000000, -0.000000000000000000 ) ) ;
#200279 = AXIS2_PLACEMENT_3D ( 'NONE', #170279, #175397, #134921 ) ;
#200280 = CIRCLE ( 'NONE', #125279, 0.5000000000000087708 ) ;
#200282 = ORIENTED_EDGE ( 'NONE', *, *, #9682, .T. ) ;
#200281 = AXIS2_PLACEMENT_3D ( 'NONE', #42899, #85836, #222795 ) ;
#200283 = ORIENTED_EDGE ( 'NONE', *, *, #30559, .F. ) ;
#200284 = ORIENTED_EDGE ( 'NONE', *, *, #1262, .F. ) ;
#200285 = ORIENTED_EDGE ( 'NONE', *, *, #157153, .T. ) ;
#200286 = EDGE_CURVE ( 'NONE', #253366, #57845, #106596, .T. ) ;
#200287 = CARTESIAN_POINT ( 'NONE',  ( -16.89060415895970735, 9.951220762813354881, -146.6459202242704691 ) ) ;
#200288 = AXIS2_PLACEMENT_3D ( 'NONE', #121093, #158926, #80619 ) ;
#200289 = VERTEX_POINT ( 'NONE', #78873 ) ;
#200290 = EDGE_CURVE ( 'NONE', #156870, #158295, #56697, .T. ) ;
#200291 = DIRECTION ( 'NONE',  ( -0.000000000000000000, 0.000000000000000000, 1.000000000000000000 ) ) ;
#200293 = EDGE_LOOP ( 'NONE', ( #140208, #216864, #239595, #10763 ) ) ;
#200292 = ORIENTED_EDGE ( 'NONE', *, *, #1060, .T. ) ;
#200294 = ORIENTED_EDGE ( 'NONE', *, *, #82800, .T. ) ;
#200295 = ORIENTED_EDGE ( 'NONE', *, *, #4608, .T. ) ;
#200296 = DIRECTION ( 'NONE',  ( 0.000000000000000000, 6.982962677686266711E-15, -1.000000000000000000 ) ) ;
#200297 = CYLINDRICAL_SURFACE ( 'NONE', #88552, 1.749999999999998002 ) ;
#200299 = ORIENTED_EDGE ( 'NONE', *, *, #65055, .F. ) ;
#200298 = DIRECTION ( 'NONE',  ( -0.000000000000000000, -6.982962677686266711E-15, 1.000000000000000000 ) ) ;
#200300 = CARTESIAN_POINT ( 'NONE',  ( 20.12518398540832010, 39.87855921381013502, -237.1784891853482122 ) ) ;
#200301 = CARTESIAN_POINT ( 'NONE',  ( 20.89192007715127986, 65.67101464000501210, -97.44043916224792667 ) ) ;
#200303 = ORIENTED_EDGE ( 'NONE', *, *, #148795, .T. ) ;
#200302 = CARTESIAN_POINT ( 'NONE',  ( 20.05000000000002913, 7.250000000011171508, -54.35000000000000142 ) ) ;
#200304 = FACE_OUTER_BOUND ( 'NONE', #228903, .T. ) ;
#200305 = ORIENTED_EDGE ( 'NONE', *, *, #18161, .F. ) ;
#200306 = DIRECTION ( 'NONE',  ( 1.000000000000000000, 0.000000000000000000, 0.000000000000000000 ) ) ;
#200307 = AXIS2_PLACEMENT_3D ( 'NONE', #192547, #229104, #109136 ) ;
#200310 = ADVANCED_FACE ( 'NONE', ( #1910 ), #61909, .T. ) ;
#200309 = ORIENTED_EDGE ( 'NONE', *, *, #60838, .F. ) ;
#200308 = DIRECTION ( 'NONE',  ( 0.000000000000000000, 0.2617529984165031243, 0.9651348961777157509 ) ) ;
#200311 = DIRECTION ( 'NONE',  ( 1.000000000000000000, 0.000000000000000000, 0.000000000000000000 ) ) ;
#200312 = CARTESIAN_POINT ( 'NONE',  ( 22.39999999999999858, 7.790779598373383408, 0.09999999999999939493 ) ) ;
#200313 = VERTEX_POINT ( 'NONE', #116739 ) ;
#200315 = LINE ( 'NONE', #174385, #133109 ) ;
#200314 = LINE ( 'NONE', #106318, #61420 ) ;
#200316 = CARTESIAN_POINT ( 'NONE',  ( -21.14999999999999858, 67.23127455305841238, -235.8551265064783991 ) ) ;
#200317 = DIRECTION ( 'NONE',  ( 0.000000000000000000, 0.000000000000000000, -1.000000000000000000 ) ) ;
#200318 = CIRCLE ( 'NONE', #121259, 11.80000000000000426 ) ;
#200319 = DIRECTION ( 'NONE',  ( 0.000000000000000000, 0.000000000000000000, -1.000000000000000000 ) ) ;
#200320 = DIRECTION ( 'NONE',  ( 1.000000000000000000, -0.000000000000000000, -0.000000000000000000 ) ) ;
#200321 = ORIENTED_EDGE ( 'NONE', *, *, #40568, .T. ) ;
#200322 = EDGE_LOOP ( 'NONE', ( #115182, #86062, #115634, #231987 ) ) ;
#200323 = ORIENTED_EDGE ( 'NONE', *, *, #217178, .F. ) ;
#200324 = ADVANCED_FACE ( 'NONE', ( #159729 ), #123377, .T. ) ;
#200326 = CIRCLE ( 'NONE', #388, 0.09999999999999939493 ) ;
#200325 = CARTESIAN_POINT ( 'NONE',  ( -21.05000000000000071, -0.01771943329720805649, -127.5589153115293186 ) ) ;
#200327 = EDGE_LOOP ( 'NONE', ( #48010, #139335, #113632, #169521 ) ) ;
#200328 = CARTESIAN_POINT ( 'NONE',  ( -20.94999999999999929, 6.256349259666489360, -229.7266095100222572 ) ) ;
#200329 = VERTEX_POINT ( 'NONE', #60604 ) ;
#200330 = CARTESIAN_POINT ( 'NONE',  ( -18.46902351632713746, -7.804936695476651032, -209.8500578355755692 ) ) ;
#200331 = DIRECTION ( 'NONE',  ( 0.000000000000000000, -0.9770955615653318382, -0.2128009952263588411 ) ) ;
#200332 = EDGE_CURVE ( 'NONE', #57819, #84546, #201407, .T. ) ;
#200333 = ORIENTED_EDGE ( 'NONE', *, *, #11076, .F. ) ;
#200334 = DIRECTION ( 'NONE',  ( -1.000000000000000000, -0.000000000000000000, 0.000000000000000000 ) ) ;
#200335 =( NAMED_UNIT ( * ) SI_UNIT ( $, .STERADIAN. ) SOLID_ANGLE_UNIT ( ) );
#200336 = EDGE_CURVE ( 'NONE', #141039, #195862, #98381, .T. ) ;
#200337 = CIRCLE ( 'NONE', #17198, 12.87500000000000000 ) ;
#200338 = EDGE_CURVE ( 'NONE', #39555, #149634, #8366, .T. ) ;
#200340 = ORIENTED_EDGE ( 'NONE', *, *, #62476, .F. ) ;
#200339 = AXIS2_PLACEMENT_3D ( 'NONE', #67201, #208015, #45069 ) ;
#200341 = VERTEX_POINT ( 'NONE', #47458 ) ;
#200342 = ORIENTED_EDGE ( 'NONE', *, *, #33615, .F. ) ;
#200343 = CIRCLE ( 'NONE', #142068, 11.74999999999999822 ) ;
#200344 = CARTESIAN_POINT ( 'NONE',  ( -18.59999999999999787, 77.83534155023598089, -57.96795619196132776 ) ) ;
#200345 = DIRECTION ( 'NONE',  ( -0.000000000000000000, -0.000000000000000000, -1.000000000000000000 ) ) ;
#200346 = DIRECTION ( 'NONE',  ( 0.000000000000000000, 0.000000000000000000, 1.000000000000000000 ) ) ;
#200347 = DIRECTION ( 'NONE',  ( 1.000000000000000000, 0.000000000000000000, 0.000000000000000000 ) ) ;
#200348 = CARTESIAN_POINT ( 'NONE',  ( -21.55000000000000071, 68.85000000001254250, -182.2731074845244166 ) ) ;
#200349 = ADVANCED_FACE ( 'NONE', ( #124461 ), #164867, .T. ) ;
#200351 = SPHERICAL_SURFACE ( 'NONE', #36858, 0.1000000000000000056 ) ;
#200350 = DIRECTION ( 'NONE',  ( 0.000000000000000000, 0.9126074666063844765, 0.4088369013363114535 ) ) ;
#200352 = DIRECTION ( 'NONE',  ( 1.000000000000000000, 0.000000000000000000, 0.000000000000000000 ) ) ;
#200354 = ORIENTED_EDGE ( 'NONE', *, *, #115781, .F. ) ;
#200353 = CARTESIAN_POINT ( 'NONE',  ( 18.59999999999999432, 77.16270174995034381, -162.0231074845243313 ) ) ;
#200355 = DIRECTION ( 'NONE',  ( -0.000000000000000000, -1.000000000000000000, -6.982962677686266711E-15 ) ) ;
#200356 = CARTESIAN_POINT ( 'NONE',  ( -18.40000000000000213, -9.499999999988851584, -141.0320693966996828 ) ) ;
#200357 = ORIENTED_EDGE ( 'NONE', *, *, #253496, .F. ) ;
#200358 = EDGE_LOOP ( 'NONE', ( #252497, #122040, #150272, #171540 ) ) ;
#200359 = CARTESIAN_POINT ( 'NONE',  ( -20.94999999999999929, -11.64999999998884306, -103.6000000000000369 ) ) ;
#200360 = CARTESIAN_POINT ( 'NONE',  ( -18.59999999999999787, 77.73625713160946304, -124.9544551555067926 ) ) ;
#200362 = EDGE_CURVE ( 'NONE', #78065, #130099, #222234, .T. ) ;
#200361 = CARTESIAN_POINT ( 'NONE',  ( -18.50000000000000000, 46.55954744353147134, -243.3218549665227783 ) ) ;
#200364 = EDGE_CURVE ( 'NONE', #203708, #218733, #127469, .T. ) ;
#200363 = ORIENTED_EDGE ( 'NONE', *, *, #95518, .T. ) ;
#200365 = B_SPLINE_CURVE_WITH_KNOTS ( 'NONE', 3,
 ( #31790, #249530, #244365, #111298, #67029, #185694, #128296, #164851, #146537, #226066, #30488, #47440, #207853, #107434, #9614, #186999, #149153, #190864, #167439 ),
 .UNSPECIFIED., .F., .F.,
 ( 4, 3, 3, 3, 3, 3, 4 ),
 ( 1.387778780781445676E-17, 2.646747978908994698E-05, 5.271166642128863382E-05, 9.008788829885137981E-05, 0.0001426648776561022008, 0.0001897378458659801945, 0.0001917382627806380965 ),
 .UNSPECIFIED. ) ;
#200366 = AXIS2_PLACEMENT_3D ( 'NONE', #229084, #50411, #205643 ) ;
#200367 = CARTESIAN_POINT ( 'NONE',  ( -18.50000000000000000, 74.93036000061670165, -233.6816308724374949 ) ) ;
#200368 = ORIENTED_EDGE ( 'NONE', *, *, #4704, .F. ) ;
#200369 = ORIENTED_EDGE ( 'NONE', *, *, #111592, .F. ) ;
#200370 = ADVANCED_FACE ( 'NONE', ( #83984 ), #203978, .F. ) ;
#200371 = CARTESIAN_POINT ( 'NONE',  ( 22.39999999999999503, 68.20922040163857503, -103.0231074845243739 ) ) ;
#200372 = ORIENTED_EDGE ( 'NONE', *, *, #228388, .T. ) ;
#200373 = CARTESIAN_POINT ( 'NONE',  ( -16.93339986808596365, 60.86418613339449024, -221.1083815558925778 ) ) ;
#200374 = DIRECTION ( 'NONE',  ( 0.000000000000000000, -0.000000000000000000, 1.000000000000000000 ) ) ;
#200375 = CARTESIAN_POINT ( 'NONE',  ( 18.50000000000000000, 85.40000000001165859, -62.64106563635156277 ) ) ;
#200376 = ADVANCED_FACE ( 'NONE', ( #48756 ), #114998, .T. ) ;
#200377 = ORIENTED_EDGE ( 'NONE', *, *, #92837, .F. ) ;
#200378 = EDGE_CURVE ( 'NONE', #115263, #255583, #223527, .T. ) ;
#200379 = CARTESIAN_POINT ( 'NONE',  ( -21.64999999999999858, 68.75000000001179501, -81.87310748452436826 ) ) ;
#200380 = AXIS2_PLACEMENT_3D ( 'NONE', #129897, #209440, #189887 ) ;
#200381 = AXIS2_PLACEMENT_3D ( 'NONE', #174445, #90998, #233108 ) ;
#200383 = DIRECTION ( 'NONE',  ( 0.000000000000000000, 0.000000000000000000, 1.000000000000000000 ) ) ;
#200382 = CIRCLE ( 'NONE', #254515, 11.64999999999999325 ) ;
#200384 = CIRCLE ( 'NONE', #121313, 0.5000000000000004441 ) ;
#200385 = DIRECTION ( 'NONE',  ( 0.000000000000000000, -0.1332476588733448597, 0.9910827722268067408 ) ) ;
#200386 = ORIENTED_EDGE ( 'NONE', *, *, #71235, .F. ) ;
#200388 = ORIENTED_EDGE ( 'NONE', *, *, #151891, .F. ) ;
#200387 = FACE_OUTER_BOUND ( 'NONE', #161779, .T. ) ;
#200389 = ADVANCED_FACE ( 'NONE', ( #64484 ), #143996, .T. ) ;
#200390 = CARTESIAN_POINT ( 'NONE',  ( 23.04999999999999716, 67.17743825834588733, -157.3731074845244109 ) ) ;
#200391 = DIRECTION ( 'NONE',  ( 1.000000000000000000, 0.000000000000000000, -0.000000000000000000 ) ) ;
#200392 = EDGE_CURVE ( 'NONE', #108958, #101410, #166180, .T. ) ;
#200393 = DIRECTION ( 'NONE',  ( -1.836970198721029934E-16, 0.9770955615653316162, 0.2128009952263604232 ) ) ;
#200394 = CARTESIAN_POINT ( 'NONE',  ( 23.24999999999999645, 9.960715529987961503, -220.4198853720552904 ) ) ;
#200395 = FACE_OUTER_BOUND ( 'NONE', #212488, .T. ) ;
#200396 = DIRECTION ( 'NONE',  ( 1.000000000000000000, 0.000000000000000000, 0.000000000000000000 ) ) ;
#200397 = AXIS2_PLACEMENT_3D ( 'NONE', #73117, #95211, #113484 ) ;
#200398 = EDGE_LOOP ( 'NONE', ( #150862, #77347, #4158, #104118 ) ) ;
#200399 = CARTESIAN_POINT ( 'NONE',  ( -16.85718274719333465, 63.08318335034096691, -213.0371462789988186 ) ) ;
#200400 = DIRECTION ( 'NONE',  ( -1.020425574104004196E-15, 6.982962677686266711E-15, -1.000000000000000000 ) ) ;
#200401 = CARTESIAN_POINT ( 'NONE',  ( -18.41817142474032565, 77.14152309475025504, -241.8237690616388420 ) ) ;
#200402 = CARTESIAN_POINT ( 'NONE',  ( 21.00023020733438628, 6.390869245278875788, -134.0000000000000000 ) ) ;
#200403 = ADVANCED_FACE ( 'NONE', ( #89163 ), #128315, .T. ) ;
#200404 = DIRECTION ( 'NONE',  ( 0.000000000000000000, -1.000000000000000000, -6.982962677686265922E-15 ) ) ;
#200405 = CARTESIAN_POINT ( 'NONE',  ( 20.12481660106788439, 66.47365600773666472, -61.29696581543134926 ) ) ;
#200406 = VERTEX_POINT ( 'NONE', #43635 ) ;
#200407 = ORIENTED_EDGE ( 'NONE', *, *, #155086, .T. ) ;
#200408 = DIRECTION ( 'NONE',  ( -0.000000000000000000, 0.9770955615653313941, 0.2128009952263603954 ) ) ;
#200409 = CARTESIAN_POINT ( 'NONE',  ( -18.59999999999999787, 4.324939842317335525, -212.0862480289983409 ) ) ;
#200410 = CARTESIAN_POINT ( 'NONE',  ( 23.25000000000000000, 85.00000000001207923, -126.6291383618717816 ) ) ;
#200411 = VECTOR ( 'NONE', #117364, 1000.000000000000000 ) ;
#200412 = ORIENTED_EDGE ( 'NONE', *, *, #131008, .T. ) ;
#200413 = CARTESIAN_POINT ( 'NONE',  ( -21.55000000000000426, 7.750000000011159074, -155.2500000000000284 ) ) ;
#200414 = CARTESIAN_POINT ( 'NONE',  ( 19.99999999999998934, 34.58225676390223668, -235.1091250528070589 ) ) ;
#200415 = TOROIDAL_SURFACE ( 'NONE', #112927, 7.800000000000000711, 0.1000000000000000056 ) ;
#200416 = ADVANCED_FACE ( 'NONE', ( #67048 ), #160816, .F. ) ;
#200417 = DIRECTION ( 'NONE',  ( 1.000000000000000000, -0.000000000000000000, -0.000000000000000000 ) ) ;
#200418 = TOROIDAL_SURFACE ( 'NONE', #192068, 0.4000000000000009104, 0.1000000000000000056 ) ;
#200419 = EDGE_CURVE ( 'NONE', #174804, #43089, #35914, .T. ) ;
#200420 = AXIS2_PLACEMENT_3D ( 'NONE', #152946, #96750, #34279 ) ;
#200421 = VERTEX_POINT ( 'NONE', #65758 ) ;
#200422 = CARTESIAN_POINT ( 'NONE',  ( 15.48841904831874849, 67.43841904833138301, -190.8731074845244393 ) ) ;
#200423 = AXIS2_PLACEMENT_3D ( 'NONE', #53497, #90036, #187881 ) ;
#200424 = EDGE_CURVE ( 'NONE', #26109, #198727, #77553, .T. ) ;
#200425 = ORIENTED_EDGE ( 'NONE', *, *, #148646, .F. ) ;
#200426 = CARTESIAN_POINT ( 'NONE',  ( 20.04142135623730070, 64.35000000001198828, -115.1731074845243796 ) ) ;
#200427 = CARTESIAN_POINT ( 'NONE',  ( 20.94999999999999929, 4.850467289730772791, -146.0342674090016999 ) ) ;
#200428 = DIRECTION ( 'NONE',  ( 1.000000000000000000, 0.000000000000000000, 0.000000000000000000 ) ) ;
#200429 = PLANE ( 'NONE',  #115786 ) ;
#200430 = CARTESIAN_POINT ( 'NONE',  ( 18.52928932188133970, 10.27928932189249878, -192.2085786437626211 ) ) ;
#200432 = ADVANCED_FACE ( 'NONE', ( #246954 ), #68336, .F. ) ;
#200431 = CARTESIAN_POINT ( 'NONE',  ( -20.54999999999999716, 85.00000000001232081, -160.6291383618718385 ) ) ;
#200434 = CARTESIAN_POINT ( 'NONE',  ( 23.24999999999999645, 67.23127455305835554, -235.8551265064784559 ) ) ;
#200433 = CIRCLE ( 'NONE', #87973, 0.2000000000000057288 ) ;
#200435 = FACE_OUTER_BOUND ( 'NONE', #134801, .T. ) ;
#200436 = DIRECTION ( 'NONE',  ( -0.000000000000000000, -1.000000000000000000, 0.000000000000000000 ) ) ;
#200437 = DIRECTION ( 'NONE',  ( 2.952720810173289112E-16, 0.9651348961777191926, -0.2617529984164898571 ) ) ;
#200438 = EDGE_CURVE ( 'NONE', #136977, #140654, #123170, .T. ) ;
#200439 = LINE ( 'NONE', #180881, #248082 ) ;
#200440 = DIRECTION ( 'NONE',  ( 2.952720810173289112E-16, -1.000000000000000000, 0.000000000000000000 ) ) ;
#200441 = AXIS2_PLACEMENT_3D ( 'NONE', #170742, #31221, #110709 ) ;
#200442 = CARTESIAN_POINT ( 'NONE',  ( -21.05000000000000071, 77.83534155023627932, -91.46795619196132066 ) ) ;
#200443 = CARTESIAN_POINT ( 'NONE',  ( 19.92426406871192412, 11.75000000001116085, -158.8500000000000227 ) ) ;
#200444 = ADVANCED_FACE ( 'NONE', ( #192152 ), #85925, .F. ) ;
#200446 = EDGE_CURVE ( 'NONE', #198148, #227337, #227597, .T. ) ;
#200445 = EDGE_CURVE ( 'NONE', #48459, #21732, #190206, .T. ) ;
#200447 = VERTEX_POINT ( 'NONE', #112600 ) ;
#200448 = CIRCLE ( 'NONE', #63061, 0.5000000000000004441 ) ;
#200449 = FACE_OUTER_BOUND ( 'NONE', #45509, .T. ) ;
#200450 = DIRECTION ( 'NONE',  ( -6.938893903907222856E-15, -1.000000000000000000, -7.272083257015735086E-15 ) ) ;
#200451 = AXIS2_PLACEMENT_3D ( 'NONE', #246986, #48790, #128347 ) ;
#200452 = ORIENTED_EDGE ( 'NONE', *, *, #242321, .T. ) ;
#200453 = CARTESIAN_POINT ( 'NONE',  ( -22.47886152344871036, 0.03750093887284931121, -55.35001135695211616 ) ) ;
#200454 = FACE_OUTER_BOUND ( 'NONE', #205058, .T. ) ;
#200455 = ORIENTED_EDGE ( 'NONE', *, *, #156232, .F. ) ;
#200456 = DIRECTION ( 'NONE',  ( -0.000000000000000000, -1.000000000000000000, -5.421010862427649374E-16 ) ) ;
#200457 = DIRECTION ( 'NONE',  ( 0.000000000000000000, -0.3042567129659849434, -0.9525900758537926283 ) ) ;
#200458 = VECTOR ( 'NONE', #97784, 1000.000000000000000 ) ;
#200459 = ORIENTED_EDGE ( 'NONE', *, *, #6253, .F. ) ;
#200460 = EDGE_CURVE ( 'NONE', #172429, #44452, #231719, .T. ) ;
#200462 = EDGE_CURVE ( 'NONE', #153115, #103735, #211047, .T. ) ;
#200461 = AXIS2_PLACEMENT_3D ( 'NONE', #228114, #89860, #49464 ) ;
#200463 = CIRCLE ( 'NONE', #233610, 0.09999999999999520384 ) ;
#200464 = TOROIDAL_SURFACE ( 'NONE', #21422, 4.099999999999999645, 0.1000000000000000056 ) ;
#200465 = ORIENTED_EDGE ( 'NONE', *, *, #80725, .T. ) ;
#200466 = DIRECTION ( 'NONE',  ( -1.000000000000000000, 2.952720810173289112E-16, 2.061873921506763405E-30 ) ) ;
#200467 = ADVANCED_FACE ( 'NONE', ( #129593 ), #132153, .F. ) ;
#200468 = EDGE_LOOP ( 'NONE', ( #60935, #204602, #34736, #100487 ) ) ;
#200469 = DIRECTION ( 'NONE',  ( 1.000000000000000000, -0.000000000000000000, -0.000000000000000000 ) ) ;
#200470 = ADVANCED_FACE ( 'NONE', ( #194723 ), #150454, .F. ) ;
#200471 = DIRECTION ( 'NONE',  ( 1.000000000000000000, 1.836970198721029934E-16, 3.186635328391151676E-31 ) ) ;
#200472 = CARTESIAN_POINT ( 'NONE',  ( 21.08884785362045378, 34.01443675994195814, -243.7698937337987104 ) ) ;
#200473 = LINE ( 'NONE', #97483, #162676 ) ;
#200474 = CARTESIAN_POINT ( 'NONE',  ( -20.94999999999999929, 64.35000000001147669, -42.80697314750250371 ) ) ;
#200475 = EDGE_CURVE ( 'NONE', #151911, #27454, #244349, .T. ) ;
#200476 = CYLINDRICAL_SURFACE ( 'NONE', #66799, 0.09999999999999850675 ) ;
#200477 = LINE ( 'NONE', #41421, #209384 ) ;
#200478 = CARTESIAN_POINT ( 'NONE',  ( 18.59999999999999787, 5.900000000011102586, -43.71909976465641989 ) ) ;
#200480 = ORIENTED_EDGE ( 'NONE', *, *, #50303, .T. ) ;
#200479 = DIRECTION ( 'NONE',  ( -0.000000000000000000, -0.1350103645451876666, 0.9908441862701600211 ) ) ;
#200481 = ORIENTED_EDGE ( 'NONE', *, *, #130826, .T. ) ;
#200483 = FACE_OUTER_BOUND ( 'NONE', #186069, .T. ) ;
#200482 = DIRECTION ( 'NONE',  ( 0.000000000000000000, -1.000000000000000000, 0.000000000000000000 ) ) ;
#200485 = VERTEX_POINT ( 'NONE', #90444 ) ;
#200484 = CARTESIAN_POINT ( 'NONE',  ( -16.82542659449988065, 60.97908861380064138, -220.9544488154746773 ) ) ;
#200486 = VERTEX_POINT ( 'NONE', #212976 ) ;
#200487 = CARTESIAN_POINT ( 'NONE',  ( -20.64999999999999858, 4.768403829798271154, -213.4961173936592331 ) ) ;
#200488 = LINE ( 'NONE', #21854, #63692 ) ;
#200489 = DIRECTION ( 'NONE',  ( 0.000000000000000000, 0.2128009952263601456, -0.9770955615653316162 ) ) ;
#200490 = CARTESIAN_POINT ( 'NONE',  ( 20.94999999999999574, 46.54031271043911033, -243.0982672308888368 ) ) ;
#200491 = DIRECTION ( 'NONE',  ( 0.000000000000000000, 0.4721928772777346239, 0.8814952561688430555 ) ) ;
#200492 = EDGE_CURVE ( 'NONE', #76326, #110160, #52606, .T. ) ;
#200493 = DIRECTION ( 'NONE',  ( -1.000000000000000000, 0.000000000000000000, -0.000000000000000000 ) ) ;
#200494 = FACE_OUTER_BOUND ( 'NONE', #64717, .T. ) ;
#200495 = DIRECTION ( 'NONE',  ( 0.000000000000000000, 0.000000000000000000, 1.000000000000000000 ) ) ;
#200496 = EDGE_CURVE ( 'NONE', #155920, #70151, #91748, .T. ) ;
#200497 = EDGE_LOOP ( 'NONE', ( #172343, #204590, #181074, #116933 ) ) ;
#200498 = ORIENTED_EDGE ( 'NONE', *, *, #59422, .T. ) ;
#200499 = DIRECTION ( 'NONE',  ( -1.073024830501117725E-15, -0.2128009952263604232, 0.9770955615653316162 ) ) ;
#200500 = ORIENTED_EDGE ( 'NONE', *, *, #175580, .F. ) ;
#200501 = CARTESIAN_POINT ( 'NONE',  ( 21.04999999999988702, 0.01471785653530134283, -27.15527659590986431 ) ) ;
#200502 = ORIENTED_EDGE ( 'NONE', *, *, #173284, .T. ) ;
#200503 = CARTESIAN_POINT ( 'NONE',  ( 18.50000000000000000, 77.35494420175977837, -241.6200040285045532 ) ) ;
#200504 = AXIS2_PLACEMENT_3D ( 'NONE', #81329, #224713, #4385 ) ;
#200505 = CARTESIAN_POINT ( 'NONE',  ( -15.15564720441980207, 49.30157392506337288, -233.5755204583867055 ) ) ;
#200506 = EDGE_CURVE ( 'NONE', #183531, #123954, #211712, .T. ) ;
#200507 = DIRECTION ( 'NONE',  ( 0.000000000000000000, 0.000000000000000000, 1.000000000000000000 ) ) ;
#200508 = DIRECTION ( 'NONE',  ( 1.000000000000000000, 0.000000000000000000, 0.000000000000000000 ) ) ;
#200509 = VERTEX_POINT ( 'NONE', #130864 ) ;
#200510 = DIRECTION ( 'NONE',  ( -0.000000000000000000, -0.1350103645451876666, 0.9908441862701600211 ) ) ;
#200511 = ORIENTED_EDGE ( 'NONE', *, *, #135902, .F. ) ;
#200512 = CARTESIAN_POINT ( 'NONE',  ( 22.44352723754029810, 0.009277095054436620969, -122.3502786546513050 ) ) ;
#200513 = SPHERICAL_SURFACE ( 'NONE', #127035, 0.1000000000000000056 ) ;
#200514 = PLANE ( 'NONE',  #238212 ) ;
#200515 = ORIENTED_EDGE ( 'NONE', *, *, #98861, .T. ) ;
#200517 = DIRECTION ( 'NONE',  ( 1.000000000000000000, 0.000000000000000000, 0.000000000000000000 ) ) ;
#200516 = AXIS2_PLACEMENT_3D ( 'NONE', #54107, #210622, #230 ) ;
#200518 = VERTEX_POINT ( 'NONE', #210426 ) ;
#200521 = ORIENTED_EDGE ( 'NONE', *, *, #106334, .T. ) ;
#200520 = CYLINDRICAL_SURFACE ( 'NONE', #59704, 11.75000000000001066 ) ;
#200519 = CARTESIAN_POINT ( 'NONE',  ( 18.51565452909138543, 47.04884642058242150, -255.1451075356969795 ) ) ;
#200522 = AXIS2_PLACEMENT_3D ( 'NONE', #145133, #87726, #241683 ) ;
#200523 = CARTESIAN_POINT ( 'NONE',  ( -21.53551880898957904, 0.09896973458281840830, -160.7152022385836574 ) ) ;
#200524 = AXIS2_PLACEMENT_3D ( 'NONE', #241181, #160374, #61244 ) ;
#200525 = CARTESIAN_POINT ( 'NONE',  ( -18.59999999999999787, 74.83412143252222393, -233.7087995678629966 ) ) ;
#200526 = ORIENTED_EDGE ( 'NONE', *, *, #203898, .T. ) ;
#200527 = CARTESIAN_POINT ( 'NONE',  ( 18.46163235739484421, 85.48015080693031109, -129.8654969446463383 ) ) ;
#200528 = LINE ( 'NONE', #257882, #228045 ) ;
#200529 = CARTESIAN_POINT ( 'NONE',  ( 18.52928932188133970, 33.71149860592453251, -236.3111109633099716 ) ) ;
#200530 = UNCERTAINTY_MEASURE_WITH_UNIT (LENGTH_MEASURE( 1.000000000000000082E-05 ), #205219, 'distance_accuracy_value', 'NONE');
#200532 = ORIENTED_EDGE ( 'NONE', *, *, #103489, .F. ) ;
#200531 = DIRECTION ( 'NONE',  ( 0.000000000000000000, -0.2617529984165152257, -0.9651348961777124202 ) ) ;
#200533 = DIRECTION ( 'NONE',  ( 0.000000000000000000, 0.9910465087640865089, 0.1335171055202864221 ) ) ;
#200534 = AXIS2_PLACEMENT_3D ( 'NONE', #236992, #235692, #219982 ) ;
#200535 = VERTEX_POINT ( 'NONE', #94299 ) ;
#200536 = CARTESIAN_POINT ( 'NONE',  ( -23.15000000000000213, 11.65000000000000036, -12.14999999999999858 ) ) ;
#200537 = CARTESIAN_POINT ( 'NONE',  ( 21.93340585971789736, 60.16248467656392052, -233.9380090624025001 ) ) ;
#200538 = CARTESIAN_POINT ( 'NONE',  ( -18.41809261886922755, -9.682403314745256395, -140.6568435500915086 ) ) ;
#200539 = EDGE_LOOP ( 'NONE', ( #142230, #93251, #252866, #33057 ) ) ;
#200540 = DIRECTION ( 'NONE',  ( 0.000000000000000000, 0.000000000000000000, 1.000000000000000000 ) ) ;
#200541 = ORIENTED_EDGE ( 'NONE', *, *, #150711, .F. ) ;
#200542 = CARTESIAN_POINT ( 'NONE',  ( -18.40000000000000213, 59.44312576075365229, -220.7395490299249445 ) ) ;
#200543 = CARTESIAN_POINT ( 'NONE',  ( -23.25000000000000000, 11.75000000001115552, -155.3500000000000227 ) ) ;
#200544 = CARTESIAN_POINT ( 'NONE',  ( 21.04386569057668410, 36.16263438457939117, -235.9556900804371082 ) ) ;
#200545 = ORIENTED_EDGE ( 'NONE', *, *, #53738, .T. ) ;
#200546 = CARTESIAN_POINT ( 'NONE',  ( -18.59999999999999787, 9.250000000011157297, -188.7499999999999716 ) ) ;
#200547 = DIRECTION ( 'NONE',  ( 1.000000000000000000, 0.000000000000000000, -0.000000000000000000 ) ) ;
#200548 = AXIS2_PLACEMENT_3D ( 'NONE', #17359, #344, #236394 ) ;
#200550 = ADVANCED_FACE ( 'NONE', ( #253380 ), #74790, .F. ) ;
#200549 = AXIS2_PLACEMENT_3D ( 'NONE', #87752, #227271, #68210 ) ;
#200551 = CARTESIAN_POINT ( 'NONE',  ( -20.99749315643150638, 64.25000000001250555, -177.0379132532823974 ) ) ;
#200552 = ORIENTED_EDGE ( 'NONE', *, *, #68482, .F. ) ;
#200553 = VECTOR ( 'NONE', #47717, 1000.000000000000000 ) ;
#200554 = DIRECTION ( 'NONE',  ( 0.000000000000000000, 0.000000000000000000, 1.000000000000000000 ) ) ;
#200555 = CARTESIAN_POINT ( 'NONE',  ( 21.14999999999999503, -11.64999999998883595, -21.75000000000000355 ) ) ;
#200556 = ORIENTED_EDGE ( 'NONE', *, *, #144280, .F. ) ;
#200557 = FACE_OUTER_BOUND ( 'NONE', #180784, .T. ) ;
#200558 = ORIENTED_EDGE ( 'NONE', *, *, #192817, .T. ) ;
#200559 = ORIENTED_EDGE ( 'NONE', *, *, #202464, .F. ) ;
#200560 = DIRECTION ( 'NONE',  ( 0.000000000000000000, 1.000000000000000000, 6.938893903907222067E-15 ) ) ;
#200561 = ORIENTED_EDGE ( 'NONE', *, *, #204291, .T. ) ;
#200563 = VERTEX_POINT ( 'NONE', #134701 ) ;
#200562 = DIRECTION ( 'NONE',  ( 0.000000000000000000, 0.000000000000000000, -1.000000000000000000 ) ) ;
#200564 = EDGE_CURVE ( 'NONE', #32708, #255703, #140104, .T. ) ;
#200565 = CIRCLE ( 'NONE', #108795, 0.1000000000000124678 ) ;
#200566 = EDGE_CURVE ( 'NONE', #14889, #235865, #31806, .T. ) ;
#200569 = VERTEX_POINT ( 'NONE', #170047 ) ;
#200568 = ORIENTED_EDGE ( 'NONE', *, *, #82329, .T. ) ;
#200567 = LINE ( 'NONE', #20670, #196912 ) ;
#200570 = LINE ( 'NONE', #84423, #224591 ) ;
#200571 = CARTESIAN_POINT ( 'NONE',  ( -20.86777300164945004, 65.66799936921481162, -30.42993998886010587 ) ) ;
#200572 = CARTESIAN_POINT ( 'NONE',  ( 18.39999999999998082, 11.47316190337362585, -109.7500000000000284 ) ) ;
#200574 = CARTESIAN_POINT ( 'NONE',  ( 18.59999999999999432, -1.261786168553869603, -41.58649896354548048 ) ) ;
#200573 = DIRECTION ( 'NONE',  ( -1.000000000000000000, 0.000000000000000000, -1.020425574104004196E-15 ) ) ;
#200575 = FACE_OUTER_BOUND ( 'NONE', #194525, .T. ) ;
#200576 = ADVANCED_FACE ( 'NONE', ( #228704 ), #190878, .T. ) ;
#200577 = DIRECTION ( 'NONE',  ( 1.000000000000000000, 0.000000000000000000, 0.000000000000000000 ) ) ;
#200578 = CARTESIAN_POINT ( 'NONE',  ( 21.05000000000000071, 76.00000000001162448, -65.22310748452429152 ) ) ;
#200580 = CARTESIAN_POINT ( 'NONE',  ( -18.50000000000000000, 72.08710075277812734, -58.04128451151338197 ) ) ;
#200579 = CARTESIAN_POINT ( 'NONE',  ( -21.05000000000000071, 68.51069317435826633, -224.1259271199053842 ) ) ;
#200581 = ORIENTED_EDGE ( 'NONE', *, *, #174037, .T. ) ;
#200582 = ORIENTED_EDGE ( 'NONE', *, *, #217476, .T. ) ;
#200583 = EDGE_CURVE ( 'NONE', #166628, #119302, #139696, .T. ) ;
#200584 = CARTESIAN_POINT ( 'NONE',  ( -23.25000000000000000, 71.65000000001253966, -182.1731074845243938 ) ) ;
#200587 = EDGE_LOOP ( 'NONE', ( #235847, #112677, #147988, #251784 ) ) ;
#200586 = EDGE_CURVE ( 'NONE', #89321, #128154, #65119, .T. ) ;
#200585 = DIRECTION ( 'NONE',  ( 0.000000000000000000, 6.308085367188393199E-16, 1.000000000000000000 ) ) ;
#200588 = ORIENTED_EDGE ( 'NONE', *, *, #181284, .F. ) ;
#200590 = DIRECTION ( 'NONE',  ( 0.000000000000000000, 0.2128009952263603677, -0.9770955615653313941 ) ) ;
#200589 = AXIS2_PLACEMENT_3D ( 'NONE', #30283, #10712, #152822 ) ;
#200591 = ORIENTED_EDGE ( 'NONE', *, *, #150844, .T. ) ;
#200592 = DIRECTION ( 'NONE',  ( 0.000000000000000000, 1.000000000000000000, 0.000000000000000000 ) ) ;
#200593 = EDGE_CURVE ( 'NONE', #3876, #71987, #202662, .T. ) ;
#200594 = CIRCLE ( 'NONE', #121519, 0.09999999999999939493 ) ;
#200595 = B_SPLINE_CURVE_WITH_KNOTS ( 'NONE', 3,
 ( #32401, #93624, #114469, #134022, #229295, #31125, #209725, #74096, #153657, #91058 ),
 .UNSPECIFIED., .F., .F.,
 ( 4, 2, 2, 2, 4 ),
 ( 5.247129907028296623E-16, 9.930191194499898442E-05, 0.0001986038238894732421, 0.0003972076477784217846, 0.0007944152955563189237 ),
 .UNSPECIFIED. ) ;
#200596 = ORIENTED_EDGE ( 'NONE', *, *, #244456, .T. ) ;
#200597 = EDGE_CURVE ( 'NONE', #176995, #2636, #83373, .T. ) ;
#200599 = CIRCLE ( 'NONE', #88134, 0.09999999999999939493 ) ;
#200598 = DIRECTION ( 'NONE',  ( 1.000000000000000000, 0.000000000000000000, 0.000000000000000000 ) ) ;
#200600 = CARTESIAN_POINT ( 'NONE',  ( 20.94999999999999929, 23.68770167995059239, -252.8127582590406348 ) ) ;
#200602 = ORIENTED_EDGE ( 'NONE', *, *, #4249, .F. ) ;
#200601 = VERTEX_POINT ( 'NONE', #24749 ) ;
#200603 = ORIENTED_EDGE ( 'NONE', *, *, #179140, .T. ) ;
#200605 = CARTESIAN_POINT ( 'NONE',  ( -21.14999999999999858, 11.65000000000000036, -0.1000000000000028644 ) ) ;
#200604 = VECTOR ( 'NONE', #223141, 1000.000000000000000 ) ;
#200607 = VERTEX_POINT ( 'NONE', #3868 ) ;
#200606 = EDGE_CURVE ( 'NONE', #147041, #228499, #136003, .T. ) ;
#200608 = ORIENTED_EDGE ( 'NONE', *, *, #218988, .F. ) ;
#200609 = CARTESIAN_POINT ( 'NONE',  ( 20.99999999999999645, 9.750000000011137757, -188.3499999999999659 ) ) ;
#200610 = AXIS2_PLACEMENT_3D ( 'NONE', #32060, #185968, #148130 ) ;
#200612 = ORIENTED_EDGE ( 'NONE', *, *, #160481, .T. ) ;
#200611 = DIRECTION ( 'NONE',  ( 0.7071067811865127117, 0.7071067811865821007, 0.000000000000000000 ) ) ;
#200613 = ADVANCED_FACE ( 'NONE', ( #125118 ), #240514, .T. ) ;
#200615 = CARTESIAN_POINT ( 'NONE',  ( 20.85000000000000142, 77.83585931145546510, -91.51866831572576189 ) ) ;
#200614 = DIRECTION ( 'NONE',  ( -1.000000000000000000, 0.000000000000000000, 0.000000000000000000 ) ) ;
#200616 = CARTESIAN_POINT ( 'NONE',  ( 5.900000000000060751, 64.35000000001120668, -22.12310748452479103 ) ) ;
#200617 = DIRECTION ( 'NONE',  ( 0.2834754621636358940, -0.2834754621636437211, 0.9161240771326893961 ) ) ;
#200618 = CARTESIAN_POINT ( 'NONE',  ( -18.37013991200266005, 11.49974761622312691, -176.7069769894828539 ) ) ;
#200619 = ORIENTED_EDGE ( 'NONE', *, *, #83752, .F. ) ;
#200620 = AXIS2_PLACEMENT_3D ( 'NONE', #232423, #20752, #119860 ) ;
#200622 = EDGE_CURVE ( 'NONE', #212963, #232095, #115184, .T. ) ;
#200621 = ORIENTED_EDGE ( 'NONE', *, *, #134485, .T. ) ;
#200623 = CARTESIAN_POINT ( 'NONE',  ( -18.59999999999999787, 77.16270174995034381, -161.9231074845243370 ) ) ;
#200624 = AXIS2_PLACEMENT_3D ( 'NONE', #3098, #180483, #1819 ) ;
#200625 = CARTESIAN_POINT ( 'NONE',  ( -0.8999999999999993561, -11.65000000000000036, 28.60000000000000142 ) ) ;
#200626 = DIRECTION ( 'NONE',  ( 0.000000000000000000, 0.000000000000000000, 1.000000000000000000 ) ) ;
#200627 = B_SPLINE_CURVE_WITH_KNOTS ( 'NONE', 3,
 ( #119199, #57910, #159610, #154499, #233990, #55325, #117895, #137451, #177895, #20100 ),
 .UNSPECIFIED., .F., .F.,
 ( 4, 3, 3, 4 ),
 ( 3.103167691559091397E-17, 0.0002000000000008536833, 0.001000000000082982687, 0.001967863649483335420 ),
 .UNSPECIFIED. ) ;
#200629 = ORIENTED_EDGE ( 'NONE', *, *, #174319, .T. ) ;
#200628 = AXIS2_PLACEMENT_3D ( 'NONE', #189912, #210754, #8705 ) ;
#200630 = CARTESIAN_POINT ( 'NONE',  ( 21.05000000000000071, 10.72371711693665652, -45.67623960113817816 ) ) ;
#200631 = CIRCLE ( 'NONE', #38321, 0.09999999999999939493 ) ;
#200632 = DIRECTION ( 'NONE',  ( 0.7071067811865474617, 0.7071067811865474617, 2.044391222244499837E-16 ) ) ;
#200633 = CARTESIAN_POINT ( 'NONE',  ( 22.84999999999999787, 0.000000000000000000, 0.000000000000000000 ) ) ;
#200634 = ORIENTED_EDGE ( 'NONE', *, *, #87162, .F. ) ;
#200635 = VERTEX_POINT ( 'NONE', #230631 ) ;
#200636 = CIRCLE ( 'NONE', #125781, 0.09999999999998898659 ) ;
#200637 = EDGE_CURVE ( 'NONE', #211554, #200161, #81823, .T. ) ;
#200638 = DIRECTION ( 'NONE',  ( -1.000000000000000000, -0.000000000000000000, -0.000000000000000000 ) ) ;
#200639 = LINE ( 'NONE', #143210, #114934 ) ;
#200640 = VERTEX_POINT ( 'NONE', #188928 ) ;
#200641 = VERTEX_POINT ( 'NONE', #89808 ) ;
#200642 = DIRECTION ( 'NONE',  ( 1.000000000000000000, 0.000000000000000000, 0.000000000000000000 ) ) ;
#200644 = VECTOR ( 'NONE', #142451, 1000.000000000000000 ) ;
#200643 = CYLINDRICAL_SURFACE ( 'NONE', #133026, 0.09999999999999892308 ) ;
#200646 = CARTESIAN_POINT ( 'NONE',  ( -20.94983749550516450, 68.01715840423028681, -224.2192812407665201 ) ) ;
#200645 = DIRECTION ( 'NONE',  ( 0.000000000000000000, 0.000000000000000000, 1.000000000000000000 ) ) ;
#200647 = DIRECTION ( 'NONE',  ( 0.000000000000000000, 1.000000000000000000, 0.000000000000000000 ) ) ;
#200648 = CARTESIAN_POINT ( 'NONE',  ( -18.59999999999999787, 9.350000000000001421, -12.14999999999999858 ) ) ;
#200649 = VERTEX_POINT ( 'NONE', #50670 ) ;
#200650 = DIRECTION ( 'NONE',  ( 0.000000000000000000, 0.2128009952263603677, -0.9770955615653313941 ) ) ;
#200651 = CIRCLE ( 'NONE', #88177, 11.65000000000000036 ) ;
#200652 = EDGE_CURVE ( 'NONE', #246496, #25668, #69409, .T. ) ;
#200654 = VERTEX_POINT ( 'NONE', #166832 ) ;
#200653 = ORIENTED_EDGE ( 'NONE', *, *, #188872, .F. ) ;
#200656 = ORIENTED_EDGE ( 'NONE', *, *, #35122, .F. ) ;
#200655 = AXIS2_PLACEMENT_3D ( 'NONE', #74346, #172173, #15650 ) ;
#200657 = ORIENTED_EDGE ( 'NONE', *, *, #43350, .F. ) ;
#200658 = CARTESIAN_POINT ( 'NONE',  ( -20.54999999999999716, 76.00000000001213607, -136.5231074845243313 ) ) ;
#200659 = DIRECTION ( 'NONE',  ( 0.000000000000000000, 0.9887567792719341719, -0.1495327102803664099 ) ) ;
#200660 = DIRECTION ( 'NONE',  ( 0.000000000000000000, 6.938893903907229955E-15, -1.000000000000000000 ) ) ;
#200661 = DIRECTION ( 'NONE',  ( 0.000000000000000000, -0.1350103645451876666, 0.9908441862701600211 ) ) ;
#200662 = ADVANCED_FACE ( 'NONE', ( #66413 ), #151090, .T. ) ;
#200664 = CARTESIAN_POINT ( 'NONE',  ( -20.94999999999999929, 87.48912529308798014, -99.92310748452423752 ) ) ;
#200663 = CARTESIAN_POINT ( 'NONE',  ( -23.25000000000000000, -8.999999999988844479, -124.1060308773475924 ) ) ;
#200666 = ORIENTED_EDGE ( 'NONE', *, *, #194767, .T. ) ;
#200665 = FACE_OUTER_BOUND ( 'NONE', #103663, .T. ) ;
#200667 = CARTESIAN_POINT ( 'NONE',  ( -20.65000000000000568, 42.13647595316535188, -239.1530172309881834 ) ) ;
#200668 = ORIENTED_EDGE ( 'NONE', *, *, #138885, .T. ) ;
#200669 = DIRECTION ( 'NONE',  ( 1.186688945009009831E-16, -1.000000000000000000, 0.000000000000000000 ) ) ;
#200670 = ORIENTED_EDGE ( 'NONE', *, *, #240222, .T. ) ;
#200671 = ORIENTED_EDGE ( 'NONE', *, *, #77415, .F. ) ;
#200672 = DIRECTION ( 'NONE',  ( 0.000000000000000000, 0.000000000000000000, -1.000000000000000000 ) ) ;
#200673 = SPHERICAL_SURFACE ( 'NONE', #189322, 0.1000000000000000056 ) ;
#200675 = ADVANCED_FACE ( 'NONE', ( #147226 ), #145934, .T. ) ;
#200674 = CARTESIAN_POINT ( 'NONE',  ( -21.05000000000000071, 76.02110330807143157, -209.8276238137888186 ) ) ;
#200676 = EDGE_CURVE ( 'NONE', #241192, #97342, #240093, .T. ) ;
#200677 = CARTESIAN_POINT ( 'NONE',  ( 21.05000000000000071, 69.28189128378591022, -247.5258150475912089 ) ) ;
#200678 = EDGE_CURVE ( 'NONE', #243219, #135228, #23644, .T. ) ;
#200679 = AXIS2_PLACEMENT_3D ( 'NONE', #11095, #9800, #255762 ) ;
#200680 = EDGE_CURVE ( 'NONE', #182596, #223140, #169392, .T. ) ;
#200681 = DIRECTION ( 'NONE',  ( 0.000000000000000000, -0.2128009952263403282, 0.9770955615653358350 ) ) ;
#200682 = ORIENTED_EDGE ( 'NONE', *, *, #119576, .F. ) ;
#200683 = ORIENTED_EDGE ( 'NONE', *, *, #103341, .T. ) ;
#200684 = ADVANCED_FACE ( 'NONE', ( #209777 ), #229086, .T. ) ;
#200685 = FACE_OUTER_BOUND ( 'NONE', #27228, .T. ) ;
#200686 = ORIENTED_EDGE ( 'NONE', *, *, #234546, .T. ) ;
#200687 = CARTESIAN_POINT ( 'NONE',  ( -23.25000000000000000, 65.66751761918619934, -30.42826094061123854 ) ) ;
#200688 = CARTESIAN_POINT ( 'NONE',  ( 21.14999999999999858, 6.650000000011155876, -79.25000000000004263 ) ) ;
#200689 = SPHERICAL_SURFACE ( 'NONE', #162796, 0.1000000000000000056 ) ;
#200690 = CARTESIAN_POINT ( 'NONE',  ( -16.77977881697927032, 66.05339806647896239, -90.36172891140932961 ) ) ;
#200691 = CARTESIAN_POINT ( 'NONE',  ( -20.85000000000000142, 7.882824859404637508, -245.3558965132535832 ) ) ;
#200692 = DIRECTION ( 'NONE',  ( 1.000000000000000000, 0.000000000000000000, 0.000000000000000000 ) ) ;
#200693 = CYLINDRICAL_SURFACE ( 'NONE', #41764, 0.09999999999999939493 ) ;
#200694 = CARTESIAN_POINT ( 'NONE',  ( 21.05000000000000071, 5.400000000011154988, -146.4052660189131245 ) ) ;
#200695 = DIRECTION ( 'NONE',  ( 1.000000000000000000, -3.265361837132813093E-16, -2.280189983783949500E-30 ) ) ;
#200696 = DIRECTION ( 'NONE',  ( -0.000000000000000000, -0.9550021345545507412, 0.2965989261549202838 ) ) ;
#200697 = ADVANCED_FACE ( 'NONE', ( #33751 ), #235740, .F. ) ;
#200699 = ORIENTED_EDGE ( 'NONE', *, *, #251716, .F. ) ;
#200698 = VECTOR ( 'NONE', #147481, 1000.000000000000000 ) ;
#200700 = CARTESIAN_POINT ( 'NONE',  ( 20.95568717954149562, 10.60199405390297400, -41.10250836826865140 ) ) ;
#200701 = EDGE_LOOP ( 'NONE', ( #209884, #148878, #4106, #97925 ) ) ;
#200702 = EDGE_CURVE ( 'NONE', #252199, #62638, #90213, .T. ) ;
#200703 = ADVANCED_FACE ( 'NONE', ( #231922 ), #254017, .T. ) ;
#200704 = LINE ( 'NONE', #53803, #229135 ) ;
#200705 = LINE ( 'NONE', #75641, #190895 ) ;
#200706 = DIRECTION ( 'NONE',  ( -1.000000000000000000, -0.000000000000000000, -0.000000000000000000 ) ) ;
#200707 = EDGE_LOOP ( 'NONE', ( #132724, #77191, #32757, #256231 ) ) ;
#200708 = CARTESIAN_POINT ( 'NONE',  ( 21.14999999999999858, 76.00000000001213607, -136.4231074845243086 ) ) ;
#200709 = DIRECTION ( 'NONE',  ( 0.000000000000000000, 0.000000000000000000, -1.000000000000000000 ) ) ;
#200710 = CARTESIAN_POINT ( 'NONE',  ( -23.25000000000000000, 7.804459559388685186, -245.4620200072988325 ) ) ;
#200711 = AXIS2_PLACEMENT_3D ( 'NONE', #35246, #114752, #16945 ) ;
#200712 = VECTOR ( 'NONE', #34883, 1000.000000000000000 ) ;
#200713 = DIRECTION ( 'NONE',  ( 0.000000000000000000, -0.01562499999996343723, -0.9998779222360104635 ) ) ;
#200714 = DIRECTION ( 'NONE',  ( 0.000000000000000000, 6.982962677686266711E-15, -1.000000000000000000 ) ) ;
#200716 = CARTESIAN_POINT ( 'NONE',  ( -18.59999999999999787, 77.85102823015273543, -91.36919421510179973 ) ) ;
#200715 = CIRCLE ( 'NONE', #234013, 0.09999999999999950595 ) ;
#200717 = ADVANCED_BREP_SHAPE_REPRESENTATION ( '', ( #190377, #2425 ), #197867 ) ;
#200718 = VERTEX_POINT ( 'NONE', #237037 ) ;
#200719 = DIRECTION ( 'NONE',  ( 1.000000000000000000, 0.000000000000000000, 0.000000000000000000 ) ) ;
#200721 = ORIENTED_EDGE ( 'NONE', *, *, #234321, .T. ) ;
#200720 = DIRECTION ( 'NONE',  ( 0.000000000000000000, 0.8660254037844419273, -0.4999999999999942824 ) ) ;
#200722 = CARTESIAN_POINT ( 'NONE',  ( 20.94999999999999929, 76.00000000001170974, -69.52310748452431710 ) ) ;
#200723 = CARTESIAN_POINT ( 'NONE',  ( 20.94999999999999929, -9.399999999988846611, -177.3939691226524076 ) ) ;
#200724 = CARTESIAN_POINT ( 'NONE',  ( -18.59999999999999787, 11.64999999999999680, -33.50000000000000000 ) ) ;
#200725 = ORIENTED_EDGE ( 'NONE', *, *, #55536, .F. ) ;
#200726 = CARTESIAN_POINT ( 'NONE',  ( 18.39999999999999503, 67.17743825834580207, -145.7731074845244450 ) ) ;
#200727 = SHAPE_DEFINITION_REPRESENTATION ( #82997, #18588 ) ;
#200728 = CARTESIAN_POINT ( 'NONE',  ( 23.24999999999999645, 71.22429906543287359, -158.1743393804784148 ) ) ;
#200729 = AXIS2_PLACEMENT_3D ( 'NONE', #137708, #239406, #19064 ) ;
#200730 = VERTEX_POINT ( 'NONE', #53270 ) ;
#200731 = FACE_OUTER_BOUND ( 'NONE', #78002, .T. ) ;
#200732 = DIRECTION ( 'NONE',  ( 0.000000000000000000, 1.000000000000000000, 0.000000000000000000 ) ) ;
#200733 = CARTESIAN_POINT ( 'NONE',  ( -22.50000000000000000, 76.00000000001173817, -81.17267829206912211 ) ) ;
#200734 = ORIENTED_EDGE ( 'NONE', *, *, #251731, .F. ) ;
#200735 = VERTEX_POINT ( 'NONE', #54542 ) ;
#200736 = DIRECTION ( 'NONE',  ( 1.073024830501117528E-15, -0.8814952561688430555, 0.4721928772777346239 ) ) ;
#200737 = DIRECTION ( 'NONE',  ( -1.073024830501117725E-15, -6.982962677686266711E-15, 1.000000000000000000 ) ) ;
#200738 = DIRECTION ( 'NONE',  ( 1.000000000000000000, -0.000000000000000000, -0.000000000000000000 ) ) ;
#200739 = LINE ( 'NONE', #101595, #2869 ) ;
#200740 = ADVANCED_FACE ( 'NONE', ( #74146 ), #235974, .T. ) ;
#200742 = DIRECTION ( 'NONE',  ( -1.000000000000000000, 0.000000000000000000, 0.000000000000000000 ) ) ;
#200741 = CIRCLE ( 'NONE', #150846, 0.1000000000000086514 ) ;
#200743 = CIRCLE ( 'NONE', #9208, 0.09999999999999158173 ) ;
#200746 = FACE_OUTER_BOUND ( 'NONE', #225823, .T. ) ;
#200745 = AXIS2_PLACEMENT_3D ( 'NONE', #44867, #141385, #65707 ) ;
#200744 = DIRECTION ( 'NONE',  ( -1.000000000000000000, -1.159508501126949537E-16, -2.525285885220370376E-17 ) ) ;
#200747 = LINE ( 'NONE', #100331, #111117 ) ;
#200748 = ADVANCED_FACE ( 'NONE', ( #92380 ), #97286, .T. ) ;
#200749 = DIRECTION ( 'NONE',  ( 0.000000000000000000, -0.2128009952263604232, 0.9770955615653316162 ) ) ;
#200750 = CARTESIAN_POINT ( 'NONE',  ( 22.46250603428203618, 0.02114417614996233138, -155.8501369026598979 ) ) ;
#200751 = PLANE ( 'NONE',  #238890 ) ;
#200752 = ORIENTED_EDGE ( 'NONE', *, *, #159460, .F. ) ;
#200753 = VERTEX_POINT ( 'NONE', #36288 ) ;
#200754 = CARTESIAN_POINT ( 'NONE',  ( 21.05000000000000071, 1.115600667400684642E-11, -67.00000000000000000 ) ) ;
#200756 = CARTESIAN_POINT ( 'NONE',  ( 21.06600267594171783, 67.22483393081269298, -191.3188447021496756 ) ) ;
#200755 = DIRECTION ( 'NONE',  ( 0.000000000000000000, -0.7071067811865479058, -0.7071067811865472397 ) ) ;
#200757 = EDGE_CURVE ( 'NONE', #197707, #41986, #46406, .T. ) ;
#200758 = EDGE_CURVE ( 'NONE', #167819, #153879, #11131, .T. ) ;
#200759 = FACE_BOUND ( 'NONE', #128857, .T. ) ;
#200760 = FACE_OUTER_BOUND ( 'NONE', #164629, .T. ) ;
#200761 = DIRECTION ( 'NONE',  ( 1.186688945009009584E-16, -0.4721928772777346239, -0.8814952561688430555 ) ) ;
#200762 = ORIENTED_EDGE ( 'NONE', *, *, #218439, .F. ) ;
#200763 = CARTESIAN_POINT ( 'NONE',  ( 20.99999999999999645, 66.25000000001190870, -93.77310748452438816 ) ) ;
#200764 = ORIENTED_EDGE ( 'NONE', *, *, #208654, .F. ) ;
#200765 = LINE ( 'NONE', #101621, #121997 ) ;
#200766 = VERTEX_POINT ( 'NONE', #77945 ) ;
#200767 = CARTESIAN_POINT ( 'NONE',  ( 23.14999999999999503, 11.75000000001116263, -160.4851942293460638 ) ) ;
#200768 = VECTOR ( 'NONE', #112420, 1000.000000000000000 ) ;
#200769 = ADVANCED_FACE ( 'NONE', ( #177089 ), #111972, .T. ) ;
#200770 = EDGE_CURVE ( 'NONE', #47818, #147926, #240892, .T. ) ;
#200771 = CARTESIAN_POINT ( 'NONE',  ( 18.46163235739468789, 85.48015080692967160, -29.36549694464667226 ) ) ;
#200772 = ORIENTED_EDGE ( 'NONE', *, *, #19837, .F. ) ;
#200773 = DIRECTION ( 'NONE',  ( 1.000000000000000000, 0.000000000000000000, 0.000000000000000000 ) ) ;
#200774 = CIRCLE ( 'NONE', #13342, 0.09999999999999939493 ) ;
#200775 = ORIENTED_EDGE ( 'NONE', *, *, #61717, .F. ) ;
#200776 = CARTESIAN_POINT ( 'NONE',  ( 23.14999999999999503, 64.35000000001249987, -177.0379132551783812 ) ) ;
#200777 = CARTESIAN_POINT ( 'NONE',  ( -18.40000000000000213, 11.47316190337362762, -46.04999999999999716 ) ) ;
#200779 = AXIS2_PLACEMENT_3D ( 'NONE', #121184, #19489, #256749 ) ;
#200778 = CARTESIAN_POINT ( 'NONE',  ( -18.50000000000000000, -1.736257131586239844, -145.5686523290175387 ) ) ;
#200780 = DIRECTION ( 'NONE',  ( 0.000000000000000000, 0.5000000000000078826, -0.8660254037844340447 ) ) ;
#200781 = DIRECTION ( 'NONE',  ( 0.000000000000000000, 0.9915357197604973694, -0.1298341882519105928 ) ) ;
#200782 = ADVANCED_FACE ( 'NONE', ( #79219 ), #34157, .T. ) ;
#200784 = DIRECTION ( 'NONE',  ( 1.000000000000000000, 0.000000000000000000, 0.000000000000000000 ) ) ;
#200783 = CARTESIAN_POINT ( 'NONE',  ( -16.97048361161167307, 66.05000000001257376, -183.1642231400940375 ) ) ;
#200785 = CIRCLE ( 'NONE', #163379, 0.09999999999999939493 ) ;
#200787 = CARTESIAN_POINT ( 'NONE',  ( 21.00000000000000000, 9.749999999999998224, -12.25000000000000000 ) ) ;
#200786 = AXIS2_PLACEMENT_3D ( 'NONE', #78211, #236004, #155226 ) ;
#200788 = TOROIDAL_SURFACE ( 'NONE', #175864, 0.9750000000000019762, 0.1000000000000000056 ) ;
#200791 = ORIENTED_EDGE ( 'NONE', *, *, #160954, .T. ) ;
#200790 = ADVANCED_FACE ( 'NONE', ( #137914 ), #143048, .F. ) ;
#200789 = DIRECTION ( 'NONE',  ( -1.000000000000000000, 0.000000000000000000, -0.000000000000000000 ) ) ;
#200793 = DIRECTION ( 'NONE',  ( 0.000000000000000000, 0.9915357197604982575, -0.1298341882519033486 ) ) ;
#200792 = CARTESIAN_POINT ( 'NONE',  ( 21.72449340488910252, 10.28395627750227703, -180.1499999999999773 ) ) ;
#200794 = EDGE_LOOP ( 'NONE', ( #130069, #186806, #140668, #12992 ) ) ;
#200796 = ORIENTED_EDGE ( 'NONE', *, *, #217708, .F. ) ;
#200795 = CARTESIAN_POINT ( 'NONE',  ( -18.50000000000000000, -1.687074390080403941, -154.6854270334582964 ) ) ;
#200797 = VERTEX_POINT ( 'NONE', #239610 ) ;
#200798 = CARTESIAN_POINT ( 'NONE',  ( 23.14999999999998437, 11.75000000000000000, 0.000000000000000000 ) ) ;
#200799 = CIRCLE ( 'NONE', #246572, 0.09999999999998898659 ) ;
#200800 = DIRECTION ( 'NONE',  ( 0.000000000000000000, 0.2128009952263403282, -0.9770955615653358350 ) ) ;
#200801 = CARTESIAN_POINT ( 'NONE',  ( -14.00000000000000178, 9.850000000011133849, -184.2499999999999716 ) ) ;
#200802 = ORIENTED_EDGE ( 'NONE', *, *, #213846, .F. ) ;
#200803 = LINE ( 'NONE', #22183, #246240 ) ;
#200804 = DIRECTION ( 'NONE',  ( 0.000000000000000000, 0.9126074666063771490, 0.4088369013363281623 ) ) ;
#200805 = PLANE ( 'NONE',  #185622 ) ;
#200806 = EDGE_CURVE ( 'NONE', #213256, #66123, #203030, .T. ) ;
#200807 = ORIENTED_EDGE ( 'NONE', *, *, #188096, .T. ) ;
#200808 = AXIS2_PLACEMENT_3D ( 'NONE', #76535, #97352, #234325 ) ;
#200809 = CARTESIAN_POINT ( 'NONE',  ( -18.50000972452446035, 46.33166059915856039, -243.0555356998360423 ) ) ;
#200810 = AXIS2_PLACEMENT_3D ( 'NONE', #201025, #100593, #156785 ) ;
#200811 = CARTESIAN_POINT ( 'NONE',  ( 21.08198257630413508, 69.66340326599708987, -136.5957508083089351 ) ) ;
#200813 = EDGE_CURVE ( 'NONE', #179043, #13961, #52629, .T. ) ;
#200812 = VECTOR ( 'NONE', #214595, 1000.000000000000000 ) ;
#200814 = VERTEX_POINT ( 'NONE', #83050 ) ;
#200815 = ORIENTED_EDGE ( 'NONE', *, *, #234164, .T. ) ;
#200816 = DIRECTION ( 'NONE',  ( 1.000000000000000000, 0.000000000000000000, 0.000000000000000000 ) ) ;
#200817 = AXIS2_PLACEMENT_3D ( 'NONE', #167665, #247163, #208073 ) ;
#200818 = EDGE_LOOP ( 'NONE', ( #94836, #172450, #151184, #48619, #192873 ) ) ;
#200819 = CARTESIAN_POINT ( 'NONE',  ( -20.54999999999999716, 7.250000000011155521, -188.7499999999999716 ) ) ;
#200820 = ORIENTED_EDGE ( 'NONE', *, *, #200806, .F. ) ;
#200821 = DIRECTION ( 'NONE',  ( 0.000000000000000000, 1.000000000000000000, 0.000000000000000000 ) ) ;
#200822 = CIRCLE ( 'NONE', #138429, 0.09999999999998898659 ) ;
#200823 = DIRECTION ( 'NONE',  ( 0.000000000000000000, 0.000000000000000000, 1.000000000000000000 ) ) ;
#200824 = DIRECTION ( 'NONE',  ( 0.000000000000000000, -1.000000000000000000, 0.000000000000000000 ) ) ;
#200825 = EDGE_CURVE ( 'NONE', #23721, #236193, #81773, .T. ) ;
#200826 = CIRCLE ( 'NONE', #188341, 12.97499999999998721 ) ;
#200827 = DIRECTION ( 'NONE',  ( 0.000000000000000000, 6.982962677686266711E-15, -1.000000000000000000 ) ) ;
#200828 = CARTESIAN_POINT ( 'NONE',  ( 18.54999999999999716, 64.24389422848744857, -213.4417251850286164 ) ) ;
#200829 = EDGE_LOOP ( 'NONE', ( #198281, #200568 ) ) ;
#200831 = ADVANCED_FACE ( 'NONE', ( #162642 ), #44021, .T. ) ;
#200830 = DIRECTION ( 'NONE',  ( 0.000000000000000000, -1.000000000000000000, 0.000000000000000000 ) ) ;
#200832 = CARTESIAN_POINT ( 'NONE',  ( 18.59999999999996945, 68.97833521811159585, -65.68954208262705663 ) ) ;
#200833 = FACE_OUTER_BOUND ( 'NONE', #185508, .T. ) ;
#200834 = EDGE_LOOP ( 'NONE', ( #147172, #220865, #229061, #42161 ) ) ;
#200836 = CARTESIAN_POINT ( 'NONE',  ( 22.48970261584622321, 64.35000000001214460, -136.5784769727417824 ) ) ;
#200835 = CARTESIAN_POINT ( 'NONE',  ( 21.05000000000000071, 44.58277672189309015, -247.4925639031954745 ) ) ;
#200837 = VECTOR ( 'NONE', #174493, 1000.000000000000000 ) ;
#200838 = VERTEX_POINT ( 'NONE', #105174 ) ;
#200841 = ORIENTED_EDGE ( 'NONE', *, *, #128612, .F. ) ;
#200840 = FILL_AREA_STYLE_COLOUR ( '', #100472 ) ;
#200839 = LINE ( 'NONE', #118746, #198812 ) ;
#200842 = AXIS2_PLACEMENT_3D ( 'NONE', #30505, #184412, #68334 ) ;
#200843 = ORIENTED_EDGE ( 'NONE', *, *, #239413, .F. ) ;
#200844 = AXIS2_PLACEMENT_3D ( 'NONE', #109257, #46717, #68883 ) ;
#200845 = LINE ( 'NONE', #160459, #65292 ) ;
#200846 = DIRECTION ( 'NONE',  ( 0.000000000000000000, 0.000000000000000000, -1.000000000000000000 ) ) ;
#200847 = ORIENTED_EDGE ( 'NONE', *, *, #69356, .F. ) ;
#200848 = CARTESIAN_POINT ( 'NONE',  ( 20.01093837587850288, 16.74863325871518427, -222.6870001686604610 ) ) ;
#200849 = DIRECTION ( 'NONE',  ( 1.000000000000000000, 0.000000000000000000, 0.000000000000000000 ) ) ;
#200851 = DIRECTION ( 'NONE',  ( 0.000000000000000000, 1.000000000000000000, 6.982962677686266711E-15 ) ) ;
#200850 = CARTESIAN_POINT ( 'NONE',  ( 21.15000000000005542, 73.94408376456904364, -49.16694968567509250 ) ) ;
#200852 = VERTEX_POINT ( 'NONE', #50357 ) ;
#200853 = ORIENTED_EDGE ( 'NONE', *, *, #127434, .T. ) ;
#200854 = AXIS2_PLACEMENT_3D ( 'NONE', #203226, #122417, #79409 ) ;
#200855 = DIRECTION ( 'NONE',  ( 0.000000000000000000, 0.000000000000000000, -1.000000000000000000 ) ) ;
#200856 = CYLINDRICAL_SURFACE ( 'NONE', #155532, 0.09999999999999939493 ) ;
#200857 = ORIENTED_EDGE ( 'NONE', *, *, #163245, .F. ) ;
#200858 = DIRECTION ( 'NONE',  ( 0.000000000000000000, 0.000000000000000000, -1.000000000000000000 ) ) ;
#200859 = ORIENTED_EDGE ( 'NONE', *, *, #67270, .T. ) ;
#200860 = DIRECTION ( 'NONE',  ( 0.000000000000000000, 0.000000000000000000, 1.000000000000000000 ) ) ;
#200861 = CARTESIAN_POINT ( 'NONE',  ( 22.50046968638156386, 75.95483015287055650, -114.7731526389968479 ) ) ;
#200862 = CARTESIAN_POINT ( 'NONE',  ( -20.54999999999999716, 66.65000000001180069, -81.77310748452437394 ) ) ;
#200863 = ORIENTED_EDGE ( 'NONE', *, *, #224641, .F. ) ;
#200864 = FACE_OUTER_BOUND ( 'NONE', #226983, .T. ) ;
#200865 = EDGE_CURVE ( 'NONE', #181359, #15440, #28292, .T. ) ;
#200866 = DIRECTION ( 'NONE',  ( 1.000000000000000000, 0.000000000000000000, 0.000000000000000000 ) ) ;
#200868 = ORIENTED_EDGE ( 'NONE', *, *, #51924, .F. ) ;
#200867 = CIRCLE ( 'NONE', #100864, 0.09999999999999939493 ) ;
#200869 = ORIENTED_EDGE ( 'NONE', *, *, #248597, .F. ) ;
#200870 = ORIENTED_EDGE ( 'NONE', *, *, #65345, .F. ) ;
#200871 = FACE_OUTER_BOUND ( 'NONE', #148969, .T. ) ;
#200873 = EDGE_CURVE ( 'NONE', #142216, #208289, #110352, .T. ) ;
#200872 = VERTEX_POINT ( 'NONE', #205591 ) ;
#200875 = ORIENTED_EDGE ( 'NONE', *, *, #201077, .F. ) ;
#200874 = CYLINDRICAL_SURFACE ( 'NONE', #188517, 0.1000000000000028644 ) ;
#200876 = ORIENTED_EDGE ( 'NONE', *, *, #161177, .F. ) ;
#200877 = EDGE_CURVE ( 'NONE', #32374, #145748, #206760, .T. ) ;
#200880 = ORIENTED_EDGE ( 'NONE', *, *, #179217, .T. ) ;
#200879 = VERTEX_POINT ( 'NONE', #106476 ) ;
#200878 = CARTESIAN_POINT ( 'NONE',  ( 21.05000000000000071, 5.400000000011154988, -121.5947339810869465 ) ) ;
#200881 = VECTOR ( 'NONE', #225382, 1000.000000000000000 ) ;
#200882 = ORIENTED_EDGE ( 'NONE', *, *, #43825, .T. ) ;
#200883 = DIRECTION ( 'NONE',  ( -7.304098846217948299E-16, -1.000000000000000000, 0.000000000000000000 ) ) ;
#200884 = CARTESIAN_POINT ( 'NONE',  ( -23.25000000000000000, 67.23127455305841238, -235.8551265064783991 ) ) ;
#200885 = CIRCLE ( 'NONE', #155141, 0.09999999999998898659 ) ;
#200886 = DIRECTION ( 'NONE',  ( -1.000000000000000000, -0.000000000000000000, 0.000000000000000000 ) ) ;
#200887 = ORIENTED_EDGE ( 'NONE', *, *, #70734, .F. ) ;
#200888 = CIRCLE ( 'NONE', #25942, 4.300000000000025580 ) ;
#200889 = EDGE_CURVE ( 'NONE', #90736, #182355, #115354, .T. ) ;
#200890 = DIRECTION ( 'NONE',  ( -1.000000000000000000, 0.000000000000000000, 0.000000000000000000 ) ) ;
#200891 =( BOUNDED_SURFACE ( )  B_SPLINE_SURFACE ( 3, 2, ( 
 ( #102378, #24182, #133538 ),
 ( #110119, #170143, #93119 ),
 ( #150543, #211802, #188374 ),
 ( #172717, #210512, #12333 ),
 ( #13601, #53998, #11024 ),
 ( #29344, #189663, #112697 ),
 ( #230070, #151845, #91845 ),
 ( #69730, #149272, #171423 ) ),
 .UNSPECIFIED., .F., .F., .F. ) 
 B_SPLINE_SURFACE_WITH_KNOTS ( ( 4, 2, 2, 4 ),
 ( 3, 3 ),
 ( 0.0001723339234021455915, 0.0002782939632049884118, 0.0003842540030078312862, 0.0005961740826135169266 ),
 ( 0.000000000000000000, 1.000000000000000000 ),
 .UNSPECIFIED. ) 
 GEOMETRIC_REPRESENTATION_ITEM ( )  RATIONAL_B_SPLINE_SURFACE ( (
 ( 1.000000000000000000, 0.9504532311154330060, 1.000000000000000000),
 ( 1.000000000000000000, 0.9506023220711246058, 1.000000000000000000),
 ( 1.000000000000000000, 0.9395774818179986054, 1.000000000000000000),
 ( 1.000000000000000000, 0.9079328464648975805, 1.000000000000000000),
 ( 1.000000000000000000, 0.8875702416209027001, 1.000000000000000000),
 ( 1.000000000000000000, 0.8205919608032546941, 1.000000000000000000),
 ( 1.000000000000000000, 0.7666842783603454725, 1.000000000000000000),
 ( 1.000000000000000000, 0.7071067811865618946, 1.000000000000000000) ) ) 
 REPRESENTATION_ITEM ( '' )  SURFACE ( )  );
#200894 = ORIENTED_EDGE ( 'NONE', *, *, #240487, .T. ) ;
#200893 = EDGE_CURVE ( 'NONE', #159889, #38095, #19701, .T. ) ;
#200892 = DIRECTION ( 'NONE',  ( 0.000000000000000000, 0.000000000000000000, 1.000000000000000000 ) ) ;
#200895 = LINE ( 'NONE', #97909, #117387 ) ;
#200897 = ORIENTED_EDGE ( 'NONE', *, *, #256894, .F. ) ;
#200896 = CARTESIAN_POINT ( 'NONE',  ( 21.05000000000000071, 36.02918351690956200, -236.0543695120161090 ) ) ;
#200898 = B_SPLINE_CURVE_WITH_KNOTS ( 'NONE', 3,
 ( #197975, #199275, #175875, #255335, #20651, #100134, #217527, #179717, #2331, #76745, #1030, #237115, #156327, #98843, #55875, #136711 ),
 .UNSPECIFIED., .F., .F.,
 ( 4, 3, 3, 3, 3, 4 ),
 ( 0.000000000000000000, 3.357088238233614221E-05, 6.714213034887457252E-05, 0.0001007408646120896615, 0.0001343627955914202031, 0.0001573956632895978950 ),
 .UNSPECIFIED. ) ;
#200899 = EDGE_LOOP ( 'NONE', ( #11786, #88122, #102516, #150790 ) ) ;
#200900 = DIRECTION ( 'NONE',  ( 0.000000000000000000, 0.000000000000000000, -1.000000000000000000 ) ) ;
#200901 = DIRECTION ( 'NONE',  ( 3.265361837132813093E-16, -1.000000000000000000, -0.000000000000000000 ) ) ;
#200902 = TOROIDAL_SURFACE ( 'NONE', #84311, 0.4000000000000012990, 0.1000000000000000056 ) ;
#200903 = AXIS2_PLACEMENT_3D ( 'NONE', #137981, #100128, #136705 ) ;
#200904 = ORIENTED_EDGE ( 'NONE', *, *, #203497, .F. ) ;
#200905 = VERTEX_POINT ( 'NONE', #29573 ) ;
#200906 = CARTESIAN_POINT ( 'NONE',  ( -16.88705144915419964, 9.950000000011137047, -180.4309785947120020 ) ) ;
#200907 = DIRECTION ( 'NONE',  ( 0.000000000000000000, 1.000000000000000000, 0.000000000000000000 ) ) ;
#200909 = VERTEX_POINT ( 'NONE', #109063 ) ;
#200908 = VERTEX_POINT ( 'NONE', #9976 ) ;
#200910 = VERTEX_POINT ( 'NONE', #244716 ) ;
#200911 = CARTESIAN_POINT ( 'NONE',  ( 21.07928932188134397, 0.09889514566555242248, -94.17148334360672379 ) ) ;
#200913 = ORIENTED_EDGE ( 'NONE', *, *, #11855, .F. ) ;
#200912 = EDGE_CURVE ( 'NONE', #215032, #167562, #102869, .T. ) ;
#200914 = EDGE_LOOP ( 'NONE', ( #111840, #184166, #198975, #90294, #71426 ) ) ;
#200916 = DIRECTION ( 'NONE',  ( 1.000000000000000000, 0.000000000000000000, 0.000000000000000000 ) ) ;
#200915 = VECTOR ( 'NONE', #181275, 1000.000000000000000 ) ;
#200918 = ORIENTED_EDGE ( 'NONE', *, *, #207808, .F. ) ;
#200917 = DIRECTION ( 'NONE',  ( -4.448008912761043807E-16, 1.000000000000000000, 0.000000000000000000 ) ) ;
#200919 = CYLINDRICAL_SURFACE ( 'NONE', #152518, 0.09999999999999939493 ) ;
#200921 = DIRECTION ( 'NONE',  ( -0.000000000000000000, 1.000000000000000000, -0.000000000000000000 ) ) ;
#200920 = DIRECTION ( 'NONE',  ( -0.000000000000000000, 0.9770955615653313941, 0.2128009952263603954 ) ) ;
#200922 = ORIENTED_EDGE ( 'NONE', *, *, #147259, .F. ) ;
#200923 = VECTOR ( 'NONE', #247199, 1000.000000000000227 ) ;
#200924 = AXIS2_PLACEMENT_3D ( 'NONE', #90805, #11291, #230323 ) ;
#200925 = AXIS2_PLACEMENT_3D ( 'NONE', #242751, #221892, #223190 ) ;
#200928 = EDGE_CURVE ( 'NONE', #194221, #79198, #165250, .T. ) ;
#200927 = ORIENTED_EDGE ( 'NONE', *, *, #185420, .T. ) ;
#200926 = VERTEX_POINT ( 'NONE', #149511 ) ;
#200929 = CIRCLE ( 'NONE', #21865, 0.09999999999999939493 ) ;
#200930 = CARTESIAN_POINT ( 'NONE',  ( -20.64999999999999858, -3.363022478626109368, -226.2703567425896267 ) ) ;
#200931 = LINE ( 'NONE', #24887, #253515 ) ;
#200932 = ORIENTED_EDGE ( 'NONE', *, *, #49871, .F. ) ;
#200933 = LINE ( 'NONE', #39318, #5098 ) ;
#200934 = ORIENTED_EDGE ( 'NONE', *, *, #85190, .F. ) ;
#200935 = EDGE_LOOP ( 'NONE', ( #127609, #202913, #108410, #169904 ) ) ;
#200936 = DIRECTION ( 'NONE',  ( 1.000000000000000000, 0.000000000000000000, 0.000000000000000000 ) ) ;
#200937 = ORIENTED_EDGE ( 'NONE', *, *, #83027, .T. ) ;
#200938 = DIRECTION ( 'NONE',  ( 0.000000000000000000, -7.272083257015735086E-15, 1.000000000000000000 ) ) ;
#200939 = DIRECTION ( 'NONE',  ( 0.000000000000000000, 1.000000000000000000, 0.000000000000000000 ) ) ;
#200940 = VERTEX_POINT ( 'NONE', #67382 ) ;
#200941 = DIRECTION ( 'NONE',  ( -4.391705002472929091E-16, 1.000000000000000000, 0.000000000000000000 ) ) ;
#200942 = CYLINDRICAL_SURFACE ( 'NONE', #207871, 0.09999999999999939493 ) ;
#200944 = CARTESIAN_POINT ( 'NONE',  ( -16.83558968593875349, 9.950000000011137047, -121.3376948123833188 ) ) ;
#200943 = FACE_OUTER_BOUND ( 'NONE', #152596, .T. ) ;
#200945 = CARTESIAN_POINT ( 'NONE',  ( -20.54999999999999716, 2.000000000011154189, -113.7246219227621395 ) ) ;
#200946 = DIRECTION ( 'NONE',  ( 0.000000000000000000, 0.9908441862701600211, -0.1350103645451876666 ) ) ;
#200947 = DIRECTION ( 'NONE',  ( -0.000000000000000000, 1.000000000000000000, 6.982962677686266711E-15 ) ) ;
#200948 = CARTESIAN_POINT ( 'NONE',  ( 17.74533788810831325, 65.18150020854128002, -126.2094848095768072 ) ) ;
#200949 = CARTESIAN_POINT ( 'NONE',  ( -22.39999999999999858, -0.09999999998884338825, -122.3504291924552234 ) ) ;
#200950 = TOROIDAL_SURFACE ( 'NONE', #5286, 12.77499999999999858, 0.1000000000000000056 ) ;
#200951 = VERTEX_POINT ( 'NONE', #209454 ) ;
#200952 = EDGE_CURVE ( 'NONE', #39176, #101974, #148705, .T. ) ;
#200954 = ORIENTED_EDGE ( 'NONE', *, *, #45292, .F. ) ;
#200953 = ORIENTED_EDGE ( 'NONE', *, *, #111945, .F. ) ;
#200955 = ORIENTED_EDGE ( 'NONE', *, *, #116473, .F. ) ;
#200957 = ORIENTED_EDGE ( 'NONE', *, *, #3430, .F. ) ;
#200956 = EDGE_CURVE ( 'NONE', #112369, #24275, #227784, .T. ) ;
#200958 = CYLINDRICAL_SURFACE ( 'NONE', #157178, 0.09999999999999939493 ) ;
#200959 = AXIS2_PLACEMENT_3D ( 'NONE', #176561, #111433, #112721 ) ;
#200960 = CARTESIAN_POINT ( 'NONE',  ( -20.64999999999999858, 27.82649702422227733, -239.8850763025288870 ) ) ;
#200961 = EDGE_CURVE ( 'NONE', #194022, #194138, #182005, .T. ) ;
#200962 = EDGE_CURVE ( 'NONE', #196929, #235213, #82010, .T. ) ;
#200963 = CARTESIAN_POINT ( 'NONE',  ( -13.43673303185029333, 9.446648990628858655, -15.08916329592318029 ) ) ;
#200964 = DIRECTION ( 'NONE',  ( 0.000000000000000000, -0.4088369013363281623, 0.9126074666063771490 ) ) ;
#200965 = ORIENTED_EDGE ( 'NONE', *, *, #72575, .T. ) ;
#200966 = AXIS2_PLACEMENT_3D ( 'NONE', #15024, #230199, #114093 ) ;
#200967 = CARTESIAN_POINT ( 'NONE',  ( -20.90851465518106167, 10.32532329027886320, -106.0699343018359997 ) ) ;
#200968 = FILL_AREA_STYLE_COLOUR ( '', #31327 ) ;
#200969 = FACE_OUTER_BOUND ( 'NONE', #222012, .T. ) ;
#200970 = DIRECTION ( 'NONE',  ( 0.000000000000000000, -1.000000000000000000, 0.000000000000000000 ) ) ;
#200971 = EDGE_CURVE ( 'NONE', #142813, #100304, #69597, .T. ) ;
#200972 = AXIS2_PLACEMENT_3D ( 'NONE', #181036, #100164, #16830 ) ;
#200973 = AXIS2_PLACEMENT_3D ( 'NONE', #91249, #229475, #166964 ) ;
#200974 = CARTESIAN_POINT ( 'NONE',  ( -17.11825945287482753, 60.84284427644114146, -221.0155524357444108 ) ) ;
#200975 = VERTEX_POINT ( 'NONE', #46515 ) ;
#200976 = EDGE_CURVE ( 'NONE', #131784, #43988, #90415, .T. ) ;
#200979 = EDGE_CURVE ( 'NONE', #227104, #46226, #194496, .T. ) ;
#200978 = ADVANCED_FACE ( 'NONE', ( #153383 ), #193750, .F. ) ;
#200977 = AXIS2_PLACEMENT_3D ( 'NONE', #137844, #79155, #38772 ) ;
#200980 = DIRECTION ( 'NONE',  ( 0.000000000000000000, 1.000000000000000000, 6.982962677686266711E-15 ) ) ;
#200981 = CIRCLE ( 'NONE', #230010, 0.09999999999998898659 ) ;
#200982 = CARTESIAN_POINT ( 'NONE',  ( -21.05000000000000071, -0.09999999998884338825, -60.45934304829880546 ) ) ;
#200983 = VERTEX_POINT ( 'NONE', #52943 ) ;
#200984 = DIRECTION ( 'NONE',  ( 0.000000000000000000, 1.000000000000000000, 0.000000000000000000 ) ) ;
#200985 = CYLINDRICAL_SURFACE ( 'NONE', #182125, 0.5000000000000004441 ) ;
#200986 = DIRECTION ( 'NONE',  ( 1.000000000000000000, -0.000000000000000000, -0.000000000000000000 ) ) ;
#200987 = CARTESIAN_POINT ( 'NONE',  ( 20.94999999999999574, 1.849084418638171856, -78.65601052144717187 ) ) ;
#200989 = TOROIDAL_SURFACE ( 'NONE', #80135, 2.100000000000002309, 0.1000000000000000056 ) ;
#200988 = CARTESIAN_POINT ( 'NONE',  ( 20.99999999999999645, 11.49509093111729108, -207.9633242410238552 ) ) ;
#200990 = ORIENTED_EDGE ( 'NONE', *, *, #92586, .F. ) ;
#200991 = DIRECTION ( 'NONE',  ( 1.000000000000000000, 0.000000000000000000, 0.000000000000000000 ) ) ;
#200992 = DIRECTION ( 'NONE',  ( 0.000000000000000000, 0.4999999999999943379, 0.8660254037844420383 ) ) ;
#200993 = DIRECTION ( 'NONE',  ( 0.000000000000000000, 0.2128009952263596183, -0.9770955615653316162 ) ) ;
#200994 = AXIS2_PLACEMENT_3D ( 'NONE', #108042, #25940, #125041 ) ;
#200995 = EDGE_CURVE ( 'NONE', #113738, #2960, #7032, .T. ) ;
#200997 = DIRECTION ( 'NONE',  ( 0.000000000000000000, 1.000000000000000000, 0.000000000000000000 ) ) ;
#200996 = CARTESIAN_POINT ( 'NONE',  ( -20.85000000000000142, 28.55432187084631224, -258.5393726171218418 ) ) ;
#200998 = CARTESIAN_POINT ( 'NONE',  ( -23.25000000000000000, 62.82351852614503684, -207.2177435922979214 ) ) ;
#200999 = DIRECTION ( 'NONE',  ( -1.000000000000000000, 1.646408749285562691E-14, 1.149681084847720908E-28 ) ) ;
#201000 = AXIS2_PLACEMENT_3D ( 'NONE', #208660, #87395, #165687 ) ;
#201001 = DIRECTION ( 'NONE',  ( 1.000000000000000000, 0.000000000000000000, 0.000000000000000000 ) ) ;
#201002 = DIRECTION ( 'NONE',  ( 0.000000000000000000, -0.8814952561688430555, 0.4721928772777346239 ) ) ;
#201003 = EDGE_CURVE ( 'NONE', #118763, #220609, #136169, .T. ) ;
#201004 = EDGE_CURVE ( 'NONE', #256904, #12568, #132491, .T. ) ;
#201006 = ORIENTED_EDGE ( 'NONE', *, *, #180367, .F. ) ;
#201005 = CARTESIAN_POINT ( 'NONE',  ( -17.27223548802547626, 10.34539739140569381, -145.3663938207882609 ) ) ;
#201007 = AXIS2_PLACEMENT_3D ( 'NONE', #15853, #36702, #116225 ) ;
#201009 =( BOUNDED_CURVE ( )  B_SPLINE_CURVE ( 3, ( #152605, #190438, #73077, #70504 ),
 .UNSPECIFIED., .F., .F. ) 
 B_SPLINE_CURVE_WITH_KNOTS ( ( 4, 4 ),
 ( 1.570796326794908992, 2.617993877991549034 ),
 .UNSPECIFIED. ) 
 CURVE ( )  GEOMETRIC_REPRESENTATION_ITEM ( )  RATIONAL_B_SPLINE_CURVE ( ( 1.000000000000000000, 0.9106836025229521070, 0.9106836025229521070, 1.000000000000000000 ) ) 
 REPRESENTATION_ITEM ( '' )  );
#201008 = TOROIDAL_SURFACE ( 'NONE', #251043, 0.2000000000000000111, 0.1000000000000000056 ) ;
#201010 = ORIENTED_EDGE ( 'NONE', *, *, #96499, .F. ) ;
#201011 = EDGE_CURVE ( 'NONE', #205515, #177471, #236163, .T. ) ;
#201012 = AXIS2_PLACEMENT_3D ( 'NONE', #84137, #120784, #123332 ) ;
#201013 = EDGE_CURVE ( 'NONE', #228476, #80209, #94637, .T. ) ;
#201014 = DIRECTION ( 'NONE',  ( 1.000000000000000000, 0.000000000000000000, 0.000000000000000000 ) ) ;
#201015 = CARTESIAN_POINT ( 'NONE',  ( 21.40925344232283578, 65.39288699657993220, -242.2555949059684508 ) ) ;
#201016 = CARTESIAN_POINT ( 'NONE',  ( 13.54556439290363912, 9.450592112144859058, -149.0561883188084096 ) ) ;
#201017 = ORIENTED_EDGE ( 'NONE', *, *, #57498, .T. ) ;
#201018 = AXIS2_PLACEMENT_3D ( 'NONE', #59000, #85936, #222902 ) ;
#201020 = DIRECTION ( 'NONE',  ( -0.000000000000000000, -0.000000000000000000, 1.000000000000000000 ) ) ;
#201019 = VECTOR ( 'NONE', #131090, 1000.000000000000000 ) ;
#201021 = CARTESIAN_POINT ( 'NONE',  ( 20.97224591636398472, 65.37484658384794045, -57.27318157986082525 ) ) ;
#201022 = DIRECTION ( 'NONE',  ( 0.000000000000000000, -0.8700118002898322711, 0.4930308989875231140 ) ) ;
#201023 = ORIENTED_EDGE ( 'NONE', *, *, #131174, .T. ) ;
#201024 = CARTESIAN_POINT ( 'NONE',  ( 20.95000000000005613, 67.85000000001119247, -3.123107484524795474 ) ) ;
#201026 = ORIENTED_EDGE ( 'NONE', *, *, #117955, .T. ) ;
#201025 = CARTESIAN_POINT ( 'NONE',  ( -21.64999999999999858, 65.95000000001181206, -82.27310748452437394 ) ) ;
#201027 = CARTESIAN_POINT ( 'NONE',  ( -18.50000000000000000, 77.83585931145570669, -125.0186683157258045 ) ) ;
#201028 = CARTESIAN_POINT ( 'NONE',  ( 20.97438252431638972, 67.07457649393631982, -161.5507367955136147 ) ) ;
#201029 = VERTEX_POINT ( 'NONE', #115486 ) ;
#201030 = CARTESIAN_POINT ( 'NONE',  ( -23.25000000000000000, 4.350000000011156054, -88.35000000000003695 ) ) ;
#201031 = VERTEX_POINT ( 'NONE', #12567 ) ;
#201032 = FACE_OUTER_BOUND ( 'NONE', #123027, .T. ) ;
#201033 = DIRECTION ( 'NONE',  ( 1.000000000000000000, 7.304098846218134667E-16, -4.607487905232622991E-31 ) ) ;
#201034 = AXIS2_PLACEMENT_3D ( 'NONE', #196457, #62098, #256375 ) ;
#201035 = CARTESIAN_POINT ( 'NONE',  ( 18.49999999999999289, 55.07829832934649517, -229.8847827466787521 ) ) ;
#201036 = VECTOR ( 'NONE', #207500, 1000.000000000000114 ) ;
#201037 = LINE ( 'NONE', #44543, #103388 ) ;
#201038 = CARTESIAN_POINT ( 'NONE',  ( -22.44366136229477249, 0.009341569497225218552, -122.3502814425261107 ) ) ;
#201039 = VERTEX_POINT ( 'NONE', #72536 ) ;
#201040 = ORIENTED_EDGE ( 'NONE', *, *, #202191, .F. ) ;
#201041 = CARTESIAN_POINT ( 'NONE',  ( -21.17356465864818560, 69.57719687377023376, -103.1220187255382399 ) ) ;
#201042 = LINE ( 'NONE', #22433, #185853 ) ;
#201043 = ADVANCED_FACE ( 'NONE', ( #133766 ), #123752, .T. ) ;
#201044 = DIRECTION ( 'NONE',  ( 0.000000000000000000, 0.9908441862701600211, -0.1350103645451876666 ) ) ;
#201045 = SPHERICAL_SURFACE ( 'NONE', #199375, 0.1000000000000000056 ) ;
#201047 = CARTESIAN_POINT ( 'NONE',  ( -21.00000000000000000, 1.410778198689825347, -7.973296578895943121 ) ) ;
#201046 = CARTESIAN_POINT ( 'NONE',  ( -16.81453046979148880, 12.41652078041931873, -211.3055207088991665 ) ) ;
#201048 = DIRECTION ( 'NONE',  ( 1.000000000000000000, 0.000000000000000000, 0.000000000000000000 ) ) ;
#201049 = EDGE_CURVE ( 'NONE', #247434, #240428, #15120, .T. ) ;
#201050 = CARTESIAN_POINT ( 'NONE',  ( -16.81453046979148880, 66.06089771857064363, -56.81138096092137602 ) ) ;
#201051 = CARTESIAN_POINT ( 'NONE',  ( 23.50000000000004263, 83.90000000001120384, -34.86056257560453986 ) ) ;
#201052 = VERTEX_POINT ( 'NONE', #111641 ) ;
#201053 = LINE ( 'NONE', #236328, #69128 ) ;
#201054 = CIRCLE ( 'NONE', #5389, 0.1000000000000028644 ) ;
#201056 = EDGE_LOOP ( 'NONE', ( #217614, #92113, #157598, #75597 ) ) ;
#201055 = CARTESIAN_POINT ( 'NONE',  ( -21.05000000000000071, 76.10000000001198828, -109.5637644362255543 ) ) ;
#201057 = DIRECTION ( 'NONE',  ( 1.000000000000000000, 0.000000000000000000, 0.000000000000000000 ) ) ;
#201059 = DIRECTION ( 'NONE',  ( -1.000000000000000000, 0.000000000000000000, -0.000000000000000000 ) ) ;
#201058 = CARTESIAN_POINT ( 'NONE',  ( 22.39999999999999503, 76.00000000001200817, -110.8138870828976934 ) ) ;
#201060 = ADVANCED_FACE ( 'NONE', ( #135031 ), #92072, .F. ) ;
#201061 = EDGE_CURVE ( 'NONE', #19574, #157545, #86110, .T. ) ;
#201062 = VERTEX_POINT ( 'NONE', #136307 ) ;
#201064 = CARTESIAN_POINT ( 'NONE',  ( -18.59999999999999787, 9.350000000011156942, -146.1500000000000341 ) ) ;
#201063 = CARTESIAN_POINT ( 'NONE',  ( -16.89935556175704079, 66.05000000001159322, -56.38343112163853021 ) ) ;
#201065 = CARTESIAN_POINT ( 'NONE',  ( 23.24999999999999645, 76.00000000001237765, -170.0231074845243597 ) ) ;
#201066 = CARTESIAN_POINT ( 'NONE',  ( 20.73486653747088937, 7.750000000000025757, -20.85000000000000142 ) ) ;
#201067 = DIRECTION ( 'NONE',  ( 1.000000000000000000, 0.000000000000000000, 0.000000000000000000 ) ) ;
#201068 = ORIENTED_EDGE ( 'NONE', *, *, #87418, .F. ) ;
#201069 = DIRECTION ( 'NONE',  ( 0.000000000000000000, -6.789366196018718420E-15, 1.000000000000000000 ) ) ;
#201070 = VERTEX_POINT ( 'NONE', #152078 ) ;
#201072 = AXIS2_PLACEMENT_3D ( 'NONE', #18874, #20179, #119281 ) ;
#201071 = LINE ( 'NONE', #86233, #38609 ) ;
#201073 = VERTEX_POINT ( 'NONE', #16416 ) ;
#201074 = CYLINDRICAL_SURFACE ( 'NONE', #126212, 0.09999999999999939493 ) ;
#201075 = EDGE_LOOP ( 'NONE', ( #113333, #112421, #194101, #151900 ) ) ;
#201076 = CIRCLE ( 'NONE', #188586, 0.09999999999998898659 ) ;
#201077 = EDGE_CURVE ( 'NONE', #44736, #231425, #98747, .T. ) ;
#201078 = FACE_BOUND ( 'NONE', #123706, .T. ) ;
#201079 = ADVANCED_FACE ( 'NONE', ( #231603 ), #254938, .T. ) ;
#201080 = TOROIDAL_SURFACE ( 'NONE', #22030, 12.97499999999999609, 0.1000000000000000056 ) ;
#201081 = DIRECTION ( 'NONE',  ( 0.000000000000000000, 0.4999999999999413247, -0.8660254037844724584 ) ) ;
#201082 = ORIENTED_EDGE ( 'NONE', *, *, #93755, .T. ) ;
#201083 = DIRECTION ( 'NONE',  ( -3.469446951953515108E-14, -1.000000000000000000, 0.000000000000000000 ) ) ;
#201084 = CARTESIAN_POINT ( 'NONE',  ( -18.59999999999999787, 64.35000000001161879, -62.50830171387039513 ) ) ;
#201085 = CARTESIAN_POINT ( 'NONE',  ( 20.96428641294273021, 11.75000000001150013, -160.6748931779423231 ) ) ;
#201086 = CIRCLE ( 'NONE', #184496, 0.09999999999999939493 ) ;
#201087 = VECTOR ( 'NONE', #47865, 1000.000000000000000 ) ;
#201088 = CARTESIAN_POINT ( 'NONE',  ( 23.24999999999999645, 67.17743825834540417, -82.17310748452437963 ) ) ;
#201089 = ADVANCED_FACE ( 'NONE', ( #155933 ), #215853, .F. ) ;
#201090 = CARTESIAN_POINT ( 'NONE',  ( 20.94999999999999929, -11.29603075033528192, -30.45210084033612929 ) ) ;
#201091 = DIRECTION ( 'NONE',  ( 0.000000000000000000, 0.2128009952264214300, -0.9770955615653181825 ) ) ;
#201093 = ORIENTED_EDGE ( 'NONE', *, *, #250862, .T. ) ;
#201092 = EDGE_CURVE ( 'NONE', #116058, #148174, #71257, .T. ) ;
#201095 = DIRECTION ( 'NONE',  ( -1.000000000000000000, 1.589006537307804524E-14, -4.309524267446607808E-15 ) ) ;
#201094 = CARTESIAN_POINT ( 'NONE',  ( 21.05000000000005400, 83.97335046823651794, -34.66234602115918051 ) ) ;
#201096 = ORIENTED_EDGE ( 'NONE', *, *, #131343, .F. ) ;
#201098 = ORIENTED_EDGE ( 'NONE', *, *, #20511, .T. ) ;
#201097 = CARTESIAN_POINT ( 'NONE',  ( -13.39999999999993996, 67.72071067812984779, -24.99381816264344991 ) ) ;
#201099 = ORIENTED_EDGE ( 'NONE', *, *, #244732, .T. ) ;
#201100 = LINE ( 'NONE', #240245, #65607 ) ;
#201101 = DIRECTION ( 'NONE',  ( 0.000000000000000000, -1.000000000000000000, -2.891205793294679805E-16 ) ) ;
#201102 = CARTESIAN_POINT ( 'NONE',  ( 21.04116576186321197, 60.20408469978575283, -221.1753446031674173 ) ) ;
#201103 = CARTESIAN_POINT ( 'NONE',  ( -21.22070241538126112, 60.96101127587400015, -234.2570688782265051 ) ) ;
#201104 = EDGE_LOOP ( 'NONE', ( #44993, #74174, #33692, #217482 ) ) ;
#201105 = DIRECTION ( 'NONE',  ( -0.000000000000000000, -1.000000000000000000, 0.000000000000000000 ) ) ;
#201106 = CARTESIAN_POINT ( 'NONE',  ( 21.14999999999999858, 6.540656951712400691, -67.10000000000005116 ) ) ;
#201107 = ADVANCED_FACE ( 'NONE', ( #217133 ), #211230, .F. ) ;
#201108 = CONICAL_SURFACE ( 'NONE', #117882, 4.299999999999956302, 0.7853981633974466137 ) ;
#201109 = VERTEX_POINT ( 'NONE', #101012 ) ;
#201110 = AXIS2_PLACEMENT_3D ( 'NONE', #192491, #154677, #217163 ) ;
#201111 = VECTOR ( 'NONE', #55767, 1000.000000000000000 ) ;
#201112 = EDGE_CURVE ( 'NONE', #239652, #66968, #19522, .T. ) ;
#201113 = DIRECTION ( 'NONE',  ( 0.000000000000000000, 0.2617529984164955192, 0.9651348961777178603 ) ) ;
#201114 = AXIS2_PLACEMENT_3D ( 'NONE', #59790, #58513, #18126 ) ;
#201115 = CARTESIAN_POINT ( 'NONE',  ( 18.49999999999999645, 74.26374286841466699, -124.9544551555068068 ) ) ;
#201116 = ADVANCED_FACE ( 'NONE', ( #197588 ), #70708, .T. ) ;
#201117 = VERTEX_POINT ( 'NONE', #178056 ) ;
#201118 = CARTESIAN_POINT ( 'NONE',  ( -16.83558968593869665, 9.950000000011137047, -146.6623051876167381 ) ) ;
#201119 = CARTESIAN_POINT ( 'NONE',  ( -22.39999999999999503, 68.20922040163824818, -69.62310748452438247 ) ) ;
#201120 = EDGE_LOOP ( 'NONE', ( #219832, #160530, #17637, #195368 ) ) ;
#201121 = CARTESIAN_POINT ( 'NONE',  ( 23.14999999999999503, 6.450000000011156587, -122.2500000000000284 ) ) ;
#201122 = DIRECTION ( 'NONE',  ( 0.000000000000000000, 0.4088369013363281623, -0.9126074666063771490 ) ) ;
#201123 = DIRECTION ( 'NONE',  ( 0.000000000000000000, -1.000000000000000000, 0.000000000000000000 ) ) ;
#201124 = EDGE_CURVE ( 'NONE', #47017, #32552, #231907, .T. ) ;
#201125 = FACE_OUTER_BOUND ( 'NONE', #54641, .T. ) ;
#201126 = ADVANCED_FACE ( 'NONE', ( #78905 ), #152815, .T. ) ;
#201127 = AXIS2_PLACEMENT_3D ( 'NONE', #207715, #29108, #108596 ) ;
#201128 = FACE_OUTER_BOUND ( 'NONE', #183319, .T. ) ;
#201129 = CARTESIAN_POINT ( 'NONE',  ( 21.05000000000000071, 8.876614585087098774, -8.385080478844676222 ) ) ;
#201130 = ORIENTED_EDGE ( 'NONE', *, *, #33269, .F. ) ;
#201132 = DIRECTION ( 'NONE',  ( 0.000000000000000000, 0.2128009952263618110, -0.9770955615653311721 ) ) ;
#201131 = CARTESIAN_POINT ( 'NONE',  ( 20.90000000000000213, 1.901609089591594470, -11.59510167572422112 ) ) ;
#201133 = ORIENTED_EDGE ( 'NONE', *, *, #6521, .F. ) ;
#201134 = CIRCLE ( 'NONE', #180866, 0.1000000000000001027 ) ;
#201135 = CARTESIAN_POINT ( 'NONE',  ( -21.05000000000000071, -1.261786168553869603, -142.0864989635454947 ) ) ;
#201137 = EDGE_CURVE ( 'NONE', #71369, #221901, #219398, .T. ) ;
#201136 = CARTESIAN_POINT ( 'NONE',  ( 23.14999999999999858, 53.62064951147646497, -235.8162552129080609 ) ) ;
#201138 = VECTOR ( 'NONE', #70750, 1000.000000000000114 ) ;
#201140 = ORIENTED_EDGE ( 'NONE', *, *, #121476, .T. ) ;
#201139 = DIRECTION ( 'NONE',  ( 1.000000000000000000, 0.000000000000000000, 0.000000000000000000 ) ) ;
#201141 = CARTESIAN_POINT ( 'NONE',  ( 21.05000000000000071, 67.22371710471909978, -57.37310748452438247 ) ) ;
#201142 = CARTESIAN_POINT ( 'NONE',  ( -18.59999999999999787, 6.933893972137497030, -104.2856458343736250 ) ) ;
#201143 = CARTESIAN_POINT ( 'NONE',  ( -21.64999999999999858, 41.27791846035906786, -237.2365415511148115 ) ) ;
#201144 = CARTESIAN_POINT ( 'NONE',  ( -16.87372386987899020, 9.880600233647912845, -80.14926987186645135 ) ) ;
#201145 = AXIS2_PLACEMENT_3D ( 'NONE', #66659, #169652, #185316 ) ;
#201146 = CARTESIAN_POINT ( 'NONE',  ( -21.14999999999999858, 87.65000000001192859, -100.1231074845242262 ) ) ;
#201148 = EDGE_LOOP ( 'NONE', ( #71661, #58604, #242511, #39919, #197317, #94974, #185800, #239454, #42504, #15210, #105845, #106964, #100763, #62185, #10973, #85988, #222977, #162384 ) ) ;
#201147 = CARTESIAN_POINT ( 'NONE',  ( -20.94999999999999929, 0.000000000000000000, -33.50000000000000000 ) ) ;
#201149 = VECTOR ( 'NONE', #87945, 1000.000000000000000 ) ;
#201150 = AXIS2_PLACEMENT_3D ( 'NONE', #65572, #8184, #185528 ) ;
#201151 = CIRCLE ( 'NONE', #97053, 11.75000000000000178 ) ;
#201152 = CIRCLE ( 'NONE', #117945, 0.09999999999999939493 ) ;
#201153 = CARTESIAN_POINT ( 'NONE',  ( 21.14999999999999503, 11.75000000001115552, -67.00000000000004263 ) ) ;
#201154 = ORIENTED_EDGE ( 'NONE', *, *, #169577, .F. ) ;
#201155 = ORIENTED_EDGE ( 'NONE', *, *, #132063, .F. ) ;
#201156 = DIRECTION ( 'NONE',  ( 1.000000000000000000, -0.000000000000000000, 0.000000000000000000 ) ) ;
#201157 = DIRECTION ( 'NONE',  ( 0.000000000000000000, 0.000000000000000000, -1.000000000000000000 ) ) ;
#201158 = VECTOR ( 'NONE', #241727, 1000.000000000000000 ) ;
#201159 = ORIENTED_EDGE ( 'NONE', *, *, #167462, .T. ) ;
#201160 = CARTESIAN_POINT ( 'NONE',  ( 23.14999999999999503, 64.25000000001222134, -148.6731074845244507 ) ) ;
#201161 = VECTOR ( 'NONE', #3241, 1000.000000000000000 ) ;
#201162 = DIRECTION ( 'NONE',  ( 0.000000000000000000, 0.000000000000000000, -1.000000000000000000 ) ) ;
#201163 = CIRCLE ( 'NONE', #5330, 0.9000000000000014655 ) ;
#201164 = ORIENTED_EDGE ( 'NONE', *, *, #164388, .T. ) ;
#201165 = LINE ( 'NONE', #42118, #172883 ) ;
#201166 = AXIS2_PLACEMENT_3D ( 'NONE', #186137, #149603, #223963 ) ;
#201167 = AXIS2_PLACEMENT_3D ( 'NONE', #213566, #146216, #127954 ) ;
#201169 = VECTOR ( 'NONE', #192216, 999.9999999999998863 ) ;
#201168 = LINE ( 'NONE', #62944, #126322 ) ;
#201170 = ORIENTED_EDGE ( 'NONE', *, *, #3562, .T. ) ;
#201171 = CIRCLE ( 'NONE', #180335, 0.09999999999999939493 ) ;
#201172 = VERTEX_POINT ( 'NONE', #22843 ) ;
#201173 = SPHERICAL_SURFACE ( 'NONE', #211109, 0.1000000000000000056 ) ;
#201174 = EDGE_LOOP ( 'NONE', ( #8054, #26443, #128654, #8354 ) ) ;
#201175 = DIRECTION ( 'NONE',  ( 1.000000000000000000, 0.000000000000000000, 0.000000000000000000 ) ) ;
#201177 = EDGE_CURVE ( 'NONE', #246161, #246982, #252715, .T. ) ;
#201176 = ORIENTED_EDGE ( 'NONE', *, *, #125693, .T. ) ;
#201179 = ORIENTED_EDGE ( 'NONE', *, *, #130895, .T. ) ;
#201178 = FACE_OUTER_BOUND ( 'NONE', #226007, .T. ) ;
#201180 = CARTESIAN_POINT ( 'NONE',  ( -15.75000000000000355, 66.65000000001185754, -86.27310748452437394 ) ) ;
#201181 = ORIENTED_EDGE ( 'NONE', *, *, #43194, .F. ) ;
#201182 = EDGE_CURVE ( 'NONE', #109070, #33939, #61202, .T. ) ;
#201183 = DIRECTION ( 'NONE',  ( 0.000000000000000000, 0.2128009952263578142, -0.9770955615653320603 ) ) ;
#201184 = EDGE_CURVE ( 'NONE', #241341, #226700, #94501, .T. ) ;
#201185 = VERTEX_POINT ( 'NONE', #161051 ) ;
#201187 = EDGE_LOOP ( 'NONE', ( #133967, #219092, #235759, #105938 ) ) ;
#201186 = ORIENTED_EDGE ( 'NONE', *, *, #105413, .F. ) ;
#201188 = CARTESIAN_POINT ( 'NONE',  ( -21.44999999999999929, 29.14863708059993286, -237.4168895852561434 ) ) ;
#201189 = CARTESIAN_POINT ( 'NONE',  ( -20.96077737575334865, 56.21923056145944742, -228.0513653586724558 ) ) ;
#201191 = EDGE_LOOP ( 'NONE', ( #70688, #241045, #107171, #158251 ) ) ;
#201190 = AXIS2_PLACEMENT_3D ( 'NONE', #160991, #140110, #240519 ) ;
#201192 = VECTOR ( 'NONE', #230295, 1000.000000000000000 ) ;
#201193 = TOROIDAL_SURFACE ( 'NONE', #159517, 0.2000000000000000111, 0.1000000000000000056 ) ;
#201194 = AXIS2_PLACEMENT_3D ( 'NONE', #40241, #100152, #16817 ) ;
#201195 = ORIENTED_EDGE ( 'NONE', *, *, #165116, .F. ) ;
#201196 = EDGE_CURVE ( 'NONE', #147363, #129128, #15425, .T. ) ;
#201197 = LINE ( 'NONE', #139920, #82844 ) ;
#201198 = DIRECTION ( 'NONE',  ( 0.000000000000000000, 0.8814952561688437216, -0.4721928772777331806 ) ) ;
#201200 = VERTEX_POINT ( 'NONE', #42379 ) ;
#201199 = DIRECTION ( 'NONE',  ( -1.000000000000000000, -3.265361837132813093E-16, 0.000000000000000000 ) ) ;
#201201 = DIRECTION ( 'NONE',  ( 0.000000000000000000, 0.000000000000000000, -1.000000000000000000 ) ) ;
#201202 = ORIENTED_EDGE ( 'NONE', *, *, #9110, .F. ) ;
#201203 = CARTESIAN_POINT ( 'NONE',  ( 18.59999999999999432, 77.16270174994990327, -94.92310748452430857 ) ) ;
#201204 = CARTESIAN_POINT ( 'NONE',  ( -15.55912972643740488, 67.50912972644997012, -182.5731074845244279 ) ) ;
#201205 = ORIENTED_EDGE ( 'NONE', *, *, #4350, .F. ) ;
#201206 = FACE_OUTER_BOUND ( 'NONE', #156365, .T. ) ;
#201207 = CARTESIAN_POINT ( 'NONE',  ( -21.05000000000000071, 76.00000000001267608, -203.5231074845243597 ) ) ;
#201208 = DIRECTION ( 'NONE',  ( 0.000000000000000000, 6.608470384673558123E-15, -1.000000000000000000 ) ) ;
#201209 = ORIENTED_EDGE ( 'NONE', *, *, #241818, .F. ) ;
#201210 = VERTEX_POINT ( 'NONE', #121926 ) ;
#201211 = EDGE_LOOP ( 'NONE', ( #182798, #118550, #94065 ) ) ;
#201212 = VERTEX_POINT ( 'NONE', #201443 ) ;
#201213 = AXIS2_PLACEMENT_3D ( 'NONE', #153037, #209110, #190872 ) ;
#201214 = EDGE_LOOP ( 'NONE', ( #192917, #132644, #183252 ) ) ;
#201215 = CYLINDRICAL_SURFACE ( 'NONE', #24225, 4.000000000000003553 ) ;
#201216 = EDGE_CURVE ( 'NONE', #233728, #55518, #61378, .T. ) ;
#201217 = VERTEX_POINT ( 'NONE', #3229 ) ;
#201218 = EDGE_CURVE ( 'NONE', #125758, #105820, #82746, .T. ) ;
#201219 = CARTESIAN_POINT ( 'NONE',  ( -20.85000000000000142, 77.83585931145570669, -125.0186683157258329 ) ) ;
#201220 = EDGE_LOOP ( 'NONE', ( #90192, #81821, #121645, #88609 ) ) ;
#201221 = FACE_OUTER_BOUND ( 'NONE', #126542, .T. ) ;
#201222 = CARTESIAN_POINT ( 'NONE',  ( 21.72449340488910252, 10.28395627750227703, -146.6500000000000341 ) ) ;
#201223 = ORIENTED_EDGE ( 'NONE', *, *, #219553, .T. ) ;
#201225 = EDGE_CURVE ( 'NONE', #167394, #229799, #182191, .T. ) ;
#201224 = EDGE_LOOP ( 'NONE', ( #51758, #33950, #153424, #106923 ) ) ;
#201226 = AXIS2_PLACEMENT_3D ( 'NONE', #226129, #139220, #178406 ) ;
#201227 = ORIENTED_EDGE ( 'NONE', *, *, #237094, .F. ) ;
#201228 = TOROIDAL_SURFACE ( 'NONE', #234550, 11.65000000000000036, 0.1000000000000000056 ) ;
#201229 = CARTESIAN_POINT ( 'NONE',  ( 21.08489834409762764, 13.00711782211248035, -210.8066890889169258 ) ) ;
#201230 = DIRECTION ( 'NONE',  ( 0.000000000000000000, -6.938893903907234689E-15, 1.000000000000000000 ) ) ;
#201231 = CARTESIAN_POINT ( 'NONE',  ( -20.99551997958415583, 11.75000000001124434, -127.1516591376888954 ) ) ;
#201232 = CARTESIAN_POINT ( 'NONE',  ( 20.94999999999999929, 0.000000000000000000, -33.50000000000000000 ) ) ;
#201233 = LINE ( 'NONE', #22630, #40278 ) ;
#201235 = ADVANCED_FACE ( 'NONE', ( #77621 ), #26695, .T. ) ;
#201234 = LINE ( 'NONE', #240380, #131320 ) ;
#201237 = CARTESIAN_POINT ( 'NONE',  ( 21.04999999999999716, 34.01621449225257976, -243.6162460527932296 ) ) ;
#201236 = DIRECTION ( 'NONE',  ( 0.000000000000000000, 0.000000000000000000, 1.000000000000000000 ) ) ;
#201238 = CARTESIAN_POINT ( 'NONE',  ( 18.59999999999999076, 6.450000000011156587, -88.25000000000005684 ) ) ;
#201239 = CARTESIAN_POINT ( 'NONE',  ( 19.95447128016623140, 4.513204987603615770, 22.00000000000000355 ) ) ;
#201240 = TOROIDAL_SURFACE ( 'NONE', #84685, 0.6000000000000015321, 0.1000000000000000056 ) ;
#201241 = CARTESIAN_POINT ( 'NONE',  ( -23.15000000000000213, 4.250000000011156409, -112.8500000000000369 ) ) ;
#201242 = DIRECTION ( 'NONE',  ( 0.000000000000000000, 0.000000000000000000, -1.000000000000000000 ) ) ;
#201243 = AXIS2_PLACEMENT_3D ( 'NONE', #18958, #116786, #16427 ) ;
#201244 = VERTEX_POINT ( 'NONE', #86614 ) ;
#201245 = CIRCLE ( 'NONE', #134597, 0.1999999999999981515 ) ;
#201246 = EDGE_CURVE ( 'NONE', #41556, #91231, #40574, .T. ) ;
#201248 = EDGE_LOOP ( 'NONE', ( #53990, #70939, #126074, #104920 ) ) ;
#201247 = DIRECTION ( 'NONE',  ( 1.000000000000000000, -0.000000000000000000, -0.000000000000000000 ) ) ;
#201249 = ORIENTED_EDGE ( 'NONE', *, *, #59003, .T. ) ;
#201250 = CARTESIAN_POINT ( 'NONE',  ( -18.59999999999999787, 77.16412189325330928, -128.6082593989527254 ) ) ;
#201251 = CARTESIAN_POINT ( 'NONE',  ( 18.59999999999999076, -1.164121893230052995, -208.9148480855715775 ) ) ;
#201252 = ADVANCED_FACE ( 'NONE', ( #5795 ), #184451, .T. ) ;
#201253 = EDGE_CURVE ( 'NONE', #121611, #23447, #140471, .T. ) ;
#201254 = CARTESIAN_POINT ( 'NONE',  ( -22.49756042579671700, 64.10656222496838552, -247.0783888534666062 ) ) ;
#201255 = ORIENTED_EDGE ( 'NONE', *, *, #168943, .F. ) ;
#201256 = CIRCLE ( 'NONE', #234582, 0.09999999999999939493 ) ;
#201257 = AXIS2_PLACEMENT_3D ( 'NONE', #218183, #117820, #252183 ) ;
#201259 = AXIS2_PLACEMENT_3D ( 'NONE', #6754, #229658, #187970 ) ;
#201258 = CARTESIAN_POINT ( 'NONE',  ( 18.59999999999999787, 0.6713328740235187109, -212.7808875799876205 ) ) ;
#201260 = DIRECTION ( 'NONE',  ( -1.836970198721029934E-16, 1.000000000000000000, 0.000000000000000000 ) ) ;
#201261 = ORIENTED_EDGE ( 'NONE', *, *, #254307, .F. ) ;
#201262 = ADVANCED_FACE ( 'NONE', ( #224855 ), #64512, .F. ) ;
#201263 = CARTESIAN_POINT ( 'NONE',  ( -17.11825945287481332, 10.05000000001113847, -54.35000000000000142 ) ) ;
#201264 = DIRECTION ( 'NONE',  ( -0.000000000000000000, 6.982962677686266711E-15, -1.000000000000000000 ) ) ;
#201265 = EDGE_CURVE ( 'NONE', #185168, #102921, #169757, .T. ) ;
#201266 = FACE_OUTER_BOUND ( 'NONE', #137087, .T. ) ;
#201267 = TOROIDAL_SURFACE ( 'NONE', #247051, 7.800000000000000711, 0.1000000000000000056 ) ;
#201268 = CARTESIAN_POINT ( 'NONE',  ( 18.59999999999999076, 15.51794587355511545, -222.9505302427971003 ) ) ;
#201270 = ORIENTED_EDGE ( 'NONE', *, *, #78535, .T. ) ;
#201269 = CARTESIAN_POINT ( 'NONE',  ( -20.91682497891423154, 67.49276774653023381, -195.4544018784149841 ) ) ;
#201271 = EDGE_CURVE ( 'NONE', #95067, #77584, #57262, .T. ) ;
#201272 = DIRECTION ( 'NONE',  ( 4.377807931758638789E-15, 0.2605042016806672911, 0.9654727137038716656 ) ) ;
#201274 = ORIENTED_EDGE ( 'NONE', *, *, #172612, .T. ) ;
#201273 = CARTESIAN_POINT ( 'NONE',  ( 18.59999999999999076, 69.01799029515566986, -132.8269553662681233 ) ) ;
#201275 = AXIS2_PLACEMENT_3D ( 'NONE', #121833, #124398, #186958 ) ;
#201276 = DIRECTION ( 'NONE',  ( 0.000000000000000000, 7.116814260417668513E-15, -1.000000000000000000 ) ) ;
#201278 = CARTESIAN_POINT ( 'NONE',  ( -18.59999999999999787, 86.87366311306884370, -199.3414869250131858 ) ) ;
#201277 = VECTOR ( 'NONE', #160475, 1000.000000000000000 ) ;
#201279 = VECTOR ( 'NONE', #35663, 1000.000000000000000 ) ;
#201280 = CARTESIAN_POINT ( 'NONE',  ( -20.94999999999999929, 70.15623657602074559, -198.0563205710787713 ) ) ;
#201281 = CARTESIAN_POINT ( 'NONE',  ( -12.60206096961792177, 9.389686005666810331, -183.1728435063512848 ) ) ;
#201282 = CIRCLE ( 'NONE', #163699, 0.09999999999998898659 ) ;
#201283 = ADVANCED_FACE ( 'NONE', ( #27990 ), #175786, .T. ) ;
#201285 = DIRECTION ( 'NONE',  ( 0.000000000000000000, 0.2128009952263603677, -0.9770955615653313941 ) ) ;
#201284 = CARTESIAN_POINT ( 'NONE',  ( 18.60000000000000497, 76.00000000001195133, -103.0231074845243171 ) ) ;
#201286 = CARTESIAN_POINT ( 'NONE',  ( 20.85000000000000142, 1.115600667400684642E-11, -208.8999999999999488 ) ) ;
#201287 = DIRECTION ( 'NONE',  ( 0.2834754621636439431, 0.2834754621636471628, 0.9161240771326858434 ) ) ;
#201288 = DIRECTION ( 'NONE',  ( 0.000000000000000000, 0.000000000000000000, 1.000000000000000000 ) ) ;
#201289 = CARTESIAN_POINT ( 'NONE',  ( -20.00857864376270001, 13.46244553689443535, -219.8161515769436107 ) ) ;
#201290 = LINE ( 'NONE', #137453, #197527 ) ;
#201291 = ADVANCED_FACE ( 'NONE', ( #29286 ), #108771, .T. ) ;
#201292 = EDGE_CURVE ( 'NONE', #156872, #212150, #168802, .T. ) ;
#201293 = ORIENTED_EDGE ( 'NONE', *, *, #22678, .T. ) ;
#201294 = LINE ( 'NONE', #25251, #222274 ) ;
#201295 = ORIENTED_EDGE ( 'NONE', *, *, #182768, .F. ) ;
#201296 = ORIENTED_EDGE ( 'NONE', *, *, #228516, .F. ) ;
#201297 = EDGE_CURVE ( 'NONE', #110864, #192851, #203015, .T. ) ;
#201298 = ORIENTED_EDGE ( 'NONE', *, *, #74542, .F. ) ;
#201299 = EDGE_CURVE ( 'NONE', #10818, #3158, #171368, .T. ) ;
#201300 = EDGE_CURVE ( 'NONE', #111810, #13016, #12268, .T. ) ;
#201301 = ORIENTED_EDGE ( 'NONE', *, *, #27971, .F. ) ;
#201302 = AXIS2_PLACEMENT_3D ( 'NONE', #32756, #195346, #10595 ) ;
#201303 =( LENGTH_UNIT ( ) NAMED_UNIT ( * ) SI_UNIT ( .MILLI., .METRE. ) );
#201304 = EDGE_CURVE ( 'NONE', #82095, #103469, #115534, .T. ) ;
#201305 = AXIS2_PLACEMENT_3D ( 'NONE', #176300, #255769, #77167 ) ;
#201306 = VERTEX_POINT ( 'NONE', #249584 ) ;
#201307 = CIRCLE ( 'NONE', #242996, 0.09999999999999939493 ) ;
#201308 = LINE ( 'NONE', #185601, #141784 ) ;
#201309 = ORIENTED_EDGE ( 'NONE', *, *, #109815, .F. ) ;
#201310 =( BOUNDED_CURVE ( )  B_SPLINE_CURVE ( 3, ( #204185, #67253, #86797, #226303 ),
 .UNSPECIFIED., .F., .T. ) 
 B_SPLINE_CURVE_WITH_KNOTS ( ( 4, 4 ),
 ( 1.570796326794892339, 3.141592653589784678 ),
 .UNSPECIFIED. ) 
 CURVE ( )  GEOMETRIC_REPRESENTATION_ITEM ( )  RATIONAL_B_SPLINE_CURVE ( ( 1.000000000000000000, 0.8047378541243659367, 0.8047378541243659367, 1.000000000000000000 ) ) 
 REPRESENTATION_ITEM ( '' )  );
#201311 = DIRECTION ( 'NONE',  ( 0.000000000000000000, -1.000000000000000000, -6.982962677686266711E-15 ) ) ;
#201312 = FACE_OUTER_BOUND ( 'NONE', #115229, .T. ) ;
#201313 = CARTESIAN_POINT ( 'NONE',  ( -20.64999999999999858, 73.50000000001229239, -156.7984855617622770 ) ) ;
#201314 = LINE ( 'NONE', #240448, #128144 ) ;
#201315 = CARTESIAN_POINT ( 'NONE',  ( 21.05000000000000071, 6.540656951712400691, -134.1000000000000227 ) ) ;
#201316 = CONICAL_SURFACE ( 'NONE', #109729, 4.299999999999956302, 0.7853981633974466137 ) ;
#201317 = FACE_OUTER_BOUND ( 'NONE', #152967, .T. ) ;
#201318 = CARTESIAN_POINT ( 'NONE',  ( 20.94999999999999574, -1.360870587180885716, -41.57299792709095954 ) ) ;
#201320 = ORIENTED_EDGE ( 'NONE', *, *, #122142, .F. ) ;
#201319 = CARTESIAN_POINT ( 'NONE',  ( -21.76363531954647357, 75.90099812571226323, -76.53604403239606313 ) ) ;
#201322 = CARTESIAN_POINT ( 'NONE',  ( 18.59999999999999076, 69.55000000001179217, -81.87310748452435405 ) ) ;
#201321 = CARTESIAN_POINT ( 'NONE',  ( 20.95325940946048249, 65.47660992931533031, -61.95864535528431105 ) ) ;
#201323 = EDGE_CURVE ( 'NONE', #221081, #253337, #148883, .T. ) ;
#201324 = DIRECTION ( 'NONE',  ( -1.000000000000000000, 0.000000000000000000, 0.000000000000000000 ) ) ;
#201325 = ORIENTED_EDGE ( 'NONE', *, *, #71221, .F. ) ;
#201326 = B_SPLINE_CURVE_WITH_KNOTS ( 'NONE', 3,
 ( #205312, #44982, #245751, #7118, #187077, #22874, #106211, #222294, #84049, #185773, #163648, #201470, #63244, #206619, #4551, #142769, #86636, #166242, #64536, #28013, #67109, #121952, #123233, #102345, #204043, #107510 ),
 .UNSPECIFIED., .F., .F.,
 ( 4, 2, 2, 2, 2, 2, 2, 2, 2, 2, 2, 2, 4 ),
 ( 0.005476422646581360389, 0.006160811967703580874, 0.006845201288825802227, 0.007187395949386906832, 0.007529590609948009702, 0.007871785270509114307, 0.008213979931070217178, 0.008556174591631321782, 0.008898369252192424653, 0.009240563912753529258, 0.009582758573314632128, 0.01026714789443683960, 0.01095153721555904708 ),
 .UNSPECIFIED. ) ;
#201327 = VECTOR ( 'NONE', #68937, 999.9999999999998863 ) ;
#201328 = CARTESIAN_POINT ( 'NONE',  ( -16.93935632781549572, 63.06259405572221510, -213.0802528019004001 ) ) ;
#201329 = DIRECTION ( 'NONE',  ( -0.000000000000000000, 0.000000000000000000, -1.000000000000000000 ) ) ;
#201330 = VERTEX_POINT ( 'NONE', #230003 ) ;
#201331 = AXIS2_PLACEMENT_3D ( 'NONE', #48541, #186792, #167244 ) ;
#201334 = SPHERICAL_SURFACE ( 'NONE', #99910, 0.1000000000000000056 ) ;
#201333 = CARTESIAN_POINT ( 'NONE',  ( 5.899999999999995914, -11.65000000000000036, 10.00000000000000178 ) ) ;
#201332 = AXIS2_PLACEMENT_3D ( 'NONE', #104661, #134519, #176260 ) ;
#201335 = VECTOR ( 'NONE', #63800, 1000.000000000000000 ) ;
#201336 = AXIS2_PLACEMENT_3D ( 'NONE', #10760, #72027, #126852 ) ;
#201337 = CARTESIAN_POINT ( 'NONE',  ( -20.54999999999999716, 84.73084112150691283, -59.92503276553992464 ) ) ;
#201338 = VERTEX_POINT ( 'NONE', #133477 ) ;
#201339 = DIRECTION ( 'NONE',  ( -0.000000000000000000, -6.982962677686266711E-15, 1.000000000000000000 ) ) ;
#201340 = DIRECTION ( 'NONE',  ( -2.978066053179068737E-16, -0.4088369013363267745, 0.9126074666063774821 ) ) ;
#201341 = CARTESIAN_POINT ( 'NONE',  ( 21.05000000000000071, 1.162701749949165642, -108.6000000000000227 ) ) ;
#201342 = FACE_OUTER_BOUND ( 'NONE', #39878, .T. ) ;
#201343 = ORIENTED_EDGE ( 'NONE', *, *, #120056, .T. ) ;
#201344 = CIRCLE ( 'NONE', #26395, 0.09999999999999913125 ) ;
#201345 = DIRECTION ( 'NONE',  ( 2.557131231893037478E-16, -0.8660254037844385966, 0.5000000000000003331 ) ) ;
#201346 = AXIS2_PLACEMENT_3D ( 'NONE', #26755, #250898, #245781 ) ;
#201347 = EDGE_CURVE ( 'NONE', #105209, #142016, #190586, .T. ) ;
#201348 = CARTESIAN_POINT ( 'NONE',  ( -21.05000000000000071, 6.977140961446278489, -233.9419795020459389 ) ) ;
#201349 = CYLINDRICAL_SURFACE ( 'NONE', #198915, 0.1000000000000028644 ) ;
#201350 = ADVANCED_FACE ( 'NONE', ( #94334 ), #186297, .T. ) ;
#201351 = CARTESIAN_POINT ( 'NONE',  ( -23.15000000000000213, 64.35000000001258513, -191.3731074845244393 ) ) ;
#201352 = AXIS2_PLACEMENT_3D ( 'NONE', #62044, #2037, #157309 ) ;
#201353 = AXIS2_PLACEMENT_3D ( 'NONE', #188345, #111380, #70997 ) ;
#201355 = EDGE_LOOP ( 'NONE', ( #174351, #48855, #201195, #218538 ) ) ;
#201354 = CARTESIAN_POINT ( 'NONE',  ( 21.07199075132371746, 8.774944999127242795, -179.7135321616128465 ) ) ;
#201356 = VECTOR ( 'NONE', #177027, 1000.000000000000000 ) ;
#201357 = CARTESIAN_POINT ( 'NONE',  ( -21.11825140030082082, 6.445407565431136021, -33.49279637936726317 ) ) ;
#201358 = CARTESIAN_POINT ( 'NONE',  ( -21.05000000000000071, -11.48912529306490349, -103.6000000000000369 ) ) ;
#201359 = CARTESIAN_POINT ( 'NONE',  ( -21.07933241753356413, 75.90662040959243484, -75.85175343290406147 ) ) ;
#201360 = DIRECTION ( 'NONE',  ( 0.000000000000000000, 0.9651348961777159730, -0.2617529984165021806 ) ) ;
#201361 = LINE ( 'NONE', #125676, #250520 ) ;
#201363 = ORIENTED_EDGE ( 'NONE', *, *, #150699, .T. ) ;
#201362 = LINE ( 'NONE', #574, #198328 ) ;
#201364 = CARTESIAN_POINT ( 'NONE',  ( -20.64999999999999858, 85.00000000001261924, -194.1291383618718385 ) ) ;
#201365 = CARTESIAN_POINT ( 'NONE',  ( -16.92209698673656249, 63.06986081158819246, -213.1861430886383459 ) ) ;
#201366 = CARTESIAN_POINT ( 'NONE',  ( -20.54999999999999716, 76.00000000001195133, -103.0231074845243171 ) ) ;
#201367 = ORIENTED_EDGE ( 'NONE', *, *, #241183, .T. ) ;
#201368 = DIRECTION ( 'NONE',  ( 0.000000000000000000, 0.000000000000000000, 1.000000000000000000 ) ) ;
#201369 = CARTESIAN_POINT ( 'NONE',  ( 21.05000000000000071, 75.98528214348799281, -176.3678308886158561 ) ) ;
#201370 = DIRECTION ( 'NONE',  ( 1.000000000000000000, 7.304098846218134667E-16, -0.000000000000000000 ) ) ;
#201371 = EDGE_CURVE ( 'NONE', #240241, #94754, #157266, .T. ) ;
#201372 = CARTESIAN_POINT ( 'NONE',  ( 20.94999999999999929, 84.66355140188123585, -126.9990063664569391 ) ) ;
#201373 = AXIS2_PLACEMENT_3D ( 'NONE', #204367, #13568, #222635 ) ;
#201374 = CARTESIAN_POINT ( 'NONE',  ( -16.87683809663752399, 9.850000000011139178, -87.09763598180373378 ) ) ;
#201375 = AXIS2_PLACEMENT_3D ( 'NONE', #132232, #34447, #91819 ) ;
#201376 = CIRCLE ( 'NONE', #143100, 2.000000000000001776 ) ;
#201377 = ORIENTED_EDGE ( 'NONE', *, *, #168743, .F. ) ;
#201378 = VERTEX_POINT ( 'NONE', #14842 ) ;
#201379 = CARTESIAN_POINT ( 'NONE',  ( -20.54999999999999716, 76.00000000001244871, -170.0231074845243597 ) ) ;
#201380 = DIRECTION ( 'NONE',  ( 1.000000000000000000, 0.000000000000000000, 0.000000000000000000 ) ) ;
#201381 = CARTESIAN_POINT ( 'NONE',  ( 23.15000000000000213, 86.19075908668452257, -209.4719249499869136 ) ) ;
#201382 = CARTESIAN_POINT ( 'NONE',  ( 23.15000000000000213, -11.48912529306489994, -63.89999999999999858 ) ) ;
#201383 = ORIENTED_EDGE ( 'NONE', *, *, #160958, .T. ) ;
#201384 = CARTESIAN_POINT ( 'NONE',  ( 20.95576188350343116, 10.60898054497455512, -175.1112337227542639 ) ) ;
#201385 = CARTESIAN_POINT ( 'NONE',  ( 20.75572585718252938, 10.48709729568783722, -207.4124676271370333 ) ) ;
#201386 = FACE_OUTER_BOUND ( 'NONE', #138542, .T. ) ;
#201387 = CARTESIAN_POINT ( 'NONE',  ( 21.05000000000000071, 0.000000000000000000, -12.15000000000000036 ) ) ;
#201388 = DIRECTION ( 'NONE',  ( 0.000000000000000000, 1.000000000000000000, -1.224646799147353207E-16 ) ) ;
#201389 = CARTESIAN_POINT ( 'NONE',  ( -20.85000000000000142, 77.83585931145546510, -91.51866831572576189 ) ) ;
#201390 = ORIENTED_EDGE ( 'NONE', *, *, #19173, .T. ) ;
#201391 = ORIENTED_EDGE ( 'NONE', *, *, #216933, .T. ) ;
#201392 = VERTEX_POINT ( 'NONE', #113910 ) ;
#201393 = CIRCLE ( 'NONE', #234726, 4.049999999999995381 ) ;
#201394 = CARTESIAN_POINT ( 'NONE',  ( 21.07928932188134397, 0.09889514566555242248, -27.17148334360669537 ) ) ;
#201395 = ORIENTED_EDGE ( 'NONE', *, *, #158048, .F. ) ;
#201396 = CARTESIAN_POINT ( 'NONE',  ( -21.09096482362052782, 0.03944827878522684517, -27.13645563459557053 ) ) ;
#201397 = CARTESIAN_POINT ( 'NONE',  ( -18.40000000000000213, 11.75000000001113953, -180.1499999999999773 ) ) ;
#201398 = CARTESIAN_POINT ( 'NONE',  ( -21.05000000000000071, 74.16465844978765176, -124.8679561919613263 ) ) ;
#201399 = ORIENTED_EDGE ( 'NONE', *, *, #136712, .F. ) ;
#201400 = FACE_OUTER_BOUND ( 'NONE', #146645, .T. ) ;
#201401 = CARTESIAN_POINT ( 'NONE',  ( -20.85000000000000142, 76.00000000001190870, -103.0231074845243029 ) ) ;
#201402 = EDGE_CURVE ( 'NONE', #48905, #156376, #155645, .T. ) ;
#201403 = ORIENTED_EDGE ( 'NONE', *, *, #87429, .F. ) ;
#201404 = CARTESIAN_POINT ( 'NONE',  ( -15.73854595235691889, 9.351413679112544841, -150.9803435675489709 ) ) ;
#201406 = VERTEX_POINT ( 'NONE', #74825 ) ;
#201405 = LINE ( 'NONE', #41082, #25876 ) ;
#201408 = EDGE_CURVE ( 'NONE', #210749, #118204, #56484, .T. ) ;
#201407 = LINE ( 'NONE', #3193, #210858 ) ;
#201409 = DIRECTION ( 'NONE',  ( 0.000000000000000000, 0.9908441862701420355, 0.1350103645453197554 ) ) ;
#201410 = CIRCLE ( 'NONE', #88968, 0.09999999999999939493 ) ;
#201411 = CIRCLE ( 'NONE', #251479, 0.09999999999998898659 ) ;
#201412 = EDGE_LOOP ( 'NONE', ( #11596, #88425, #138955, #39301 ) ) ;
#201413 = AXIS2_PLACEMENT_3D ( 'NONE', #22986, #137746, #255088 ) ;
#201414 = DIRECTION ( 'NONE',  ( 0.000000000000000000, 0.000000000000000000, -1.000000000000000000 ) ) ;
#201416 = ADVANCED_FACE ( 'NONE', ( #55182 ), #154369, .F. ) ;
#201415 = CARTESIAN_POINT ( 'NONE',  ( -22.50000000000000000, 7.176052627820866725, -233.6445517868224044 ) ) ;
#201417 = CARTESIAN_POINT ( 'NONE',  ( 21.14999999999999858, 11.65000000001116298, -122.2500000000000284 ) ) ;
#201418 = VERTEX_POINT ( 'NONE', #134736 ) ;
#201419 = DIRECTION ( 'NONE',  ( 1.000000000000000000, 0.000000000000000000, 0.000000000000000000 ) ) ;
#201421 = EDGE_CURVE ( 'NONE', #213770, #229112, #33138, .T. ) ;
#201420 = CARTESIAN_POINT ( 'NONE',  ( 15.51872946208854920, 48.91191486804444111, -233.7874788057928868 ) ) ;
#201422 = CARTESIAN_POINT ( 'NONE',  ( 23.24999999999999645, 5.650000000011139001, -46.15000000000001279 ) ) ;
#201423 = EDGE_CURVE ( 'NONE', #140720, #107194, #210460, .T. ) ;
#201424 = EDGE_LOOP ( 'NONE', ( #187528, #63789, #232163, #243115 ) ) ;
#201425 = VECTOR ( 'NONE', #185728, 1000.000000000000000 ) ;
#201426 = EDGE_CURVE ( 'NONE', #118177, #31646, #8513, .T. ) ;
#201427 = VECTOR ( 'NONE', #171056, 1000.000000000000000 ) ;
#201428 = CIRCLE ( 'NONE', #147641, 0.1000000000000028644 ) ;
#201429 = ORIENTED_EDGE ( 'NONE', *, *, #41408, .T. ) ;
#201430 = AXIS2_PLACEMENT_3D ( 'NONE', #155048, #177177, #54621 ) ;
#201431 = ORIENTED_EDGE ( 'NONE', *, *, #236806, .T. ) ;
#201432 = CARTESIAN_POINT ( 'NONE',  ( -18.69999999999999929, -10.13229168743236031, -1.028467303599445826 ) ) ;
#201434 = EDGE_CURVE ( 'NONE', #98329, #91307, #94686, .T. ) ;
#201433 = CARTESIAN_POINT ( 'NONE',  ( -33.72168855820451938, 9.950000000000001066, -12.64999999999994529 ) ) ;
#201436 = VERTEX_POINT ( 'NONE', #198575 ) ;
#201435 = CARTESIAN_POINT ( 'NONE',  ( -16.83794237512073622, 9.926359221118632448, -146.8035421586989742 ) ) ;
#201437 = CARTESIAN_POINT ( 'NONE',  ( 20.73486653747088937, 68.25000000001203659, -123.8731074845243540 ) ) ;
#201438 = LINE ( 'NONE', #124491, #215607 ) ;
#201439 = LINE ( 'NONE', #198873, #13044 ) ;
#201440 = DIRECTION ( 'NONE',  ( -4.391705002472921695E-16, 0.4721928772777337913, 0.8814952561688434995 ) ) ;
#201441 = CARTESIAN_POINT ( 'NONE',  ( -21.05000000000000071, 64.40000000001249703, -176.9513107147999449 ) ) ;
#201442 = AXIS2_PLACEMENT_3D ( 'NONE', #236682, #215827, #100986 ) ;
#201444 = EDGE_LOOP ( 'NONE', ( #102870, #42948 ) ) ;
#201443 = CARTESIAN_POINT ( 'NONE',  ( -20.65000000000000568, 5.650000000011139001, -79.65000000000004832 ) ) ;
#201446 = ORIENTED_EDGE ( 'NONE', *, *, #209531, .T. ) ;
#201445 = DIRECTION ( 'NONE',  ( -1.000000000000000000, -0.000000000000000000, 0.000000000000000000 ) ) ;
#201447 = CARTESIAN_POINT ( 'NONE',  ( -20.85000000000000142, -11.64999999998884483, -64.10000000000000853 ) ) ;
#201448 = VERTEX_POINT ( 'NONE', #99458 ) ;
#201449 = ORIENTED_EDGE ( 'NONE', *, *, #187712, .F. ) ;
#201450 = CARTESIAN_POINT ( 'NONE',  ( 23.14999999999999858, 72.00000000001244871, -170.0231074845243882 ) ) ;
#201451 = FACE_OUTER_BOUND ( 'NONE', #104251, .T. ) ;
#201452 = TOROIDAL_SURFACE ( 'NONE', #43250, 0.2000000000000000111, 0.1000000000000000056 ) ;
#201453 = CARTESIAN_POINT ( 'NONE',  ( -20.64999999999999858, 7.150000000011155876, -79.35000000000005116 ) ) ;
#201454 = DIRECTION ( 'NONE',  ( -0.000000000000000000, 0.8660254037844411501, 0.4999999999999956701 ) ) ;
#201455 = CARTESIAN_POINT ( 'NONE',  ( 20.22483756094572271, 66.49809532114224453, -195.3835683558092171 ) ) ;
#201456 = CIRCLE ( 'NONE', #147304, 3.999999999999996447 ) ;
#201458 = ORIENTED_EDGE ( 'NONE', *, *, #160872, .F. ) ;
#201457 = CIRCLE ( 'NONE', #197369, 0.1000000000000030864 ) ;
#201459 = DIRECTION ( 'NONE',  ( -0.000000000000000000, -6.982962677686266711E-15, 1.000000000000000000 ) ) ;
#201460 = EDGE_LOOP ( 'NONE', ( #128759, #112065, #29747, #16580 ) ) ;
#201461 = ORIENTED_EDGE ( 'NONE', *, *, #199179, .F. ) ;
#201462 = CARTESIAN_POINT ( 'NONE',  ( -18.40000000000000213, 64.51332499825495859, -194.2731074845244450 ) ) ;
#201463 = ORIENTED_EDGE ( 'NONE', *, *, #195783, .T. ) ;
#201465 = EDGE_CURVE ( 'NONE', #134756, #16193, #207142, .T. ) ;
#201464 = CARTESIAN_POINT ( 'NONE',  ( -15.39946565075089779, 66.61046543766484263, -53.84829818013443514 ) ) ;
#201466 = DIRECTION ( 'NONE',  ( 0.000000000000000000, 0.9910827722268055195, 0.1332476588733540468 ) ) ;
#201467 = ORIENTED_EDGE ( 'NONE', *, *, #46683, .T. ) ;
#201468 = DIRECTION ( 'NONE',  ( -1.000000000000000000, 2.849773892568378313E-16, -7.728835255496647986E-17 ) ) ;
#201469 = VERTEX_POINT ( 'NONE', #120370 ) ;
#201471 = EDGE_CURVE ( 'NONE', #256658, #46658, #78620, .T. ) ;
#201470 = CARTESIAN_POINT ( 'NONE',  ( -14.23072895065543086, 9.455987233623892152, -48.51153116689782507 ) ) ;
#201472 = ORIENTED_EDGE ( 'NONE', *, *, #224893, .T. ) ;
#201473 = LINE ( 'NONE', #103643, #65042 ) ;
#201474 = EDGE_CURVE ( 'NONE', #84969, #211780, #211415, .T. ) ;
#201475 = DIRECTION ( 'NONE',  ( 1.000000000000000000, 0.000000000000000000, 0.000000000000000000 ) ) ;
#201476 = ADVANCED_FACE ( 'NONE', ( #158217 ), #100724, .T. ) ;
#201477 = ORIENTED_EDGE ( 'NONE', *, *, #166314, .F. ) ;
#201478 = VECTOR ( 'NONE', #56775, 1000.000000000000000 ) ;
#201479 = DIRECTION ( 'NONE',  ( -0.000000000000000000, -6.982962677686266711E-15, 1.000000000000000000 ) ) ;
#201481 = ORIENTED_EDGE ( 'NONE', *, *, #26808, .T. ) ;
#201480 = CARTESIAN_POINT ( 'NONE',  ( -21.59780538579341425, 6.847090529954407145, -100.4010213304020454 ) ) ;
#201482 = VECTOR ( 'NONE', #134065, 1000.000000000000000 ) ;
#201483 = PLANE ( 'NONE',  #106336 ) ;
#201484 = ORIENTED_EDGE ( 'NONE', *, *, #98942, .T. ) ;
#201485 = AXIS2_PLACEMENT_3D ( 'NONE', #23815, #203703, #103291 ) ;
#201486 = CARTESIAN_POINT ( 'NONE',  ( -16.97683809663753252, 66.05000000001263061, -190.2515827158545392 ) ) ;
#201487 = VERTEX_POINT ( 'NONE', #81181 ) ;
#201488 = EDGE_CURVE ( 'NONE', #32779, #3546, #69774, .T. ) ;
#201489 = CARTESIAN_POINT ( 'NONE',  ( -23.25000000000000000, 4.350000000011156054, -188.8499999999999659 ) ) ;
#201490 = CARTESIAN_POINT ( 'NONE',  ( -21.05000000000000071, 46.45388641681647357, -243.1520440498138385 ) ) ;
#201491 = LINE ( 'NONE', #703, #157283 ) ;
#201492 = DIRECTION ( 'NONE',  ( -1.000000000000000000, -3.190570557967288949E-16, -6.948722487160392945E-17 ) ) ;
#201493 = AXIS2_PLACEMENT_3D ( 'NONE', #78848, #220933, #77558 ) ;
#201494 = ADVANCED_FACE ( 'NONE', ( #219410 ), #140742, .T. ) ;
#201495 = DIRECTION ( 'NONE',  ( -0.000000000000000000, 1.000000000000000000, 0.000000000000000000 ) ) ;
#201496 = FACE_OUTER_BOUND ( 'NONE', #233306, .T. ) ;
#201497 = AXIS2_PLACEMENT_3D ( 'NONE', #19569, #161662, #144622 ) ;
#201498 = ORIENTED_EDGE ( 'NONE', *, *, #227138, .F. ) ;
#201499 = LINE ( 'NONE', #84072, #158652 ) ;
#201500 = AXIS2_PLACEMENT_3D ( 'NONE', #228008, #187617, #226708 ) ;
#201502 = CARTESIAN_POINT ( 'NONE',  ( 23.14999999999998437, 76.00000000001237765, -170.0231074845243597 ) ) ;
#201501 = PRODUCT_RELATED_PRODUCT_CATEGORY ( 'part', '', ( #147169 ) ) ;
#201504 = DIRECTION ( 'NONE',  ( 0.000000000000000000, -0.1350103645451876944, -0.9908441862701601321 ) ) ;
#201503 = AXIS2_PLACEMENT_3D ( 'NONE', #160569, #122723, #60139 ) ;
#201505 = ORIENTED_EDGE ( 'NONE', *, *, #227408, .T. ) ;
#201506 = CARTESIAN_POINT ( 'NONE',  ( 20.94999675878240808, 68.00468331834515823, -224.2298952291173464 ) ) ;
#201507 = ORIENTED_EDGE ( 'NONE', *, *, #19645, .T. ) ;
#201508 = CYLINDRICAL_SURFACE ( 'NONE', #89912, 0.09999999999998304689 ) ;
#201510 = VERTEX_POINT ( 'NONE', #98161 ) ;
#201509 = VECTOR ( 'NONE', #45322, 1000.000000000000000 ) ;
#201511 = DIRECTION ( 'NONE',  ( -0.000000000000000000, -0.07893460099012301889, 0.9968797965484754720 ) ) ;
#201512 = CARTESIAN_POINT ( 'NONE',  ( -23.25000000000000000, 36.65892442174472876, -249.5511627012454596 ) ) ;
#201513 = EDGE_CURVE ( 'NONE', #36910, #53762, #24240, .T. ) ;
#201514 = VERTEX_POINT ( 'NONE', #11829 ) ;
#201516 = VERTEX_POINT ( 'NONE', #73095 ) ;
#201515 = DIRECTION ( 'NONE',  ( -0.000000000000000000, -0.2617529984165031243, -0.9651348961777157509 ) ) ;
#201517 = EDGE_CURVE ( 'NONE', #38688, #74064, #95793, .T. ) ;
#201518 = LINE ( 'NONE', #244499, #188034 ) ;
#201519 = EDGE_LOOP ( 'NONE', ( #40744, #114626, #150596, #248348 ) ) ;
#201520 = ADVANCED_FACE ( 'NONE', ( #16947 ), #53496, .F. ) ;
#201521 = CIRCLE ( 'NONE', #172363, 0.2000000000000057288 ) ;
#201522 = DIRECTION ( 'NONE',  ( 0.7071067811865463515, 0.7071067811865487940, 7.587431340288849180E-16 ) ) ;
#201523 = DIRECTION ( 'NONE',  ( 0.000000000000000000, 0.6855225566104692358, 0.7280513885559494192 ) ) ;
#201524 = EDGE_LOOP ( 'NONE', ( #108982, #47381, #26700, #78018 ) ) ;
#201525 = EDGE_LOOP ( 'NONE', ( #89665, #21069, #162440, #128050 ) ) ;
#201526 = CIRCLE ( 'NONE', #109758, 3.900000000000000355 ) ;
#201527 = CARTESIAN_POINT ( 'NONE',  ( -23.15000000000000213, 4.349999999999999645, -12.15000000000000391 ) ) ;
#201528 = CARTESIAN_POINT ( 'NONE',  ( -23.15000000000000213, 4.350000000011156054, -112.7500000000000284 ) ) ;
#201529 = DIRECTION ( 'NONE',  ( 0.000000000000000000, -0.4721928772776568528, -0.8814952561688845778 ) ) ;
#201531 = VERTEX_POINT ( 'NONE', #136877 ) ;
#201530 = AXIS2_PLACEMENT_3D ( 'NONE', #164369, #122689, #215648 ) ;
#201532 = VERTEX_POINT ( 'NONE', #151329 ) ;
#201533 = CIRCLE ( 'NONE', #72771, 0.2000000000000057288 ) ;
#201534 = AXIS2_PLACEMENT_3D ( 'NONE', #130834, #151721, #69598 ) ;
#201535 = CARTESIAN_POINT ( 'NONE',  ( 18.49999999999999645, 1.115600667400684642E-11, -100.5000000000000426 ) ) ;
#201537 = VERTEX_POINT ( 'NONE', #176033 ) ;
#201536 = DIRECTION ( 'NONE',  ( 0.000000000000000000, 0.000000000000000000, -1.000000000000000000 ) ) ;
#201538 = CARTESIAN_POINT ( 'NONE',  ( -18.40000000000000213, 64.52683809665012404, -190.9731074845244621 ) ) ;
#201539 = CARTESIAN_POINT ( 'NONE',  ( -22.45372860728439690, 75.98507938046324739, -81.17290461922820555 ) ) ;
#201541 = EDGE_CURVE ( 'NONE', #214613, #24834, #32381, .T. ) ;
#201540 = CARTESIAN_POINT ( 'NONE',  ( -20.65000000000000568, 62.65526179112262639, -225.0299194783148948 ) ) ;
#201543 = DIRECTION ( 'NONE',  ( -0.000000000000000000, -0.1332476588733589318, 0.9910827722268049644 ) ) ;
#201542 = DIRECTION ( 'NONE',  ( -0.7071067811865475727, 0.7071067811865475727, 4.937700262164531476E-15 ) ) ;
#201544 = CARTESIAN_POINT ( 'NONE',  ( -21.04999999999999716, 75.90156250001219007, -142.8223383946111937 ) ) ;
#201545 = DIRECTION ( 'NONE',  ( -4.336808689942017736E-16, 0.000000000000000000, -1.000000000000000000 ) ) ;
#201546 = CYLINDRICAL_SURFACE ( 'NONE', #155952, 0.09999999999999939493 ) ;
#201547 = VECTOR ( 'NONE', #167489, 1000.000000000000000 ) ;
#201548 = CARTESIAN_POINT ( 'NONE',  ( 22.40000000000020819, -3.275978944803190185, -228.2735455795370854 ) ) ;
#201549 = AXIS2_PLACEMENT_3D ( 'NONE', #188609, #167802, #149516 ) ;
#201550 = AXIS2_PLACEMENT_3D ( 'NONE', #227517, #189689, #107569 ) ;
#201551 = VERTEX_POINT ( 'NONE', #54763 ) ;
#201552 = EDGE_LOOP ( 'NONE', ( #244183, #157428, #200802, #189369 ) ) ;
#201553 = EDGE_CURVE ( 'NONE', #8374, #70373, #86296, .T. ) ;
#201554 = CARTESIAN_POINT ( 'NONE',  ( 18.59999999999999076, 10.20857864377385127, -121.8500000000000369 ) ) ;
#201555 = ORIENTED_EDGE ( 'NONE', *, *, #38950, .T. ) ;
#201556 = EDGE_CURVE ( 'NONE', #203555, #58341, #235967, .T. ) ;
#201557 = EDGE_LOOP ( 'NONE', ( #80839, #1342, #57249 ) ) ;
#201559 = EDGE_CURVE ( 'NONE', #127088, #90102, #52993, .T. ) ;
#201558 = CARTESIAN_POINT ( 'NONE',  ( 17.74533788810830259, 32.67593350423081233, -235.1446872901578899 ) ) ;
#201561 = ORIENTED_EDGE ( 'NONE', *, *, #230608, .F. ) ;
#201560 = ORIENTED_EDGE ( 'NONE', *, *, #105039, .T. ) ;
#201562 = DIRECTION ( 'NONE',  ( -3.035766082959430717E-14, 0.000000000000000000, -1.000000000000000000 ) ) ;
#201563 = ORIENTED_EDGE ( 'NONE', *, *, #57873, .T. ) ;
#201564 = ORIENTED_EDGE ( 'NONE', *, *, #37975, .F. ) ;
#201565 = EDGE_CURVE ( 'NONE', #181475, #12569, #232097, .T. ) ;
#201566 = CARTESIAN_POINT ( 'NONE',  ( 18.49999999999999645, 76.00000000001244871, -170.0231074845243597 ) ) ;
#201567 = AXIS2_PLACEMENT_3D ( 'NONE', #123841, #2585, #82106 ) ;
#201568 = CARTESIAN_POINT ( 'NONE',  ( 21.97500000000000497, 66.25000000001223555, -148.8731074845244393 ) ) ;
#201571 = ADVANCED_FACE ( 'NONE', ( #71793 ), #124006, .T. ) ;
#201570 = ORIENTED_EDGE ( 'NONE', *, *, #131149, .T. ) ;
#201569 = DIRECTION ( 'NONE',  ( 0.000000000000000000, 0.000000000000000000, -1.000000000000000000 ) ) ;
#201572 = CARTESIAN_POINT ( 'NONE',  ( 20.21494484322108676, 40.46683321215910922, -237.6512114454242521 ) ) ;
#201573 = FACE_OUTER_BOUND ( 'NONE', #25474, .T. ) ;
#201575 = ORIENTED_EDGE ( 'NONE', *, *, #167268, .F. ) ;
#201574 = CARTESIAN_POINT ( 'NONE',  ( 20.95568717954149562, 10.60199405390297400, -141.6025083682686727 ) ) ;
#201576 = CARTESIAN_POINT ( 'NONE',  ( 19.86930884467607328, 11.68691006698174739, -125.2392226389383012 ) ) ;
#201577 = ORIENTED_EDGE ( 'NONE', *, *, #171213, .F. ) ;
#201578 = CARTESIAN_POINT ( 'NONE',  ( 20.94999999999999929, 84.73084112150753811, -146.1211822035086527 ) ) ;
#201580 = ORIENTED_EDGE ( 'NONE', *, *, #183646, .F. ) ;
#201579 = DIRECTION ( 'NONE',  ( -1.000000000000000000, 0.000000000000000000, -0.000000000000000000 ) ) ;
#201581 = CARTESIAN_POINT ( 'NONE',  ( 21.05000000000000071, 18.82290990851281975, -233.3604470821920529 ) ) ;
#201582 = CARTESIAN_POINT ( 'NONE',  ( -23.15000000000000213, 74.08971962617972906, -48.65447533972326966 ) ) ;
#201583 = DIRECTION ( 'NONE',  ( 0.000000000000000000, 0.1455152366551700771, 0.9893560106964479628 ) ) ;
#201584 = EDGE_LOOP ( 'NONE', ( #43319, #89982, #206814, #144211 ) ) ;
#201586 = CARTESIAN_POINT ( 'NONE',  ( 20.97107704358301916, 8.875478152032441059, -109.0589732293892951 ) ) ;
#201585 = DIRECTION ( 'NONE',  ( 3.469446951953635015E-14, -0.000000000000000000, 1.000000000000000000 ) ) ;
#201587 = CARTESIAN_POINT ( 'NONE',  ( -15.73854595235691889, 66.64858632091043944, -86.04276391697541726 ) ) ;
#201588 = AXIS2_PLACEMENT_3D ( 'NONE', #211436, #152782, #208869 ) ;
#201589 = FACE_OUTER_BOUND ( 'NONE', #6261, .T. ) ;
#201590 = EDGE_CURVE ( 'NONE', #113945, #162078, #124126, .T. ) ;
#201591 = CIRCLE ( 'NONE', #114102, 0.1000000000000024342 ) ;
#201592 = DIRECTION ( 'NONE',  ( -3.035766082959430717E-14, -6.982962677686266711E-15, 1.000000000000000000 ) ) ;
#201593 = CARTESIAN_POINT ( 'NONE',  ( -16.87242674293850797, 44.13448673903910446, -235.2993773395560311 ) ) ;
#201594 = EDGE_CURVE ( 'NONE', #230546, #154466, #186469, .T. ) ;
#201595 = ORIENTED_EDGE ( 'NONE', *, *, #115962, .T. ) ;
#201597 = ORIENTED_EDGE ( 'NONE', *, *, #98097, .T. ) ;
#201596 = VECTOR ( 'NONE', #178881, 1000.000000000000000 ) ;
#201598 = ORIENTED_EDGE ( 'NONE', *, *, #135325, .F. ) ;
#201599 = AXIS2_PLACEMENT_3D ( 'NONE', #42839, #257981, #2405 ) ;
#201600 = CARTESIAN_POINT ( 'NONE',  ( -21.04999999999999716, -0.01465611850265158278, -127.5033134142315987 ) ) ;
#201601 = ORIENTED_EDGE ( 'NONE', *, *, #63256, .T. ) ;
#201602 = CARTESIAN_POINT ( 'NONE',  ( 21.05000000000000071, 1.349084418627015447, -7.986498963545480834 ) ) ;
#201603 = ORIENTED_EDGE ( 'NONE', *, *, #5215, .T. ) ;
#201604 = EDGE_CURVE ( 'NONE', #244131, #178769, #190776, .T. ) ;
#201605 = DIRECTION ( 'NONE',  ( 1.000000000000000000, 0.000000000000000000, -0.000000000000000000 ) ) ;
#201606 = DIRECTION ( 'NONE',  ( -0.000000000000000000, 6.982962677686266711E-15, -1.000000000000000000 ) ) ;
#201607 = ADVANCED_FACE ( 'NONE', ( #7877 ), #165671, .F. ) ;
#201608 = ORIENTED_EDGE ( 'NONE', *, *, #151575, .T. ) ;
#201609 = CARTESIAN_POINT ( 'NONE',  ( 18.79999999999999716, 0.000000000000000000, 0.000000000000000000 ) ) ;
#201610 = FILL_AREA_STYLE_COLOUR ( '', #102525 ) ;
#201611 = EDGE_CURVE ( 'NONE', #1095, #16549, #174036, .T. ) ;
#201612 = VERTEX_POINT ( 'NONE', #69139 ) ;
#201613 = EDGE_LOOP ( 'NONE', ( #7668, #158725 ) ) ;
#201614 = AXIS2_PLACEMENT_3D ( 'NONE', #151484, #212729, #154077 ) ;
#201615 = ORIENTED_EDGE ( 'NONE', *, *, #175028, .T. ) ;
#201616 = TOROIDAL_SURFACE ( 'NONE', #68358, 0.2000000000000000111, 0.1000000000000000056 ) ;
#201617 = EDGE_CURVE ( 'NONE', #109454, #204085, #67826, .T. ) ;
#201618 = CARTESIAN_POINT ( 'NONE',  ( -20.64999999999999858, 71.75000000001205080, -124.2731074845243313 ) ) ;
#201619 = DIRECTION ( 'NONE',  ( 0.000000000000000000, -0.2128009952263485993, 0.9770955615653341697 ) ) ;
#201620 = DIRECTION ( 'NONE',  ( -1.000000000000000000, -1.394253735153569469E-16, -2.602809386958778209E-16 ) ) ;
#201621 = AXIS2_PLACEMENT_3D ( 'NONE', #228339, #186653, #225736 ) ;
#201622 = DIRECTION ( 'NONE',  ( 1.000000000000000000, 0.000000000000000000, 0.000000000000000000 ) ) ;
#201623 = CARTESIAN_POINT ( 'NONE',  ( 22.50000000000000000, 1.115600667400684642E-11, -33.50000000000000000 ) ) ;
#201625 = DIRECTION ( 'NONE',  ( 0.000000000000000000, 6.982962677686266711E-15, -1.000000000000000000 ) ) ;
#201624 = CYLINDRICAL_SURFACE ( 'NONE', #95662, 0.09999999999999939493 ) ;
#201626 = DIRECTION ( 'NONE',  ( -1.000000000000000000, 0.000000000000000000, 0.000000000000000000 ) ) ;
#201628 = ORIENTED_EDGE ( 'NONE', *, *, #218005, .T. ) ;
#201627 = FACE_OUTER_BOUND ( 'NONE', #238907, .T. ) ;
#201629 = CARTESIAN_POINT ( 'NONE',  ( 21.08621493067296626, 69.65070570884027745, -103.0793023240004658 ) ) ;
#201630 = CARTESIAN_POINT ( 'NONE',  ( 20.12500000000000355, 66.74195072709500209, -161.6597686473819806 ) ) ;
#201631 = ADVANCED_FACE ( 'NONE', ( #185212 ), #199969, .F. ) ;
#201632 = EDGE_LOOP ( 'NONE', ( #205837, #133326, #53705, #232841, #29507, #54185 ) ) ;
#201633 = LINE ( 'NONE', #137795, #133873 ) ;
#201635 = AXIS2_PLACEMENT_3D ( 'NONE', #204148, #145465, #129761 ) ;
#201634 = DIRECTION ( 'NONE',  ( 0.000000000000000000, 0.3994087351226822125, 0.9167729611565227366 ) ) ;
#201636 = DIRECTION ( 'NONE',  ( 0.000000000000000000, 0.000000000000000000, -1.000000000000000000 ) ) ;
#201637 = AXIS2_PLACEMENT_3D ( 'NONE', #163593, #142719, #27962 ) ;
#201638 = VERTEX_POINT ( 'NONE', #6569 ) ;
#201639 = CIRCLE ( 'NONE', #80812, 0.1000000000000028644 ) ;
#201640 = CIRCLE ( 'NONE', #105756, 0.1000000000000021289 ) ;
#201641 = CARTESIAN_POINT ( 'NONE',  ( 21.08035267497491105, 69.66829316022966623, -203.6057961093005417 ) ) ;
#201642 = DIRECTION ( 'NONE',  ( 1.000000000000000000, 0.000000000000000000, -0.000000000000000000 ) ) ;
#201643 = ORIENTED_EDGE ( 'NONE', *, *, #222397, .F. ) ;
#201644 = ORIENTED_EDGE ( 'NONE', *, *, #158322, .F. ) ;
#201645 = VECTOR ( 'NONE', #256265, 1000.000000000000000 ) ;
#201646 = CARTESIAN_POINT ( 'NONE',  ( -16.86445178670637546, 9.962211629115978795, -12.60922256188275092 ) ) ;
#201647 = ORIENTED_EDGE ( 'NONE', *, *, #79120, .T. ) ;
#201648 = CARTESIAN_POINT ( 'NONE',  ( -20.94999999999999929, -11.48912529307605546, -30.39999999999999503 ) ) ;
#201649 = CARTESIAN_POINT ( 'NONE',  ( -18.52309608778520200, -9.642476320044035987, -174.2145963411697096 ) ) ;
#201650 = CARTESIAN_POINT ( 'NONE',  ( 20.94999999999999929, 1.835341550235569663, -145.5551512925629822 ) ) ;
#201651 = CARTESIAN_POINT ( 'NONE',  ( 21.14999999999999503, 11.65000000001116298, -134.1000000000000227 ) ) ;
#201652 = ORIENTED_EDGE ( 'NONE', *, *, #101499, .F. ) ;
#201653 = VECTOR ( 'NONE', #1341, 1000.000000000000000 ) ;
#201654 = CIRCLE ( 'NONE', #105952, 11.75000000000001066 ) ;
#201655 = AXIS2_PLACEMENT_3D ( 'NONE', #184700, #221250, #124746 ) ;
#201656 = DIRECTION ( 'NONE',  ( 0.000000000000000000, -0.9126074666063769270, -0.4088369013363280513 ) ) ;
#201657 = CARTESIAN_POINT ( 'NONE',  ( -20.94999999999999929, 77.36242903720516040, -95.13422623660308375 ) ) ;
#201658 = CARTESIAN_POINT ( 'NONE',  ( -18.59999999999999787, 4.158309866074138661, -211.9342015984041439 ) ) ;
#201659 = CARTESIAN_POINT ( 'NONE',  ( 20.94999999999999929, 10.72371710471867701, -41.16491356908760935 ) ) ;
#201660 = EDGE_CURVE ( 'NONE', #195402, #71875, #88649, .T. ) ;
#201661 = ORIENTED_EDGE ( 'NONE', *, *, #242816, .F. ) ;
#201663 = ORIENTED_EDGE ( 'NONE', *, *, #236638, .T. ) ;
#201662 = CARTESIAN_POINT ( 'NONE',  ( 18.49999999999999289, 10.20857864376269575, 11.75000000000000000 ) ) ;
#201664 = DIRECTION ( 'NONE',  ( 0.000000000000000000, -6.938893903907222067E-15, 1.000000000000000000 ) ) ;
#201665 = CARTESIAN_POINT ( 'NONE',  ( 18.49999999999997513, 78.12133356376092763, -231.3112718935514920 ) ) ;
#201666 = CARTESIAN_POINT ( 'NONE',  ( -20.54999999999999716, 85.00000000001149658, -45.91707660717669626 ) ) ;
#201667 = CARTESIAN_POINT ( 'NONE',  ( -23.25000000000000000, 51.33926024308902214, -230.0993571250899379 ) ) ;
#201668 = CARTESIAN_POINT ( 'NONE',  ( 21.51976009735019346, 10.39190259496836433, -227.6411649781647384 ) ) ;
#201669 = CYLINDRICAL_SURFACE ( 'NONE', #148909, 0.09999999999999935330 ) ;
#201670 = VERTEX_POINT ( 'NONE', #65260 ) ;
#201671 = DIRECTION ( 'NONE',  ( 0.000000000000000000, 7.026728003956683390E-15, -1.000000000000000000 ) ) ;
#201672 = AXIS2_PLACEMENT_3D ( 'NONE', #215408, #216694, #13370 ) ;
#201673 = CARTESIAN_POINT ( 'NONE',  ( -16.77828822508139694, 9.946229374931901290, -146.6626282513739739 ) ) ;
#201674 = CARTESIAN_POINT ( 'NONE',  ( -18.33682934331483949, 77.42195030185330040, -241.7118189958663095 ) ) ;
#201676 = AXIS2_PLACEMENT_3D ( 'NONE', #126430, #143425, #169455 ) ;
#201675 = CARTESIAN_POINT ( 'NONE',  ( 21.07016717456945187, 6.320940838111423155, -134.0000000000000000 ) ) ;
#201677 = EDGE_CURVE ( 'NONE', #128733, #218531, #182383, .T. ) ;
#201678 = CIRCLE ( 'NONE', #51815, 0.1000000000000028644 ) ;
#201679 = DIRECTION ( 'NONE',  ( 0.000000000000000000, 0.000000000000000000, -1.000000000000000000 ) ) ;
#201680 = CARTESIAN_POINT ( 'NONE',  ( -23.15000000000000213, 2.000000000011154189, -113.7246219227621395 ) ) ;
#201681 = ORIENTED_EDGE ( 'NONE', *, *, #19651, .T. ) ;
#201682 = ORIENTED_EDGE ( 'NONE', *, *, #119188, .F. ) ;
#201683 = LINE ( 'NONE', #20505, #83283 ) ;
#201684 = CIRCLE ( 'NONE', #205777, 0.09999999999999939493 ) ;
#201685 = DIRECTION ( 'NONE',  ( 1.000000000000000000, -0.000000000000000000, -0.000000000000000000 ) ) ;
#201686 = CARTESIAN_POINT ( 'NONE',  ( 21.15000000000005542, 74.26359666348515987, -47.54092689884382850 ) ) ;
#201687 = TOROIDAL_SURFACE ( 'NONE', #18532, 0.4000000000000005773, 0.1000000000000000056 ) ;
#201688 = DIRECTION ( 'NONE',  ( 0.000000000000000000, 0.000000000000000000, 1.000000000000000000 ) ) ;
#201689 =( BOUNDED_CURVE ( )  B_SPLINE_CURVE ( 3, ( #189033, #89915, #208612, #249024 ),
 .UNSPECIFIED., .F., .F. ) 
 B_SPLINE_CURVE_WITH_KNOTS ( ( 4, 4 ),
 ( 5.731445031868799056, 5.983100554402348337 ),
 .UNSPECIFIED. ) 
 CURVE ( )  GEOMETRIC_REPRESENTATION_ITEM ( )  RATIONAL_B_SPLINE_CURVE ( ( 1.000000000000000000, 0.9947294176030464508, 0.9947294176030464508, 1.000000000000000000 ) ) 
 REPRESENTATION_ITEM ( '' )  );
#201690 = VERTEX_POINT ( 'NONE', #9147 ) ;
#201691 = CIRCLE ( 'NONE', #51831, 11.70000000000000284 ) ;
#201693 = AXIS2_PLACEMENT_3D ( 'NONE', #184579, #89320, #165024 ) ;
#201692 = LINE ( 'NONE', #200414, #113530 ) ;
#201694 = DIRECTION ( 'NONE',  ( 2.952720810173289605E-16, -0.9770955615653313941, -0.2128009952263610616 ) ) ;
#201695 = CIRCLE ( 'NONE', #151839, 4.099999999999992539 ) ;
#201696 = AXIS2_PLACEMENT_3D ( 'NONE', #7230, #183326, #4659 ) ;
#201697 = PRODUCT_DEFINITION_SHAPE ( 'NONE', 'NONE',  #70844 ) ;
#201698 = FACE_OUTER_BOUND ( 'NONE', #80510, .T. ) ;
#201699 = CIRCLE ( 'NONE', #214184, 0.1000000000000055844 ) ;
#201700 = VERTEX_POINT ( 'NONE', #245193 ) ;
#201701 = DIRECTION ( 'NONE',  ( 0.000000000000000000, -0.9651348961777157509, 0.2617529984165031243 ) ) ;
#201702 = ORIENTED_EDGE ( 'NONE', *, *, #63785, .F. ) ;
#201703 = CARTESIAN_POINT ( 'NONE',  ( 18.60000000000000142, 85.32100840337392356, -196.2871692354463846 ) ) ;
#201704 = CARTESIAN_POINT ( 'NONE',  ( 21.07954763557393818, 69.67070900997511274, -170.0889834031426915 ) ) ;
#201706 = AXIS2_PLACEMENT_3D ( 'NONE', #215768, #78819, #239202 ) ;
#201705 = CARTESIAN_POINT ( 'NONE',  ( 20.94999999999999929, 6.846123162363745074, -171.2377262668498759 ) ) ;
#201707 = CARTESIAN_POINT ( 'NONE',  ( 18.55807992284871588, 65.67101464000481315, -63.94043916224794089 ) ) ;
#201708 = DIRECTION ( 'NONE',  ( 0.000000000000000000, -0.2128009952263604232, 0.9770955615653316162 ) ) ;
#201709 = PLANE ( 'NONE',  #2076 ) ;
#201710 = FACE_OUTER_BOUND ( 'NONE', #159568, .T. ) ;
#201711 = CARTESIAN_POINT ( 'NONE',  ( -14.00000000000000178, 9.850000000011133849, -50.25000000000000711 ) ) ;
#201712 = CARTESIAN_POINT ( 'NONE',  ( -21.93340585971692391, 7.324147022868191748, -67.00000000000004263 ) ) ;
#201713 = VECTOR ( 'NONE', #115594, 1000.000000000000000 ) ;
#201714 = CARTESIAN_POINT ( 'NONE',  ( 5.899999999999996803, -11.25000000000000000, 13.90000000000000213 ) ) ;
#201716 = ADVANCED_FACE ( 'NONE', ( #86075 ), #99536, .F. ) ;
#201715 = DIRECTION ( 'NONE',  ( 1.000000000000000000, -0.000000000000000000, 0.000000000000000000 ) ) ;
#201717 = CARTESIAN_POINT ( 'NONE',  ( 20.94999999999999929, 54.36558989155976462, -236.3448031251562327 ) ) ;
#201718 = CIRCLE ( 'NONE', #155959, 0.09999999999998898659 ) ;
#201719 = CARTESIAN_POINT ( 'NONE',  ( -21.04999999999999716, 69.69257478044623610, -69.50628761613869244 ) ) ;
#201720 = PLANE ( 'NONE',  #199482 ) ;
#201721 = AXIS2_PLACEMENT_3D ( 'NONE', #98888, #57203, #19395 ) ;
#201722 = CIRCLE ( 'NONE', #230979, 6.329289321881358177 ) ;
#201723 = ORIENTED_EDGE ( 'NONE', *, *, #45106, .F. ) ;
#201724 = DIRECTION ( 'NONE',  ( -0.000000000000000000, -0.01283462868040327436, 0.9999176327611370985 ) ) ;
#201726 = EDGE_CURVE ( 'NONE', #214984, #232621, #74073, .T. ) ;
#201725 = DIRECTION ( 'NONE',  ( -1.000000000000000000, 0.000000000000000000, 0.000000000000000000 ) ) ;
#201727 = VERTEX_POINT ( 'NONE', #191665 ) ;
#201729 = ADVANCED_FACE ( 'NONE', ( #33889 ), #249056, .T. ) ;
#201728 = CARTESIAN_POINT ( 'NONE',  ( -22.50000000000000000, 0.09263750062063526303, -55.35030279295929745 ) ) ;
#201730 = FACE_OUTER_BOUND ( 'NONE', #62961, .T. ) ;
#201731 = CARTESIAN_POINT ( 'NONE',  ( -21.05000000000000071, 28.50120599808395028, -258.2149742250584268 ) ) ;
#201732 = ORIENTED_EDGE ( 'NONE', *, *, #153553, .T. ) ;
#201733 = CARTESIAN_POINT ( 'NONE',  ( -23.25000000000000000, 76.00000000001190870, -103.0231074845243029 ) ) ;
#201734 = DIRECTION ( 'NONE',  ( -1.000000000000000000, -0.000000000000000000, 0.000000000000000000 ) ) ;
#201735 = EDGE_CURVE ( 'NONE', #220516, #210647, #69955, .T. ) ;
#201736 = VERTEX_POINT ( 'NONE', #229482 ) ;
#201737 = EDGE_LOOP ( 'NONE', ( #144754, #87620 ) ) ;
#201738 = DIRECTION ( 'NONE',  ( -1.000000000000000000, -0.000000000000000000, -0.000000000000000000 ) ) ;
#201739 = VERTEX_POINT ( 'NONE', #228200 ) ;
#201740 = EDGE_CURVE ( 'NONE', #234652, #240390, #170839, .T. ) ;
#201741 = DIRECTION ( 'NONE',  ( 1.000000000000000000, 0.000000000000000000, 0.000000000000000000 ) ) ;
#201742 = DIRECTION ( 'NONE',  ( 1.000000000000000000, 0.000000000000000000, 0.000000000000000000 ) ) ;
#201744 = DIRECTION ( 'NONE',  ( -1.000000000000000000, 7.304098846218134667E-16, 2.111765289898285610E-31 ) ) ;
#201743 = UNCERTAINTY_MEASURE_WITH_UNIT (LENGTH_MEASURE( 1.000000000000000082E-05 ), #93212, 'distance_accuracy_value', 'NONE');
#201745 = DIRECTION ( 'NONE',  ( -0.000000000000000000, -0.9875055080513799322, 0.1575844902526464253 ) ) ;
#201746 = DIRECTION ( 'NONE',  ( 1.000000000000000000, 7.304098846218133681E-16, 5.100424963727255128E-30 ) ) ;
#201747 = CARTESIAN_POINT ( 'NONE',  ( 13.40000000000000036, -11.65000000000000036, 12.30000000000000426 ) ) ;
#201748 = DIRECTION ( 'NONE',  ( 0.000000000000000000, -6.853228547068871147E-15, 1.000000000000000000 ) ) ;
#201749 = CARTESIAN_POINT ( 'NONE',  ( -21.14999999999999858, 6.257814610476114758, 0.09779029130879343668 ) ) ;
#201751 = ORIENTED_EDGE ( 'NONE', *, *, #94653, .T. ) ;
#201750 = CARTESIAN_POINT ( 'NONE',  ( -18.40000000000000213, -9.519327731081286714, -40.47297637655933045 ) ) ;
#201752 = VERTEX_POINT ( 'NONE', #251603 ) ;
#201754 = CARTESIAN_POINT ( 'NONE',  ( 18.59999999999999787, 74.14897176987071248, -57.86919421510183525 ) ) ;
#201753 = DIRECTION ( 'NONE',  ( -1.000000000000000000, -0.000000000000000000, 0.000000000000000000 ) ) ;
#201756 = ORIENTED_EDGE ( 'NONE', *, *, #240200, .T. ) ;
#201755 = CARTESIAN_POINT ( 'NONE',  ( 21.12769345151713196, 10.71928767695172624, -146.2474803461975057 ) ) ;
#201757 = EDGE_LOOP ( 'NONE', ( #257028, #66600, #207453, #167226 ) ) ;
#201758 = DIRECTION ( 'NONE',  ( -1.000000000000000000, -2.952720810173289112E-16, 0.000000000000000000 ) ) ;
#201759 = CARTESIAN_POINT ( 'NONE',  ( 20.50589344625199217, 10.48318793148705197, -175.0729949786710051 ) ) ;
#201760 = DIRECTION ( 'NONE',  ( 0.000000000000000000, 0.000000000000000000, 1.000000000000000000 ) ) ;
#201761 = CARTESIAN_POINT ( 'NONE',  ( 21.14999999999999858, 21.13195309841794867, -243.6318585593223816 ) ) ;
#201762 = LINE ( 'NONE', #83063, #20841 ) ;
#201763 = CARTESIAN_POINT ( 'NONE',  ( -18.59999999999999787, 3.912899247233453615, -11.48182297301096888 ) ) ;
#201764 = EDGE_CURVE ( 'NONE', #94186, #77399, #219763, .T. ) ;
#201765 = FACE_OUTER_BOUND ( 'NONE', #185171, .T. ) ;
#201766 = ORIENTED_EDGE ( 'NONE', *, *, #242190, .F. ) ;
#201767 = VERTEX_POINT ( 'NONE', #109510 ) ;
#201768 = DIRECTION ( 'NONE',  ( -1.000000000000000000, -0.000000000000000000, 0.000000000000000000 ) ) ;
#201769 = AXIS2_PLACEMENT_3D ( 'NONE', #132888, #169482, #251530 ) ;
#201770 = CIRCLE ( 'NONE', #235119, 11.80000000000000426 ) ;
#201771 = ORIENTED_EDGE ( 'NONE', *, *, #247165, .F. ) ;
#201772 = DIRECTION ( 'NONE',  ( 0.000000000000000000, -7.086529944415894657E-15, 1.000000000000000000 ) ) ;
#201773 = VERTEX_POINT ( 'NONE', #190368 ) ;
#201774 = CARTESIAN_POINT ( 'NONE',  ( 18.59999999999999076, 77.16412189325286874, -61.60825939895269698 ) ) ;
#201775 = AXIS2_PLACEMENT_3D ( 'NONE', #157740, #139386, #58567 ) ;
#201776 = VECTOR ( 'NONE', #185722, 1000.000000000000227 ) ;
#201777 = ADVANCED_FACE ( 'NONE', ( #113379 ), #35165, .T. ) ;
#201778 = CARTESIAN_POINT ( 'NONE',  ( -14.56336952470180179, 49.59862664907820573, -233.4030665626792711 ) ) ;
#201779 = CARTESIAN_POINT ( 'NONE',  ( 20.97224591636399538, 10.62515341617478271, -146.2499259046635984 ) ) ;
#201780 = CARTESIAN_POINT ( 'NONE',  ( -16.86445178670605216, 22.94788858557290467, -230.9050441021552160 ) ) ;
#201781 = ORIENTED_EDGE ( 'NONE', *, *, #126351, .T. ) ;
#201783 = EDGE_CURVE ( 'NONE', #200249, #129114, #35681, .T. ) ;
#201782 = DIRECTION ( 'NONE',  ( -1.000000000000000000, -0.000000000000000000, -0.000000000000000000 ) ) ;
#201784 = VERTEX_POINT ( 'NONE', #95095 ) ;
#201785 = DIRECTION ( 'NONE',  ( 0.000000000000000000, 0.000000000000000000, 1.000000000000000000 ) ) ;
#201786 = DIRECTION ( 'NONE',  ( 1.000000000000000000, 0.000000000000000000, 0.000000000000000000 ) ) ;
#201788 = CIRCLE ( 'NONE', #226736, 0.1000000000000028644 ) ;
#201787 = DIRECTION ( 'NONE',  ( 0.000000000000000000, 0.000000000000000000, 1.000000000000000000 ) ) ;
#201789 = DIRECTION ( 'NONE',  ( 1.000000000000000000, 0.000000000000000000, 0.000000000000000000 ) ) ;
#201790 = EDGE_CURVE ( 'NONE', #7857, #62333, #230776, .T. ) ;
#201791 = ORIENTED_EDGE ( 'NONE', *, *, #114847, .T. ) ;
#201792 = CARTESIAN_POINT ( 'NONE',  ( -20.85000000000000497, 36.10799525571641766, -235.9264213948819702 ) ) ;
#201794 = ORIENTED_EDGE ( 'NONE', *, *, #3215, .T. ) ;
#201793 = CIRCLE ( 'NONE', #135141, 11.65000000000000036 ) ;
#201796 = ORIENTED_EDGE ( 'NONE', *, *, #250997, .F. ) ;
#201795 = CARTESIAN_POINT ( 'NONE',  ( -21.05000000000000071, 11.40444339177023814, -198.6185779617709670 ) ) ;
#201797 = DIRECTION ( 'NONE',  ( 0.000000000000000000, 0.000000000000000000, -1.000000000000000000 ) ) ;
#201799 = VERTEX_POINT ( 'NONE', #232059 ) ;
#201798 = CIRCLE ( 'NONE', #160141, 0.09999999999999939493 ) ;
#201800 = CIRCLE ( 'NONE', #239409, 0.1000000000000028644 ) ;
#201801 = DIRECTION ( 'NONE',  ( 0.000000000000000000, 0.000000000000000000, -1.000000000000000000 ) ) ;
#201802 = ORIENTED_EDGE ( 'NONE', *, *, #85294, .T. ) ;
#201804 = DIRECTION ( 'NONE',  ( 0.000000000000000000, 0.000000000000000000, -1.000000000000000000 ) ) ;
#201803 = VECTOR ( 'NONE', #232205, 1000.000000000000000 ) ;
#201806 = EDGE_CURVE ( 'NONE', #7200, #250279, #91255, .T. ) ;
#201805 = DIRECTION ( 'NONE',  ( 0.000000000000000000, 1.224646799142185182E-16, 1.000000000000000000 ) ) ;
#201807 = CARTESIAN_POINT ( 'NONE',  ( 21.30000000000002558, 7.128833340093095217, -233.7327013124392749 ) ) ;
#201808 = CARTESIAN_POINT ( 'NONE',  ( 23.40000000000005187, 74.25000000001119815, -47.64205752314703801 ) ) ;
#201809 = AXIS2_PLACEMENT_3D ( 'NONE', #251439, #136605, #37538 ) ;
#201810 = CIRCLE ( 'NONE', #60804, 0.1000000000000045158 ) ;
#201811 = EDGE_CURVE ( 'NONE', #194623, #184568, #257318, .T. ) ;
#201812 = AXIS2_PLACEMENT_3D ( 'NONE', #59630, #101301, #20564 ) ;
#201813 = EDGE_CURVE ( 'NONE', #232370, #190072, #208646, .T. ) ;
#201814 = CARTESIAN_POINT ( 'NONE',  ( -16.87435696428308063, 9.950002462932223679, -12.64999176516656654 ) ) ;
#201815 = AXIS2_PLACEMENT_3D ( 'NONE', #123191, #223550, #51323 ) ;
#201816 = EDGE_LOOP ( 'NONE', ( #74970, #211317, #188773, #42830 ) ) ;
#201817 = DIRECTION ( 'NONE',  ( 1.000000000000000000, 0.000000000000000000, 0.000000000000000000 ) ) ;
#201818 = CARTESIAN_POINT ( 'NONE',  ( 22.47007471830798764, 59.77974727959318813, -233.8342073434304211 ) ) ;
#201819 = CIRCLE ( 'NONE', #51769, 0.09999999999998898659 ) ;
#201820 = CARTESIAN_POINT ( 'NONE',  ( -20.64999999999999858, 76.52350599684427834, -201.5928376921694678 ) ) ;
#201821 = ORIENTED_EDGE ( 'NONE', *, *, #335, .T. ) ;
#201822 = DIRECTION ( 'NONE',  ( -0.000000000000000000, 0.4856429311786307212, 0.8741572761215384846 ) ) ;
#201823 = ORIENTED_EDGE ( 'NONE', *, *, #63875, .F. ) ;
#201824 = CARTESIAN_POINT ( 'NONE',  ( 20.09999999999999787, 9.749999999999982236, -20.84999999999999787 ) ) ;
#201825 = EDGE_CURVE ( 'NONE', #116784, #137324, #136559, .T. ) ;
#201826 = CIRCLE ( 'NONE', #135361, 0.8750000000000007772 ) ;
#201827 = LINE ( 'NONE', #102698, #193168 ) ;
#201828 = CARTESIAN_POINT ( 'NONE',  ( 20.96428641293828576, 36.19089144327175944, -235.9708266132240055 ) ) ;
#201830 = ORIENTED_EDGE ( 'NONE', *, *, #23501, .T. ) ;
#201829 = CARTESIAN_POINT ( 'NONE',  ( -16.94275863009466576, 9.989496048673542461, -146.6083026179589126 ) ) ;
#201831 = EDGE_CURVE ( 'NONE', #222470, #159949, #107343, .T. ) ;
#201832 = DIRECTION ( 'NONE',  ( 0.000000000000000000, 1.000000000000000000, 0.000000000000000000 ) ) ;
#201833 = EDGE_CURVE ( 'NONE', #240390, #90545, #86473, .T. ) ;
#201834 = VECTOR ( 'NONE', #116836, 1000.000000000000000 ) ;
#201835 = AXIS2_PLACEMENT_3D ( 'NONE', #51980, #128980, #229368 ) ;
#201836 = CARTESIAN_POINT ( 'NONE',  ( 20.94999999999999574, -11.41227409413852989, -103.5000000000000426 ) ) ;
#201837 = ORIENTED_EDGE ( 'NONE', *, *, #81499, .F. ) ;
#201838 = CARTESIAN_POINT ( 'NONE',  ( -21.14999999999999858, 64.35000000001238618, -169.9231074845244507 ) ) ;
#201839 = DIRECTION ( 'NONE',  ( 0.000000000000000000, -0.4088369013362687654, 0.9126074666064034613 ) ) ;
#201840 = ORIENTED_EDGE ( 'NONE', *, *, #117614, .T. ) ;
#201841 = FACE_OUTER_BOUND ( 'NONE', #189954, .T. ) ;
#201842 = ORIENTED_EDGE ( 'NONE', *, *, #150055, .F. ) ;
#201843 = LINE ( 'NONE', #81861, #54377 ) ;
#201844 = ORIENTED_EDGE ( 'NONE', *, *, #70321, .T. ) ;
#201846 = ORIENTED_EDGE ( 'NONE', *, *, #166492, .F. ) ;
#201845 = CARTESIAN_POINT ( 'NONE',  ( -21.05000000000000071, 11.65000000001115232, -107.2838656629781724 ) ) ;
#201847 = EDGE_CURVE ( 'NONE', #78551, #22582, #15813, .T. ) ;
#201848 = EDGE_CURVE ( 'NONE', #168409, #22177, #32563, .T. ) ;
#201851 = VERTEX_POINT ( 'NONE', #70439 ) ;
#201850 = ORIENTED_EDGE ( 'NONE', *, *, #108550, .F. ) ;
#201849 = DIRECTION ( 'NONE',  ( 0.000000000000000000, 0.000000000000000000, -1.000000000000000000 ) ) ;
#201852 = VECTOR ( 'NONE', #35029, 1000.000000000000000 ) ;
#201853 = DIRECTION ( 'NONE',  ( 0.000000000000000000, 0.9916376685811618685, -0.1290532225514649800 ) ) ;
#201854 = DIRECTION ( 'NONE',  ( 0.000000000000000000, 0.000000000000000000, -1.000000000000000000 ) ) ;
#201855 = CIRCLE ( 'NONE', #31220, 0.1000000000000028644 ) ;
#201857 = EDGE_CURVE ( 'NONE', #222045, #178174, #149958, .T. ) ;
#201856 = DIRECTION ( 'NONE',  ( 1.000000000000000000, 2.952720810173289112E-16, -0.000000000000000000 ) ) ;
#201859 = DIRECTION ( 'NONE',  ( 1.000000000000000000, 0.000000000000000000, 0.000000000000000000 ) ) ;
#201858 = CARTESIAN_POINT ( 'NONE',  ( -20.85000000000000142, 76.00000000001207923, -128.6231074845243540 ) ) ;
#201860 = CARTESIAN_POINT ( 'NONE',  ( -0.8999999999999986899, -12.25000000000000355, 26.00000000000000355 ) ) ;
#201861 = CIRCLE ( 'NONE', #185117, 0.1000000000000028644 ) ;
#201862 = CARTESIAN_POINT ( 'NONE',  ( 21.05000000000000071, 5.000000000011153745, -45.90526601891310321 ) ) ;
#201863 = CARTESIAN_POINT ( 'NONE',  ( 22.48660254037844197, 11.65000000000000746, 0.04999999999999796274 ) ) ;
#201865 = CARTESIAN_POINT ( 'NONE',  ( -23.25000000000000000, 72.03510814376021187, -246.5782642391033903 ) ) ;
#201864 = CYLINDRICAL_SURFACE ( 'NONE', #251015, 0.1000000000000001443 ) ;
#201866 = ORIENTED_EDGE ( 'NONE', *, *, #159806, .F. ) ;
#201868 = VERTEX_POINT ( 'NONE', #57225 ) ;
#201867 = AXIS2_PLACEMENT_3D ( 'NONE', #147268, #207267, #28664 ) ;
#201869 = CARTESIAN_POINT ( 'NONE',  ( 20.94999999999999929, 11.65000000001115943, -100.5000000000000426 ) ) ;
#201870 = AXIS2_PLACEMENT_3D ( 'NONE', #171501, #227583, #192320 ) ;
#201872 = EDGE_LOOP ( 'NONE', ( #118802, #174618 ) ) ;
#201871 = DIRECTION ( 'NONE',  ( -4.448008912761042820E-16, -1.000000000000000000, -7.116814260417668513E-15 ) ) ;
#201873 = EDGE_LOOP ( 'NONE', ( #204873, #252242, #66039, #153796 ) ) ;
#201874 = FACE_OUTER_BOUND ( 'NONE', #179844, .T. ) ;
#201875 = VERTEX_POINT ( 'NONE', #59788 ) ;
#201876 = FACE_OUTER_BOUND ( 'NONE', #100792, .T. ) ;
#201877 = VECTOR ( 'NONE', #176600, 1000.000000000000114 ) ;
#201878 = EDGE_CURVE ( 'NONE', #189061, #4212, #55942, .T. ) ;
#201879 = AXIS2_PLACEMENT_3D ( 'NONE', #234774, #156557, #217752 ) ;
#201880 = ORIENTED_EDGE ( 'NONE', *, *, #123122, .F. ) ;
#201881 = CIRCLE ( 'NONE', #172892, 0.09999999999998898659 ) ;
#201882 = DIRECTION ( 'NONE',  ( 0.000000000000000000, 0.000000000000000000, -1.000000000000000000 ) ) ;
#201884 = ADVANCED_FACE ( 'NONE', ( #139332 ), #138054, .T. ) ;
#201883 = LINE ( 'NONE', #42811, #219520 ) ;
#201885 = CIRCLE ( 'NONE', #35519, 11.75000000000001066 ) ;
#201887 = ORIENTED_EDGE ( 'NONE', *, *, #7, .F. ) ;
#201886 = ORIENTED_EDGE ( 'NONE', *, *, #217165, .F. ) ;
#201888 = ORIENTED_EDGE ( 'NONE', *, *, #103009, .T. ) ;
#201889 = DIRECTION ( 'NONE',  ( 0.000000000000000000, 0.5000000000000014433, -0.8660254037844378194 ) ) ;
#201890 = ORIENTED_EDGE ( 'NONE', *, *, #87131, .F. ) ;
#201891 = EDGE_LOOP ( 'NONE', ( #184254, #123742, #109330, #226668 ) ) ;
#201892 = DIRECTION ( 'NONE',  ( 1.073024830501117725E-15, -0.000000000000000000, -1.000000000000000000 ) ) ;
#201895 = EDGE_CURVE ( 'NONE', #11153, #61360, #169944, .T. ) ;
#201894 = EDGE_LOOP ( 'NONE', ( #211131, #5391, #76562, #123492 ) ) ;
#201893 = CARTESIAN_POINT ( 'NONE',  ( 18.49999999999999645, 5.699452464332751767, -154.9577260434301422 ) ) ;
#201896 = CIRCLE ( 'NONE', #151856, 0.09999999999999982514 ) ;
#201898 = CARTESIAN_POINT ( 'NONE',  ( -23.25000000000000000, 76.00000000001142553, -36.02310748452432421 ) ) ;
#201897 = DIRECTION ( 'NONE',  ( -4.408576920032448588E-17, -0.3896596508880098009, -0.9209589331071361684 ) ) ;
#201899 = DIRECTION ( 'NONE',  ( 0.000000000000000000, 1.000000000000000000, 0.000000000000000000 ) ) ;
#201900 = FACE_OUTER_BOUND ( 'NONE', #73435, .T. ) ;
#201901 = FACE_OUTER_BOUND ( 'NONE', #256591, .T. ) ;
#201902 = ORIENTED_EDGE ( 'NONE', *, *, #146564, .T. ) ;
#201903 = EDGE_CURVE ( 'NONE', #43421, #106103, #78084, .T. ) ;
#201904 = EDGE_LOOP ( 'NONE', ( #31121, #71393, #206273, #143918 ) ) ;
#201905 = DIRECTION ( 'NONE',  ( 1.000000000000000000, 0.000000000000000000, 0.000000000000000000 ) ) ;
#201906 = DIRECTION ( 'NONE',  ( 0.000000000000000000, 0.000000000000000000, 1.000000000000000000 ) ) ;
#201907 = EDGE_CURVE ( 'NONE', #145277, #128109, #140670, .T. ) ;
#201908 = VERTEX_POINT ( 'NONE', #16859 ) ;
#201909 = DIRECTION ( 'NONE',  ( 1.000000000000000000, -2.952720810173289112E-16, -2.061873921506763405E-30 ) ) ;
#201910 = VECTOR ( 'NONE', #8814, 1000.000000000000000 ) ;
#201911 = ADVANCED_FACE ( 'NONE', ( #255395 ), #76808, .F. ) ;
#201912 = CARTESIAN_POINT ( 'NONE',  ( -18.59999999999999787, 79.19526988099229925, -196.1889237952725296 ) ) ;
#201913 = AXIS2_PLACEMENT_3D ( 'NONE', #187310, #132452, #13791 ) ;
#201914 = CARTESIAN_POINT ( 'NONE',  ( -15.15766958671844300, 12.47908687115373105, -214.0766389635195139 ) ) ;
#201916 = ADVANCED_FACE ( 'NONE', ( #218874, #256683 ), #96356, .T. ) ;
#201915 = EDGE_CURVE ( 'NONE', #203994, #176131, #232285, .T. ) ;
#201917 = VERTEX_POINT ( 'NONE', #2389 ) ;
#201918 = EDGE_LOOP ( 'NONE', ( #130751, #173803, #79171, #202599, #2655, #11719, #49339, #249327, #12123, #179677, #85640, #39963 ) ) ;
#201919 = CARTESIAN_POINT ( 'NONE',  ( 18.79999999999999005, -1.212568896937008089, -8.000000000000000000 ) ) ;
#201920 = DIRECTION ( 'NONE',  ( 0.000000000000000000, -0.4646089985449268767, -0.8855159391400474478 ) ) ;
#201921 = ORIENTED_EDGE ( 'NONE', *, *, #34749, .T. ) ;
#201922 = DIRECTION ( 'NONE',  ( -0.000000000000000000, 0.1298341882520022694, 0.9915357197604853789 ) ) ;
#201923 = VERTEX_POINT ( 'NONE', #19417 ) ;
#201924 = EDGE_CURVE ( 'NONE', #114500, #97606, #98910, .T. ) ;
#201925 = CARTESIAN_POINT ( 'NONE',  ( -21.14999999999999858, 76.00000000001246292, -181.6726782920691505 ) ) ;
#201926 = DIRECTION ( 'NONE',  ( 0.000000000000000000, 0.000000000000000000, -1.000000000000000000 ) ) ;
#201928 = CARTESIAN_POINT ( 'NONE',  ( -20.64999999999999858, 2.000000000011154189, -54.27537807723790309 ) ) ;
#201927 = CARTESIAN_POINT ( 'NONE',  ( -21.93642651522410247, 10.58866904893262628, -227.2738390313130878 ) ) ;
#201929 = FACE_OUTER_BOUND ( 'NONE', #190542, .T. ) ;
#201930 = DIRECTION ( 'NONE',  ( 3.469446951953635015E-14, 6.982962677686266711E-15, -1.000000000000000000 ) ) ;
#201931 = VERTEX_POINT ( 'NONE', #119815 ) ;
#201932 = CARTESIAN_POINT ( 'NONE',  ( 18.52326479938690795, -9.642364444904243825, -207.7147574134057493 ) ) ;
#201933 = EDGE_CURVE ( 'NONE', #139671, #86511, #136777, .T. ) ;
#201934 = AXIS2_PLACEMENT_3D ( 'NONE', #144799, #160555, #83524 ) ;
#201935 = EDGE_CURVE ( 'NONE', #7608, #121941, #132476, .T. ) ;
#201937 = VERTEX_POINT ( 'NONE', #177230 ) ;
#201936 = ORIENTED_EDGE ( 'NONE', *, *, #50008, .T. ) ;
#201938 = ORIENTED_EDGE ( 'NONE', *, *, #78014, .T. ) ;
#201939 = ORIENTED_EDGE ( 'NONE', *, *, #225424, .T. ) ;
#201940 = EDGE_CURVE ( 'NONE', #99842, #29322, #7384, .T. ) ;
#201941 = CARTESIAN_POINT ( 'NONE',  ( 22.14074124539698829, 7.390077851054901892, -33.40094710415593227 ) ) ;
#201942 = DIRECTION ( 'NONE',  ( 0.000000000000000000, -0.2128009952263604232, 0.9770955615653316162 ) ) ;
#201943 = CIRCLE ( 'NONE', #89481, 0.1000000000000106498 ) ;
#201944 = CARTESIAN_POINT ( 'NONE',  ( -20.65000000000000568, 9.052352027203962592, -208.4953267290897543 ) ) ;
#201945 = DIRECTION ( 'NONE',  ( -0.000000000000000000, -0.1298341882519805091, -0.9915357197604881545 ) ) ;
#201946 = DIRECTION ( 'NONE',  ( 0.000000000000000000, 0.000000000000000000, -1.000000000000000000 ) ) ;
#201948 = CARTESIAN_POINT ( 'NONE',  ( -18.59999999999999787, 64.25000000001203659, -114.7731074845243882 ) ) ;
#201947 = CARTESIAN_POINT ( 'NONE',  ( 22.39999999999999503, -3.140208063160686791, -228.2318569537739847 ) ) ;
#201949 = EDGE_CURVE ( 'NONE', #66247, #88568, #40762, .T. ) ;
#201951 = ORIENTED_EDGE ( 'NONE', *, *, #53749, .F. ) ;
#201950 = CARTESIAN_POINT ( 'NONE',  ( 18.31325810956139577, 77.39829188374345392, -241.7500340231811720 ) ) ;
#201952 = CARTESIAN_POINT ( 'NONE',  ( -21.13435531349817964, 6.493721063603158150, -167.4999999999999716 ) ) ;
#201953 = ORIENTED_EDGE ( 'NONE', *, *, #124539, .F. ) ;
#201954 = CARTESIAN_POINT ( 'NONE',  ( 21.76363531954645936, 33.70142732455086332, -243.1915800643360512 ) ) ;
#201955 = EDGE_CURVE ( 'NONE', #182870, #190086, #160233, .T. ) ;
#201956 = EDGE_LOOP ( 'NONE', ( #129947, #148315, #214042, #183921 ) ) ;
#201957 = VERTEX_POINT ( 'NONE', #61098 ) ;
#201958 = CARTESIAN_POINT ( 'NONE',  ( 21.05000000000000071, 69.45934304831089889, -136.4231074845243654 ) ) ;
#201959 = DIRECTION ( 'NONE',  ( -1.000000000000000000, 0.000000000000000000, 0.000000000000000000 ) ) ;
#201960 = CARTESIAN_POINT ( 'NONE',  ( -16.85722902420167202, 66.05000000001153637, -48.78865495829463583 ) ) ;
#201961 = DIRECTION ( 'NONE',  ( 0.000000000000000000, -0.2128009952263604232, 0.9770955615653316162 ) ) ;
#201962 = CIRCLE ( 'NONE', #72803, 0.09999999999999939493 ) ;
#201963 = TOROIDAL_SURFACE ( 'NONE', #226888, 0.2000000000000000111, 0.1000000000000000056 ) ;
#201964 = CARTESIAN_POINT ( 'NONE',  ( -20.94999999999999929, 1.115600667400684642E-11, -196.8999999999999773 ) ) ;
#201965 = EDGE_LOOP ( 'NONE', ( #42464, #148906, #39590, #87793 ) ) ;
#201966 = ORIENTED_EDGE ( 'NONE', *, *, #174729, .F. ) ;
#201967 = CARTESIAN_POINT ( 'NONE',  ( 21.14999999999999858, 69.45934304831089889, -136.4231074845243654 ) ) ;
#201969 = EDGE_CURVE ( 'NONE', #101051, #251464, #136742, .T. ) ;
#201968 = EDGE_LOOP ( 'NONE', ( #219273, #168047, #47796, #64480 ) ) ;
#201970 = CARTESIAN_POINT ( 'NONE',  ( -16.93388492042258875, 22.95171134730065887, -230.8772219302610722 ) ) ;
#201971 = DIRECTION ( 'NONE',  ( -1.000000000000000000, 2.952720810173289112E-16, 2.061873921506763405E-30 ) ) ;
#201972 = DIRECTION ( 'NONE',  ( 1.000000000000000000, 0.000000000000000000, 0.000000000000000000 ) ) ;
#201973 = FACE_OUTER_BOUND ( 'NONE', #61708, .T. ) ;
#201974 = CARTESIAN_POINT ( 'NONE',  ( 21.07928932188134397, 0.09889514566555242248, -60.67148334360673800 ) ) ;
#201975 = DIRECTION ( 'NONE',  ( -1.000000000000000000, 0.000000000000000000, 0.000000000000000000 ) ) ;
#201976 = DIRECTION ( 'NONE',  ( -0.000000000000000000, 0.000000000000000000, 1.000000000000000000 ) ) ;
#201977 = CYLINDRICAL_SURFACE ( 'NONE', #204223, 0.09999999999999939493 ) ;
#201979 = EDGE_CURVE ( 'NONE', #81245, #172317, #11891, .T. ) ;
#201978 = CARTESIAN_POINT ( 'NONE',  ( -21.04999999999896687, 6.296993352176364134, -199.6465916771296349 ) ) ;
#201980 = CARTESIAN_POINT ( 'NONE',  ( 21.05000000000000071, 78.50726470275242264, -228.6618886302502176 ) ) ;
#201981 = AXIS2_PLACEMENT_3D ( 'NONE', #256286, #178129, #232969 ) ;
#201982 = DIRECTION ( 'NONE',  ( -0.000000000000000000, 1.000000000000000000, 6.982962677686266711E-15 ) ) ;
#201983 = AXIS2_PLACEMENT_3D ( 'NONE', #37911, #59995, #39198 ) ;
#201984 = VERTEX_POINT ( 'NONE', #105319 ) ;
#201985 = EDGE_CURVE ( 'NONE', #253683, #85377, #203950, .T. ) ;
#201986 = ORIENTED_EDGE ( 'NONE', *, *, #165004, .T. ) ;
#201987 = DIRECTION ( 'NONE',  ( 0.000000000000000000, 0.01283462868040226822, 0.9999176327611370985 ) ) ;
#201988 = CARTESIAN_POINT ( 'NONE',  ( -23.25000000000000000, -1.835859311432481045, -179.0044391687985410 ) ) ;
#201989 = CARTESIAN_POINT ( 'NONE',  ( 23.14999999999999858, 76.00000000001190870, -103.0231074845243029 ) ) ;
#201990 = ORIENTED_EDGE ( 'NONE', *, *, #55814, .F. ) ;
#201991 = FACE_OUTER_BOUND ( 'NONE', #38259, .T. ) ;
#201992 = CARTESIAN_POINT ( 'NONE',  ( -20.64999999999999858, 84.66355140188075268, -59.99900636645695329 ) ) ;
#201993 = CARTESIAN_POINT ( 'NONE',  ( -22.59999999999999787, 11.74956712350054744, -100.3991416309013260 ) ) ;
#201994 = EDGE_CURVE ( 'NONE', #136081, #84389, #28473, .T. ) ;
#201995 = DIRECTION ( 'NONE',  ( 1.000000000000000000, 0.000000000000000000, 0.000000000000000000 ) ) ;
#201996 = AXIS2_PLACEMENT_3D ( 'NONE', #22239, #61346, #237419 ) ;
#201997 = DIRECTION ( 'NONE',  ( 1.000000000000000000, 0.000000000000000000, 0.000000000000000000 ) ) ;
#201998 = FACE_OUTER_BOUND ( 'NONE', #15836, .T. ) ;
#201999 = CIRCLE ( 'NONE', #14772, 0.09999999999999939493 ) ;
#202000 = CIRCLE ( 'NONE', #218717, 2.099999999999990763 ) ;
#202001 = VERTEX_POINT ( 'NONE', #66241 ) ;
#202002 = DIRECTION ( 'NONE',  ( 1.073024830501117725E-15, 0.000000000000000000, 1.000000000000000000 ) ) ;
#202004 = ORIENTED_EDGE ( 'NONE', *, *, #40094, .T. ) ;
#202003 = DIRECTION ( 'NONE',  ( 0.000000000000000000, -0.2617529984165035128, -0.9651348961777155289 ) ) ;
#202005 = CARTESIAN_POINT ( 'NONE',  ( -20.64999999999999858, -8.999999999988846255, -76.89396912265249284 ) ) ;
#202006 = DIRECTION ( 'NONE',  ( 0.000000000000000000, 0.000000000000000000, -1.000000000000000000 ) ) ;
#202007 = DIRECTION ( 'NONE',  ( 0.000000000000000000, -1.000000000000000000, 0.000000000000000000 ) ) ;
#202008 = ORIENTED_EDGE ( 'NONE', *, *, #53661, .F. ) ;
#202009 = CARTESIAN_POINT ( 'NONE',  ( -21.05000000000000071, 18.18127959618848166, -237.5711165786817389 ) ) ;
#202010 = AXIS2_PLACEMENT_3D ( 'NONE', #124158, #120336, #121606 ) ;
#202011 = ITEM_DEFINED_TRANSFORMATION ( 'NONE', 'NONE', #81859,  #2425 ) ;
#202012 = TOROIDAL_SURFACE ( 'NONE', #43779, 0.2000000000000000111, 0.1000000000000000056 ) ;
#202013 = AXIS2_PLACEMENT_3D ( 'NONE', #212995, #248276, #228732 ) ;
#202014 = DIRECTION ( 'NONE',  ( 0.000000000000000000, 0.000000000000000000, -1.000000000000000000 ) ) ;
#202015 = ORIENTED_EDGE ( 'NONE', *, *, #246433, .F. ) ;
#202016 = DIRECTION ( 'NONE',  ( 1.000000000000000000, 0.000000000000000000, 0.000000000000000000 ) ) ;
#202017 = DIRECTION ( 'NONE',  ( 1.000000000000000000, 0.000000000000000000, 0.000000000000000000 ) ) ;
#202018 = AXIS2_PLACEMENT_3D ( 'NONE', #173009, #212101, #251192 ) ;
#202019 = CARTESIAN_POINT ( 'NONE',  ( 18.69999999999999929, 8.000000000000000000, -1.212568896937008089 ) ) ;
#202021 = VERTEX_POINT ( 'NONE', #145755 ) ;
#202020 = CIRCLE ( 'NONE', #214476, 0.09999999999999507894 ) ;
#202022 = ORIENTED_EDGE ( 'NONE', *, *, #152368, .F. ) ;
#202023 = DIRECTION ( 'NONE',  ( 2.952720810173290098E-16, -0.4721928772777354011, -0.8814952561688427224 ) ) ;
#202024 = AXIS2_PLACEMENT_3D ( 'NONE', #63268, #241903, #257565 ) ;
#202025 = CARTESIAN_POINT ( 'NONE',  ( -0.8999999999999986899, -12.25000000000000355, 26.00000000000000355 ) ) ;
#202026 = CIRCLE ( 'NONE', #251902, 0.09999999999999993616 ) ;
#202027 = FACE_OUTER_BOUND ( 'NONE', #202609, .T. ) ;
#202028 = CARTESIAN_POINT ( 'NONE',  ( -23.25000000000000000, 1.148907358139439339E-11, -201.0000000000015064 ) ) ;
#202029 = CARTESIAN_POINT ( 'NONE',  ( 23.15000000000000213, -12.41227409413852811, -197.8999999999999773 ) ) ;
#202030 = EDGE_CURVE ( 'NONE', #159227, #38202, #84463, .T. ) ;
#202031 = CARTESIAN_POINT ( 'NONE',  ( -23.25000000000000000, 64.25000000001170974, -69.52310748452438816 ) ) ;
#202033 = DIRECTION ( 'NONE',  ( 1.000000000000000000, 0.000000000000000000, 0.000000000000000000 ) ) ;
#202032 = DIRECTION ( 'NONE',  ( 0.000000000000000000, -0.8660254037844468122, -0.4999999999999859557 ) ) ;
#202034 = FACE_OUTER_BOUND ( 'NONE', #48525, .T. ) ;
#202035 = DIRECTION ( 'NONE',  ( 0.000000000000000000, 6.982962677686266711E-15, -1.000000000000000000 ) ) ;
#202036 = DIRECTION ( 'NONE',  ( 1.000000000000000000, -0.000000000000000000, -0.000000000000000000 ) ) ;
#202037 = DIRECTION ( 'NONE',  ( 0.000000000000000000, 1.000000000000000000, 0.000000000000000000 ) ) ;
#202038 = ORIENTED_EDGE ( 'NONE', *, *, #12906, .F. ) ;
#202039 = ORIENTED_EDGE ( 'NONE', *, *, #190179, .F. ) ;
#202040 = DIRECTION ( 'NONE',  ( 1.000000000000000000, 0.000000000000000000, 0.000000000000000000 ) ) ;
#202041 = CARTESIAN_POINT ( 'NONE',  ( 23.24999999999999645, -3.899999999988843502, -67.00000000000000000 ) ) ;
#202043 = CARTESIAN_POINT ( 'NONE',  ( -21.33487959338958362, 6.725558151911188887, -1.166372555419965823E-16 ) ) ;
#202042 = CARTESIAN_POINT ( 'NONE',  ( -21.04999999999999361, 69.69257478044653453, -103.0062876161386640 ) ) ;
#202044 = CARTESIAN_POINT ( 'NONE',  ( 18.59999999999999076, 69.60000000001187459, -93.09268285446279378 ) ) ;
#202046 = ADVANCED_FACE ( 'NONE', ( #85756 ), #187487, .T. ) ;
#202045 = DIRECTION ( 'NONE',  ( -1.000000000000000000, 0.000000000000000000, 0.000000000000000000 ) ) ;
#202047 = CARTESIAN_POINT ( 'NONE',  ( -20.64999999999999858, 76.00000000001143974, -38.02310748452432421 ) ) ;
#202048 = ORIENTED_EDGE ( 'NONE', *, *, #127259, .F. ) ;
#202049 = DIRECTION ( 'NONE',  ( 1.000000000000000000, 0.000000000000000000, 0.000000000000000000 ) ) ;
#202050 = ORIENTED_EDGE ( 'NONE', *, *, #17351, .F. ) ;
#202051 = EDGE_CURVE ( 'NONE', #60484, #10835, #95057, .T. ) ;
#202052 = AXIS2_PLACEMENT_3D ( 'NONE', #66098, #223870, #204312 ) ;
#202053 = CIRCLE ( 'NONE', #35672, 0.1000000000000124678 ) ;
#202054 = CARTESIAN_POINT ( 'NONE',  ( -14.56336952470180179, 9.446645344695243196, -18.41080645610019673 ) ) ;
#202055 = ORIENTED_EDGE ( 'NONE', *, *, #216471, .T. ) ;
#202056 = DIRECTION ( 'NONE',  ( 1.000000000000000000, 0.000000000000000000, 0.000000000000000000 ) ) ;
#202057 = CIRCLE ( 'NONE', #43833, 0.1000000000000000472 ) ;
#202058 = EDGE_CURVE ( 'NONE', #128967, #176136, #86850, .T. ) ;
#202059 = DIRECTION ( 'NONE',  ( -2.952720810173288619E-16, 1.000000000000000000, 0.000000000000000000 ) ) ;
#202060 = CIRCLE ( 'NONE', #131310, 11.65000000000000036 ) ;
#202061 = ADVANCED_FACE ( 'NONE', ( #81908 ), #107927, .F. ) ;
#202062 = EDGE_CURVE ( 'NONE', #147074, #142179, #161738, .T. ) ;
#202063 = ORIENTED_EDGE ( 'NONE', *, *, #180388, .T. ) ;
#202064 = CARTESIAN_POINT ( 'NONE',  ( -16.87242674293850087, 66.05000000001263061, -190.8741977308967819 ) ) ;
#202065 = ORIENTED_EDGE ( 'NONE', *, *, #94052, .T. ) ;
#202066 = EDGE_CURVE ( 'NONE', #199040, #248456, #15988, .T. ) ;
#202068 = TOROIDAL_SURFACE ( 'NONE', #35509, 0.2000000000000000111, 0.1000000000000000056 ) ;
#202067 = FACE_OUTER_BOUND ( 'NONE', #129146, .T. ) ;
#202069 = LINE ( 'NONE', #200778, #253225 ) ;
#202070 = DIRECTION ( 'NONE',  ( 1.000000000000000000, 0.000000000000000000, 0.000000000000000000 ) ) ;
#202071 = FACE_OUTER_BOUND ( 'NONE', #102455, .T. ) ;
#202073 = DIRECTION ( 'NONE',  ( 0.000000000000000000, 0.000000000000000000, -1.000000000000000000 ) ) ;
#202072 = CARTESIAN_POINT ( 'NONE',  ( 21.72449340488910252, 65.71604372252119219, -160.7731074845244166 ) ) ;
#202074 = EDGE_CURVE ( 'NONE', #214650, #50827, #102767, .T. ) ;
#202075 = AXIS2_PLACEMENT_3D ( 'NONE', #151005, #92297, #231833 ) ;
#202076 = CARTESIAN_POINT ( 'NONE',  ( 20.94999999999999929, 70.50000000001260503, -191.1178414656113205 ) ) ;
#202078 = ORIENTED_EDGE ( 'NONE', *, *, #1009, .F. ) ;
#202077 = CARTESIAN_POINT ( 'NONE',  ( 21.09696443733127325, 65.27599011609412116, -191.2883299574762077 ) ) ;
#202080 = LINE ( 'NONE', #61280, #68595 ) ;
#202079 = CARTESIAN_POINT ( 'NONE',  ( -18.59999999999999787, 38.30077178631846380, -261.1858881914067751 ) ) ;
#202081 = EDGE_LOOP ( 'NONE', ( #188761, #108053, #158166 ) ) ;
#202083 = ORIENTED_EDGE ( 'NONE', *, *, #120878, .F. ) ;
#202082 = DIRECTION ( 'NONE',  ( 0.000000000000000000, 0.000000000000000000, 1.000000000000000000 ) ) ;
#202084 = EDGE_LOOP ( 'NONE', ( #186689, #141440, #17033, #72684 ) ) ;
#202085 = CARTESIAN_POINT ( 'NONE',  ( 18.60000000000001208, 85.36423601037837727, -62.34285308379966040 ) ) ;
#202086 = DIRECTION ( 'NONE',  ( 0.000000000000000000, -0.1350103645451876666, 0.9908441862701600211 ) ) ;
#202087 = DIRECTION ( 'NONE',  ( 1.000000000000000000, -3.265361837132813093E-16, -2.280189983783949500E-30 ) ) ;
#202088 = ORIENTED_EDGE ( 'NONE', *, *, #39884, .T. ) ;
#202089 = DIRECTION ( 'NONE',  ( -0.000000000000000000, 1.000000000000000000, 6.982962677686266711E-15 ) ) ;
#202090 = CARTESIAN_POINT ( 'NONE',  ( -20.94999999999999929, 77.83534155023670564, -158.3679561919613548 ) ) ;
#202092 = CARTESIAN_POINT ( 'NONE',  ( 18.42636655943170965, 38.00040813105046311, -261.0434348347492914 ) ) ;
#202091 = AXIS2_PLACEMENT_3D ( 'NONE', #113955, #149262, #94392 ) ;
#202093 = DIRECTION ( 'NONE',  ( 0.000000000000000000, 0.000000000000000000, 1.000000000000000000 ) ) ;
#202095 = EDGE_CURVE ( 'NONE', #159233, #180230, #157648, .T. ) ;
#202094 = CARTESIAN_POINT ( 'NONE',  ( -18.55807992284872299, 46.45729338110134421, -243.0823073233429170 ) ) ;
#202096 = DIRECTION ( 'NONE',  ( 0.000000000000000000, 7.993605777301153912E-15, 1.000000000000000000 ) ) ;
#202097 = ORIENTED_EDGE ( 'NONE', *, *, #198970, .F. ) ;
#202098 = ORIENTED_EDGE ( 'NONE', *, *, #255835, .F. ) ;
#202099 = DIRECTION ( 'NONE',  ( 0.000000000000000000, 0.000000000000000000, 1.000000000000000000 ) ) ;
#202100 = VECTOR ( 'NONE', #78414, 1000.000000000000000 ) ;
#202101 = EDGE_LOOP ( 'NONE', ( #147741, #243791, #217076, #242720 ) ) ;
#202102 = AXIS2_PLACEMENT_3D ( 'NONE', #41085, #65759, #26657 ) ;
#202103 = LINE ( 'NONE', #102976, #71775 ) ;
#202104 = ORIENTED_EDGE ( 'NONE', *, *, #200069, .T. ) ;
#202105 = CARTESIAN_POINT ( 'NONE',  ( -20.85000000000000142, 7.021664781911246322, -137.8335654018973457 ) ) ;
#202106 = EDGE_CURVE ( 'NONE', #118795, #70529, #228353, .T. ) ;
#202107 = CARTESIAN_POINT ( 'NONE',  ( -20.54999999999999716, 54.34471204062663219, -239.4366250215122420 ) ) ;
#202108 = DIRECTION ( 'NONE',  ( 0.000000000000000000, 0.9908441862701596881, -0.1350103645451904977 ) ) ;
#202109 = CARTESIAN_POINT ( 'NONE',  ( -21.08035267497491816, 30.84675532226686911, -252.0643358494183985 ) ) ;
#202110 = DIRECTION ( 'NONE',  ( 0.000000000000000000, 0.000000000000000000, -1.000000000000000000 ) ) ;
#202111 = VERTEX_POINT ( 'NONE', #3687 ) ;
#202112 = DIRECTION ( 'NONE',  ( 0.5000000000001139089, 0.7633972851576313889, -0.4089310272085548981 ) ) ;
#202113 = CARTESIAN_POINT ( 'NONE',  ( -16.86733706339143879, 66.03400947037287949, -182.6199921825257206 ) ) ;
#202114 = CARTESIAN_POINT ( 'NONE',  ( -21.07971444708686093, 0.08782343632898161057, -27.17020791837345328 ) ) ;
#202115 = LINE ( 'NONE', #121332, #210080 ) ;
#202116 = ORIENTED_EDGE ( 'NONE', *, *, #252883, .F. ) ;
#202117 = TOROIDAL_SURFACE ( 'NONE', #147947, 0.4000000000000012990, 0.1000000000000000056 ) ;
#202119 = CARTESIAN_POINT ( 'NONE',  ( 20.85000000000000142, 77.83585931145526615, -58.01866831572577610 ) ) ;
#202118 = CARTESIAN_POINT ( 'NONE',  ( 20.94999999999999574, 1.162701749938009677, -8.099999999999999645 ) ) ;
#202120 = EDGE_LOOP ( 'NONE', ( #221580, #245168, #85975, #151514 ) ) ;
#202123 = EDGE_LOOP ( 'NONE', ( #72957, #114959, #209930, #251605 ) ) ;
#202122 = FILL_AREA_STYLE ('',( #200840 ) ) ;
#202121 = DIRECTION ( 'NONE',  ( 0.000000000000000000, 1.000000000000000000, -1.156482317317873105E-15 ) ) ;
#202124 = EDGE_CURVE ( 'NONE', #201531, #81754, #115919, .T. ) ;
#202125 = EDGE_LOOP ( 'NONE', ( #191465, #21005, #210968, #188427 ) ) ;
#202126 = DIRECTION ( 'NONE',  ( -1.000000000000000000, 0.000000000000000000, 0.000000000000000000 ) ) ;
#202127 = CYLINDRICAL_SURFACE ( 'NONE', #224910, 0.9000000000000014655 ) ;
#202128 = VECTOR ( 'NONE', #115765, 1000.000000000000000 ) ;
#202129 = EDGE_LOOP ( 'NONE', ( #168721, #125524, #157274, #233195 ) ) ;
#202130 = CARTESIAN_POINT ( 'NONE',  ( 19.87657994472051115, 16.75105720888964100, -222.6981299613315741 ) ) ;
#202132 = EDGE_CURVE ( 'NONE', #143544, #188149, #162787, .T. ) ;
#202131 = CARTESIAN_POINT ( 'NONE',  ( -21.44999999999999929, 68.65000000001150227, -48.27310748452437394 ) ) ;
#202133 = CARTESIAN_POINT ( 'NONE',  ( -14.00000000000000178, 66.15000000001258229, -186.7731074845244166 ) ) ;
#202135 = ORIENTED_EDGE ( 'NONE', *, *, #24050, .T. ) ;
#202134 = DIRECTION ( 'NONE',  ( -0.000000000000000000, -0.000000000000000000, 1.000000000000000000 ) ) ;
#202136 = EDGE_CURVE ( 'NONE', #187820, #120408, #79599, .T. ) ;
#202137 = ADVANCED_FACE ( 'NONE', ( #203173 ), #104051, .T. ) ;
#202138 = EDGE_LOOP ( 'NONE', ( #253535, #170240, #54951, #119795 ) ) ;
#202139 = CARTESIAN_POINT ( 'NONE',  ( -18.59999999999999787, -1.637172712959223952, -112.0821533654720383 ) ) ;
#202140 = DIRECTION ( 'NONE',  ( -1.000000000000000000, -0.000000000000000000, -0.000000000000000000 ) ) ;
#202141 = STYLED_ITEM ( 'NONE', ( #209229 ), #104549 ) ;
#202142 = AXIS2_PLACEMENT_3D ( 'NONE', #39087, #242389, #200709 ) ;
#202143 = DIRECTION ( 'NONE',  ( 1.000000000000000000, -0.000000000000000000, -0.000000000000000000 ) ) ;
#202144 = ORIENTED_EDGE ( 'NONE', *, *, #89929, .F. ) ;
#202145 = CARTESIAN_POINT ( 'NONE',  ( 20.94999999999999574, 62.00000000001233502, -164.5960149541419071 ) ) ;
#202146 = VERTEX_POINT ( 'NONE', #247432 ) ;
#202147 = ADVANCED_FACE ( 'NONE', ( #12708 ), #252557, .F. ) ;
#202148 = FACE_OUTER_BOUND ( 'NONE', #84167, .T. ) ;
#202149 = DIRECTION ( 'NONE',  ( 1.000000000000000000, -7.304098846218133681E-16, -4.639676173203992654E-30 ) ) ;
#202150 = CARTESIAN_POINT ( 'NONE',  ( 21.93340585971920476, 7.324147022865875378, -33.50000000000000711 ) ) ;
#202151 = ORIENTED_EDGE ( 'NONE', *, *, #239956, .F. ) ;
#202152 = CARTESIAN_POINT ( 'NONE',  ( -18.59999999999999787, 7.021664781911246322, -171.3335654018973173 ) ) ;
#202153 = CIRCLE ( 'NONE', #77233, 0.09999999999999543976 ) ;
#202154 = LINE ( 'NONE', #166915, #56468 ) ;
#202155 = CIRCLE ( 'NONE', #39858, 0.9000000000000014655 ) ;
#202156 = VECTOR ( 'NONE', #25279, 1000.000000000000000 ) ;
#202157 = AXIS2_PLACEMENT_3D ( 'NONE', #5223, #125211, #87339 ) ;
#202158 = ADVANCED_FACE ( 'NONE', ( #248729 ), #257209, .F. ) ;
#202159 = ORIENTED_EDGE ( 'NONE', *, *, #187873, .T. ) ;
#202160 = VERTEX_POINT ( 'NONE', #72682 ) ;
#202161 = EDGE_LOOP ( 'NONE', ( #30234, #218867, #133230, #54683 ) ) ;
#202162 = DIRECTION ( 'NONE',  ( 1.000000000000000000, 0.000000000000000000, 0.000000000000000000 ) ) ;
#202163 = VERTEX_POINT ( 'NONE', #210879 ) ;
#202165 = EDGE_LOOP ( 'NONE', ( #58242, #257447, #84440, #210326 ) ) ;
#202164 = CARTESIAN_POINT ( 'NONE',  ( 14.22916352759893677, 66.54258906972242471, -185.0231915757782133 ) ) ;
#202166 = EDGE_CURVE ( 'NONE', #99532, #89234, #152222, .T. ) ;
#202167 = EDGE_CURVE ( 'NONE', #72339, #116858, #240820, .T. ) ;
#202168 = ORIENTED_EDGE ( 'NONE', *, *, #239089, .F. ) ;
#202171 = ORIENTED_EDGE ( 'NONE', *, *, #213281, .T. ) ;
#202170 = ORIENTED_EDGE ( 'NONE', *, *, #119206, .T. ) ;
#202169 = CARTESIAN_POINT ( 'NONE',  ( -16.77732147278574715, 9.945966932584587639, -113.1635087568758422 ) ) ;
#202172 = ORIENTED_EDGE ( 'NONE', *, *, #227821, .F. ) ;
#202173 = DIRECTION ( 'NONE',  ( -1.000000000000000000, -0.000000000000000000, -0.000000000000000000 ) ) ;
#202174 = AXIS2_PLACEMENT_3D ( 'NONE', #114595, #214971, #54608 ) ;
#202175 = CARTESIAN_POINT ( 'NONE',  ( 18.59999999999999076, 6.650000000011155876, -54.65000000000000568 ) ) ;
#202176 = CARTESIAN_POINT ( 'NONE',  ( -18.59999999999999787, 86.96699927712943179, -199.3055931863049466 ) ) ;
#202177 = AXIS2_PLACEMENT_3D ( 'NONE', #117127, #58396, #79250 ) ;
#202178 = ORIENTED_EDGE ( 'NONE', *, *, #94311, .T. ) ;
#202179 = DIRECTION ( 'NONE',  ( 1.000000000000000000, -0.000000000000000000, -0.000000000000000000 ) ) ;
#202181 = ORIENTED_EDGE ( 'NONE', *, *, #78112, .T. ) ;
#202180 = CYLINDRICAL_SURFACE ( 'NONE', #95078, 0.5000000000000004441 ) ;
#202183 = CARTESIAN_POINT ( 'NONE',  ( -16.86420534634261514, 14.19368693413156635, -219.3174569077499996 ) ) ;
#202182 = AXIS2_PLACEMENT_3D ( 'NONE', #108423, #150134, #187963 ) ;
#202185 = VERTEX_POINT ( 'NONE', #110489 ) ;
#202184 = CARTESIAN_POINT ( 'NONE',  ( 18.59999999999999076, 78.57744179526842743, -232.8011145694030972 ) ) ;
#202186 = ORIENTED_EDGE ( 'NONE', *, *, #190454, .F. ) ;
#202187 = AXIS2_PLACEMENT_3D ( 'NONE', #148537, #186387, #85952 ) ;
#202188 = AXIS2_PLACEMENT_3D ( 'NONE', #157890, #219081, #78288 ) ;
#202189 = CIRCLE ( 'NONE', #98101, 0.1000000000000075273 ) ;
#202191 = EDGE_CURVE ( 'NONE', #212047, #101749, #170125, .T. ) ;
#202190 = DIRECTION ( 'NONE',  ( 0.7071067811865127117, 0.7071067811865821007, 0.000000000000000000 ) ) ;
#202192 = EDGE_LOOP ( 'NONE', ( #105038, #40752, #244379, #14439 ) ) ;
#202193 = ORIENTED_EDGE ( 'NONE', *, *, #71042, .T. ) ;
#202194 = CARTESIAN_POINT ( 'NONE',  ( 23.14999999999999147, 71.85000000001214460, -136.5231074845243029 ) ) ;
#202196 = EDGE_CURVE ( 'NONE', #230675, #112967, #256922, .T. ) ;
#202195 = CARTESIAN_POINT ( 'NONE',  ( 20.94999999999999574, 69.45000000001230944, -160.1792853948412869 ) ) ;
#202199 = ORIENTED_EDGE ( 'NONE', *, *, #97858, .T. ) ;
#202198 = ORIENTED_EDGE ( 'NONE', *, *, #238765, .T. ) ;
#202197 = CIRCLE ( 'NONE', #89753, 1.899999999999993028 ) ;
#202200 = EDGE_LOOP ( 'NONE', ( #250791, #67388, #39292, #146665, #209004 ) ) ;
#202201 = DIRECTION ( 'NONE',  ( -1.000000000000000000, 0.000000000000000000, 0.000000000000000000 ) ) ;
#202202 = ORIENTED_EDGE ( 'NONE', *, *, #95562, .F. ) ;
#202203 = VECTOR ( 'NONE', #96926, 1000.000000000000000 ) ;
#202204 = VERTEX_POINT ( 'NONE', #167936 ) ;
#202205 = CARTESIAN_POINT ( 'NONE',  ( -18.39999999999999858, 85.50000000001189449, -95.99103808782457747 ) ) ;
#202208 = ADVANCED_FACE ( 'NONE', ( #90924 ), #70116, .T. ) ;
#202207 = ORIENTED_EDGE ( 'NONE', *, *, #188319, .T. ) ;
#202206 = CARTESIAN_POINT ( 'NONE',  ( 18.59999999999999787, -1.851028230129704522, -179.1539132694224463 ) ) ;
#202209 = CYLINDRICAL_SURFACE ( 'NONE', #139979, 4.000000000000003553 ) ;
#202210 = VECTOR ( 'NONE', #158773, 1000.000000000000000 ) ;
#202211 = AXIS2_PLACEMENT_3D ( 'NONE', #221015, #99770, #179356 ) ;
#202213 = FACE_OUTER_BOUND ( 'NONE', #89411, .T. ) ;
#202212 = CYLINDRICAL_SURFACE ( 'NONE', #65526, 0.1000000000000028644 ) ;
#202214 = ORIENTED_EDGE ( 'NONE', *, *, #114369, .F. ) ;
#202215 = EDGE_CURVE ( 'NONE', #40998, #68348, #113066, .T. ) ;
#202217 = ORIENTED_EDGE ( 'NONE', *, *, #135235, .T. ) ;
#202216 = ORIENTED_EDGE ( 'NONE', *, *, #93877, .T. ) ;
#202218 = LINE ( 'NONE', #103087, #241083 ) ;
#202219 = ADVANCED_FACE ( 'NONE', ( #227877 ), #89634, .F. ) ;
#202220 = ORIENTED_EDGE ( 'NONE', *, *, #43001, .T. ) ;
#202221 = EDGE_CURVE ( 'NONE', #131644, #223333, #195037, .T. ) ;
#202222 = CYLINDRICAL_SURFACE ( 'NONE', #180493, 11.79999999999999716 ) ;
#202223 = EDGE_CURVE ( 'NONE', #237745, #105777, #109195, .T. ) ;
#202224 = ORIENTED_EDGE ( 'NONE', *, *, #69077, .T. ) ;
#202225 = ORIENTED_EDGE ( 'NONE', *, *, #92766, .T. ) ;
#202226 = DIRECTION ( 'NONE',  ( 0.000000000000000000, 0.5000000000000209832, 0.8660254037844264952 ) ) ;
#202227 = ORIENTED_EDGE ( 'NONE', *, *, #257468, .T. ) ;
#202228 = LINE ( 'NONE', #46978, #176408 ) ;
#202229 = CARTESIAN_POINT ( 'NONE',  ( 21.05000000000000426, 75.93429838968991419, -109.2814235418563555 ) ) ;
#202230 = ORIENTED_EDGE ( 'NONE', *, *, #115796, .T. ) ;
#202231 = CARTESIAN_POINT ( 'NONE',  ( 20.94999999999999929, 71.00000000001253397, -182.4283735034374843 ) ) ;
#202232 = FACE_OUTER_BOUND ( 'NONE', #83690, .T. ) ;
#202234 = CARTESIAN_POINT ( 'NONE',  ( 22.39999999999999858, 75.90000000001273861, -211.3138870828977360 ) ) ;
#202233 = CARTESIAN_POINT ( 'NONE',  ( 18.59999999999998721, 14.61354176542825201, -235.9279552357344016 ) ) ;
#202235 = CARTESIAN_POINT ( 'NONE',  ( 21.00000000000000000, -11.65000000000000036, 11.89999999999999680 ) ) ;
#202236 = AXIS2_PLACEMENT_3D ( 'NONE', #45911, #88865, #204963 ) ;
#202237 = DIRECTION ( 'NONE',  ( 0.000000000000000000, 0.000000000000000000, 1.000000000000000000 ) ) ;
#202238 = CIRCLE ( 'NONE', #148237, 0.1000000000000000472 ) ;
#202239 = DIRECTION ( 'NONE',  ( 0.000000000000000000, -1.000000000000000000, -6.860497997771531562E-15 ) ) ;
#202240 = DIRECTION ( 'NONE',  ( 1.000000000000000000, -0.000000000000000000, -0.000000000000000000 ) ) ;
#202241 = CIRCLE ( 'NONE', #48106, 0.1000000000000055844 ) ;
#202242 = VERTEX_POINT ( 'NONE', #188743 ) ;
#202243 = ADVANCED_FACE ( 'NONE', ( #93491 ), #40932, .T. ) ;
#202244 = EDGE_CURVE ( 'NONE', #257983, #196680, #255079, .T. ) ;
#202245 = AXIS2_PLACEMENT_3D ( 'NONE', #242552, #67774, #44377 ) ;
#202247 = ORIENTED_EDGE ( 'NONE', *, *, #92069, .T. ) ;
#202246 = EDGE_LOOP ( 'NONE', ( #204335, #37824, #12746 ) ) ;
#202248 = ORIENTED_EDGE ( 'NONE', *, *, #179673, .F. ) ;
#202249 = EDGE_CURVE ( 'NONE', #21932, #15038, #78479, .T. ) ;
#202250 = DIRECTION ( 'NONE',  ( 0.000000000000000000, -6.982962677686266711E-15, 1.000000000000000000 ) ) ;
#202251 = CARTESIAN_POINT ( 'NONE',  ( -16.87304349924914604, 66.03825492205463377, -82.13404080947913144 ) ) ;
#202253 = CARTESIAN_POINT ( 'NONE',  ( -15.52965525596987639, 9.375538102048002642, -15.86987588099083446 ) ) ;
#202252 = DIRECTION ( 'NONE',  ( 0.000000000000000000, 0.9908441862701596881, -0.1350103645451904977 ) ) ;
#202254 = CARTESIAN_POINT ( 'NONE',  ( 21.05000000000000071, 67.22371735104120205, -161.5355151060043113 ) ) ;
#202256 = ORIENTED_EDGE ( 'NONE', *, *, #40961, .F. ) ;
#202255 = AXIS2_PLACEMENT_3D ( 'NONE', #243313, #158688, #103786 ) ;
#202257 = DIRECTION ( 'NONE',  ( 0.000000000000000000, -1.000000000000000000, 0.000000000000000000 ) ) ;
#202258 = EDGE_CURVE ( 'NONE', #121293, #73463, #66024, .T. ) ;
#202259 = PLANE ( 'NONE',  #170988 ) ;
#202260 = TOROIDAL_SURFACE ( 'NONE', #31421, 0.2000000000000000111, 0.1000000000000000056 ) ;
#202261 = DIRECTION ( 'NONE',  ( -0.000000000000000000, 0.1298341882519953583, 0.9915357197604862671 ) ) ;
#202262 = EDGE_CURVE ( 'NONE', #195967, #251749, #111826, .T. ) ;
#202263 = CARTESIAN_POINT ( 'NONE',  ( -16.94389599337535657, 9.991197989767881538, -87.89235519820165621 ) ) ;
#202264 = ORIENTED_EDGE ( 'NONE', *, *, #76755, .T. ) ;
#202265 = CARTESIAN_POINT ( 'NONE',  ( -20.00857864376270001, 9.150000000011157653, -188.6499999999999488 ) ) ;
#202266 = CYLINDRICAL_SURFACE ( 'NONE', #184457, 0.1000000000000028644 ) ;
#202267 = ORIENTED_EDGE ( 'NONE', *, *, #99980, .T. ) ;
#202268 = DIRECTION ( 'NONE',  ( -0.000000000000000000, -0.000000000000000000, 1.000000000000000000 ) ) ;
#202269 = AXIS2_PLACEMENT_3D ( 'NONE', #117813, #104328, #183889 ) ;
#202270 = DIRECTION ( 'NONE',  ( 0.000000000000000000, 1.000000000000000000, 0.000000000000000000 ) ) ;
#202271 = EDGE_CURVE ( 'NONE', #233837, #166393, #92082, .T. ) ;
#202272 = DIRECTION ( 'NONE',  ( -0.000000000000000000, 0.2617529984165031243, 0.9651348961777157509 ) ) ;
#202273 = FACE_OUTER_BOUND ( 'NONE', #98199, .T. ) ;
#202274 = DIRECTION ( 'NONE',  ( -1.000000000000000000, -0.000000000000000000, 0.000000000000000000 ) ) ;
#202275 = ORIENTED_EDGE ( 'NONE', *, *, #239528, .F. ) ;
#202276 = DIRECTION ( 'NONE',  ( 0.5735764363510460484, 0.8191520442889919096, -0.000000000000000000 ) ) ;
#202277 = DIRECTION ( 'NONE',  ( 0.000000000000000000, -0.8660254037844420383, 0.4999999999999943379 ) ) ;
#202278 = CARTESIAN_POINT ( 'NONE',  ( 20.95262331984781667, 11.87253000080046306, -206.1524153088024320 ) ) ;
#202279 = B_SPLINE_CURVE_WITH_KNOTS ( 'NONE', 3,
 ( #67539, #87084, #66266, #62417 ),
 .UNSPECIFIED., .F., .F.,
 ( 4, 4 ),
 ( 0.000000000000000000, 0.0001048066582182451801 ),
 .UNSPECIFIED. ) ;
#202281 = CARTESIAN_POINT ( 'NONE',  ( 23.14999999999999858, 1.115625160336667635E-11, -198.9999999999999432 ) ) ;
#202280 = CARTESIAN_POINT ( 'NONE',  ( -20.64999999999999858, 68.85000000001200249, -115.3731074845243540 ) ) ;
#202282 = DIRECTION ( 'NONE',  ( 0.000000000000000000, 0.000000000000000000, 1.000000000000000000 ) ) ;
#202284 = EDGE_CURVE ( 'NONE', #18158, #65394, #199018, .T. ) ;
#202283 = CARTESIAN_POINT ( 'NONE',  ( -21.14999999999999858, 1.115600667400684642E-11, -127.7414213562373106 ) ) ;
#202285 = CARTESIAN_POINT ( 'NONE',  ( 20.94999999999999929, 6.450000000011156587, -177.5170271704400022 ) ) ;
#202286 = DIRECTION ( 'NONE',  ( 0.000000000000000000, 0.000000000000000000, -1.000000000000000000 ) ) ;
#202287 = AXIS2_PLACEMENT_3D ( 'NONE', #125647, #6981, #86490 ) ;
#202290 = ORIENTED_EDGE ( 'NONE', *, *, #42357, .F. ) ;
#202289 = CIRCLE ( 'NONE', #206376, 0.09999999999998898659 ) ;
#202288 = CARTESIAN_POINT ( 'NONE',  ( -1.820710678118658388, 85.92928932189330737, -111.8731074845242262 ) ) ;
#202291 = VECTOR ( 'NONE', #95589, 1000.000000000000000 ) ;
#202292 = AXIS2_PLACEMENT_3D ( 'NONE', #77840, #213505, #235632 ) ;
#202293 = ORIENTED_EDGE ( 'NONE', *, *, #132824, .F. ) ;
#202294 = ADVANCED_FACE ( 'NONE', ( #98584 ), #99316, .F. ) ;
#202295 = FACE_OUTER_BOUND ( 'NONE', #82870, .T. ) ;
#202296 = CARTESIAN_POINT ( 'NONE',  ( -18.50000972452446035, 65.70673848566926267, -30.56382523348289837 ) ) ;
#202297 = LINE ( 'NONE', #104447, #233579 ) ;
#202298 = AXIS2_PLACEMENT_3D ( 'NONE', #181724, #141307, #123037 ) ;
#202299 = ORIENTED_EDGE ( 'NONE', *, *, #136424, .F. ) ;
#202300 = FACE_OUTER_BOUND ( 'NONE', #72389, .T. ) ;
#202301 = DIRECTION ( 'NONE',  ( 1.000000000000000000, 0.000000000000000000, 0.000000000000000000 ) ) ;
#202302 = CARTESIAN_POINT ( 'NONE',  ( -21.05000000000000071, 11.59999999999999964, -26.57179676972449656 ) ) ;
#202303 = CIRCLE ( 'NONE', #89865, 0.1000000000000024342 ) ;
#202304 = ORIENTED_EDGE ( 'NONE', *, *, #35265, .F. ) ;
#202305 = DIRECTION ( 'NONE',  ( 1.000000000000000000, -0.000000000000000000, -0.000000000000000000 ) ) ;
#202307 = ORIENTED_EDGE ( 'NONE', *, *, #228617, .F. ) ;
#202306 = LINE ( 'NONE', #67926, #230017 ) ;
#202309 = CARTESIAN_POINT ( 'NONE',  ( 23.24999999999999645, 8.822561741666397950, -12.65000000000000746 ) ) ;
#202308 = DIRECTION ( 'NONE',  ( -1.000000000000000000, 0.000000000000000000, 0.000000000000000000 ) ) ;
#202310 = CARTESIAN_POINT ( 'NONE',  ( -21.05000000000000071, -0.09999999998884338825, -21.85042919245520210 ) ) ;
#202311 = ORIENTED_EDGE ( 'NONE', *, *, #166969, .T. ) ;
#202312 = PLANE ( 'NONE',  #254232 ) ;
#202313 = CARTESIAN_POINT ( 'NONE',  ( 21.05000000000000071, 67.12791932463434819, -128.0020600656931720 ) ) ;
#202314 = ORIENTED_EDGE ( 'NONE', *, *, #20749, .F. ) ;
#202315 = DIRECTION ( 'NONE',  ( -0.000000000000000000, 0.1350103645451876666, 0.9908441862701600211 ) ) ;
#202316 = TOROIDAL_SURFACE ( 'NONE', #144037, 7.800000000000000711, 0.1000000000000000056 ) ;
#202317 = CARTESIAN_POINT ( 'NONE',  ( 18.49999999999999289, 55.08862955830016261, -229.9605662146666134 ) ) ;
#202318 = DIRECTION ( 'NONE',  ( -0.000000000000000000, 0.9126074666063770380, 0.4088369013363281068 ) ) ;
#202319 = CARTESIAN_POINT ( 'NONE',  ( -22.49917693094574389, 0.08522996423282774847, -122.3502042154693612 ) ) ;
#202320 = ORIENTED_EDGE ( 'NONE', *, *, #243962, .F. ) ;
#202321 = VERTEX_POINT ( 'NONE', #238127 ) ;
#202322 = CARTESIAN_POINT ( 'NONE',  ( -18.59999999999999787, 11.65000000001115232, -188.8499999999999659 ) ) ;
#202323 = CARTESIAN_POINT ( 'NONE',  ( 20.85000000000000142, 1.115600667400684642E-11, -175.3000000000000398 ) ) ;
#202324 = DIRECTION ( 'NONE',  ( 1.000000000000000000, 0.000000000000000000, 0.000000000000000000 ) ) ;
#202325 = CARTESIAN_POINT ( 'NONE',  ( 21.04999999999999716, 10.50253167713776392, -141.5588298170757184 ) ) ;
#202326 = DIRECTION ( 'NONE',  ( 1.000000000000000000, 0.000000000000000000, 0.000000000000000000 ) ) ;
#202327 = EDGE_CURVE ( 'NONE', #83582, #26573, #166016, .T. ) ;
#202330 = CARTESIAN_POINT ( 'NONE',  ( -23.15000000000000213, 4.350000000011156054, -88.35000000000003695 ) ) ;
#202329 = VECTOR ( 'NONE', #29548, 1000.000000000000000 ) ;
#202328 = FACE_OUTER_BOUND ( 'NONE', #53890, .T. ) ;
#202331 = CARTESIAN_POINT ( 'NONE',  ( 0.9000000000000554223, 63.75000000001118394, -10.02310748452479139 ) ) ;
#202332 = CIRCLE ( 'NONE', #119137, 0.09999999999999939493 ) ;
#202333 = CARTESIAN_POINT ( 'NONE',  ( -16.83794237512074332, 66.07364077890409249, -56.71956532582543531 ) ) ;
#202334 = CARTESIAN_POINT ( 'NONE',  ( 18.50000000000000000, -9.399999999988843058, -107.3820418481727188 ) ) ;
#202336 = ORIENTED_EDGE ( 'NONE', *, *, #168690, .T. ) ;
#202335 = AXIS2_PLACEMENT_3D ( 'NONE', #74066, #12803, #253936 ) ;
#202337 = CARTESIAN_POINT ( 'NONE',  ( -23.15000000000000213, -13.98128454229089357, -192.0195388455185821 ) ) ;
#202338 = AXIS2_PLACEMENT_3D ( 'NONE', #152185, #50456, #171751 ) ;
#202340 = ORIENTED_EDGE ( 'NONE', *, *, #69720, .F. ) ;
#202339 = FACE_OUTER_BOUND ( 'NONE', #129327, .T. ) ;
#202341 = LINE ( 'NONE', #103218, #51851 ) ;
#202342 = CARTESIAN_POINT ( 'NONE',  ( -20.54999999999999716, 1.115600667400684642E-11, -67.00000000000000000 ) ) ;
#202344 = DIRECTION ( 'NONE',  ( 1.000000000000000000, 0.000000000000000000, 0.000000000000000000 ) ) ;
#202343 = CARTESIAN_POINT ( 'NONE',  ( 21.53752568622137886, 75.90102553874137925, -109.8099153590728605 ) ) ;
#202345 = MECHANICAL_DESIGN_GEOMETRIC_PRESENTATION_REPRESENTATION (  '', ( #23306 ), #231570 ) ;
#202346 = ORIENTED_EDGE ( 'NONE', *, *, #176747, .T. ) ;
#202348 = CARTESIAN_POINT ( 'NONE',  ( 23.14999999999998437, 67.23127455305841238, -235.8551265064783991 ) ) ;
#202347 = CARTESIAN_POINT ( 'NONE',  ( -20.64999999999999858, 4.350000000011156054, -79.25000000000004263 ) ) ;
#202349 = CARTESIAN_POINT ( 'NONE',  ( 18.49999999999999289, 64.35000000001214460, -136.5231074845244166 ) ) ;
#202350 = CARTESIAN_POINT ( 'NONE',  ( 21.05000000000000071, 5.000000000011153745, -188.5947339810868755 ) ) ;
#202351 = DIRECTION ( 'NONE',  ( 0.000000000000000000, 0.000000000000000000, -1.000000000000000000 ) ) ;
#202352 = CARTESIAN_POINT ( 'NONE',  ( -14.87770893841225650, 66.56936289831583053, -185.2548468664635379 ) ) ;
#202353 = ORIENTED_EDGE ( 'NONE', *, *, #219772, .F. ) ;
#202355 = EDGE_CURVE ( 'NONE', #45873, #84436, #199309, .T. ) ;
#202354 = ORIENTED_EDGE ( 'NONE', *, *, #236028, .F. ) ;
#202356 = CARTESIAN_POINT ( 'NONE',  ( -23.25000000000000000, -9.599999999999997868, -23.60603087734755690 ) ) ;
#202357 = ORIENTED_EDGE ( 'NONE', *, *, #194171, .F. ) ;
#202358 = CARTESIAN_POINT ( 'NONE',  ( -20.64999999999999858, -3.770473190032741062, -225.9805569534692324 ) ) ;
#202359 = CIRCLE ( 'NONE', #139802, 0.09999999999999939493 ) ;
#202360 = ORIENTED_EDGE ( 'NONE', *, *, #142453, .T. ) ;
#202361 = DIRECTION ( 'NONE',  ( -0.000000000000000000, -0.4721928772777351790, -0.8814952561688427224 ) ) ;
#202362 = CIRCLE ( 'NONE', #248512, 12.87499999999999822 ) ;
#202363 = B_SPLINE_CURVE_WITH_KNOTS ( 'NONE', 3,
 ( #179178, #489, #60466, #162175, #241688, #120489, #136134, #81294, #240411, #42214, #201269, #121764, #167316, #202561, #64341, #83851, #184276, #163441, #87731 ),
 .UNSPECIFIED., .F., .F.,
 ( 4, 3, 3, 3, 3, 3, 4 ),
 ( -2.000416914638703597E-06, 0.000000000000000000, 4.714008503745425717E-05, 9.979203887779529328E-05, 0.0001372215519229583788, 0.0001635031576221022021, 0.0001900083748504252776 ),
 .UNSPECIFIED. ) ;
#202364 = EDGE_CURVE ( 'NONE', #109246, #115263, #120233, .T. ) ;
#202366 = EDGE_CURVE ( 'NONE', #31072, #209903, #120047, .T. ) ;
#202365 = FACE_OUTER_BOUND ( 'NONE', #132500, .T. ) ;
#202368 = ORIENTED_EDGE ( 'NONE', *, *, #218835, .T. ) ;
#202367 = AXIS2_PLACEMENT_3D ( 'NONE', #12215, #227378, #26638 ) ;
#202369 = AXIS2_PLACEMENT_3D ( 'NONE', #59664, #21857, #2267 ) ;
#202370 = ADVANCED_FACE ( 'NONE', ( #60772 ), #163747, .F. ) ;
#202371 = DIRECTION ( 'NONE',  ( 0.000000000000000000, 0.000000000000000000, 1.000000000000000000 ) ) ;
#202373 = CARTESIAN_POINT ( 'NONE',  ( 22.37643362114956247, 68.37421000605377230, -136.6221888582057318 ) ) ;
#202372 = CIRCLE ( 'NONE', #219110, 12.77499999999999503 ) ;
#202374 = CARTESIAN_POINT ( 'NONE',  ( 18.59999999999999787, 77.85102823015292017, -124.8691942151017855 ) ) ;
#202375 = DIRECTION ( 'NONE',  ( -1.000000000000000000, 0.000000000000000000, 0.000000000000000000 ) ) ;
#202376 = CARTESIAN_POINT ( 'NONE',  ( -16.97683809663752186, 44.82209472663103611, -234.9913374327310578 ) ) ;
#202377 = CARTESIAN_POINT ( 'NONE',  ( -21.05000000000000071, 1.250000000011155299, -75.00000000000004263 ) ) ;
#202378 = EDGE_CURVE ( 'NONE', #26640, #157564, #186667, .T. ) ;
#202379 = CARTESIAN_POINT ( 'NONE',  ( 12.25000000000000000, 62.59162599727320497, -217.2417264603073761 ) ) ;
#202380 = ORIENTED_EDGE ( 'NONE', *, *, #39991, .T. ) ;
#202382 = DIRECTION ( 'NONE',  ( 1.000000000000000000, 0.000000000000000000, 0.000000000000000000 ) ) ;
#202381 = DIRECTION ( 'NONE',  ( 0.000000000000000000, 1.000000000000000000, 0.000000000000000000 ) ) ;
#202383 = ORIENTED_EDGE ( 'NONE', *, *, #103873, .T. ) ;
#202385 = ORIENTED_EDGE ( 'NONE', *, *, #180289, .T. ) ;
#202384 = DIRECTION ( 'NONE',  ( 0.000000000000000000, 0.000000000000000000, 1.000000000000000000 ) ) ;
#202386 = AXIS2_PLACEMENT_3D ( 'NONE', #121073, #58468, #78048 ) ;
#202387 = VERTEX_POINT ( 'NONE', #223691 ) ;
#202388 = CARTESIAN_POINT ( 'NONE',  ( 18.59999999999999076, 77.83585931145600512, -158.5186683157258187 ) ) ;
#202389 = ADVANCED_FACE ( 'NONE', ( #240713 ), #3359, .F. ) ;
#202390 = DIRECTION ( 'NONE',  ( 0.000000000000000000, 1.000000000000000000, 6.982962677686266711E-15 ) ) ;
#202391 = VECTOR ( 'NONE', #40736, 1000.000000000000000 ) ;
#202392 = CARTESIAN_POINT ( 'NONE',  ( -20.85000000000000142, 7.021664781911246322, -70.83356540189728889 ) ) ;
#202393 = DIRECTION ( 'NONE',  ( 0.000000000000000000, -0.9770955615653320603, -0.2128009952263577587 ) ) ;
#202394 = ORIENTED_EDGE ( 'NONE', *, *, #224465, .F. ) ;
#202395 = CARTESIAN_POINT ( 'NONE',  ( -23.15000000000000213, 71.65000000001151648, -48.27310748452435263 ) ) ;
#202396 = DIRECTION ( 'NONE',  ( 1.000000000000000000, 0.000000000000000000, 0.000000000000000000 ) ) ;
#202397 = AXIS2_PLACEMENT_3D ( 'NONE', #211304, #32713, #245300 ) ;
#202398 = ORIENTED_EDGE ( 'NONE', *, *, #207472, .T. ) ;
#202400 = ADVANCED_FACE ( 'NONE', ( #201573 ), #45073, .T. ) ;
#202399 = DIRECTION ( 'NONE',  ( 0.000000000000000000, 1.000000000000000000, 1.224646799147353207E-16 ) ) ;
#202401 = FACE_OUTER_BOUND ( 'NONE', #184988, .T. ) ;
#202402 = ORIENTED_EDGE ( 'NONE', *, *, #57426, .T. ) ;
#202403 = CARTESIAN_POINT ( 'NONE',  ( -16.84793658983432252, 9.950000000011138823, -146.7336466778100430 ) ) ;
#202404 = DIRECTION ( 'NONE',  ( 0.000000000000000000, -6.982962677686266711E-15, 1.000000000000000000 ) ) ;
#202405 = VERTEX_POINT ( 'NONE', #24250 ) ;
#202406 = LINE ( 'NONE', #177742, #179429 ) ;
#202407 = DIRECTION ( 'NONE',  ( 0.000000000000000000, 0.000000000000000000, -1.000000000000000000 ) ) ;
#202409 = CARTESIAN_POINT ( 'NONE',  ( -23.15000000000000213, 67.23127455305835554, -235.8551265064784559 ) ) ;
#202408 = APPLICATION_CONTEXT ( 'automotive_design' ) ;
#202410 = FACE_OUTER_BOUND ( 'NONE', #42264, .T. ) ;
#202411 = AXIS2_PLACEMENT_3D ( 'NONE', #90846, #149573, #68734 ) ;
#202412 = CIRCLE ( 'NONE', #123309, 0.1000000000000124678 ) ;
#202413 = TOROIDAL_SURFACE ( 'NONE', #110835, 4.041421356237310469, 0.1000000000000000056 ) ;
#202414 = DIRECTION ( 'NONE',  ( 1.000000000000000000, -0.000000000000000000, -0.000000000000000000 ) ) ;
#202415 = DIRECTION ( 'NONE',  ( -0.000000000000000000, 0.000000000000000000, -1.000000000000000000 ) ) ;
#202416 = FACE_OUTER_BOUND ( 'NONE', #12302, .T. ) ;
#202417 = ORIENTED_EDGE ( 'NONE', *, *, #76212, .F. ) ;
#202419 = FACE_OUTER_BOUND ( 'NONE', #175821, .T. ) ;
#202418 = DIRECTION ( 'NONE',  ( -0.000000000000000000, -0.000000000000000000, -1.000000000000000000 ) ) ;
#202420 = AXIS2_PLACEMENT_3D ( 'NONE', #71339, #188691, #11346 ) ;
#202421 = EDGE_CURVE ( 'NONE', #246341, #6807, #27010, .T. ) ;
#202422 = ADVANCED_FACE ( 'NONE', ( #145445 ), #122479, .T. ) ;
#202423 = ORIENTED_EDGE ( 'NONE', *, *, #42989, .F. ) ;
#202424 = CARTESIAN_POINT ( 'NONE',  ( -18.41418431465368499, 85.50000000001263345, -163.4229180933028260 ) ) ;
#202425 = FACE_OUTER_BOUND ( 'NONE', #216310, .T. ) ;
#202428 = ORIENTED_EDGE ( 'NONE', *, *, #59638, .T. ) ;
#202427 = FACE_OUTER_BOUND ( 'NONE', #173645, .T. ) ;
#202426 =( BOUNDED_CURVE ( )  B_SPLINE_CURVE ( 3, ( #169608, #90009, #146134, #9196 ),
 .UNSPECIFIED., .F., .F. ) 
 B_SPLINE_CURVE_WITH_KNOTS ( ( 4, 4 ),
 ( 4.937700262165045813E-15, 1.570796326794912323 ),
 .UNSPECIFIED. ) 
 CURVE ( )  GEOMETRIC_REPRESENTATION_ITEM ( )  RATIONAL_B_SPLINE_CURVE ( ( 1.000000000000000000, 0.8047378541243623840, 0.8047378541243623840, 1.000000000000000000 ) ) 
 REPRESENTATION_ITEM ( '' )  );
#202430 = EDGE_LOOP ( 'NONE', ( #247027, #87732, #174459, #16848, #204481 ) ) ;
#202429 = CARTESIAN_POINT ( 'NONE',  ( -23.15000000000000213, 71.65000000001222702, -148.8731074845244109 ) ) ;
#202432 = EDGE_CURVE ( 'NONE', #239767, #66395, #182751, .T. ) ;
#202431 = CARTESIAN_POINT ( 'NONE',  ( 18.43565242384935132, 46.91436717984745286, -255.3877622108296066 ) ) ;
#202435 = ADVANCED_FACE ( 'NONE', ( #180744 ), #249386, .T. ) ;
#202434 = DIRECTION ( 'NONE',  ( 0.7071067811865473507, 0.3338907855510733769, 0.6233112732207618523 ) ) ;
#202433 = AXIS2_PLACEMENT_3D ( 'NONE', #18457, #238796, #135817 ) ;
#202436 = DIRECTION ( 'NONE',  ( 1.000000000000000000, -7.136802563874198121E-16, -1.554319503706929745E-16 ) ) ;
#202437 = DIRECTION ( 'NONE',  ( 0.000000000000000000, -1.000000000000000000, 0.000000000000000000 ) ) ;
#202439 = EDGE_LOOP ( 'NONE', ( #49185, #160090, #184679, #80012 ) ) ;
#202438 = LINE ( 'NONE', #85024, #169556 ) ;
#202440 = CIRCLE ( 'NONE', #235737, 0.09999999999999530098 ) ;
#202441 = ADVANCED_FACE ( 'NONE', ( #2078 ), #93180, .F. ) ;
#202442 = ADVANCED_FACE ( 'NONE', ( #230129 ), #149336, .F. ) ;
#202443 = EDGE_CURVE ( 'NONE', #241281, #75576, #50193, .T. ) ;
#202444 = DIRECTION ( 'NONE',  ( 0.000000000000000000, -0.2617529984165031243, -0.9651348961777157509 ) ) ;
#202445 = ORIENTED_EDGE ( 'NONE', *, *, #170165, .F. ) ;
#202446 = ORIENTED_EDGE ( 'NONE', *, *, #1084, .T. ) ;
#202447 = ADVANCED_FACE ( 'NONE', ( #172773 ), #112756, .F. ) ;
#202448 = CIRCLE ( 'NONE', #164859, 0.5000000000000013323 ) ;
#202449 = CARTESIAN_POINT ( 'NONE',  ( -18.44448725179914561, 85.49008171549472479, -29.39414719046178348 ) ) ;
#202450 = DIRECTION ( 'NONE',  ( 1.000000000000000000, 0.000000000000000000, 0.000000000000000000 ) ) ;
#202451 = ORIENTED_EDGE ( 'NONE', *, *, #231621, .F. ) ;
#202452 = DIRECTION ( 'NONE',  ( 0.000000000000000000, 1.000000000000000000, -6.308085367188393199E-16 ) ) ;
#202453 = EDGE_CURVE ( 'NONE', #140654, #52463, #70348, .T. ) ;
#202454 = CARTESIAN_POINT ( 'NONE',  ( -18.50000000000000000, -1.362429037182155023, -208.8888812479211765 ) ) ;
#202455 = ORIENTED_EDGE ( 'NONE', *, *, #199970, .F. ) ;
#202456 = EDGE_CURVE ( 'NONE', #149886, #37861, #154012, .T. ) ;
#202457 = EDGE_CURVE ( 'NONE', #223762, #32631, #191138, .T. ) ;
#202458 = CIRCLE ( 'NONE', #23427, 0.09999999999999635569 ) ;
#202459 = AXIS2_PLACEMENT_3D ( 'NONE', #243611, #64968, #144489 ) ;
#202460 = CYLINDRICAL_SURFACE ( 'NONE', #52012, 0.09999999999999939493 ) ;
#202461 = AXIS2_PLACEMENT_3D ( 'NONE', #32784, #113565, #74479 ) ;
#202462 = CIRCLE ( 'NONE', #52415, 0.09999999999999939493 ) ;
#202463 = DIRECTION ( 'NONE',  ( 0.000000000000000000, 0.000000000000000000, -1.000000000000000000 ) ) ;
#202464 = EDGE_CURVE ( 'NONE', #14295, #237997, #153199, .T. ) ;
#202465 = ORIENTED_EDGE ( 'NONE', *, *, #217818, .F. ) ;
#202466 = ORIENTED_EDGE ( 'NONE', *, *, #108175, .F. ) ;
#202467 = ORIENTED_EDGE ( 'NONE', *, *, #225350, .T. ) ;
#202468 = CARTESIAN_POINT ( 'NONE',  ( -21.64999999999999858, 68.75000000001179501, -81.77310748452435973 ) ) ;
#202469 = ORIENTED_EDGE ( 'NONE', *, *, #100672, .F. ) ;
#202471 = VERTEX_POINT ( 'NONE', #88022 ) ;
#202470 = FACE_OUTER_BOUND ( 'NONE', #147382, .T. ) ;
#202472 = EDGE_CURVE ( 'NONE', #154148, #149376, #232828, .T. ) ;
#202473 = ADVANCED_FACE ( 'NONE', ( #131027 ), #108892, .F. ) ;
#202474 = CARTESIAN_POINT ( 'NONE',  ( -21.14999999999999858, 12.76524917372336709, -223.4223513401831553 ) ) ;
#202475 = ORIENTED_EDGE ( 'NONE', *, *, #145536, .T. ) ;
#202476 = DIRECTION ( 'NONE',  ( 0.000000000000000000, -0.8660254037844459241, -0.4999999999999873990 ) ) ;
#202477 = VERTEX_POINT ( 'NONE', #127186 ) ;
#202479 = EDGE_LOOP ( 'NONE', ( #174865, #85960, #140186, #203530 ) ) ;
#202478 = ORIENTED_EDGE ( 'NONE', *, *, #147802, .F. ) ;
#202480 = CARTESIAN_POINT ( 'NONE',  ( 21.05000000000000071, 69.74115287693305731, -136.5548658375798254 ) ) ;
#202481 = AXIS2_PLACEMENT_3D ( 'NONE', #226981, #10513, #209996 ) ;
#202482 = DIRECTION ( 'NONE',  ( 0.000000000000000000, 0.000000000000000000, -1.000000000000000000 ) ) ;
#202483 = CIRCLE ( 'NONE', #190007, 0.2000000000000057288 ) ;
#202484 = ORIENTED_EDGE ( 'NONE', *, *, #20559, .F. ) ;
#202485 = TOROIDAL_SURFACE ( 'NONE', #252353, 0.2000000000000000111, 0.1000000000000000056 ) ;
#202486 = ORIENTED_EDGE ( 'NONE', *, *, #173834, .T. ) ;
#202487 = CARTESIAN_POINT ( 'NONE',  ( 23.14999999999998437, 76.00000000001195133, -103.0231074845243171 ) ) ;
#202488 = DIRECTION ( 'NONE',  ( 1.000000000000000000, 0.000000000000000000, 0.000000000000000000 ) ) ;
#202490 = ORIENTED_EDGE ( 'NONE', *, *, #226869, .T. ) ;
#202489 = DIRECTION ( 'NONE',  ( 0.000000000000000000, 0.9856811345164800953, 0.1686199900910462790 ) ) ;
#202491 = CYLINDRICAL_SURFACE ( 'NONE', #102203, 0.09999999999999939493 ) ;
#202492 = VERTEX_POINT ( 'NONE', #167612 ) ;
#202493 = CARTESIAN_POINT ( 'NONE',  ( -18.50016250449483479, 65.70233904877031250, -131.0487410911968595 ) ) ;
#202494 = DIRECTION ( 'NONE',  ( -0.7071067811865301422, 0.7071067811865648922, 0.000000000000000000 ) ) ;
#202495 = ORIENTED_EDGE ( 'NONE', *, *, #234524, .T. ) ;
#202496 = CARTESIAN_POINT ( 'NONE',  ( -16.87683809663752399, 9.850000000011140955, -180.1499999999999773 ) ) ;
#202497 = DIRECTION ( 'NONE',  ( 0.000000000000000000, 0.000000000000000000, -1.000000000000000000 ) ) ;
#202498 = VERTEX_POINT ( 'NONE', #9797 ) ;
#202499 = DIRECTION ( 'NONE',  ( 0.000000000000000000, 0.000000000000000000, 1.000000000000000000 ) ) ;
#202500 = ORIENTED_EDGE ( 'NONE', *, *, #88840, .F. ) ;
#202501 = AXIS2_PLACEMENT_3D ( 'NONE', #156695, #35469, #155417 ) ;
#202503 = ORIENTED_EDGE ( 'NONE', *, *, #70853, .T. ) ;
#202502 = EDGE_LOOP ( 'NONE', ( #5527, #188323, #188754, #10448 ) ) ;
#202504 = EDGE_LOOP ( 'NONE', ( #39391, #176668, #77932, #102786, #57805, #138021, #52270 ) ) ;
#202505 = CARTESIAN_POINT ( 'NONE',  ( -16.97048326478264002, 9.950000000011133494, -80.14110688012718242 ) ) ;
#202506 = EDGE_LOOP ( 'NONE', ( #88336, #139277, #86377, #124958 ) ) ;
#202507 = CARTESIAN_POINT ( 'NONE',  ( 18.39999999999999503, 14.17280543801757986, -210.8598471598932349 ) ) ;
#202508 = ORIENTED_EDGE ( 'NONE', *, *, #217535, .T. ) ;
#202509 = DIRECTION ( 'NONE',  ( -1.000000000000000000, 0.000000000000000000, 0.000000000000000000 ) ) ;
#202510 = DIRECTION ( 'NONE',  ( 0.000000000000000000, 1.000000000000000000, 6.982962677686266711E-15 ) ) ;
#202511 = ORIENTED_EDGE ( 'NONE', *, *, #238707, .T. ) ;
#202512 = EDGE_CURVE ( 'NONE', #43685, #188264, #20435, .T. ) ;
#202513 = ORIENTED_EDGE ( 'NONE', *, *, #168474, .T. ) ;
#202514 = TOROIDAL_SURFACE ( 'NONE', #173346, 11.89999999999999858, 0.1000000000000000056 ) ;
#202515 = EDGE_CURVE ( 'NONE', #144797, #47719, #211872, .T. ) ;
#202516 = VERTEX_POINT ( 'NONE', #248414 ) ;
#202517 = AXIS2_PLACEMENT_3D ( 'NONE', #54148, #152008, #13751 ) ;
#202518 = AXIS2_PLACEMENT_3D ( 'NONE', #136405, #192569, #75211 ) ;
#202519 =( BOUNDED_CURVE ( )  B_SPLINE_CURVE ( 3, ( #60342, #237714, #218122, #119057 ),
 .UNSPECIFIED., .F., .F. ) 
 B_SPLINE_CURVE_WITH_KNOTS ( ( 4, 4 ),
 ( -9.769962616701377556E-15, 1.570796326794891673 ),
 .UNSPECIFIED. ) 
 CURVE ( )  GEOMETRIC_REPRESENTATION_ITEM ( )  RATIONAL_B_SPLINE_CURVE ( ( 1.000000000000000000, 0.8047378541243637162, 0.8047378541243637162, 1.000000000000000000 ) ) 
 REPRESENTATION_ITEM ( '' )  );
#202520 = ADVANCED_FACE ( 'NONE', ( #69794 ), #189725, .F. ) ;
#202521 = CARTESIAN_POINT ( 'NONE',  ( -16.94107738177414291, 65.98576071487519812, -82.07310748452438531 ) ) ;
#202522 = EDGE_CURVE ( 'NONE', #47404, #115127, #153758, .T. ) ;
#202523 = ORIENTED_EDGE ( 'NONE', *, *, #188236, .T. ) ;
#202524 = CARTESIAN_POINT ( 'NONE',  ( 23.14999999999999503, 10.99842653345846699, -220.2504445088529792 ) ) ;
#202525 = LINE ( 'NONE', #103397, #72167 ) ;
#202526 = SPHERICAL_SURFACE ( 'NONE', #218280, 0.1000000000000000056 ) ;
#202527 = CARTESIAN_POINT ( 'NONE',  ( 20.94999999999999929, -1.835859311432481045, -212.5044391687984842 ) ) ;
#202528 = DIRECTION ( 'NONE',  ( 1.000000000000000000, 2.952720810173289112E-16, -0.000000000000000000 ) ) ;
#202529 = DIRECTION ( 'NONE',  ( 1.000000000000000000, -0.000000000000000000, -0.000000000000000000 ) ) ;
#202531 = FACE_OUTER_BOUND ( 'NONE', #51617, .T. ) ;
#202530 = CARTESIAN_POINT ( 'NONE',  ( -18.39999999999999858, -9.519327731081281385, -107.4729763765593589 ) ) ;
#202532 = CARTESIAN_POINT ( 'NONE',  ( -21.05000000000000071, -4.892732937820630568, -233.2805462221312496 ) ) ;
#202533 = DIRECTION ( 'NONE',  ( 0.000000000000000000, -0.2128009952263601456, 0.9770955615653316162 ) ) ;
#202534 = LINE ( 'NONE', #40927, #35353 ) ;
#202535 = CARTESIAN_POINT ( 'NONE',  ( -21.05000000000000071, 55.11435547888748232, -226.8560373590520101 ) ) ;
#202536 = EDGE_LOOP ( 'NONE', ( #96913, #52360, #71066, #85788 ) ) ;
#202538 = ADVANCED_FACE ( 'NONE', ( #157033 ), #257334, .T. ) ;
#202537 = CIRCLE ( 'NONE', #90098, 11.65000000000000213 ) ;
#202540 = VERTEX_POINT ( 'NONE', #488 ) ;
#202539 = DIRECTION ( 'NONE',  ( -1.000000000000000000, -2.952720810173289112E-16, 0.000000000000000000 ) ) ;
#202541 = CIRCLE ( 'NONE', #256462, 0.09999999999999971412 ) ;
#202542 = ORIENTED_EDGE ( 'NONE', *, *, #173852, .F. ) ;
#202543 = FACE_OUTER_BOUND ( 'NONE', #153528, .T. ) ;
#202544 = CARTESIAN_POINT ( 'NONE',  ( 20.97438252431638972, 8.925423506087151182, -142.4723706890108303 ) ) ;
#202545 = VECTOR ( 'NONE', #102323, 1000.000000000000000 ) ;
#202546 = CIRCLE ( 'NONE', #248336, 4.000000000000003553 ) ;
#202547 = LINE ( 'NONE', #241674, #61397 ) ;
#202548 = ORIENTED_EDGE ( 'NONE', *, *, #251012, .F. ) ;
#202549 = ADVANCED_FACE ( 'NONE', ( #174053 ), #215682, .T. ) ;
#202550 = CARTESIAN_POINT ( 'NONE',  ( -21.55000000000000426, 68.29142135624910281, -81.87310748452436826 ) ) ;
#202551 = EDGE_CURVE ( 'NONE', #56225, #178238, #207694, .T. ) ;
#202552 = DIRECTION ( 'NONE',  ( 0.000000000000000000, 0.000000000000000000, -1.000000000000000000 ) ) ;
#202553 = VERTEX_POINT ( 'NONE', #20084 ) ;
#202555 = DIRECTION ( 'NONE',  ( 0.000000000000000000, 0.000000000000000000, -1.000000000000000000 ) ) ;
#202554 = AXIS2_PLACEMENT_3D ( 'NONE', #200269, #219819, #236811 ) ;
#202556 = CARTESIAN_POINT ( 'NONE',  ( 22.39999999999999503, 68.20922040163827660, -69.52310748452437394 ) ) ;
#202557 = AXIS2_PLACEMENT_3D ( 'NONE', #231461, #52790, #9827 ) ;
#202558 = CARTESIAN_POINT ( 'NONE',  ( -18.50000000000000000, -9.399999999988850163, -73.91465834296965909 ) ) ;
#202559 = CIRCLE ( 'NONE', #131645, 0.1000000000000008937 ) ;
#202560 = CARTESIAN_POINT ( 'NONE',  ( 20.95429402530532315, 40.80824126842007615, -237.9661292884959778 ) ) ;
#202562 = ORIENTED_EDGE ( 'NONE', *, *, #148579, .F. ) ;
#202561 = CARTESIAN_POINT ( 'NONE',  ( -20.89192007715128341, 67.49241595948059569, -195.4314365843280541 ) ) ;
#202564 = DIRECTION ( 'NONE',  ( 7.304098846218134667E-16, 0.4088369013363281068, -0.9126074666063770380 ) ) ;
#202563 = AXIS2_PLACEMENT_3D ( 'NONE', #167873, #28372, #246107 ) ;
#202565 = EDGE_CURVE ( 'NONE', #157661, #141295, #82733, .T. ) ;
#202567 = ORIENTED_EDGE ( 'NONE', *, *, #222075, .T. ) ;
#202566 = LINE ( 'NONE', #23951, #14877 ) ;
#202568 = CYLINDRICAL_SURFACE ( 'NONE', #116707, 0.5000000000000004441 ) ;
#202569 = CARTESIAN_POINT ( 'NONE',  ( -21.05000000000000071, 5.899999999999947065, -10.21909976465641456 ) ) ;
#202570 = ORIENTED_EDGE ( 'NONE', *, *, #167375, .T. ) ;
#202571 = CARTESIAN_POINT ( 'NONE',  ( -16.93658211146646408, 66.00589133767111605, -157.4274025544800963 ) ) ;
#202572 = EDGE_CURVE ( 'NONE', #17438, #245624, #78741, .T. ) ;
#202573 = CARTESIAN_POINT ( 'NONE',  ( -23.15000000000000213, 11.75000000000000000, -26.48519422934605672 ) ) ;
#202575 = DIRECTION ( 'NONE',  ( 0.000000000000000000, -0.9594490217226113726, -0.2818822000686178608 ) ) ;
#202574 = DIRECTION ( 'NONE',  ( 0.000000000000000000, 0.6728971962617102953, 0.7397360091702507301 ) ) ;
#202576 = CARTESIAN_POINT ( 'NONE',  ( 18.59999999999999787, 48.04585786805223080, -246.4610531646956417 ) ) ;
#202577 = CARTESIAN_POINT ( 'NONE',  ( 12.25000000000000000, 9.350000000011140955, -83.75000000000004263 ) ) ;
#202578 = AXIS2_PLACEMENT_3D ( 'NONE', #36076, #748, #217241 ) ;
#202580 = EDGE_CURVE ( 'NONE', #56413, #144623, #228538, .T. ) ;
#202579 = CARTESIAN_POINT ( 'NONE',  ( -18.55121869061588669, 10.32747123226657493, -39.07740328502493554 ) ) ;
#202581 = CARTESIAN_POINT ( 'NONE',  ( -1.739115166359751170E-14, 54.57427006634497957, -228.7596887170734306 ) ) ;
#202582 = DIRECTION ( 'NONE',  ( 0.000000000000000000, 0.000000000000000000, 1.000000000000000000 ) ) ;
#202583 = VERTEX_POINT ( 'NONE', #116603 ) ;
#202584 = CARTESIAN_POINT ( 'NONE',  ( 23.40000000000005187, 76.00000000001119815, -36.02310748452479316 ) ) ;
#202585 = ORIENTED_EDGE ( 'NONE', *, *, #254764, .F. ) ;
#202586 = ORIENTED_EDGE ( 'NONE', *, *, #187879, .F. ) ;
#202587 = DIRECTION ( 'NONE',  ( 0.000000000000000000, 6.982962677686266711E-15, -1.000000000000000000 ) ) ;
#202588 = CARTESIAN_POINT ( 'NONE',  ( -18.50000000000000000, 13.53887499352833146, -219.6971619212644669 ) ) ;
#202589 = ORIENTED_EDGE ( 'NONE', *, *, #167730, .F. ) ;
#202590 = EDGE_CURVE ( 'NONE', #142060, #121241, #236538, .T. ) ;
#202591 = VECTOR ( 'NONE', #110393, 1000.000000000000000 ) ;
#202592 = VECTOR ( 'NONE', #243730, 1000.000000000000000 ) ;
#202593 = ORIENTED_EDGE ( 'NONE', *, *, #209137, .T. ) ;
#202594 = EDGE_CURVE ( 'NONE', #9522, #49603, #57892, .T. ) ;
#202595 = CIRCLE ( 'NONE', #119393, 0.09999999999998712696 ) ;
#202596 = CIRCLE ( 'NONE', #206693, 7.900000000000014566 ) ;
#202597 = VERTEX_POINT ( 'NONE', #35805 ) ;
#202598 = DIRECTION ( 'NONE',  ( 0.000000000000000000, -1.000000000000000000, -8.717686153663073805E-15 ) ) ;
#202599 = ORIENTED_EDGE ( 'NONE', *, *, #9129, .T. ) ;
#202600 = CIRCLE ( 'NONE', #2675, 0.2000000000000057288 ) ;
#202601 = CARTESIAN_POINT ( 'NONE',  ( -20.54999999999999716, 63.56320957583155717, -222.0641766000055668 ) ) ;
#202602 = DIRECTION ( 'NONE',  ( 0.000000000000000000, -0.9908441862701596881, -0.1350103645451904977 ) ) ;
#202603 = CARTESIAN_POINT ( 'NONE',  ( -23.25000000000000000, 86.43238724539048690, -209.5644480942280836 ) ) ;
#202604 = CARTESIAN_POINT ( 'NONE',  ( -21.05000000000000071, 11.75000000001115552, -93.48519422934610645 ) ) ;
#202605 = DIRECTION ( 'NONE',  ( 0.000000000000000000, -1.000000000000000000, 0.000000000000000000 ) ) ;
#202606 = DIRECTION ( 'NONE',  ( 0.000000000000000000, -0.4088369013363280513, 0.9126074666063769270 ) ) ;
#202607 = DIRECTION ( 'NONE',  ( 0.000000000000000000, -0.8814952561688431665, 0.4721928772777346794 ) ) ;
#202609 = EDGE_LOOP ( 'NONE', ( #17874, #191710, #95010, #181351 ) ) ;
#202608 = DIRECTION ( 'NONE',  ( 0.000000000000000000, 1.224646799142015331E-16, 1.000000000000000000 ) ) ;
#202610 = CARTESIAN_POINT ( 'NONE',  ( -16.94226253665225101, 66.05000000001226113, -149.4698420801402392 ) ) ;
#202611 = CARTESIAN_POINT ( 'NONE',  ( 22.50000000000000000, 64.35042919246758686, -170.1231074845244393 ) ) ;
#202612 = AXIS2_PLACEMENT_3D ( 'NONE', #200312, #141613, #221141 ) ;
#202613 = EDGE_LOOP ( 'NONE', ( #170290, #169091, #133131, #248911, #198217, #96489, #69196, #234095, #34605, #69343, #249347, #2012 ) ) ;
#202614 = DIRECTION ( 'NONE',  ( -1.000000000000000000, 0.000000000000000000, -0.000000000000000000 ) ) ;
#202615 = DIRECTION ( 'NONE',  ( -0.000000000000000000, 0.9770955615653316162, 0.2128009952263604232 ) ) ;
#202617 = VERTEX_POINT ( 'NONE', #114020 ) ;
#202616 = CIRCLE ( 'NONE', #60947, 0.1000000000000124678 ) ;
#202619 = DIRECTION ( 'NONE',  ( 0.000000000000000000, 6.982962677686266711E-15, -1.000000000000000000 ) ) ;
#202618 = DIRECTION ( 'NONE',  ( 1.000000000000000000, -9.792504721693619684E-16, -4.386921467590155985E-16 ) ) ;
#202620 = FACE_OUTER_BOUND ( 'NONE', #55937, .T. ) ;
#202621 = EDGE_LOOP ( 'NONE', ( #67047, #27296, #187136 ) ) ;
#202622 = DIRECTION ( 'NONE',  ( -1.000000000000000000, 1.335000415235278971E-16, -2.979993593738921214E-16 ) ) ;
#202623 = DIRECTION ( 'NONE',  ( 0.000000000000000000, 0.000000000000000000, -1.000000000000000000 ) ) ;
#202624 = AXIS2_PLACEMENT_3D ( 'NONE', #60735, #200270, #159878 ) ;
#202625 = FACE_OUTER_BOUND ( 'NONE', #205486, .T. ) ;
#202626 = EDGE_LOOP ( 'NONE', ( #214726, #85170, #21574, #226949 ) ) ;
#202627 = CARTESIAN_POINT ( 'NONE',  ( 20.95512820512820440, 67.12384868372375024, -90.87310748452436826 ) ) ;
#202628 = DIRECTION ( 'NONE',  ( 0.000000000000000000, -0.2128009952263604232, 0.9770955615653316162 ) ) ;
#202629 = CARTESIAN_POINT ( 'NONE',  ( 23.15000000000000213, 87.48912529308749697, -39.12310748452424747 ) ) ;
#202630 = CARTESIAN_POINT ( 'NONE',  ( -20.65000000000000568, 68.75000000001202238, -115.6731074845243512 ) ) ;
#202631 = CIRCLE ( 'NONE', #19497, 0.09999999999998898659 ) ;
#202632 = AXIS2_PLACEMENT_3D ( 'NONE', #176628, #256075, #94488 ) ;
#202633 = CARTESIAN_POINT ( 'NONE',  ( -0.8999999999999994671, -8.279289321881350361, 29.97071067811866030 ) ) ;
#202634 = AXIS2_PLACEMENT_3D ( 'NONE', #175650, #59502, #80349 ) ;
#202635 = CARTESIAN_POINT ( 'NONE',  ( -23.25000000000000000, 49.36776662947724503, -253.7196102226803021 ) ) ;
#202637 = ORIENTED_EDGE ( 'NONE', *, *, #236403, .F. ) ;
#202636 = CARTESIAN_POINT ( 'NONE',  ( 20.85000000000000142, 67.23127455305835554, -235.8551265064784559 ) ) ;
#202638 = CARTESIAN_POINT ( 'NONE',  ( -23.49999999999994316, 76.00000000001119815, -36.02310748452479316 ) ) ;
#202639 = DIRECTION ( 'NONE',  ( -1.000000000000000000, 0.000000000000000000, 0.000000000000000000 ) ) ;
#202640 = DIRECTION ( 'NONE',  ( 1.000000000000000000, 0.000000000000000000, 0.000000000000000000 ) ) ;
#202641 = ADVANCED_FACE ( 'NONE', ( #38359 ), #218247, .F. ) ;
#202642 = CARTESIAN_POINT ( 'NONE',  ( 18.79999999999999716, 10.88519226655716565, -15.14794223642649840 ) ) ;
#202644 = VERTEX_POINT ( 'NONE', #232718 ) ;
#202643 = DIRECTION ( 'NONE',  ( 1.000000000000000000, 0.000000000000000000, 0.000000000000000000 ) ) ;
#202645 = DIRECTION ( 'NONE',  ( -0.000000000000000000, 0.9876197685951276783, 0.1568667991644721316 ) ) ;
#202646 = DIRECTION ( 'NONE',  ( 0.000000000000000000, 0.2605042016806715099, 0.9654727137038706664 ) ) ;
#202647 = DIRECTION ( 'NONE',  ( -1.000000000000000000, -0.000000000000000000, -0.000000000000000000 ) ) ;
#202648 = ORIENTED_EDGE ( 'NONE', *, *, #161250, .F. ) ;
#202649 = CARTESIAN_POINT ( 'NONE',  ( -14.77538296656413586, 66.56333706821317264, -151.7000707522295215 ) ) ;
#202650 = FACE_OUTER_BOUND ( 'NONE', #49116, .T. ) ;
#202651 = EDGE_CURVE ( 'NONE', #176398, #234302, #178679, .T. ) ;
#202652 = EDGE_CURVE ( 'NONE', #216154, #215604, #236892, .T. ) ;
#202653 = DIRECTION ( 'NONE',  ( 1.000000000000000000, 0.000000000000000000, 0.000000000000000000 ) ) ;
#202654 = AXIS2_PLACEMENT_3D ( 'NONE', #30739, #125944, #29467 ) ;
#202655 = AXIS2_PLACEMENT_3D ( 'NONE', #33954, #113439, #234672 ) ;
#202657 = CIRCLE ( 'NONE', #98555, 0.1000000000000028644 ) ;
#202656 = DIRECTION ( 'NONE',  ( 1.000000000000000000, 0.000000000000000000, 0.000000000000000000 ) ) ;
#202658 = VERTEX_POINT ( 'NONE', #177879 ) ;
#202659 = FACE_OUTER_BOUND ( 'NONE', #159422, .T. ) ;
#202660 = B_SPLINE_CURVE_WITH_KNOTS ( 'NONE', 3,
 ( #157823, #237320, #59934, #34020, #176087, #79503, #217726, #95232, #255537, #58649, #35305, #156533, #37854, #198182, #138187, #57370, #117370, #99056, #196894 ),
 .UNSPECIFIED., .F., .F.,
 ( 4, 3, 3, 3, 3, 3, 4 ),
 ( 0.000000000000000000, 7.110282409889255887E-05, 0.0001508797727291325019, 0.0002027344179858315892, 0.0002343294522348972884, 0.0002454816334821104942, 0.0002619873080085499098 ),
 .UNSPECIFIED. ) ;
#202661 = ORIENTED_EDGE ( 'NONE', *, *, #46708, .F. ) ;
#202663 = DIRECTION ( 'NONE',  ( 0.000000000000000000, -0.2617529984165034573, -0.9651348961777156399 ) ) ;
#202662 = CIRCLE ( 'NONE', #106793, 0.09999999999999507894 ) ;
#202664 = DIRECTION ( 'NONE',  ( 0.000000000000000000, -0.9126074666063545004, -0.4088369013363783999 ) ) ;
#202665 = EDGE_CURVE ( 'NONE', #137004, #171323, #91156, .T. ) ;
#202666 = LINE ( 'NONE', #87835, #207962 ) ;
#202667 = CARTESIAN_POINT ( 'NONE',  ( 20.85000000000000142, 1.115600667400684642E-11, -200.9999999999999432 ) ) ;
#202668 = EDGE_LOOP ( 'NONE', ( #138656, #178705, #21697, #72568 ) ) ;
#202669 = CARTESIAN_POINT ( 'NONE',  ( 21.00000000000000000, 7.973296578895943121, -1.410778198689825347 ) ) ;
#202670 = CARTESIAN_POINT ( 'NONE',  ( 21.05000000000000071, 13.06362847850371445, -210.5896934006125889 ) ) ;
#202671 = DIRECTION ( 'NONE',  ( -0.000000000000000000, -1.000000000000000000, -0.000000000000000000 ) ) ;
#202672 = CARTESIAN_POINT ( 'NONE',  ( 5.900000000000059863, 64.75000000001119815, -25.92310748452479174 ) ) ;
#202673 = CIRCLE ( 'NONE', #177767, 0.09999999999999459321 ) ;
#202674 = LINE ( 'NONE', #157499, #48895 ) ;
#202675 = ORIENTED_EDGE ( 'NONE', *, *, #252339, .T. ) ;
#202677 = ORIENTED_EDGE ( 'NONE', *, *, #94979, .T. ) ;
#202676 = FACE_OUTER_BOUND ( 'NONE', #20278, .T. ) ;
#202678 = ORIENTED_EDGE ( 'NONE', *, *, #34749, .F. ) ;
#202679 = CARTESIAN_POINT ( 'NONE',  ( -16.79140778683509794, 9.944941598854562415, -20.82973723377078201 ) ) ;
#202680 = EDGE_LOOP ( 'NONE', ( #169548, #160271, #35642, #190807 ) ) ;
#202681 = EDGE_CURVE ( 'NONE', #41100, #145487, #211973, .T. ) ;
#202682 = DIRECTION ( 'NONE',  ( 0.000000000000000000, 0.000000000000000000, -1.000000000000000000 ) ) ;
#202683 = CARTESIAN_POINT ( 'NONE',  ( 20.95512820512820440, 8.876151316299271343, -112.6500000000000341 ) ) ;
#202684 = EDGE_CURVE ( 'NONE', #240363, #161820, #51394, .T. ) ;
#202685 = CYLINDRICAL_SURFACE ( 'NONE', #208032, 0.09999999999999867328 ) ;
#202686 = ORIENTED_EDGE ( 'NONE', *, *, #169781, .T. ) ;
#202687 = DIRECTION ( 'NONE',  ( 1.734723475976817507E-14, 1.000000000000000000, 6.982962677686266711E-15 ) ) ;
#202688 = CARTESIAN_POINT ( 'NONE',  ( 19.97071067811864609, 64.27928932189284694, -48.17310748452440805 ) ) ;
#202689 = AXIS2_PLACEMENT_3D ( 'NONE', #240159, #180191, #40707 ) ;
#202690 = EDGE_LOOP ( 'NONE', ( #241669, #141215, #146328, #245776 ) ) ;
#202691 = CARTESIAN_POINT ( 'NONE',  ( -14.22969084473441370, 9.456007326080465347, -152.4886334941467965 ) ) ;
#202693 = EDGE_LOOP ( 'NONE', ( #104375, #113201, #210864, #28738 ) ) ;
#202692 = DIRECTION ( 'NONE',  ( 0.000000000000000000, 0.9126074666063772600, 0.4088369013363274407 ) ) ;
#202694 = DIRECTION ( 'NONE',  ( -1.000000000000000000, 0.000000000000000000, 0.000000000000000000 ) ) ;
#202696 = ADVANCED_FACE ( 'NONE', ( #145136 ), #64340, .T. ) ;
#202695 = DIRECTION ( 'NONE',  ( 1.000000000000000000, 0.000000000000000000, 0.000000000000000000 ) ) ;
#202697 = CIRCLE ( 'NONE', #90249, 0.1000000000000028644 ) ;
#202699 = B_SPLINE_CURVE_WITH_KNOTS ( 'NONE', 3,
 ( #64303, #8197, #87698, #44751, #47281, #6891, #205076, #124290, #167288, #105969 ),
 .UNSPECIFIED., .F., .F.,
 ( 4, 2, 2, 2, 4 ),
 ( 0.000000000000000000, 3.990160268011731543E-05, 7.980320536023463086E-05, 0.0001596064107204822450, 0.0003192128214409942514 ),
 .UNSPECIFIED. ) ;
#202698 = VECTOR ( 'NONE', #93149, 1000.000000000000000 ) ;
#202700 = ORIENTED_EDGE ( 'NONE', *, *, #230352, .T. ) ;
#202702 = DIRECTION ( 'NONE',  ( 0.000000000000000000, 0.000000000000000000, -1.000000000000000000 ) ) ;
#202701 = STYLED_ITEM ( 'NONE', ( #211615 ), #76170 ) ;
#202703 = CARTESIAN_POINT ( 'NONE',  ( 21.13507111622890022, 10.71768338700954537, -79.24916858636082395 ) ) ;
#202704 = LINE ( 'NONE', #206564, #68371 ) ;
#202705 = ORIENTED_EDGE ( 'NONE', *, *, #254209, .F. ) ;
#202706 = DIRECTION ( 'NONE',  ( 0.000000000000000000, -6.938893903907030216E-14, 1.000000000000000000 ) ) ;
#202707 = LINE ( 'NONE', #121909, #218157 ) ;
#202708 = ORIENTED_EDGE ( 'NONE', *, *, #92950, .T. ) ;
#202709 = AXIS2_PLACEMENT_3D ( 'NONE', #203909, #85213, #146489 ) ;
#202710 = VECTOR ( 'NONE', #76429, 1000.000000000000000 ) ;
#202711 = EDGE_LOOP ( 'NONE', ( #177285, #88662, #220076, #159449 ) ) ;
#202712 = ADVANCED_FACE ( 'NONE', ( #42213 ), #123033, .T. ) ;
#202713 = CIRCLE ( 'NONE', #248516, 0.09999999999999986677 ) ;
#202714 = EDGE_CURVE ( 'NONE', #160733, #206540, #183014, .T. ) ;
#202715 = ORIENTED_EDGE ( 'NONE', *, *, #118159, .T. ) ;
#202716 = TOROIDAL_SURFACE ( 'NONE', #236043, 12.97499999999999787, 0.1000000000000000056 ) ;
#202717 = DIRECTION ( 'NONE',  ( -1.000000000000000000, 0.000000000000000000, 0.000000000000000000 ) ) ;
#202718 = CARTESIAN_POINT ( 'NONE',  ( -16.80891096016306463, 66.05000000001255955, -182.6554446772547635 ) ) ;
#202720 = ORIENTED_EDGE ( 'NONE', *, *, #52531, .F. ) ;
#202719 = DIRECTION ( 'NONE',  ( 3.616040088954497272E-32, -1.224646799147352961E-16, 1.000000000000000000 ) ) ;
#202721 = CARTESIAN_POINT ( 'NONE',  ( 21.00000000000000000, 9.750000000011153745, -179.7499999999999716 ) ) ;
#202723 = AXIS2_PLACEMENT_3D ( 'NONE', #31845, #238685, #77035 ) ;
#202722 = CARTESIAN_POINT ( 'NONE',  ( -21.05000000000000071, 64.35000000001234355, -163.2392418215462726 ) ) ;
#202724 = EDGE_CURVE ( 'NONE', #184009, #212706, #120488, .T. ) ;
#202726 = ADVANCED_FACE ( 'NONE', ( #103435 ), #142266, .F. ) ;
#202725 = CARTESIAN_POINT ( 'NONE',  ( -20.85000000000000142, 11.65000000001115232, -100.5000000000000426 ) ) ;
#202727 = CIRCLE ( 'NONE', #65361, 0.1000000000000017958 ) ;
#202728 = PLANE ( 'NONE',  #118685 ) ;
#202729 = LINE ( 'NONE', #243141, #213851 ) ;
#202731 = ORIENTED_EDGE ( 'NONE', *, *, #148262, .F. ) ;
#202730 = CARTESIAN_POINT ( 'NONE',  ( -16.89318236219974523, 66.04846474213741203, -182.6679778524186020 ) ) ;
#202733 = EDGE_LOOP ( 'NONE', ( #110498, #50496, #61191 ) ) ;
#202732 = DIRECTION ( 'NONE',  ( 0.000000000000000000, 0.9915357197604982575, -0.1298341882519033486 ) ) ;
#202734 = CARTESIAN_POINT ( 'NONE',  ( -23.15000000000000213, -9.599999999988845900, -191.1060308773475356 ) ) ;
#202735 = ORIENTED_EDGE ( 'NONE', *, *, #148817, .F. ) ;
#202736 = CARTESIAN_POINT ( 'NONE',  ( 21.03670563405601612, 65.37517631068362789, -90.69756059831524908 ) ) ;
#202737 = ADVANCED_FACE ( 'NONE', ( #220831 ), #83850, .F. ) ;
#202738 = AXIS2_PLACEMENT_3D ( 'NONE', #142540, #205075, #146383 ) ;
#202740 = ADVANCED_FACE ( 'NONE', ( #164725 ), #159589, .F. ) ;
#202739 = EDGE_CURVE ( 'NONE', #23245, #166638, #245285, .T. ) ;
#202741 = AXIS2_PLACEMENT_3D ( 'NONE', #95762, #158367, #237863 ) ;
#202742 = VECTOR ( 'NONE', #178002, 1000.000000000000000 ) ;
#202743 = DIRECTION ( 'NONE',  ( 1.000000000000000000, 0.000000000000000000, 0.000000000000000000 ) ) ;
#202744 = CARTESIAN_POINT ( 'NONE',  ( 22.49231231312462853, 11.64998490368843953, -66.93894711239866524 ) ) ;
#202745 = CARTESIAN_POINT ( 'NONE',  ( -21.05000000000000071, 74.16465844978819177, -191.9679561919613775 ) ) ;
#202746 = EDGE_CURVE ( 'NONE', #129693, #86347, #149440, .T. ) ;
#202747 = DIRECTION ( 'NONE',  ( 0.000000000000000000, 0.000000000000000000, 1.000000000000000000 ) ) ;
#202748 = ORIENTED_EDGE ( 'NONE', *, *, #34340, .T. ) ;
#202749 = DIRECTION ( 'NONE',  ( 0.000000000000000000, 0.000000000000000000, 1.000000000000000000 ) ) ;
#202751 = ORIENTED_EDGE ( 'NONE', *, *, #119203, .F. ) ;
#202750 = EDGE_CURVE ( 'NONE', #185772, #224326, #255684, .T. ) ;
#202752 = LINE ( 'NONE', #142760, #185198 ) ;
#202753 = CIRCLE ( 'NONE', #90318, 14.20833333333333748 ) ;
#202754 = EDGE_LOOP ( 'NONE', ( #220948, #225989, #25435, #29667, #111722, #202193, #125570, #121386, #67577, #166677, #225440, #58481, #212942, #114945, #183599, #234287, #52945, #129664, #244550, #188232, #138406, #67716, #2233, #94044, #249762 ) ) ;
#202755 = EDGE_CURVE ( 'NONE', #188642, #186448, #240410, .T. ) ;
#202756 = ADVANCED_FACE ( 'NONE', ( #22666 ), #7960, .T. ) ;
#202757 = DIRECTION ( 'NONE',  ( -1.000000000000000000, 2.952720810173289112E-16, 2.061873921506763405E-30 ) ) ;
#202758 = CARTESIAN_POINT ( 'NONE',  ( -18.42637059832562940, 86.89577927498417864, -199.6303102917484011 ) ) ;
#202759 = EDGE_CURVE ( 'NONE', #133788, #239144, #61765, .T. ) ;
#202760 = VERTEX_POINT ( 'NONE', #181719 ) ;
#202761 = LINE ( 'NONE', #679, #85990 ) ;
#202762 = VERTEX_POINT ( 'NONE', #111174 ) ;
#202763 = FACE_OUTER_BOUND ( 'NONE', #10548, .T. ) ;
#202764 = ORIENTED_EDGE ( 'NONE', *, *, #95512, .F. ) ;
#202765 = ADVANCED_FACE ( 'NONE', ( #210281 ), #53921, .T. ) ;
#202766 = VECTOR ( 'NONE', #64542, 1000.000000000000000 ) ;
#202767 = LINE ( 'NONE', #42412, #252280 ) ;
#202768 = CARTESIAN_POINT ( 'NONE',  ( 12.60053434924910754, 9.389534562357859215, -183.1748093043899530 ) ) ;
#202769 = AXIS2_PLACEMENT_3D ( 'NONE', #118895, #96708, #198411 ) ;
#202770 = CIRCLE ( 'NONE', #61129, 0.09999999999998898659 ) ;
#202772 = ORIENTED_EDGE ( 'NONE', *, *, #236076, .T. ) ;
#202771 = EDGE_CURVE ( 'NONE', #127786, #228568, #25747, .T. ) ;
#202773 = DIRECTION ( 'NONE',  ( 0.000000000000000000, -0.4930308989874653269, -0.8700118002898649117 ) ) ;
#202775 = ORIENTED_EDGE ( 'NONE', *, *, #216611, .T. ) ;
#202774 = CARTESIAN_POINT ( 'NONE',  ( -15.75000000000000355, 66.15000000001228386, -153.2731074845244166 ) ) ;
#202776 = CARTESIAN_POINT ( 'NONE',  ( 21.14999999999999858, 67.21339244341248786, -191.2731074845244166 ) ) ;
#202777 = ORIENTED_EDGE ( 'NONE', *, *, #81195, .F. ) ;
#202778 = AXIS2_PLACEMENT_3D ( 'NONE', #86060, #24869, #225577 ) ;
#202779 = ORIENTED_EDGE ( 'NONE', *, *, #155228, .T. ) ;
#202780 = ADVANCED_FACE ( 'NONE', ( #8227 ), #66398, .T. ) ;
#202781 = DIRECTION ( 'NONE',  ( -2.978066053179066272E-16, -1.000000000000000000, -7.147358527629759053E-15 ) ) ;
#202782 = CARTESIAN_POINT ( 'NONE',  ( 22.41477678272288188, 26.02708908150256661, -254.3131911847732454 ) ) ;
#202783 = AXIS2_PLACEMENT_3D ( 'NONE', #214136, #113741, #253244 ) ;
#202784 = CARTESIAN_POINT ( 'NONE',  ( -20.64999999999999858, 68.85000000001200249, -115.3731074845243540 ) ) ;
#202785 = CIRCLE ( 'NONE', #157023, 7.899999999999990585 ) ;
#202786 = CARTESIAN_POINT ( 'NONE',  ( -12.84409460144756743, 66.58931770574463371, -188.0919640425761372 ) ) ;
#202787 = DIRECTION ( 'NONE',  ( -0.000000000000000000, 1.000000000000000000, -0.000000000000000000 ) ) ;
#202788 = CIRCLE ( 'NONE', #86056, 7.720710678118691384 ) ;
#202789 = VERTEX_POINT ( 'NONE', #12094 ) ;
#202790 = DIRECTION ( 'NONE',  ( 0.000000000000000000, 0.000000000000000000, -1.000000000000000000 ) ) ;
#202791 = CARTESIAN_POINT ( 'NONE',  ( 23.25000000000000000, 85.60000000001177511, -79.41707660717668205 ) ) ;
#202792 = CARTESIAN_POINT ( 'NONE',  ( 20.99999999999999645, 9.749999999999982236, -20.84999999999999787 ) ) ;
#202793 = DIRECTION ( 'NONE',  ( -0.000000000000000000, -0.000000000000000000, -1.000000000000000000 ) ) ;
#202794 = ORIENTED_EDGE ( 'NONE', *, *, #85710, .T. ) ;
#202795 = CARTESIAN_POINT ( 'NONE',  ( -21.05000000000000071, 76.01465611852468385, -109.5197940702921642 ) ) ;
#202796 = ORIENTED_EDGE ( 'NONE', *, *, #118265, .T. ) ;
#202797 = CARTESIAN_POINT ( 'NONE',  ( 15.39793903038207823, 9.389686005666810331, -116.1728435063513416 ) ) ;
#202799 = VERTEX_POINT ( 'NONE', #112467 ) ;
#202798 = AXIS2_PLACEMENT_3D ( 'NONE', #73484, #76018, #115149 ) ;
#202800 = CARTESIAN_POINT ( 'NONE',  ( -22.24259225415828567, 68.50806212944726781, -203.6221733679772399 ) ) ;
#202801 = CARTESIAN_POINT ( 'NONE',  ( -20.92356734117541706, 10.31973158071402175, -72.55053347133544150 ) ) ;
#202802 = EDGE_LOOP ( 'NONE', ( #152808, #174993, #251856, #8758 ) ) ;
#202804 = ORIENTED_EDGE ( 'NONE', *, *, #152688, .F. ) ;
#202803 = DIRECTION ( 'NONE',  ( 0.000000000000000000, 0.000000000000000000, -1.000000000000000000 ) ) ;
#202805 = CARTESIAN_POINT ( 'NONE',  ( -20.85000000000000142, 76.00000000001190870, -103.0231074845243029 ) ) ;
#202806 = ORIENTED_EDGE ( 'NONE', *, *, #245235, .T. ) ;
#202807 = CARTESIAN_POINT ( 'NONE',  ( 18.59999999999999076, -1.149570369564537842, -141.8159124845019790 ) ) ;
#202808 = CARTESIAN_POINT ( 'NONE',  ( -20.85000000000000142, -11.64999999998884483, -167.5000000000000284 ) ) ;
#202809 = ORIENTED_EDGE ( 'NONE', *, *, #199225, .T. ) ;
#202810 = EDGE_LOOP ( 'NONE', ( #23629, #101124, #212875, #235801 ) ) ;
#202811 = EDGE_CURVE ( 'NONE', #158833, #128191, #188140, .T. ) ;
#202812 = SPHERICAL_SURFACE ( 'NONE', #114132, 0.1000000000000000056 ) ;
#202813 = CARTESIAN_POINT ( 'NONE',  ( 21.05000000000000426, 75.93429838969065315, -209.7814235418563840 ) ) ;
#202814 = DIRECTION ( 'NONE',  ( -0.000000000000000000, 1.000000000000000000, 6.982962677686267499E-15 ) ) ;
#202815 = AXIS2_PLACEMENT_3D ( 'NONE', #171231, #233735, #211601 ) ;
#202816 = VECTOR ( 'NONE', #98018, 1000.000000000000000 ) ;
#202817 = ADVANCED_FACE ( 'NONE', ( #192013 ), #116299, .T. ) ;
#202818 = CIRCLE ( 'NONE', #181983, 0.09999999999999939493 ) ;
#202819 = ORIENTED_EDGE ( 'NONE', *, *, #4360, .T. ) ;
#202820 = ORIENTED_EDGE ( 'NONE', *, *, #254311, .F. ) ;
#202821 = DIRECTION ( 'NONE',  ( -1.000000000000000000, 0.000000000000000000, 0.000000000000000000 ) ) ;
#202822 = EDGE_CURVE ( 'NONE', #168103, #89874, #27814, .T. ) ;
#202823 = EDGE_CURVE ( 'NONE', #254324, #74301, #12251, .T. ) ;
#202825 = ORIENTED_EDGE ( 'NONE', *, *, #234905, .F. ) ;
#202824 = DIRECTION ( 'NONE',  ( 0.000000000000000000, 0.2617529984165031243, 0.9651348961777157509 ) ) ;
#202826 = CARTESIAN_POINT ( 'NONE',  ( -18.40000000000000213, 64.58541674041282477, -190.8731074845244393 ) ) ;
#202827 = LINE ( 'NONE', #7179, #160881 ) ;
#202828 = DIRECTION ( 'NONE',  ( -1.000000000000000000, -0.000000000000000000, -0.000000000000000000 ) ) ;
#202830 = CARTESIAN_POINT ( 'NONE',  ( -16.87331047859649757, 9.950000000011138823, -188.3499999999999659 ) ) ;
#202829 = DIRECTION ( 'NONE',  ( -0.000000000000000000, 0.000000000000000000, 1.000000000000000000 ) ) ;
#202831 = CARTESIAN_POINT ( 'NONE',  ( 20.95429693346636313, 10.54330487990688958, -108.0608825383130522 ) ) ;
#202832 = DIRECTION ( 'NONE',  ( -1.000000000000000000, 0.000000000000000000, 0.000000000000000000 ) ) ;
#202833 = AXIS2_PLACEMENT_3D ( 'NONE', #212249, #196507, #56978 ) ;
#202834 = AXIS2_PLACEMENT_3D ( 'NONE', #186427, #29929, #31234 ) ;
#202835 = CARTESIAN_POINT ( 'NONE',  ( -23.15000000000000213, 36.65892442174935439, -249.5511627012433848 ) ) ;
#202836 = DIRECTION ( 'NONE',  ( 0.000000000000000000, -1.000000000000000000, 0.000000000000000000 ) ) ;
#202837 = ORIENTED_EDGE ( 'NONE', *, *, #256621, .F. ) ;
#202838 = AXIS2_PLACEMENT_3D ( 'NONE', #166511, #54223, #230298 ) ;
#202839 = ORIENTED_EDGE ( 'NONE', *, *, #111779, .T. ) ;
#202840 = FACE_OUTER_BOUND ( 'NONE', #927, .T. ) ;
#202841 = ORIENTED_EDGE ( 'NONE', *, *, #135616, .F. ) ;
#202842 = CYLINDRICAL_SURFACE ( 'NONE', #11012, 0.1000000000000033362 ) ;
#202843 = B_SPLINE_CURVE_WITH_KNOTS ( 'NONE', 3,
 ( #69958, #209438, #169077, #30837, #110339, #11252 ),
 .UNSPECIFIED., .F., .F.,
 ( 4, 2, 4 ),
 ( 0.000000000000000000, 0.0001497467027049187481, 0.0002994934054098374963 ),
 .UNSPECIFIED. ) ;
#202844 = ORIENTED_EDGE ( 'NONE', *, *, #219451, .F. ) ;
#202845 = CARTESIAN_POINT ( 'NONE',  ( 21.05000000000000071, 1.148907358139439339E-11, -201.0000000000015064 ) ) ;
#202846 = ORIENTED_EDGE ( 'NONE', *, *, #195755, .F. ) ;
#202847 = EDGE_CURVE ( 'NONE', #10056, #99738, #257877, .T. ) ;
#202848 = DIRECTION ( 'NONE',  ( 1.000000000000000000, 3.265361837132813093E-16, -0.000000000000000000 ) ) ;
#202849 = ORIENTED_EDGE ( 'NONE', *, *, #2341, .T. ) ;
#202850 = ORIENTED_EDGE ( 'NONE', *, *, #76155, .F. ) ;
#202851 = CARTESIAN_POINT ( 'NONE',  ( 21.05000000000000071, 67.23127455305841238, -235.8551265064783991 ) ) ;
#202852 = CARTESIAN_POINT ( 'NONE',  ( -21.11101077989000174, 75.98471473109772489, -109.4467922192504403 ) ) ;
#202854 = VERTEX_POINT ( 'NONE', #150308 ) ;
#202853 = DIRECTION ( 'NONE',  ( 1.000000000000000000, 0.000000000000000000, 0.000000000000000000 ) ) ;
#202855 = CARTESIAN_POINT ( 'NONE',  ( 20.84999999999998721, 65.66751761918668251, -97.42826094061121012 ) ) ;
#202857 = ORIENTED_EDGE ( 'NONE', *, *, #173872, .F. ) ;
#202856 = DIRECTION ( 'NONE',  ( 0.000000000000000000, 0.000000000000000000, -1.000000000000000000 ) ) ;
#202858 = CARTESIAN_POINT ( 'NONE',  ( 18.59999999999999076, 10.25000000001115552, -58.25000000000000000 ) ) ;
#202859 = VERTEX_POINT ( 'NONE', #206414 ) ;
#202861 = DIRECTION ( 'NONE',  ( 0.000000000000000000, 0.000000000000000000, 1.000000000000000000 ) ) ;
#202860 = AXIS2_PLACEMENT_3D ( 'NONE', #86839, #225064, #67296 ) ;
#202862 = ADVANCED_FACE ( 'NONE', ( #51160 ), #107307, .F. ) ;
#202864 = ORIENTED_EDGE ( 'NONE', *, *, #6358, .T. ) ;
#202863 = CARTESIAN_POINT ( 'NONE',  ( 23.24999999999999645, 76.00000000001126921, -203.5231074845248997 ) ) ;
#202865 = DIRECTION ( 'NONE',  ( 0.000000000000000000, -1.000000000000000000, 0.000000000000000000 ) ) ;
#202866 = CARTESIAN_POINT ( 'NONE',  ( -12.60829076262180592, 27.26819834643091056, -233.8689871410715853 ) ) ;
#202867 = EDGE_CURVE ( 'NONE', #122792, #38996, #166460, .T. ) ;
#202868 = CARTESIAN_POINT ( 'NONE',  ( 20.99780126800942526, 11.60538868788779432, -60.08735257170526722 ) ) ;
#202869 = AXIS2_PLACEMENT_3D ( 'NONE', #158164, #236365, #180255 ) ;
#202870 = ORIENTED_EDGE ( 'NONE', *, *, #3784, .T. ) ;
#202872 = CARTESIAN_POINT ( 'NONE',  ( -21.10257677756356998, 69.60161825747997000, -203.5480582340924229 ) ) ;
#202871 = CARTESIAN_POINT ( 'NONE',  ( -16.27683809663751191, 60.62847850914942427, -224.4802381816402601 ) ) ;
#202873 = DIRECTION ( 'NONE',  ( 1.000000000000000000, 0.000000000000000000, 0.000000000000000000 ) ) ;
#202874 = CARTESIAN_POINT ( 'NONE',  ( 18.49362639424878196, 85.44260436790082736, -163.2586665510135049 ) ) ;
#202875 = AXIS2_PLACEMENT_3D ( 'NONE', #135048, #52957, #75130 ) ;
#202876 = AXIS2_PLACEMENT_3D ( 'NONE', #232071, #74296, #5584 ) ;
#202877 = DIRECTION ( 'NONE',  ( 0.000000000000000000, 0.8814952561688437216, -0.4721928772777334582 ) ) ;
#202878 = LINE ( 'NONE', #5942, #71872 ) ;
#202879 = EDGE_LOOP ( 'NONE', ( #72753, #223038, #131944, #77575 ) ) ;
#202880 = ORIENTED_EDGE ( 'NONE', *, *, #37310, .T. ) ;
#202881 = ORIENTED_EDGE ( 'NONE', *, *, #100552, .T. ) ;
#202882 = PRODUCT_DEFINITION_FORMATION_WITH_SPECIFIED_SOURCE ( 'ANY', '', #126320, .NOT_KNOWN. ) ;
#202883 = EDGE_CURVE ( 'NONE', #54334, #163312, #72057, .T. ) ;
#202884 = DIRECTION ( 'NONE',  ( 1.000000000000000000, -3.265361837132813093E-16, -2.280189983783949500E-30 ) ) ;
#202885 = AXIS2_PLACEMENT_3D ( 'NONE', #140621, #121102, #139323 ) ;
#202886 = ORIENTED_EDGE ( 'NONE', *, *, #93778, .T. ) ;
#202887 = CARTESIAN_POINT ( 'NONE',  ( 18.49999999999999289, 63.62814136979439184, -224.4990371885399441 ) ) ;
#202888 = ORIENTED_EDGE ( 'NONE', *, *, #235000, .F. ) ;
#202890 = DIRECTION ( 'NONE',  ( 0.000000000000000000, 0.000000000000000000, 1.000000000000000000 ) ) ;
#202889 = AXIS2_PLACEMENT_3D ( 'NONE', #38737, #19159, #96113 ) ;
#202891 = DIRECTION ( 'NONE',  ( -1.000000000000000000, 0.000000000000000000, 0.000000000000000000 ) ) ;
#202892 = ADVANCED_FACE ( 'NONE', ( #207717 ), #191324, .T. ) ;
#202893 = EDGE_CURVE ( 'NONE', #215603, #14186, #228727, .T. ) ;
#202894 = VERTEX_POINT ( 'NONE', #68192 ) ;
#202895 = ADVANCED_FACE ( 'NONE', ( #29109 ), #208980, .T. ) ;
#202896 = CARTESIAN_POINT ( 'NONE',  ( 12.25000000000000000, 9.350000000011140955, -150.7500000000000284 ) ) ;
#202897 = ORIENTED_EDGE ( 'NONE', *, *, #24505, .F. ) ;
#202898 = VERTEX_POINT ( 'NONE', #257049 ) ;
#202899 = AXIS2_PLACEMENT_3D ( 'NONE', #192544, #135109, #38601 ) ;
#202900 = ORIENTED_EDGE ( 'NONE', *, *, #40981, .T. ) ;
#202902 = DIRECTION ( 'NONE',  ( 0.000000000000000000, 0.3896596508880124654, 0.9209589331071350582 ) ) ;
#202901 = CIRCLE ( 'NONE', #161419, 11.65000000000000036 ) ;
#202903 = CARTESIAN_POINT ( 'NONE',  ( -20.94999999999999929, 4.348235979057646361, -245.2768893876484810 ) ) ;
#202904 = LINE ( 'NONE', #227599, #178038 ) ;
#202905 = PLANE ( 'NONE',  #156525 ) ;
#202906 = AXIS2_PLACEMENT_3D ( 'NONE', #66769, #224543, #147583 ) ;
#202907 = DIRECTION ( 'NONE',  ( -1.000000000000000000, -2.952720810173289112E-16, 0.000000000000000000 ) ) ;
#202908 = EDGE_CURVE ( 'NONE', #154129, #148702, #112209, .T. ) ;
#202910 = DIRECTION ( 'NONE',  ( -1.000000000000000000, -3.265361837132813093E-16, 0.000000000000000000 ) ) ;
#202909 = CARTESIAN_POINT ( 'NONE',  ( 20.94999999999999574, 8.366615838327078336, -209.3410474610450365 ) ) ;
#202911 = CARTESIAN_POINT ( 'NONE',  ( 21.05000000000000071, 60.98273731152020360, -225.3658424485014109 ) ) ;
#202913 = ORIENTED_EDGE ( 'NONE', *, *, #114639, .T. ) ;
#202912 = DIRECTION ( 'NONE',  ( -1.000000000000000000, 0.000000000000000000, 0.000000000000000000 ) ) ;
#202915 = DIRECTION ( 'NONE',  ( 1.000000000000000000, -0.000000000000000000, -0.000000000000000000 ) ) ;
#202914 = CARTESIAN_POINT ( 'NONE',  ( -23.25000000000000000, 68.29137419664525055, -231.9463301769586394 ) ) ;
#202916 = TOROIDAL_SURFACE ( 'NONE', #227854, 4.150000000000000355, 0.1000000000000000056 ) ;
#202917 = CARTESIAN_POINT ( 'NONE',  ( -22.50000000000000000, 67.13476106344063510, -235.8289512066367024 ) ) ;
#202918 = VERTEX_POINT ( 'NONE', #38075 ) ;
#202919 = LINE ( 'NONE', #122109, #225250 ) ;
#202920 = FACE_OUTER_BOUND ( 'NONE', #36053, .T. ) ;
#202921 = FACE_OUTER_BOUND ( 'NONE', #205617, .T. ) ;
#202922 = ORIENTED_EDGE ( 'NONE', *, *, #193242, .F. ) ;
#202923 = CARTESIAN_POINT ( 'NONE',  ( 21.11927991906888025, 69.55150688152127714, -203.5321911639982773 ) ) ;
#202924 = CARTESIAN_POINT ( 'NONE',  ( -23.39999999999994529, 74.16448838626247664, -47.52760213295649550 ) ) ;
#202925 = AXIS2_PLACEMENT_3D ( 'NONE', #207496, #182797, #206193 ) ;
#202927 = EDGE_LOOP ( 'NONE', ( #254129, #129885, #208808, #73282 ) ) ;
#202926 = CIRCLE ( 'NONE', #148781, 11.65000000000000213 ) ;
#202928 = ORIENTED_EDGE ( 'NONE', *, *, #167212, .T. ) ;
#202929 = LINE ( 'NONE', #199084, #215781 ) ;
#202930 = ORIENTED_EDGE ( 'NONE', *, *, #230843, .T. ) ;
#202931 = DIRECTION ( 'NONE',  ( 0.000000000000000000, 0.000000000000000000, 1.000000000000000000 ) ) ;
#202932 = CARTESIAN_POINT ( 'NONE',  ( -18.46154800491012082, -9.480206274230850383, -174.1574508383815214 ) ) ;
#202933 = PLANE ( 'NONE',  #57346 ) ;
#202934 = FACE_OUTER_BOUND ( 'NONE', #129651, .T. ) ;
#202935 = ORIENTED_EDGE ( 'NONE', *, *, #146295, .F. ) ;
#202936 = DIRECTION ( 'NONE',  ( 1.000000000000000000, 0.000000000000000000, 0.000000000000000000 ) ) ;
#202937 = CIRCLE ( 'NONE', #48810, 0.09999999999999108213 ) ;
#202938 = LINE ( 'NONE', #245928, #70887 ) ;
#202939 = CARTESIAN_POINT ( 'NONE',  ( 18.56308993302939925, 10.38069115533503961, -192.2392226389382301 ) ) ;
#202940 = LINE ( 'NONE', #82957, #57432 ) ;
#202941 = ADVANCED_FACE ( 'NONE', ( #215401 ), #78450, .T. ) ;
#202942 = VERTEX_POINT ( 'NONE', #15955 ) ;
#202943 = ORIENTED_EDGE ( 'NONE', *, *, #110636, .T. ) ;
#202944 = DIRECTION ( 'NONE',  ( -0.000000000000000000, -0.8814952561688430555, 0.4721928772777346239 ) ) ;
#202945 = CARTESIAN_POINT ( 'NONE',  ( -18.79999999999999716, 1.885425182446134107, -11.59641995933507808 ) ) ;
#202946 = EDGE_CURVE ( 'NONE', #53100, #27906, #253235, .T. ) ;
#202947 = DIRECTION ( 'NONE',  ( -0.000000000000000000, 0.01283462868039629209, -0.9999176327611372095 ) ) ;
#202948 = DIRECTION ( 'NONE',  ( 0.000000000000000000, -0.1350103645451876666, 0.9908441862701600211 ) ) ;
#202949 = AXIS2_PLACEMENT_3D ( 'NONE', #205015, #227167, #26424 ) ;
#202950 = DIRECTION ( 'NONE',  ( 2.840903330521631775E-16, -0.8700118002898321601, 0.4930308989875230585 ) ) ;
#202951 = PLANE ( 'NONE',  #19730 ) ;
#202953 = ORIENTED_EDGE ( 'NONE', *, *, #228094, .F. ) ;
#202952 = CIRCLE ( 'NONE', #236276, 12.77499999999999858 ) ;
#202954 = CARTESIAN_POINT ( 'NONE',  ( 20.97239005616515328, 61.87236729066745511, -221.7090595676594944 ) ) ;
#202955 = CARTESIAN_POINT ( 'NONE',  ( -16.77732147278574715, 9.945966932584589415, -146.6635087568758422 ) ) ;
#202956 = ADVANCED_FACE ( 'NONE', ( #36807 ), #95453, .T. ) ;
#202958 = EDGE_CURVE ( 'NONE', #90836, #67070, #145488, .T. ) ;
#202957 = AXIS2_PLACEMENT_3D ( 'NONE', #222786, #104119, #123715 ) ;
#202959 = VECTOR ( 'NONE', #119541, 1000.000000000000000 ) ;
#202960 = CARTESIAN_POINT ( 'NONE',  ( -18.50000000000000000, 65.50527602196416410, -248.6645148362614748 ) ) ;
#202961 = DIRECTION ( 'NONE',  ( 0.000000000000000000, 0.000000000000000000, 1.000000000000000000 ) ) ;
#202962 = CARTESIAN_POINT ( 'NONE',  ( 18.59999999999999076, 19.00443933019177578, -232.7770257915295531 ) ) ;
#202963 = DIRECTION ( 'NONE',  ( 0.000000000000000000, -0.9910465087640866200, 0.1335171055202867274 ) ) ;
#202964 = CIRCLE ( 'NONE', #94620, 0.1000000000000028644 ) ;
#202965 = VERTEX_POINT ( 'NONE', #175049 ) ;
#202966 = ORIENTED_EDGE ( 'NONE', *, *, #241089, .T. ) ;
#202967 = CARTESIAN_POINT ( 'NONE',  ( -21.55000000000000426, 7.708578643773852157, -155.2500000000000284 ) ) ;
#202968 = CARTESIAN_POINT ( 'NONE',  ( 21.05000000000000071, 76.00000000001247713, -172.9231074845243654 ) ) ;
#202969 = CARTESIAN_POINT ( 'NONE',  ( 20.96077737575322431, 17.02684875966464872, -224.5570219545472810 ) ) ;
#202970 = EDGE_CURVE ( 'NONE', #109854, #107334, #197114, .T. ) ;
#202971 = EDGE_LOOP ( 'NONE', ( #4132, #200870, #54930, #144835, #142709 ) ) ;
#202972 = CARTESIAN_POINT ( 'NONE',  ( -16.87683809663752399, 66.15000000001188596, -90.37310748452438247 ) ) ;
#202973 = EDGE_CURVE ( 'NONE', #256102, #136922, #70525, .T. ) ;
#202974 = LINE ( 'NONE', #179588, #67740 ) ;
#202975 = VECTOR ( 'NONE', #151044, 1000.000000000000000 ) ;
#202976 = FACE_BOUND ( 'NONE', #86786, .T. ) ;
#202977 = DIRECTION ( 'NONE',  ( -1.000000000000000000, -7.304098846218134667E-16, 4.217023435051678980E-16 ) ) ;
#202978 = VECTOR ( 'NONE', #10614, 1000.000000000000000 ) ;
#202979 = ORIENTED_EDGE ( 'NONE', *, *, #198119, .F. ) ;
#202980 = CARTESIAN_POINT ( 'NONE',  ( -18.50000000000000000, 77.16412189325258453, -28.10825939895270764 ) ) ;
#202981 = EDGE_CURVE ( 'NONE', #63725, #122081, #141226, .T. ) ;
#202982 = ORIENTED_EDGE ( 'NONE', *, *, #152545, .T. ) ;
#202983 = ADVANCED_FACE ( 'NONE', ( #155476, #234979 ), #176305, .T. ) ;
#202984 = DIRECTION ( 'NONE',  ( 0.000000000000000000, -0.8814952561688430555, 0.4721928772777346239 ) ) ;
#202985 = EDGE_CURVE ( 'NONE', #39467, #154121, #162091, .T. ) ;
#202986 = CARTESIAN_POINT ( 'NONE',  ( 20.94999999999999574, 77.83534155023598089, -57.96795619196132776 ) ) ;
#202987 = CARTESIAN_POINT ( 'NONE',  ( -21.05000000000000071, 1.148907358139439339E-11, -201.0000000000015064 ) ) ;
#202988 = DIRECTION ( 'NONE',  ( 1.000000000000000000, 0.000000000000000000, 0.000000000000000000 ) ) ;
#202989 = CARTESIAN_POINT ( 'NONE',  ( 18.59999999999999076, 10.49142135624846439, -192.2499999999999716 ) ) ;
#202990 = CARTESIAN_POINT ( 'NONE',  ( -23.25000000000000000, 76.00000000001173817, -73.42310748452430857 ) ) ;
#202991 = CARTESIAN_POINT ( 'NONE',  ( 23.40000000000005542, 87.50449464844290048, -37.85861909827351468 ) ) ;
#202992 = CARTESIAN_POINT ( 'NONE',  ( 20.94999999999999929, 1.115600667400684642E-11, -167.5000000000000284 ) ) ;
#202993 = CARTESIAN_POINT ( 'NONE',  ( -16.87683809663752399, 9.949999999999986855, -12.65000000000000213 ) ) ;
#202994 = B_SPLINE_CURVE_WITH_KNOTS ( 'NONE', 3,
 ( #111574, #170307, #249796, #230228, #47723, #188535, #127281, #150698, #191134, #28216 ),
 .UNSPECIFIED., .F., .F.,
 ( 4, 3, 3, 4 ),
 ( 7.632826238673810152E-06, 4.756916949875324721E-05, 9.484459048150249510E-05, 0.0001435500935099965052 ),
 .UNSPECIFIED. ) ;
#202996 = EDGE_CURVE ( 'NONE', #245998, #122770, #113734, .T. ) ;
#202995 = DIRECTION ( 'NONE',  ( 1.000000000000000000, -0.000000000000000000, -0.000000000000000000 ) ) ;
#202997 = AXIS2_PLACEMENT_3D ( 'NONE', #218980, #179883, #255497 ) ;
#202998 = AXIS2_PLACEMENT_3D ( 'NONE', #205809, #105390, #184967 ) ;
#202999 = AXIS2_PLACEMENT_3D ( 'NONE', #53483, #251677, #73085 ) ;
#203000 = DIRECTION ( 'NONE',  ( -1.000000000000000000, 2.952720810173289112E-16, 2.061873921506763405E-30 ) ) ;
#203001 = CARTESIAN_POINT ( 'NONE',  ( 20.95512820512820440, 8.876151316299273120, -176.0586289951409071 ) ) ;
#203002 = ORIENTED_EDGE ( 'NONE', *, *, #48487, .T. ) ;
#203003 = CARTESIAN_POINT ( 'NONE',  ( 18.42636655943171675, 85.49694431578275555, -129.9140269133687866 ) ) ;
#203004 = SPHERICAL_SURFACE ( 'NONE', #79437, 0.1000000000000000056 ) ;
#203005 = VERTEX_POINT ( 'NONE', #97997 ) ;
#203006 = CARTESIAN_POINT ( 'NONE',  ( 23.14999999999999858, 71.22429906543310096, -181.8718755885703615 ) ) ;
#203007 = CARTESIAN_POINT ( 'NONE',  ( 21.05095171578076574, 67.22382012124126049, -157.8572342078865347 ) ) ;
#203008 = EDGE_CURVE ( 'NONE', #28626, #34288, #224600, .T. ) ;
#203009 = FACE_OUTER_BOUND ( 'NONE', #136138, .T. ) ;
#203010 = ORIENTED_EDGE ( 'NONE', *, *, #25504, .T. ) ;
#203011 = VECTOR ( 'NONE', #168164, 1000.000000000000000 ) ;
#203012 = CARTESIAN_POINT ( 'NONE',  ( -18.59999999999999787, 77.36242903720516040, -95.13422623660308375 ) ) ;
#203013 = CIRCLE ( 'NONE', #90582, 4.149999999999993250 ) ;
#203014 = ORIENTED_EDGE ( 'NONE', *, *, #131614, .F. ) ;
#203015 = CIRCLE ( 'NONE', #65650, 2.000000000000001776 ) ;
#203016 = ORIENTED_EDGE ( 'NONE', *, *, #156821, .F. ) ;
#203017 = DIRECTION ( 'NONE',  ( -3.265361837132813093E-16, 1.000000000000000000, 0.000000000000000000 ) ) ;
#203018 = ADVANCED_FACE ( 'NONE', ( #134560 ), #177600, .T. ) ;
#203019 = VERTEX_POINT ( 'NONE', #73358 ) ;
#203020 = DIRECTION ( 'NONE',  ( 1.000000000000000000, 0.000000000000000000, 0.000000000000000000 ) ) ;
#203021 = CARTESIAN_POINT ( 'NONE',  ( 22.49999999999999645, 0.1008583691098678403, -21.75043287651060808 ) ) ;
#203022 = FACE_OUTER_BOUND ( 'NONE', #116904, .T. ) ;
#203023 = CARTESIAN_POINT ( 'NONE',  ( -23.25000000000000000, 1.115600667400684642E-11, -138.1500000000000057 ) ) ;
#203024 = ADVANCED_FACE ( 'NONE', ( #152900 ), #49638, .F. ) ;
#203025 = DIRECTION ( 'NONE',  ( 0.000000000000000000, -0.9887567792719341719, -0.1495327102803664099 ) ) ;
#203026 = CARTESIAN_POINT ( 'NONE',  ( -16.87683809663750623, 66.05000000001230376, -156.6207434663279230 ) ) ;
#203027 = CARTESIAN_POINT ( 'NONE',  ( 21.05000000000000071, 76.00000000001143974, -37.92310748452432989 ) ) ;
#203028 = CARTESIAN_POINT ( 'NONE',  ( 21.00000000000000000, 66.25000000001179501, -81.77310748452437394 ) ) ;
#203029 = DIRECTION ( 'NONE',  ( 0.000000000000000000, 0.000000000000000000, 1.000000000000000000 ) ) ;
#203031 = VERTEX_POINT ( 'NONE', #34233 ) ;
#203030 = LINE ( 'NONE', #102624, #65297 ) ;
#203032 = ORIENTED_EDGE ( 'NONE', *, *, #118359, .T. ) ;
#203034 = CARTESIAN_POINT ( 'NONE',  ( 23.24999999999999645, 20.83093076766827423, -227.7429161672744442 ) ) ;
#203033 = DIRECTION ( 'NONE',  ( 1.000000000000000000, 0.000000000000000000, 0.000000000000000000 ) ) ;
#203036 = EDGE_LOOP ( 'NONE', ( #18956, #42476 ) ) ;
#203035 = CARTESIAN_POINT ( 'NONE',  ( -16.82055514392408213, 60.94637224242198670, -221.0158639786953358 ) ) ;
#203037 = AXIS2_PLACEMENT_3D ( 'NONE', #19779, #21076, #138391 ) ;
#203038 = EDGE_LOOP ( 'NONE', ( #54942, #3755, #216179, #54852 ) ) ;
#203039 = DIRECTION ( 'NONE',  ( 1.000000000000000000, 2.670994536826046953E-16, 9.848483305199541222E-16 ) ) ;
#203041 = CARTESIAN_POINT ( 'NONE',  ( -22.39999999999999858, 1.115600667400684642E-11, -133.9000000000000057 ) ) ;
#203040 = CIRCLE ( 'NONE', #78138, 0.09999999999999938105 ) ;
#203042 = EDGE_CURVE ( 'NONE', #64464, #243852, #237088, .T. ) ;
#203043 = EDGE_CURVE ( 'NONE', #200038, #49697, #133047, .T. ) ;
#203044 = DIRECTION ( 'NONE',  ( 0.000000000000000000, 0.000000000000000000, -1.000000000000000000 ) ) ;
#203045 = DIRECTION ( 'NONE',  ( -1.000000000000000000, 0.000000000000000000, -0.000000000000000000 ) ) ;
#203047 = DIRECTION ( 'NONE',  ( 1.000000000000000000, 0.000000000000000000, 0.000000000000000000 ) ) ;
#203046 = AXIS2_PLACEMENT_3D ( 'NONE', #142657, #141387, #117981 ) ;
#203048 = DIRECTION ( 'NONE',  ( -0.000000000000000000, 0.8814952561688430555, -0.4721928772777346239 ) ) ;
#203049 = DIRECTION ( 'NONE',  ( -1.000000000000000000, 7.049440681616512959E-16, -1.911869773728122357E-16 ) ) ;
#203051 = ORIENTED_EDGE ( 'NONE', *, *, #152545, .F. ) ;
#203050 = EDGE_CURVE ( 'NONE', #160572, #197727, #178889, .T. ) ;
#203052 = ORIENTED_EDGE ( 'NONE', *, *, #177305, .F. ) ;
#203053 = DIRECTION ( 'NONE',  ( -1.000000000000000000, 0.000000000000000000, 0.000000000000000000 ) ) ;
#203054 = CIRCLE ( 'NONE', #82228, 0.1999999999999987899 ) ;
#203055 = AXIS2_PLACEMENT_3D ( 'NONE', #122377, #106630, #2400 ) ;
#203056 = ORIENTED_EDGE ( 'NONE', *, *, #127990, .F. ) ;
#203057 = DIRECTION ( 'NONE',  ( -0.000000000000000000, 0.9770955615653313941, 0.2128009952263603954 ) ) ;
#203059 = EDGE_CURVE ( 'NONE', #199909, #141516, #166381, .T. ) ;
#203058 = ORIENTED_EDGE ( 'NONE', *, *, #140857, .F. ) ;
#203061 = LINE ( 'NONE', #27030, #205705 ) ;
#203060 = CIRCLE ( 'NONE', #90624, 0.09999999999999939493 ) ;
#203062 = CARTESIAN_POINT ( 'NONE',  ( -23.25000000000000355, 5.650000000011139001, -113.1500000000000341 ) ) ;
#203063 = EDGE_CURVE ( 'NONE', #142144, #253366, #45753, .T. ) ;
#203064 = AXIS2_PLACEMENT_3D ( 'NONE', #11142, #95786, #93231 ) ;
#203065 = CARTESIAN_POINT ( 'NONE',  ( 21.08489834409762054, 10.62232389474667293, -146.3499999999999659 ) ) ;
#203066 = FACE_OUTER_BOUND ( 'NONE', #114184, .T. ) ;
#203067 = ORIENTED_EDGE ( 'NONE', *, *, #47040, .F. ) ;
#203068 = LINE ( 'NONE', #106514, #225345 ) ;
#203069 = ORIENTED_EDGE ( 'NONE', *, *, #59714, .T. ) ;
#203070 = CARTESIAN_POINT ( 'NONE',  ( 22.48508240969612615, 0.04627641452807085970, -122.3499892684264552 ) ) ;
#203071 = DIRECTION ( 'NONE',  ( -1.000000000000000000, 0.000000000000000000, 0.000000000000000000 ) ) ;
#203072 = EDGE_CURVE ( 'NONE', #229726, #14256, #220548, .T. ) ;
#203073 = FACE_OUTER_BOUND ( 'NONE', #251705, .T. ) ;
#203074 = FACE_OUTER_BOUND ( 'NONE', #92401, .T. ) ;
#203076 = EDGE_LOOP ( 'NONE', ( #248513, #133512, #231196, #84666 ) ) ;
#203075 = EDGE_CURVE ( 'NONE', #147359, #187000, #143572, .T. ) ;
#203077 = CARTESIAN_POINT ( 'NONE',  ( -20.94999999999999929, 64.25000000001189449, -96.00830171387038092 ) ) ;
#203078 = ORIENTED_EDGE ( 'NONE', *, *, #51186, .F. ) ;
#203081 = ORIENTED_EDGE ( 'NONE', *, *, #79613, .F. ) ;
#203080 = CARTESIAN_POINT ( 'NONE',  ( 18.59999999999999432, -9.480686695267811714, -107.4411151687579036 ) ) ;
#203079 = CARTESIAN_POINT ( 'NONE',  ( 18.46947024752492084, 46.92278096310428026, -255.3730018242404469 ) ) ;
#203082 = CARTESIAN_POINT ( 'NONE',  ( 21.05000000000000071, 18.71396320652088718, -229.9379713345707614 ) ) ;
#203083 = CIRCLE ( 'NONE', #157141, 0.09999999999999939493 ) ;
#203084 = EDGE_LOOP ( 'NONE', ( #21816, #124568, #162746, #187854 ) ) ;
#203085 = CIRCLE ( 'NONE', #174095, 0.09999999999999939493 ) ;
#203086 = DIRECTION ( 'NONE',  ( 0.000000000000000000, -1.000000000000000000, -6.860497997771532351E-15 ) ) ;
#203087 = ORIENTED_EDGE ( 'NONE', *, *, #228860, .T. ) ;
#203089 = AXIS2_PLACEMENT_3D ( 'NONE', #255993, #39609, #240353 ) ;
#203088 = CARTESIAN_POINT ( 'NONE',  ( -16.94107738177415712, 65.98576071487568129, -157.4731074845244336 ) ) ;
#203090 = MECHANICAL_DESIGN_GEOMETRIC_PRESENTATION_REPRESENTATION (  '', ( #136421 ), #190648 ) ;
#203091 = DIRECTION ( 'NONE',  ( 1.000000000000000000, 0.000000000000000000, 0.000000000000000000 ) ) ;
#203092 = ADVANCED_FACE ( 'NONE', ( #139700 ), #141020, .T. ) ;
#203093 = AXIS2_PLACEMENT_3D ( 'NONE', #69058, #112029, #27386 ) ;
#203094 = DIRECTION ( 'NONE',  ( 0.000000000000000000, 0.9651348961777157509, -0.2617529984165031243 ) ) ;
#203095 = UNCERTAINTY_MEASURE_WITH_UNIT (LENGTH_MEASURE( 1.000000000000000082E-05 ), #48959, 'distance_accuracy_value', 'NONE');
#203096 = EDGE_CURVE ( 'NONE', #187671, #235449, #35748, .T. ) ;
#203097 = CARTESIAN_POINT ( 'NONE',  ( -18.60000000000000853, -9.364240527579749340, -74.18024858184081438 ) ) ;
#203098 = CARTESIAN_POINT ( 'NONE',  ( -20.54999999999999716, -3.444512620907437039, -226.2123967847655592 ) ) ;
#203099 = ORIENTED_EDGE ( 'NONE', *, *, #108436, .F. ) ;
#203100 = CARTESIAN_POINT ( 'NONE',  ( 5.551115123125782702E-14, 64.75000000001119815, -22.12310748452479103 ) ) ;
#203101 = FACE_OUTER_BOUND ( 'NONE', #248717, .T. ) ;
#203102 = CARTESIAN_POINT ( 'NONE',  ( 23.15000000000000213, 52.55093873171406216, -255.3069320826340061 ) ) ;
#203103 = AXIS2_PLACEMENT_3D ( 'NONE', #94468, #33262, #34533 ) ;
#203104 = VERTEX_POINT ( 'NONE', #2760 ) ;
#203105 = CYLINDRICAL_SURFACE ( 'NONE', #213356, 0.1000000000000033362 ) ;
#203107 = ORIENTED_EDGE ( 'NONE', *, *, #145470, .T. ) ;
#203106 = TOROIDAL_SURFACE ( 'NONE', #61646, 0.4000000000000009104, 0.1000000000000000056 ) ;
#203109 = CIRCLE ( 'NONE', #228071, 0.1000000000000028644 ) ;
#203108 = DIRECTION ( 'NONE',  ( 1.000000000000000000, 0.000000000000000000, 0.000000000000000000 ) ) ;
#203110 = DIRECTION ( 'NONE',  ( 0.000000000000000000, 0.000000000000000000, 1.000000000000000000 ) ) ;
#203112 = VERTEX_POINT ( 'NONE', #4057 ) ;
#203111 = CARTESIAN_POINT ( 'NONE',  ( -16.89155683852559164, 44.70802594024834775, -235.0424388436548213 ) ) ;
#203113 = FACE_OUTER_BOUND ( 'NONE', #133412, .T. ) ;
#203114 = CARTESIAN_POINT ( 'NONE',  ( -15.75000000000000355, 62.59162599727320497, -217.2417264603073477 ) ) ;
#203115 = CIRCLE ( 'NONE', #153095, 0.2000000000000057288 ) ;
#203116 = DIRECTION ( 'NONE',  ( 0.000000000000000000, 0.9667078373770112698, 0.2558827019434133376 ) ) ;
#203117 = VECTOR ( 'NONE', #135514, 1000.000000000000000 ) ;
#203118 = ORIENTED_EDGE ( 'NONE', *, *, #78815, .T. ) ;
#203119 = CARTESIAN_POINT ( 'NONE',  ( -20.64999999999999858, 54.27339256631721298, -236.8935360681107625 ) ) ;
#203120 = CYLINDRICAL_SURFACE ( 'NONE', #81573, 11.75000000000000533 ) ;
#203121 = AXIS2_PLACEMENT_3D ( 'NONE', #33051, #70875, #250754 ) ;
#203122 = ORIENTED_EDGE ( 'NONE', *, *, #210810, .F. ) ;
#203123 = CARTESIAN_POINT ( 'NONE',  ( 22.57320508075688537, 64.25000000001236344, -170.0231074845244450 ) ) ;
#203124 = EDGE_CURVE ( 'NONE', #115688, #197537, #233008, .T. ) ;
#203125 = ORIENTED_EDGE ( 'NONE', *, *, #245753, .T. ) ;
#203126 = CIRCLE ( 'NONE', #119765, 0.1999999999999945155 ) ;
#203127 = CARTESIAN_POINT ( 'NONE',  ( -16.80100426158790938, 44.16834856606528348, -235.2917130533355135 ) ) ;
#203129 = ORIENTED_EDGE ( 'NONE', *, *, #87891, .F. ) ;
#203128 = CARTESIAN_POINT ( 'NONE',  ( -21.55000000000000426, 65.31373032403179479, -213.3174242249740189 ) ) ;
#203130 = AXIS2_PLACEMENT_3D ( 'NONE', #257594, #39925, #195147 ) ;
#203133 = ORIENTED_EDGE ( 'NONE', *, *, #34121, .T. ) ;
#203132 = EDGE_LOOP ( 'NONE', ( #254377, #209376, #35981, #99002 ) ) ;
#203131 = CARTESIAN_POINT ( 'NONE',  ( -21.65000000000000213, 9.950000000011140600, -180.1499999999999773 ) ) ;
#203134 = CARTESIAN_POINT ( 'NONE',  ( -21.56666275994539816, 30.30957806568256885, -252.3955916421750203 ) ) ;
#203135 = CIRCLE ( 'NONE', #107467, 0.09999999999998898659 ) ;
#203136 = LINE ( 'NONE', #104011, #14947 ) ;
#203137 = AXIS2_PLACEMENT_3D ( 'NONE', #149070, #147775, #113765 ) ;
#203138 = DIRECTION ( 'NONE',  ( 0.000000000000000000, -1.000000000000000000, -6.982962677686267499E-15 ) ) ;
#203139 = VECTOR ( 'NONE', #65786, 1000.000000000000000 ) ;
#203141 = CARTESIAN_POINT ( 'NONE',  ( -18.59999999999999787, 66.65000000001229807, -157.7731074845244166 ) ) ;
#203140 = CARTESIAN_POINT ( 'NONE',  ( 22.41477678272288188, 0.0008238657741001872850, -88.85041471548463221 ) ) ;
#203143 = EDGE_CURVE ( 'NONE', #250290, #188385, #52378, .T. ) ;
#203142 = DIRECTION ( 'NONE',  ( -0.000000000000000000, 0.01283462868039629209, -0.9999176327611372095 ) ) ;
#203144 = CARTESIAN_POINT ( 'NONE',  ( -22.60000000000081144, 25.91621687215759806, -254.3113673292270391 ) ) ;
#203145 = CIRCLE ( 'NONE', #173983, 0.3999999999999975797 ) ;
#203146 = PLANE ( 'NONE',  #192531 ) ;
#203147 = CARTESIAN_POINT ( 'NONE',  ( -22.50000000000000000, 7.790779598384560245, -66.90000000000004832 ) ) ;
#203148 = ORIENTED_EDGE ( 'NONE', *, *, #174858, .T. ) ;
#203149 = ORIENTED_EDGE ( 'NONE', *, *, #94403, .T. ) ;
#203150 = CARTESIAN_POINT ( 'NONE',  ( 21.13461538461538325, 65.38541703798651383, -124.1731074845243654 ) ) ;
#203152 = ORIENTED_EDGE ( 'NONE', *, *, #192162, .F. ) ;
#203151 = DIRECTION ( 'NONE',  ( 0.000000000000000000, -0.1350103645451876944, 0.9908441862701601321 ) ) ;
#203153 = ORIENTED_EDGE ( 'NONE', *, *, #73235, .F. ) ;
#203154 = DIRECTION ( 'NONE',  ( 1.186688945009010077E-16, 1.000000000000000000, 6.982962677686266711E-15 ) ) ;
#203155 = ORIENTED_EDGE ( 'NONE', *, *, #137362, .F. ) ;
#203156 = CARTESIAN_POINT ( 'NONE',  ( -21.05000000000000071, 69.45934304831089889, -136.5231074845243313 ) ) ;
#203157 = ORIENTED_EDGE ( 'NONE', *, *, #77677, .T. ) ;
#203158 = DIRECTION ( 'NONE',  ( -1.000000000000000000, -0.000000000000000000, 0.000000000000000000 ) ) ;
#203159 = DIRECTION ( 'NONE',  ( 0.000000000000000000, 0.9651348961777157509, -0.2617529984165031243 ) ) ;
#203160 = VECTOR ( 'NONE', #148531, 1000.000000000000114 ) ;
#203162 = ORIENTED_EDGE ( 'NONE', *, *, #127616, .F. ) ;
#203161 = ORIENTED_EDGE ( 'NONE', *, *, #55787, .T. ) ;
#203163 = ORIENTED_EDGE ( 'NONE', *, *, #65223, .F. ) ;
#203164 = CARTESIAN_POINT ( 'NONE',  ( -18.50000000000000000, 6.846123162363745074, -70.73772626684986164 ) ) ;
#203165 = ORIENTED_EDGE ( 'NONE', *, *, #68647, .T. ) ;
#203166 = ORIENTED_EDGE ( 'NONE', *, *, #13681, .F. ) ;
#203167 = DIRECTION ( 'NONE',  ( 1.000000000000000000, -0.000000000000000000, 0.000000000000000000 ) ) ;
#203168 = CARTESIAN_POINT ( 'NONE',  ( 18.43709777086140278, -9.682403433465236020, -73.65684337741278398 ) ) ;
#203170 = ORIENTED_EDGE ( 'NONE', *, *, #144185, .F. ) ;
#203169 = CARTESIAN_POINT ( 'NONE',  ( 18.37172112093850274, -9.570961652232023553, -107.3167344534833916 ) ) ;
#203172 = DIRECTION ( 'NONE',  ( 0.000000000000000000, -0.9875055080513754913, 0.1575844902526733482 ) ) ;
#203171 = CYLINDRICAL_SURFACE ( 'NONE', #99011, 11.80000000000000426 ) ;
#203173 = FACE_OUTER_BOUND ( 'NONE', #198654, .T. ) ;
#203175 = ORIENTED_EDGE ( 'NONE', *, *, #181564, .T. ) ;
#203174 = CARTESIAN_POINT ( 'NONE',  ( 18.39999999999999503, 64.25000000001224976, -149.1731074845244507 ) ) ;
#203176 = CARTESIAN_POINT ( 'NONE',  ( -18.50000000000000000, 7.021664781911246322, -171.1335654018973003 ) ) ;
#203177 = ORIENTED_EDGE ( 'NONE', *, *, #252883, .T. ) ;
#203178 = DIRECTION ( 'NONE',  ( 0.000000000000000000, 0.000000000000000000, 1.000000000000000000 ) ) ;
#203179 = ORIENTED_EDGE ( 'NONE', *, *, #83397, .T. ) ;
#203180 = DIRECTION ( 'NONE',  ( -3.265361837132812600E-16, 0.9770955615653313941, 0.2128009952263603677 ) ) ;
#203181 = FACE_OUTER_BOUND ( 'NONE', #189353, .T. ) ;
#203182 = EDGE_CURVE ( 'NONE', #215277, #203821, #242664, .T. ) ;
#203183 = ORIENTED_EDGE ( 'NONE', *, *, #190902, .F. ) ;
#203184 = CIRCLE ( 'NONE', #53166, 0.09999999999998898659 ) ;
#203185 = CIRCLE ( 'NONE', #190755, 2.000000000000001776 ) ;
#203186 = CARTESIAN_POINT ( 'NONE',  ( 21.15000000000005187, 76.00000000001119815, -36.02310748452479316 ) ) ;
#203187 = CIRCLE ( 'NONE', #182359, 0.09999999999999939493 ) ;
#203188 = DIRECTION ( 'NONE',  ( 0.000000000000000000, -0.8454177738465993297, -0.5341055959866553016 ) ) ;
#203189 = CARTESIAN_POINT ( 'NONE',  ( -12.93407622233968191, 12.47014700295942369, -214.0015173037735678 ) ) ;
#203190 = VERTEX_POINT ( 'NONE', #61474 ) ;
#203191 = ORIENTED_EDGE ( 'NONE', *, *, #105184, .T. ) ;
#203192 = EDGE_CURVE ( 'NONE', #242283, #91307, #74809, .T. ) ;
#203193 = CARTESIAN_POINT ( 'NONE',  ( 21.97500000000000497, 43.85220609964365224, -235.6449878604632886 ) ) ;
#203194 = CARTESIAN_POINT ( 'NONE',  ( -23.25000000000000000, 1.115600667400684642E-11, -100.5000000000000426 ) ) ;
#203195 = ORIENTED_EDGE ( 'NONE', *, *, #179764, .T. ) ;
#203196 = CARTESIAN_POINT ( 'NONE',  ( 23.15000000000000213, 87.65000000001215597, -139.6231074845242688 ) ) ;
#203197 = ORIENTED_EDGE ( 'NONE', *, *, #14933, .F. ) ;
#203198 = DIRECTION ( 'NONE',  ( 1.000000000000000000, 0.000000000000000000, 0.000000000000000000 ) ) ;
#203199 = CARTESIAN_POINT ( 'NONE',  ( 21.02374657821587434, 64.39999999919200491, -143.4513107143263824 ) ) ;
#203201 = CARTESIAN_POINT ( 'NONE',  ( -18.59999999999999787, 59.16775194334852728, -221.0793150863668473 ) ) ;
#203200 = CARTESIAN_POINT ( 'NONE',  ( -23.15000000000000213, 64.25000000001206502, -124.2731074845243882 ) ) ;
#203202 = ADVANCED_FACE ( 'NONE', ( #100558 ), #79721, .F. ) ;
#203203 = CARTESIAN_POINT ( 'NONE',  ( 22.47809213839789066, 0.03753706763967752658, -55.35002666521224057 ) ) ;
#203204 = DIRECTION ( 'NONE',  ( 0.000000000000000000, 6.982962677686267499E-15, -1.000000000000000000 ) ) ;
#203205 = ORIENTED_EDGE ( 'NONE', *, *, #65877, .T. ) ;
#203206 = AXIS2_PLACEMENT_3D ( 'NONE', #229950, #50026, #68316 ) ;
#203207 = ADVANCED_FACE ( 'NONE', ( #24934 ), #104419, .T. ) ;
#203208 = DIRECTION ( 'NONE',  ( -0.000000000000000000, 0.2617529984165031243, 0.9651348961777157509 ) ) ;
#203210 = VERTEX_POINT ( 'NONE', #164433 ) ;
#203209 = ORIENTED_EDGE ( 'NONE', *, *, #15092, .T. ) ;
#203211 = AXIS2_PLACEMENT_3D ( 'NONE', #54678, #250318, #53403 ) ;
#203212 = ORIENTED_EDGE ( 'NONE', *, *, #100074, .T. ) ;
#203213 = ORIENTED_EDGE ( 'NONE', *, *, #185958, .F. ) ;
#203214 = CARTESIAN_POINT ( 'NONE',  ( -16.90257928357874206, 66.04589317890692257, -157.3868220544107430 ) ) ;
#203215 = DIRECTION ( 'NONE',  ( -1.000000000000000000, 0.000000000000000000, 0.000000000000000000 ) ) ;
#203216 = DIRECTION ( 'NONE',  ( 0.000000000000000000, 0.2128009952263611726, -0.9770955615653312831 ) ) ;
#203217 = DIRECTION ( 'NONE',  ( 0.000000000000000000, -0.8660254037844384856, 0.5000000000000002220 ) ) ;
#203218 = CARTESIAN_POINT ( 'NONE',  ( 19.90000000000000568, 1.350000000000000089, 16.60000000000000142 ) ) ;
#203219 = EDGE_CURVE ( 'NONE', #29923, #8334, #165729, .T. ) ;
#203220 =( BOUNDED_CURVE ( )  B_SPLINE_CURVE ( 3, ( #235305, #94510, #37139, #192343 ),
 .UNSPECIFIED., .F., .F. ) 
 B_SPLINE_CURVE_WITH_KNOTS ( ( 4, 4 ),
 ( 0.3000847527772370071, 0.5497968875596828120 ),
 .UNSPECIFIED. ) 
 CURVE ( )  GEOMETRIC_REPRESENTATION_ITEM ( )  RATIONAL_B_SPLINE_CURVE ( ( 1.000000000000000000, 0.9948104011409417691, 0.9948104011409417691, 1.000000000000000000 ) ) 
 REPRESENTATION_ITEM ( '' )  );
#203221 = CARTESIAN_POINT ( 'NONE',  ( -18.59999999999999787, -1.164121893230052995, -108.4148480855716485 ) ) ;
#203223 = EDGE_LOOP ( 'NONE', ( #79538, #89302, #190654, #167861 ) ) ;
#203222 = CARTESIAN_POINT ( 'NONE',  ( -21.05000000000000071, 5.850000000000001421, -23.36750277572207679 ) ) ;
#203224 = DIRECTION ( 'NONE',  ( -1.000000000000000000, -0.000000000000000000, 0.000000000000000000 ) ) ;
#203225 = ORIENTED_EDGE ( 'NONE', *, *, #74826, .F. ) ;
#203226 = CARTESIAN_POINT ( 'NONE',  ( 20.94999999999999574, 1.162701749949165642, -74.90000000000004832 ) ) ;
#203227 = ORIENTED_EDGE ( 'NONE', *, *, #42869, .T. ) ;
#203228 = EDGE_LOOP ( 'NONE', ( #254161, #3665, #90799, #238968 ) ) ;
#203229 = DIRECTION ( 'NONE',  ( 0.000000000000000000, 0.000000000000000000, -1.000000000000000000 ) ) ;
#203230 = DIRECTION ( 'NONE',  ( 0.000000000000000000, -1.000000000000000000, -8.717686153663073805E-15 ) ) ;
#203231 = CARTESIAN_POINT ( 'NONE',  ( -21.07928932188134397, 75.90110485435833709, -209.8516241409176928 ) ) ;
#203232 = CARTESIAN_POINT ( 'NONE',  ( 21.05000000000000426, 65.43724016256159359, -196.0662935266058184 ) ) ;
#203233 = TOROIDAL_SURFACE ( 'NONE', #40942, 7.800000000000000711, 0.1000000000000000056 ) ;
#203234 = AXIS2_PLACEMENT_3D ( 'NONE', #130646, #85068, #45975 ) ;
#203235 = AXIS2_PLACEMENT_3D ( 'NONE', #84589, #205864, #102894 ) ;
#203236 = CARTESIAN_POINT ( 'NONE',  ( 18.69999999999999929, -9.849999999999994316, 30.09999999999999787 ) ) ;
#203237 = ORIENTED_EDGE ( 'NONE', *, *, #118864, .F. ) ;
#203238 = ORIENTED_EDGE ( 'NONE', *, *, #152237, .F. ) ;
#203239 =( BOUNDED_SURFACE ( )  B_SPLINE_SURFACE ( 3, 2, ( 
 ( #245143, #106896, #66507 ),
 ( #91203, #207314, #186457 ),
 ( #7824, #88605, #129048 ),
 ( #166924, #28707, #147315 ) ),
 .UNSPECIFIED., .F., .F., .F. ) 
 B_SPLINE_SURFACE_WITH_KNOTS ( ( 4, 4 ),
 ( 3, 3 ),
 ( 1.355252715606880543E-20, 0.0003124336117481269631 ),
 ( 0.000000000000000000, 1.000000000000000000 ),
 .UNSPECIFIED. ) 
 GEOMETRIC_REPRESENTATION_ITEM ( )  RATIONAL_B_SPLINE_SURFACE ( (
 ( 1.000000000000000000, 0.7040654476015975050, 1.000000000000000000),
 ( 1.000000000000000000, 0.7039193538781914894, 1.000000000000000000),
 ( 1.000000000000000000, 0.7089171279145413118, 1.000000000000000000),
 ( 1.000000000000000000, 0.7071067811865506814, 1.000000000000000000) ) ) 
 REPRESENTATION_ITEM ( '' )  SURFACE ( )  );
#203240 = DIRECTION ( 'NONE',  ( 0.000000000000000000, 0.000000000000000000, 1.000000000000000000 ) ) ;
#203241 = EDGE_LOOP ( 'NONE', ( #250698, #131756, #119241 ) ) ;
#203242 = CARTESIAN_POINT ( 'NONE',  ( -21.95218792049438861, 0.09902843981107177507, -126.7984924387533567 ) ) ;
#203243 = CARTESIAN_POINT ( 'NONE',  ( -21.05000000000000071, 64.35000000001208775, -129.7392418215462158 ) ) ;
#203245 = CARTESIAN_POINT ( 'NONE',  ( 21.05000000000000071, 54.26566224370346703, -236.3486064386993633 ) ) ;
#203244 = CIRCLE ( 'NONE', #157486, 0.09999999999999939493 ) ;
#203246 = FACE_OUTER_BOUND ( 'NONE', #142889, .T. ) ;
#203247 = CARTESIAN_POINT ( 'NONE',  ( 21.05000000000000071, 74.63912941281955682, -61.45010955743337178 ) ) ;
#203248 = DIRECTION ( 'NONE',  ( 0.000000000000000000, 0.000000000000000000, -1.000000000000000000 ) ) ;
#203249 = CYLINDRICAL_SURFACE ( 'NONE', #175009, 0.09999999999999939493 ) ;
#203250 = DIRECTION ( 'NONE',  ( -1.000000000000000000, 0.000000000000000000, 0.000000000000000000 ) ) ;
#203251 = DIRECTION ( 'NONE',  ( 0.000000000000000000, -7.086529944415894657E-15, 1.000000000000000000 ) ) ;
#203252 = DIRECTION ( 'NONE',  ( -0.000000000000000000, 1.000000000000000000, 0.000000000000000000 ) ) ;
#203253 = CIRCLE ( 'NONE', #40966, 0.1000000000000007272 ) ;
#203254 = CARTESIAN_POINT ( 'NONE',  ( 18.79999999999999716, 9.511171963237318394, 1.617965922123945521 ) ) ;
#203255 = AXIS2_PLACEMENT_3D ( 'NONE', #72375, #146726, #226262 ) ;
#203256 = CIRCLE ( 'NONE', #236393, 11.80000000000000426 ) ;
#203257 =( BOUNDED_SURFACE ( )  B_SPLINE_SURFACE ( 3, 2, ( 
 ( #236696, #197576, #140160 ),
 ( #120646, #77609, #637 ),
 ( #98436, #157207, #179333 ),
 ( #198867, #58052, #101002 ),
 ( #257497, #22832, #17651 ),
 ( #158491, #219707, #181883 ) ),
 .UNSPECIFIED., .F., .F., .F. ) 
 B_SPLINE_SURFACE_WITH_KNOTS ( ( 4, 2, 4 ),
 ( 3, 3 ),
 ( 0.0001381104793128061785, 0.0002947094729387697305, 0.0004513084665647332824 ),
 ( 0.000000000000000000, 1.000000000000000000 ),
 .UNSPECIFIED. ) 
 GEOMETRIC_REPRESENTATION_ITEM ( )  RATIONAL_B_SPLINE_SURFACE ( (
 ( 1.000000000000000000, 0.7071067811865494601, 1.000000000000000000),
 ( 1.000000000000000000, 0.6919563088099112136, 1.000000000000000000),
 ( 1.000000000000000000, 0.6959445945717440685, 1.000000000000000000),
 ( 1.000000000000000000, 0.7137882985313291906, 1.000000000000000000),
 ( 1.000000000000000000, 0.7257496306096311578, 1.000000000000000000),
 ( 1.000000000000000000, 0.7250110520819876836, 1.000000000000000000) ) ) 
 REPRESENTATION_ITEM ( '' )  SURFACE ( )  );
#203258 = EDGE_CURVE ( 'NONE', #18380, #144444, #241381, .T. ) ;
#203259 = ORIENTED_EDGE ( 'NONE', *, *, #55049, .F. ) ;
#203260 = CARTESIAN_POINT ( 'NONE',  ( 20.95512820512820440, 10.62384868372303615, -41.16491356908760935 ) ) ;
#203261 = EDGE_LOOP ( 'NONE', ( #200212, #256004, #5266, #247346 ) ) ;
#203262 = EDGE_CURVE ( 'NONE', #242287, #429, #24912, .T. ) ;
#203263 = DIRECTION ( 'NONE',  ( -0.000000000000000000, -1.000000000000000000, -6.982962677686266711E-15 ) ) ;
#203264 = CARTESIAN_POINT ( 'NONE',  ( -20.94999999999999929, -1.162701749938009677, -8.099999999999999645 ) ) ;
#203265 = CARTESIAN_POINT ( 'NONE',  ( 21.04999999999999716, 61.84959188511203365, -221.8066534603183868 ) ) ;
#203266 = VERTEX_POINT ( 'NONE', #151299 ) ;
#203267 = CARTESIAN_POINT ( 'NONE',  ( -21.44999999999999929, 7.250000000011155521, -121.6500000000000341 ) ) ;
#203268 = CARTESIAN_POINT ( 'NONE',  ( -20.09999999673964410, 5.571292164246353984, 16.50791943615039159 ) ) ;
#203269 = EDGE_CURVE ( 'NONE', #27850, #131288, #150718, .T. ) ;
#203270 = EDGE_CURVE ( 'NONE', #18900, #155597, #202426, .T. ) ;
#203271 = LINE ( 'NONE', #126294, #126740 ) ;
#203272 = LINE ( 'NONE', #1196, #229660 ) ;
#203273 = AXIS2_PLACEMENT_3D ( 'NONE', #192127, #150431, #250785 ) ;
#203274 = CARTESIAN_POINT ( 'NONE',  ( -23.25000000000000000, 76.10000000001245724, -181.6726782920691505 ) ) ;
#203275 = AXIS2_PLACEMENT_3D ( 'NONE', #158285, #223336, #40897 ) ;
#203276 = DIRECTION ( 'NONE',  ( -1.000000000000000000, 8.034189347746081825E-16, -2.566115377699053685E-16 ) ) ;
#203277 = CIRCLE ( 'NONE', #257368, 0.1000000000000016986 ) ;
#203278 = CIRCLE ( 'NONE', #90832, 7.720710678118663850 ) ;
#203279 = EDGE_LOOP ( 'NONE', ( #47523, #203791, #201681, #154229 ) ) ;
#203282 = ORIENTED_EDGE ( 'NONE', *, *, #30509, .T. ) ;
#203281 = CARTESIAN_POINT ( 'NONE',  ( -20.54999999999999716, 20.06933876993645782, -235.7297789824848451 ) ) ;
#203280 = TOROIDAL_SURFACE ( 'NONE', #90834, 0.2000000000000000111, 0.1000000000000000056 ) ;
#203283 = CARTESIAN_POINT ( 'NONE',  ( -22.39999999999999858, 0.1000000000111554016, -59.20922040162664501 ) ) ;
#203284 = ADVANCED_FACE ( 'NONE', ( #87437 ), #190430, .T. ) ;
#203285 = DIRECTION ( 'NONE',  ( 0.000000000000000000, -0.7960711469212456981, 0.6052030477777622375 ) ) ;
#203286 = EDGE_CURVE ( 'NONE', #32887, #128006, #207419, .T. ) ;
#203287 = CIRCLE ( 'NONE', #111523, 12.87499999999999822 ) ;
#203288 = FACE_OUTER_BOUND ( 'NONE', #229519, .T. ) ;
#203289 = ORIENTED_EDGE ( 'NONE', *, *, #247018, .T. ) ;
#203290 = CARTESIAN_POINT ( 'NONE',  ( -22.46246831459151494, 75.97808783307279157, -148.1729720457342694 ) ) ;
#203291 = EDGE_CURVE ( 'NONE', #17738, #142484, #49609, .T. ) ;
#203292 = PRODUCT_CONTEXT ( 'NONE', #248882, 'mechanical' ) ;
#203293 = DIRECTION ( 'NONE',  ( -7.304098846218134667E-16, -1.000000000000000000, 0.000000000000000000 ) ) ;
#203294 = VERTEX_POINT ( 'NONE', #150019 ) ;
#203295 = CARTESIAN_POINT ( 'NONE',  ( 19.75857864376268935, 64.35000000001220144, -145.2731074845244450 ) ) ;
#203296 = PLANE ( 'NONE',  #5205 ) ;
#203297 = PRODUCT ( 'Injection Molded Chain Links', 'Injection Molded Chain Links', '', ( #157797 ) ) ;
#203298 = CIRCLE ( 'NONE', #95151, 0.1000000000000028644 ) ;
#203299 = AXIS2_PLACEMENT_3D ( 'NONE', #246881, #27879, #66967 ) ;
#203300 = ADVANCED_FACE ( 'NONE', ( #167027 ), #228260, .F. ) ;
#203301 = CLOSED_SHELL ( 'NONE', ( #62779, #175509, #246791, #116509, #238278, #220421, #47886, #234474, #112767, #176236, #17680, #207163, #83177, #202740, #44386, #10463, #224795, #256384, #152797, #23961, #112257, #72135, #45577, #247430, #226560, #101915, #187413, #12601, #199569, #251414, #61472, #98748, #255427, #62784, #185372, #128223, #138787, #199312, #243368, #88551, #83276, #72666, #11432, #78647, #228088, #19571, #984, #6125, #136194, #124458, #201116, #238245, #47302 ) ) ;
#203302 = DIRECTION ( 'NONE',  ( -0.000000000000000000, -0.9667078373770112698, -0.2558827019434132821 ) ) ;
#203303 = ORIENTED_EDGE ( 'NONE', *, *, #131801, .F. ) ;
#203304 = EDGE_CURVE ( 'NONE', #219222, #252182, #204814, .T. ) ;
#203305 = ORIENTED_EDGE ( 'NONE', *, *, #126195, .F. ) ;
#203306 = ADVANCED_FACE ( 'NONE', ( #130424 ), #209981, .F. ) ;
#203307 = ADVANCED_FACE ( 'NONE', ( #109569 ), #66591, .T. ) ;
#203308 = DIRECTION ( 'NONE',  ( -0.000000000000000000, -0.000000000000000000, 1.000000000000000000 ) ) ;
#203309 = CARTESIAN_POINT ( 'NONE',  ( -23.25000000000000000, 68.97833521811203639, -132.6895420826271277 ) ) ;
#203310 = DIRECTION ( 'NONE',  ( 0.000000000000000000, -1.000000000000000000, -0.000000000000000000 ) ) ;
#203312 = CIRCLE ( 'NONE', #161639, 0.1999999999999987899 ) ;
#203311 = FACE_OUTER_BOUND ( 'NONE', #42660, .T. ) ;
#203313 = DIRECTION ( 'NONE',  ( 0.000000000000000000, -0.4088369013363205573, 0.9126074666063803686 ) ) ;
#203314 = FACE_OUTER_BOUND ( 'NONE', #42872, .T. ) ;
#203315 = AXIS2_PLACEMENT_3D ( 'NONE', #216982, #236552, #111820 ) ;
#203317 = CARTESIAN_POINT ( 'NONE',  ( -20.94999999999999929, 28.56975825374500388, -258.1421690862028413 ) ) ;
#203316 = CARTESIAN_POINT ( 'NONE',  ( 20.95132126680579887, 65.51005012986510678, -95.45278294608985448 ) ) ;
#203318 = LINE ( 'NONE', #123782, #152849 ) ;
#203319 = AXIS2_PLACEMENT_3D ( 'NONE', #139783, #58945, #219328 ) ;
#203320 = CARTESIAN_POINT ( 'NONE',  ( -21.05000000000000071, -1.261786168553869603, -108.5864989635455089 ) ) ;
#203321 = DIRECTION ( 'NONE',  ( 2.978066053179069723E-16, 1.000000000000000000, 7.147358527629766941E-15 ) ) ;
#203322 = CARTESIAN_POINT ( 'NONE',  ( -16.77683809663752257, 23.65833333334447985, -83.75000000000004263 ) ) ;
#203323 = ORIENTED_EDGE ( 'NONE', *, *, #30866, .T. ) ;
#203324 = VERTEX_POINT ( 'NONE', #185272 ) ;
#203325 = FACE_OUTER_BOUND ( 'NONE', #255556, .T. ) ;
#203326 = FACE_OUTER_BOUND ( 'NONE', #8425, .T. ) ;
#203327 = CARTESIAN_POINT ( 'NONE',  ( -15.31895204843005942, 12.99171346507298530, -216.4962224982960777 ) ) ;
#203328 = AXIS2_PLACEMENT_3D ( 'NONE', #47284, #225912, #43461 ) ;
#203329 = EDGE_CURVE ( 'NONE', #7257, #103638, #181662, .T. ) ;
#203330 = CARTESIAN_POINT ( 'NONE',  ( -18.50000000000000000, -26.43935341560094443, -18.14150860750746475 ) ) ;
#203332 = EDGE_CURVE ( 'NONE', #212737, #164375, #212344, .T. ) ;
#203331 = LINE ( 'NONE', #166803, #241577 ) ;
#203333 = FACE_OUTER_BOUND ( 'NONE', #86559, .T. ) ;
#203334 = VECTOR ( 'NONE', #64159, 1000.000000000000114 ) ;
#203335 = DIRECTION ( 'NONE',  ( 1.000000000000000000, 3.265361837132813093E-16, -0.000000000000000000 ) ) ;
#203336 = ORIENTED_EDGE ( 'NONE', *, *, #184925, .T. ) ;
#203337 = AXIS2_PLACEMENT_3D ( 'NONE', #211933, #131094, #136195 ) ;
#203338 = AXIS2_PLACEMENT_3D ( 'NONE', #182753, #204846, #220584 ) ;
#203339 = EDGE_CURVE ( 'NONE', #95688, #102195, #208059, .T. ) ;
#203340 = CARTESIAN_POINT ( 'NONE',  ( -16.89797118371607354, 51.68774209830978350, -231.8867050212883498 ) ) ;
#203341 = VECTOR ( 'NONE', #226158, 1000.000000000000000 ) ;
#203342 = ORIENTED_EDGE ( 'NONE', *, *, #120677, .T. ) ;
#203343 = CARTESIAN_POINT ( 'NONE',  ( 20.95512820512820440, 67.12384868372348024, -60.96447848938343839 ) ) ;
#203344 = DIRECTION ( 'NONE',  ( 1.000000000000000000, 0.000000000000000000, 0.000000000000000000 ) ) ;
#203345 = EDGE_LOOP ( 'NONE', ( #21662, #68087, #110633, #185045 ) ) ;
#203346 = CARTESIAN_POINT ( 'NONE',  ( -18.52643265882458579, 18.39335631088233214, -236.9600537807593525 ) ) ;
#203347 = ORIENTED_EDGE ( 'NONE', *, *, #102978, .F. ) ;
#203348 = DIRECTION ( 'NONE',  ( 0.000000000000000000, 6.853228547068871147E-15, -1.000000000000000000 ) ) ;
#203349 = DIRECTION ( 'NONE',  ( 0.000000000000000000, 0.000000000000000000, -1.000000000000000000 ) ) ;
#203351 = AXIS2_PLACEMENT_3D ( 'NONE', #162958, #226751, #48117 ) ;
#203350 = CARTESIAN_POINT ( 'NONE',  ( -20.85000000000000142, -1.362429037182151470, -208.8888812479211765 ) ) ;
#203352 = ADVANCED_FACE ( 'NONE', ( #157411 ), #196485, .F. ) ;
#203353 = LINE ( 'NONE', #178687, #229121 ) ;
#203354 = DIRECTION ( 'NONE',  ( 1.000000000000000000, 0.000000000000000000, 0.000000000000000000 ) ) ;
#203355 = CARTESIAN_POINT ( 'NONE',  ( -21.05000000000000071, 61.16604239671104892, -234.3115055913011417 ) ) ;
#203356 = CARTESIAN_POINT ( 'NONE',  ( -20.54999999999999716, 68.75000000001158185, -57.27310748452437394 ) ) ;
#203357 = CARTESIAN_POINT ( 'NONE',  ( 21.30000000000002558, 7.128833340093095217, -233.7327013124392749 ) ) ;
#203358 = ADVANCED_FACE ( 'NONE', ( #829 ), #220701, .T. ) ;
#203360 = EDGE_LOOP ( 'NONE', ( #51834, #148243, #235494, #184876, #518, #75050, #127599, #88373, #231459, #32168 ) ) ;
#203359 = DIRECTION ( 'NONE',  ( 0.000000000000000000, 0.3488585713686159218, 0.9371753822965306346 ) ) ;
#203362 = DIRECTION ( 'NONE',  ( 0.000000000000000000, 0.000000000000000000, 1.000000000000000000 ) ) ;
#203361 = CARTESIAN_POINT ( 'NONE',  ( -18.58671080940899145, 85.40693285883926933, -196.3989530196196256 ) ) ;
#203363 = VERTEX_POINT ( 'NONE', #38717 ) ;
#203365 = EDGE_LOOP ( 'NONE', ( #44467, #209716, #200955 ) ) ;
#203364 = LINE ( 'NONE', #166837, #148388 ) ;
#203366 = ORIENTED_EDGE ( 'NONE', *, *, #164127, .T. ) ;
#203367 = CARTESIAN_POINT ( 'NONE',  ( 21.05000000000000071, 85.40000000001148805, -45.91707660717669626 ) ) ;
#203368 = CARTESIAN_POINT ( 'NONE',  ( 23.14999999999999503, 64.25000000001249134, -177.0379132551784096 ) ) ;
#203369 = CARTESIAN_POINT ( 'NONE',  ( 18.59999999999996945, 68.97833521811233481, -166.1895420826271277 ) ) ;
#203370 = ADVANCED_FACE ( 'NONE', ( #158687 ), #2131, .T. ) ;
#203371 = ORIENTED_EDGE ( 'NONE', *, *, #140396, .T. ) ;
#203372 = EDGE_CURVE ( 'NONE', #16586, #181858, #17844, .T. ) ;
#203373 = CARTESIAN_POINT ( 'NONE',  ( 21.05000000000000426, 0.01471785653553484702, -127.6552765959085036 ) ) ;
#203374 = CARTESIAN_POINT ( 'NONE',  ( 18.39999999999999858, -9.599999999988842347, -74.03206939669971121 ) ) ;
#203375 = DIRECTION ( 'NONE',  ( -0.000000000000000000, -0.8814952561688430555, 0.4721928772777346239 ) ) ;
#203376 = EDGE_CURVE ( 'NONE', #60192, #34777, #245649, .T. ) ;
#203377 = FACE_OUTER_BOUND ( 'NONE', #103461, .T. ) ;
#203378 = CARTESIAN_POINT ( 'NONE',  ( 21.11101077988997332, 69.57631526528609811, -136.5383927534386430 ) ) ;
#203379 = AXIS2_PLACEMENT_3D ( 'NONE', #238911, #124108, #163231 ) ;
#203380 = VERTEX_POINT ( 'NONE', #120846 ) ;
#203382 = ORIENTED_EDGE ( 'NONE', *, *, #81043, .F. ) ;
#203381 = CIRCLE ( 'NONE', #74231, 0.09999999999999939493 ) ;
#203383 = AXIS2_PLACEMENT_3D ( 'NONE', #107571, #71048, #227520 ) ;
#203384 = FACE_OUTER_BOUND ( 'NONE', #12647, .T. ) ;
#203385 = VECTOR ( 'NONE', #175400, 1000.000000000000227 ) ;
#203386 = EDGE_CURVE ( 'NONE', #180208, #78167, #101199, .T. ) ;
#203387 = ORIENTED_EDGE ( 'NONE', *, *, #213883, .F. ) ;
#203388 = DIRECTION ( 'NONE',  ( 0.000000000000000000, 0.000000000000000000, 1.000000000000000000 ) ) ;
#203390 = ADVANCED_FACE ( 'NONE', ( #178247 ), #119546, .T. ) ;
#203389 = ORIENTED_EDGE ( 'NONE', *, *, #132632, .F. ) ;
#203391 = DIRECTION ( 'NONE',  ( 0.000000000000000000, 0.000000000000000000, -1.000000000000000000 ) ) ;
#203392 = CARTESIAN_POINT ( 'NONE',  ( -18.59999999999999787, -1.835341550224411922, -11.65515129256297833 ) ) ;
#203393 = CARTESIAN_POINT ( 'NONE',  ( -22.00411653962179415, 68.74655713164197834, -103.1221455903250330 ) ) ;
#203394 = EDGE_CURVE ( 'NONE', #253488, #126100, #136498, .T. ) ;
#203395 = CARTESIAN_POINT ( 'NONE',  ( -21.09316766718153247, 30.82942261761470704, -252.1196843684382429 ) ) ;
#203396 = CARTESIAN_POINT ( 'NONE',  ( 21.04999999999999716, 10.62872031401550466, -179.6499999999999488 ) ) ;
#203397 = ORIENTED_EDGE ( 'NONE', *, *, #8490, .F. ) ;
#203398 = CARTESIAN_POINT ( 'NONE',  ( -18.59999999999999787, 77.83534155023670564, -158.4679561919613491 ) ) ;
#203399 = VECTOR ( 'NONE', #94239, 1000.000000000000000 ) ;
#203401 = AXIS2_PLACEMENT_3D ( 'NONE', #221913, #129267, #45871 ) ;
#203400 = LINE ( 'NONE', #205956, #58939 ) ;
#203402 = DIRECTION ( 'NONE',  ( -0.000000000000000000, 1.000000000000000000, 0.000000000000000000 ) ) ;
#203404 = ORIENTED_EDGE ( 'NONE', *, *, #223728, .T. ) ;
#203403 = ADVANCED_FACE ( 'NONE', ( #20447 ), #108097, .F. ) ;
#203406 = DIRECTION ( 'NONE',  ( -0.000000000000000000, 0.9651348961777157509, -0.2617529984165031243 ) ) ;
#203405 = CARTESIAN_POINT ( 'NONE',  ( -22.94999999999999929, 1.885425182446134107, -11.49641995933507843 ) ) ;
#203407 = VERTEX_POINT ( 'NONE', #179522 ) ;
#203410 = ORIENTED_EDGE ( 'NONE', *, *, #129078, .F. ) ;
#203409 =( LENGTH_UNIT ( ) NAMED_UNIT ( * ) SI_UNIT ( .MILLI., .METRE. ) );
#203408 = CARTESIAN_POINT ( 'NONE',  ( -20.94999999999999929, 74.16465844978819177, -191.9679561919613775 ) ) ;
#203411 = ORIENTED_EDGE ( 'NONE', *, *, #19361, .F. ) ;
#203412 = AXIS2_PLACEMENT_3D ( 'NONE', #36435, #41566, #121110 ) ;
#203413 = PLANE ( 'NONE',  #118490 ) ;
#203414 = DIRECTION ( 'NONE',  ( 0.000000000000000000, -0.1480365673253004333, 0.9889818879709283417 ) ) ;
#203415 = ADVANCED_FACE ( 'NONE', ( #239485 ), #140360, .F. ) ;
#203416 = DIRECTION ( 'NONE',  ( 0.000000000000000000, -6.982962677686266711E-15, 1.000000000000000000 ) ) ;
#203417 = ORIENTED_EDGE ( 'NONE', *, *, #104843, .F. ) ;
#203418 = CYLINDRICAL_SURFACE ( 'NONE', #96915, 0.1000000000000013933 ) ;
#203419 = EDGE_CURVE ( 'NONE', #217669, #133237, #183116, .T. ) ;
#203421 = CARTESIAN_POINT ( 'NONE',  ( 18.59999999999999076, 63.61019970229975229, -209.1253633388161006 ) ) ;
#203420 = CARTESIAN_POINT ( 'NONE',  ( 21.05000000000000071, -11.64999999998883595, -131.0000000000000284 ) ) ;
#203422 = ADVANCED_FACE ( 'NONE', ( #131715 ), #32663, .F. ) ;
#203424 = VERTEX_POINT ( 'NONE', #92573 ) ;
#203423 = FACE_OUTER_BOUND ( 'NONE', #252825, .T. ) ;
#203425 = EDGE_LOOP ( 'NONE', ( #230679, #244904, #42482 ) ) ;
#203426 = CIRCLE ( 'NONE', #115937, 0.09999999999999939493 ) ;
#203427 = CARTESIAN_POINT ( 'NONE',  ( 19.75857864376269291, 64.25000000001176659, -78.17310748452437963 ) ) ;
#203428 = CARTESIAN_POINT ( 'NONE',  ( -23.25000000000000000, 64.35000000001218723, -143.5379132551784096 ) ) ;
#203429 = CIRCLE ( 'NONE', #120255, 0.09999999999999939493 ) ;
#203430 = AXIS2_PLACEMENT_3D ( 'NONE', #107113, #65420, #27623 ) ;
#203431 = DIRECTION ( 'NONE',  ( 0.000000000000000000, -1.000000000000000000, 0.000000000000000000 ) ) ;
#203432 = ORIENTED_EDGE ( 'NONE', *, *, #135028, .F. ) ;
#203433 = CARTESIAN_POINT ( 'NONE',  ( -23.15000000000000213, 73.50000000001254818, -183.2477294072864709 ) ) ;
#203434 = EDGE_LOOP ( 'NONE', ( #127220, #254946, #138950, #246498 ) ) ;
#203436 = ADVANCED_FACE ( 'NONE', ( #172176 ), #37443, .F. ) ;
#203435 = CARTESIAN_POINT ( 'NONE',  ( 21.05000000000000071, 28.50120599808395028, -258.2149742250584268 ) ) ;
#203437 = CARTESIAN_POINT ( 'NONE',  ( 21.53699400380134676, 6.787711793207312994, -33.50000000000000711 ) ) ;
#203438 = CIRCLE ( 'NONE', #41134, 0.1999999999999987899 ) ;
#203439 = EDGE_LOOP ( 'NONE', ( #190326, #87611, #203734, #51461, #100032 ) ) ;
#203440 = SPHERICAL_SURFACE ( 'NONE', #212610, 0.1000000000000000056 ) ;
#203441 = CIRCLE ( 'NONE', #82766, 12.97499999999999964 ) ;
#203442 = AXIS2_PLACEMENT_3D ( 'NONE', #9500, #129461, #51171 ) ;
#203443 = CARTESIAN_POINT ( 'NONE',  ( -18.39418127959864790, 64.51609439831364057, -78.77310748452438816 ) ) ;
#203444 = AXIS2_PLACEMENT_3D ( 'NONE', #116478, #73526, #171360 ) ;
#203445 = EDGE_LOOP ( 'NONE', ( #168761, #51982, #188082, #236496, #27170 ) ) ;
#203446 = ORIENTED_EDGE ( 'NONE', *, *, #163565, .F. ) ;
#203447 = AXIS2_PLACEMENT_3D ( 'NONE', #213884, #153965, #96482 ) ;
#203448 = ORIENTED_EDGE ( 'NONE', *, *, #110922, .F. ) ;
#203449 = FACE_OUTER_BOUND ( 'NONE', #171089, .T. ) ;
#203450 = EDGE_CURVE ( 'NONE', #147029, #23656, #141399, .T. ) ;
#203451 = ORIENTED_EDGE ( 'NONE', *, *, #24001, .T. ) ;
#203453 = ORIENTED_EDGE ( 'NONE', *, *, #134671, .T. ) ;
#203452 = CARTESIAN_POINT ( 'NONE',  ( -20.64999999999999858, -9.400000000000005684, -9.893969122652444881 ) ) ;
#203454 = ORIENTED_EDGE ( 'NONE', *, *, #197278, .F. ) ;
#203455 = AXIS2_PLACEMENT_3D ( 'NONE', #219316, #120266, #202326 ) ;
#203458 = ORIENTED_EDGE ( 'NONE', *, *, #165434, .F. ) ;
#203457 = EDGE_LOOP ( 'NONE', ( #207555, #11926, #117343, #117149 ) ) ;
#203456 = CARTESIAN_POINT ( 'NONE',  ( -16.78569801330232636, 9.947933733124651567, -113.1569129053475393 ) ) ;
#203459 = DIRECTION ( 'NONE',  ( -3.787827842127535236E-15, 0.7397360091702777085, 0.6728971962616808744 ) ) ;
#203461 = ORIENTED_EDGE ( 'NONE', *, *, #21353, .F. ) ;
#203460 = VECTOR ( 'NONE', #181236, 1000.000000000000114 ) ;
#203462 = CARTESIAN_POINT ( 'NONE',  ( 23.15000000000000213, 86.27712145182582049, -209.5223386573213702 ) ) ;
#203463 = EDGE_CURVE ( 'NONE', #130496, #214472, #137296, .T. ) ;
#203464 = CARTESIAN_POINT ( 'NONE',  ( -20.64999999999999858, 74.05981308412395947, -82.35222669557765585 ) ) ;
#203465 = AXIS2_PLACEMENT_3D ( 'NONE', #39973, #197725, #174369 ) ;
#203466 = DIRECTION ( 'NONE',  ( 0.000000000000000000, 0.8814952561688449428, -0.4721928772777311267 ) ) ;
#203467 = AXIS2_PLACEMENT_3D ( 'NONE', #213885, #247876, #249173 ) ;
#203468 = AXIS2_PLACEMENT_3D ( 'NONE', #238800, #120173, #122722 ) ;
#203469 = EDGE_LOOP ( 'NONE', ( #78511, #144517, #250734, #37385 ) ) ;
#203470 = AXIS2_PLACEMENT_3D ( 'NONE', #203919, #9570, #25308 ) ;
#203471 = DIRECTION ( 'NONE',  ( -1.836970198721030427E-16, -0.4088369013363281623, 0.9126074666063771490 ) ) ;
#203473 = ORIENTED_EDGE ( 'NONE', *, *, #149109, .F. ) ;
#203472 = CARTESIAN_POINT ( 'NONE',  ( -16.94107738177414291, 65.98576071487592287, -182.5731074845244279 ) ) ;
#203474 = CARTESIAN_POINT ( 'NONE',  ( 18.49999999999999645, 0.8650195716890431985, -212.6652626294507229 ) ) ;
#203476 = VERTEX_POINT ( 'NONE', #223743 ) ;
#203475 = DIRECTION ( 'NONE',  ( -1.000000000000000000, -3.265361837132813093E-16, 0.000000000000000000 ) ) ;
#203477 = EDGE_LOOP ( 'NONE', ( #93733, #153201, #35461, #29189, #187330 ) ) ;
#203478 = ORIENTED_EDGE ( 'NONE', *, *, #46310, .T. ) ;
#203479 = ORIENTED_EDGE ( 'NONE', *, *, #244517, .T. ) ;
#203480 = CARTESIAN_POINT ( 'NONE',  ( -23.25000000000000355, 64.25000000001222134, -145.7731074845244450 ) ) ;
#203481 = VECTOR ( 'NONE', #177659, 1000.000000000000114 ) ;
#203483 = EDGE_LOOP ( 'NONE', ( #52073, #30781 ) ) ;
#203482 = VERTEX_POINT ( 'NONE', #240769 ) ;
#203485 = ORIENTED_EDGE ( 'NONE', *, *, #71887, .F. ) ;
#203484 = CLOSED_SHELL ( 'NONE', ( #110742, #195798, #215471, #49905, #215411, #220503, #30798, #238943, #227242, #48769, #213229, #256014, #232799, #233090, #252327, #56646, #75434, #12707, #28524, #154124, #177161, #118578, #76877, #49160, #198786, #36373, #242000, #211984, #800, #209576, #173442, #114641, #219768, #128887, #118282, #192393, #228842, #160024, #70283, #200444, #77001, #162889, #80273, #76827, #226934, #164304, #2587, #23641, #107358, #214745, #108179, #167757, #124586, #81794, #81153, #21584, #215681, #2506, #189820, #1921, #106034, #231265, #201916, #159823, #254283, #233765, #64631, #68797, #49189, #127802, #167068, #112315, #109789, #82360, #173944, #85543, #254613, #236347, #245243, #108797, #256203, #30237, #21225, #70007, #106345, #98788, #81959, #106223, #156008, #39656, #118420, #212122, #116622, #119429, #118251, #143780, #119099, #174341, #114518, #93385, #120359, #122343, #173794, #20433, #1080, #130587, #201777, #34788, #74745, #5840, #149533, #117399, #121573, #67468, #178974, #159140, #227740, #74177, #59293, #139027, #9925, #248429, #110585, #181617, #26748, #254768, #226819, #227655, #87083, #66664, #232997, #244754, #17835, #202538, #37923, #154006, #152426, #215693, #139669, #98801, #10599, #190994, #208420, #234549, #87914, #32487, #228362, #61478, #194346, #144697, #109610, #132951, #157014, #163952, #93703, #193566, #94652, #231007, #243701, #215375, #207689, #131181, #30846, #230538, #142414, #252392, #201060, #239633, #238342, #180158, #96807, #193689, #103576, #30898, #121175, #90487, #73795, #9604, #53652, #82660, #246364, #156698, #107454, #27352, #112704, #242186, #79020, #176636, #98892, #172321, #164171, #43829, #72179, #4609, #118400, #58161, #100230, #101867, #8867, #38817, #210320, #221054, #234741, #98985, #70816, #30003, #206443, #122028, #1806, #188643, #171561, #80565, #140892, #134302, #220713, #257951, #159002, #56144, #199842, #89111, #18202, #73849, #254700, #83991, #238088, #199906, #112631, #105787, #55922, #189345, #178667, #217000, #149672, #192670, #185057, #217894, #56934, #105328, #221538, #115562, #35702, #36535, #33909, #149541, #138734, #94982, #36714, #178954, #116337, #234466, #71288, #212936, #106369, #168108, #73994, #138155, #95028, #107320, #111232, #56125, #20117, #115732, #90797, #220645, #64098, #95277, #189614, #216688, #192205, #253668, #133863, #219882, #121653, #156162, #141530, #167050, #222426, #134420, #228230, #153595, #209233, #190978, #250032, #25442, #90147, #28878, #148354, #215074, #7790, #73127, #236326, #1116, #91116, #70420, #50089, #172569, #28739, #27231, #191701, #129425, #220938, #14492, #223166, #120334, #77642, #241238, #153144, #17579, #125905, #136207, #225407, #131514, #175070, #90363, #67299, #37197, #33070, #144095, #148258, #129818, #131796, #175740, #24072, #52791, #204568, #76198, #257300, #122431, #249844, #170695, #218856, #220442, #55331, #150656, #179035, #251652, #88442, #37240, #41231, #181066, #60152, #203415, #228898, #71707, #58112, #123133, #218624, #71275, #87304, #165960, #252355, #178774, #208313, #26390, #89893, #61924, #34163, #120996, #255157, #211257, #201571, #236678, #74639, #90639, #204534, #162630, #254447, #246171, #198952, #185234, #255851, #118249, #173049, #59039, #227359, #220429, #232730, #199295, #55264, #70659, #46110, #168656, #58137, #135096, #88761, #113363, #186355, #118179, #180982, #86029, #58214, #179259, #233032, #4547, #20009, #184759, #4574, #4304, #247711, #162943, #248129, #196774, #91927, #256467, #92623, #105864, #198705, #10593, #5551, #138368, #84435, #25535, #162513, #178870, #58176, #51121, #95216, #246658, #14153, #105473, #218770, #42244, #73619, #136483, #63377, #264, #21970, #30550, #227557, #187752, #3468, #206147, #117639, #177065, #223965, #159873, #51360, #22105, #145037, #227188, #185732, #186033, #166051, #257009, #246204, #24984, #172312, #67233, #195382, #159808, #192674, #68105, #108566, #226501, #70401, #30160, #190680, #189264, #174565, #62683, #162356, #225612, #145959, #127827, #110611, #180826, #140610, #179973, #195046, #95696, #249845, #117863, #32373, #94489, #201235, #89047, #251513, #141303 ) ) ;
#203486 = CYLINDRICAL_SURFACE ( 'NONE', #61247, 0.09999999999999939493 ) ;
#203487 = VERTEX_POINT ( 'NONE', #8571 ) ;
#203488 = ORIENTED_EDGE ( 'NONE', *, *, #205657, .T. ) ;
#203489 = DIRECTION ( 'NONE',  ( 0.000000000000000000, 0.000000000000000000, -1.000000000000000000 ) ) ;
#203491 = ORIENTED_EDGE ( 'NONE', *, *, #222865, .F. ) ;
#203490 = CARTESIAN_POINT ( 'NONE',  ( -23.25000000000000000, 7.783179459866048866, -245.3643104511423019 ) ) ;
#203492 = CARTESIAN_POINT ( 'NONE',  ( -23.15000000000000213, 28.42524210734032053, -258.3567845160494585 ) ) ;
#203494 = DIRECTION ( 'NONE',  ( 0.000000000000000000, 0.9126074666063660468, 0.4088369013363524762 ) ) ;
#203493 = CARTESIAN_POINT ( 'NONE',  ( 18.59999999999999432, 38.30077178631847801, -261.1858881914067751 ) ) ;
#203495 = EDGE_LOOP ( 'NONE', ( #7255, #8988, #156070, #246312, #107438, #231574, #6254, #185785, #96662, #48301, #6019, #79533, #23932, #100788, #191637, #223685, #257813, #34473, #252769, #15078, #11704, #121327, #101365 ) ) ;
#203496 = VECTOR ( 'NONE', #26548, 1000.000000000000000 ) ;
#203497 = EDGE_CURVE ( 'NONE', #1926, #209826, #122549, .T. ) ;
#203498 = AXIS2_PLACEMENT_3D ( 'NONE', #69334, #148873, #228408 ) ;
#203500 = EDGE_LOOP ( 'NONE', ( #257324, #62960, #21628, #22387 ) ) ;
#203499 = ORIENTED_EDGE ( 'NONE', *, *, #47471, .T. ) ;
#203501 = FACE_OUTER_BOUND ( 'NONE', #218931, .T. ) ;
#203502 = CARTESIAN_POINT ( 'NONE',  ( -20.64999999999999858, 4.350000000011156054, -54.65000000000000568 ) ) ;
#203503 = VECTOR ( 'NONE', #134340, 1000.000000000000000 ) ;
#203504 = ORIENTED_EDGE ( 'NONE', *, *, #19014, .T. ) ;
#203505 = VECTOR ( 'NONE', #191696, 1000.000000000000000 ) ;
#203506 = DIRECTION ( 'NONE',  ( -1.000000000000000000, 0.000000000000000000, 0.000000000000000000 ) ) ;
#203507 = ORIENTED_EDGE ( 'NONE', *, *, #92662, .F. ) ;
#203508 = EDGE_LOOP ( 'NONE', ( #71660, #166102, #37555, #197714 ) ) ;
#203509 = ADVANCED_FACE ( 'NONE', ( #146759 ), #47669, .T. ) ;
#203510 = FACE_OUTER_BOUND ( 'NONE', #199257, .T. ) ;
#203511 = ORIENTED_EDGE ( 'NONE', *, *, #51425, .T. ) ;
#203512 = CARTESIAN_POINT ( 'NONE',  ( -20.00857864376270001, 9.350000000011156942, -179.7499999999999716 ) ) ;
#203513 = DIRECTION ( 'NONE',  ( 1.000000000000000000, 0.000000000000000000, 0.000000000000000000 ) ) ;
#203514 = ORIENTED_EDGE ( 'NONE', *, *, #109471, .T. ) ;
#203515 = CYLINDRICAL_SURFACE ( 'NONE', #181455, 0.1000000000000021844 ) ;
#203516 = DIRECTION ( 'NONE',  ( 0.000000000000000000, 6.982962677686266711E-15, -1.000000000000000000 ) ) ;
#203518 = CARTESIAN_POINT ( 'NONE',  ( 20.94999999999999929, 45.65843669757526158, -240.2045374387683410 ) ) ;
#203517 = DIRECTION ( 'NONE',  ( 0.000000000000000000, 0.2128009952263403282, -0.9770955615653358350 ) ) ;
#203519 = EDGE_CURVE ( 'NONE', #109246, #160984, #3412, .T. ) ;
#203520 = DIRECTION ( 'NONE',  ( -4.408576920032448588E-17, 0.1350103645451876944, -0.9908441862701601321 ) ) ;
#203522 = AXIS2_PLACEMENT_3D ( 'NONE', #166105, #125651, #245610 ) ;
#203521 = DIRECTION ( 'NONE',  ( 0.000000000000000000, 0.1350103645451876666, 0.9908441862701600211 ) ) ;
#203523 = AXIS2_PLACEMENT_3D ( 'NONE', #86833, #107698, #188521 ) ;
#203524 = CARTESIAN_POINT ( 'NONE',  ( -15.55912972643741199, 10.98832424774994365, -211.5533932092509417 ) ) ;
#203525 = CARTESIAN_POINT ( 'NONE',  ( 21.05000000000000426, 76.01681986839787442, -142.8305327040896771 ) ) ;
#203526 = CIRCLE ( 'NONE', #12004, 0.09999999999999939493 ) ;
#203527 = EDGE_CURVE ( 'NONE', #190837, #60760, #191510, .T. ) ;
#203528 = ORIENTED_EDGE ( 'NONE', *, *, #142557, .T. ) ;
#203529 = EDGE_CURVE ( 'NONE', #199985, #21668, #42479, .T. ) ;
#203531 = ORIENTED_EDGE ( 'NONE', *, *, #49750, .F. ) ;
#203530 = ORIENTED_EDGE ( 'NONE', *, *, #43740, .F. ) ;
#203532 = ORIENTED_EDGE ( 'NONE', *, *, #171310, .F. ) ;
#203533 = DIRECTION ( 'NONE',  ( -1.000000000000000000, -2.952720810173289112E-16, 0.000000000000000000 ) ) ;
#203534 = EDGE_CURVE ( 'NONE', #229996, #104319, #127232, .T. ) ;
#203536 = LINE ( 'NONE', #143552, #136366 ) ;
#203535 = FACE_OUTER_BOUND ( 'NONE', #118810, .T. ) ;
#203537 = LINE ( 'NONE', #223087, #107871 ) ;
#203538 = VERTEX_POINT ( 'NONE', #102495 ) ;
#203539 = CIRCLE ( 'NONE', #215976, 0.09999999999999939493 ) ;
#203540 = CARTESIAN_POINT ( 'NONE',  ( -21.29999999999995808, 67.23127455305841238, -235.8551265064783991 ) ) ;
#203541 = PLANE ( 'NONE',  #17014 ) ;
#203542 = EDGE_CURVE ( 'NONE', #47883, #26579, #79016, .T. ) ;
#203543 = LINE ( 'NONE', #40660, #201596 ) ;
#203544 = CARTESIAN_POINT ( 'NONE',  ( -23.15000000000000213, 11.65000000000000036, 11.75000000000000000 ) ) ;
#203545 = VERTEX_POINT ( 'NONE', #82932 ) ;
#203546 = CARTESIAN_POINT ( 'NONE',  ( 20.85000000000000142, 76.00000000001142553, -36.02310748452432421 ) ) ;
#203547 = DIRECTION ( 'NONE',  ( -1.000000000000000000, -0.000000000000000000, 0.000000000000000000 ) ) ;
#203548 = VERTEX_POINT ( 'NONE', #204184 ) ;
#203549 = CARTESIAN_POINT ( 'NONE',  ( -20.05000000000000426, 66.75000000001260503, -191.1731074845244223 ) ) ;
#203550 = FACE_OUTER_BOUND ( 'NONE', #137879, .T. ) ;
#203551 = DIRECTION ( 'NONE',  ( 0.000000000000000000, 0.000000000000000000, 1.000000000000000000 ) ) ;
#203552 = CARTESIAN_POINT ( 'NONE',  ( -18.59999999999999787, 68.97833521811179480, -99.18954208262705663 ) ) ;
#203553 = CARTESIAN_POINT ( 'NONE',  ( -20.15000000000000568, 9.291421356248463326, -188.6499999999999488 ) ) ;
#203554 = FACE_OUTER_BOUND ( 'NONE', #220787, .T. ) ;
#203555 = VERTEX_POINT ( 'NONE', #125928 ) ;
#203556 = CARTESIAN_POINT ( 'NONE',  ( 20.85000000000000142, 11.65000000000000391, -26.71613433702190932 ) ) ;
#203557 = DIRECTION ( 'NONE',  ( 1.000000000000000000, 0.000000000000000000, 0.000000000000000000 ) ) ;
#203559 = EDGE_CURVE ( 'NONE', #160781, #17664, #37368, .T. ) ;
#203558 = CARTESIAN_POINT ( 'NONE',  ( -21.04999999999999716, 0.01485563490477569658, -60.65564095795671307 ) ) ;
#203561 = CARTESIAN_POINT ( 'NONE',  ( -21.14999999999999858, 31.98723526783714988, -238.8784020251475511 ) ) ;
#203560 = CARTESIAN_POINT ( 'NONE',  ( -16.87683809663753465, 66.13508622147364235, -123.2473918488858544 ) ) ;
#203562 = DIRECTION ( 'NONE',  ( 1.000000000000000000, -3.265361837132813093E-16, -2.280189983783949500E-30 ) ) ;
#203563 = CARTESIAN_POINT ( 'NONE',  ( 23.40000000000005187, 64.35000000001120668, -36.02310748452479316 ) ) ;
#203564 = VECTOR ( 'NONE', #191800, 1000.000000000000000 ) ;
#203565 = LINE ( 'NONE', #24951, #53730 ) ;
#203566 = DIRECTION ( 'NONE',  ( 0.000000000000000000, -8.232585987686539041E-15, 1.000000000000000000 ) ) ;
#203567 = AXIS2_PLACEMENT_3D ( 'NONE', #221863, #184044, #43262 ) ;
#203569 = VERTEX_POINT ( 'NONE', #67252 ) ;
#203568 = CARTESIAN_POINT ( 'NONE',  ( -23.15000000000000213, 78.57160958314655375, -238.9307242378722833 ) ) ;
#203570 = ADVANCED_FACE ( 'NONE', ( #187224 ), #225020, .T. ) ;
#203571 = VECTOR ( 'NONE', #145185, 1000.000000000000000 ) ;
#203572 = DIRECTION ( 'NONE',  ( 1.000000000000000000, 0.000000000000000000, 0.000000000000000000 ) ) ;
#203573 = AXIS2_PLACEMENT_3D ( 'NONE', #186546, #83549, #103126 ) ;
#203574 = CARTESIAN_POINT ( 'NONE',  ( -18.56579813702276027, 65.66974365629616273, -30.43601455626049912 ) ) ;
#203575 = EDGE_CURVE ( 'NONE', #127123, #137948, #216414, .T. ) ;
#203576 = CARTESIAN_POINT ( 'NONE',  ( 13.43443725621852636, 9.446557523083688679, -149.0899419543459032 ) ) ;
#203577 = ORIENTED_EDGE ( 'NONE', *, *, #14809, .T. ) ;
#203578 = ADVANCED_FACE ( 'NONE', ( #141654 ), #103785, .F. ) ;
#203579 = AXIS2_PLACEMENT_3D ( 'NONE', #37095, #95735, #256053 ) ;
#203580 = CARTESIAN_POINT ( 'NONE',  ( -20.85000000000000142, 77.73670573947995877, -158.5056848969006182 ) ) ;
#203581 = FACE_OUTER_BOUND ( 'NONE', #119973, .T. ) ;
#203582 = DIRECTION ( 'NONE',  ( -1.000000000000000000, -0.000000000000000000, -0.000000000000000000 ) ) ;
#203583 = ORIENTED_EDGE ( 'NONE', *, *, #93376, .T. ) ;
#203584 = CARTESIAN_POINT ( 'NONE',  ( 21.05000000000000071, 23.68770167995059239, -252.8127582590406348 ) ) ;
#203586 = ORIENTED_EDGE ( 'NONE', *, *, #171619, .T. ) ;
#203585 = CARTESIAN_POINT ( 'NONE',  ( -18.50000000000000000, 11.75000000001115552, -112.6500000000000341 ) ) ;
#203588 = CARTESIAN_POINT ( 'NONE',  ( -16.80100914604134132, 66.05685090590822028, -82.20606335723671521 ) ) ;
#203587 = DIRECTION ( 'NONE',  ( 1.000000000000000000, -0.000000000000000000, -0.000000000000000000 ) ) ;
#203589 = EDGE_CURVE ( 'NONE', #78774, #120951, #233198, .T. ) ;
#203590 = CARTESIAN_POINT ( 'NONE',  ( -20.94999999999999929, 87.29603075034744109, -139.5710066441881452 ) ) ;
#203591 = ORIENTED_EDGE ( 'NONE', *, *, #168060, .T. ) ;
#203592 = CARTESIAN_POINT ( 'NONE',  ( 17.23472005113828232, 10.30788195451192379, -145.4534231399313740 ) ) ;
#203593 = EDGE_CURVE ( 'NONE', #169497, #40979, #8336, .T. ) ;
#203594 = CYLINDRICAL_SURFACE ( 'NONE', #191748, 0.1000000000000028644 ) ;
#203595 = EDGE_CURVE ( 'NONE', #39887, #95398, #151953, .T. ) ;
#203596 = CARTESIAN_POINT ( 'NONE',  ( 20.94999999999999929, 70.62751970751253339, -223.3325012285725109 ) ) ;
#203597 = CARTESIAN_POINT ( 'NONE',  ( -21.05000000000000071, 70.15000000001148805, -46.15560470880229360 ) ) ;
#203598 = ORIENTED_EDGE ( 'NONE', *, *, #10772, .T. ) ;
#203599 = DIRECTION ( 'NONE',  ( 1.000000000000000000, 0.000000000000000000, 0.000000000000000000 ) ) ;
#203600 = AXIS2_PLACEMENT_3D ( 'NONE', #35325, #75708, #215206 ) ;
#203601 = FACE_OUTER_BOUND ( 'NONE', #183536, .T. ) ;
#203602 = EDGE_CURVE ( 'NONE', #23492, #245468, #7759, .T. ) ;
#203603 = DIRECTION ( 'NONE',  ( 1.000000000000000000, 0.000000000000000000, 0.000000000000000000 ) ) ;
#203604 = DIRECTION ( 'NONE',  ( 0.000000000000000000, 0.1350103645451945777, -0.9908441862701589109 ) ) ;
#203605 = EDGE_LOOP ( 'NONE', ( #47412, #90331, #250912, #22965, #155210 ) ) ;
#203606 = CIRCLE ( 'NONE', #78688, 0.9000000000000014655 ) ;
#203607 = ORIENTED_EDGE ( 'NONE', *, *, #249812, .F. ) ;
#203608 = DIRECTION ( 'NONE',  ( 1.000000000000000000, 0.000000000000000000, -0.000000000000000000 ) ) ;
#203609 = DIRECTION ( 'NONE',  ( -1.000000000000000000, 0.000000000000000000, -1.020425574104004196E-15 ) ) ;
#203610 = CYLINDRICAL_SURFACE ( 'NONE', #94278, 0.1000000000000052097 ) ;
#203611 = DIRECTION ( 'NONE',  ( -0.000000000000000000, 0.1335171055202901413, 0.9910465087640860649 ) ) ;
#203612 = LINE ( 'NONE', #238898, #161780 ) ;
#203614 = CARTESIAN_POINT ( 'NONE',  ( -23.25000000000000000, 1.115600667400684642E-11, -134.0000000000000284 ) ) ;
#203613 = DIRECTION ( 'NONE',  ( 1.000000000000000000, 0.000000000000000000, 0.000000000000000000 ) ) ;
#203615 = CIRCLE ( 'NONE', #53207, 0.1000000000000028644 ) ;
#203617 = DIRECTION ( 'NONE',  ( 0.000000000000000000, -1.000000000000000000, 0.000000000000000000 ) ) ;
#203616 = CIRCLE ( 'NONE', #91193, 0.09999999999999892308 ) ;
#203618 = CYLINDRICAL_SURFACE ( 'NONE', #218470, 0.09999999999998898659 ) ;
#203619 = CARTESIAN_POINT ( 'NONE',  ( -22.48660254037843131, 64.25000000001212186, -136.5731074845243711 ) ) ;
#203620 = AXIS2_PLACEMENT_3D ( 'NONE', #151132, #48159, #32497 ) ;
#203621 = DIRECTION ( 'NONE',  ( 1.000000000000000000, 0.000000000000000000, 0.000000000000000000 ) ) ;
#203623 = ORIENTED_EDGE ( 'NONE', *, *, #53020, .T. ) ;
#203622 = DIRECTION ( 'NONE',  ( -1.000000000000000000, 0.000000000000000000, -0.000000000000000000 ) ) ;
#203624 = CARTESIAN_POINT ( 'NONE',  ( 20.95512820512820440, 65.37615131630076348, -195.8581939154368285 ) ) ;
#203625 = AXIS2_PLACEMENT_3D ( 'NONE', #14784, #52583, #50023 ) ;
#203626 = CARTESIAN_POINT ( 'NONE',  ( 18.49999999999999289, 64.25000000001232081, -161.9231074845244223 ) ) ;
#203628 = FACE_OUTER_BOUND ( 'NONE', #114763, .T. ) ;
#203627 = LINE ( 'NONE', #25018, #21987 ) ;
#203629 = EDGE_CURVE ( 'NONE', #67043, #102764, #197353, .T. ) ;
#203630 = ORIENTED_EDGE ( 'NONE', *, *, #36982, .F. ) ;
#203631 = DIRECTION ( 'NONE',  ( 1.000000000000000000, -0.000000000000000000, -0.000000000000000000 ) ) ;
#203632 = ADVANCED_FACE ( 'NONE', ( #188480 ), #210614, .F. ) ;
#203633 = CARTESIAN_POINT ( 'NONE',  ( 20.94999999999999929, 76.00000000001126921, -203.5231074845248997 ) ) ;
#203634 = CARTESIAN_POINT ( 'NONE',  ( -23.25000000000000000, 0.000000000000000000, -33.50000000000000000 ) ) ;
#203635 = CARTESIAN_POINT ( 'NONE',  ( -21.05000000000000071, 87.65000000001192859, -106.0231074845242176 ) ) ;
#203636 = EDGE_LOOP ( 'NONE', ( #171787, #27858, #105202, #13623 ) ) ;
#203637 = AXIS2_PLACEMENT_3D ( 'NONE', #35535, #95464, #194602 ) ;
#203638 = VECTOR ( 'NONE', #51908, 1000.000000000000000 ) ;
#203639 = VERTEX_POINT ( 'NONE', #9846 ) ;
#203640 = ADVANCED_FACE ( 'NONE', ( #131074 ), #105681, .T. ) ;
#203641 = CYLINDRICAL_SURFACE ( 'NONE', #100912, 0.09999999999999939493 ) ;
#203642 = AXIS2_PLACEMENT_3D ( 'NONE', #187657, #12873, #145924 ) ;
#203643 = ORIENTED_EDGE ( 'NONE', *, *, #157717, .T. ) ;
#203644 = FACE_OUTER_BOUND ( 'NONE', #13203, .T. ) ;
#203645 = ORIENTED_EDGE ( 'NONE', *, *, #55475, .T. ) ;
#203646 = AXIS2_PLACEMENT_3D ( 'NONE', #129136, #31354, #208690 ) ;
#203647 = CARTESIAN_POINT ( 'NONE',  ( -18.40000000000000213, 64.51332499825412015, -78.77310748452438816 ) ) ;
#203648 = AXIS2_PLACEMENT_3D ( 'NONE', #33708, #168082, #70254 ) ;
#203650 = AXIS2_PLACEMENT_3D ( 'NONE', #75591, #37745, #216347 ) ;
#203649 = CARTESIAN_POINT ( 'NONE',  ( 21.05000000000000071, 1.115600667400684642E-11, -67.00000000000000000 ) ) ;
#203651 = AXIS2_PLACEMENT_3D ( 'NONE', #245201, #66562, #146078 ) ;
#203652 = CARTESIAN_POINT ( 'NONE',  ( -20.94560253601877164, 62.83003337064300808, -207.1937220765705661 ) ) ;
#203653 = EDGE_LOOP ( 'NONE', ( #177449, #145490, #233301, #34795 ) ) ;
#203654 = AXIS2_PLACEMENT_3D ( 'NONE', #253505, #155736, #78710 ) ;
#203655 = DIRECTION ( 'NONE',  ( 0.000000000000000000, 0.000000000000000000, 1.000000000000000000 ) ) ;
#203656 = FACE_OUTER_BOUND ( 'NONE', #156276, .T. ) ;
#203657 = DIRECTION ( 'NONE',  ( 1.000000000000000000, 0.000000000000000000, 0.000000000000000000 ) ) ;
#203658 = DIRECTION ( 'NONE',  ( 0.000000000000000000, 0.000000000000000000, -1.000000000000000000 ) ) ;
#203659 = CARTESIAN_POINT ( 'NONE',  ( 18.39999999999999858, 85.40000000001276703, -215.2731074845243029 ) ) ;
#203660 = DIRECTION ( 'NONE',  ( 0.000000000000000000, 0.000000000000000000, 1.000000000000000000 ) ) ;
#203661 = CARTESIAN_POINT ( 'NONE',  ( 21.06600267594171783, 11.17125508431878878, -211.0573669240345112 ) ) ;
#203662 = ADVANCED_FACE ( 'NONE', ( #68546 ), #28653, .T. ) ;
#203663 = ORIENTED_EDGE ( 'NONE', *, *, #102039, .F. ) ;
#203665 = CARTESIAN_POINT ( 'NONE',  ( -22.39999999999999858, 76.00000000001276135, -215.1726782920691505 ) ) ;
#203664 = CARTESIAN_POINT ( 'NONE',  ( -23.15000000000000213, 68.28002175382172823, -222.4371999040225774 ) ) ;
#203666 = VECTOR ( 'NONE', #42946, 1000.000000000000000 ) ;
#203667 = ORIENTED_EDGE ( 'NONE', *, *, #100150, .F. ) ;
#203669 = ORIENTED_EDGE ( 'NONE', *, *, #229525, .T. ) ;
#203668 = DIRECTION ( 'NONE',  ( 0.000000000000000000, 0.2617529984165035128, 0.9651348961777155289 ) ) ;
#203670 = VERTEX_POINT ( 'NONE', #29453 ) ;
#203671 = CARTESIAN_POINT ( 'NONE',  ( -20.85000000000000142, -1.149570369564537842, -141.8159124845019790 ) ) ;
#203672 = AXIS2_PLACEMENT_3D ( 'NONE', #168141, #69015, #229364 ) ;
#203673 = CARTESIAN_POINT ( 'NONE',  ( -2.995603634470829482E-16, -11.74999999998884448, -155.2500000000000284 ) ) ;
#203674 = CARTESIAN_POINT ( 'NONE',  ( 22.39999999999999503, 64.35000000001267040, -203.6231074845244393 ) ) ;
#203675 = CARTESIAN_POINT ( 'NONE',  ( 20.94999999999999929, -11.48912529306489994, -164.6000000000000227 ) ) ;
#203676 = EDGE_LOOP ( 'NONE', ( #71114, #12141 ) ) ;
#203677 = EDGE_CURVE ( 'NONE', #4373, #93991, #16149, .T. ) ;
#203678 = LINE ( 'NONE', #124156, #247182 ) ;
#203679 = CARTESIAN_POINT ( 'NONE',  ( -21.05000000000000071, 2.817198581588411077, -208.4716308468294130 ) ) ;
#203680 = TOROIDAL_SURFACE ( 'NONE', #99580, 0.2000000000000000111, 0.1000000000000000056 ) ;
#203681 = ADVANCED_FACE ( 'NONE', ( #17531 ), #115359, .F. ) ;
#203682 = EDGE_LOOP ( 'NONE', ( #193614, #158972, #16350, #180918, #187386, #123753 ) ) ;
#203683 = AXIS2_PLACEMENT_3D ( 'NONE', #20609, #100092, #135385 ) ;
#203684 = CARTESIAN_POINT ( 'NONE',  ( -20.90851465518106167, 10.32532329026770590, -39.06993430183595706 ) ) ;
#203685 = ADVANCED_FACE ( 'NONE', ( #76224 ), #157077, .T. ) ;
#203686 = CIRCLE ( 'NONE', #107811, 0.2000000000000057288 ) ;
#203687 = CARTESIAN_POINT ( 'NONE',  ( -23.25000000000000355, 9.957490673325212427, -220.1701168356097469 ) ) ;
#203688 = VERTEX_POINT ( 'NONE', #155805 ) ;
#203689 = LINE ( 'NONE', #185407, #239386 ) ;
#203690 = CIRCLE ( 'NONE', #128681, 2.000000000000001776 ) ;
#203691 = ADVANCED_FACE ( 'NONE', ( #55350 ), #236580, .T. ) ;
#203692 = ORIENTED_EDGE ( 'NONE', *, *, #145336, .T. ) ;
#203693 = DIRECTION ( 'NONE',  ( 0.000000000000000000, 0.2818822000685679008, -0.9594490217226259166 ) ) ;
#203696 = ADVANCED_FACE ( 'NONE', ( #39710 ), #137475, .T. ) ;
#203695 = EDGE_CURVE ( 'NONE', #197749, #253373, #240980, .T. ) ;
#203694 = VERTEX_POINT ( 'NONE', #174105 ) ;
#203697 = LINE ( 'NONE', #167168, #37970 ) ;
#203698 = CARTESIAN_POINT ( 'NONE',  ( -22.39999999999999858, 1.115600667400684642E-11, -126.2092204016266379 ) ) ;
#203699 = CARTESIAN_POINT ( 'NONE',  ( 23.14999999999999858, 7.128833340094563376, -233.7327013124401276 ) ) ;
#203700 = TOROIDAL_SURFACE ( 'NONE', #174532, 12.77499999999999858, 0.1000000000000000056 ) ;
#203701 = CIRCLE ( 'NONE', #178798, 0.1999999999999987899 ) ;
#203702 = CARTESIAN_POINT ( 'NONE',  ( 23.25000000000000000, -11.64999999998883595, -88.75000000000004263 ) ) ;
#203703 = DIRECTION ( 'NONE',  ( 2.879366945564059217E-14, -0.9875055080513751582, 0.1575844902526747915 ) ) ;
#203704 = EDGE_CURVE ( 'NONE', #173885, #81780, #95235, .T. ) ;
#203707 = ADVANCED_FACE ( 'NONE', ( #217016 ), #69181, .T. ) ;
#203706 = CARTESIAN_POINT ( 'NONE',  ( -21.98333005346336932, 1.115600667400684642E-11, -26.12592467094331994 ) ) ;
#203705 = AXIS2_PLACEMENT_3D ( 'NONE', #234609, #93807, #153846 ) ;
#203708 = VERTEX_POINT ( 'NONE', #253579 ) ;
#203710 = CARTESIAN_POINT ( 'NONE',  ( -20.64999999999999858, 7.128833340093095217, -233.7327013124392749 ) ) ;
#203709 = SURFACE_SIDE_STYLE ('',( #101999 ) ) ;
#203711 = ORIENTED_EDGE ( 'NONE', *, *, #169881, .T. ) ;
#203712 = DIRECTION ( 'NONE',  ( 0.5932847527679308008, -0.3801118060259208176, -0.7095972217059532960 ) ) ;
#203713 = EDGE_CURVE ( 'NONE', #173980, #19723, #149420, .T. ) ;
#203714 = CYLINDRICAL_SURFACE ( 'NONE', #224735, 0.5000000000000004441 ) ;
#203716 = EDGE_LOOP ( 'NONE', ( #165769, #155593, #58832, #56077 ) ) ;
#203715 = LINE ( 'NONE', #238995, #229465 ) ;
#203718 = VERTEX_POINT ( 'NONE', #16295 ) ;
#203717 = CYLINDRICAL_SURFACE ( 'NONE', #45487, 0.1000000000000028644 ) ;
#203719 = DIRECTION ( 'NONE',  ( -6.938893903907224433E-15, -0.9651348961777157509, 0.2617529984165031243 ) ) ;
#203720 = DIRECTION ( 'NONE',  ( 1.000000000000000000, 0.000000000000000000, 0.000000000000000000 ) ) ;
#203721 = CYLINDRICAL_SURFACE ( 'NONE', #168785, 0.8750000000000007772 ) ;
#203722 = CARTESIAN_POINT ( 'NONE',  ( 18.59999999999999076, 63.81702857804527440, -209.2850695923107480 ) ) ;
#203723 = EDGE_CURVE ( 'NONE', #32289, #145080, #136175, .T. ) ;
#203725 = EDGE_LOOP ( 'NONE', ( #94945, #131020, #448, #49786 ) ) ;
#203724 = FACE_OUTER_BOUND ( 'NONE', #78079, .T. ) ;
#203726 = EDGE_CURVE ( 'NONE', #116896, #74961, #216018, .T. ) ;
#203727 = AXIS2_PLACEMENT_3D ( 'NONE', #160087, #98762, #255256 ) ;
#203728 = CARTESIAN_POINT ( 'NONE',  ( 18.59999999999999432, 70.30054753569015702, -82.06538144109418909 ) ) ;
#203729 = EDGE_LOOP ( 'NONE', ( #122918, #88899, #216241, #107251 ) ) ;
#203730 = ORIENTED_EDGE ( 'NONE', *, *, #112161, .T. ) ;
#203732 = EDGE_CURVE ( 'NONE', #243045, #148687, #160928, .T. ) ;
#203731 = CARTESIAN_POINT ( 'NONE',  ( -20.64999999999999858, 85.00000000001251976, -179.9170766071767389 ) ) ;
#203733 = CARTESIAN_POINT ( 'NONE',  ( 19.96984138294287092, 34.47169263967519726, -235.0498988782159131 ) ) ;
#203734 = ORIENTED_EDGE ( 'NONE', *, *, #165022, .F. ) ;
#203735 = CARTESIAN_POINT ( 'NONE',  ( 21.00000000000000000, 43.94346684630428967, -235.6041041703296344 ) ) ;
#203736 = LINE ( 'NONE', #26399, #57526 ) ;
#203737 = EDGE_CURVE ( 'NONE', #246882, #172022, #22714, .T. ) ;
#203738 = CIRCLE ( 'NONE', #120383, 3.970710678118657189 ) ;
#203739 = CIRCLE ( 'NONE', #224570, 0.09999999999999939493 ) ;
#203740 = ORIENTED_EDGE ( 'NONE', *, *, #216985, .T. ) ;
#203741 = VECTOR ( 'NONE', #77890, 1000.000000000000000 ) ;
#203742 = DIRECTION ( 'NONE',  ( 0.000000000000000000, 7.086529944415894657E-15, -1.000000000000000000 ) ) ;
#203743 = DIRECTION ( 'NONE',  ( -0.000000000000000000, 0.2617529984165031243, 0.9651348961777157509 ) ) ;
#203744 = EDGE_LOOP ( 'NONE', ( #27794, #93561, #56809, #107808 ) ) ;
#203745 = AXIS2_PLACEMENT_3D ( 'NONE', #6659, #84879, #220588 ) ;
#203746 = ORIENTED_EDGE ( 'NONE', *, *, #133585, .F. ) ;
#203747 = CARTESIAN_POINT ( 'NONE',  ( -21.07928932188134041, 61.09751618602216894, -234.2940654522710986 ) ) ;
#203748 = ORIENTED_EDGE ( 'NONE', *, *, #174806, .T. ) ;
#203750 = EDGE_CURVE ( 'NONE', #173650, #219752, #245076, .T. ) ;
#203749 = CARTESIAN_POINT ( 'NONE',  ( -16.83199030136658081, 23.07682551944007443, -231.0099189692009816 ) ) ;
#203751 = VERTEX_POINT ( 'NONE', #240450 ) ;
#203753 = VERTEX_POINT ( 'NONE', #61819 ) ;
#203752 = DIRECTION ( 'NONE',  ( 0.000000000000000000, 0.2617529984165045120, 0.9651348961777153068 ) ) ;
#203754 = CARTESIAN_POINT ( 'NONE',  ( -21.05000000000000071, 76.00000000001237765, -170.0231074845243597 ) ) ;
#203755 = ORIENTED_EDGE ( 'NONE', *, *, #58285, .F. ) ;
#203756 = CARTESIAN_POINT ( 'NONE',  ( -22.00356870069490967, -4.067518095897675031E-12, -93.24575763824979902 ) ) ;
#203757 = CIRCLE ( 'NONE', #137126, 0.5999999999999894307 ) ;
#203758 = CIRCLE ( 'NONE', #12248, 0.1999999999999987899 ) ;
#203759 = ORIENTED_EDGE ( 'NONE', *, *, #151545, .F. ) ;
#203761 = EDGE_LOOP ( 'NONE', ( #110354, #202542, #171437, #19755 ) ) ;
#203760 = ORIENTED_EDGE ( 'NONE', *, *, #36460, .T. ) ;
#203762 = DIRECTION ( 'NONE',  ( 1.000000000000000000, 0.000000000000000000, 0.000000000000000000 ) ) ;
#203763 = CARTESIAN_POINT ( 'NONE',  ( 23.24999999999999289, 51.38014393322265505, -230.1906178717505327 ) ) ;
#203764 = ORIENTED_EDGE ( 'NONE', *, *, #103839, .T. ) ;
#203765 = AXIS2_PLACEMENT_3D ( 'NONE', #30364, #48617, #52456 ) ;
#203766 = ORIENTED_EDGE ( 'NONE', *, *, #58259, .T. ) ;
#203767 = FACE_OUTER_BOUND ( 'NONE', #23616, .T. ) ;
#203768 = DIRECTION ( 'NONE',  ( 0.000000000000000000, -1.000000000000000000, -0.000000000000000000 ) ) ;
#203770 = ORIENTED_EDGE ( 'NONE', *, *, #203072, .F. ) ;
#203769 = CYLINDRICAL_SURFACE ( 'NONE', #144956, 0.09999999999999939493 ) ;
#203771 = CARTESIAN_POINT ( 'NONE',  ( -20.94999999999999929, -11.41227409413852989, -36.50000000000000711 ) ) ;
#203772 = EDGE_LOOP ( 'NONE', ( #80732, #177269, #88764, #224480 ) ) ;
#203773 = CARTESIAN_POINT ( 'NONE',  ( -20.54999999999999716, -9.000000000000001776, -23.60603087734756045 ) ) ;
#203774 = FACE_OUTER_BOUND ( 'NONE', #49509, .T. ) ;
#203775 = ORIENTED_EDGE ( 'NONE', *, *, #151936, .F. ) ;
#203776 = DIRECTION ( 'NONE',  ( -1.000000000000000000, -2.952720810173289112E-16, 0.000000000000000000 ) ) ;
#203777 = ORIENTED_EDGE ( 'NONE', *, *, #188171, .F. ) ;
#203778 = CARTESIAN_POINT ( 'NONE',  ( 20.94999999999999929, 19.09887790564731702, -232.6007267402957837 ) ) ;
#203779 = VERTEX_POINT ( 'NONE', #85185 ) ;
#203780 = AXIS2_PLACEMENT_3D ( 'NONE', #186363, #66404, #3861 ) ;
#203782 = ORIENTED_EDGE ( 'NONE', *, *, #159180, .T. ) ;
#203781 = ORIENTED_EDGE ( 'NONE', *, *, #40078, .T. ) ;
#203783 = ORIENTED_EDGE ( 'NONE', *, *, #100753, .T. ) ;
#203784 = DIRECTION ( 'NONE',  ( 0.000000000000000000, 7.056502275159894776E-15, -1.000000000000000000 ) ) ;
#203785 = ORIENTED_EDGE ( 'NONE', *, *, #30368, .F. ) ;
#203786 = CARTESIAN_POINT ( 'NONE',  ( -17.05016517656093811, 66.05000000001152216, -48.69580548052332603 ) ) ;
#203787 = VECTOR ( 'NONE', #139694, 1000.000000000000000 ) ;
#203788 = ORIENTED_EDGE ( 'NONE', *, *, #14282, .F. ) ;
#203789 = DIRECTION ( 'NONE',  ( -1.000000000000000000, -0.000000000000000000, -0.000000000000000000 ) ) ;
#203790 = DIRECTION ( 'NONE',  ( 0.000000000000000000, 7.026728003956683390E-15, -1.000000000000000000 ) ) ;
#203791 = ORIENTED_EDGE ( 'NONE', *, *, #21054, .T. ) ;
#203792 = EDGE_CURVE ( 'NONE', #103016, #199581, #257663, .T. ) ;
#203793 = VERTEX_POINT ( 'NONE', #222137 ) ;
#203794 = VECTOR ( 'NONE', #98335, 1000.000000000000000 ) ;
#203796 = EDGE_LOOP ( 'NONE', ( #20341, #164703, #117745, #66832 ) ) ;
#203795 = AXIS2_PLACEMENT_3D ( 'NONE', #130819, #16040, #31758 ) ;
#203797 = TOROIDAL_SURFACE ( 'NONE', #124704, 0.2000000000000000111, 0.1000000000000000056 ) ;
#203798 = CARTESIAN_POINT ( 'NONE',  ( -21.14999999999999858, 64.25000000001195133, -102.9231074845243938 ) ) ;
#203799 = ORIENTED_EDGE ( 'NONE', *, *, #68917, .F. ) ;
#203800 = EDGE_CURVE ( 'NONE', #146336, #59523, #121802, .T. ) ;
#203801 = DIRECTION ( 'NONE',  ( 0.000000000000000000, 0.9126074666063660468, 0.4088369013363524762 ) ) ;
#203802 = CARTESIAN_POINT ( 'NONE',  ( -23.25000000000000355, 64.25000000001230660, -157.3731074845244393 ) ) ;
#203803 = DIRECTION ( 'NONE',  ( 1.000000000000000000, 0.000000000000000000, 0.000000000000000000 ) ) ;
#203804 = CARTESIAN_POINT ( 'NONE',  ( -20.94999999999999929, 11.65000000001115588, -127.2161343370219413 ) ) ;
#203805 = TOROIDAL_SURFACE ( 'NONE', #174832, 11.65000000000000036, 0.1000000000000000056 ) ;
#203806 = FACE_OUTER_BOUND ( 'NONE', #189203, .T. ) ;
#203807 = CARTESIAN_POINT ( 'NONE',  ( 21.05000000000000071, 0.09779029131994770863, -127.7421853895238968 ) ) ;
#203808 = EDGE_CURVE ( 'NONE', #189424, #252337, #49446, .T. ) ;
#203809 = CARTESIAN_POINT ( 'NONE',  ( 20.94999999999999929, 70.60000000001205933, -124.1178414656112352 ) ) ;
#203811 = DIRECTION ( 'NONE',  ( 0.000000000000000000, 1.265107689135680095E-16, -1.000000000000000000 ) ) ;
#203810 = CARTESIAN_POINT ( 'NONE',  ( -16.77732147262506146, 66.05403306739360403, -149.1866162412485437 ) ) ;
#203812 = DIRECTION ( 'NONE',  ( 1.000000000000000000, 0.000000000000000000, 0.000000000000000000 ) ) ;
#203813 = FACE_OUTER_BOUND ( 'NONE', #110001, .T. ) ;
#203814 = DIRECTION ( 'NONE',  ( -6.938893903907221278E-15, 0.4721928772777346239, 0.8814952561688430555 ) ) ;
#203815 = CYLINDRICAL_SURFACE ( 'NONE', #105375, 0.09999999999998898659 ) ;
#203816 = ORIENTED_EDGE ( 'NONE', *, *, #94732, .T. ) ;
#203817 = AXIS2_PLACEMENT_3D ( 'NONE', #203854, #125603, #201288 ) ;
#203818 = AXIS2_PLACEMENT_3D ( 'NONE', #23295, #121118, #224020 ) ;
#203819 = EDGE_CURVE ( 'NONE', #184466, #60897, #224721, .T. ) ;
#203821 = VERTEX_POINT ( 'NONE', #47364 ) ;
#203820 = CARTESIAN_POINT ( 'NONE',  ( 18.49999999999999645, 70.30054753569064019, -149.0653814410941607 ) ) ;
#203822 = EDGE_CURVE ( 'NONE', #111919, #121611, #42257, .T. ) ;
#203823 = VERTEX_POINT ( 'NONE', #102182 ) ;
#203824 = VECTOR ( 'NONE', #18458, 1000.000000000000227 ) ;
#203825 = CARTESIAN_POINT ( 'NONE',  ( -20.64999999999999858, 1.999999999999998224, -20.27537807723789953 ) ) ;
#203826 = CARTESIAN_POINT ( 'NONE',  ( 12.25000000000000000, 66.15000000001228386, -153.2731074845244450 ) ) ;
#203827 = EDGE_CURVE ( 'NONE', #244974, #201200, #178464, .T. ) ;
#203828 = ORIENTED_EDGE ( 'NONE', *, *, #3965, .T. ) ;
#203829 = DIRECTION ( 'NONE',  ( 1.000000000000000000, -1.207181226542539700E-16, 2.694675058168174199E-16 ) ) ;
#203830 = ADVANCED_FACE ( 'NONE', ( #223437 ), #46087, .F. ) ;
#203831 = CARTESIAN_POINT ( 'NONE',  ( -21.65000000000000213, 30.25354784785470486, -234.7188954791831748 ) ) ;
#203832 = AXIS2_PLACEMENT_3D ( 'NONE', #202234, #62725, #97961 ) ;
#203833 = ORIENTED_EDGE ( 'NONE', *, *, #33245, .T. ) ;
#203834 = CARTESIAN_POINT ( 'NONE',  ( 20.94999999999999929, -11.64999999998883595, -134.0000000000000284 ) ) ;
#203835 = EDGE_CURVE ( 'NONE', #83655, #208426, #3097, .T. ) ;
#203836 = CARTESIAN_POINT ( 'NONE',  ( 21.05000000000000071, 40.88152484246180052, -238.0427780438910759 ) ) ;
#203838 = EDGE_LOOP ( 'NONE', ( #229148, #47387, #224836, #120869, #33549, #103465 ) ) ;
#203837 = LINE ( 'NONE', #145137, #147719 ) ;
#203839 = DIRECTION ( 'NONE',  ( 0.000000000000000000, -0.9126074666063771490, -0.4088369013363281623 ) ) ;
#203841 = VERTEX_POINT ( 'NONE', #23993 ) ;
#203840 = DIRECTION ( 'NONE',  ( 1.000000000000000000, -0.000000000000000000, -0.000000000000000000 ) ) ;
#203842 = DIRECTION ( 'NONE',  ( 0.000000000000000000, -0.2617529984165031243, -0.9651348961777158619 ) ) ;
#203843 = DIRECTION ( 'NONE',  ( -6.938893903907222856E-15, -1.000000000000000000, -6.982962677686266711E-15 ) ) ;
#203844 = VERTEX_POINT ( 'NONE', #244286 ) ;
#203845 = CARTESIAN_POINT ( 'NONE',  ( -16.94180778212363236, 66.00755694428015374, -157.4189239139911649 ) ) ;
#203846 = CIRCLE ( 'NONE', #12347, 0.09999999999999459321 ) ;
#203848 = EDGE_CURVE ( 'NONE', #74863, #207108, #65656, .T. ) ;
#203847 = DIRECTION ( 'NONE',  ( -1.000000000000000000, 1.652117596168391700E-15, 0.000000000000000000 ) ) ;
#203850 = DIRECTION ( 'NONE',  ( 0.000000000000000000, 0.2128009952263403282, -0.9770955615653358350 ) ) ;
#203849 = CARTESIAN_POINT ( 'NONE',  ( -16.93826681692523550, 63.05143189155258909, -213.0194121372203995 ) ) ;
#203851 = DIRECTION ( 'NONE',  ( 0.000000000000000000, 0.000000000000000000, 1.000000000000000000 ) ) ;
#203852 = CIRCLE ( 'NONE', #141318, 12.97499999999998721 ) ;
#203853 = FACE_OUTER_BOUND ( 'NONE', #60145, .T. ) ;
#203854 = CARTESIAN_POINT ( 'NONE',  ( -22.50000000000000000, 1.115600667400684642E-11, -100.5000000000000284 ) ) ;
#203855 = CARTESIAN_POINT ( 'NONE',  ( 19.99999999999998934, 16.76897757977919312, -222.7804130109902871 ) ) ;
#203856 = CARTESIAN_POINT ( 'NONE',  ( 21.97500000000000497, 66.25000000001179501, -81.77310748452437394 ) ) ;
#203858 = ORIENTED_EDGE ( 'NONE', *, *, #184549, .F. ) ;
#203857 = AXIS2_PLACEMENT_3D ( 'NONE', #169920, #212861, #32977 ) ;
#203859 = DIRECTION ( 'NONE',  ( 1.000000000000000000, 0.000000000000000000, 0.000000000000000000 ) ) ;
#203860 = ORIENTED_EDGE ( 'NONE', *, *, #161085, .F. ) ;
#203861 = ORIENTED_EDGE ( 'NONE', *, *, #50896, .T. ) ;
#203862 = CARTESIAN_POINT ( 'NONE',  ( -21.04386569057570355, 11.74999999999978506, -26.64283735177988532 ) ) ;
#203863 = DIRECTION ( 'NONE',  ( 0.000000000000000000, 0.9908441862701791170, -0.1350103645450472789 ) ) ;
#203864 = ORIENTED_EDGE ( 'NONE', *, *, #209350, .T. ) ;
#203865 = AXIS2_PLACEMENT_3D ( 'NONE', #59575, #93609, #74080 ) ;
#203866 = ORIENTED_EDGE ( 'NONE', *, *, #250205, .F. ) ;
#203867 = AXIS2_PLACEMENT_3D ( 'NONE', #97906, #220472, #43110 ) ;
#203868 =( NAMED_UNIT ( * ) SI_UNIT ( $, .STERADIAN. ) SOLID_ANGLE_UNIT ( ) );
#203869 = B_SPLINE_CURVE_WITH_KNOTS ( 'NONE', 3,
 ( #62519, #123779, #19549, #238582, #99044, #41685 ),
 .UNSPECIFIED., .F., .F.,
 ( 4, 2, 4 ),
 ( 4.336808689942017736E-19, 0.0001569047307838686138, 0.0003138094615677367938 ),
 .UNSPECIFIED. ) ;
#203870 = VERTEX_POINT ( 'NONE', #26555 ) ;
#203871 = CARTESIAN_POINT ( 'NONE',  ( 18.59999999999999787, 86.35479209693758662, -142.7665665014505407 ) ) ;
#203872 = AXIS2_PLACEMENT_3D ( 'NONE', #118539, #206707, #161512 ) ;
#203873 = ORIENTED_EDGE ( 'NONE', *, *, #79163, .F. ) ;
#203874 = EDGE_CURVE ( 'NONE', #98813, #123176, #106045, .T. ) ;
#203875 = DIRECTION ( 'NONE',  ( 1.000000000000000000, 0.000000000000000000, 0.000000000000000000 ) ) ;
#203876 = DIRECTION ( 'NONE',  ( 0.000000000000000000, 0.000000000000000000, -1.000000000000000000 ) ) ;
#203877 = LINE ( 'NONE', #25267, #201158 ) ;
#203878 = LINE ( 'NONE', #244282, #107468 ) ;
#203879 = CARTESIAN_POINT ( 'NONE',  ( -20.64999999999999858, 76.00000000001244871, -170.0231074845243597 ) ) ;
#203880 = CARTESIAN_POINT ( 'NONE',  ( 23.24999999999997513, 56.02567683926420727, -227.9999002286038774 ) ) ;
#203881 = DIRECTION ( 'NONE',  ( 1.186688945009010077E-16, 0.4088369013363281068, -0.9126074666063770380 ) ) ;
#203883 = ORIENTED_EDGE ( 'NONE', *, *, #187446, .F. ) ;
#203882 = LINE ( 'NONE', #83896, #154860 ) ;
#203885 = DIRECTION ( 'NONE',  ( 0.000000000000000000, 0.000000000000000000, -1.000000000000000000 ) ) ;
#203884 = CARTESIAN_POINT ( 'NONE',  ( -16.97683809663752186, 66.05000000001226113, -149.9254715027207681 ) ) ;
#203886 = EDGE_CURVE ( 'NONE', #247461, #183161, #91135, .T. ) ;
#203887 = DIRECTION ( 'NONE',  ( 0.000000000000000000, 0.000000000000000000, -1.000000000000000000 ) ) ;
#203888 = EDGE_CURVE ( 'NONE', #121144, #168296, #103481, .T. ) ;
#203889 = VERTEX_POINT ( 'NONE', #86478 ) ;
#203890 = DIRECTION ( 'NONE',  ( 1.000000000000000000, 0.000000000000000000, 0.000000000000000000 ) ) ;
#203891 = CARTESIAN_POINT ( 'NONE',  ( -20.54999999999999716, 1.115600667400684642E-11, -54.12500000000000711 ) ) ;
#203892 = ORIENTED_EDGE ( 'NONE', *, *, #138143, .F. ) ;
#203893 = ADVANCED_FACE ( 'NONE', ( #166084 ), #145288, .F. ) ;
#203895 = CARTESIAN_POINT ( 'NONE',  ( -21.08479644141222664, 6.345038657743046429, -33.44144555743587688 ) ) ;
#203894 = DIRECTION ( 'NONE',  ( -1.000000000000000000, 0.000000000000000000, -0.000000000000000000 ) ) ;
#203896 = ADVANCED_FACE ( 'NONE', ( #66944 ), #12139, .F. ) ;
#203897 = AXIS2_PLACEMENT_3D ( 'NONE', #43965, #46514, #132490 ) ;
#203898 = EDGE_CURVE ( 'NONE', #191859, #148589, #128212, .T. ) ;
#203899 = DIRECTION ( 'NONE',  ( 0.000000000000000000, 6.982962677686266711E-15, -1.000000000000000000 ) ) ;
#203900 = EDGE_CURVE ( 'NONE', #173746, #54193, #45340, .T. ) ;
#203901 = VERTEX_POINT ( 'NONE', #129495 ) ;
#203902 = CARTESIAN_POINT ( 'NONE',  ( -22.47071067811865319, 68.27992525551432834, -170.1221999392270163 ) ) ;
#203903 = DIRECTION ( 'NONE',  ( 0.000000000000000000, 0.000000000000000000, 1.000000000000000000 ) ) ;
#203904 = EDGE_CURVE ( 'NONE', #61363, #125880, #66008, .T. ) ;
#203905 = DIRECTION ( 'NONE',  ( 1.000000000000000000, 0.000000000000000000, 0.000000000000000000 ) ) ;
#203906 = DIRECTION ( 'NONE',  ( 0.000000000000000000, 0.000000000000000000, 1.000000000000000000 ) ) ;
#203907 = ORIENTED_EDGE ( 'NONE', *, *, #93518, .F. ) ;
#203908 = ORIENTED_EDGE ( 'NONE', *, *, #30844, .T. ) ;
#203909 = CARTESIAN_POINT ( 'NONE',  ( 23.14999999999999503, 64.35000000001204512, -124.3731074845243825 ) ) ;
#203910 = DIRECTION ( 'NONE',  ( 0.000000000000000000, -0.9651348961777379554, 0.2617529984164210233 ) ) ;
#203911 = VECTOR ( 'NONE', #61900, 1000.000000000000000 ) ;
#203912 = CARTESIAN_POINT ( 'NONE',  ( 22.50000000000000000, 75.90000000001222702, -148.2731074845243029 ) ) ;
#203914 = DIRECTION ( 'NONE',  ( 1.000000000000000000, 0.000000000000000000, 0.000000000000000000 ) ) ;
#203913 = AXIS2_PLACEMENT_3D ( 'NONE', #126547, #125265, #26173 ) ;
#203915 = VECTOR ( 'NONE', #38469, 1000.000000000000000 ) ;
#203916 = AXIS2_PLACEMENT_3D ( 'NONE', #251647, #173456, #70484 ) ;
#203917 = DIRECTION ( 'NONE',  ( 1.000000000000000000, 0.000000000000000000, 0.000000000000000000 ) ) ;
#203918 = DIRECTION ( 'NONE',  ( 0.000000000000000000, -1.000000000000000000, 0.000000000000000000 ) ) ;
#203919 = CARTESIAN_POINT ( 'NONE',  ( 23.15000000000000213, 88.41227409416113403, -39.12310748452424036 ) ) ;
#203920 = EDGE_CURVE ( 'NONE', #182190, #15852, #171234, .T. ) ;
#203922 = VERTEX_POINT ( 'NONE', #186924 ) ;
#203921 = CARTESIAN_POINT ( 'NONE',  ( -23.25000000000000355, 45.89348038176515843, -239.2231437130149061 ) ) ;
#203923 = CIRCLE ( 'NONE', #162254, 0.09999999999999939493 ) ;
#203924 = CARTESIAN_POINT ( 'NONE',  ( -21.07928932188134041, 0.09889514566555068775, -94.17148334360673800 ) ) ;
#203925 = CARTESIAN_POINT ( 'NONE',  ( -16.77431908686106610, 66.05419424549388907, -90.35894670217462021 ) ) ;
#203926 = DIRECTION ( 'NONE',  ( -0.000000000000000000, 1.000000000000000000, 6.982962677686266711E-15 ) ) ;
#203927 = DIRECTION ( 'NONE',  ( 0.000000000000000000, -0.7071067811865479058, -0.7071067811865472397 ) ) ;
#203928 = CARTESIAN_POINT ( 'NONE',  ( -20.85000000000000142, 7.021664781911246322, -104.3335654018973315 ) ) ;
#203929 = EDGE_CURVE ( 'NONE', #167394, #30387, #191117, .T. ) ;
#203931 = EDGE_LOOP ( 'NONE', ( #195156, #60809, #239859, #16148, #175880 ) ) ;
#203930 = CARTESIAN_POINT ( 'NONE',  ( 21.05000000000000071, 70.60000000001259934, -191.1178414656113205 ) ) ;
#203933 = FACE_OUTER_BOUND ( 'NONE', #18690, .T. ) ;
#203932 = APPLICATION_CONTEXT ( 'automotive_design' ) ;
#203935 = ADVANCED_FACE ( 'NONE', ( #147780 ), #169949, .F. ) ;
#203934 = CARTESIAN_POINT ( 'NONE',  ( -18.56579813702275672, 65.66974365629718591, -164.4360145562605169 ) ) ;
#203936 = FACE_OUTER_BOUND ( 'NONE', #50128, .T. ) ;
#203937 = PLANE ( 'NONE',  #11536 ) ;
#203938 = ORIENTED_EDGE ( 'NONE', *, *, #104406, .T. ) ;
#203939 = CARTESIAN_POINT ( 'NONE',  ( -19.89999999999999858, 11.61130914238355771, 16.60000000000000142 ) ) ;
#203940 = DIRECTION ( 'NONE',  ( 0.000000000000000000, -1.000000000000000000, -6.982962677686265922E-15 ) ) ;
#203941 = AXIS2_PLACEMENT_3D ( 'NONE', #252634, #231822, #34928 ) ;
#203942 = CARTESIAN_POINT ( 'NONE',  ( 23.25000000000000000, 11.75000000001116263, -155.3500000000000227 ) ) ;
#203943 = VECTOR ( 'NONE', #96565, 1000.000000000000114 ) ;
#203944 = DIRECTION ( 'NONE',  ( 1.000000000000000000, 0.000000000000000000, 0.000000000000000000 ) ) ;
#203945 = ORIENTED_EDGE ( 'NONE', *, *, #130440, .F. ) ;
#203946 = CARTESIAN_POINT ( 'NONE',  ( -16.87401514999228525, 9.950000000011137047, -87.78001799253213733 ) ) ;
#203947 = ORIENTED_EDGE ( 'NONE', *, *, #18022, .T. ) ;
#203948 = CARTESIAN_POINT ( 'NONE',  ( 22.32929514600007792, 59.89092396606481117, -233.9670141766093536 ) ) ;
#203949 = DIRECTION ( 'NONE',  ( 1.000000000000000000, 0.000000000000000000, 0.000000000000000000 ) ) ;
#203950 =( BOUNDED_CURVE ( )  B_SPLINE_CURVE ( 3, ( #207035, #106618, #184895, #122367 ),
 .UNSPECIFIED., .F., .F. ) 
 B_SPLINE_CURVE_WITH_KNOTS ( ( 4, 4 ),
 ( 0.06456096931748307732, 3.077031684272310219 ),
 .UNSPECIFIED. ) 
 CURVE ( )  GEOMETRIC_REPRESENTATION_ITEM ( )  RATIONAL_B_SPLINE_CURVE ( ( 1.000000000000000000, 0.3763440860215093164, 0.3763440860215093164, 1.000000000000000000 ) ) 
 REPRESENTATION_ITEM ( '' )  );
#203951 = PLANE ( 'NONE',  #174674 ) ;
#203952 = CARTESIAN_POINT ( 'NONE',  ( 18.54116936837187879, -9.463564198361289925, -174.5485424908883090 ) ) ;
#203953 = ORIENTED_EDGE ( 'NONE', *, *, #33022, .T. ) ;
#203954 = CARTESIAN_POINT ( 'NONE',  ( 20.85000000000000142, 78.55027968977005060, -232.7019340424676841 ) ) ;
#203955 = CARTESIAN_POINT ( 'NONE',  ( 20.95512820512820440, 12.96604748760833203, -210.6109454999921411 ) ) ;
#203956 = DIRECTION ( 'NONE',  ( 0.000000000000000000, 1.000000000000000000, 0.000000000000000000 ) ) ;
#203957 = DIRECTION ( 'NONE',  ( 0.000000000000000000, -0.5000000000000078826, 0.8660254037844340447 ) ) ;
#203958 = DIRECTION ( 'NONE',  ( -1.000000000000000000, -0.000000000000000000, 0.000000000000000000 ) ) ;
#203959 = EDGE_LOOP ( 'NONE', ( #223121, #25134 ) ) ;
#203961 = VERTEX_POINT ( 'NONE', #52502 ) ;
#203960 = DIRECTION ( 'NONE',  ( 1.000000000000000000, 0.000000000000000000, 0.000000000000000000 ) ) ;
#203962 = ORIENTED_EDGE ( 'NONE', *, *, #216324, .F. ) ;
#203963 = FACE_OUTER_BOUND ( 'NONE', #122199, .T. ) ;
#203964 = VERTEX_POINT ( 'NONE', #151654 ) ;
#203965 = CARTESIAN_POINT ( 'NONE',  ( 21.07928932188134397, 61.09751618602741985, -234.2940654522722639 ) ) ;
#203966 = DIRECTION ( 'NONE',  ( 1.000000000000000000, -3.265361837132813093E-16, -2.280189983783949500E-30 ) ) ;
#203967 = DIRECTION ( 'NONE',  ( 0.000000000000000000, 1.000000000000000000, 0.000000000000000000 ) ) ;
#203968 = CIRCLE ( 'NONE', #150021, 0.5000000000000022204 ) ;
#203969 = VERTEX_POINT ( 'NONE', #91649 ) ;
#203970 = CARTESIAN_POINT ( 'NONE',  ( 18.39999999999999503, 9.957490673325212427, -220.1701168356097469 ) ) ;
#203971 = FACE_OUTER_BOUND ( 'NONE', #59981, .T. ) ;
#203972 = CARTESIAN_POINT ( 'NONE',  ( 23.14999999999999147, 36.65892442174472876, -249.5511627012454596 ) ) ;
#203973 = ORIENTED_EDGE ( 'NONE', *, *, #88852, .F. ) ;
#203974 = CARTESIAN_POINT ( 'NONE',  ( 22.50014994444007499, 11.74971973190324448, -100.4169198432808372 ) ) ;
#203975 = EDGE_CURVE ( 'NONE', #14901, #218733, #211761, .T. ) ;
#203977 = VERTEX_POINT ( 'NONE', #111211 ) ;
#203976 = DIRECTION ( 'NONE',  ( 1.000000000000000000, 0.000000000000000000, 0.000000000000000000 ) ) ;
#203978 = PLANE ( 'NONE',  #10955 ) ;
#203979 = DIRECTION ( 'NONE',  ( 0.000000000000000000, 0.000000000000000000, 1.000000000000000000 ) ) ;
#203980 = ADVANCED_FACE ( 'NONE', ( #48658 ), #248152, .F. ) ;
#203981 = TOROIDAL_SURFACE ( 'NONE', #78875, 11.70000000000000639, 0.1000000000000000056 ) ;
#203982 = AXIS2_PLACEMENT_3D ( 'NONE', #75422, #179642, #57081 ) ;
#203983 = ORIENTED_EDGE ( 'NONE', *, *, #167510, .F. ) ;
#203984 = CARTESIAN_POINT ( 'NONE',  ( 21.05000000000000071, 69.52293297888763846, -169.9231074845244507 ) ) ;
#203986 = EDGE_CURVE ( 'NONE', #20467, #181320, #220137, .T. ) ;
#203985 = DIRECTION ( 'NONE',  ( 0.000000000000000000, -0.8660254037844377084, -0.5000000000000016653 ) ) ;
#203987 = CARTESIAN_POINT ( 'NONE',  ( -23.25000000000000000, 71.85000000001254250, -182.3731074845244109 ) ) ;
#203989 = ADVANCED_FACE ( 'NONE', ( #70830 ), #152943, .T. ) ;
#203988 = VERTEX_POINT ( 'NONE', #232465 ) ;
#203990 = FACE_OUTER_BOUND ( 'NONE', #146366, .T. ) ;
#203991 = CIRCLE ( 'NONE', #96213, 2.700000000000001066 ) ;
#203992 = CARTESIAN_POINT ( 'NONE',  ( -21.33487959338958362, 6.725558151922345296, -100.5000000000000284 ) ) ;
#203993 = TOROIDAL_SURFACE ( 'NONE', #79071, 11.70000000000000639, 0.1000000000000000056 ) ;
#203994 = VERTEX_POINT ( 'NONE', #132057 ) ;
#203995 = TOROIDAL_SURFACE ( 'NONE', #104017, 0.6000000000000013101, 0.1000000000000000056 ) ;
#203996 = ADVANCED_FACE ( 'NONE', ( #211603 ), #209028, .F. ) ;
#203998 = EDGE_CURVE ( 'NONE', #95676, #234784, #120393, .T. ) ;
#203997 = AXIS2_PLACEMENT_3D ( 'NONE', #146551, #74457, #27950 ) ;
#203999 = AXIS2_PLACEMENT_3D ( 'NONE', #180162, #81024, #160615 ) ;
#204000 = ORIENTED_EDGE ( 'NONE', *, *, #221851, .T. ) ;
#204001 = DIRECTION ( 'NONE',  ( 0.000000000000000000, 6.769652589177784668E-15, -1.000000000000000000 ) ) ;
#204002 = ORIENTED_EDGE ( 'NONE', *, *, #199536, .F. ) ;
#204003 = DIRECTION ( 'NONE',  ( -0.000000000000000000, 0.000000000000000000, -1.000000000000000000 ) ) ;
#204004 = AXIS2_PLACEMENT_3D ( 'NONE', #170541, #250020, #71406 ) ;
#204005 = CARTESIAN_POINT ( 'NONE',  ( -16.97683810757273193, 66.05000000001255955, -183.2866841969855614 ) ) ;
#204007 = VERTEX_POINT ( 'NONE', #73400 ) ;
#204006 = FACE_OUTER_BOUND ( 'NONE', #233884, .T. ) ;
#204008 = DIRECTION ( 'NONE',  ( 0.000000000000000000, 0.1332476588733589318, -0.9910827722268049644 ) ) ;
#204009 = CARTESIAN_POINT ( 'NONE',  ( 18.39999999999999503, 11.75000000001113953, -154.8500000000000227 ) ) ;
#204010 = CARTESIAN_POINT ( 'NONE',  ( 21.08479644141222309, 75.94144555744755110, -75.86814614225623643 ) ) ;
#204011 = FACE_OUTER_BOUND ( 'NONE', #124207, .T. ) ;
#204012 = DIRECTION ( 'NONE',  ( 1.000000000000000000, 0.000000000000000000, 0.000000000000000000 ) ) ;
#204013 = DIRECTION ( 'NONE',  ( 0.000000000000000000, 0.9394191166662618775, 0.3427706569150580362 ) ) ;
#204015 = EDGE_CURVE ( 'NONE', #91470, #164331, #103758, .T. ) ;
#204014 = DIRECTION ( 'NONE',  ( 0.000000000000000000, 1.000000000000000000, 0.000000000000000000 ) ) ;
#204017 = ORIENTED_EDGE ( 'NONE', *, *, #253911, .T. ) ;
#204016 = CYLINDRICAL_SURFACE ( 'NONE', #223470, 0.09999999999999939493 ) ;
#204018 = DIRECTION ( 'NONE',  ( 1.000000000000000000, 0.000000000000000000, 0.000000000000000000 ) ) ;
#204019 = ORIENTED_EDGE ( 'NONE', *, *, #251302, .T. ) ;
#204020 = EDGE_CURVE ( 'NONE', #32089, #66589, #45534, .T. ) ;
#204021 = CARTESIAN_POINT ( 'NONE',  ( 21.13736287352038445, 44.91364453899298326, -237.0359499855415777 ) ) ;
#204022 = DIRECTION ( 'NONE',  ( -0.000000000000000000, 0.9579639084728051035, 0.2868887416116349121 ) ) ;
#204023 = DIRECTION ( 'NONE',  ( 0.000000000000000000, -0.01562499999996343723, -0.9998779222360104635 ) ) ;
#204025 = ADVANCED_FACE ( 'NONE', ( #29153, #38108, #94201 ), #159344, .T. ) ;
#204024 = CARTESIAN_POINT ( 'NONE',  ( -22.39999999999999858, 64.35000000001195986, -102.9231074845243938 ) ) ;
#204026 = DIRECTION ( 'NONE',  ( 0.000000000000000000, 0.000000000000000000, 1.000000000000000000 ) ) ;
#204027 = ORIENTED_EDGE ( 'NONE', *, *, #117874, .T. ) ;
#204028 = EDGE_CURVE ( 'NONE', #127614, #36019, #176341, .T. ) ;
#204029 = CIRCLE ( 'NONE', #204214, 0.09999999999998898659 ) ;
#204030 = CARTESIAN_POINT ( 'NONE',  ( 20.94999999999999574, 6.550000000000003375, -9.843822089683131438 ) ) ;
#204031 = CARTESIAN_POINT ( 'NONE',  ( -21.14999999999999858, 6.540656951712397138, -100.5000000000000284 ) ) ;
#204032 = CIRCLE ( 'NONE', #62400, 0.2000000000000057288 ) ;
#204033 = ADVANCED_FACE ( 'NONE', ( #57636 ), #207879, .T. ) ;
#204034 = VERTEX_POINT ( 'NONE', #178925 ) ;
#204035 = CIRCLE ( 'NONE', #8248, 0.1000000000000028644 ) ;
#204036 = CARTESIAN_POINT ( 'NONE',  ( -18.50000000000000000, 30.09302283515540211, -235.6538990729184491 ) ) ;
#204037 =( BOUNDED_CURVE ( )  B_SPLINE_CURVE ( 3, ( #139467, #238581, #162922, #182479 ),
 .UNSPECIFIED., .F., .T. ) 
 B_SPLINE_CURVE_WITH_KNOTS ( ( 4, 4 ),
 ( 1.570796326794892339, 3.141592653589784678 ),
 .UNSPECIFIED. ) 
 CURVE ( )  GEOMETRIC_REPRESENTATION_ITEM ( )  RATIONAL_B_SPLINE_CURVE ( ( 1.000000000000000000, 0.8047378541243659367, 0.8047378541243659367, 1.000000000000000000 ) ) 
 REPRESENTATION_ITEM ( '' )  );
#204038 = CARTESIAN_POINT ( 'NONE',  ( 21.05000000000000071, 69.35000000001207354, -126.6792853948412159 ) ) ;
#204039 = ORIENTED_EDGE ( 'NONE', *, *, #36737, .T. ) ;
#204040 = DIRECTION ( 'NONE',  ( -0.000000000000000000, -0.000000000000000000, -1.000000000000000000 ) ) ;
#204041 = EDGE_LOOP ( 'NONE', ( #85823, #242442, #35182, #133936 ) ) ;
#204042 = ADVANCED_FACE ( 'NONE', ( #236286 ), #235017, .T. ) ;
#204043 = CARTESIAN_POINT ( 'NONE',  ( -12.25000000000000533, 9.350000000011133849, -50.01856895740264264 ) ) ;
#204044 = VERTEX_POINT ( 'NONE', #239 ) ;
#204045 = AXIS2_PLACEMENT_3D ( 'NONE', #176704, #211979, #153311 ) ;
#204046 = DIRECTION ( 'NONE',  ( -1.000000000000000000, 0.000000000000000000, 1.073024830501117725E-15 ) ) ;
#204047 = EDGE_CURVE ( 'NONE', #179805, #109234, #3842, .T. ) ;
#204048 = CIRCLE ( 'NONE', #241490, 11.80000000000000426 ) ;
#204049 = CARTESIAN_POINT ( 'NONE',  ( 18.59999999999999076, 16.67126802362266247, -222.8016931105129004 ) ) ;
#204050 = ORIENTED_EDGE ( 'NONE', *, *, #57283, .F. ) ;
#204051 = DIRECTION ( 'NONE',  ( 0.000000000000000000, 6.982962677686266711E-15, -1.000000000000000000 ) ) ;
#204053 = VERTEX_POINT ( 'NONE', #34276 ) ;
#204052 = DIRECTION ( 'NONE',  ( 0.000000000000000000, 0.000000000000000000, -1.000000000000000000 ) ) ;
#204054 = CARTESIAN_POINT ( 'NONE',  ( -21.65000000000000213, 66.05000000001157900, -56.77310748452439526 ) ) ;
#204055 = AXIS2_PLACEMENT_3D ( 'NONE', #94152, #173758, #154188 ) ;
#204056 = ORIENTED_EDGE ( 'NONE', *, *, #189777, .F. ) ;
#204057 = ORIENTED_EDGE ( 'NONE', *, *, #153853, .T. ) ;
#204058 = DIRECTION ( 'NONE',  ( -1.000000000000000000, 1.207181226542539700E-16, -2.694675058168174199E-16 ) ) ;
#204059 = CARTESIAN_POINT ( 'NONE',  ( -20.94999999999999929, 79.19526988099229925, -196.1889237952725296 ) ) ;
#204060 = CARTESIAN_POINT ( 'NONE',  ( -21.05000000000000071, 6.300000000011169554, -100.6000000000000369 ) ) ;
#204061 = CARTESIAN_POINT ( 'NONE',  ( -18.50000000000000000, -1.164121893230052995, -175.2148480855716173 ) ) ;
#204062 = CARTESIAN_POINT ( 'NONE',  ( -15.39946565075091200, 66.61046543766590844, -187.8482981801344920 ) ) ;
#204063 = CARTESIAN_POINT ( 'NONE',  ( 23.24999999999999645, 70.35000000001255671, -182.6731074845243938 ) ) ;
#204064 = ORIENTED_EDGE ( 'NONE', *, *, #122270, .F. ) ;
#204065 = DIRECTION ( 'NONE',  ( -1.000000000000000000, 7.304098846218135653E-16, -4.607487905232624742E-31 ) ) ;
#204066 = FACE_OUTER_BOUND ( 'NONE', #3778, .T. ) ;
#204067 = CARTESIAN_POINT ( 'NONE',  ( 18.59999999999999076, 6.550000000011156231, -188.7499999999999716 ) ) ;
#204068 = AXIS2_PLACEMENT_3D ( 'NONE', #44632, #21244, #254937 ) ;
#204069 = FACE_OUTER_BOUND ( 'NONE', #44957, .T. ) ;
#204070 = AXIS2_PLACEMENT_3D ( 'NONE', #132182, #193455, #34391 ) ;
#204071 = ORIENTED_EDGE ( 'NONE', *, *, #174155, .F. ) ;
#204072 = CARTESIAN_POINT ( 'NONE',  ( -23.25000000000000000, 76.00000000001126921, -203.5231074845248997 ) ) ;
#204073 = ORIENTED_EDGE ( 'NONE', *, *, #232337, .F. ) ;
#204074 = DIRECTION ( 'NONE',  ( 1.000000000000000000, 0.000000000000000000, 0.000000000000000000 ) ) ;
#204075 = ORIENTED_EDGE ( 'NONE', *, *, #81200, .T. ) ;
#204076 = CARTESIAN_POINT ( 'NONE',  ( -15.15766958671842879, 25.17626390180108231, -232.7245615205268336 ) ) ;
#204077 = CARTESIAN_POINT ( 'NONE',  ( 20.85000000000000142, -11.64999999999999147, -30.59999999999999432 ) ) ;
#204078 = ORIENTED_EDGE ( 'NONE', *, *, #54465, .T. ) ;
#204080 = ORIENTED_EDGE ( 'NONE', *, *, #34592, .F. ) ;
#204079 = LINE ( 'NONE', #5871, #257025 ) ;
#204081 = DIRECTION ( 'NONE',  ( 5.421010862427554711E-16, -1.000000000000000000, -3.252606517456533024E-15 ) ) ;
#204082 = VERTEX_POINT ( 'NONE', #99320 ) ;
#204083 = CARTESIAN_POINT ( 'NONE',  ( -22.49756042579671700, 0.07804633702833754794, -21.85013503889767605 ) ) ;
#204084 = CARTESIAN_POINT ( 'NONE',  ( -18.59999999999999787, 65.66751761918648356, -63.92826094061123143 ) ) ;
#204085 = VERTEX_POINT ( 'NONE', #177635 ) ;
#204087 = VECTOR ( 'NONE', #46052, 1000.000000000000000 ) ;
#204086 = DIRECTION ( 'NONE',  ( -0.000000000000000000, 1.000000000000000000, 1.734723475976807292E-15 ) ) ;
#204088 = EDGE_CURVE ( 'NONE', #219655, #66786, #255807, .T. ) ;
#204089 = CIRCLE ( 'NONE', #191675, 0.09999999999999939493 ) ;
#204091 = CARTESIAN_POINT ( 'NONE',  ( 23.24999999999999289, 23.34004772283015683, -229.2004250369967338 ) ) ;
#204090 = AXIS2_PLACEMENT_3D ( 'NONE', #40029, #14026, #34893 ) ;
#204092 = ORIENTED_EDGE ( 'NONE', *, *, #236961, .F. ) ;
#204093 = ORIENTED_EDGE ( 'NONE', *, *, #212736, .F. ) ;
#204094 = AXIS2_PLACEMENT_3D ( 'NONE', #171896, #252661, #37497 ) ;
#204095 = CYLINDRICAL_SURFACE ( 'NONE', #172369, 0.09999999999999939493 ) ;
#204096 = EDGE_CURVE ( 'NONE', #101735, #219381, #24719, .T. ) ;
#204097 = DIRECTION ( 'NONE',  ( 0.000000000000000000, 0.000000000000000000, 1.000000000000000000 ) ) ;
#204099 = ORIENTED_EDGE ( 'NONE', *, *, #14035, .T. ) ;
#204098 = CARTESIAN_POINT ( 'NONE',  ( 18.39999999999999858, 85.50000000001189449, -95.99103808782457747 ) ) ;
#204100 = ADVANCED_FACE ( 'NONE', ( #215440 ), #137187, .T. ) ;
#204101 = DIRECTION ( 'NONE',  ( 1.000000000000000000, 0.000000000000000000, 0.000000000000000000 ) ) ;
#204103 = EDGE_CURVE ( 'NONE', #103641, #194468, #167424, .T. ) ;
#204102 = AXIS2_PLACEMENT_3D ( 'NONE', #216075, #161266, #196517 ) ;
#204104 = CARTESIAN_POINT ( 'NONE',  ( 20.94999999999999929, 85.40000000001221281, -146.4170766071767389 ) ) ;
#204105 = CARTESIAN_POINT ( 'NONE',  ( -16.89797118371625828, 9.976380722655289190, -121.4372933675582260 ) ) ;
#204106 = VECTOR ( 'NONE', #139002, 1000.000000000000000 ) ;
#204108 = CARTESIAN_POINT ( 'NONE',  ( -23.15000000000000213, 31.44980407958350455, -233.5445995079518866 ) ) ;
#204107 = DIRECTION ( 'NONE',  ( 0.000000000000000000, 0.000000000000000000, -1.000000000000000000 ) ) ;
#204109 = CARTESIAN_POINT ( 'NONE',  ( 20.95262331984758575, 39.26456045904023284, -236.8738201967949806 ) ) ;
#204110 = CARTESIAN_POINT ( 'NONE',  ( 18.49999999999999645, 4.324939842317335525, -212.0862480289983409 ) ) ;
#204111 = DIRECTION ( 'NONE',  ( 1.000000000000000000, 0.000000000000000000, 0.000000000000000000 ) ) ;
#204112 = FACE_OUTER_BOUND ( 'NONE', #221446, .T. ) ;
#204113 = ORIENTED_EDGE ( 'NONE', *, *, #82498, .T. ) ;
#204114 = EDGE_LOOP ( 'NONE', ( #78369, #47534, #142278, #8006 ) ) ;
#204115 = EDGE_CURVE ( 'NONE', #228568, #209999, #175085, .T. ) ;
#204116 = DIRECTION ( 'NONE',  ( 1.000000000000000000, 0.000000000000000000, 0.000000000000000000 ) ) ;
#204117 = ORIENTED_EDGE ( 'NONE', *, *, #225726, .T. ) ;
#204118 = CARTESIAN_POINT ( 'NONE',  ( -20.94999999999999929, 64.36312671090811932, -143.3448666978491133 ) ) ;
#204119 = ORIENTED_EDGE ( 'NONE', *, *, #183003, .F. ) ;
#204120 = SURFACE_SIDE_STYLE ('',( #102429 ) ) ;
#204121 = DIRECTION ( 'NONE',  ( 1.000000000000000000, 0.000000000000000000, 0.000000000000000000 ) ) ;
#204122 = VECTOR ( 'NONE', #255923, 1000.000000000000000 ) ;
#204123 = ORIENTED_EDGE ( 'NONE', *, *, #154390, .T. ) ;
#204124 = DIRECTION ( 'NONE',  ( -0.000000000000000000, 0.8700118002898356018, -0.4930308989875170078 ) ) ;
#204125 = ORIENTED_EDGE ( 'NONE', *, *, #116697, .T. ) ;
#204126 = ORIENTED_EDGE ( 'NONE', *, *, #214597, .F. ) ;
#204127 = LINE ( 'NONE', #184573, #208733 ) ;
#204128 = CARTESIAN_POINT ( 'NONE',  ( -21.08884785362073089, 75.95021690494527888, -109.3803008519499258 ) ) ;
#204130 = EDGE_LOOP ( 'NONE', ( #143243, #8791, #62478, #81816 ) ) ;
#204129 = CARTESIAN_POINT ( 'NONE',  ( 23.40000000000005542, 62.43959356634987046, -37.55748533175129467 ) ) ;
#204131 = EDGE_CURVE ( 'NONE', #198561, #214263, #134598, .T. ) ;
#204132 = VECTOR ( 'NONE', #124993, 1000.000000000000000 ) ;
#204133 = DIRECTION ( 'NONE',  ( 0.000000000000000000, 0.000000000000000000, 1.000000000000000000 ) ) ;
#204135 = ORIENTED_EDGE ( 'NONE', *, *, #57269, .F. ) ;
#204134 = CARTESIAN_POINT ( 'NONE',  ( 18.49999999999999289, 18.51199663233067838, -231.2535697180530292 ) ) ;
#204136 = DIRECTION ( 'NONE',  ( 1.000000000000000000, 0.000000000000000000, 0.000000000000000000 ) ) ;
#204137 = CARTESIAN_POINT ( 'NONE',  ( 23.14999999999999858, -13.98128454229088291, -192.0195388455185821 ) ) ;
#204139 = VERTEX_POINT ( 'NONE', #156783 ) ;
#204138 = DIRECTION ( 'NONE',  ( 2.659396599871503635E-15, -0.6132151058540604716, 0.7899159663865477077 ) ) ;
#204140 = CARTESIAN_POINT ( 'NONE',  ( 23.24999999999999289, 11.75000000001116263, -45.65000000000000568 ) ) ;
#204141 = DIRECTION ( 'NONE',  ( -0.000000000000000000, -0.000000000000000000, -1.000000000000000000 ) ) ;
#204143 = EDGE_CURVE ( 'NONE', #182615, #144364, #199496, .T. ) ;
#204142 = CARTESIAN_POINT ( 'NONE',  ( -16.89020380669786903, 12.43689062641632326, -211.3478399073821947 ) ) ;
#204144 = ORIENTED_EDGE ( 'NONE', *, *, #52025, .F. ) ;
#204145 = CARTESIAN_POINT ( 'NONE',  ( 20.22483756094572271, 9.501904678882469923, -108.6395391287147305 ) ) ;
#204146 = CARTESIAN_POINT ( 'NONE',  ( 18.57071067811864040, 65.82071067813065213, -115.2731074845243597 ) ) ;
#204147 = DIRECTION ( 'NONE',  ( 1.000000000000000000, 0.000000000000000000, 0.000000000000000000 ) ) ;
#204148 = CARTESIAN_POINT ( 'NONE',  ( 20.73486653747088582, 68.75000000001156764, -60.27310748452437394 ) ) ;
#204149 = CARTESIAN_POINT ( 'NONE',  ( 21.05000000000000071, 1.115600667400684642E-11, -134.0000000000000284 ) ) ;
#204150 = CIRCLE ( 'NONE', #233426, 4.049999999999998046 ) ;
#204151 = ORIENTED_EDGE ( 'NONE', *, *, #16108, .T. ) ;
#204152 = EDGE_LOOP ( 'NONE', ( #49852, #234640, #256634, #220044 ) ) ;
#204153 = ORIENTED_EDGE ( 'NONE', *, *, #173561, .F. ) ;
#204154 = CARTESIAN_POINT ( 'NONE',  ( -23.25000000000000000, 1.115600667400684642E-11, -67.00000000000000000 ) ) ;
#204155 = VERTEX_POINT ( 'NONE', #216722 ) ;
#204157 = LINE ( 'NONE', #127209, #168430 ) ;
#204156 = VECTOR ( 'NONE', #25280, 1000.000000000000000 ) ;
#204158 = EDGE_LOOP ( 'NONE', ( #94951, #230780, #216883, #212420 ) ) ;
#204159 = CARTESIAN_POINT ( 'NONE',  ( 18.55857864376267941, 10.36715728753653565, -91.75000000000005684 ) ) ;
#204160 = CARTESIAN_POINT ( 'NONE',  ( 18.60000000000000142, -9.321008403350125704, -40.73593824907789696 ) ) ;
#204161 = AXIS2_PLACEMENT_3D ( 'NONE', #73413, #87784, #130780 ) ;
#204162 = CIRCLE ( 'NONE', #216651, 0.3999999999999926392 ) ;
#204163 = EDGE_CURVE ( 'NONE', #123901, #197693, #253275, .T. ) ;
#204164 = ORIENTED_EDGE ( 'NONE', *, *, #42890, .T. ) ;
#204165 = CARTESIAN_POINT ( 'NONE',  ( 13.54577453029516931, 9.450602096099684601, -152.4438959630967645 ) ) ;
#204167 = VERTEX_POINT ( 'NONE', #173811 ) ;
#204166 = AXIS2_PLACEMENT_3D ( 'NONE', #172522, #251999, #253273 ) ;
#204168 = ORIENTED_EDGE ( 'NONE', *, *, #9175, .F. ) ;
#204169 = AXIS2_PLACEMENT_3D ( 'NONE', #94237, #250743, #111244 ) ;
#204170 = AXIS2_PLACEMENT_3D ( 'NONE', #112187, #109584, #70508 ) ;
#204171 = EDGE_LOOP ( 'NONE', ( #188634, #43088, #53507, #108114 ) ) ;
#204172 = AXIS2_PLACEMENT_3D ( 'NONE', #44781, #23953, #102146 ) ;
#204173 = CIRCLE ( 'NONE', #254244, 0.09999999999998898659 ) ;
#204174 = EDGE_CURVE ( 'NONE', #14224, #109498, #211952, .T. ) ;
#204175 = CARTESIAN_POINT ( 'NONE',  ( -20.85000000000000142, -1.164121893230052995, -108.4148480855716485 ) ) ;
#204176 = CARTESIAN_POINT ( 'NONE',  ( -21.29999999999995808, 1.115650265596050101E-11, -129.9500000000000171 ) ) ;
#204177 = CARTESIAN_POINT ( 'NONE',  ( 20.94999999999999929, 1.115600667400684642E-11, -67.00000000000000000 ) ) ;
#204178 = ADVANCED_FACE ( 'NONE', ( #214165 ), #103180, .T. ) ;
#204179 = CARTESIAN_POINT ( 'NONE',  ( 14.88075390448864255, 27.69551741609592455, -234.0500622709107859 ) ) ;
#204180 = CARTESIAN_POINT ( 'NONE',  ( 23.25000000000000355, -22.45632476061176774, -140.7938984477316353 ) ) ;
#204181 = CYLINDRICAL_SURFACE ( 'NONE', #213538, 0.1000000000000057648 ) ;
#204183 = CARTESIAN_POINT ( 'NONE',  ( 21.05000000000000071, 76.00000000001156764, -56.64810748452432421 ) ) ;
#204182 = CARTESIAN_POINT ( 'NONE',  ( 20.93284271247462414, 11.75000000001116085, -193.9851942293460354 ) ) ;
#204184 = CARTESIAN_POINT ( 'NONE',  ( 21.14999999999999503, 11.65000000001116298, -33.50000000000000000 ) ) ;
#204186 = ORIENTED_EDGE ( 'NONE', *, *, #52927, .F. ) ;
#204185 = CARTESIAN_POINT ( 'NONE',  ( -18.40000000000000213, 64.66825945288714195, -157.3731074845244393 ) ) ;
#204188 = DIRECTION ( 'NONE',  ( 0.000000000000000000, -7.034366652768107165E-15, 1.000000000000000000 ) ) ;
#204187 = CARTESIAN_POINT ( 'NONE',  ( -20.94999999999999929, 11.60000000001115339, -40.42820323027555673 ) ) ;
#204189 = EDGE_CURVE ( 'NONE', #54475, #416, #16324, .T. ) ;
#204190 = CARTESIAN_POINT ( 'NONE',  ( -21.05000000000000071, 1.115600667400684642E-11, -134.0000000000000284 ) ) ;
#204191 = EDGE_CURVE ( 'NONE', #236913, #229203, #137110, .T. ) ;
#204192 = ORIENTED_EDGE ( 'NONE', *, *, #9600, .F. ) ;
#204193 = CARTESIAN_POINT ( 'NONE',  ( 20.95325940946048249, 10.52339007070744437, -74.56446212924012684 ) ) ;
#204194 = CARTESIAN_POINT ( 'NONE',  ( 21.98333005346336222, 76.00000000001273293, -210.8971828135810256 ) ) ;
#204195 = CARTESIAN_POINT ( 'NONE',  ( 21.14999999999999503, 76.00000000001237765, -170.0231074845243597 ) ) ;
#204196 = B_SPLINE_CURVE_WITH_KNOTS ( 'NONE', 3,
 ( #11348, #208276, #33523, #8780, #12652, #10058, #68759, #192559 ),
 .UNSPECIFIED., .F., .F.,
 ( 4, 2, 2, 4 ),
 ( 0.000000000000000000, 0.0001881495939909263277, 0.0002822243909863877704, 0.0003762991879818492402 ),
 .UNSPECIFIED. ) ;
#204197 = ORIENTED_EDGE ( 'NONE', *, *, #62413, .T. ) ;
#204198 = VECTOR ( 'NONE', #172086, 1000.000000000000000 ) ;
#204199 = ADVANCED_FACE ( 'NONE', ( #82320 ), #124064, .F. ) ;
#204200 = CARTESIAN_POINT ( 'NONE',  ( -16.89268316805465986, 30.21221237062500720, -234.8082435139909592 ) ) ;
#204201 = EDGE_CURVE ( 'NONE', #120786, #60871, #220332, .T. ) ;
#204202 = CARTESIAN_POINT ( 'NONE',  ( -18.50000000000000000, 52.81534179157634412, -244.1198638051726277 ) ) ;
#204203 = DIRECTION ( 'NONE',  ( -0.000000000000000000, 6.982962677686266711E-15, -1.000000000000000000 ) ) ;
#204205 = EDGE_CURVE ( 'NONE', #117549, #127088, #237065, .T. ) ;
#204204 = EDGE_CURVE ( 'NONE', #82492, #44319, #153736, .T. ) ;
#204206 = ORIENTED_EDGE ( 'NONE', *, *, #113583, .F. ) ;
#204207 = EDGE_LOOP ( 'NONE', ( #115734, #227409, #92815 ) ) ;
#204208 = ORIENTED_EDGE ( 'NONE', *, *, #74318, .F. ) ;
#204209 = CARTESIAN_POINT ( 'NONE',  ( -20.85000000000000142, -1.736705739467587772, -45.01742258762372728 ) ) ;
#204210 = CARTESIAN_POINT ( 'NONE',  ( -23.25000000000000000, 80.78317333349157536, -192.9003134612049166 ) ) ;
#204211 = CARTESIAN_POINT ( 'NONE',  ( -21.05000000000000071, 13.59055429284667404, -238.6121134008722038 ) ) ;
#204212 = CYLINDRICAL_SURFACE ( 'NONE', #138393, 0.09999999999999789613 ) ;
#204213 = ORIENTED_EDGE ( 'NONE', *, *, #47424, .T. ) ;
#204214 = AXIS2_PLACEMENT_3D ( 'NONE', #228451, #68075, #227142 ) ;
#204215 = DIRECTION ( 'NONE',  ( -1.000000000000000000, 0.000000000000000000, 0.000000000000000000 ) ) ;
#204216 = EDGE_CURVE ( 'NONE', #241914, #103462, #91338, .T. ) ;
#204217 = FACE_OUTER_BOUND ( 'NONE', #40191, .T. ) ;
#204218 = CIRCLE ( 'NONE', #121051, 0.5000000000000004441 ) ;
#204219 = CARTESIAN_POINT ( 'NONE',  ( 18.49999999999999289, 10.34378108836433263, -192.3284452778769662 ) ) ;
#204220 = DIRECTION ( 'NONE',  ( -1.000000000000000000, -0.000000000000000000, 0.000000000000000000 ) ) ;
#204221 = EDGE_CURVE ( 'NONE', #159190, #33900, #122788, .T. ) ;
#204222 = EDGE_CURVE ( 'NONE', #47209, #185202, #107876, .T. ) ;
#204223 = AXIS2_PLACEMENT_3D ( 'NONE', #143273, #123724, #87142 ) ;
#204224 = ORIENTED_EDGE ( 'NONE', *, *, #103701, .F. ) ;
#204225 = EDGE_CURVE ( 'NONE', #181843, #87673, #2797, .T. ) ;
#204227 = VERTEX_POINT ( 'NONE', #165767 ) ;
#204226 = CARTESIAN_POINT ( 'NONE',  ( -18.59999999999999787, 14.80545736607782814, -235.9842437978701639 ) ) ;
#204228 = DIRECTION ( 'NONE',  ( 0.000000000000000000, 0.000000000000000000, -1.000000000000000000 ) ) ;
#204229 = PLANE ( 'NONE',  #136164 ) ;
#204230 = FACE_OUTER_BOUND ( 'NONE', #111628, .T. ) ;
#204231 = CARTESIAN_POINT ( 'NONE',  ( 18.49999999999999645, 76.00000000001237765, -170.0231074845243597 ) ) ;
#204232 = EDGE_CURVE ( 'NONE', #11304, #24198, #41283, .T. ) ;
#204233 = DIRECTION ( 'NONE',  ( 2.952720810173289112E-16, -1.000000000000000000, 0.000000000000000000 ) ) ;
#204234 = CYLINDRICAL_SURFACE ( 'NONE', #28110, 0.09999999999999939493 ) ;
#204235 = ORIENTED_EDGE ( 'NONE', *, *, #171261, .T. ) ;
#204236 = DIRECTION ( 'NONE',  ( -0.000000000000000000, 0.2128009952263604232, -0.9770955615653316162 ) ) ;
#204237 = CARTESIAN_POINT ( 'NONE',  ( -20.94999999999999929, 7.872214528623318053, -209.6555322433423498 ) ) ;
#204238 = CARTESIAN_POINT ( 'NONE',  ( 22.39999999999999858, 7.790779598384538041, -134.0000000000000000 ) ) ;
#204240 = CIRCLE ( 'NONE', #200156, 12.87500000000000178 ) ;
#204239 = DIRECTION ( 'NONE',  ( 0.000000000000000000, 0.000000000000000000, 1.000000000000000000 ) ) ;
#204241 = PLANE ( 'NONE',  #182356 ) ;
#204242 = AXIS2_PLACEMENT_3D ( 'NONE', #245278, #167049, #224407 ) ;
#204243 = ORIENTED_EDGE ( 'NONE', *, *, #12990, .F. ) ;
#204244 = ORIENTED_EDGE ( 'NONE', *, *, #66794, .F. ) ;
#204245 = CIRCLE ( 'NONE', #196071, 0.09999999999998898659 ) ;
#204246 = DIRECTION ( 'NONE',  ( 0.000000000000000000, -1.000000000000000000, 0.000000000000000000 ) ) ;
#204247 = LINE ( 'NONE', #25626, #247321 ) ;
#204248 = CARTESIAN_POINT ( 'NONE',  ( 20.87155475150661132, 17.14044013043753267, -224.4860178609578156 ) ) ;
#204249 = CARTESIAN_POINT ( 'NONE',  ( 18.39999999999999858, 85.68240343348826116, -96.36626410711143365 ) ) ;
#204250 = DIRECTION ( 'NONE',  ( 0.000000000000000000, 0.000000000000000000, 1.000000000000000000 ) ) ;
#204251 = DIRECTION ( 'NONE',  ( 0.000000000000000000, 0.000000000000000000, 1.000000000000000000 ) ) ;
#204252 = CIRCLE ( 'NONE', #45867, 0.09999999999999961697 ) ;
#204253 = VECTOR ( 'NONE', #78309, 1000.000000000000000 ) ;
#204254 = CARTESIAN_POINT ( 'NONE',  ( -19.99999999999999645, 4.547418889303922462, 21.90000000000000213 ) ) ;
#204255 = ORIENTED_EDGE ( 'NONE', *, *, #114921, .T. ) ;
#204256 = DIRECTION ( 'NONE',  ( 0.000000000000000000, 1.000000000000000000, 0.000000000000000000 ) ) ;
#204257 = ORIENTED_EDGE ( 'NONE', *, *, #2109, .F. ) ;
#204258 = CARTESIAN_POINT ( 'NONE',  ( -21.13422380239054021, 76.00000000001170974, -76.01643399932983414 ) ) ;
#204259 = DIRECTION ( 'NONE',  ( 0.000000000000000000, 6.982962677686267499E-15, -1.000000000000000000 ) ) ;
#204260 = FACE_OUTER_BOUND ( 'NONE', #48145, .T. ) ;
#204261 = LINE ( 'NONE', #90420, #161608 ) ;
#204262 = CARTESIAN_POINT ( 'NONE',  ( -23.25000000000000000, 11.75000000000000000, 11.75000000000000000 ) ) ;
#204263 = CARTESIAN_POINT ( 'NONE',  ( -18.59999996769639097, -9.363273769830332327, -7.181493915465814837 ) ) ;
#204264 = CARTESIAN_POINT ( 'NONE',  ( -16.95709691156445587, 66.05000000001182059, -82.18316504703474834 ) ) ;
#204265 = CARTESIAN_POINT ( 'NONE',  ( -21.46681500593267700, 6.857511159395791367, -67.00000000000004263 ) ) ;
#204266 = CIRCLE ( 'NONE', #41817, 7.900000000000009237 ) ;
#204267 = EDGE_CURVE ( 'NONE', #6405, #49802, #78818, .T. ) ;
#204268 = DIRECTION ( 'NONE',  ( 0.000000000000000000, -0.9947597004326491632, 0.1022405907413782566 ) ) ;
#204269 = TOROIDAL_SURFACE ( 'NONE', #20977, 0.2000000000000000111, 0.1000000000000000056 ) ;
#204270 = CARTESIAN_POINT ( 'NONE',  ( 18.49999999999998934, 15.28205413790855971, -223.0019049476732675 ) ) ;
#204271 = FACE_OUTER_BOUND ( 'NONE', #246543, .T. ) ;
#204272 = AXIS2_PLACEMENT_3D ( 'NONE', #44822, #124369, #203885 ) ;
#204273 = EDGE_CURVE ( 'NONE', #242599, #33168, #195397, .T. ) ;
#204274 = CARTESIAN_POINT ( 'NONE',  ( 20.94999999999999929, 85.00000000001188027, -93.12913836187181005 ) ) ;
#204275 = CARTESIAN_POINT ( 'NONE',  ( 20.94999999999999929, 64.35000000001249987, -176.8069731475025321 ) ) ;
#204276 = VECTOR ( 'NONE', #163853, 1000.000000000000114 ) ;
#204277 = ORIENTED_EDGE ( 'NONE', *, *, #118530, .T. ) ;
#204278 = CARTESIAN_POINT ( 'NONE',  ( 23.50000000000004263, 77.16254490893143725, -43.92310748452479885 ) ) ;
#204280 = EDGE_CURVE ( 'NONE', #221081, #95915, #245276, .T. ) ;
#204279 = FACE_OUTER_BOUND ( 'NONE', #16818, .T. ) ;
#204281 = ADVANCED_FACE ( 'NONE', ( #219288 ), #45793, .T. ) ;
#204282 = EDGE_LOOP ( 'NONE', ( #59042, #254679, #35114, #207103 ) ) ;
#204283 = DIRECTION ( 'NONE',  ( -3.265361837132813093E-16, 1.000000000000000000, -0.000000000000000000 ) ) ;
#204284 = SPHERICAL_SURFACE ( 'NONE', #77409, 0.1000000000000000056 ) ;
#204285 = AXIS2_PLACEMENT_3D ( 'NONE', #49660, #129208, #116071 ) ;
#204286 = DIRECTION ( 'NONE',  ( 0.000000000000000000, -1.000000000000000000, 0.000000000000000000 ) ) ;
#204287 = ORIENTED_EDGE ( 'NONE', *, *, #120550, .T. ) ;
#204288 = CARTESIAN_POINT ( 'NONE',  ( -18.59999999999999787, 67.23127455305835554, -235.8551265064784559 ) ) ;
#204289 = DIRECTION ( 'NONE',  ( 0.000000000000000000, -0.03181660087583042251, 0.9994937237965568766 ) ) ;
#204290 = ORIENTED_EDGE ( 'NONE', *, *, #237508, .F. ) ;
#204291 = EDGE_CURVE ( 'NONE', #89464, #179303, #257856, .T. ) ;
#204292 = ADVANCED_FACE ( 'NONE', ( #240153 ), #224423, .F. ) ;
#204293 = CARTESIAN_POINT ( 'NONE',  ( -18.40000000000000213, 11.47316190337364183, -158.1740539331920559 ) ) ;
#204294 = ORIENTED_EDGE ( 'NONE', *, *, #213030, .T. ) ;
#204295 = LINE ( 'NONE', #103902, #87564 ) ;
#204296 = AXIS2_PLACEMENT_3D ( 'NONE', #254864, #76278, #155852 ) ;
#204297 = DIRECTION ( 'NONE',  ( 0.000000000000000000, 0.000000000000000000, 1.000000000000000000 ) ) ;
#204298 = DIRECTION ( 'NONE',  ( 0.000000000000000000, -6.982962677686266711E-15, 1.000000000000000000 ) ) ;
#204300 = DIRECTION ( 'NONE',  ( -0.000000000000000000, -0.8814952561688430555, 0.4721928772777346239 ) ) ;
#204299 = PRODUCT_DEFINITION_CONTEXT ( 'detailed design', #24210, 'design' ) ;
#204301 = CARTESIAN_POINT ( 'NONE',  ( -21.07094088545304444, 69.67983277809619835, -203.6220011870766200 ) ) ;
#204302 = CARTESIAN_POINT ( 'NONE',  ( -16.77180007708461673, 66.05000000001230376, -157.3874933655695827 ) ) ;
#204303 = DIRECTION ( 'NONE',  ( 9.044546369203337730E-15, -0.5795995782408065455, -0.8149014228132623883 ) ) ;
#204304 = VECTOR ( 'NONE', #15037, 1000.000000000000114 ) ;
#204305 = DIRECTION ( 'NONE',  ( -0.000000000000000000, -0.3896596508880123544, -0.9209589331071349472 ) ) ;
#204306 = CARTESIAN_POINT ( 'NONE',  ( -0.8999999999999993561, -8.250000000000005329, 30.04142135623731136 ) ) ;
#204309 = ORIENTED_EDGE ( 'NONE', *, *, #178987, .T. ) ;
#204308 = EDGE_CURVE ( 'NONE', #52704, #184931, #181473, .T. ) ;
#204307 = DIRECTION ( 'NONE',  ( 1.000000000000000000, 0.000000000000000000, 0.000000000000000000 ) ) ;
#204310 = ORIENTED_EDGE ( 'NONE', *, *, #194607, .T. ) ;
#204312 = DIRECTION ( 'NONE',  ( 1.000000000000000000, 0.000000000000000000, 0.000000000000000000 ) ) ;
#204311 = DIRECTION ( 'NONE',  ( 0.000000000000000000, 0.000000000000000000, -1.000000000000000000 ) ) ;
#204314 = EDGE_LOOP ( 'NONE', ( #108642, #183507, #181152, #133836 ) ) ;
#204313 = DIRECTION ( 'NONE',  ( 1.000000000000000000, 0.000000000000000000, 0.000000000000000000 ) ) ;
#204315 = AXIS2_PLACEMENT_3D ( 'NONE', #181885, #202719, #65783 ) ;
#204316 = ORIENTED_EDGE ( 'NONE', *, *, #89826, .T. ) ;
#204317 = EDGE_CURVE ( 'NONE', #84480, #131827, #28840, .T. ) ;
#204318 = DIRECTION ( 'NONE',  ( 0.000000000000000000, 0.000000000000000000, -1.000000000000000000 ) ) ;
#204319 = DIRECTION ( 'NONE',  ( 0.000000000000000000, -0.9915357197604982575, 0.1298341882519033486 ) ) ;
#204320 = DIRECTION ( 'NONE',  ( 0.000000000000000000, 0.9910827722268048534, -0.1332476588733589040 ) ) ;
#204321 = AXIS2_PLACEMENT_3D ( 'NONE', #162212, #164758, #68227 ) ;
#204322 = CARTESIAN_POINT ( 'NONE',  ( -20.90851465518106167, 10.32532329027886320, -173.0699343018359855 ) ) ;
#204323 = CARTESIAN_POINT ( 'NONE',  ( 21.07928932188134397, 69.67148334361883144, -136.6220026301787414 ) ) ;
#204325 = EDGE_CURVE ( 'NONE', #253599, #19453, #174584, .T. ) ;
#204324 = LINE ( 'NONE', #25706, #11349 ) ;
#204326 = EDGE_CURVE ( 'NONE', #111418, #44904, #203923, .T. ) ;
#204327 = LINE ( 'NONE', #62265, #206126 ) ;
#204328 = EDGE_LOOP ( 'NONE', ( #98303, #25847, #77703, #90475 ) ) ;
#204329 = ORIENTED_EDGE ( 'NONE', *, *, #190365, .F. ) ;
#204330 = CARTESIAN_POINT ( 'NONE',  ( 20.09999999999999787, 13.96358247574307043, -219.2976327551816951 ) ) ;
#204331 = AXIS2_PLACEMENT_3D ( 'NONE', #105143, #41395, #6080 ) ;
#204332 = ORIENTED_EDGE ( 'NONE', *, *, #213593, .F. ) ;
#204333 = DIRECTION ( 'NONE',  ( 1.836970198721029934E-16, 1.000000000000000000, 6.982962677686266711E-15 ) ) ;
#204335 = ORIENTED_EDGE ( 'NONE', *, *, #150204, .T. ) ;
#204334 = CIRCLE ( 'NONE', #54507, 0.09999999999999939493 ) ;
#204336 = FACE_OUTER_BOUND ( 'NONE', #107502, .T. ) ;
#204337 = EDGE_CURVE ( 'NONE', #63872, #110634, #127909, .T. ) ;
#204338 = AXIS2_PLACEMENT_3D ( 'NONE', #125447, #249248, #204953 ) ;
#204339 = CARTESIAN_POINT ( 'NONE',  ( 21.14999999999999858, 69.45000000001186891, -90.87310748452435405 ) ) ;
#204340 = DIRECTION ( 'NONE',  ( 0.000000000000000000, 1.000000000000000000, -0.000000000000000000 ) ) ;
#204341 = CARTESIAN_POINT ( 'NONE',  ( -21.10320863425827298, 75.97497774878561927, -209.9233848709835684 ) ) ;
#204342 = ORIENTED_EDGE ( 'NONE', *, *, #239268, .F. ) ;
#204343 = CIRCLE ( 'NONE', #12661, 0.1999999999999987899 ) ;
#204344 = ADVANCED_FACE ( 'NONE', ( #190471 ), #132357, .T. ) ;
#204346 = VECTOR ( 'NONE', #89490, 1000.000000000000227 ) ;
#204345 = CARTESIAN_POINT ( 'NONE',  ( -21.03922262424671885, 11.62390063400470375, -6.859208042893458313 ) ) ;
#204347 = ORIENTED_EDGE ( 'NONE', *, *, #238534, .F. ) ;
#204348 = DIRECTION ( 'NONE',  ( 3.616040088954490704E-32, 7.105427357601001859E-15, -1.000000000000000000 ) ) ;
#204349 = CARTESIAN_POINT ( 'NONE',  ( 21.05000000000000071, 67.17357026049512569, -161.6090527715807070 ) ) ;
#204350 = CARTESIAN_POINT ( 'NONE',  ( 23.14999999999999858, 1.115600667400684642E-11, -169.5000000000000284 ) ) ;
#204351 = EDGE_CURVE ( 'NONE', #112987, #146298, #60164, .T. ) ;
#204352 = DIRECTION ( 'NONE',  ( 0.000000000000000000, -1.000000000000000000, 6.308085367188393199E-16 ) ) ;
#204353 = VERTEX_POINT ( 'NONE', #49645 ) ;
#204354 = CARTESIAN_POINT ( 'NONE',  ( -20.95613430942401223, 64.25000000001188027, -96.16594483630493073 ) ) ;
#204355 = VERTEX_POINT ( 'NONE', #7967 ) ;
#204358 = EDGE_LOOP ( 'NONE', ( #256952, #58817, #238316, #192611 ) ) ;
#204357 = CARTESIAN_POINT ( 'NONE',  ( 21.05000000000000426, 6.413826288824128419, -67.08574093703344943 ) ) ;
#204356 = LINE ( 'NONE', #167841, #157526 ) ;
#204359 = DIRECTION ( 'NONE',  ( 0.000000000000000000, -1.000000000000000000, 0.000000000000000000 ) ) ;
#204360 = TOROIDAL_SURFACE ( 'NONE', #179446, 11.70000000000000107, 0.1000000000000000056 ) ;
#204362 = VERTEX_POINT ( 'NONE', #146169 ) ;
#204361 = AXIS2_PLACEMENT_3D ( 'NONE', #239512, #162554, #101222 ) ;
#204363 = AXIS2_PLACEMENT_3D ( 'NONE', #89688, #28493, #8889 ) ;
#204364 = AXIS2_PLACEMENT_3D ( 'NONE', #181138, #24648, #205816 ) ;
#204365 = CARTESIAN_POINT ( 'NONE',  ( -21.07928932188134041, 65.47931918658504458, -241.9371126717015841 ) ) ;
#204366 = VERTEX_POINT ( 'NONE', #208741 ) ;
#204367 = CARTESIAN_POINT ( 'NONE',  ( -23.15000000000000213, -11.48912529306489816, -97.40000000000004832 ) ) ;
#204368 = EDGE_CURVE ( 'NONE', #75640, #22692, #183094, .T. ) ;
#204369 = DIRECTION ( 'NONE',  ( 1.000000000000000000, 0.000000000000000000, 0.000000000000000000 ) ) ;
#204370 = CARTESIAN_POINT ( 'NONE',  ( 21.14999999999999858, 6.650000000011155876, -45.65000000000000568 ) ) ;
#204371 = DIRECTION ( 'NONE',  ( 0.000000000000000000, -0.1569827930593259702, 0.9876013379310970564 ) ) ;
#204372 = CARTESIAN_POINT ( 'NONE',  ( -20.64999999999999858, 21.39147882631411335, -233.2615922652120730 ) ) ;
#204373 = AXIS2_PLACEMENT_3D ( 'NONE', #205715, #104033, #164041 ) ;
#204374 = ORIENTED_EDGE ( 'NONE', *, *, #59120, .F. ) ;
#204375 = CARTESIAN_POINT ( 'NONE',  ( -23.15000000000000213, 76.00000000001189449, -100.9231074845242944 ) ) ;
#204376 = CARTESIAN_POINT ( 'NONE',  ( -16.77683809663752257, 14.15196434607590348, -219.2423291894720307 ) ) ;
#204377 = CARTESIAN_POINT ( 'NONE',  ( 23.50000000000005684, 77.83551161375993388, -47.52760213295649550 ) ) ;
#204378 = EDGE_LOOP ( 'NONE', ( #195175, #158876, #52976, #100616, #223262 ) ) ;
#204379 = DIRECTION ( 'NONE',  ( 0.000000000000000000, -0.000000000000000000, 1.000000000000000000 ) ) ;
#204380 = ORIENTED_EDGE ( 'NONE', *, *, #207763, .T. ) ;
#204381 = LINE ( 'NONE', #188678, #206272 ) ;
#204382 = DIRECTION ( 'NONE',  ( -1.000000000000000000, 0.000000000000000000, 0.000000000000000000 ) ) ;
#204383 = CARTESIAN_POINT ( 'NONE',  ( 20.87155475150661132, 36.12098300858676936, -235.9333785785471775 ) ) ;
#204385 = VERTEX_POINT ( 'NONE', #110905 ) ;
#204384 = CARTESIAN_POINT ( 'NONE',  ( -16.94389599338512298, 9.991197989766199328, -146.6076448018102667 ) ) ;
#204386 = DIRECTION ( 'NONE',  ( 1.000000000000000000, -0.000000000000000000, -0.000000000000000000 ) ) ;
#204387 = DIRECTION ( 'NONE',  ( -1.000000000000000000, 0.000000000000000000, 0.000000000000000000 ) ) ;
#204388 = CARTESIAN_POINT ( 'NONE',  ( -21.05000000000000071, 1.835341550235569663, -145.5551512925629822 ) ) ;
#204389 = ORIENTED_EDGE ( 'NONE', *, *, #226237, .T. ) ;
#204390 = CARTESIAN_POINT ( 'NONE',  ( 22.47007471830798409, 68.27928934808623751, -203.5231074845244450 ) ) ;
#204391 = CARTESIAN_POINT ( 'NONE',  ( 20.85000000000000142, 76.00000000001244871, -170.0231074845243597 ) ) ;
#204392 = ORIENTED_EDGE ( 'NONE', *, *, #157563, .T. ) ;
#204393 = CARTESIAN_POINT ( 'NONE',  ( -22.00356870066586623, 65.33245486361551002, -242.8564489551603458 ) ) ;
#204394 = VECTOR ( 'NONE', #177824, 1000.000000000000000 ) ;
#204395 = EDGE_CURVE ( 'NONE', #109854, #98224, #120563, .T. ) ;
#204396 = ORIENTED_EDGE ( 'NONE', *, *, #24279, .F. ) ;
#204398 = CARTESIAN_POINT ( 'NONE',  ( -23.15000000000000213, 76.00000000001126921, -203.5231074845248997 ) ) ;
#204397 = CIRCLE ( 'NONE', #221153, 1.900000000000002132 ) ;
#204400 = ORIENTED_EDGE ( 'NONE', *, *, #227696, .T. ) ;
#204399 = CARTESIAN_POINT ( 'NONE',  ( 20.04142135623730070, 16.62870782457739338, -222.6062739981998391 ) ) ;
#204401 = ADVANCED_FACE ( 'NONE', ( #28854 ), #91356, .F. ) ;
#204404 = ORIENTED_EDGE ( 'NONE', *, *, #194905, .F. ) ;
#204403 = ORIENTED_EDGE ( 'NONE', *, *, #197703, .T. ) ;
#204402 = CARTESIAN_POINT ( 'NONE',  ( -23.15000000000000213, -11.48912529306489994, -97.40000000000004832 ) ) ;
#204405 = AXIS2_PLACEMENT_3D ( 'NONE', #78407, #160552, #99247 ) ;
#204406 = EDGE_CURVE ( 'NONE', #163089, #8860, #249722, .T. ) ;
#204407 = DIRECTION ( 'NONE',  ( 0.000000000000000000, 3.552713678800413366E-15, -1.000000000000000000 ) ) ;
#204408 = ADVANCED_FACE ( 'NONE', ( #131750 ), #108348, .T. ) ;
#204409 = FACE_OUTER_BOUND ( 'NONE', #41781, .T. ) ;
#204410 = CYLINDRICAL_SURFACE ( 'NONE', #181612, 0.09999999999999939493 ) ;
#204412 = CARTESIAN_POINT ( 'NONE',  ( -12.42749937872396160, 66.62931007840893471, -51.99664235786332966 ) ) ;
#204411 = CARTESIAN_POINT ( 'NONE',  ( 20.94403535211772294, 46.37740828070795374, -243.0652246697500800 ) ) ;
#204413 = CARTESIAN_POINT ( 'NONE',  ( 21.14999999999999858, 10.71339244341104013, -79.25000000000004263 ) ) ;
#204414 = CIRCLE ( 'NONE', #91999, 0.09999999999999899247 ) ;
#204415 = CARTESIAN_POINT ( 'NONE',  ( -16.92132318717937522, 44.10372977203042666, -235.2955471704553929 ) ) ;
#204416 = VECTOR ( 'NONE', #27174, 1000.000000000000000 ) ;
#204417 = DIRECTION ( 'NONE',  ( 0.000000000000000000, 1.000000000000000000, 0.000000000000000000 ) ) ;
#204418 = CARTESIAN_POINT ( 'NONE',  ( -18.50000000000000000, 64.35000000001222986, -148.2731074845243882 ) ) ;
#204420 = ORIENTED_EDGE ( 'NONE', *, *, #132824, .T. ) ;
#204419 = AXIS2_PLACEMENT_3D ( 'NONE', #135421, #20640, #79289 ) ;
#204421 = ORIENTED_EDGE ( 'NONE', *, *, #111459, .T. ) ;
#204422 = CARTESIAN_POINT ( 'NONE',  ( -20.94999999999999929, 64.35000000001176090, -76.30697314750248950 ) ) ;
#204424 = ORIENTED_EDGE ( 'NONE', *, *, #106749, .T. ) ;
#204423 = SPHERICAL_SURFACE ( 'NONE', #62790, 0.1000000000000000056 ) ;
#204425 = ORIENTED_EDGE ( 'NONE', *, *, #134877, .T. ) ;
#204426 = EDGE_CURVE ( 'NONE', #170769, #72122, #208044, .T. ) ;
#204427 = DIRECTION ( 'NONE',  ( 2.952720810173289112E-16, 1.000000000000000000, -6.088138035986627436E-46 ) ) ;
#204428 = ORIENTED_EDGE ( 'NONE', *, *, #162483, .T. ) ;
#204429 = CARTESIAN_POINT ( 'NONE',  ( -21.04999999999999716, 69.69982018209529429, -136.5745903664069090 ) ) ;
#204430 = ORIENTED_EDGE ( 'NONE', *, *, #26412, .F. ) ;
#204431 = VECTOR ( 'NONE', #74207, 1000.000000000000000 ) ;
#204432 = CARTESIAN_POINT ( 'NONE',  ( -16.94445028196807002, 66.00793639031407167, -82.13043766294282477 ) ) ;
#204433 = DIRECTION ( 'NONE',  ( 0.000000000000000000, 0.000000000000000000, 1.000000000000000000 ) ) ;
#204435 = VERTEX_POINT ( 'NONE', #9231 ) ;
#204434 = ORIENTED_EDGE ( 'NONE', *, *, #72833, .F. ) ;
#204436 = EDGE_LOOP ( 'NONE', ( #91149, #132817, #184055, #234213 ) ) ;
#204437 = DIRECTION ( 'NONE',  ( 0.000000000000000000, 0.8814952561688431665, -0.4721928772777344574 ) ) ;
#204438 = ORIENTED_EDGE ( 'NONE', *, *, #187017, .T. ) ;
#204439 = ORIENTED_EDGE ( 'NONE', *, *, #76553, .F. ) ;
#204440 = LINE ( 'NONE', #105313, #59646 ) ;
#204441 = DIRECTION ( 'NONE',  ( 0.000000000000000000, 0.9999631594459055250, 0.008583690987131395445 ) ) ;
#204443 = EDGE_LOOP ( 'NONE', ( #125694, #203788, #238090, #99937 ) ) ;
#204442 = DIRECTION ( 'NONE',  ( -1.000000000000000000, 0.000000000000000000, 0.000000000000000000 ) ) ;
#204444 = EDGE_CURVE ( 'NONE', #7639, #23846, #177336, .T. ) ;
#204445 = ADVANCED_FACE ( 'NONE', ( #39097 ), #4011, .T. ) ;
#204446 = CARTESIAN_POINT ( 'NONE',  ( -18.50000000000000000, 85.40000000001187175, -96.10844914155457275 ) ) ;
#204447 = CARTESIAN_POINT ( 'NONE',  ( -23.25000000000000000, 82.09643798151613225, -215.4278993322501208 ) ) ;
#204449 = ORIENTED_EDGE ( 'NONE', *, *, #200637, .F. ) ;
#204448 = CARTESIAN_POINT ( 'NONE',  ( 18.59999999999999076, 16.76897757977919312, -222.7804130109902871 ) ) ;
#204450 = CARTESIAN_POINT ( 'NONE',  ( -17.27223548801929454, 10.34539739139951209, -178.8663938208082413 ) ) ;
#204451 = VERTEX_POINT ( 'NONE', #95196 ) ;
#204452 = DIRECTION ( 'NONE',  ( 1.000000000000000000, 0.000000000000000000, 0.000000000000000000 ) ) ;
#204453 = ORIENTED_EDGE ( 'NONE', *, *, #38192, .F. ) ;
#204455 = VECTOR ( 'NONE', #171644, 1000.000000000000000 ) ;
#204454 = CARTESIAN_POINT ( 'NONE',  ( 22.42357213249528769, 68.32706761365247417, -170.1221944485259314 ) ) ;
#204456 = CYLINDRICAL_SURFACE ( 'NONE', #153814, 11.79999999999999361 ) ;
#204457 = AXIS2_PLACEMENT_3D ( 'NONE', #116025, #174748, #131720 ) ;
#204458 = AXIS2_PLACEMENT_3D ( 'NONE', #199827, #177707, #255874 ) ;
#204459 = EDGE_CURVE ( 'NONE', #91651, #13016, #16505, .T. ) ;
#204460 = AXIS2_PLACEMENT_3D ( 'NONE', #126620, #53175, #245294 ) ;
#204461 = EDGE_LOOP ( 'NONE', ( #257577, #36966, #256253, #67074 ) ) ;
#204463 = CARTESIAN_POINT ( 'NONE',  ( -23.25000000000000000, -11.75000000000000000, -30.39999999999999858 ) ) ;
#204462 = CARTESIAN_POINT ( 'NONE',  ( 22.01447462590973458, 0.09903700007069084210, -26.23619979877009101 ) ) ;
#204464 = DIRECTION ( 'NONE',  ( 0.000000000000000000, 0.000000000000000000, -1.000000000000000000 ) ) ;
#204465 = DIRECTION ( 'NONE',  ( 6.938893903907224433E-15, 1.000000000000000000, 7.272083257015735086E-15 ) ) ;
#204466 = VERTEX_POINT ( 'NONE', #153938 ) ;
#204467 = ORIENTED_EDGE ( 'NONE', *, *, #168433, .F. ) ;
#204468 = DIRECTION ( 'NONE',  ( 0.000000000000000000, 0.9654727137038726648, -0.2605042016806632943 ) ) ;
#204469 = FACE_OUTER_BOUND ( 'NONE', #59947, .T. ) ;
#204470 = ORIENTED_EDGE ( 'NONE', *, *, #95299, .T. ) ;
#204471 = FACE_OUTER_BOUND ( 'NONE', #52400, .T. ) ;
#204472 = VERTEX_POINT ( 'NONE', #152636 ) ;
#204473 = CARTESIAN_POINT ( 'NONE',  ( 20.04142135623730070, 16.72641738073392403, -222.5849938986771974 ) ) ;
#204474 = CARTESIAN_POINT ( 'NONE',  ( -20.94999999999999929, 86.43238724539048690, -209.5644480942280836 ) ) ;
#204475 = CIRCLE ( 'NONE', #129483, 0.09999999999999939493 ) ;
#204476 = CARTESIAN_POINT ( 'NONE',  ( 18.49999999999999289, 54.98105481382776816, -230.1569079895687366 ) ) ;
#204477 = EDGE_CURVE ( 'NONE', #237011, #130783, #166368, .T. ) ;
#204478 = DIRECTION ( 'NONE',  ( 1.000000000000000000, 0.000000000000000000, -3.469446951953635015E-14 ) ) ;
#204479 = VERTEX_POINT ( 'NONE', #36541 ) ;
#204480 = CARTESIAN_POINT ( 'NONE',  ( 18.43466021071414218, -9.494190690445382330, -207.6170615601278371 ) ) ;
#204481 = ORIENTED_EDGE ( 'NONE', *, *, #13411, .F. ) ;
#204482 = VERTEX_POINT ( 'NONE', #37817 ) ;
#204483 = ORIENTED_EDGE ( 'NONE', *, *, #170920, .F. ) ;
#204484 = ADVANCED_FACE ( 'NONE', ( #173508 ), #174782, .F. ) ;
#204485 = CARTESIAN_POINT ( 'NONE',  ( 22.39999999999999503, 64.25000000001269029, -203.6231074845244393 ) ) ;
#204486 = DIRECTION ( 'NONE',  ( 1.000000000000000000, -0.000000000000000000, -0.000000000000000000 ) ) ;
#204487 = DIRECTION ( 'NONE',  ( -1.000000000000000000, 0.000000000000000000, 0.000000000000000000 ) ) ;
#204488 = FACE_OUTER_BOUND ( 'NONE', #9117, .T. ) ;
#204489 = CARTESIAN_POINT ( 'NONE',  ( 23.14999999999998437, 1.148907358139439339E-11, -201.0000000000015064 ) ) ;
#204490 = AXIS2_PLACEMENT_3D ( 'NONE', #166790, #42964, #5078 ) ;
#204492 = DIRECTION ( 'NONE',  ( 0.000000000000000000, -1.000000000000000000, 1.387778780781406043E-13 ) ) ;
#204491 = CARTESIAN_POINT ( 'NONE',  ( 22.47071067811865319, 68.27992525551361780, -69.62219993922698791 ) ) ;
#204494 = ORIENTED_EDGE ( 'NONE', *, *, #31110, .F. ) ;
#204493 = CARTESIAN_POINT ( 'NONE',  ( 18.43630871534895732, 77.26727690582558239, -241.9658728844706559 ) ) ;
#204495 = CARTESIAN_POINT ( 'NONE',  ( -21.14999999999999858, 6.540656951712399803, -167.4999999999999716 ) ) ;
#204496 = ORIENTED_EDGE ( 'NONE', *, *, #92980, .F. ) ;
#204497 = EDGE_CURVE ( 'NONE', #31772, #128154, #45707, .T. ) ;
#204498 = CARTESIAN_POINT ( 'NONE',  ( 20.95512820512820440, 8.876151316299273120, -79.20017285912881277 ) ) ;
#204499 = ADVANCED_FACE ( 'NONE', ( #35259 ), #194326, .T. ) ;
#204500 = ORIENTED_EDGE ( 'NONE', *, *, #133041, .T. ) ;
#204501 = ORIENTED_EDGE ( 'NONE', *, *, #28417, .F. ) ;
#204502 = DIRECTION ( 'NONE',  ( 1.000000000000000000, 0.000000000000000000, -0.000000000000000000 ) ) ;
#204503 = VECTOR ( 'NONE', #248196, 1000.000000000000000 ) ;
#204504 = LINE ( 'NONE', #224065, #168514 ) ;
#204505 = CARTESIAN_POINT ( 'NONE',  ( -16.93710578446422588, 66.05000000001153637, -48.94191146832373107 ) ) ;
#204506 = DIRECTION ( 'NONE',  ( 0.000000000000000000, -1.000000000000000000, -6.982962677686266711E-15 ) ) ;
#204507 = AXIS2_PLACEMENT_3D ( 'NONE', #230666, #72897, #14202 ) ;
#204508 = ADVANCED_FACE ( 'NONE', ( #156491 ), #215143, .T. ) ;
#204509 = CARTESIAN_POINT ( 'NONE',  ( 18.69999999999999929, -8.150000000000007461, 33.00000000000000000 ) ) ;
#204511 = EDGE_CURVE ( 'NONE', #208600, #67483, #70683, .T. ) ;
#204510 = AXIS2_PLACEMENT_3D ( 'NONE', #217019, #93229, #114073 ) ;
#204512 = ORIENTED_EDGE ( 'NONE', *, *, #168561, .T. ) ;
#204513 = EDGE_LOOP ( 'NONE', ( #43872, #256411, #104530, #109542, #108218, #110406, #131890 ) ) ;
#204514 = AXIS2_PLACEMENT_3D ( 'NONE', #95481, #18525, #180179 ) ;
#204515 = ORIENTED_EDGE ( 'NONE', *, *, #227215, .T. ) ;
#204516 = LINE ( 'NONE', #25904, #194546 ) ;
#204517 = CARTESIAN_POINT ( 'NONE',  ( 20.94999999999999929, 71.00000000001186606, -90.61784146561124942 ) ) ;
#204518 = FACE_OUTER_BOUND ( 'NONE', #167139, .T. ) ;
#204520 = EDGE_CURVE ( 'NONE', #148919, #95393, #216401, .T. ) ;
#204519 = CARTESIAN_POINT ( 'NONE',  ( 23.24999999999999645, 5.600000000011153389, -112.9052660189131245 ) ) ;
#204521 = DIRECTION ( 'NONE',  ( -0.000000000000000000, -0.2128009952263603677, 0.9770955615653313941 ) ) ;
#204522 = DIRECTION ( 'NONE',  ( 0.000000000000000000, 6.938893903907222067E-15, -1.000000000000000000 ) ) ;
#204523 = VERTEX_POINT ( 'NONE', #196847 ) ;
#204524 = CARTESIAN_POINT ( 'NONE',  ( -18.69999999999999929, -11.65000000000000036, 30.09999999999999787 ) ) ;
#204525 = LINE ( 'NONE', #184974, #237328 ) ;
#204526 = CARTESIAN_POINT ( 'NONE',  ( 18.49999999999999645, 74.83729825007388570, -94.92310748452432279 ) ) ;
#204527 = CYLINDRICAL_SURFACE ( 'NONE', #87651, 0.09999999999999810429 ) ;
#204528 = EDGE_CURVE ( 'NONE', #227433, #102301, #91505, .T. ) ;
#204529 = LINE ( 'NONE', #145836, #99844 ) ;
#204530 = AXIS2_PLACEMENT_3D ( 'NONE', #42353, #104849, #120625 ) ;
#204531 = DIRECTION ( 'NONE',  ( -0.7071067811865475727, 0.2890913453342130457, -0.6453109281988448354 ) ) ;
#204532 = EDGE_CURVE ( 'NONE', #9164, #159242, #149796, .T. ) ;
#204534 = ADVANCED_FACE ( 'NONE', ( #232154 ), #136885, .F. ) ;
#204533 = VECTOR ( 'NONE', #74501, 1000.000000000000000 ) ;
#204535 = ORIENTED_EDGE ( 'NONE', *, *, #79424, .T. ) ;
#204536 = COLOUR_RGB ( '', 0.72549020, 0.75294118, 0.79215686) ;
#204537 = ADVANCED_FACE ( 'NONE', ( #256778 ), #241358, .T. ) ;
#204538 = CARTESIAN_POINT ( 'NONE',  ( -23.25000000000000355, 61.34848953995435039, -212.6564661897791098 ) ) ;
#204539 = ORIENTED_EDGE ( 'NONE', *, *, #95071, .F. ) ;
#204540 = AXIS2_PLACEMENT_3D ( 'NONE', #205698, #85720, #23253 ) ;
#204541 = CIRCLE ( 'NONE', #62898, 0.09999999999999609201 ) ;
#204542 = DIRECTION ( 'NONE',  ( -1.000000000000000000, 1.652117596168391700E-15, 0.000000000000000000 ) ) ;
#204543 = EDGE_CURVE ( 'NONE', #253194, #179449, #199674, .T. ) ;
#204544 = CARTESIAN_POINT ( 'NONE',  ( -20.54999999999999716, 25.94586868676353575, -241.5435999122864530 ) ) ;
#204545 = CARTESIAN_POINT ( 'NONE',  ( 22.10000000000000142, -1.467286812112899463, 32.90000000000000568 ) ) ;
#204546 = EDGE_CURVE ( 'NONE', #15533, #158454, #170670, .T. ) ;
#204547 = ORIENTED_EDGE ( 'NONE', *, *, #129068, .F. ) ;
#204548 = DIRECTION ( 'NONE',  ( 0.000000000000000000, 0.000000000000000000, 1.000000000000000000 ) ) ;
#204549 = DIRECTION ( 'NONE',  ( -0.000000000000000000, 1.000000000000000000, 0.000000000000000000 ) ) ;
#204550 = EDGE_CURVE ( 'NONE', #219970, #241382, #116461, .T. ) ;
#204551 = DIRECTION ( 'NONE',  ( -1.000000000000000000, 0.000000000000000000, -0.000000000000000000 ) ) ;
#204552 = AXIS2_PLACEMENT_3D ( 'NONE', #77534, #237916, #257422 ) ;
#204553 = FACE_OUTER_BOUND ( 'NONE', #86670, .T. ) ;
#204554 = AXIS2_PLACEMENT_3D ( 'NONE', #15492, #55845, #156299 ) ;
#204555 = TOROIDAL_SURFACE ( 'NONE', #138087, 0.2000000000000000111, 0.1000000000000000056 ) ;
#204556 = DIRECTION ( 'NONE',  ( 0.000000000000000000, -0.000000000000000000, 1.000000000000000000 ) ) ;
#204557 = AXIS2_PLACEMENT_3D ( 'NONE', #67130, #64556, #45002 ) ;
#204558 = ORIENTED_EDGE ( 'NONE', *, *, #93626, .F. ) ;
#204559 = VERTEX_POINT ( 'NONE', #80744 ) ;
#204560 = CARTESIAN_POINT ( 'NONE',  ( -20.94999999999994600, 66.15000000001120384, -5.923107484524795296 ) ) ;
#204562 = ORIENTED_EDGE ( 'NONE', *, *, #220343, .T. ) ;
#204561 = CARTESIAN_POINT ( 'NONE',  ( 18.54999999999999716, 67.25000000001257661, -190.8731074845244109 ) ) ;
#204563 = CARTESIAN_POINT ( 'NONE',  ( 23.14999999999999858, 5.600000000011153389, -188.5947339810868755 ) ) ;
#204564 = DIRECTION ( 'NONE',  ( 0.000000000000000000, 6.938893903907234689E-15, -1.000000000000000000 ) ) ;
#204565 = EDGE_CURVE ( 'NONE', #92187, #239104, #58153, .T. ) ;
#204566 = ORIENTED_EDGE ( 'NONE', *, *, #89613, .T. ) ;
#204567 = CARTESIAN_POINT ( 'NONE',  ( -18.40000000000000213, 8.212522512469059066, -212.1579332307740344 ) ) ;
#204568 = ADVANCED_FACE ( 'NONE', ( #100305 ), #42927, .T. ) ;
#204569 = FACE_OUTER_BOUND ( 'NONE', #186192, .T. ) ;
#204570 = VERTEX_POINT ( 'NONE', #121218 ) ;
#204571 = CARTESIAN_POINT ( 'NONE',  ( -23.15000000000000213, -9.000000000000001776, -23.60603087734756045 ) ) ;
#204572 = FACE_OUTER_BOUND ( 'NONE', #172726, .T. ) ;
#204573 = ORIENTED_EDGE ( 'NONE', *, *, #61683, .F. ) ;
#204574 = ORIENTED_EDGE ( 'NONE', *, *, #107422, .F. ) ;
#204575 = FACE_OUTER_BOUND ( 'NONE', #223303, .T. ) ;
#204576 = DIRECTION ( 'NONE',  ( 1.000000000000000000, 0.000000000000000000, 0.000000000000000000 ) ) ;
#204577 = CIRCLE ( 'NONE', #4647, 11.70000000000000284 ) ;
#204578 = CARTESIAN_POINT ( 'NONE',  ( -21.05000000000000071, 0.000000000000000000, -21.80000000000000071 ) ) ;
#204579 = CARTESIAN_POINT ( 'NONE',  ( -23.15000000000000213, 16.02417409648692725, -219.3605785455116006 ) ) ;
#204580 = DIRECTION ( 'NONE',  ( 0.000000000000000000, 0.000000000000000000, 1.000000000000000000 ) ) ;
#204581 = DIRECTION ( 'NONE',  ( 0.000000000000000000, 0.2128009952263603677, -0.9770955615653313941 ) ) ;
#204583 = DIRECTION ( 'NONE',  ( 6.938893903907224433E-15, 1.000000000000000000, 7.272083257015735086E-15 ) ) ;
#204582 = CARTESIAN_POINT ( 'NONE',  ( 21.14999999999999858, 64.35000000001156195, -57.27310748452440237 ) ) ;
#204584 = EDGE_CURVE ( 'NONE', #33881, #199540, #124827, .T. ) ;
#204585 = CYLINDRICAL_SURFACE ( 'NONE', #60446, 11.80000000000000426 ) ;
#204586 = DIRECTION ( 'NONE',  ( 0.000000000000000000, 0.9126074666063920260, 0.4088369013362946891 ) ) ;
#204587 = CARTESIAN_POINT ( 'NONE',  ( -20.94999999999999929, -1.162701749926853712, -74.90000000000004832 ) ) ;
#204588 = ORIENTED_EDGE ( 'NONE', *, *, #113924, .F. ) ;
#204589 = ADVANCED_FACE ( 'NONE', ( #101576 ), #139434, .T. ) ;
#204590 = ORIENTED_EDGE ( 'NONE', *, *, #90224, .F. ) ;
#204591 = CARTESIAN_POINT ( 'NONE',  ( -20.94999999999999929, 1.835341550235567887, -78.65515129256301918 ) ) ;
#204592 = DIRECTION ( 'NONE',  ( 1.000000000000000000, -0.000000000000000000, -0.000000000000000000 ) ) ;
#204594 = CARTESIAN_POINT ( 'NONE',  ( -15.51798037960204368, 12.91318972656261188, -216.2290661304645880 ) ) ;
#204593 = PLANE ( 'NONE',  #589 ) ;
#204595 = AXIS2_PLACEMENT_3D ( 'NONE', #12432, #13685, #95773 ) ;
#204596 = CARTESIAN_POINT ( 'NONE',  ( 20.95017935633852346, 39.29138598153966910, -236.8932159614766420 ) ) ;
#204597 = DIRECTION ( 'NONE',  ( 0.000000000000000000, 0.000000000000000000, 1.000000000000000000 ) ) ;
#204598 = DIRECTION ( 'NONE',  ( -1.000000000000000000, 2.952720810173289112E-16, 2.061873921506763405E-30 ) ) ;
#204599 = ORIENTED_EDGE ( 'NONE', *, *, #137245, .F. ) ;
#204600 = ORIENTED_EDGE ( 'NONE', *, *, #219609, .T. ) ;
#204601 = CARTESIAN_POINT ( 'NONE',  ( -12.26136940704872380, 9.351403174141657004, -16.97953043683849117 ) ) ;
#204602 = ORIENTED_EDGE ( 'NONE', *, *, #99735, .T. ) ;
#204603 = EDGE_CURVE ( 'NONE', #156438, #34617, #84564, .T. ) ;
#204604 = LINE ( 'NONE', #238611, #68144 ) ;
#204605 = AXIS2_PLACEMENT_3D ( 'NONE', #98021, #257078, #237573 ) ;
#204606 = AXIS2_PLACEMENT_3D ( 'NONE', #201566, #60764, #81589 ) ;
#204607 = CARTESIAN_POINT ( 'NONE',  ( -15.75000000000000355, 66.15000000001204228, -119.7731074845243739 ) ) ;
#204608 = CIRCLE ( 'NONE', #212991, 12.97499999999999254 ) ;
#204609 = ORIENTED_EDGE ( 'NONE', *, *, #80074, .T. ) ;
#204610 = DIRECTION ( 'NONE',  ( 1.000000000000000000, -3.265361837132813093E-16, -2.280189983783949500E-30 ) ) ;
#204611 = ORIENTED_EDGE ( 'NONE', *, *, #231957, .F. ) ;
#204612 = DIRECTION ( 'NONE',  ( 0.000000000000000000, -0.8814952561688431665, 0.4721928772777346794 ) ) ;
#204613 = DIRECTION ( 'NONE',  ( 0.000000000000000000, 0.2128009952263601456, -0.9770955615653316162 ) ) ;
#204614 = CARTESIAN_POINT ( 'NONE',  ( -21.05000000000000071, 70.15000000001252545, -180.1556047088023149 ) ) ;
#204615 = CARTESIAN_POINT ( 'NONE',  ( 18.40000000000000568, -9.499999999988844479, -140.9993620971801533 ) ) ;
#204616 = CARTESIAN_POINT ( 'NONE',  ( -18.59999999999999787, 7.783179459866048866, -245.3643104511423019 ) ) ;
#204617 = CARTESIAN_POINT ( 'NONE',  ( -16.94445028196807002, 9.992063609697737547, -20.89266982158155628 ) ) ;
#204618 = AXIS2_PLACEMENT_3D ( 'NONE', #134760, #8749, #47844 ) ;
#204619 = DIRECTION ( 'NONE',  ( 1.000000000000000000, 7.304098846218134667E-16, 5.100424963727256530E-30 ) ) ;
#204620 = DIRECTION ( 'NONE',  ( 0.000000000000000000, 0.8814952561688434995, -0.4721928772777335137 ) ) ;
#204622 = VERTEX_POINT ( 'NONE', #40398 ) ;
#204621 = CARTESIAN_POINT ( 'NONE',  ( 20.58091095332318332, 66.98152984665834708, -128.1044573023665691 ) ) ;
#204624 = DIRECTION ( 'NONE',  ( 2.342056488767301376E-15, 0.1350103645451835865, 0.9908441862701605762 ) ) ;
#204623 = DIRECTION ( 'NONE',  ( -1.000000000000000000, 0.000000000000000000, 0.000000000000000000 ) ) ;
#204625 = VERTEX_POINT ( 'NONE', #222830 ) ;
#204627 = ORIENTED_EDGE ( 'NONE', *, *, #123972, .T. ) ;
#204626 = CARTESIAN_POINT ( 'NONE',  ( 21.14999999999999858, 11.19216743630477673, -211.0996217964688810 ) ) ;
#204628 = ORIENTED_EDGE ( 'NONE', *, *, #146797, .T. ) ;
#204629 = DIRECTION ( 'NONE',  ( -1.000000000000000000, 0.000000000000000000, 0.000000000000000000 ) ) ;
#204630 = CARTESIAN_POINT ( 'NONE',  ( -20.94999999999999929, 30.48950451747912993, -239.6099224343151946 ) ) ;
#204631 = CARTESIAN_POINT ( 'NONE',  ( 21.05000000000000071, -0.02138556592653190550, -127.6950388873150075 ) ) ;
#204632 = DIRECTION ( 'NONE',  ( -0.000000000000000000, -6.982962677686266711E-15, 1.000000000000000000 ) ) ;
#204633 = DIRECTION ( 'NONE',  ( 1.000000000000000000, 0.000000000000000000, -0.000000000000000000 ) ) ;
#204634 = CARTESIAN_POINT ( 'NONE',  ( -16.92570016628984675, 9.958788957751012916, -154.8793493299610304 ) ) ;
#204635 = EDGE_CURVE ( 'NONE', #19541, #200766, #133035, .T. ) ;
#204636 = DIRECTION ( 'NONE',  ( 0.000000000000000000, 0.1332476588733448597, -0.9910827722268067408 ) ) ;
#204637 = AXIS2_PLACEMENT_3D ( 'NONE', #228789, #127101, #107531 ) ;
#204638 = AXIS2_PLACEMENT_3D ( 'NONE', #212341, #51934, #173244 ) ;
#204639 = EDGE_CURVE ( 'NONE', #173650, #69817, #20604, .T. ) ;
#204641 = AXIS2_PLACEMENT_3D ( 'NONE', #154876, #117003, #56994 ) ;
#204640 = FACE_OUTER_BOUND ( 'NONE', #232362, .T. ) ;
#204642 = ORIENTED_EDGE ( 'NONE', *, *, #171245, .T. ) ;
#204643 = ORIENTED_EDGE ( 'NONE', *, *, #124223, .F. ) ;
#204644 = LINE ( 'NONE', #26036, #114671 ) ;
#204645 = ORIENTED_EDGE ( 'NONE', *, *, #133816, .F. ) ;
#204646 = FACE_OUTER_BOUND ( 'NONE', #34212, .T. ) ;
#204647 = ORIENTED_EDGE ( 'NONE', *, *, #11389, .F. ) ;
#204648 = CARTESIAN_POINT ( 'NONE',  ( 23.14999999999999503, 14.05000000001115623, -195.4863049292390542 ) ) ;
#204649 = ADVANCED_FACE ( 'NONE', ( #122474 ), #174764, .T. ) ;
#204650 = CARTESIAN_POINT ( 'NONE',  ( -16.95709691156899268, 9.950000000010779999, -180.1600575625135150 ) ) ;
#204651 = LINE ( 'NONE', #61308, #234547 ) ;
#204652 = CARTESIAN_POINT ( 'NONE',  ( -20.54999999999999716, 76.00000000001126921, -203.5231074845248997 ) ) ;
#204653 = EDGE_CURVE ( 'NONE', #60670, #237888, #41245, .T. ) ;
#204654 = DIRECTION ( 'NONE',  ( -1.000000000000000000, -0.000000000000000000, -0.000000000000000000 ) ) ;
#204655 = ORIENTED_EDGE ( 'NONE', *, *, #186572, .T. ) ;
#204656 = CIRCLE ( 'NONE', #63007, 0.1000000000000024342 ) ;
#204657 = DIRECTION ( 'NONE',  ( -1.000000000000000000, 0.000000000000000000, -0.000000000000000000 ) ) ;
#204658 = CARTESIAN_POINT ( 'NONE',  ( 21.05000000000000071, 69.35000000001205933, -124.3731074845243540 ) ) ;
#204659 = EDGE_CURVE ( 'NONE', #40901, #69129, #29193, .T. ) ;
#204660 = CARTESIAN_POINT ( 'NONE',  ( -21.10320863425827298, 0.02502225123826237740, -27.09972261354077006 ) ) ;
#204661 = CARTESIAN_POINT ( 'NONE',  ( -20.85000000000000142, 64.35000000001195986, -109.8069731475024753 ) ) ;
#204662 = EDGE_LOOP ( 'NONE', ( #168432, #131649, #7386, #213945 ) ) ;
#204664 = CYLINDRICAL_SURFACE ( 'NONE', #48292, 11.74999999999999645 ) ;
#204663 = CARTESIAN_POINT ( 'NONE',  ( 23.14999999999999503, 6.650000000011155876, -155.3500000000000227 ) ) ;
#204665 = EDGE_LOOP ( 'NONE', ( #169263, #21963, #226396 ) ) ;
#204667 = ORIENTED_EDGE ( 'NONE', *, *, #208611, .T. ) ;
#204666 = LINE ( 'NONE', #163011, #142010 ) ;
#204668 = ORIENTED_EDGE ( 'NONE', *, *, #27279, .T. ) ;
#204669 = FACE_OUTER_BOUND ( 'NONE', #44113, .T. ) ;
#204670 = DIRECTION ( 'NONE',  ( -1.000000000000000000, 0.000000000000000000, 0.000000000000000000 ) ) ;
#204671 = FACE_OUTER_BOUND ( 'NONE', #71365, .T. ) ;
#204672 = ORIENTED_EDGE ( 'NONE', *, *, #159863, .F. ) ;
#204673 = SPHERICAL_SURFACE ( 'NONE', #138614, 0.1000000000000000056 ) ;
#204674 = EDGE_CURVE ( 'NONE', #163151, #234522, #99013, .T. ) ;
#204675 = CIRCLE ( 'NONE', #9058, 0.09999999999999939493 ) ;
#204676 = DIRECTION ( 'NONE',  ( 1.000000000000000000, 0.000000000000000000, 0.000000000000000000 ) ) ;
#204678 = DIRECTION ( 'NONE',  ( -3.265361837132813093E-16, -1.000000000000000000, 7.445645354460596589E-46 ) ) ;
#204677 = DIRECTION ( 'NONE',  ( -0.000000000000000000, -0.000000000000000000, 1.000000000000000000 ) ) ;
#204680 = ORIENTED_EDGE ( 'NONE', *, *, #13518, .F. ) ;
#204679 = DIRECTION ( 'NONE',  ( -0.000000000000000000, -6.982962677686266711E-15, 1.000000000000000000 ) ) ;
#204681 = CIRCLE ( 'NONE', #113119, 12.77500000000000391 ) ;
#204682 = ORIENTED_EDGE ( 'NONE', *, *, #331, .T. ) ;
#204683 = VECTOR ( 'NONE', #111675, 1000.000000000000000 ) ;
#204684 = CARTESIAN_POINT ( 'NONE',  ( -18.59999999999999787, 42.99798587058931076, -254.2674462307522560 ) ) ;
#204685 = DIRECTION ( 'NONE',  ( 0.000000000000000000, 1.000000000000000000, 0.000000000000000000 ) ) ;
#204686 = DIRECTION ( 'NONE',  ( -1.652117596168391700E-15, -1.000000000000000000, 0.000000000000000000 ) ) ;
#204688 = ORIENTED_EDGE ( 'NONE', *, *, #162807, .F. ) ;
#204687 = AXIS2_PLACEMENT_3D ( 'NONE', #43237, #78487, #98032 ) ;
#204689 = DIRECTION ( 'NONE',  ( -0.000000000000000000, 0.4088369013363297166, -0.9126074666063763718 ) ) ;
#204690 = ORIENTED_EDGE ( 'NONE', *, *, #183164, .F. ) ;
#204691 = DIRECTION ( 'NONE',  ( -1.000000000000000000, 2.849773892568378313E-16, -7.728835255496647986E-17 ) ) ;
#204692 = AXIS2_PLACEMENT_3D ( 'NONE', #7648, #70214, #209696 ) ;
#204693 = DIRECTION ( 'NONE',  ( 0.000000000000000000, 0.2617529984165031243, 0.9651348961777157509 ) ) ;
#204694 = CARTESIAN_POINT ( 'NONE',  ( -23.15000000000000213, 69.20602499728043711, -247.8456586332460176 ) ) ;
#204695 = VERTEX_POINT ( 'NONE', #179885 ) ;
#204696 = CARTESIAN_POINT ( 'NONE',  ( -21.05000000000000071, 43.10494791715829166, -239.6505508802563327 ) ) ;
#204697 = AXIS2_PLACEMENT_3D ( 'NONE', #65609, #99573, #179173 ) ;
#204698 = ORIENTED_EDGE ( 'NONE', *, *, #62969, .T. ) ;
#204699 = CIRCLE ( 'NONE', #92286, 0.1999999999999987899 ) ;
#204700 = FACE_OUTER_BOUND ( 'NONE', #206786, .T. ) ;
#204701 = AXIS2_PLACEMENT_3D ( 'NONE', #33786, #230671, #113279 ) ;
#204702 = EDGE_CURVE ( 'NONE', #130418, #255894, #87389, .T. ) ;
#204703 = EDGE_LOOP ( 'NONE', ( #41076, #130649, #233931, #245826, #183737, #223969, #172677, #13181, #125793, #64655 ) ) ;
#204704 = ORIENTED_EDGE ( 'NONE', *, *, #168463, .F. ) ;
#204705 = AXIS2_PLACEMENT_3D ( 'NONE', #88967, #210240, #249360 ) ;
#204706 = ORIENTED_EDGE ( 'NONE', *, *, #198498, .F. ) ;
#204707 = DIRECTION ( 'NONE',  ( 0.000000000000000000, -1.000000000000000000, -6.982962677686265922E-15 ) ) ;
#204708 = ORIENTED_EDGE ( 'NONE', *, *, #96506, .F. ) ;
#204710 = ORIENTED_EDGE ( 'NONE', *, *, #116114, .T. ) ;
#204709 = CARTESIAN_POINT ( 'NONE',  ( 21.05000000000005400, 76.00000000001119815, -36.02310748452479316 ) ) ;
#204712 = EDGE_CURVE ( 'NONE', #40935, #45962, #1203, .T. ) ;
#204711 = AXIS2_PLACEMENT_3D ( 'NONE', #167194, #245423, #107174 ) ;
#204713 = ORIENTED_EDGE ( 'NONE', *, *, #232144, .F. ) ;
#204715 = ORIENTED_EDGE ( 'NONE', *, *, #143483, .F. ) ;
#204714 = VERTEX_POINT ( 'NONE', #243691 ) ;
#204716 = EDGE_CURVE ( 'NONE', #183161, #182093, #220295, .T. ) ;
#204717 = EDGE_CURVE ( 'NONE', #58672, #83997, #159049, .T. ) ;
#204718 = DIRECTION ( 'NONE',  ( 1.000000000000000000, 0.000000000000000000, 0.000000000000000000 ) ) ;
#204719 = VERTEX_POINT ( 'NONE', #208441 ) ;
#204720 = DIRECTION ( 'NONE',  ( 0.000000000000000000, -1.000000000000000000, 0.000000000000000000 ) ) ;
#204721 = AXIS2_PLACEMENT_3D ( 'NONE', #20880, #198199, #139497 ) ;
#204722 = CIRCLE ( 'NONE', #8933, 12.87499999999999822 ) ;
#204723 = DIRECTION ( 'NONE',  ( 0.000000000000000000, 0.000000000000000000, -1.000000000000000000 ) ) ;
#204724 = TOROIDAL_SURFACE ( 'NONE', #21592, 0.6000000000000013101, 0.1000000000000000056 ) ;
#204726 = CARTESIAN_POINT ( 'NONE',  ( -18.59999994787167310, 86.99309687513043343, -199.3734559884612452 ) ) ;
#204725 = CIRCLE ( 'NONE', #134005, 11.74999999999999645 ) ;
#204727 = ORIENTED_EDGE ( 'NONE', *, *, #109341, .F. ) ;
#204728 = CARTESIAN_POINT ( 'NONE',  ( -20.00857864376270001, 9.150000000000002132, -21.25000000000000000 ) ) ;
#204730 = ORIENTED_EDGE ( 'NONE', *, *, #182181, .F. ) ;
#204729 = CARTESIAN_POINT ( 'NONE',  ( 18.58143601961857883, 63.63777463829045900, -209.2364543610155465 ) ) ;
#204731 = CARTESIAN_POINT ( 'NONE',  ( -16.79184697841823848, 9.948761661669548673, -180.1541422706025060 ) ) ;
#204733 = VERTEX_POINT ( 'NONE', #148457 ) ;
#204732 = PLANE ( 'NONE',  #52472 ) ;
#204734 = EDGE_CURVE ( 'NONE', #52565, #85287, #253987, .T. ) ;
#204735 =( BOUNDED_CURVE ( )  B_SPLINE_CURVE ( 3, ( #126048, #66091, #145614, #102620 ),
 .UNSPECIFIED., .F., .T. ) 
 B_SPLINE_CURVE_WITH_KNOTS ( ( 4, 4 ),
 ( 3.141592653589793116, 4.712388980384689674 ),
 .UNSPECIFIED. ) 
 CURVE ( )  GEOMETRIC_REPRESENTATION_ITEM ( )  RATIONAL_B_SPLINE_CURVE ( ( 1.000000000000000000, 0.8047378541243649375, 0.8047378541243649375, 1.000000000000000000 ) ) 
 REPRESENTATION_ITEM ( '' )  );
#204736 = EDGE_LOOP ( 'NONE', ( #195959, #106640, #174503, #79562 ) ) ;
#204737 = FACE_OUTER_BOUND ( 'NONE', #46234, .T. ) ;
#204738 = ADVANCED_FACE ( 'NONE', ( #29819 ), #169336, .T. ) ;
#204739 = VERTEX_POINT ( 'NONE', #127601 ) ;
#204741 = ORIENTED_EDGE ( 'NONE', *, *, #91189, .F. ) ;
#204740 = B_SPLINE_CURVE_WITH_KNOTS ( 'NONE', 3,
 ( #116873, #97264, #77723, #38624, #118157, #159874, #65884, #46306, #3319, #204098 ),
 .UNSPECIFIED., .F., .F.,
 ( 4, 2, 2, 2, 4 ),
 ( 0.000000000000000000, 0.0001584437871625089497, 0.0002376656807437646035, 0.0002772766275343924169, 0.0003168875743250202845 ),
 .UNSPECIFIED. ) ;
#204742 = DIRECTION ( 'NONE',  ( 0.000000000000000000, 0.000000000000000000, -1.000000000000000000 ) ) ;
#204743 = CARTESIAN_POINT ( 'NONE',  ( -21.05000000000000071, 1.115873073196521464E-11, -160.9593430482987344 ) ) ;
#204744 = CIRCLE ( 'NONE', #84078, 0.09999999999999939493 ) ;
#204746 = EDGE_LOOP ( 'NONE', ( #145262, #216452, #28134, #44417, #148270, #105255 ) ) ;
#204745 = ORIENTED_EDGE ( 'NONE', *, *, #234125, .T. ) ;
#204747 = VERTEX_POINT ( 'NONE', #11518 ) ;
#204748 = DIRECTION ( 'NONE',  ( 0.000000000000000000, 0.000000000000000000, 1.000000000000000000 ) ) ;
#204749 = VERTEX_POINT ( 'NONE', #49340 ) ;
#204750 =( BOUNDED_SURFACE ( )  B_SPLINE_SURFACE ( 3, 2, ( 
 ( #239368, #140239, #21613 ),
 ( #60706, #43732, #120727 ),
 ( #22912, #80249, #124565 ),
 ( #142801, #183249, #20338 ) ),
 .UNSPECIFIED., .F., .F., .F. ) 
 B_SPLINE_SURFACE_WITH_KNOTS ( ( 4, 4 ),
 ( 3, 3 ),
 ( 0.3000847527772363410, 0.5552748953338753068 ),
 ( 0.000000000000000000, 1.000000000000000000 ),
 .UNSPECIFIED. ) 
 GEOMETRIC_REPRESENTATION_ITEM ( )  RATIONAL_B_SPLINE_SURFACE ( (
 ( 1.000000000000000000, 0.9152888060719485130, 1.000000000000000000),
 ( 1.000000000000000000, 0.9104333467450282935, 1.000000000000000000),
 ( 1.000000000000000000, 0.9035312726220630086, 1.000000000000000000),
 ( 1.000000000000000000, 0.8946697475932141597, 1.000000000000000000) ) ) 
 REPRESENTATION_ITEM ( '' )  SURFACE ( )  );
#204751 = ORIENTED_EDGE ( 'NONE', *, *, #155700, .T. ) ;
#204752 = EDGE_CURVE ( 'NONE', #222344, #197418, #71502, .T. ) ;
#204753 = CARTESIAN_POINT ( 'NONE',  ( -18.59999999999999787, 77.26327546522891510, -61.62124281777789037 ) ) ;
#204755 = VERTEX_POINT ( 'NONE', #186300 ) ;
#204754 = CARTESIAN_POINT ( 'NONE',  ( 23.14999999999999503, 53.42432843990430058, -234.7536552047824330 ) ) ;
#204756 = ADVANCED_FACE ( 'NONE', ( #91039 ), #74963, .F. ) ;
#204757 = DIRECTION ( 'NONE',  ( -0.000000000000000000, -0.2814428106787469352, -0.9595780032479105381 ) ) ;
#204758 = EDGE_CURVE ( 'NONE', #256719, #53312, #109297, .T. ) ;
#204759 = CARTESIAN_POINT ( 'NONE',  ( 21.05000000000000071, -11.64999999998883595, -167.4999999999999716 ) ) ;
#204760 = CARTESIAN_POINT ( 'NONE',  ( -23.25000000000000000, 76.00000000001213607, -136.5231074845242745 ) ) ;
#204761 = CARTESIAN_POINT ( 'NONE',  ( 18.39999999999999503, 70.35000000001207354, -123.8731074845243398 ) ) ;
#204762 = ORIENTED_EDGE ( 'NONE', *, *, #44905, .T. ) ;
#204763 = ORIENTED_EDGE ( 'NONE', *, *, #104411, .T. ) ;
#204764 = DIRECTION ( 'NONE',  ( 1.000000000000000000, 0.000000000000000000, 0.000000000000000000 ) ) ;
#204765 = CARTESIAN_POINT ( 'NONE',  ( -18.50000000000000000, 3.912899247244609580, -44.98182297301097066 ) ) ;
#204766 = ORIENTED_EDGE ( 'NONE', *, *, #96436, .T. ) ;
#204767 =( BOUNDED_SURFACE ( )  B_SPLINE_SURFACE ( 3, 2, ( 
 ( #32097, #71218, #227692 ),
 ( #208161, #49060, #128611 ),
 ( #248547, #150738, #29538 ),
 ( #109025, #9941, #69939 ) ),
 .UNSPECIFIED., .F., .F., .T. ) 
 B_SPLINE_SURFACE_WITH_KNOTS ( ( 4, 4 ),
 ( 3, 3 ),
 ( 0.0006461284895273765793, 0.0007503702773986197947 ),
 ( 0.000000000000000000, 1.000000000000000000 ),
 .UNSPECIFIED. ) 
 GEOMETRIC_REPRESENTATION_ITEM ( )  RATIONAL_B_SPLINE_SURFACE ( (
 ( 1.000000000000000000, 0.7071067811865475727, 1.000000000000000000),
 ( 1.000000000000000000, 0.7076476444649250075, 1.000000000000000000),
 ( 1.000000000000000000, 0.7075727925191404033, 1.000000000000000000),
 ( 1.000000000000000000, 0.7071067811865581199, 1.000000000000000000) ) ) 
 REPRESENTATION_ITEM ( '' )  SURFACE ( )  );
#204768 = AXIS2_PLACEMENT_3D ( 'NONE', #216432, #112226, #194340 ) ;
#204769 = DIRECTION ( 'NONE',  ( 1.000000000000000000, -0.000000000000000000, -0.000000000000000000 ) ) ;
#204770 = ORIENTED_EDGE ( 'NONE', *, *, #1769, .F. ) ;
#204771 = ORIENTED_EDGE ( 'NONE', *, *, #127580, .T. ) ;
#204772 = CARTESIAN_POINT ( 'NONE',  ( -21.03922262424653056, 64.37609936600787819, -196.6638994416307753 ) ) ;
#204773 = ORIENTED_EDGE ( 'NONE', *, *, #46531, .F. ) ;
#204774 = CARTESIAN_POINT ( 'NONE',  ( 23.15000000000000213, -11.48912529306489994, -63.89999999999999858 ) ) ;
#204775 = CARTESIAN_POINT ( 'NONE',  ( -21.09610168723072832, 6.378955715235936630, -167.4664104931084410 ) ) ;
#204776 = VERTEX_POINT ( 'NONE', #185005 ) ;
#204777 = DIRECTION ( 'NONE',  ( 1.000000000000000000, 0.000000000000000000, 0.000000000000000000 ) ) ;
#204778 = CARTESIAN_POINT ( 'NONE',  ( -20.64999999999999858, 27.82649702422227733, -239.8850763025288870 ) ) ;
#204780 = CARTESIAN_POINT ( 'NONE',  ( 23.24999999999999645, 4.775700934590584090, -112.3487681040460160 ) ) ;
#204779 = DIRECTION ( 'NONE',  ( 0.000000000000000000, -0.9595780032479205301, 0.2814428106787130734 ) ) ;
#204781 = CARTESIAN_POINT ( 'NONE',  ( 18.49999999999998934, 65.75000000001222134, -145.3731074845244109 ) ) ;
#204782 = LINE ( 'NONE', #143533, #182497 ) ;
#204783 = DIRECTION ( 'NONE',  ( 0.000000000000000000, 0.8814952561688444987, -0.4721928772777320149 ) ) ;
#204784 = EDGE_CURVE ( 'NONE', #222143, #165593, #129106, .T. ) ;
#204785 = CARTESIAN_POINT ( 'NONE',  ( 18.69999999999999929, 1.149999999999999911, -15.00000000000000000 ) ) ;
#204786 = AXIS2_PLACEMENT_3D ( 'NONE', #2484, #161604, #123743 ) ;
#204787 = EDGE_LOOP ( 'NONE', ( #111391, #200612, #107834, #207960 ) ) ;
#204788 = AXIS2_PLACEMENT_3D ( 'NONE', #78121, #157725, #215078 ) ;
#204789 = AXIS2_PLACEMENT_3D ( 'NONE', #184400, #48742, #187004 ) ;
#204791 = ORIENTED_EDGE ( 'NONE', *, *, #56481, .F. ) ;
#204790 = ORIENTED_EDGE ( 'NONE', *, *, #52959, .F. ) ;
#204792 = ORIENTED_EDGE ( 'NONE', *, *, #97641, .T. ) ;
#204793 = ADVANCED_FACE ( 'NONE', ( #227983 ), #141562, .T. ) ;
#204794 = DIRECTION ( 'NONE',  ( -1.000000000000000000, 0.000000000000000000, 0.000000000000000000 ) ) ;
#204795 = CARTESIAN_POINT ( 'NONE',  ( 23.15000000000000213, -4.914013037343258894, -233.1828366659746905 ) ) ;
#204797 = CARTESIAN_POINT ( 'NONE',  ( -14.87779219673428699, 9.430633469072795094, -15.23176579482408499 ) ) ;
#204796 = FACE_OUTER_BOUND ( 'NONE', #87328, .T. ) ;
#204798 = DIRECTION ( 'NONE',  ( -1.000000000000000000, -0.000000000000000000, 0.000000000000000000 ) ) ;
#204799 = ORIENTED_EDGE ( 'NONE', *, *, #245388, .F. ) ;
#204800 = ADVANCED_FACE ( 'NONE', ( #209704 ), #88437, .T. ) ;
#204801 = CARTESIAN_POINT ( 'NONE',  ( -20.64999999999999858, -9.399999999988846611, -124.1060308773475924 ) ) ;
#204802 = CARTESIAN_POINT ( 'NONE',  ( -18.59999999999999787, -9.399999999988787991, -174.7972597596632625 ) ) ;
#204804 = AXIS2_PLACEMENT_3D ( 'NONE', #50625, #132774, #251413 ) ;
#204803 = DIRECTION ( 'NONE',  ( 1.713247197920696616E-14, -0.9876197685951263461, 0.1568667991644794590 ) ) ;
#204805 = EDGE_CURVE ( 'NONE', #256646, #212939, #108041, .T. ) ;
#204806 = CARTESIAN_POINT ( 'NONE',  ( -23.25000000000000000, -1.835859311432481045, -145.6044391687985637 ) ) ;
#204807 = EDGE_LOOP ( 'NONE', ( #173895, #136349, #197780, #240414 ) ) ;
#204808 = DIRECTION ( 'NONE',  ( -1.000000000000000000, -0.000000000000000000, -0.000000000000000000 ) ) ;
#204809 = EDGE_CURVE ( 'NONE', #127058, #33291, #87168, .T. ) ;
#204810 = CARTESIAN_POINT ( 'NONE',  ( -23.25000000000000000, 74.00000000001152500, -48.64772940728643391 ) ) ;
#204811 = EDGE_CURVE ( 'NONE', #200447, #121012, #51885, .T. ) ;
#204812 = ORIENTED_EDGE ( 'NONE', *, *, #72054, .F. ) ;
#204813 = ORIENTED_EDGE ( 'NONE', *, *, #168474, .F. ) ;
#204814 = LINE ( 'NONE', #108307, #170681 ) ;
#204815 = CARTESIAN_POINT ( 'NONE',  ( -22.32929514600008503, 0.4950742925550095652, -230.0667831724111068 ) ) ;
#204816 = DIRECTION ( 'NONE',  ( 0.000000000000000000, 0.000000000000000000, 1.000000000000000000 ) ) ;
#204817 = SPHERICAL_SURFACE ( 'NONE', #164467, 0.1000000000000000056 ) ;
#204818 = DIRECTION ( 'NONE',  ( 0.000000000000000000, 0.000000000000000000, -1.000000000000000000 ) ) ;
#204819 = CARTESIAN_POINT ( 'NONE',  ( 20.95000000000005613, 67.85000000001119247, -25.49719488170504533 ) ) ;
#204820 = VERTEX_POINT ( 'NONE', #7660 ) ;
#204821 = CARTESIAN_POINT ( 'NONE',  ( 21.14999999999999858, -11.64999999998883595, -134.0000000000000000 ) ) ;
#204822 = CARTESIAN_POINT ( 'NONE',  ( -20.85000000000000142, 76.00000000001213607, -136.5231074845243313 ) ) ;
#204823 = DIRECTION ( 'NONE',  ( 0.000000000000000000, 0.2617529984165152257, 0.9651348961777124202 ) ) ;
#204826 = CARTESIAN_POINT ( 'NONE',  ( -23.25000000000000000, 76.00000000001240608, -174.0731074845243711 ) ) ;
#204825 = CIRCLE ( 'NONE', #246353, 0.09999999999999609201 ) ;
#204824 = LINE ( 'NONE', #207429, #116154 ) ;
#204828 = CARTESIAN_POINT ( 'NONE',  ( -20.12071067811865888, 61.46818095087364497, -221.4959865713132956 ) ) ;
#204827 = AXIS2_PLACEMENT_3D ( 'NONE', #231532, #227653, #128571 ) ;
#204829 = AXIS2_PLACEMENT_3D ( 'NONE', #22758, #43584, #42298 ) ;
#204830 = SURFACE_STYLE_FILL_AREA ( #82298 ) ;
#204831 = DIRECTION ( 'NONE',  ( 0.000000000000000000, 0.2128009952263601734, -0.9770955615653316162 ) ) ;
#204832 = LINE ( 'NONE', #103161, #27550 ) ;
#204834 = VERTEX_POINT ( 'NONE', #8937 ) ;
#204833 = CARTESIAN_POINT ( 'NONE',  ( -21.05000000000000071, 14.90151243843701856, -203.3975529985363551 ) ) ;
#204835 = EDGE_CURVE ( 'NONE', #138742, #25677, #67616, .T. ) ;
#204836 = EDGE_CURVE ( 'NONE', #43656, #202799, #89, .T. ) ;
#204837 = EDGE_CURVE ( 'NONE', #93986, #58809, #79192, .T. ) ;
#204838 = TOROIDAL_SURFACE ( 'NONE', #75697, 0.9750000000000019762, 0.1000000000000000056 ) ;
#204839 = CARTESIAN_POINT ( 'NONE',  ( 20.27550659511089037, 66.78395627750344943, -157.3731074845244393 ) ) ;
#204840 = EDGE_CURVE ( 'NONE', #234233, #231766, #46760, .T. ) ;
#204841 = CARTESIAN_POINT ( 'NONE',  ( 22.24259225415828922, 65.17462541034674928, -243.0599263933218595 ) ) ;
#204842 = EDGE_CURVE ( 'NONE', #174151, #165186, #58335, .T. ) ;
#204843 = CARTESIAN_POINT ( 'NONE',  ( 12.47034474403013071, 9.375538102059163492, -149.8698758809908611 ) ) ;
#204844 = VERTEX_POINT ( 'NONE', #135277 ) ;
#204845 = CYLINDRICAL_SURFACE ( 'NONE', #197051, 0.09999999999999867328 ) ;
#204846 = DIRECTION ( 'NONE',  ( 0.000000000000000000, 1.000000000000000000, 6.352154140967427193E-15 ) ) ;
#204847 = DIRECTION ( 'NONE',  ( 1.000000000000000000, 0.000000000000000000, 0.000000000000000000 ) ) ;
#204848 = ADVANCED_FACE ( 'NONE', ( #236968 ), #54469, .F. ) ;
#204849 = ORIENTED_EDGE ( 'NONE', *, *, #31623, .T. ) ;
#204850 = CARTESIAN_POINT ( 'NONE',  ( -23.15000000000000213, 11.75000000000000000, -12.24999999999999822 ) ) ;
#204852 = ORIENTED_EDGE ( 'NONE', *, *, #63303, .F. ) ;
#204851 = CYLINDRICAL_SURFACE ( 'NONE', #59287, 12.87499999999999822 ) ;
#204854 = CARTESIAN_POINT ( 'NONE',  ( -20.85000000000000142, 0.1610488207298751417, -167.2158101556397867 ) ) ;
#204853 = FACE_OUTER_BOUND ( 'NONE', #151415, .T. ) ;
#204855 = AXIS2_PLACEMENT_3D ( 'NONE', #91232, #208618, #152512 ) ;
#204856 = CARTESIAN_POINT ( 'NONE',  ( -0.8999999999999980238, -8.279289321881348584, 22.02928932188134326 ) ) ;
#204857 = EDGE_LOOP ( 'NONE', ( #147945, #40005, #55674, #127770 ) ) ;
#204858 = CARTESIAN_POINT ( 'NONE',  ( -21.05000000000000071, 76.00000000001264766, -199.2231074845243768 ) ) ;
#204859 = EDGE_CURVE ( 'NONE', #130466, #241566, #179200, .T. ) ;
#204860 = CIRCLE ( 'NONE', #125754, 6.329289321881370611 ) ;
#204861 = DIRECTION ( 'NONE',  ( 0.000000000000000000, 0.000000000000000000, 1.000000000000000000 ) ) ;
#204862 = DIRECTION ( 'NONE',  ( -1.000000000000000000, -0.000000000000000000, -0.000000000000000000 ) ) ;
#204863 = CARTESIAN_POINT ( 'NONE',  ( 21.05000000000000071, 77.36087058720364951, -61.45010955743335046 ) ) ;
#204865 = TOROIDAL_SURFACE ( 'NONE', #196673, 0.2000000000000000111, 0.1000000000000000056 ) ;
#204864 = DIRECTION ( 'NONE',  ( -1.000000000000000000, -0.000000000000000000, -0.000000000000000000 ) ) ;
#204866 = ORIENTED_EDGE ( 'NONE', *, *, #133002, .F. ) ;
#204867 = VECTOR ( 'NONE', #230032, 1000.000000000000000 ) ;
#204868 = DIRECTION ( 'NONE',  ( -1.000000000000000000, -2.952720810173289112E-16, 0.000000000000000000 ) ) ;
#204869 = CIRCLE ( 'NONE', #238189, 0.1000000000000124678 ) ;
#204870 = CIRCLE ( 'NONE', #38473, 7.899999999999990585 ) ;
#204871 = CIRCLE ( 'NONE', #171599, 0.09999999999999939493 ) ;
#204872 = CARTESIAN_POINT ( 'NONE',  ( 11.60000000000006004, 67.75000000001118394, -16.98168612828748891 ) ) ;
#204873 = ORIENTED_EDGE ( 'NONE', *, *, #50045, .F. ) ;
#204874 = EDGE_LOOP ( 'NONE', ( #227895, #102569, #160990, #138327 ) ) ;
#204876 = AXIS2_PLACEMENT_3D ( 'NONE', #251956, #231139, #73356 ) ;
#204875 = CARTESIAN_POINT ( 'NONE',  ( 23.24999999999999645, 76.00000000001170974, -69.52310748452431710 ) ) ;
#204878 = VECTOR ( 'NONE', #196188, 1000.000000000000000 ) ;
#204877 = CARTESIAN_POINT ( 'NONE',  ( 23.25000000000000000, 11.75000000001116263, -121.8500000000000369 ) ) ;
#204879 = CYLINDRICAL_SURFACE ( 'NONE', #248401, 0.5000000000000022204 ) ;
#204880 = CARTESIAN_POINT ( 'NONE',  ( 21.05193202509564543, 13.06863776538323307, -210.6116652761761827 ) ) ;
#204881 = DIRECTION ( 'NONE',  ( 0.000000000000000000, 0.1350103645451876666, -0.9908441862701600211 ) ) ;
#204883 = DIRECTION ( 'NONE',  ( 0.000000000000000000, 0.000000000000000000, -1.000000000000000000 ) ) ;
#204882 = DIRECTION ( 'NONE',  ( 0.000000000000000000, 0.2128009952263403282, -0.9770955615653358350 ) ) ;
#204884 = TOROIDAL_SURFACE ( 'NONE', #221441, 0.2000000000000000111, 0.1000000000000000056 ) ;
#204885 = DIRECTION ( 'NONE',  ( 1.000000000000000000, 0.000000000000000000, 0.000000000000000000 ) ) ;
#204886 = DIRECTION ( 'NONE',  ( 0.000000000000000000, 0.000000000000000000, 1.000000000000000000 ) ) ;
#204888 = CARTESIAN_POINT ( 'NONE',  ( -21.05000000000000071, 76.00000000001142553, -36.02310748452432421 ) ) ;
#204887 = AXIS2_PLACEMENT_3D ( 'NONE', #175840, #255298, #197936 ) ;
#204889 = CARTESIAN_POINT ( 'NONE',  ( 21.14999999999999858, 6.650000000011155876, -179.8499999999999943 ) ) ;
#204891 = ORIENTED_EDGE ( 'NONE', *, *, #121865, .F. ) ;
#204890 = CARTESIAN_POINT ( 'NONE',  ( 15.74999999999999645, 62.62192211835341027, -217.1300186905771170 ) ) ;
#204892 = CARTESIAN_POINT ( 'NONE',  ( -20.94999999999999929, 64.25000000001209344, -129.6815067946272677 ) ) ;
#204893 = DIRECTION ( 'NONE',  ( 0.000000000000000000, 0.2617529984164506107, 0.9651348961777299618 ) ) ;
#204895 = CARTESIAN_POINT ( 'NONE',  ( -23.15000000000000213, 64.25000000001179501, -81.67310748452439384 ) ) ;
#204894 = CARTESIAN_POINT ( 'NONE',  ( 21.05000000000000071, 5.000000000011153745, -188.5947339810868755 ) ) ;
#204896 = CIRCLE ( 'NONE', #92468, 12.87499999999999822 ) ;
#204897 = ADVANCED_FACE ( 'NONE', ( #251389 ), #133199, .F. ) ;
#204898 = VERTEX_POINT ( 'NONE', #175735 ) ;
#204899 = DIRECTION ( 'NONE',  ( -0.000000000000000000, 0.9126074666063770380, 0.4088369013363281068 ) ) ;
#204900 = CYLINDRICAL_SURFACE ( 'NONE', #45770, 0.1000000000000000472 ) ;
#204901 = LINE ( 'NONE', #143654, #147198 ) ;
#204902 = DIRECTION ( 'NONE',  ( -1.000000000000000000, -0.000000000000000000, -0.000000000000000000 ) ) ;
#204904 = CARTESIAN_POINT ( 'NONE',  ( 22.49544290803734725, 12.61946619309020790, -223.3444065952062942 ) ) ;
#204903 = TOROIDAL_SURFACE ( 'NONE', #92474, 0.4000000000000003553, 0.1000000000000000056 ) ;
#204905 = VERTEX_POINT ( 'NONE', #76599 ) ;
#204906 = ORIENTED_EDGE ( 'NONE', *, *, #170169, .F. ) ;
#204907 = DIRECTION ( 'NONE',  ( 0.000000000000000000, -6.982962677686266711E-15, 1.000000000000000000 ) ) ;
#204908 = ORIENTED_EDGE ( 'NONE', *, *, #93257, .T. ) ;
#204909 = ADVANCED_FACE ( 'NONE', ( #214824 ), #216580, .T. ) ;
#204911 = CARTESIAN_POINT ( 'NONE',  ( -20.64999999999999858, 53.12864924257549148, -234.3382351616128858 ) ) ;
#204910 = CIRCLE ( 'NONE', #229867, 0.09999999999999982514 ) ;
#204912 = CIRCLE ( 'NONE', #25875, 0.09999999999999918676 ) ;
#204913 = ORIENTED_EDGE ( 'NONE', *, *, #67489, .T. ) ;
#204914 = AXIS2_PLACEMENT_3D ( 'NONE', #72496, #152039, #44917 ) ;
#204915 = LINE ( 'NONE', #185366, #251798 ) ;
#204916 = AXIS2_PLACEMENT_3D ( 'NONE', #208397, #25899, #184959 ) ;
#204917 = CARTESIAN_POINT ( 'NONE',  ( -23.25000000000000000, 74.00000000001180922, -82.14772940728641970 ) ) ;
#204918 = CARTESIAN_POINT ( 'NONE',  ( 21.05000000000000071, 0.7653315920341953182, -212.6731560895497353 ) ) ;
#204919 = VERTEX_POINT ( 'NONE', #156171 ) ;
#204920 = DIRECTION ( 'NONE',  ( 0.000000000000000000, 0.000000000000000000, -1.000000000000000000 ) ) ;
#204921 = CARTESIAN_POINT ( 'NONE',  ( 23.14999999999998437, 66.17117490947157421, -239.7639228359981303 ) ) ;
#204922 = CARTESIAN_POINT ( 'NONE',  ( 18.59999999999998721, 67.84340367245323478, -228.0791829662263410 ) ) ;
#204923 = CARTESIAN_POINT ( 'NONE',  ( -21.14999999999999858, 11.65000000001115588, -33.60000000000000142 ) ) ;
#204924 = DIRECTION ( 'NONE',  ( 0.000000000000000000, -1.000000000000000000, -6.352154140967427193E-15 ) ) ;
#204925 = CARTESIAN_POINT ( 'NONE',  ( -18.59999999999999787, 11.65000000001115232, -121.8500000000000369 ) ) ;
#204926 = CARTESIAN_POINT ( 'NONE',  ( 15.52844286134408769, 62.33593033127508676, -218.0864590324956964 ) ) ;
#204927 = ORIENTED_EDGE ( 'NONE', *, *, #166224, .T. ) ;
#204928 = CIRCLE ( 'NONE', #246629, 4.050000000000006040 ) ;
#204930 = CARTESIAN_POINT ( 'NONE',  ( -18.50000000000000000, 68.97833521811179480, -99.18954208262705663 ) ) ;
#204929 = FACE_OUTER_BOUND ( 'NONE', #74407, .T. ) ;
#204931 = ORIENTED_EDGE ( 'NONE', *, *, #194843, .T. ) ;
#204933 = ORIENTED_EDGE ( 'NONE', *, *, #227671, .F. ) ;
#204932 = DIRECTION ( 'NONE',  ( -1.000000000000000000, -0.000000000000000000, -0.000000000000000000 ) ) ;
#204934 = ORIENTED_EDGE ( 'NONE', *, *, #217507, .F. ) ;
#204935 = DIRECTION ( 'NONE',  ( -1.000000000000000000, 0.000000000000000000, 0.000000000000000000 ) ) ;
#204936 = FACE_OUTER_BOUND ( 'NONE', #24147, .T. ) ;
#204937 = DIRECTION ( 'NONE',  ( 0.000000000000000000, 0.8127272543710951647, -0.5826443254700256480 ) ) ;
#204938 = CARTESIAN_POINT ( 'NONE',  ( 18.59999999999999432, -1.162701749926853712, -108.6000000000000227 ) ) ;
#204939 = ORIENTED_EDGE ( 'NONE', *, *, #144468, .F. ) ;
#204940 = DIRECTION ( 'NONE',  ( 1.000000000000000000, 0.000000000000000000, 0.000000000000000000 ) ) ;
#204941 = DIRECTION ( 'NONE',  ( 0.000000000000000000, -1.000000000000000000, -6.982962677686265922E-15 ) ) ;
#204942 = ORIENTED_EDGE ( 'NONE', *, *, #32682, .T. ) ;
#204943 = EDGE_CURVE ( 'NONE', #144437, #24890, #195764, .T. ) ;
#204944 = DIRECTION ( 'NONE',  ( -1.000000000000000000, -1.836970198721029934E-16, -0.000000000000000000 ) ) ;
#204945 = EDGE_CURVE ( 'NONE', #11272, #151129, #59196, .T. ) ;
#204946 = FACE_OUTER_BOUND ( 'NONE', #83098, .T. ) ;
#204947 = ORIENTED_EDGE ( 'NONE', *, *, #169866, .T. ) ;
#204948 = CARTESIAN_POINT ( 'NONE',  ( 20.85000000000000142, -11.64999999998883595, -167.5000000000000284 ) ) ;
#204949 = AXIS2_PLACEMENT_3D ( 'NONE', #97098, #39769, #585 ) ;
#204950 = ORIENTED_EDGE ( 'NONE', *, *, #7523, .T. ) ;
#204951 = DIRECTION ( 'NONE',  ( -0.000000000000000000, 0.9594490217226120388, 0.2818822000686155849 ) ) ;
#204952 = ORIENTED_EDGE ( 'NONE', *, *, #136510, .F. ) ;
#204953 = DIRECTION ( 'NONE',  ( 0.000000000000000000, 0.000000000000000000, 1.000000000000000000 ) ) ;
#204954 = ADVANCED_FACE ( 'NONE', ( #72792 ), #41644, .T. ) ;
#204955 = CARTESIAN_POINT ( 'NONE',  ( 20.94999999999999929, 64.35000000001176090, -76.30697314750248950 ) ) ;
#204956 = CARTESIAN_POINT ( 'NONE',  ( 19.97071067811867451, 16.71026450801412366, -222.6484636283461498 ) ) ;
#204957 = EDGE_CURVE ( 'NONE', #240431, #139907, #12598, .T. ) ;
#204958 = FACE_OUTER_BOUND ( 'NONE', #179635, .T. ) ;
#204959 = VECTOR ( 'NONE', #91027, 1000.000000000000000 ) ;
#204960 = EDGE_CURVE ( 'NONE', #35199, #53814, #187374, .T. ) ;
#204961 = DIRECTION ( 'NONE',  ( -0.000000000000000000, 6.982962677686266711E-15, -1.000000000000000000 ) ) ;
#204962 = DIRECTION ( 'NONE',  ( 1.000000000000000000, 0.000000000000000000, 0.000000000000000000 ) ) ;
#204963 = DIRECTION ( 'NONE',  ( 0.000000000000000000, 1.000000000000000000, 6.938893903907222067E-15 ) ) ;
#204965 = ORIENTED_EDGE ( 'NONE', *, *, #244203, .F. ) ;
#204964 = CIRCLE ( 'NONE', #238289, 12.97499999999999964 ) ;
#204966 = CARTESIAN_POINT ( 'NONE',  ( -16.89268316805465986, 66.04827818677006235, -149.1673550059788909 ) ) ;
#204967 = DIRECTION ( 'NONE',  ( 0.000000000000000000, 0.000000000000000000, -1.000000000000000000 ) ) ;
#204968 = VECTOR ( 'NONE', #17841, 1000.000000000000000 ) ;
#204969 = DIRECTION ( 'NONE',  ( 0.000000000000000000, 1.000000000000000000, 1.321694076934707365E-14 ) ) ;
#204971 = ORIENTED_EDGE ( 'NONE', *, *, #193478, .F. ) ;
#204970 = DIRECTION ( 'NONE',  ( 0.000000000000000000, 1.072103779144464410E-14, -1.000000000000000000 ) ) ;
#204973 = ORIENTED_EDGE ( 'NONE', *, *, #89160, .T. ) ;
#204972 = CARTESIAN_POINT ( 'NONE',  ( 23.14999999999999503, 64.35000000001186038, -90.87310748452438247 ) ) ;
#204974 = EDGE_CURVE ( 'NONE', #12197, #186900, #4191, .T. ) ;
#204975 = CARTESIAN_POINT ( 'NONE',  ( -21.05000000000000071, 1.851028230152016674, -145.6539132694225032 ) ) ;
#204976 = CARTESIAN_POINT ( 'NONE',  ( -21.05000000000000071, 74.95298800634525094, -207.3836470692357636 ) ) ;
#204977 = CARTESIAN_POINT ( 'NONE',  ( 23.15000000000000213, 87.48912529308822172, -139.6231074845242688 ) ) ;
#204979 = ORIENTED_EDGE ( 'NONE', *, *, #4526, .T. ) ;
#204978 = CARTESIAN_POINT ( 'NONE',  ( 21.09787244211742419, 67.22462929267497600, -157.7838541002068666 ) ) ;
#204980 = AXIS2_PLACEMENT_3D ( 'NONE', #205703, #85726, #27112 ) ;
#204981 = CIRCLE ( 'NONE', #948, 2.000000000000001776 ) ;
#204982 = DIRECTION ( 'NONE',  ( -1.000000000000000000, 0.000000000000000000, -0.000000000000000000 ) ) ;
#204983 = CARTESIAN_POINT ( 'NONE',  ( -20.64999999999999858, -3.770473190032741062, -225.9805569534692324 ) ) ;
#204984 = ORIENTED_EDGE ( 'NONE', *, *, #138589, .T. ) ;
#204985 = DIRECTION ( 'NONE',  ( 0.000000000000000000, 0.000000000000000000, -1.000000000000000000 ) ) ;
#204986 = ORIENTED_EDGE ( 'NONE', *, *, #123244, .T. ) ;
#204987 = DIRECTION ( 'NONE',  ( 0.000000000000000000, 0.000000000000000000, 1.000000000000000000 ) ) ;
#204988 = CARTESIAN_POINT ( 'NONE',  ( -20.00857864376270001, 9.350000000011156942, -121.6500000000000341 ) ) ;
#204989 = ORIENTED_EDGE ( 'NONE', *, *, #98760, .F. ) ;
#204990 = DIRECTION ( 'NONE',  ( 0.000000000000000000, -0.1568667991644355497, -0.9876197685951332295 ) ) ;
#204991 = EDGE_CURVE ( 'NONE', #166025, #141665, #149974, .T. ) ;
#204992 = CIRCLE ( 'NONE', #217465, 11.74999999999999645 ) ;
#204993 = VECTOR ( 'NONE', #38450, 1000.000000000000000 ) ;
#204994 = CARTESIAN_POINT ( 'NONE',  ( -16.86422026484316916, 9.970447360871808939, -180.0822132256729731 ) ) ;
#204995 = AXIS2_PLACEMENT_3D ( 'NONE', #61560, #82366, #101933 ) ;
#204996 = VERTEX_POINT ( 'NONE', #74076 ) ;
#204997 = CARTESIAN_POINT ( 'NONE',  ( 21.09813707148777340, 6.232144213543900690, -199.6106190182799480 ) ) ;
#204998 = EDGE_CURVE ( 'NONE', #100578, #226855, #99837, .T. ) ;
#204999 = ORIENTED_EDGE ( 'NONE', *, *, #95881, .T. ) ;
#205000 = ORIENTED_EDGE ( 'NONE', *, *, #222237, .F. ) ;
#205001 = FACE_OUTER_BOUND ( 'NONE', #254782, .T. ) ;
#205002 = ORIENTED_EDGE ( 'NONE', *, *, #244093, .F. ) ;
#205003 = CARTESIAN_POINT ( 'NONE',  ( 20.94999999999999574, 77.34908441863910866, -128.5366085209788025 ) ) ;
#205004 = ORIENTED_EDGE ( 'NONE', *, *, #86583, .F. ) ;
#205006 = ORIENTED_EDGE ( 'NONE', *, *, #197234, .T. ) ;
#205005 = CARTESIAN_POINT ( 'NONE',  ( 18.59999999999999787, -9.399999999988843058, -107.3820418481727188 ) ) ;
#205007 = EDGE_CURVE ( 'NONE', #73306, #51689, #17903, .T. ) ;
#205008 = AXIS2_PLACEMENT_3D ( 'NONE', #224789, #142679, #46163 ) ;
#205009 = CARTESIAN_POINT ( 'NONE',  ( 20.94999999999999929, 76.00000000001186606, -90.14810748452431710 ) ) ;
#205010 = ORIENTED_EDGE ( 'NONE', *, *, #115129, .T. ) ;
#205011 = DIRECTION ( 'NONE',  ( 0.000000000000000000, -0.2768012769485524438, -0.9609271840673728748 ) ) ;
#205012 = ORIENTED_EDGE ( 'NONE', *, *, #156647, .T. ) ;
#205014 = EDGE_LOOP ( 'NONE', ( #172922, #147302, #83762, #66753 ) ) ;
#205013 = ORIENTED_EDGE ( 'NONE', *, *, #173297, .F. ) ;
#205015 = CARTESIAN_POINT ( 'NONE',  ( 22.50000000000000000, 1.115600667400684642E-11, -167.4999999999999716 ) ) ;
#205016 = ADVANCED_FACE ( 'NONE', ( #177023 ), #62479, .F. ) ;
#205017 = CARTESIAN_POINT ( 'NONE',  ( -20.99780126800934354, 56.17802974602408739, -228.0901074916681637 ) ) ;
#205018 = VERTEX_POINT ( 'NONE', #92312 ) ;
#205019 = AXIS2_PLACEMENT_3D ( 'NONE', #245207, #187809, #49565 ) ;
#205020 = ORIENTED_EDGE ( 'NONE', *, *, #84046, .T. ) ;
#205021 = DIRECTION ( 'NONE',  ( -1.000000000000000000, 0.000000000000000000, 0.000000000000000000 ) ) ;
#205023 = CARTESIAN_POINT ( 'NONE',  ( -20.94999999999999929, 87.39257802171802325, -166.9491579046923277 ) ) ;
#205022 = AXIS2_PLACEMENT_3D ( 'NONE', #99538, #181687, #242927 ) ;
#205024 = EDGE_CURVE ( 'NONE', #87660, #97691, #125022, .T. ) ;
#205026 = EDGE_LOOP ( 'NONE', ( #50072, #5825, #171432, #138559 ) ) ;
#205025 = CARTESIAN_POINT ( 'NONE',  ( 21.05000000000000071, -11.48912529307605546, -30.39999999999999503 ) ) ;
#205027 = DIRECTION ( 'NONE',  ( 0.000000000000000000, 0.000000000000000000, -1.000000000000000000 ) ) ;
#205028 = ORIENTED_EDGE ( 'NONE', *, *, #117263, .T. ) ;
#205029 = FACE_OUTER_BOUND ( 'NONE', #256414, .T. ) ;
#205030 = DIRECTION ( 'NONE',  ( 0.000000000000000000, 0.8660254037844281605, -0.5000000000000185407 ) ) ;
#205031 = AXIS2_PLACEMENT_3D ( 'NONE', #111540, #35874, #168989 ) ;
#205033 = EDGE_LOOP ( 'NONE', ( #163492, #112671, #12023, #110790 ) ) ;
#205032 = EDGE_CURVE ( 'NONE', #195496, #102722, #21784, .T. ) ;
#205034 = EDGE_CURVE ( 'NONE', #250601, #135741, #201683, .T. ) ;
#205035 = FACE_OUTER_BOUND ( 'NONE', #69442, .T. ) ;
#205036 = CARTESIAN_POINT ( 'NONE',  ( 5.899999999999995914, -11.34999999999999964, 10.00000000000000178 ) ) ;
#205037 = CIRCLE ( 'NONE', #138575, 0.5999999999999998668 ) ;
#205038 = CIRCLE ( 'NONE', #9248, 0.1000000000000017542 ) ;
#205040 = ORIENTED_EDGE ( 'NONE', *, *, #94170, .F. ) ;
#205039 = AXIS2_PLACEMENT_3D ( 'NONE', #44423, #104356, #5251 ) ;
#205041 = DIRECTION ( 'NONE',  ( -0.000000000000000000, -6.982962677686266711E-15, 1.000000000000000000 ) ) ;
#205042 = ORIENTED_EDGE ( 'NONE', *, *, #153309, .F. ) ;
#205043 = CIRCLE ( 'NONE', #146786, 0.09999999999999939493 ) ;
#205044 = EDGE_CURVE ( 'NONE', #26537, #61614, #95757, .T. ) ;
#205046 = ORIENTED_EDGE ( 'NONE', *, *, #18394, .F. ) ;
#205045 = ORIENTED_EDGE ( 'NONE', *, *, #137418, .T. ) ;
#205047 = VERTEX_POINT ( 'NONE', #101249 ) ;
#205048 = VERTEX_POINT ( 'NONE', #2183 ) ;
#205049 = DIRECTION ( 'NONE',  ( 0.000000000000000000, 0.1480365673253023762, -0.9889818879709281196 ) ) ;
#205050 = ORIENTED_EDGE ( 'NONE', *, *, #229156, .F. ) ;
#205051 = EDGE_CURVE ( 'NONE', #117707, #49547, #180850, .T. ) ;
#205052 = DIRECTION ( 'NONE',  ( 0.000000000000000000, -0.4721928772777346239, -0.8814952561688430555 ) ) ;
#205053 = EDGE_CURVE ( 'NONE', #252623, #118654, #199860, .T. ) ;
#205054 = AXIS2_PLACEMENT_3D ( 'NONE', #91942, #231474, #189763 ) ;
#205055 = DIRECTION ( 'NONE',  ( 0.000000000000000000, -6.467318590049456648E-15, 1.000000000000000000 ) ) ;
#205057 = ORIENTED_EDGE ( 'NONE', *, *, #99455, .F. ) ;
#205056 = CIRCLE ( 'NONE', #196692, 0.6000000000000015321 ) ;
#205058 = EDGE_LOOP ( 'NONE', ( #92897, #118390, #37613, #94016 ) ) ;
#205059 = CIRCLE ( 'NONE', #84221, 0.09999999999998898659 ) ;
#205060 = CIRCLE ( 'NONE', #75918, 0.1000000000000012407 ) ;
#205061 = ORIENTED_EDGE ( 'NONE', *, *, #198084, .T. ) ;
#205062 = AXIS2_PLACEMENT_3D ( 'NONE', #165932, #148928, #171092 ) ;
#205063 = CIRCLE ( 'NONE', #34255, 0.1000000000000002554 ) ;
#205064 = CARTESIAN_POINT ( 'NONE',  ( 21.05000000000000071, 33.04479387145709524, -247.6151719044046899 ) ) ;
#205065 = EDGE_CURVE ( 'NONE', #184662, #197543, #120937, .T. ) ;
#205066 = ORIENTED_EDGE ( 'NONE', *, *, #232207, .F. ) ;
#205067 = EDGE_CURVE ( 'NONE', #76136, #191527, #212686, .T. ) ;
#205068 = PLANE ( 'NONE',  #241834 ) ;
#205069 = CIRCLE ( 'NONE', #192637, 0.4000000000000045186 ) ;
#205071 = ORIENTED_EDGE ( 'NONE', *, *, #192654, .F. ) ;
#205070 = DIRECTION ( 'NONE',  ( 0.000000000000000000, -0.01283462868042125823, -0.9999176327611367654 ) ) ;
#205072 = DIRECTION ( 'NONE',  ( 0.000000000000000000, 0.000000000000000000, 1.000000000000000000 ) ) ;
#205073 = DIRECTION ( 'NONE',  ( 1.000000000000000000, 0.000000000000000000, 0.000000000000000000 ) ) ;
#205074 = CARTESIAN_POINT ( 'NONE',  ( 18.59999999999999076, 6.649999999999999467, -21.15000000000000213 ) ) ;
#205075 = DIRECTION ( 'NONE',  ( 1.000000000000000000, -1.335000415235278971E-16, 2.979993593738921214E-16 ) ) ;
#205076 = CARTESIAN_POINT ( 'NONE',  ( -18.47653818581420992, 85.46528038777560710, -196.3971466683844938 ) ) ;
#205078 = DIRECTION ( 'NONE',  ( -1.000000000000000000, 0.000000000000000000, -0.000000000000000000 ) ) ;
#205077 = DIRECTION ( 'NONE',  ( 0.000000000000000000, 0.000000000000000000, -1.000000000000000000 ) ) ;
#205079 = DIRECTION ( 'NONE',  ( -1.836970198721029934E-16, -1.000000000000000000, -6.982962677686266711E-15 ) ) ;
#205080 = DIRECTION ( 'NONE',  ( 0.000000000000000000, 0.000000000000000000, -1.000000000000000000 ) ) ;
#205081 = EDGE_CURVE ( 'NONE', #52463, #176327, #139105, .T. ) ;
#205082 = DIRECTION ( 'NONE',  ( -1.000000000000000000, 0.000000000000000000, 0.000000000000000000 ) ) ;
#205083 = DIRECTION ( 'NONE',  ( 0.000000000000000000, -0.9955484899852801162, 0.09425075112713271475 ) ) ;
#205084 = AXIS2_PLACEMENT_3D ( 'NONE', #46455, #67316, #148140 ) ;
#205086 = EDGE_LOOP ( 'NONE', ( #130161, #48745, #133951, #222029 ) ) ;
#205085 = AXIS2_PLACEMENT_3D ( 'NONE', #186369, #123824, #225458 ) ;
#205087 = AXIS2_PLACEMENT_3D ( 'NONE', #172840, #189789, #168983 ) ;
#205089 = ORIENTED_EDGE ( 'NONE', *, *, #42067, .T. ) ;
#205088 = DIRECTION ( 'NONE',  ( 3.469446951953728416E-14, 0.8660254037844343777, -0.5000000000000074385 ) ) ;
#205090 = ORIENTED_EDGE ( 'NONE', *, *, #58218, .T. ) ;
#205091 = PLANE ( 'NONE',  #257426 ) ;
#205092 = CARTESIAN_POINT ( 'NONE',  ( 20.53930447207977039, 8.977148687535430938, -142.4425071415754189 ) ) ;
#205093 = CARTESIAN_POINT ( 'NONE',  ( -20.64999999999999858, 8.751106741858205140, -220.7398867978736234 ) ) ;
#205094 = EDGE_LOOP ( 'NONE', ( #131611, #16451, #80039 ) ) ;
#205095 = ADVANCED_FACE ( 'NONE', ( #3476 ), #63450, .F. ) ;
#205096 = DIRECTION ( 'NONE',  ( 0.000000000000000000, -0.9889818879709260102, -0.1480365673253158931 ) ) ;
#205097 = EDGE_CURVE ( 'NONE', #160136, #124309, #187576, .T. ) ;
#205098 = CARTESIAN_POINT ( 'NONE',  ( 21.04999999999999716, 65.63508186416100898, -242.0676793166472294 ) ) ;
#205099 = AXIS2_PLACEMENT_3D ( 'NONE', #86764, #45094, #8539 ) ;
#205100 = EDGE_LOOP ( 'NONE', ( #190382, #120623, #11957, #31140 ) ) ;
#205101 = FACE_OUTER_BOUND ( 'NONE', #87476, .T. ) ;
#205102 = CARTESIAN_POINT ( 'NONE',  ( -18.59999999999999787, 1.115600667400684642E-11, -200.9999999999999432 ) ) ;
#205103 = LINE ( 'NONE', #126880, #255239 ) ;
#205104 = AXIS2_PLACEMENT_3D ( 'NONE', #160683, #240202, #5394 ) ;
#205105 = EDGE_CURVE ( 'NONE', #58804, #233793, #120901, .T. ) ;
#205106 = CARTESIAN_POINT ( 'NONE',  ( 21.14999999999999858, 64.25000000001276135, -215.2731074845244450 ) ) ;
#205108 = ORIENTED_EDGE ( 'NONE', *, *, #153268, .F. ) ;
#205107 = CARTESIAN_POINT ( 'NONE',  ( -16.81744102076749314, 66.05000000001230376, -157.3731074845244393 ) ) ;
#205109 = CARTESIAN_POINT ( 'NONE',  ( -21.05000000000000071, -11.29603075032412463, -197.9521008403361009 ) ) ;
#205110 = CARTESIAN_POINT ( 'NONE',  ( -20.64999999999999858, 2.400000000011155432, -187.7753780772378889 ) ) ;
#205112 = ADVANCED_FACE ( 'NONE', ( #59570 ), #99987, .F. ) ;
#205111 = CARTESIAN_POINT ( 'NONE',  ( -20.85000000000000142, 7.783179459866048866, -245.3643104511423019 ) ) ;
#205113 = DIRECTION ( 'NONE',  ( 0.7071067811865487940, 8.659560562354918067E-17, 0.7071067811865463515 ) ) ;
#205114 = VERTEX_POINT ( 'NONE', #257753 ) ;
#205115 = CARTESIAN_POINT ( 'NONE',  ( 23.14999999999999503, 11.65000000001116298, -88.35000000000003695 ) ) ;
#205116 = DIRECTION ( 'NONE',  ( 0.7070776581708965169, 4.937903618720407826E-15, -0.7071359030027827286 ) ) ;
#205118 = FACE_OUTER_BOUND ( 'NONE', #136622, .T. ) ;
#205117 = CARTESIAN_POINT ( 'NONE',  ( 23.14999999999998437, 76.00000000001270450, -207.5731074845243427 ) ) ;
#205120 = ADVANCED_FACE ( 'NONE', ( #242086 ), #4742, .T. ) ;
#205119 = CARTESIAN_POINT ( 'NONE',  ( -21.05000000000000071, 0.6656436123793491033, -212.6810495496487476 ) ) ;
#205121 = CARTESIAN_POINT ( 'NONE',  ( -16.87683809663752399, 9.865889849343641771, -53.73257319293013978 ) ) ;
#205122 = PLANE ( 'NONE',  #156133 ) ;
#205123 = CARTESIAN_POINT ( 'NONE',  ( -20.85000000000000142, 77.16412189325330928, -128.7082593989527197 ) ) ;
#205124 = CARTESIAN_POINT ( 'NONE',  ( -20.64999999999999858, 74.00000000001259082, -190.2984855617622770 ) ) ;
#205125 = VERTEX_POINT ( 'NONE', #179577 ) ;
#205126 = EDGE_CURVE ( 'NONE', #12728, #109914, #24357, .T. ) ;
#205127 = DIRECTION ( 'NONE',  ( 0.7071067811865388020, -0.7071067811865561215, 0.000000000000000000 ) ) ;
#205129 = ADVANCED_FACE ( 'NONE', ( #43900 ), #233367, .F. ) ;
#205128 = EDGE_CURVE ( 'NONE', #10477, #217558, #115607, .T. ) ;
#205130 = ORIENTED_EDGE ( 'NONE', *, *, #208750, .F. ) ;
#205131 = ORIENTED_EDGE ( 'NONE', *, *, #196040, .F. ) ;
#205132 = CARTESIAN_POINT ( 'NONE',  ( 23.14999999999999858, 40.18490544642472884, -251.4399342103543233 ) ) ;
#205133 = CYLINDRICAL_SURFACE ( 'NONE', #69491, 0.09999999999999817368 ) ;
#205134 = VERTEX_POINT ( 'NONE', #98692 ) ;
#205135 = SHAPE_REPRESENTATION ( 'Fixed End Mounting Bracket', ( #2425 ), #231390 ) ;
#205136 = ORIENTED_EDGE ( 'NONE', *, *, #200419, .F. ) ;
#205137 = VECTOR ( 'NONE', #93276, 1000.000000000000000 ) ;
#205138 = EDGE_LOOP ( 'NONE', ( #119333, #238180, #188044 ) ) ;
#205139 = EDGE_CURVE ( 'NONE', #231216, #191603, #129291, .T. ) ;
#205140 = DIRECTION ( 'NONE',  ( 0.000000000000000000, 0.000000000000000000, 1.000000000000000000 ) ) ;
#205141 = EDGE_CURVE ( 'NONE', #70872, #116247, #175128, .T. ) ;
#205142 = VERTEX_POINT ( 'NONE', #12182 ) ;
#205143 = CIRCLE ( 'NONE', #109474, 0.1000000000000028644 ) ;
#205144 = DIRECTION ( 'NONE',  ( 0.000000000000000000, -6.454785026890489601E-15, 1.000000000000000000 ) ) ;
#205145 = DIRECTION ( 'NONE',  ( 0.000000000000000000, 0.000000000000000000, -1.000000000000000000 ) ) ;
#205146 = DIRECTION ( 'NONE',  ( 0.000000000000000000, 0.000000000000000000, -1.000000000000000000 ) ) ;
#205147 = DIRECTION ( 'NONE',  ( 0.000000000000000000, -2.362176648138631684E-15, -1.000000000000000000 ) ) ;
#205148 = CARTESIAN_POINT ( 'NONE',  ( -21.64999999999999858, 65.95000000001208207, -123.8731074845243683 ) ) ;
#205149 = AXIS2_PLACEMENT_3D ( 'NONE', #193311, #92902, #233726 ) ;
#205150 = EDGE_CURVE ( 'NONE', #103023, #182231, #146023, .T. ) ;
#205151 = DIRECTION ( 'NONE',  ( 0.000000000000000000, -0.4088369013363280513, 0.9126074666063769270 ) ) ;
#205152 = DIRECTION ( 'NONE',  ( 0.000000000000000000, -7.545205021724366615E-15, 1.000000000000000000 ) ) ;
#205154 = ORIENTED_EDGE ( 'NONE', *, *, #151131, .F. ) ;
#205153 = CYLINDRICAL_SURFACE ( 'NONE', #88341, 0.09999999999999939493 ) ;
#205156 = CARTESIAN_POINT ( 'NONE',  ( 18.49999999999999289, 69.15387683765952431, -132.7853812176745407 ) ) ;
#205155 = DIRECTION ( 'NONE',  ( 1.040834085586049673E-13, 0.7899159663865300551, 0.6132151058540831201 ) ) ;
#205157 = DIRECTION ( 'NONE',  ( 0.000000000000000000, 0.000000000000000000, -1.000000000000000000 ) ) ;
#205158 = ADVANCED_FACE ( 'NONE', ( #30453 ), #195944, .F. ) ;
#205159 = ORIENTED_EDGE ( 'NONE', *, *, #182007, .F. ) ;
#205160 = DIRECTION ( 'NONE',  ( -1.000000000000000000, -0.000000000000000000, 0.000000000000000000 ) ) ;
#205161 = DIRECTION ( 'NONE',  ( 0.000000000000000000, -0.7092521942343974484, -0.7049548389604062271 ) ) ;
#205162 = CARTESIAN_POINT ( 'NONE',  ( 21.05000000000000071, -0.01681986837452062455, -60.69257478043463294 ) ) ;
#205163 = EDGE_LOOP ( 'NONE', ( #763, #257292, #65485, #200197 ) ) ;
#205164 = EDGE_CURVE ( 'NONE', #134353, #88487, #200024, .T. ) ;
#205165 = CIRCLE ( 'NONE', #213354, 0.1000000000000028644 ) ;
#205167 = CARTESIAN_POINT ( 'NONE',  ( -21.05000000000000071, 64.35000000001195986, -102.9231074845243938 ) ) ;
#205166 = AXIS2_PLACEMENT_3D ( 'NONE', #242223, #220111, #200540 ) ;
#205168 = CYLINDRICAL_SURFACE ( 'NONE', #2339, 0.1000000000000024342 ) ;
#205169 = ORIENTED_EDGE ( 'NONE', *, *, #96406, .F. ) ;
#205170 = CARTESIAN_POINT ( 'NONE',  ( 21.14999999999999858, 6.540656951712401579, -67.00000000000004263 ) ) ;
#205171 = CARTESIAN_POINT ( 'NONE',  ( -23.15000000000000213, 87.48912529308749697, -39.12310748452424747 ) ) ;
#205172 = CIRCLE ( 'NONE', #163501, 0.09999999999998898659 ) ;
#205173 = CYLINDRICAL_SURFACE ( 'NONE', #98922, 0.09999999999999971412 ) ;
#205174 = CARTESIAN_POINT ( 'NONE',  ( -22.59999970745345976, -0.009356377315856832799, -122.2494867923307993 ) ) ;
#205175 = ADVANCED_FACE ( 'NONE', ( #108687 ), #50845, .T. ) ;
#205176 = ORIENTED_EDGE ( 'NONE', *, *, #165875, .T. ) ;
#205177 = ADVANCED_FACE ( 'NONE', ( #229922 ), #104313, .F. ) ;
#205178 = VERTEX_POINT ( 'NONE', #111262 ) ;
#205179 = CIRCLE ( 'NONE', #209283, 2.000000000000001776 ) ;
#205180 = AXIS2_PLACEMENT_3D ( 'NONE', #14192, #108134, #187690 ) ;
#205181 = CIRCLE ( 'NONE', #255016, 4.049999999999998934 ) ;
#205182 = CIRCLE ( 'NONE', #92767, 0.09999999999999949207 ) ;
#205184 = EDGE_CURVE ( 'NONE', #171694, #13123, #190830, .T. ) ;
#205183 = CARTESIAN_POINT ( 'NONE',  ( -16.97092634996622706, 65.99911103366466136, -182.6532502508223104 ) ) ;
#205185 = DIRECTION ( 'NONE',  ( 0.000000000000000000, 0.000000000000000000, -1.000000000000000000 ) ) ;
#205186 = DIRECTION ( 'NONE',  ( 0.000000000000000000, -0.4721928772777346239, -0.8814952561688430555 ) ) ;
#205187 = DIRECTION ( 'NONE',  ( -0.000000000000000000, -0.000000000000000000, -1.000000000000000000 ) ) ;
#205188 = DIRECTION ( 'NONE',  ( 1.000000000000000000, 0.000000000000000000, 0.000000000000000000 ) ) ;
#205189 = DIRECTION ( 'NONE',  ( 1.000000000000000000, 0.000000000000000000, 0.000000000000000000 ) ) ;
#205190 = ORIENTED_EDGE ( 'NONE', *, *, #65539, .T. ) ;
#205191 = CARTESIAN_POINT ( 'NONE',  ( -20.93975676684922504, 65.68895814178239334, -97.50265578621379348 ) ) ;
#205193 = ORIENTED_EDGE ( 'NONE', *, *, #39770, .F. ) ;
#205192 = CARTESIAN_POINT ( 'NONE',  ( 21.05000000000000071, 58.88775506787933978, -225.6504858384382999 ) ) ;
#205194 = CARTESIAN_POINT ( 'NONE',  ( -21.05000000000000071, 6.540656951712400691, -33.50000000000000000 ) ) ;
#205195 = CYLINDRICAL_SURFACE ( 'NONE', #232191, 0.1000000000000002554 ) ;
#205196 = LINE ( 'NONE', #186966, #25423 ) ;
#205197 = DIRECTION ( 'NONE',  ( 1.000000000000000000, 0.000000000000000000, 0.000000000000000000 ) ) ;
#205198 = EDGE_CURVE ( 'NONE', #132890, #195387, #125194, .T. ) ;
#205199 = DIRECTION ( 'NONE',  ( 1.000000000000000000, -0.000000000000000000, 0.000000000000000000 ) ) ;
#205201 = ORIENTED_EDGE ( 'NONE', *, *, #163640, .F. ) ;
#205200 = CARTESIAN_POINT ( 'NONE',  ( 23.30000000000000426, -11.79999999999999538, -347.0000000000001137 ) ) ;
#205202 = DIRECTION ( 'NONE',  ( -0.000000000000000000, 0.000000000000000000, 1.000000000000000000 ) ) ;
#205203 = FACE_OUTER_BOUND ( 'NONE', #219702, .T. ) ;
#205204 = DIRECTION ( 'NONE',  ( 0.000000000000000000, 0.9126074666063753726, 0.4088369013363317150 ) ) ;
#205205 = FACE_OUTER_BOUND ( 'NONE', #190604, .T. ) ;
#205206 = VERTEX_POINT ( 'NONE', #45178 ) ;
#205207 = CARTESIAN_POINT ( 'NONE',  ( 20.94999999999999929, -3.685352791942192674, -226.3713951780953550 ) ) ;
#205208 = FACE_OUTER_BOUND ( 'NONE', #137361, .T. ) ;
#205209 = DIRECTION ( 'NONE',  ( 0.000000000000000000, -0.2617529984165030132, -0.9651348961777157509 ) ) ;
#205210 = VECTOR ( 'NONE', #53917, 1000.000000000000000 ) ;
#205211 = DIRECTION ( 'NONE',  ( 1.000000000000000000, 0.000000000000000000, 0.000000000000000000 ) ) ;
#205212 = ORIENTED_EDGE ( 'NONE', *, *, #57176, .F. ) ;
#205213 = EDGE_CURVE ( 'NONE', #177501, #46909, #124726, .T. ) ;
#205214 = CARTESIAN_POINT ( 'NONE',  ( -16.85722902420147662, 9.950000000011105072, -87.73445252622929047 ) ) ;
#205215 = ORIENTED_EDGE ( 'NONE', *, *, #13720, .F. ) ;
#205216 = CARTESIAN_POINT ( 'NONE',  ( 11.60000000000000142, -8.250000000000003553, 12.40000000000000391 ) ) ;
#205217 = CYLINDRICAL_SURFACE ( 'NONE', #66701, 0.09999999999999939493 ) ;
#205218 = AXIS2_PLACEMENT_3D ( 'NONE', #15913, #91568, #171153 ) ;
#205219 =( LENGTH_UNIT ( ) NAMED_UNIT ( * ) SI_UNIT ( .MILLI., .METRE. ) );
#205220 = CARTESIAN_POINT ( 'NONE',  ( -23.15000000000000213, 76.00000000001215028, -138.6231074845243256 ) ) ;
#205221 = ORIENTED_EDGE ( 'NONE', *, *, #143768, .F. ) ;
#205222 = AXIS2_PLACEMENT_3D ( 'NONE', #147469, #225687, #250418 ) ;
#205223 = DIRECTION ( 'NONE',  ( 0.000000000000000000, 0.000000000000000000, -1.000000000000000000 ) ) ;
#205224 = AXIS2_PLACEMENT_3D ( 'NONE', #126108, #32188, #169142 ) ;
#205225 = CARTESIAN_POINT ( 'NONE',  ( 21.14999999999999858, 13.07482039728800061, -210.6896000549707537 ) ) ;
#205226 = AXIS2_PLACEMENT_3D ( 'NONE', #79330, #121081, #138019 ) ;
#205227 = AXIS2_PLACEMENT_3D ( 'NONE', #225276, #126191, #47935 ) ;
#205228 = B_SPLINE_CURVE_WITH_KNOTS ( 'NONE', 3,
 ( #98338, #158397, #194938, #16306 ),
 .UNSPECIFIED., .F., .F.,
 ( 4, 4 ),
 ( 0.000000000000000000, 0.0001048066582182473756 ),
 .UNSPECIFIED. ) ;
#205229 = DIRECTION ( 'NONE',  ( 1.000000000000000000, 0.000000000000000000, 0.000000000000000000 ) ) ;
#205230 = CARTESIAN_POINT ( 'NONE',  ( 22.10000000000000142, -11.65000000000000036, 33.00000000000000000 ) ) ;
#205231 = DIRECTION ( 'NONE',  ( -0.000000000000000000, 6.982962677686266711E-15, -1.000000000000000000 ) ) ;
#205232 = EDGE_LOOP ( 'NONE', ( #26323, #188734, #11299, #152172 ) ) ;
#205234 = ORIENTED_EDGE ( 'NONE', *, *, #10938, .T. ) ;
#205233 = CARTESIAN_POINT ( 'NONE',  ( -20.64999999999999858, 76.00000000001165290, -69.52310748452431710 ) ) ;
#205235 = AXIS2_PLACEMENT_3D ( 'NONE', #13862, #73867, #153414 ) ;
#205236 = ORIENTED_EDGE ( 'NONE', *, *, #153792, .F. ) ;
#205237 = CARTESIAN_POINT ( 'NONE',  ( -23.25000000000000000, 67.55989888862310977, -211.9120700681549465 ) ) ;
#205238 = ORIENTED_EDGE ( 'NONE', *, *, #244692, .F. ) ;
#205239 = CARTESIAN_POINT ( 'NONE',  ( 21.05933563467872105, 65.27547528793073184, -124.3294597355684346 ) ) ;
#205240 = CARTESIAN_POINT ( 'NONE',  ( -18.40000000000000213, 13.19198836721619017, -207.5937580722650466 ) ) ;
#205241 = ORIENTED_EDGE ( 'NONE', *, *, #181535, .F. ) ;
#205242 = CARTESIAN_POINT ( 'NONE',  ( 23.14999999999999503, 6.650000000011155876, -146.2500000000000284 ) ) ;
#205243 = DIRECTION ( 'NONE',  ( 0.000000000000000000, -1.000000000000000000, 0.000000000000000000 ) ) ;
#205245 = CARTESIAN_POINT ( 'NONE',  ( 20.21494484322224849, 9.303170737879936425, -41.84026519177099601 ) ) ;
#205244 = AXIS2_PLACEMENT_3D ( 'NONE', #218285, #14996, #138730 ) ;
#205246 = ORIENTED_EDGE ( 'NONE', *, *, #160644, .T. ) ;
#205247 = DIRECTION ( 'NONE',  ( -1.000000000000000000, -0.000000000000000000, -0.000000000000000000 ) ) ;
#205248 = AXIS2_PLACEMENT_3D ( 'NONE', #7662, #127602, #202003 ) ;
#205250 = ORIENTED_EDGE ( 'NONE', *, *, #205798, .F. ) ;
#205249 = CARTESIAN_POINT ( 'NONE',  ( -20.94999999999999929, -11.64999999998884483, -100.5000000000000426 ) ) ;
#205251 = ADVANCED_FACE ( 'NONE', ( #34608 ), #114110, .F. ) ;
#205252 = DIRECTION ( 'NONE',  ( 0.000000000000000000, 0.8660254037844411501, 0.4999999999999956701 ) ) ;
#205253 = CARTESIAN_POINT ( 'NONE',  ( -20.64999999999999858, 74.00000000001205080, -123.2984855617622060 ) ) ;
#205254 = CIRCLE ( 'NONE', #76082, 7.800000000000001599 ) ;
#205255 = ORIENTED_EDGE ( 'NONE', *, *, #94430, .T. ) ;
#205256 = CIRCLE ( 'NONE', #184419, 0.09999999999999971412 ) ;
#205257 = AXIS2_PLACEMENT_3D ( 'NONE', #145012, #9355, #5489 ) ;
#205258 = CARTESIAN_POINT ( 'NONE',  ( 20.94999999999999929, 76.00000000001168132, -65.52310748452430289 ) ) ;
#205259 = CARTESIAN_POINT ( 'NONE',  ( -16.94107738177415357, 44.01795756907897328, -235.2811900454759666 ) ) ;
#205260 = AXIS2_PLACEMENT_3D ( 'NONE', #257103, #232484, #252016 ) ;
#205261 = DIRECTION ( 'NONE',  ( 0.000000000000000000, -0.4088369013363783999, 0.9126074666063545004 ) ) ;
#205262 = ORIENTED_EDGE ( 'NONE', *, *, #171223, .T. ) ;
#205263 = FACE_OUTER_BOUND ( 'NONE', #141663, .T. ) ;
#205264 = ADVANCED_FACE ( 'NONE', ( #108974 ), #158526, .F. ) ;
#205265 = DIRECTION ( 'NONE',  ( -0.000000000000000000, 0.8660254037844411501, 0.4999999999999956701 ) ) ;
#205266 = EDGE_CURVE ( 'NONE', #12740, #177752, #108442, .T. ) ;
#205267 = ORIENTED_EDGE ( 'NONE', *, *, #47482, .F. ) ;
#205268 = EDGE_CURVE ( 'NONE', #253940, #208884, #46069, .T. ) ;
#205269 = AXIS2_PLACEMENT_3D ( 'NONE', #169088, #127355, #107785 ) ;
#205270 = CIRCLE ( 'NONE', #192841, 0.09999999999998898659 ) ;
#205271 = EDGE_LOOP ( 'NONE', ( #38876, #249101, #132993, #163462, #250320 ) ) ;
#205272 = DIRECTION ( 'NONE',  ( 0.000000000000000000, 0.8814952561688430555, -0.4721928772777347905 ) ) ;
#205273 = EDGE_CURVE ( 'NONE', #217297, #21635, #208422, .T. ) ;
#205274 = ORIENTED_EDGE ( 'NONE', *, *, #107701, .F. ) ;
#205275 = ADVANCED_FACE ( 'NONE', ( #149422 ), #150154, .T. ) ;
#205276 = CARTESIAN_POINT ( 'NONE',  ( -23.49999999999994316, 76.00000000001119815, -36.02310748452479316 ) ) ;
#205278 = ORIENTED_EDGE ( 'NONE', *, *, #143355, .T. ) ;
#205277 = DIRECTION ( 'NONE',  ( 0.000000000000000000, 0.000000000000000000, 1.000000000000000000 ) ) ;
#205279 = DIRECTION ( 'NONE',  ( 1.000000000000000000, -0.000000000000000000, -0.000000000000000000 ) ) ;
#205280 = DIRECTION ( 'NONE',  ( 4.239556034732056743E-17, 0.08413937888704772772, -0.9964539953858894128 ) ) ;
#205281 = ADVANCED_FACE ( 'NONE', ( #230217 ), #225114, .F. ) ;
#205282 = FILL_AREA_STYLE_COLOUR ( '', #168500 ) ;
#205283 = CARTESIAN_POINT ( 'NONE',  ( -23.25000000000000000, 4.150000000011156764, -188.7499999999999716 ) ) ;
#205284 = DIRECTION ( 'NONE',  ( 0.000000000000000000, -0.8660254037844445918, -0.4999999999999897304 ) ) ;
#205285 = CARTESIAN_POINT ( 'NONE',  ( 18.59999999999999076, 10.20857864377385127, -54.85000000000000142 ) ) ;
#205286 = DIRECTION ( 'NONE',  ( 0.000000000000000000, 0.8814952561688429444, -0.4721928772777345684 ) ) ;
#205287 = DIRECTION ( 'NONE',  ( 0.000000000000000000, -1.000000000000000000, 0.000000000000000000 ) ) ;
#205289 = ORIENTED_EDGE ( 'NONE', *, *, #115068, .F. ) ;
#205288 = CARTESIAN_POINT ( 'NONE',  ( -23.15000000000000213, 1.115600667400684642E-11, -134.0000000000000000 ) ) ;
#205290 = DIRECTION ( 'NONE',  ( -1.000000000000000000, 0.000000000000000000, 0.000000000000000000 ) ) ;
#205291 = EDGE_CURVE ( 'NONE', #189565, #255281, #183455, .T. ) ;
#205292 = VERTEX_POINT ( 'NONE', #228941 ) ;
#205293 = DIRECTION ( 'NONE',  ( -1.000000000000000000, 0.000000000000000000, 0.000000000000000000 ) ) ;
#205294 = AXIS2_PLACEMENT_3D ( 'NONE', #1481, #203547, #74960 ) ;
#205295 = FACE_OUTER_BOUND ( 'NONE', #175919, .T. ) ;
#205296 = AXIS2_PLACEMENT_3D ( 'NONE', #172610, #231271, #252090 ) ;
#205297 = DIRECTION ( 'NONE',  ( 0.000000000000000000, 0.9910827722268055195, -0.1332476588733540468 ) ) ;
#205298 = CARTESIAN_POINT ( 'NONE',  ( 22.50000000000000000, 11.64957080755595520, -167.3999999999999773 ) ) ;
#205299 = DIRECTION ( 'NONE',  ( 0.000000000000000000, -0.9908441862701600211, -0.1350103645451876666 ) ) ;
#205300 = EDGE_LOOP ( 'NONE', ( #6882, #223546, #169693, #44173 ) ) ;
#205301 = ADVANCED_FACE ( 'NONE', ( #249783 ), #83459, .T. ) ;
#205302 = CARTESIAN_POINT ( 'NONE',  ( 18.69999999999999929, 7.800000000000000711, -1.212568896937008089 ) ) ;
#205303 = CARTESIAN_POINT ( 'NONE',  ( 21.05000000000000071, 76.00000000001229239, -157.8731074845243540 ) ) ;
#205304 = VERTEX_POINT ( 'NONE', #191120 ) ;
#205305 = CARTESIAN_POINT ( 'NONE',  ( 21.05000000000000071, 75.96798630682469877, -209.7819502080617156 ) ) ;
#205306 = AXIS2_PLACEMENT_3D ( 'NONE', #189536, #74756, #177699 ) ;
#205307 = CARTESIAN_POINT ( 'NONE',  ( 22.60000000000000142, 0.1008583691098682150, -21.75043287651061164 ) ) ;
#205308 = ADVANCED_FACE ( 'NONE', ( #32047 ), #171562, .F. ) ;
#205309 = ORIENTED_EDGE ( 'NONE', *, *, #161975, .T. ) ;
#205310 = CARTESIAN_POINT ( 'NONE',  ( -21.05000000000000071, 6.258842723548713849, -66.96798630681233533 ) ) ;
#205311 = VERTEX_POINT ( 'NONE', #33342 ) ;
#205312 = CARTESIAN_POINT ( 'NONE',  ( -15.75000000000000355, 9.350000000011140955, -50.25000000000000711 ) ) ;
#205313 = ORIENTED_EDGE ( 'NONE', *, *, #137670, .F. ) ;
#205314 = DIRECTION ( 'NONE',  ( 1.000000000000000000, 3.265361837132813093E-16, -0.000000000000000000 ) ) ;
#205315 = CARTESIAN_POINT ( 'NONE',  ( 13.22261339317536866, 9.436552840015581367, -182.6779554727603738 ) ) ;
#205316 = ORIENTED_EDGE ( 'NONE', *, *, #204712, .F. ) ;
#205318 = ORIENTED_EDGE ( 'NONE', *, *, #111451, .T. ) ;
#205317 = B_SPLINE_CURVE_WITH_KNOTS ( 'NONE', 3,
 ( #251079, #110295, #12511, #189841 ),
 .UNSPECIFIED., .F., .F.,
 ( 4, 4 ),
 ( 0.000000000000000000, 7.713889350929433657E-05 ),
 .UNSPECIFIED. ) ;
#205320 = CARTESIAN_POINT ( 'NONE',  ( 22.39999999999999503, 29.54900078958455367, -252.7363208912387051 ) ) ;
#205319 = CIRCLE ( 'NONE', #72267, 0.09999999999999939493 ) ;
#205322 = ORIENTED_EDGE ( 'NONE', *, *, #184609, .T. ) ;
#205321 = CARTESIAN_POINT ( 'NONE',  ( 13.76927104934457269, 9.455987233623899257, -48.51153116689782507 ) ) ;
#205323 = CARTESIAN_POINT ( 'NONE',  ( 21.05000000000000071, 67.22371711014486095, -191.3468923434563465 ) ) ;
#205324 = VERTEX_POINT ( 'NONE', #189816 ) ;
#205325 = AXIS2_PLACEMENT_3D ( 'NONE', #186732, #26362, #657 ) ;
#205326 = EDGE_CURVE ( 'NONE', #255102, #95156, #95942, .T. ) ;
#205327 = AXIS2_PLACEMENT_3D ( 'NONE', #67248, #226299, #100582 ) ;
#205328 = ORIENTED_EDGE ( 'NONE', *, *, #135002, .T. ) ;
#205329 = CARTESIAN_POINT ( 'NONE',  ( 28.12018973533754362, 11.62642356364896123, -347.0000000000001137 ) ) ;
#205330 = DIRECTION ( 'NONE',  ( 0.7071067811865463515, -0.6909108974501249056, -0.1504730267678058564 ) ) ;
#205331 = EDGE_CURVE ( 'NONE', #229007, #214712, #131569, .T. ) ;
#205332 = CARTESIAN_POINT ( 'NONE',  ( -23.15000000000000213, 76.00000000001237765, -170.0231074845243597 ) ) ;
#205333 = DIRECTION ( 'NONE',  ( 1.000000000000000000, 0.000000000000000000, 0.000000000000000000 ) ) ;
#205334 = DIRECTION ( 'NONE',  ( 0.000000000000000000, -0.9908441862701596881, 0.1350103645451904977 ) ) ;
#205335 = LINE ( 'NONE', #184495, #83716 ) ;
#205336 = AXIS2_PLACEMENT_3D ( 'NONE', #93817, #173418, #74298 ) ;
#205338 = ORIENTED_EDGE ( 'NONE', *, *, #50060, .F. ) ;
#205337 = EDGE_CURVE ( 'NONE', #132493, #130829, #116808, .T. ) ;
#205339 = CIRCLE ( 'NONE', #17915, 0.1000000000000028644 ) ;
#205341 = ADVANCED_FACE ( 'NONE', ( #192378 ), #133682, .F. ) ;
#205340 = CARTESIAN_POINT ( 'NONE',  ( -18.50000000000000000, 64.35000000001254250, -182.1731074845244507 ) ) ;
#205342 = FACE_OUTER_BOUND ( 'NONE', #32508, .T. ) ;
#205343 = CARTESIAN_POINT ( 'NONE',  ( 20.94999999999999929, -11.48912529306489994, -131.0000000000000284 ) ) ;
#205344 = AXIS2_PLACEMENT_3D ( 'NONE', #44907, #203966, #222225 ) ;
#205345 = CARTESIAN_POINT ( 'NONE',  ( -18.59999999999999787, 74.83729825007388570, -94.92310748452432279 ) ) ;
#205346 = EDGE_LOOP ( 'NONE', ( #49543, #70777, #252880, #121811 ) ) ;
#205347 = DIRECTION ( 'NONE',  ( -0.000000000000000000, 0.9887567792719327286, 0.1495327102803745423 ) ) ;
#205349 = ADVANCED_FACE ( 'NONE', ( #78821 ), #155838, .T. ) ;
#205348 = VERTEX_POINT ( 'NONE', #80086 ) ;
#205350 = CARTESIAN_POINT ( 'NONE',  ( -20.85000000000000497, 64.25000000001176659, -76.44225473048308572 ) ) ;
#205351 = ORIENTED_EDGE ( 'NONE', *, *, #71368, .F. ) ;
#205352 = CARTESIAN_POINT ( 'NONE',  ( 20.95000000000005258, 65.35000000001120668, -4.423107484524790856 ) ) ;
#205353 = DIRECTION ( 'NONE',  ( -0.000000000000000000, 0.8814952561688430555, -0.4721928772777346239 ) ) ;
#205354 = ADVANCED_FACE ( 'NONE', ( #214495, #60552 ), #177961, .F. ) ;
#205356 = VERTEX_POINT ( 'NONE', #236622 ) ;
#205355 = AXIS2_PLACEMENT_3D ( 'NONE', #145775, #8853, #208356 ) ;
#205357 = EDGE_LOOP ( 'NONE', ( #40594, #118109, #78256, #32198 ) ) ;
#205359 = ORIENTED_EDGE ( 'NONE', *, *, #183129, .F. ) ;
#205358 = DIRECTION ( 'NONE',  ( -0.000000000000000000, 1.000000000000000000, -0.000000000000000000 ) ) ;
#205360 = DIRECTION ( 'NONE',  ( -4.801466763864314121E-15, 0.2605042016806606298, 0.9654727137038736640 ) ) ;
#205361 = EDGE_LOOP ( 'NONE', ( #43233, #207857, #251980, #247560 ) ) ;
#205362 = DIRECTION ( 'NONE',  ( 0.000000000000000000, -1.000000000000000000, 0.000000000000000000 ) ) ;
#205363 = AXIS2_PLACEMENT_3D ( 'NONE', #163515, #243041, #138768 ) ;
#205364 = AXIS2_PLACEMENT_3D ( 'NONE', #242443, #63828, #41709 ) ;
#205365 = CARTESIAN_POINT ( 'NONE',  ( -23.15000000000000213, -4.831324760611774849, -50.46969694219875180 ) ) ;
#205366 = AXIS2_PLACEMENT_3D ( 'NONE', #224763, #220906, #46134 ) ;
#205367 = VERTEX_POINT ( 'NONE', #158418 ) ;
#205368 = CARTESIAN_POINT ( 'NONE',  ( -17.01825945287482966, 10.05000000001113847, -79.65000000000004832 ) ) ;
#205369 = ORIENTED_EDGE ( 'NONE', *, *, #245974, .T. ) ;
#205370 = EDGE_CURVE ( 'NONE', #176716, #16688, #61858, .T. ) ;
#205371 = DIRECTION ( 'NONE',  ( 1.000000000000000000, 0.000000000000000000, 0.000000000000000000 ) ) ;
#205372 = EDGE_CURVE ( 'NONE', #119433, #175127, #115860, .T. ) ;
#205373 = ADVANCED_FACE ( 'NONE', ( #176683 ), #21170, .T. ) ;
#205374 = CARTESIAN_POINT ( 'NONE',  ( -18.40000000000000213, 11.33174054713633261, -54.35000000000000142 ) ) ;
#205376 = ORIENTED_EDGE ( 'NONE', *, *, #66534, .T. ) ;
#205375 = CARTESIAN_POINT ( 'NONE',  ( -16.77683809663752257, 9.945835743215301505, -46.16394901910421567 ) ) ;
#205377 = CARTESIAN_POINT ( 'NONE',  ( 21.05000000000000071, 36.65892442174935439, -249.5511627012433848 ) ) ;
#205378 = DIRECTION ( 'NONE',  ( 0.000000000000000000, 1.000000000000000000, 0.000000000000000000 ) ) ;
#205379 = CARTESIAN_POINT ( 'NONE',  ( -20.94999999999999929, -0.2576658302507160991, -201.0204024091695487 ) ) ;
#205380 = CIRCLE ( 'NONE', #92981, 12.87500000000000355 ) ;
#205382 = CARTESIAN_POINT ( 'NONE',  ( 23.24999999999999645, 71.22429906543236200, -81.37187558857031888 ) ) ;
#205381 = CARTESIAN_POINT ( 'NONE',  ( -18.60000000000000142, -9.523954320741633950, -140.8820170568273795 ) ) ;
#205383 = CARTESIAN_POINT ( 'NONE',  ( 20.95429693346636668, 39.24855018340224433, -236.8380961568129806 ) ) ;
#205384 = CARTESIAN_POINT ( 'NONE',  ( 23.14999999999999858, 1.115600667400684642E-11, -46.37500000000000000 ) ) ;
#205385 = ADVANCED_FACE ( 'NONE', ( #81375 ), #99662, .T. ) ;
#205386 = CARTESIAN_POINT ( 'NONE',  ( -16.86379686415369861, 60.89319167309326275, -221.1156094034376451 ) ) ;
#205387 = DIRECTION ( 'NONE',  ( 0.000000000000000000, -1.000000000000000000, -6.860497997771532351E-15 ) ) ;
#205388 = ORIENTED_EDGE ( 'NONE', *, *, #124211, .F. ) ;
#205389 = CIRCLE ( 'NONE', #142838, 12.87499999999999822 ) ;
#205390 = ORIENTED_EDGE ( 'NONE', *, *, #142129, .F. ) ;
#205392 = DIRECTION ( 'NONE',  ( 0.000000000000000000, 0.2128009952263604232, -0.9770955615653316162 ) ) ;
#205391 = AXIS2_PLACEMENT_3D ( 'NONE', #251625, #234626, #173427 ) ;
#205393 = ORIENTED_EDGE ( 'NONE', *, *, #145340, .T. ) ;
#205394 = CARTESIAN_POINT ( 'NONE',  ( -21.05000000000000071, 64.25000000001220712, -143.5379132551784096 ) ) ;
#205395 = VECTOR ( 'NONE', #212293, 1000.000000000000000 ) ;
#205397 = EDGE_CURVE ( 'NONE', #21107, #245368, #18864, .T. ) ;
#205396 = ORIENTED_EDGE ( 'NONE', *, *, #23485, .T. ) ;
#205398 = VECTOR ( 'NONE', #193513, 1000.000000000000000 ) ;
#205400 = AXIS2_PLACEMENT_3D ( 'NONE', #113985, #174019, #233942 ) ;
#205399 =( NAMED_UNIT ( * ) SI_UNIT ( $, .STERADIAN. ) SOLID_ANGLE_UNIT ( ) );
#205401 = CARTESIAN_POINT ( 'NONE',  ( 20.88420186297724612, 65.66974365629688748, -130.9360145562605169 ) ) ;
#205402 = AXIS2_PLACEMENT_3D ( 'NONE', #196721, #170805, #250286 ) ;
#205403 = DIRECTION ( 'NONE',  ( 1.000000000000000000, -0.000000000000000000, -0.000000000000000000 ) ) ;
#205404 = CIRCLE ( 'NONE', #197604, 1.900000000000002132 ) ;
#205405 = PRODUCT ( 'Injection Molded Chain Links 11', 'Injection Molded Chain Links 11', '', ( #39107 ) ) ;
#205406 = ORIENTED_EDGE ( 'NONE', *, *, #163849, .F. ) ;
#205407 = FACE_BOUND ( 'NONE', #194611, .T. ) ;
#205408 = VERTEX_POINT ( 'NONE', #140083 ) ;
#205409 = VERTEX_POINT ( 'NONE', #218331 ) ;
#205410 = AXIS2_PLACEMENT_3D ( 'NONE', #155663, #138594, #116508 ) ;
#205411 = DIRECTION ( 'NONE',  ( 1.000000000000000000, 0.000000000000000000, 0.000000000000000000 ) ) ;
#205412 = DIRECTION ( 'NONE',  ( -0.000000000000000000, 1.000000000000000000, 6.982962677686266711E-15 ) ) ;
#205414 = ORIENTED_EDGE ( 'NONE', *, *, #171941, .F. ) ;
#205413 = CARTESIAN_POINT ( 'NONE',  ( 21.13461538461538680, 67.11458296203710461, -57.17310748452437963 ) ) ;
#205415 = CARTESIAN_POINT ( 'NONE',  ( 20.00000000000000355, 11.75000000001116263, -158.6500000000000341 ) ) ;
#205417 = VERTEX_POINT ( 'NONE', #571 ) ;
#205416 = CARTESIAN_POINT ( 'NONE',  ( 18.59999999999999076, 68.92903212821255465, -32.27654326265606954 ) ) ;
#205418 = CARTESIAN_POINT ( 'NONE',  ( -22.39999999999999503, 7.790779598373403836, 0.09999999999999939493 ) ) ;
#205419 = DIRECTION ( 'NONE',  ( 0.000000000000000000, 0.000000000000000000, -1.000000000000000000 ) ) ;
#205420 = TOROIDAL_SURFACE ( 'NONE', #109575, 12.97499999999999609, 0.1000000000000000056 ) ;
#205422 = ORIENTED_EDGE ( 'NONE', *, *, #209290, .T. ) ;
#205421 = CARTESIAN_POINT ( 'NONE',  ( -21.14999999999999858, 76.10085836911093793, -148.2726746080136877 ) ) ;
#205423 = CARTESIAN_POINT ( 'NONE',  ( 18.49999999999998934, 6.650000000011155876, -45.85000000000000142 ) ) ;
#205425 = ADVANCED_FACE ( 'NONE', ( #256127 ), #98359, .T. ) ;
#205424 = CARTESIAN_POINT ( 'NONE',  ( -18.53317502108577131, 10.32263460347359540, -72.56059579686720440 ) ) ;
#205426 = DIRECTION ( 'NONE',  ( 0.000000000000000000, -0.9908441862701605762, -0.1350103645451835310 ) ) ;
#205427 = CIRCLE ( 'NONE', #242858, 0.09999999999999939493 ) ;
#205429 = CARTESIAN_POINT ( 'NONE',  ( -21.37071067811865532, 67.92928932189313684, -81.87310748452436826 ) ) ;
#205428 = CARTESIAN_POINT ( 'NONE',  ( -17.11825945287481687, 9.950000000011138823, -121.2500000000000284 ) ) ;
#205431 = ADVANCED_FACE ( 'NONE', ( #41028 ), #117972, .F. ) ;
#205430 = CARTESIAN_POINT ( 'NONE',  ( -23.25000000000000000, -0.09999999999999939493, 11.64957080754479968 ) ) ;
#205432 = DIRECTION ( 'NONE',  ( -0.000000000000000000, -0.000000000000000000, 1.000000000000000000 ) ) ;
#205433 = CARTESIAN_POINT ( 'NONE',  ( 23.14999999999999858, 71.00000000001260503, -191.1178414656112921 ) ) ;
#205434 = CARTESIAN_POINT ( 'NONE',  ( -21.04999999999994387, 66.25000000001119815, -4.623107484524796362 ) ) ;
#205436 = ORIENTED_EDGE ( 'NONE', *, *, #85638, .T. ) ;
#205435 = AXIS2_PLACEMENT_3D ( 'NONE', #240982, #169176, #49188 ) ;
#205437 = EDGE_LOOP ( 'NONE', ( #95070, #41160, #49096, #255413, #107628, #165011 ) ) ;
#205438 = VECTOR ( 'NONE', #173220, 1000.000000000000000 ) ;
#205440 = EDGE_LOOP ( 'NONE', ( #180261, #70026, #76654, #67797 ) ) ;
#205439 = CIRCLE ( 'NONE', #9642, 0.09999999999999939493 ) ;
#205441 = EDGE_CURVE ( 'NONE', #204362, #240802, #100923, .T. ) ;
#205442 = CARTESIAN_POINT ( 'NONE',  ( 21.14999999999998082, -11.74999999998884448, -33.50000000000000000 ) ) ;
#205443 = AXIS2_PLACEMENT_3D ( 'NONE', #180204, #1536, #61532 ) ;
#205444 = ADVANCED_FACE ( 'NONE', ( #95816 ), #37913, .T. ) ;
#205445 = EDGE_LOOP ( 'NONE', ( #216466, #177833, #148226, #179280, #221858 ) ) ;
#205446 = CARTESIAN_POINT ( 'NONE',  ( 20.94999999999999574, 5.900000000011102586, -144.2190997646564483 ) ) ;
#205447 = EDGE_LOOP ( 'NONE', ( #132048, #39266, #63931, #20593 ) ) ;
#205448 = CARTESIAN_POINT ( 'NONE',  ( -21.53699400380730111, 6.787711793201517629, -100.5000000000000426 ) ) ;
#205449 = CARTESIAN_POINT ( 'NONE',  ( 23.14999999999999503, 11.75000000001116263, -121.8500000000000369 ) ) ;
#205450 = ORIENTED_EDGE ( 'NONE', *, *, #57751, .T. ) ;
#205451 = CARTESIAN_POINT ( 'NONE',  ( 15.31784899511109010, 9.396630376328873879, -151.9070573928183592 ) ) ;
#205452 = AXIS2_PLACEMENT_3D ( 'NONE', #145674, #165252, #244773 ) ;
#205453 = AXIS2_PLACEMENT_3D ( 'NONE', #80179, #21543, #222263 ) ;
#205454 = EDGE_LOOP ( 'NONE', ( #208652, #139231, #235674, #142475 ) ) ;
#205455 = EDGE_CURVE ( 'NONE', #6765, #116410, #235338, .T. ) ;
#205457 = VERTEX_POINT ( 'NONE', #116681 ) ;
#205456 = AXIS2_PLACEMENT_3D ( 'NONE', #158594, #135131, #99841 ) ;
#205458 = ADVANCED_FACE ( 'NONE', ( #25317 ), #8320, .F. ) ;
#205459 = ORIENTED_EDGE ( 'NONE', *, *, #184046, .T. ) ;
#205460 = CARTESIAN_POINT ( 'NONE',  ( 23.24999999999999289, 11.75000000000000711, 11.75000000000000000 ) ) ;
#205461 = CARTESIAN_POINT ( 'NONE',  ( 21.05000000000000071, 10.72371710470752149, -7.664913569087605794 ) ) ;
#205462 = CARTESIAN_POINT ( 'NONE',  ( 20.94999999999999574, 2.838478681111047841, -208.5693404029859437 ) ) ;
#205463 = DIRECTION ( 'NONE',  ( 0.000000000000000000, 0.8814952561688429444, -0.4721928772777345684 ) ) ;
#205464 = FACE_OUTER_BOUND ( 'NONE', #66303, .T. ) ;
#205465 = CARTESIAN_POINT ( 'NONE',  ( 13.99999999999999822, 66.15000000001185754, -86.27310748452437394 ) ) ;
#205466 =( BOUNDED_CURVE ( )  B_SPLINE_CURVE ( 3, ( #118271, #179544, #115701, #236924 ),
 .UNSPECIFIED., .F., .F. ) 
 B_SPLINE_CURVE_WITH_KNOTS ( ( 4, 4 ),
 ( 4.937700262165045813E-15, 1.570796326794912323 ),
 .UNSPECIFIED. ) 
 CURVE ( )  GEOMETRIC_REPRESENTATION_ITEM ( )  RATIONAL_B_SPLINE_CURVE ( ( 1.000000000000000000, 0.8047378541243623840, 0.8047378541243623840, 1.000000000000000000 ) ) 
 REPRESENTATION_ITEM ( '' )  );
#205468 = CARTESIAN_POINT ( 'NONE',  ( -20.94999999999999929, 4.639061695946149477, -222.3006832421257286 ) ) ;
#205467 = DIRECTION ( 'NONE',  ( 0.7071067811865492381, 0.3338907855510725997, 0.6233112732207602980 ) ) ;
#205469 = CARTESIAN_POINT ( 'NONE',  ( 21.05000000000000071, 60.85896401437205583, -225.4389122456526025 ) ) ;
#205471 = ORIENTED_EDGE ( 'NONE', *, *, #29398, .F. ) ;
#205470 = LINE ( 'NONE', #245903, #123147 ) ;
#205473 = DIRECTION ( 'NONE',  ( 0.000000000000000000, 0.000000000000000000, 1.000000000000000000 ) ) ;
#205472 = DIRECTION ( 'NONE',  ( 0.000000000000000000, 0.000000000000000000, -1.000000000000000000 ) ) ;
#205474 = CARTESIAN_POINT ( 'NONE',  ( -23.15000000000000213, 74.00000000001205080, -123.7984855617622060 ) ) ;
#205475 = ORIENTED_EDGE ( 'NONE', *, *, #70742, .T. ) ;
#205476 = DIRECTION ( 'NONE',  ( 0.000000000000000000, 0.000000000000000000, -1.000000000000000000 ) ) ;
#205477 = DIRECTION ( 'NONE',  ( -1.000000000000000000, 0.000000000000000000, 0.000000000000000000 ) ) ;
#205478 = CARTESIAN_POINT ( 'NONE',  ( -18.59999999999999787, 19.09764897702175546, -235.7051342141560042 ) ) ;
#205479 = EDGE_LOOP ( 'NONE', ( #37589, #153551, #24125, #137842 ) ) ;
#205480 = ADVANCED_FACE ( 'NONE', ( #22751 ), #87809, .F. ) ;
#205481 = CARTESIAN_POINT ( 'NONE',  ( 23.40000000000005187, 87.60324567546805952, -34.17184040628037422 ) ) ;
#205482 = EDGE_CURVE ( 'NONE', #163086, #54629, #205196, .T. ) ;
#205483 = CARTESIAN_POINT ( 'NONE',  ( 20.12500000000000000, 9.750000000011153745, -108.6117712821143186 ) ) ;
#205484 = LINE ( 'NONE', #128531, #134358 ) ;
#205485 = VERTEX_POINT ( 'NONE', #102218 ) ;
#205486 = EDGE_LOOP ( 'NONE', ( #127755, #232055, #242940, #56392, #252048, #142735, #256350, #219761, #77917, #76202, #46334, #39904, #112427, #137565, #224712, #244049, #227731, #66007, #91038, #189598, #185904, #159699, #113367, #151712, #17137, #119480, #53943 ) ) ;
#205487 = AXIS2_PLACEMENT_3D ( 'NONE', #208815, #109695, #107134 ) ;
#205488 = CARTESIAN_POINT ( 'NONE',  ( -23.15000000000000213, 64.35000000001187459, -90.87310748452438247 ) ) ;
#205489 = VERTEX_POINT ( 'NONE', #65700 ) ;
#205490 = CARTESIAN_POINT ( 'NONE',  ( 19.90000000000000568, 5.586869315528661062, 16.41686199900910736 ) ) ;
#205491 = CARTESIAN_POINT ( 'NONE',  ( -18.44232395689728676, -9.552282557040124189, -174.3422519848069783 ) ) ;
#205492 = CARTESIAN_POINT ( 'NONE',  ( 21.15000000000005542, 64.35000000001120668, -30.12310748452479103 ) ) ;
#205494 = EDGE_CURVE ( 'NONE', #84065, #239961, #183642, .T. ) ;
#205493 = CARTESIAN_POINT ( 'NONE',  ( -18.59999999999999787, 77.25000000001232081, -162.0231074845243313 ) ) ;
#205495 = ORIENTED_EDGE ( 'NONE', *, *, #200362, .T. ) ;
#205496 = CARTESIAN_POINT ( 'NONE',  ( -15.51798037960204368, 9.376659938544690931, -118.1281925482173136 ) ) ;
#205497 = CYLINDRICAL_SURFACE ( 'NONE', #20803, 0.1000000000000028644 ) ;
#205499 = EDGE_CURVE ( 'NONE', #228476, #60596, #212867, .T. ) ;
#205498 = CARTESIAN_POINT ( 'NONE',  ( 20.94999999999999574, 13.71992543034163958, -238.5823796952984992 ) ) ;
#205500 = FACE_OUTER_BOUND ( 'NONE', #206399, .T. ) ;
#205501 = AXIS2_PLACEMENT_3D ( 'NONE', #51342, #171375, #30556 ) ;
#205503 = ORIENTED_EDGE ( 'NONE', *, *, #204565, .F. ) ;
#205502 = AXIS2_PLACEMENT_3D ( 'NONE', #126673, #67981, #87527 ) ;
#205504 = DIRECTION ( 'NONE',  ( 1.000000000000000000, 0.000000000000000000, 0.000000000000000000 ) ) ;
#205505 = AXIS2_PLACEMENT_3D ( 'NONE', #116314, #53752, #236240 ) ;
#205507 = ORIENTED_EDGE ( 'NONE', *, *, #234558, .T. ) ;
#205506 = CARTESIAN_POINT ( 'NONE',  ( -17.11825945287481332, 66.05000000001201954, -115.7731074845243597 ) ) ;
#205508 = DIRECTION ( 'NONE',  ( 0.000000000000000000, -1.000000000000000000, -6.982962677686266711E-15 ) ) ;
#205509 = CARTESIAN_POINT ( 'NONE',  ( 18.39999999999999858, 78.24390740893980478, -231.6169762517609456 ) ) ;
#205510 = EDGE_CURVE ( 'NONE', #238533, #188914, #83635, .T. ) ;
#205511 = CARTESIAN_POINT ( 'NONE',  ( -17.11825945287482753, 65.95000000001206786, -123.7731074845243739 ) ) ;
#205512 = DIRECTION ( 'NONE',  ( 0.000000000000000000, 0.5000000000000078826, -0.8660254037844340447 ) ) ;
#205513 = DIRECTION ( 'NONE',  ( 0.000000000000000000, 0.000000000000000000, -1.000000000000000000 ) ) ;
#205514 = CARTESIAN_POINT ( 'NONE',  ( 23.25000000000000000, -9.000000000000001776, -9.893969122652443104 ) ) ;
#205515 = VERTEX_POINT ( 'NONE', #123119 ) ;
#205516 = CARTESIAN_POINT ( 'NONE',  ( 21.00000000000000000, 12.15477401631902232, -210.9923204818763622 ) ) ;
#205517 = DIRECTION ( 'NONE',  ( 0.000000000000000000, -0.000000000000000000, -1.000000000000000000 ) ) ;
#205518 = LINE ( 'NONE', #209380, #175688 ) ;
#205519 = AXIS2_PLACEMENT_3D ( 'NONE', #226101, #183165, #25385 ) ;
#205521 = CARTESIAN_POINT ( 'NONE',  ( 21.14999999999999858, 76.00000000001186606, -90.87310748452429721 ) ) ;
#205520 = CIRCLE ( 'NONE', #167972, 0.09999999999999939493 ) ;
#205523 = ORIENTED_EDGE ( 'NONE', *, *, #40974, .T. ) ;
#205522 = VECTOR ( 'NONE', #121493, 1000.000000000000000 ) ;
#205524 = VERTEX_POINT ( 'NONE', #3138 ) ;
#205526 = FACE_OUTER_BOUND ( 'NONE', #106224, .T. ) ;
#205525 = CIRCLE ( 'NONE', #1332, 0.5000000000000004441 ) ;
#205527 = PLANE ( 'NONE',  #234691 ) ;
#205528 = DIRECTION ( 'NONE',  ( 1.000000000000000000, 0.000000000000000000, 0.000000000000000000 ) ) ;
#205529 = CARTESIAN_POINT ( 'NONE',  ( 20.85000000000000142, 36.18002604163306302, -236.0784499204090991 ) ) ;
#205530 = CARTESIAN_POINT ( 'NONE',  ( -23.15000000000000213, 73.50000000001180922, -82.74772940728641402 ) ) ;
#205531 = VECTOR ( 'NONE', #92221, 1000.000000000000114 ) ;
#205532 = FACE_BOUND ( 'NONE', #48557, .T. ) ;
#205533 = AXIS2_PLACEMENT_3D ( 'NONE', #64167, #164559, #244073 ) ;
#205534 = LINE ( 'NONE', #208141, #82895 ) ;
#205535 = ORIENTED_EDGE ( 'NONE', *, *, #161959, .F. ) ;
#205536 = CARTESIAN_POINT ( 'NONE',  ( 24.30000000000000071, 3.175288713399624818, -347.0000000000001137 ) ) ;
#205537 = ORIENTED_EDGE ( 'NONE', *, *, #1754, .F. ) ;
#205538 = CARTESIAN_POINT ( 'NONE',  ( -20.64999999999999858, -8.730841121484170131, -157.9019252810156786 ) ) ;
#205539 = CARTESIAN_POINT ( 'NONE',  ( -23.24999999999999645, 77.17949092533254429, -241.9177572069595783 ) ) ;
#205540 = DIRECTION ( 'NONE',  ( 0.000000000000000000, 0.000000000000000000, -1.000000000000000000 ) ) ;
#205542 = CIRCLE ( 'NONE', #247240, 0.09999999999999939493 ) ;
#205541 = CARTESIAN_POINT ( 'NONE',  ( -16.81744102076749314, 9.950000000011142376, -46.15000000000000568 ) ) ;
#205543 = CARTESIAN_POINT ( 'NONE',  ( 20.94999999999999929, 42.15997144203495139, -239.2817429668763793 ) ) ;
#205545 = CARTESIAN_POINT ( 'NONE',  ( -18.60000000000000142, -9.321008403361288330, -7.235938249077881856 ) ) ;
#205544 = AXIS2_PLACEMENT_3D ( 'NONE', #249287, #70667, #232302 ) ;
#205546 = AXIS2_PLACEMENT_3D ( 'NONE', #157515, #237018, #92361 ) ;
#205547 = LINE ( 'NONE', #247244, #147537 ) ;
#205549 = CARTESIAN_POINT ( 'NONE',  ( 22.00411653889210228, 0.09903810579707052197, -93.24655713235962651 ) ) ;
#205548 = CIRCLE ( 'NONE', #151431, 0.9000000000000014655 ) ;
#205550 = CARTESIAN_POINT ( 'NONE',  ( -23.39999999999994529, 82.74366731733570646, -26.36310895752070138 ) ) ;
#205551 = ADVANCED_FACE ( 'NONE', ( #83928 ), #44860, .T. ) ;
#205552 = CARTESIAN_POINT ( 'NONE',  ( -21.05000000000000071, 13.66123737402873495, -238.6633470470287648 ) ) ;
#205553 = FACE_OUTER_BOUND ( 'NONE', #147386, .T. ) ;
#205554 = CARTESIAN_POINT ( 'NONE',  ( 18.39999999999999858, 85.50000000001166711, -62.92291809330220786 ) ) ;
#205555 = CARTESIAN_POINT ( 'NONE',  ( 20.85000000000000142, -1.835859311432481045, -212.5044391687984842 ) ) ;
#205556 = EDGE_LOOP ( 'NONE', ( #13317, #77743, #52991, #148361 ) ) ;
#205557 =( BOUNDED_CURVE ( )  B_SPLINE_CURVE ( 3, ( #235743, #136636, #160091, #196618 ),
 .UNSPECIFIED., .F., .T. ) 
 B_SPLINE_CURVE_WITH_KNOTS ( ( 4, 4 ),
 ( 3.141592653589793116, 4.712388980384689674 ),
 .UNSPECIFIED. ) 
 CURVE ( )  GEOMETRIC_REPRESENTATION_ITEM ( )  RATIONAL_B_SPLINE_CURVE ( ( 1.000000000000000000, 0.8047378541243649375, 0.8047378541243649375, 1.000000000000000000 ) ) 
 REPRESENTATION_ITEM ( '' )  );
#205558 = CARTESIAN_POINT ( 'NONE',  ( -21.44999999999999929, 52.95562111564758823, -234.1965973584252652 ) ) ;
#205559 = CARTESIAN_POINT ( 'NONE',  ( -21.05000000000000071, 76.00000000001213607, -136.5231074845242745 ) ) ;
#205560 = ORIENTED_EDGE ( 'NONE', *, *, #175685, .F. ) ;
#205561 = CARTESIAN_POINT ( 'NONE',  ( -16.91776028072577631, 51.63622145944459163, -231.9240089757377916 ) ) ;
#205562 = CARTESIAN_POINT ( 'NONE',  ( 21.09546886439506608, 11.27926058993681302, -211.0674451492174057 ) ) ;
#205563 = EDGE_CURVE ( 'NONE', #144573, #112792, #140801, .T. ) ;
#205564 = DIRECTION ( 'NONE',  ( 0.000000000000000000, 0.3738317757009345654, 0.9274965247785492695 ) ) ;
#205565 = AXIS2_PLACEMENT_3D ( 'NONE', #251105, #72507, #231575 ) ;
#205566 = EDGE_LOOP ( 'NONE', ( #67472, #61868, #157799, #134805 ) ) ;
#205567 = DIRECTION ( 'NONE',  ( 1.000000000000000000, -0.000000000000000000, -0.000000000000000000 ) ) ;
#205568 = DIRECTION ( 'NONE',  ( 0.000000000000000000, 0.000000000000000000, -1.000000000000000000 ) ) ;
#205569 = TOROIDAL_SURFACE ( 'NONE', #59820, 0.2000000000000000111, 0.1000000000000000056 ) ;
#205571 = ORIENTED_EDGE ( 'NONE', *, *, #8307, .F. ) ;
#205570 = CIRCLE ( 'NONE', #43294, 0.1999999999999987899 ) ;
#205573 = CARTESIAN_POINT ( 'NONE',  ( -22.39999999999999858, 11.75000000001115552, -67.00000000000004263 ) ) ;
#205572 = VECTOR ( 'NONE', #232275, 999.9999999999998863 ) ;
#205574 = EDGE_CURVE ( 'NONE', #243017, #17324, #142650, .T. ) ;
#205575 = AXIS2_PLACEMENT_3D ( 'NONE', #185232, #28775, #245215 ) ;
#205576 = ORIENTED_EDGE ( 'NONE', *, *, #9503, .T. ) ;
#205577 = EDGE_CURVE ( 'NONE', #141902, #39339, #85229, .T. ) ;
#205578 = DIRECTION ( 'NONE',  ( 0.000000000000000000, 0.000000000000000000, 1.000000000000000000 ) ) ;
#205579 = CARTESIAN_POINT ( 'NONE',  ( 18.59999999999999076, 77.14957036958736580, -61.70719500002233815 ) ) ;
#205580 = DIRECTION ( 'NONE',  ( 0.000000000000000000, 6.938893903907222067E-15, -1.000000000000000000 ) ) ;
#205582 = AXIS2_PLACEMENT_3D ( 'NONE', #153314, #232834, #133706 ) ;
#205581 = DIRECTION ( 'NONE',  ( 0.000000000000000000, 0.9126074666063813678, 0.4088369013363182813 ) ) ;
#205583 = EDGE_CURVE ( 'NONE', #206022, #30032, #92039, .T. ) ;
#205584 = CARTESIAN_POINT ( 'NONE',  ( 23.24999999999999645, 8.822561741677553471, -76.25000000000004263 ) ) ;
#205585 = CARTESIAN_POINT ( 'NONE',  ( -16.80621392010918314, 66.05779742250456366, -157.3335155191072374 ) ) ;
#205586 = CARTESIAN_POINT ( 'NONE',  ( 21.05000000000000071, 0.000000000000000000, -33.50000000000000000 ) ) ;
#205587 = AXIS2_PLACEMENT_3D ( 'NONE', #151828, #23879, #43413 ) ;
#205588 = CARTESIAN_POINT ( 'NONE',  ( -5.999999999999938716, 64.35000000001120668, -26.02310748452479316 ) ) ;
#205589 = DIRECTION ( 'NONE',  ( -1.000000000000000000, 0.000000000000000000, -0.000000000000000000 ) ) ;
#205590 = VECTOR ( 'NONE', #118662, 1000.000000000000000 ) ;
#205592 = ORIENTED_EDGE ( 'NONE', *, *, #108514, .T. ) ;
#205591 = CARTESIAN_POINT ( 'NONE',  ( 20.94999999999999574, -11.64999999998883595, -36.50000000000000711 ) ) ;
#205593 = ORIENTED_EDGE ( 'NONE', *, *, #34130, .T. ) ;
#205595 = DIRECTION ( 'NONE',  ( 0.000000000000000000, 0.000000000000000000, 1.000000000000000000 ) ) ;
#205594 = DIRECTION ( 'NONE',  ( 0.000000000000000000, -1.000000000000000000, -6.982962677686266711E-15 ) ) ;
#205596 = ADVANCED_FACE ( 'NONE', ( #223477 ), #175290, .F. ) ;
#205597 = CONICAL_SURFACE ( 'NONE', #93172, 4.299999999999945643, 0.7853981633974466137 ) ;
#205599 = VERTEX_POINT ( 'NONE', #146503 ) ;
#205598 = CARTESIAN_POINT ( 'NONE',  ( 23.14999999999999858, 71.22429906543287359, -158.1743393804784148 ) ) ;
#205600 = VERTEX_POINT ( 'NONE', #91690 ) ;
#205601 = PLANE ( 'NONE',  #170755 ) ;
#205602 = DIRECTION ( 'NONE',  ( 0.000000000000000000, 0.000000000000000000, 1.000000000000000000 ) ) ;
#205603 = AXIS2_PLACEMENT_3D ( 'NONE', #160167, #239679, #61024 ) ;
#205604 = EDGE_CURVE ( 'NONE', #5002, #190272, #132104, .T. ) ;
#205605 = DIRECTION ( 'NONE',  ( 0.000000000000000000, 0.000000000000000000, -1.000000000000000000 ) ) ;
#205606 = CARTESIAN_POINT ( 'NONE',  ( -20.89878130938411616, 10.32747123227773045, -173.0774032850249569 ) ) ;
#205607 = DIRECTION ( 'NONE',  ( 0.000000000000000000, 0.1290532225515392817, 0.9916376685811522096 ) ) ;
#205608 = AXIS2_PLACEMENT_3D ( 'NONE', #251692, #131745, #112210 ) ;
#205609 = CARTESIAN_POINT ( 'NONE',  ( -21.56666275994540172, 76.00000000001219291, -143.4804758914176261 ) ) ;
#205610 = EDGE_CURVE ( 'NONE', #80694, #245081, #46243, .T. ) ;
#205611 = AXIS2_PLACEMENT_3D ( 'NONE', #249978, #128757, #13944 ) ;
#205612 = VERTEX_POINT ( 'NONE', #111260 ) ;
#205613 = EDGE_LOOP ( 'NONE', ( #150442, #92788, #89894, #134513 ) ) ;
#205614 = CARTESIAN_POINT ( 'NONE',  ( 18.39999999999999503, 34.05335961020092839, -234.8258093264404636 ) ) ;
#205615 = EDGE_LOOP ( 'NONE', ( #153368, #95888, #173125, #61447 ) ) ;
#205616 = CARTESIAN_POINT ( 'NONE',  ( 20.94999999999999929, 80.78317333349157536, -192.9003134612048882 ) ) ;
#205617 = EDGE_LOOP ( 'NONE', ( #186851, #4032, #152531, #118138 ) ) ;
#205619 = CIRCLE ( 'NONE', #218093, 0.09999999999998898659 ) ;
#205618 = DIRECTION ( 'NONE',  ( -3.265361837132813586E-16, 0.4721928772777346239, 0.8814952561688430555 ) ) ;
#205620 = AXIS2_PLACEMENT_3D ( 'NONE', #208887, #109776, #130633 ) ;
#205621 = AXIS2_PLACEMENT_3D ( 'NONE', #63139, #123140, #202663 ) ;
#205622 = DIRECTION ( 'NONE',  ( 0.000000000000000000, -0.9651348961777157509, 0.2617529984165031243 ) ) ;
#205623 = CARTESIAN_POINT ( 'NONE',  ( 18.59999999999999432, 0.5876173420563349792, -209.1618981382189588 ) ) ;
#205624 = DIRECTION ( 'NONE',  ( -0.000000000000000000, -0.000000000000000000, -1.000000000000000000 ) ) ;
#205625 = EDGE_LOOP ( 'NONE', ( #218613, #204741, #125529, #216998 ) ) ;
#205626 = CARTESIAN_POINT ( 'NONE',  ( -21.14999999893415250, 11.74999999999999645, -6.844495343526469711 ) ) ;
#205627 = ORIENTED_EDGE ( 'NONE', *, *, #41597, .F. ) ;
#205628 = DIRECTION ( 'NONE',  ( -0.7071067811865475727, 0.6824534298470373850, -0.1850873201762210096 ) ) ;
#205629 = CARTESIAN_POINT ( 'NONE',  ( -18.50000000000000000, 16.44800918141279311, -240.8068063186265135 ) ) ;
#205630 = CARTESIAN_POINT ( 'NONE',  ( -20.94999999999999929, -1.261786168553869603, -142.0864989635454947 ) ) ;
#205631 = CARTESIAN_POINT ( 'NONE',  ( -18.59999999999999787, 64.35000000001190301, -96.00830171387039513 ) ) ;
#205632 = ORIENTED_EDGE ( 'NONE', *, *, #194972, .F. ) ;
#205633 = VECTOR ( 'NONE', #116515, 1000.000000000000000 ) ;
#205634 = ORIENTED_EDGE ( 'NONE', *, *, #44341, .F. ) ;
#205637 = ORIENTED_EDGE ( 'NONE', *, *, #180068, .F. ) ;
#205636 = CARTESIAN_POINT ( 'NONE',  ( 18.50000972452444969, 46.33166059915859591, -243.0555356998358718 ) ) ;
#205635 = DIRECTION ( 'NONE',  ( -1.186688945009010077E-16, 1.000000000000000000, 0.000000000000000000 ) ) ;
#205638 = CIRCLE ( 'NONE', #168297, 11.74999999999999645 ) ;
#205639 = CARTESIAN_POINT ( 'NONE',  ( 21.05000000000000071, 18.81732247075047937, -230.0377732242114632 ) ) ;
#205640 = AXIS2_PLACEMENT_3D ( 'NONE', #13622, #87989, #167580 ) ;
#205641 = ORIENTED_EDGE ( 'NONE', *, *, #217221, .F. ) ;
#205642 = EDGE_CURVE ( 'NONE', #65394, #19933, #192035, .T. ) ;
#205643 = DIRECTION ( 'NONE',  ( 2.952720810173289112E-16, 1.000000000000000000, 6.308085367188367561E-15 ) ) ;
#205644 = VERTEX_POINT ( 'NONE', #227340 ) ;
#205645 = EDGE_CURVE ( 'NONE', #185809, #149671, #17062, .T. ) ;
#205646 = DIRECTION ( 'NONE',  ( 1.000000000000000000, 0.000000000000000000, 0.000000000000000000 ) ) ;
#205647 = EDGE_CURVE ( 'NONE', #250577, #61689, #137822, .T. ) ;
#205648 = DIRECTION ( 'NONE',  ( -1.000000000000000000, 0.000000000000000000, 0.000000000000000000 ) ) ;
#205649 = ADVANCED_FACE ( 'NONE', ( #169991 ), #154446, .T. ) ;
#205650 = CARTESIAN_POINT ( 'NONE',  ( -18.37013991200266005, 54.12739742602126114, -229.1245229108895956 ) ) ;
#205651 = DIRECTION ( 'NONE',  ( 0.000000000000000000, 0.9126074666063844765, 0.4088369013363114535 ) ) ;
#205653 = ORIENTED_EDGE ( 'NONE', *, *, #137353, .F. ) ;
#205652 = EDGE_CURVE ( 'NONE', #168551, #228214, #252043, .T. ) ;
#205654 = CARTESIAN_POINT ( 'NONE',  ( 13.99999999999999822, 26.54497872210689735, -232.9592037335782209 ) ) ;
#205655 = CARTESIAN_POINT ( 'NONE',  ( -16.87683809663752399, 13.90118822005493371, -218.5412211127979845 ) ) ;
#205656 = CARTESIAN_POINT ( 'NONE',  ( -15.75000000000000000, 66.65000000001228386, -153.5015881126992667 ) ) ;
#205657 = EDGE_CURVE ( 'NONE', #201917, #243244, #33052, .T. ) ;
#205658 = ORIENTED_EDGE ( 'NONE', *, *, #91118, .T. ) ;
#205659 = CARTESIAN_POINT ( 'NONE',  ( 21.05000000000005400, 61.72892516158560028, -36.56695479651062186 ) ) ;
#205662 = EDGE_CURVE ( 'NONE', #31578, #32586, #188222, .T. ) ;
#205661 = EDGE_CURVE ( 'NONE', #4716, #236840, #89117, .T. ) ;
#205660 = ORIENTED_EDGE ( 'NONE', *, *, #175032, .T. ) ;
#205663 = DIRECTION ( 'NONE',  ( 0.000000000000000000, 0.3565161741896938907, -0.9342891509276685102 ) ) ;
#205664 = CIRCLE ( 'NONE', #51709, 0.1000000000000054040 ) ;
#205665 = DIRECTION ( 'NONE',  ( 0.000000000000000000, 0.000000000000000000, 1.000000000000000000 ) ) ;
#205666 = DIRECTION ( 'NONE',  ( -2.602085213965226419E-14, -0.000000000000000000, -1.000000000000000000 ) ) ;
#205668 = ORIENTED_EDGE ( 'NONE', *, *, #82790, .F. ) ;
#205667 = CARTESIAN_POINT ( 'NONE',  ( -16.91247567987037570, 9.959082683680401615, -146.6287244585373628 ) ) ;
#205669 = DIRECTION ( 'NONE',  ( 1.000000000000000000, 0.000000000000000000, 0.000000000000000000 ) ) ;
#205670 = DIRECTION ( 'NONE',  ( -1.000000000000000000, -1.116774769942150098E-16, -0.000000000000000000 ) ) ;
#205671 = ADVANCED_FACE ( 'NONE', ( #172566 ), #189518, .T. ) ;
#205672 = LINE ( 'NONE', #27086, #226885 ) ;
#205673 = ORIENTED_EDGE ( 'NONE', *, *, #35846, .T. ) ;
#205674 = LINE ( 'NONE', #109141, #76714 ) ;
#205675 = DIRECTION ( 'NONE',  ( 0.000000000000000000, 0.000000000000000000, -1.000000000000000000 ) ) ;
#205677 = ORIENTED_EDGE ( 'NONE', *, *, #134860, .F. ) ;
#205676 = ADVANCED_FACE ( 'NONE', ( #168713 ), #248200, .T. ) ;
#205680 = ADVANCED_FACE ( 'NONE', ( #228655 ), #130811, .F. ) ;
#205679 = DIRECTION ( 'NONE',  ( 0.000000000000000000, 0.000000000000000000, 1.000000000000000000 ) ) ;
#205678 = AXIS2_PLACEMENT_3D ( 'NONE', #84722, #83449, #164315 ) ;
#205681 = AXIS2_PLACEMENT_3D ( 'NONE', #119984, #125096, #24732 ) ;
#205682 = ORIENTED_EDGE ( 'NONE', *, *, #167061, .T. ) ;
#205683 = AXIS2_PLACEMENT_3D ( 'NONE', #92564, #174738, #33944 ) ;
#205684 = ADVANCED_FACE ( 'NONE', ( #129539 ), #21344, .T. ) ;
#205685 = DIRECTION ( 'NONE',  ( 0.000000000000000000, 0.000000000000000000, -1.000000000000000000 ) ) ;
#205687 = ORIENTED_EDGE ( 'NONE', *, *, #208451, .T. ) ;
#205686 = LINE ( 'NONE', #248681, #138769 ) ;
#205688 = EDGE_CURVE ( 'NONE', #52103, #181022, #171280, .T. ) ;
#205689 = EDGE_CURVE ( 'NONE', #207616, #188655, #73441, .T. ) ;
#205692 = ORIENTED_EDGE ( 'NONE', *, *, #86654, .T. ) ;
#205691 = ORIENTED_EDGE ( 'NONE', *, *, #233408, .F. ) ;
#205690 = CARTESIAN_POINT ( 'NONE',  ( -5.899999999999938183, 64.65000000001120384, -25.92310748452479174 ) ) ;
#205693 = FACE_OUTER_BOUND ( 'NONE', #158547, .T. ) ;
#205694 = PLANE ( 'NONE',  #194025 ) ;
#205695 = CARTESIAN_POINT ( 'NONE',  ( -20.54999999999999716, -11.74999999998884626, -112.8500000000000369 ) ) ;
#205696 = AXIS2_PLACEMENT_3D ( 'NONE', #214560, #137579, #17642 ) ;
#205698 = CARTESIAN_POINT ( 'NONE',  ( -20.64999999999999858, 2.000000000011154189, -113.7246219227621395 ) ) ;
#205697 = CARTESIAN_POINT ( 'NONE',  ( -18.59999999999999787, 52.13794731297493712, -232.3713824252124880 ) ) ;
#205699 = CARTESIAN_POINT ( 'NONE',  ( -20.54999999999999716, 69.05648948627111849, -235.0374527038057977 ) ) ;
#205700 = CARTESIAN_POINT ( 'NONE',  ( -22.94999999999999929, 4.513204987021263825, 22.10000000000000142 ) ) ;
#205701 = CARTESIAN_POINT ( 'NONE',  ( -16.94107738177415357, 65.98576071487495653, -56.97310748452440521 ) ) ;
#205702 = AXIS2_PLACEMENT_3D ( 'NONE', #114436, #250098, #230540 ) ;
#205703 = CARTESIAN_POINT ( 'NONE',  ( 18.59999999999997655, 76.00000000001142553, -36.02310748452432421 ) ) ;
#205704 = CARTESIAN_POINT ( 'NONE',  ( -22.50047199487877947, 75.95509394809208459, -148.2731549034355112 ) ) ;
#205705 = VECTOR ( 'NONE', #24461, 1000.000000000000000 ) ;
#205706 = EDGE_LOOP ( 'NONE', ( #18428, #178785, #133504, #172741 ) ) ;
#205707 = ORIENTED_EDGE ( 'NONE', *, *, #157507, .T. ) ;
#205708 = VECTOR ( 'NONE', #41503, 1000.000000000000114 ) ;
#205709 = DIRECTION ( 'NONE',  ( 0.000000000000000000, 1.000000000000000000, 6.982962677686266711E-15 ) ) ;
#205711 = ORIENTED_EDGE ( 'NONE', *, *, #217306, .T. ) ;
#205710 = DIRECTION ( 'NONE',  ( 1.186688945009010077E-16, -1.000000000000000000, -0.000000000000000000 ) ) ;
#205712 = ORIENTED_EDGE ( 'NONE', *, *, #83148, .F. ) ;
#205713 = DIRECTION ( 'NONE',  ( 0.000000000000000000, 0.000000000000000000, -1.000000000000000000 ) ) ;
#205714 = ORIENTED_EDGE ( 'NONE', *, *, #197103, .F. ) ;
#205715 = CARTESIAN_POINT ( 'NONE',  ( 20.85000000000000142, 7.225717546301074989, -233.4207493275448257 ) ) ;
#205716 = VECTOR ( 'NONE', #166362, 1000.000000000000000 ) ;
#205717 = AXIS2_PLACEMENT_3D ( 'NONE', #100165, #138020, #1069 ) ;
#205718 = ORIENTED_EDGE ( 'NONE', *, *, #230827, .F. ) ;
#205719 = AXIS2_PLACEMENT_3D ( 'NONE', #212670, #78266, #155287 ) ;
#205720 = CARTESIAN_POINT ( 'NONE',  ( 21.30000000000002558, 1.115600667400684642E-11, -100.5000000000000284 ) ) ;
#205721 = CARTESIAN_POINT ( 'NONE',  ( -18.39999999999999858, -9.682403433465239573, -174.1568433774127982 ) ) ;
#205722 = CIRCLE ( 'NONE', #64089, 4.149999999999996803 ) ;
#205724 = ORIENTED_EDGE ( 'NONE', *, *, #69772, .T. ) ;
#205723 = ORIENTED_EDGE ( 'NONE', *, *, #162852, .T. ) ;
#205725 = ORIENTED_EDGE ( 'NONE', *, *, #231016, .F. ) ;
#205726 = DIRECTION ( 'NONE',  ( 0.000000000000000000, 6.982962677686266711E-15, -1.000000000000000000 ) ) ;
#205727 = ORIENTED_EDGE ( 'NONE', *, *, #95693, .F. ) ;
#205728 = ORIENTED_EDGE ( 'NONE', *, *, #84445, .T. ) ;
#205730 = CARTESIAN_POINT ( 'NONE',  ( 20.94999999999999929, 4.850467289719620823, -21.46573259099832498 ) ) ;
#205729 = AXIS2_PLACEMENT_3D ( 'NONE', #46068, #143883, #142587 ) ;
#205731 = CARTESIAN_POINT ( 'NONE',  ( 18.60000000000000142, -9.523946312306550865, -73.88202799533824816 ) ) ;
#205733 = ORIENTED_EDGE ( 'NONE', *, *, #10899, .F. ) ;
#205732 = CARTESIAN_POINT ( 'NONE',  ( 20.94999999999999929, 1.835341550235569663, -145.5551512925629822 ) ) ;
#205734 = CARTESIAN_POINT ( 'NONE',  ( 20.85000000000000142, -11.74999999998883560, -164.5000000000000000 ) ) ;
#205735 = CARTESIAN_POINT ( 'NONE',  ( -20.90000000000000213, 1.885425182446133885, -11.49641995933507843 ) ) ;
#205737 = ORIENTED_EDGE ( 'NONE', *, *, #99045, .F. ) ;
#205736 = CARTESIAN_POINT ( 'NONE',  ( -20.54999999999999716, 85.00000000001261924, -193.6291383618718385 ) ) ;
#205738 = DIRECTION ( 'NONE',  ( 1.000000000000000000, 3.265361837132813093E-16, -0.000000000000000000 ) ) ;
#205739 = VERTEX_POINT ( 'NONE', #68284 ) ;
#205740 = CIRCLE ( 'NONE', #93311, 7.899999999999990585 ) ;
#205741 = DIRECTION ( 'NONE',  ( 0.000000000000000000, -0.7397360091702744889, 0.6728971962616842051 ) ) ;
#205742 = AXIS2_PLACEMENT_3D ( 'NONE', #172311, #251792, #230973 ) ;
#205743 = EDGE_LOOP ( 'NONE', ( #43446, #16740, #53099, #36312 ) ) ;
#205744 = AXIS2_PLACEMENT_3D ( 'NONE', #53214, #228002, #171917 ) ;
#205746 = ADVANCED_FACE ( 'NONE', ( #212924 ), #19874, .F. ) ;
#205745 = CYLINDRICAL_SURFACE ( 'NONE', #257936, 0.1000000000000028644 ) ;
#205747 = EDGE_LOOP ( 'NONE', ( #239373, #118372, #244085, #198909 ) ) ;
#205749 = DIRECTION ( 'NONE',  ( 0.000000000000000000, -0.2128009952263625604, 0.9770955615653310611 ) ) ;
#205748 = DIRECTION ( 'NONE',  ( 0.000000000000000000, -1.000000000000000000, -6.982962677686266711E-15 ) ) ;
#205750 = EDGE_CURVE ( 'NONE', #107596, #232238, #60255, .T. ) ;
#205751 = DIRECTION ( 'NONE',  ( 1.000000000000000000, 0.000000000000000000, -0.000000000000000000 ) ) ;
#205752 = DIRECTION ( 'NONE',  ( -3.265361837132813093E-16, -1.000000000000000000, -7.086529944415894657E-15 ) ) ;
#205753 = VERTEX_POINT ( 'NONE', #75980 ) ;
#205754 = ORIENTED_EDGE ( 'NONE', *, *, #237014, .F. ) ;
#205755 = ADVANCED_FACE ( 'NONE', ( #176386 ), #255849, .F. ) ;
#205756 = CARTESIAN_POINT ( 'NONE',  ( 18.59999999999996945, 7.021664781911246322, -137.8335654018973457 ) ) ;
#205758 = ADVANCED_FACE ( 'NONE', ( #77248 ), #108620, .F. ) ;
#205757 = DIRECTION ( 'NONE',  ( 0.000000000000000000, 0.8068669527897506244, 0.5907332058516622242 ) ) ;
#205759 = ORIENTED_EDGE ( 'NONE', *, *, #182163, .F. ) ;
#205760 = FACE_OUTER_BOUND ( 'NONE', #214439, .T. ) ;
#205761 = VERTEX_POINT ( 'NONE', #238910 ) ;
#205762 = DIRECTION ( 'NONE',  ( -0.000000000000000000, 0.2617529984165031243, 0.9651348961777157509 ) ) ;
#205763 = VERTEX_POINT ( 'NONE', #156832 ) ;
#205764 = CARTESIAN_POINT ( 'NONE',  ( 23.24999999999999289, 11.65000000001116298, -55.25000000000004974 ) ) ;
#205765 = CARTESIAN_POINT ( 'NONE',  ( -20.94999999999999929, 64.35000000001147669, -42.80697314750250371 ) ) ;
#205766 = CARTESIAN_POINT ( 'NONE',  ( -23.25000000000000355, 62.96304356361481780, -213.1979597767049484 ) ) ;
#205767 = AXIS2_PLACEMENT_3D ( 'NONE', #193296, #55031, #155483 ) ;
#205768 = CIRCLE ( 'NONE', #14259, 4.000000000000006217 ) ;
#205769 = ORIENTED_EDGE ( 'NONE', *, *, #107044, .T. ) ;
#205770 = CARTESIAN_POINT ( 'NONE',  ( 18.59999996954842771, -9.523204137847535833, -207.8830417119165759 ) ) ;
#205771 = AXIS2_PLACEMENT_3D ( 'NONE', #208189, #127352, #8689 ) ;
#205772 = ADVANCED_FACE ( 'NONE', ( #134641 ), #199800, .F. ) ;
#205773 = VERTEX_POINT ( 'NONE', #236333 ) ;
#205774 = ORIENTED_EDGE ( 'NONE', *, *, #11778, .F. ) ;
#205775 = EDGE_CURVE ( 'NONE', #144437, #133820, #96129, .T. ) ;
#205776 = ORIENTED_EDGE ( 'NONE', *, *, #69585, .T. ) ;
#205777 = AXIS2_PLACEMENT_3D ( 'NONE', #204661, #165568, #2611 ) ;
#205778 = DIRECTION ( 'NONE',  ( 1.000000000000000000, 0.000000000000000000, 0.000000000000000000 ) ) ;
#205779 = DIRECTION ( 'NONE',  ( 1.000000000000000000, -0.000000000000000000, 0.000000000000000000 ) ) ;
#205780 = AXIS2_PLACEMENT_3D ( 'NONE', #105343, #88360, #87081 ) ;
#205781 = CARTESIAN_POINT ( 'NONE',  ( -20.54999999999999716, -8.663551401858004652, -177.0241011180672785 ) ) ;
#205782 = DIRECTION ( 'NONE',  ( -0.000000000000000000, -0.000000000000000000, 1.000000000000000000 ) ) ;
#205783 = CARTESIAN_POINT ( 'NONE',  ( 20.94999999999999574, 74.73821383144705521, -128.4366085209788366 ) ) ;
#205785 = CARTESIAN_POINT ( 'NONE',  ( 21.72449340488910252, 12.74034062369345399, -211.1718227230884963 ) ) ;
#205784 = DIRECTION ( 'NONE',  ( -4.408576920032447972E-17, -0.1350103645451946055, 0.9908441862701591329 ) ) ;
#205787 = VERTEX_POINT ( 'NONE', #137231 ) ;
#205786 = CARTESIAN_POINT ( 'NONE',  ( -21.04999999999999716, 61.00622636567305079, -234.0632267055443378 ) ) ;
#205788 = CARTESIAN_POINT ( 'NONE',  ( -21.09107601085566586, 6.363877975370981765, -167.4606928352826003 ) ) ;
#205789 = ORIENTED_EDGE ( 'NONE', *, *, #239238, .F. ) ;
#205790 = VECTOR ( 'NONE', #127294, 1000.000000000000000 ) ;
#205791 = CARTESIAN_POINT ( 'NONE',  ( -18.59999999999999787, 11.75000000001115552, -121.7500000000000426 ) ) ;
#205792 = ORIENTED_EDGE ( 'NONE', *, *, #58888, .T. ) ;
#205793 = EDGE_LOOP ( 'NONE', ( #40563, #94949, #162463, #42215, #253334 ) ) ;
#205794 = DIRECTION ( 'NONE',  ( -1.000000000000000000, -0.000000000000000000, -0.000000000000000000 ) ) ;
#205795 = AXIS2_PLACEMENT_3D ( 'NONE', #242440, #63826, #183771 ) ;
#205796 = DIRECTION ( 'NONE',  ( 0.000000000000000000, 0.9371753822965315228, -0.3488585713686134238 ) ) ;
#205797 = CARTESIAN_POINT ( 'NONE',  ( -21.05000000000000071, 75.90220970870393558, -209.7809220950004772 ) ) ;
#205798 = EDGE_CURVE ( 'NONE', #226069, #152713, #46899, .T. ) ;
#205799 = CIRCLE ( 'NONE', #1768, 3.900000000000000799 ) ;
#205800 = EDGE_CURVE ( 'NONE', #221637, #254141, #118970, .T. ) ;
#205801 = TOROIDAL_SURFACE ( 'NONE', #135042, 0.6000000000000015321, 0.1000000000000000056 ) ;
#205802 = DIRECTION ( 'NONE',  ( 1.000000000000000000, 0.000000000000000000, 0.000000000000000000 ) ) ;
#205803 = ORIENTED_EDGE ( 'NONE', *, *, #115170, .F. ) ;
#205804 = ORIENTED_EDGE ( 'NONE', *, *, #139725, .T. ) ;
#205805 = CARTESIAN_POINT ( 'NONE',  ( 21.05000000000000071, 70.15000000001148805, -46.15560470880229360 ) ) ;
#205806 = VERTEX_POINT ( 'NONE', #95536 ) ;
#205807 = CARTESIAN_POINT ( 'NONE',  ( -18.59999999999999787, 70.47363787294415260, -228.3418745167492432 ) ) ;
#205808 = CARTESIAN_POINT ( 'NONE',  ( -20.94999999999994245, 67.75000000001118394, -3.023107484524792277 ) ) ;
#205809 = CARTESIAN_POINT ( 'NONE',  ( -18.50000000000000000, 9.350000000011156942, -79.35000000000005116 ) ) ;
#205811 = AXIS2_PLACEMENT_3D ( 'NONE', #77530, #237912, #55390 ) ;
#205810 = FACE_OUTER_BOUND ( 'NONE', #229953, .T. ) ;
#205812 = CARTESIAN_POINT ( 'NONE',  ( 21.05000000000000071, 87.65000000001172964, -72.52310748452423184 ) ) ;
#205814 = EDGE_CURVE ( 'NONE', #136758, #98196, #180205, .T. ) ;
#205813 = CARTESIAN_POINT ( 'NONE',  ( 21.05000000000000071, 87.75000000001234923, -167.1231074845242688 ) ) ;
#205815 = ORIENTED_EDGE ( 'NONE', *, *, #36357, .T. ) ;
#205816 = DIRECTION ( 'NONE',  ( 0.000000000000000000, 0.000000000000000000, 1.000000000000000000 ) ) ;
#205817 = DIRECTION ( 'NONE',  ( 1.000000000000000000, 0.000000000000000000, 0.000000000000000000 ) ) ;
#205818 = CARTESIAN_POINT ( 'NONE',  ( 21.05000000000000071, -8.663551401858002876, -43.02410111806730697 ) ) ;
#205819 = EDGE_CURVE ( 'NONE', #183504, #158368, #135932, .T. ) ;
#205820 = CARTESIAN_POINT ( 'NONE',  ( -18.40000000000000213, 11.48667500176882861, -91.25000000000005684 ) ) ;
#205821 = CIRCLE ( 'NONE', #47576, 0.09999999999999939493 ) ;
#205822 = CARTESIAN_POINT ( 'NONE',  ( 22.39999999999999503, 64.25000000001269029, -203.6231074845244393 ) ) ;
#205823 = EDGE_CURVE ( 'NONE', #5646, #119280, #216764, .T. ) ;
#205824 = DIRECTION ( 'NONE',  ( -0.000000000000000000, -0.9126074666063770380, -0.4088369013363281068 ) ) ;
#205825 = AXIS2_PLACEMENT_3D ( 'NONE', #63978, #123961, #183923 ) ;
#205826 = AXIS2_PLACEMENT_3D ( 'NONE', #70693, #189335, #69397 ) ;
#205827 = ORIENTED_EDGE ( 'NONE', *, *, #45244, .F. ) ;
#205828 = AXIS2_PLACEMENT_3D ( 'NONE', #153008, #149136, #232533 ) ;
#205829 = CARTESIAN_POINT ( 'NONE',  ( -21.46681500593010838, 69.14248884062493516, -136.5231074845243597 ) ) ;
#205830 = EDGE_LOOP ( 'NONE', ( #124, #168662, #242703, #41978 ) ) ;
#205831 = APPLICATION_CONTEXT ( 'automotive_design' ) ;
#205832 = EDGE_CURVE ( 'NONE', #76104, #235005, #56395, .T. ) ;
#205833 = DIRECTION ( 'NONE',  ( 0.000000000000000000, 0.000000000000000000, 1.000000000000000000 ) ) ;
#205834 = CARTESIAN_POINT ( 'NONE',  ( -22.19999999999999929, -11.65000000000000036, 32.89999999999999858 ) ) ;
#205835 = DIRECTION ( 'NONE',  ( -0.000000000000000000, 0.000000000000000000, -1.000000000000000000 ) ) ;
#205836 = DIRECTION ( 'NONE',  ( 0.000000000000000000, -1.000000000000000000, -5.551115123125768187E-14 ) ) ;
#205837 = ORIENTED_EDGE ( 'NONE', *, *, #255895, .F. ) ;
#205838 = PLANE ( 'NONE',  #246663 ) ;
#205839 = ADVANCED_FACE ( 'NONE', ( #36891 ), #218029, .T. ) ;
#205840 = CARTESIAN_POINT ( 'NONE',  ( -18.50000000000000000, 30.18746141061095045, -235.4776000216846796 ) ) ;
#205841 = SURFACE_SIDE_STYLE ('',( #65043 ) ) ;
#205842 = CARTESIAN_POINT ( 'NONE',  ( -20.85000000000000142, 77.83585931145600512, -158.5186683157258187 ) ) ;
#205844 = DIRECTION ( 'NONE',  ( 1.000000000000000000, 0.000000000000000000, 0.000000000000000000 ) ) ;
#205843 = AXIS2_PLACEMENT_3D ( 'NONE', #211520, #245516, #32925 ) ;
#205845 = CARTESIAN_POINT ( 'NONE',  ( 22.49806830649814060, 75.92253568368695937, -181.6729971393634457 ) ) ;
#205846 = ORIENTED_EDGE ( 'NONE', *, *, #228412, .T. ) ;
#205847 = ORIENTED_EDGE ( 'NONE', *, *, #164570, .T. ) ;
#205848 = DIRECTION ( 'NONE',  ( -1.000000000000000000, -3.265361837132813093E-16, 0.000000000000000000 ) ) ;
#205850 = ORIENTED_EDGE ( 'NONE', *, *, #204603, .F. ) ;
#205849 = CARTESIAN_POINT ( 'NONE',  ( 23.14999999999999858, 76.00000000001139711, -32.02310748452432421 ) ) ;
#205851 = LINE ( 'NONE', #243694, #142510 ) ;
#205852 = CYLINDRICAL_SURFACE ( 'NONE', #74563, 11.74999999999999645 ) ;
#205853 = ORIENTED_EDGE ( 'NONE', *, *, #139782, .F. ) ;
#205854 = DIRECTION ( 'NONE',  ( 0.000000000000000000, 0.4999999999999088507, -0.8660254037844913322 ) ) ;
#205855 = CONTEXT_DEPENDENT_SHAPE_REPRESENTATION ( #29203, #178762 ) ;
#205856 = DIRECTION ( 'NONE',  ( 0.000000000000000000, -2.168404344970946706E-14, -1.000000000000000000 ) ) ;
#205857 = ORIENTED_EDGE ( 'NONE', *, *, #71657, .F. ) ;
#205858 = CARTESIAN_POINT ( 'NONE',  ( 18.59999999999999787, -8.250000000000005329, 10.52591260281975138 ) ) ;
#205859 = AXIS2_PLACEMENT_3D ( 'NONE', #252744, #195379, #96239 ) ;
#205860 = ORIENTED_EDGE ( 'NONE', *, *, #115048, .F. ) ;
#205861 = ORIENTED_EDGE ( 'NONE', *, *, #124749, .T. ) ;
#205862 = CARTESIAN_POINT ( 'NONE',  ( 23.14999999999999503, 11.75000000001116263, -45.65000000000000568 ) ) ;
#205863 = CARTESIAN_POINT ( 'NONE',  ( 21.14999999999999858, 10.71339244339988461, -12.35000000000000142 ) ) ;
#205864 = DIRECTION ( 'NONE',  ( 1.000000000000000000, 0.000000000000000000, 0.000000000000000000 ) ) ;
#205865 = CARTESIAN_POINT ( 'NONE',  ( 20.73486653747088582, 68.75000000001149658, -48.67310748452437963 ) ) ;
#205866 = DIRECTION ( 'NONE',  ( 0.000000000000000000, 0.000000000000000000, -1.000000000000000000 ) ) ;
#205867 = DIRECTION ( 'NONE',  ( 1.000000000000000000, 0.000000000000000000, 0.000000000000000000 ) ) ;
#205868 = CARTESIAN_POINT ( 'NONE',  ( 21.05000000000000071, 7.128833340094563376, -233.7327013124401276 ) ) ;
#205870 = CARTESIAN_POINT ( 'NONE',  ( 19.58285714285715073, 10.60044124276980959, -207.3093812031132472 ) ) ;
#205869 = CARTESIAN_POINT ( 'NONE',  ( 22.47007471830798409, 7.720710651926455448, -9.757819552369539906E-16 ) ) ;
#205871 = DIRECTION ( 'NONE',  ( -0.000000000000000000, -1.000000000000000000, -0.000000000000000000 ) ) ;
#205872 = CARTESIAN_POINT ( 'NONE',  ( 22.42196299218230493, 0.002441673998456600492, -155.8503882973504915 ) ) ;
#205874 = CARTESIAN_POINT ( 'NONE',  ( -21.14999999999999858, 1.115600667400684642E-11, -55.35042919245524473 ) ) ;
#205873 = AXIS2_PLACEMENT_3D ( 'NONE', #61025, #101393, #119749 ) ;
#205875 = ORIENTED_EDGE ( 'NONE', *, *, #66151, .T. ) ;
#205876 = CIRCLE ( 'NONE', #89167, 4.099999999999992539 ) ;
#205877 = ORIENTED_EDGE ( 'NONE', *, *, #95977, .F. ) ;
#205878 = DIRECTION ( 'NONE',  ( 2.775557561562881759E-13, 0.8825714802517645730, -0.4701782451860243017 ) ) ;
#205879 = DIRECTION ( 'NONE',  ( -1.000000000000000000, 3.265361837132813093E-16, 2.280189983783949500E-30 ) ) ;
#205882 = CARTESIAN_POINT ( 'NONE',  ( -15.15564720441981095, 13.04030727965138503, -216.6527351471937664 ) ) ;
#205881 = DIRECTION ( 'NONE',  ( -0.000000000000000000, 0.4088369013363281068, -0.9126074666063770380 ) ) ;
#205880 = CIRCLE ( 'NONE', #235120, 11.90000000000001101 ) ;
#205883 = VECTOR ( 'NONE', #55633, 1000.000000000000000 ) ;
#205884 = CARTESIAN_POINT ( 'NONE',  ( 18.59999999999999076, 66.47189219944506533, -213.6315278230738102 ) ) ;
#205885 = CARTESIAN_POINT ( 'NONE',  ( -21.05000000000000071, 77.83534155023598089, -57.96795619196132776 ) ) ;
#205887 = EDGE_CURVE ( 'NONE', #144175, #130629, #159382, .T. ) ;
#205886 = DIRECTION ( 'NONE',  ( 0.000000000000000000, 0.000000000000000000, -1.000000000000000000 ) ) ;
#205888 = EDGE_LOOP ( 'NONE', ( #38485, #108702, #171783, #165008, #229762 ) ) ;
#205889 = ORIENTED_EDGE ( 'NONE', *, *, #174921, .T. ) ;
#205890 = EDGE_CURVE ( 'NONE', #182680, #8100, #116400, .T. ) ;
#205891 = EDGE_CURVE ( 'NONE', #153125, #250378, #230077, .T. ) ;
#205892 = CARTESIAN_POINT ( 'NONE',  ( 21.87500000000000355, 66.25000000001155342, -57.17310748452438673 ) ) ;
#205893 = VERTEX_POINT ( 'NONE', #241476 ) ;
#205894 = CARTESIAN_POINT ( 'NONE',  ( -20.94999999999999929, 1.360870587203197646, -75.07299792709100927 ) ) ;
#205895 = CIRCLE ( 'NONE', #93455, 0.1999999999999987899 ) ;
#205896 = B_SPLINE_CURVE_WITH_KNOTS ( 'NONE', 3,
 ( #121262, #66382, #219023, #41698 ),
 .UNSPECIFIED., .F., .F.,
 ( 4, 4 ),
 ( 0.000000000000000000, 0.001767853679387143117 ),
 .UNSPECIFIED. ) ;
#205898 = DIRECTION ( 'NONE',  ( -0.7071067811865487940, -0.2890913453342125461, 0.6453109281988438362 ) ) ;
#205897 = AXIS2_PLACEMENT_3D ( 'NONE', #49785, #141494, #87610 ) ;
#205899 = ORIENTED_EDGE ( 'NONE', *, *, #220573, .T. ) ;
#205900 = FACE_OUTER_BOUND ( 'NONE', #187607, .T. ) ;
#205901 = EDGE_CURVE ( 'NONE', #88951, #39669, #67765, .T. ) ;
#205902 = ORIENTED_EDGE ( 'NONE', *, *, #243834, .T. ) ;
#205903 = CARTESIAN_POINT ( 'NONE',  ( 21.30000000000002558, 76.00000000001267608, -203.5231074845243597 ) ) ;
#205904 = FACE_OUTER_BOUND ( 'NONE', #139901, .T. ) ;
#205905 = FACE_OUTER_BOUND ( 'NONE', #22029, .T. ) ;
#205906 = AXIS2_PLACEMENT_3D ( 'NONE', #79739, #75917, #159325 ) ;
#205908 = DIRECTION ( 'NONE',  ( -0.000000000000000000, 0.9651348961777155289, -0.2617529984165036794 ) ) ;
#205907 = CIRCLE ( 'NONE', #185063, 0.1000000000000055844 ) ;
#205909 = CARTESIAN_POINT ( 'NONE',  ( -18.59999999999999787, 74.16465844978819177, -191.9679561919613775 ) ) ;
#205911 = TOROIDAL_SURFACE ( 'NONE', #110057, 4.150000000000000355, 0.1000000000000000056 ) ;
#205910 = DIRECTION ( 'NONE',  ( -1.000000000000000000, -0.000000000000000000, -0.000000000000000000 ) ) ;
#205912 = PLANE ( 'NONE',  #201018 ) ;
#205913 = CARTESIAN_POINT ( 'NONE',  ( -18.50000000000000355, 7.576017155224048061, -241.7224044826512284 ) ) ;
#205915 = ORIENTED_EDGE ( 'NONE', *, *, #53963, .F. ) ;
#205914 = DIRECTION ( 'NONE',  ( -0.000000000000000000, -6.982962677686266711E-15, 1.000000000000000000 ) ) ;
#205917 = CARTESIAN_POINT ( 'NONE',  ( -21.44999999999999929, 7.150000000011155876, -88.25000000000005684 ) ) ;
#205916 = DIRECTION ( 'NONE',  ( 0.000000000000000000, -6.982962677686266711E-15, 1.000000000000000000 ) ) ;
#205918 = CIRCLE ( 'NONE', #105941, 0.1000000000000000472 ) ;
#205919 = ORIENTED_EDGE ( 'NONE', *, *, #9143, .F. ) ;
#205921 = ORIENTED_EDGE ( 'NONE', *, *, #134033, .F. ) ;
#205920 = FACE_OUTER_BOUND ( 'NONE', #31546, .T. ) ;
#205922 = ORIENTED_EDGE ( 'NONE', *, *, #47963, .T. ) ;
#205923 = DIRECTION ( 'NONE',  ( -0.4999999999999799050, -6.047423072554995242E-15, 0.8660254037844502539 ) ) ;
#205924 = CARTESIAN_POINT ( 'NONE',  ( -20.64999999999999858, 85.00000000001197975, -112.5170766071766764 ) ) ;
#205925 = AXIS2_PLACEMENT_3D ( 'NONE', #143108, #126110, #222642 ) ;
#205926 = EDGE_CURVE ( 'NONE', #81259, #87080, #117649, .T. ) ;
#205928 = EDGE_CURVE ( 'NONE', #136482, #56290, #96944, .T. ) ;
#205927 = CARTESIAN_POINT ( 'NONE',  ( 21.05000000000000071, -0.08559286335101129461, -127.5863372651308225 ) ) ;
#205929 = DIRECTION ( 'NONE',  ( 0.000000000000000000, 0.1495327102803689356, -0.9887567792719336168 ) ) ;
#205930 = LINE ( 'NONE', #248927, #194017 ) ;
#205931 = AXIS2_PLACEMENT_3D ( 'NONE', #114585, #235800, #191587 ) ;
#205932 = DIRECTION ( 'NONE',  ( 1.000000000000000000, 0.000000000000000000, 0.000000000000000000 ) ) ;
#205933 = CIRCLE ( 'NONE', #210048, 11.74999999999999822 ) ;
#205934 = PLANE ( 'NONE',  #8806 ) ;
#205935 = CARTESIAN_POINT ( 'NONE',  ( -23.25000000000000355, 11.74999999999998224, -9.250000000000001776 ) ) ;
#205936 = CIRCLE ( 'NONE', #164261, 0.1999999999999987899 ) ;
#205937 = EDGE_CURVE ( 'NONE', #86338, #43174, #1093, .T. ) ;
#205938 = DIRECTION ( 'NONE',  ( 0.000000000000000000, 0.000000000000000000, -1.000000000000000000 ) ) ;
#205939 = VERTEX_POINT ( 'NONE', #4135 ) ;
#205940 = ORIENTED_EDGE ( 'NONE', *, *, #81642, .T. ) ;
#205941 = CYLINDRICAL_SURFACE ( 'NONE', #110374, 0.1000000000000001305 ) ;
#205942 = B_SPLINE_CURVE_WITH_KNOTS ( 'NONE', 3,
 ( #179054, #117754, #120366, #239000, #19962, #159461, #42100, #221962, #121637, #257217, #198571, #201144, #102015, #219408 ),
 .UNSPECIFIED., .F., .F.,
 ( 4, 2, 2, 2, 2, 2, 4 ),
 ( 0.000000000000000000, 2.389617747645615524E-05, 4.779235495291231047E-05, 9.558470990578232351E-05, 0.0001911694198114826000, 0.0003823388396228848064, 0.0007646776792456892735 ),
 .UNSPECIFIED. ) ;
#205943 = VERTEX_POINT ( 'NONE', #220630 ) ;
#205944 = DIRECTION ( 'NONE',  ( 0.000000000000000000, -0.8700118002898356018, 0.4930308989875170078 ) ) ;
#205945 = ORIENTED_EDGE ( 'NONE', *, *, #114301, .F. ) ;
#205946 = CARTESIAN_POINT ( 'NONE',  ( -21.45000000000000284, 7.708578643773852157, -146.3500000000000227 ) ) ;
#205947 = DIRECTION ( 'NONE',  ( 1.000000000000000000, 0.000000000000000000, 0.000000000000000000 ) ) ;
#205948 = DIRECTION ( 'NONE',  ( 1.000000000000000000, 0.000000000000000000, 0.000000000000000000 ) ) ;
#205949 = CARTESIAN_POINT ( 'NONE',  ( -21.11927991906891222, 30.77026771008070583, -252.1792548123860627 ) ) ;
#205950 = DIRECTION ( 'NONE',  ( 0.000000000000000000, 0.000000000000000000, -1.000000000000000000 ) ) ;
#205951 = ORIENTED_EDGE ( 'NONE', *, *, #89405, .T. ) ;
#205952 = EDGE_CURVE ( 'NONE', #172675, #133508, #203627, .T. ) ;
#205953 = CARTESIAN_POINT ( 'NONE',  ( 23.14999999999999503, 11.75000000001116263, -59.98519422934606382 ) ) ;
#205954 = AXIS2_PLACEMENT_3D ( 'NONE', #67696, #72866, #33754 ) ;
#205955 = AXIS2_PLACEMENT_3D ( 'NONE', #145988, #28673, #105546 ) ;
#205956 = CARTESIAN_POINT ( 'NONE',  ( 27.30103769104855971, 12.20000000000000284, 33.00000000000000000 ) ) ;
#205957 = CARTESIAN_POINT ( 'NONE',  ( -21.11927991906891222, 0.009083679485027933501, -27.05150688150849092 ) ) ;
#205958 = CARTESIAN_POINT ( 'NONE',  ( -20.54999999999999716, 1.999999999999998224, -12.72462192276209869 ) ) ;
#205959 = AXIS2_PLACEMENT_3D ( 'NONE', #93055, #151778, #235144 ) ;
#205960 = ORIENTED_EDGE ( 'NONE', *, *, #237213, .T. ) ;
#205962 = DIRECTION ( 'NONE',  ( 0.000000000000000000, 0.000000000000000000, -1.000000000000000000 ) ) ;
#205961 = CARTESIAN_POINT ( 'NONE',  ( -18.50000000000000000, -1.362429037182155023, -175.3888812479212334 ) ) ;
#205963 = ORIENTED_EDGE ( 'NONE', *, *, #73238, .T. ) ;
#205966 = ORIENTED_EDGE ( 'NONE', *, *, #199882, .T. ) ;
#205965 = CARTESIAN_POINT ( 'NONE',  ( -18.39418127959864790, 64.51609439831383952, -112.2731074845243739 ) ) ;
#205964 = FACE_OUTER_BOUND ( 'NONE', #149937, .T. ) ;
#205967 = ORIENTED_EDGE ( 'NONE', *, *, #257792, .F. ) ;
#205968 = LINE ( 'NONE', #27380, #26926 ) ;
#205969 = AXIS2_PLACEMENT_3D ( 'NONE', #247008, #108788, #44976 ) ;
#205970 = DIRECTION ( 'NONE',  ( 0.000000000000000000, 0.6728971962616697722, 0.7397360091702875895 ) ) ;
#205971 = EDGE_CURVE ( 'NONE', #62684, #215984, #5195, .T. ) ;
#205972 = DIRECTION ( 'NONE',  ( -1.000000000000000000, 0.000000000000000000, 0.000000000000000000 ) ) ;
#205973 = AXIS2_PLACEMENT_3D ( 'NONE', #7243, #184607, #162503 ) ;
#205974 = ORIENTED_EDGE ( 'NONE', *, *, #218740, .T. ) ;
#205976 = EDGE_CURVE ( 'NONE', #242949, #213781, #161957, .T. ) ;
#205975 = FACE_OUTER_BOUND ( 'NONE', #116236, .T. ) ;
#205977 = CARTESIAN_POINT ( 'NONE',  ( -20.85000000000000142, 7.070967871809997973, -204.7465642218682547 ) ) ;
#205978 = EDGE_CURVE ( 'NONE', #96084, #125974, #95779, .T. ) ;
#205980 = DIRECTION ( 'NONE',  ( 2.557131231893036985E-16, -0.8660254037844383745, 0.5000000000000003331 ) ) ;
#205979 = FACE_OUTER_BOUND ( 'NONE', #118218, .T. ) ;
#205981 = EDGE_CURVE ( 'NONE', #33613, #50040, #184274, .T. ) ;
#205983 = ORIENTED_EDGE ( 'NONE', *, *, #114124, .F. ) ;
#205982 = CARTESIAN_POINT ( 'NONE',  ( 21.02374657821571446, 11.60000000083146787, -93.57179677019814790 ) ) ;
#205984 = CIRCLE ( 'NONE', #10177, 3.999999999999989786 ) ;
#205985 = AXIS2_PLACEMENT_3D ( 'NONE', #73788, #18606, #120315 ) ;
#205986 = VECTOR ( 'NONE', #88037, 1000.000000000000000 ) ;
#205987 = ORIENTED_EDGE ( 'NONE', *, *, #71251, .T. ) ;
#205988 = CARTESIAN_POINT ( 'NONE',  ( 19.83283456528359423, 64.25000000001176659, -78.17310748510507779 ) ) ;
#205989 = DIRECTION ( 'NONE',  ( -1.000000000000000000, -1.836970198721029934E-16, -3.186635328391151676E-31 ) ) ;
#205990 = ADVANCED_FACE ( 'NONE', ( #146209 ), #159053, .F. ) ;
#205991 = DIRECTION ( 'NONE',  ( 0.000000000000000000, 0.000000000000000000, -1.000000000000000000 ) ) ;
#205993 = EDGE_CURVE ( 'NONE', #109375, #145911, #118625, .T. ) ;
#205992 = VERTEX_POINT ( 'NONE', #23741 ) ;
#205994 = CARTESIAN_POINT ( 'NONE',  ( -23.25000000000000000, 31.11065811373596190, -259.9087319612273177 ) ) ;
#205995 = CARTESIAN_POINT ( 'NONE',  ( 20.94999999999999574, -11.39257802169451672, -170.5739495798319183 ) ) ;
#205996 = CARTESIAN_POINT ( 'NONE',  ( -21.14999999999999858, 11.65000000001115588, -33.60000000000000142 ) ) ;
#205998 = ADVANCED_FACE ( 'NONE', ( #242739 ), #196748, .T. ) ;
#205997 = AXIS2_PLACEMENT_3D ( 'NONE', #206497, #27898, #107387 ) ;
#205999 = ORIENTED_EDGE ( 'NONE', *, *, #210773, .T. ) ;
#206000 = DIRECTION ( 'NONE',  ( -1.000000000000000000, 0.000000000000000000, -0.000000000000000000 ) ) ;
#206001 = AXIS2_PLACEMENT_3D ( 'NONE', #160860, #44757, #124296 ) ;
#206002 = ADVANCED_FACE ( 'NONE', ( #125384 ), #44563, .F. ) ;
#206003 = ORIENTED_EDGE ( 'NONE', *, *, #152011, .T. ) ;
#206004 = LINE ( 'NONE', #88597, #180416 ) ;
#206005 = CYLINDRICAL_SURFACE ( 'NONE', #123139, 0.1000000000000028644 ) ;
#206006 = EDGE_CURVE ( 'NONE', #96525, #177565, #86216, .T. ) ;
#206007 = EDGE_CURVE ( 'NONE', #205761, #34506, #13605, .T. ) ;
#206008 = CIRCLE ( 'NONE', #118546, 0.09999999999999986677 ) ;
#206009 = AXIS2_PLACEMENT_3D ( 'NONE', #58177, #54341, #133884 ) ;
#206010 = ORIENTED_EDGE ( 'NONE', *, *, #218913, .T. ) ;
#206011 = AXIS2_PLACEMENT_3D ( 'NONE', #249204, #155261, #234761 ) ;
#206012 = VERTEX_POINT ( 'NONE', #50945 ) ;
#206013 = EDGE_CURVE ( 'NONE', #242376, #168873, #42821, .T. ) ;
#206014 = LINE ( 'NONE', #106894, #124944 ) ;
#206015 = ORIENTED_EDGE ( 'NONE', *, *, #108846, .T. ) ;
#206017 = VERTEX_POINT ( 'NONE', #208776 ) ;
#206016 = CARTESIAN_POINT ( 'NONE',  ( -21.59780538579341425, 6.847090529943250736, 0.09897866959798369557 ) ) ;
#206019 = EDGE_CURVE ( 'NONE', #226316, #225564, #80192, .T. ) ;
#206018 = VERTEX_POINT ( 'NONE', #71841 ) ;
#206020 = EDGE_CURVE ( 'NONE', #66775, #38016, #38543, .T. ) ;
#206022 = VERTEX_POINT ( 'NONE', #112250 ) ;
#206021 = ORIENTED_EDGE ( 'NONE', *, *, #111069, .T. ) ;
#206023 = EDGE_CURVE ( 'NONE', #60454, #30910, #108386, .T. ) ;
#206024 = CARTESIAN_POINT ( 'NONE',  ( -18.37151313414686982, -9.571014125767112191, -107.3166629092389854 ) ) ;
#206025 = VERTEX_POINT ( 'NONE', #167105 ) ;
#206026 = CARTESIAN_POINT ( 'NONE',  ( -23.15000000000000213, 1.115600667400684642E-11, -67.00000000000004263 ) ) ;
#206027 = VECTOR ( 'NONE', #13981, 1000.000000000000000 ) ;
#206028 = CARTESIAN_POINT ( 'NONE',  ( 21.05000000000000071, 67.12791932463488820, -195.0020600656924614 ) ) ;
#206029 = CARTESIAN_POINT ( 'NONE',  ( -18.40904629823846506, 86.89640092179662645, -199.6396877013420692 ) ) ;
#206030 = VERTEX_POINT ( 'NONE', #250452 ) ;
#206031 = ORIENTED_EDGE ( 'NONE', *, *, #243413, .F. ) ;
#206032 = DIRECTION ( 'NONE',  ( 1.000000000000000000, 0.000000000000000000, 0.000000000000000000 ) ) ;
#206033 = VECTOR ( 'NONE', #142352, 1000.000000000000000 ) ;
#206035 = EDGE_LOOP ( 'NONE', ( #182556, #141213, #204257, #60352 ) ) ;
#206034 = DIRECTION ( 'NONE',  ( 1.000000000000000000, 0.000000000000000000, 0.000000000000000000 ) ) ;
#206036 = DIRECTION ( 'NONE',  ( 0.000000000000000000, 0.000000000000000000, -1.000000000000000000 ) ) ;
#206038 = ORIENTED_EDGE ( 'NONE', *, *, #87062, .T. ) ;
#206037 = LINE ( 'NONE', #166945, #135679 ) ;
#206039 = EDGE_CURVE ( 'NONE', #52417, #54460, #227035, .T. ) ;
#206040 = ORIENTED_EDGE ( 'NONE', *, *, #170687, .T. ) ;
#206041 = DIRECTION ( 'NONE',  ( -1.284434275755705296E-16, 0.7071067811865471286, 0.7071067811865479058 ) ) ;
#206042 = VERTEX_POINT ( 'NONE', #246595 ) ;
#206043 = VERTEX_POINT ( 'NONE', #67967 ) ;
#206044 = CARTESIAN_POINT ( 'NONE',  ( -16.77308656112214535, 9.950000000011142376, -180.1501931917022716 ) ) ;
#206045 = DIRECTION ( 'NONE',  ( -1.000000000000000000, 0.000000000000000000, 0.000000000000000000 ) ) ;
#206047 = ORIENTED_EDGE ( 'NONE', *, *, #71889, .T. ) ;
#206046 = ORIENTED_EDGE ( 'NONE', *, *, #138596, .F. ) ;
#206048 = AXIS2_PLACEMENT_3D ( 'NONE', #117316, #101564, #140724 ) ;
#206049 = ORIENTED_EDGE ( 'NONE', *, *, #240929, .F. ) ;
#206050 = CARTESIAN_POINT ( 'NONE',  ( -22.50000000000094147, 64.05844819680045532, -247.1686437718134357 ) ) ;
#206051 = VERTEX_POINT ( 'NONE', #49688 ) ;
#206052 = ORIENTED_EDGE ( 'NONE', *, *, #244603, .T. ) ;
#206053 = DIRECTION ( 'NONE',  ( -0.000000000000000000, -0.1298341882520022694, -0.9915357197604853789 ) ) ;
#206055 = ORIENTED_EDGE ( 'NONE', *, *, #881, .F. ) ;
#206054 = CARTESIAN_POINT ( 'NONE',  ( -18.59999999999999787, 77.86671491006960366, -158.2704322382423356 ) ) ;
#206056 = DIRECTION ( 'NONE',  ( 0.000000000000000000, 1.000000000000000000, 0.000000000000000000 ) ) ;
#206058 = SPHERICAL_SURFACE ( 'NONE', #98394, 0.1000000000000000056 ) ;
#206057 = CARTESIAN_POINT ( 'NONE',  ( -20.54999999999999716, 4.350000000011156054, -121.6500000000000341 ) ) ;
#206059 = CARTESIAN_POINT ( 'NONE',  ( 18.41789779300686192, 85.50000000001263345, -196.4910378181636190 ) ) ;
#206060 = LINE ( 'NONE', #204761, #169527 ) ;
#206061 = VERTEX_POINT ( 'NONE', #52236 ) ;
#206062 = EDGE_LOOP ( 'NONE', ( #110332, #244533, #220944, #231091 ) ) ;
#206063 = CARTESIAN_POINT ( 'NONE',  ( -22.59999999999999787, 1.115600667400684642E-11, -33.50000000000000000 ) ) ;
#206065 = ADVANCED_FACE ( 'NONE', ( #251741 ), #189208, .F. ) ;
#206064 = DIRECTION ( 'NONE',  ( 0.000000000000000000, -0.6728388485993130885, 0.7397890806274115549 ) ) ;
#206066 = AXIS2_PLACEMENT_3D ( 'NONE', #116850, #196377, #93422 ) ;
#206067 = VERTEX_POINT ( 'NONE', #170974 ) ;
#206068 = EDGE_CURVE ( 'NONE', #7826, #158463, #246813, .T. ) ;
#206069 = VECTOR ( 'NONE', #107144, 1000.000000000000000 ) ;
#206070 = AXIS2_PLACEMENT_3D ( 'NONE', #240776, #122110, #201634 ) ;
#206071 = VECTOR ( 'NONE', #202702, 1000.000000000000000 ) ;
#206072 = CARTESIAN_POINT ( 'NONE',  ( -20.94999999999999929, 76.00000000001142553, -36.02310748452432421 ) ) ;
#206073 = ORIENTED_EDGE ( 'NONE', *, *, #150293, .F. ) ;
#206074 = EDGE_LOOP ( 'NONE', ( #67258, #182562, #2544, #223234, #196674 ) ) ;
#206075 = STYLED_ITEM ( 'NONE', ( #116311 ), #154111 ) ;
#206076 = EDGE_CURVE ( 'NONE', #73365, #47971, #73140, .T. ) ;
#206077 = FACE_OUTER_BOUND ( 'NONE', #210774, .T. ) ;
#206079 = ADVANCED_FACE ( 'NONE', ( #211337 ), #70571, .F. ) ;
#206078 = CARTESIAN_POINT ( 'NONE',  ( -18.40000000000000213, 31.17298305880675002, -240.2029303890703886 ) ) ;
#206080 = EDGE_LOOP ( 'NONE', ( #250269, #25440, #219885, #143800 ) ) ;
#206081 = CARTESIAN_POINT ( 'NONE',  ( -20.97625342178427843, 11.60000000083146077, -107.4282032298019800 ) ) ;
#206082 = CARTESIAN_POINT ( 'NONE',  ( 18.49999999999999289, 10.20857864377385127, -158.6500000000000057 ) ) ;
#206083 = EDGE_LOOP ( 'NONE', ( #2117, #164016, #69527, #2455 ) ) ;
#206084 = CARTESIAN_POINT ( 'NONE',  ( -21.05000000000000071, 7.128833340093095217, -233.7327013124392749 ) ) ;
#206085 = DIRECTION ( 'NONE',  ( 0.000000000000000000, 0.9126074666063660468, 0.4088369013363524762 ) ) ;
#206087 = CARTESIAN_POINT ( 'NONE',  ( -21.05000000000000426, 6.477046381801003783, -67.10000000000006537 ) ) ;
#206086 = FACE_OUTER_BOUND ( 'NONE', #221120, .T. ) ;
#206088 = DIRECTION ( 'NONE',  ( 0.000000000000000000, 6.608470384673536035E-15, -1.000000000000000000 ) ) ;
#206089 = DIRECTION ( 'NONE',  ( 0.000000000000000000, -0.8814952561688266242, 0.4721928772777652106 ) ) ;
#206090 = DIRECTION ( 'NONE',  ( 0.000000000000000000, 0.000000000000000000, -1.000000000000000000 ) ) ;
#206091 = LINE ( 'NONE', #204785, #78557 ) ;
#206092 = VECTOR ( 'NONE', #62084, 1000.000000000000000 ) ;
#206093 = EDGE_LOOP ( 'NONE', ( #105311, #60094, #11804, #16602, #250648, #74861, #50785 ) ) ;
#206094 = AXIS2_PLACEMENT_3D ( 'NONE', #224930, #187133, #8480 ) ;
#206096 = ORIENTED_EDGE ( 'NONE', *, *, #120406, .F. ) ;
#206095 = ORIENTED_EDGE ( 'NONE', *, *, #75312, .T. ) ;
#206097 = ORIENTED_EDGE ( 'NONE', *, *, #80459, .T. ) ;
#206098 = AXIS2_PLACEMENT_3D ( 'NONE', #149797, #109337, #188900 ) ;
#206099 = FACE_OUTER_BOUND ( 'NONE', #197171, .T. ) ;
#206100 = CARTESIAN_POINT ( 'NONE',  ( 18.59999999999999787, 1.115600667400684642E-11, -33.50000000000000000 ) ) ;
#206102 = FACE_OUTER_BOUND ( 'NONE', #244487, .T. ) ;
#206101 = CARTESIAN_POINT ( 'NONE',  ( -23.15000000000000213, 11.59999999999999964, -26.57179676972450011 ) ) ;
#206103 = ORIENTED_EDGE ( 'NONE', *, *, #208734, .T. ) ;
#206104 = AXIS2_PLACEMENT_3D ( 'NONE', #139159, #106143, #239582 ) ;
#206105 = LINE ( 'NONE', #185259, #109073 ) ;
#206107 = AXIS2_PLACEMENT_3D ( 'NONE', #69351, #90159, #109727 ) ;
#206106 = DIRECTION ( 'NONE',  ( 0.000000000000000000, -0.000000000000000000, 1.000000000000000000 ) ) ;
#206108 = CARTESIAN_POINT ( 'NONE',  ( 21.05000000000000071, 60.85896401437205583, -225.4389122456526025 ) ) ;
#206109 = FACE_OUTER_BOUND ( 'NONE', #14001, .T. ) ;
#206111 = EDGE_LOOP ( 'NONE', ( #226876, #102330, #26085, #16224 ) ) ;
#206110 = AXIS2_PLACEMENT_3D ( 'NONE', #192032, #95468, #13379 ) ;
#206112 = EDGE_CURVE ( 'NONE', #115416, #257696, #221853, .T. ) ;
#206113 = DIRECTION ( 'NONE',  ( -1.000000000000000000, -0.000000000000000000, 0.000000000000000000 ) ) ;
#206114 = AXIS2_PLACEMENT_3D ( 'NONE', #20322, #98505, #64555 ) ;
#206115 = CARTESIAN_POINT ( 'NONE',  ( 18.69999999999999929, 1.350000000000000089, 21.90000000000000213 ) ) ;
#206116 = ORIENTED_EDGE ( 'NONE', *, *, #67633, .T. ) ;
#206117 = ORIENTED_EDGE ( 'NONE', *, *, #43489, .F. ) ;
#206118 = CARTESIAN_POINT ( 'NONE',  ( -18.40000000000000213, 64.51332499825421962, -93.77310748452438816 ) ) ;
#206119 = MECHANICAL_DESIGN_GEOMETRIC_PRESENTATION_REPRESENTATION (  '', ( #181189 ), #139458 ) ;
#206120 = DIRECTION ( 'NONE',  ( 0.000000000000000000, 0.000000000000000000, 1.000000000000000000 ) ) ;
#206121 = CARTESIAN_POINT ( 'NONE',  ( 18.49999999999999289, 15.24523260243583600, -223.0274837629937963 ) ) ;
#206122 = PLANE ( 'NONE',  #64501 ) ;
#206123 = DIRECTION ( 'NONE',  ( 0.000000000000000000, -0.1335171055202901691, 0.9910465087640861759 ) ) ;
#206124 = TOROIDAL_SURFACE ( 'NONE', #56254, 0.6000000000000006439, 0.1000000000000000056 ) ;
#206125 = LINE ( 'NONE', #249120, #158715 ) ;
#206127 = ORIENTED_EDGE ( 'NONE', *, *, #145977, .T. ) ;
#206126 = VECTOR ( 'NONE', #243462, 1000.000000000000000 ) ;
#206129 = EDGE_CURVE ( 'NONE', #32720, #179132, #50986, .T. ) ;
#206128 = DIRECTION ( 'NONE',  ( -1.000000000000000000, 0.000000000000000000, 0.000000000000000000 ) ) ;
#206130 = CARTESIAN_POINT ( 'NONE',  ( -21.05000000000000071, 0.09779029131994597390, -60.74218538952392521 ) ) ;
#206132 = DIRECTION ( 'NONE',  ( -1.000000000000000000, 0.000000000000000000, 0.000000000000000000 ) ) ;
#206131 = CARTESIAN_POINT ( 'NONE',  ( -16.93826681692523550, 10.01142872029886810, -87.94545846735948658 ) ) ;
#206133 = DIRECTION ( 'NONE',  ( 0.000000000000000000, -1.000000000000000000, 0.000000000000000000 ) ) ;
#206134 = EDGE_CURVE ( 'NONE', #12289, #43410, #63656, .T. ) ;
#206135 = CARTESIAN_POINT ( 'NONE',  ( -18.45068461519105796, -9.486506529089087536, -7.068777168904707864 ) ) ;
#206136 = DIRECTION ( 'NONE',  ( -1.000000000000000000, -7.304098846218133681E-16, 4.217023435051677994E-16 ) ) ;
#206137 = CYLINDRICAL_SURFACE ( 'NONE', #210848, 0.1000000000000028644 ) ;
#206139 = ORIENTED_EDGE ( 'NONE', *, *, #63267, .F. ) ;
#206138 = FACE_OUTER_BOUND ( 'NONE', #34657, .T. ) ;
#206140 = EDGE_CURVE ( 'NONE', #21323, #109005, #255145, .T. ) ;
#206141 = EDGE_CURVE ( 'NONE', #89984, #188719, #234347, .T. ) ;
#206142 = EDGE_CURVE ( 'NONE', #107106, #19404, #242546, .T. ) ;
#206143 = CARTESIAN_POINT ( 'NONE',  ( 21.07928932188134397, 6.328516656404459262, -100.4011048543456468 ) ) ;
#206144 = VECTOR ( 'NONE', #230303, 1000.000000000000114 ) ;
#206145 = AXIS2_PLACEMENT_3D ( 'NONE', #999, #160140, #180968 ) ;
#206146 = CARTESIAN_POINT ( 'NONE',  ( 20.85000000000000142, 87.65000000001190017, -103.0231074845242176 ) ) ;
#206147 = ADVANCED_FACE ( 'NONE', ( #177377 ), #121935, .T. ) ;
#206148 = AXIS2_PLACEMENT_3D ( 'NONE', #36328, #115847, #134105 ) ;
#206149 = CARTESIAN_POINT ( 'NONE',  ( 21.00023020733502577, 65.55844536562159419, -242.0231774319958049 ) ) ;
#206150 = VERTEX_POINT ( 'NONE', #215181 ) ;
#206151 = LINE ( 'NONE', #88746, #117952 ) ;
#206152 = DIRECTION ( 'NONE',  ( 1.000000000000000000, 0.000000000000000000, 0.000000000000000000 ) ) ;
#206153 = DIRECTION ( 'NONE',  ( 0.000000000000000000, -1.000000000000000000, 0.000000000000000000 ) ) ;
#206154 = AXIS2_PLACEMENT_3D ( 'NONE', #257238, #159491, #219428 ) ;
#206155 = AXIS2_PLACEMENT_3D ( 'NONE', #237545, #43200, #158054 ) ;
#206156 = ORIENTED_EDGE ( 'NONE', *, *, #7570, .F. ) ;
#206157 = DIRECTION ( 'NONE',  ( 0.000000000000000000, 1.224646799147363807E-16, 1.000000000000000000 ) ) ;
#206159 = ORIENTED_EDGE ( 'NONE', *, *, #154801, .T. ) ;
#206158 = CARTESIAN_POINT ( 'NONE',  ( 23.14999999999999858, 1.115600667400684642E-11, -200.9999999999999432 ) ) ;
#206161 = FACE_OUTER_BOUND ( 'NONE', #137891, .T. ) ;
#206160 = CARTESIAN_POINT ( 'NONE',  ( 21.07946286933444924, -1.271897997408519165, -194.7996073284550675 ) ) ;
#206162 = EDGE_CURVE ( 'NONE', #168985, #82680, #142752, .T. ) ;
#206163 = DIRECTION ( 'NONE',  ( -1.000000000000000000, -0.000000000000000000, -0.000000000000000000 ) ) ;
#206164 = ORIENTED_EDGE ( 'NONE', *, *, #200364, .T. ) ;
#206165 = LINE ( 'NONE', #204858, #84572 ) ;
#206166 = AXIS2_PLACEMENT_3D ( 'NONE', #198707, #100844, #96998 ) ;
#206167 = CARTESIAN_POINT ( 'NONE',  ( 0.000000000000000000, 0.000000000000000000, 0.000000000000000000 ) ) ;
#206168 = CARTESIAN_POINT ( 'NONE',  ( -20.93302460841142931, 65.68434038414338261, -63.98668807260656166 ) ) ;
#206169 = CARTESIAN_POINT ( 'NONE',  ( -22.39999999999999858, 68.20922040163927136, -203.5231074845243882 ) ) ;
#206170 = DIRECTION ( 'NONE',  ( 0.000000000000000000, 0.2128009952263603954, -0.9770955615653315052 ) ) ;
#206171 = VECTOR ( 'NONE', #212423, 1000.000000000000000 ) ;
#206172 = ORIENTED_EDGE ( 'NONE', *, *, #167206, .T. ) ;
#206173 = FACE_OUTER_BOUND ( 'NONE', #172266, .T. ) ;
#206174 = DIRECTION ( 'NONE',  ( 0.000000000000000000, 0.000000000000000000, -1.000000000000000000 ) ) ;
#206175 = FILL_AREA_STYLE ('',( #181490 ) ) ;
#206176 = CARTESIAN_POINT ( 'NONE',  ( -22.48479450179659977, 0.04699158119804078271, -122.3500015537484131 ) ) ;
#206177 = EDGE_LOOP ( 'NONE', ( #73295, #18119, #198738, #138715 ) ) ;
#206178 = CIRCLE ( 'NONE', #39622, 0.1000000000000002554 ) ;
#206179 = ORIENTED_EDGE ( 'NONE', *, *, #142620, .F. ) ;
#206180 = CARTESIAN_POINT ( 'NONE',  ( 21.12400247839514122, 65.27851195598167067, -124.2731074845243739 ) ) ;
#206181 = CYLINDRICAL_SURFACE ( 'NONE', #144628, 0.09999999999998898659 ) ;
#206182 = DIRECTION ( 'NONE',  ( 0.000000000000000000, -1.000000000000000000, -8.717686153663073805E-15 ) ) ;
#206183 = CARTESIAN_POINT ( 'NONE',  ( 21.08750232978087524, 13.08152960257287489, -210.6665014416416284 ) ) ;
#206184 = CARTESIAN_POINT ( 'NONE',  ( 21.05000000000000071, 8.776282889879928106, -146.1762151410683543 ) ) ;
#206186 = PRESENTATION_STYLE_ASSIGNMENT (( #43265 ) ) ;
#206185 = DIRECTION ( 'NONE',  ( 4.504528286903032433E-15, -0.1298341882520124002, -0.9915357197604841577 ) ) ;
#206187 = SPHERICAL_SURFACE ( 'NONE', #165103, 0.1000000000000000056 ) ;
#206188 = CARTESIAN_POINT ( 'NONE',  ( -17.22767730082837900, 65.65075578754613161, -114.3806787939587650 ) ) ;
#206189 = CYLINDRICAL_SURFACE ( 'NONE', #118075, 11.74999999999999645 ) ;
#206190 = CARTESIAN_POINT ( 'NONE',  ( -18.59999999999999787, 1.736257131608553550, -78.56865232901755292 ) ) ;
#206191 = AXIS2_PLACEMENT_3D ( 'NONE', #121440, #21048, #96666 ) ;
#206192 = EDGE_CURVE ( 'NONE', #9758, #102432, #256111, .T. ) ;
#206194 = ORIENTED_EDGE ( 'NONE', *, *, #18524, .F. ) ;
#206193 = DIRECTION ( 'NONE',  ( 1.000000000000000000, 0.000000000000000000, 0.000000000000000000 ) ) ;
#206195 = VECTOR ( 'NONE', #16379, 1000.000000000000000 ) ;
#206196 = DIRECTION ( 'NONE',  ( -1.000000000000000000, 0.000000000000000000, 0.000000000000000000 ) ) ;
#206197 = DIRECTION ( 'NONE',  ( 0.000000000000000000, -6.982962677686266711E-15, 1.000000000000000000 ) ) ;
#206199 = DIRECTION ( 'NONE',  ( 0.000000000000000000, 1.000000000000000000, 0.000000000000000000 ) ) ;
#206198 = CARTESIAN_POINT ( 'NONE',  ( 22.60000000000000142, 64.25043287652255231, -103.1239658536231047 ) ) ;
#206200 = ORIENTED_EDGE ( 'NONE', *, *, #143991, .F. ) ;
#206201 = CARTESIAN_POINT ( 'NONE',  ( 23.25000000000000000, 84.59626168225496201, -112.4732350016745244 ) ) ;
#206202 = DIRECTION ( 'NONE',  ( 0.000000000000000000, 0.000000000000000000, 1.000000000000000000 ) ) ;
#206203 = DIRECTION ( 'NONE',  ( 0.000000000000000000, 0.000000000000000000, -1.000000000000000000 ) ) ;
#206204 = DIRECTION ( 'NONE',  ( 0.000000000000000000, 0.000000000000000000, -1.000000000000000000 ) ) ;
#206206 = EDGE_CURVE ( 'NONE', #178265, #188196, #74428, .T. ) ;
#206205 = CARTESIAN_POINT ( 'NONE',  ( 22.57320508075689247, 12.67709964810646817, -223.3751320524553705 ) ) ;
#206207 = ORIENTED_EDGE ( 'NONE', *, *, #57400, .T. ) ;
#206208 = B_SPLINE_CURVE_WITH_KNOTS ( 'NONE', 3,
 ( #156051, #175602, #118182, #255052, #235546, #257621, #157339, #16529, #236830, #20384 ),
 .UNSPECIFIED., .F., .F.,
 ( 4, 3, 3, 4 ),
 ( 0.000000000000000000, 3.394313611810755905E-05, 6.779740500699913091E-05, 0.0001049857339142649037 ),
 .UNSPECIFIED. ) ;
#206209 = ORIENTED_EDGE ( 'NONE', *, *, #95041, .T. ) ;
#206210 = EDGE_CURVE ( 'NONE', #104724, #110479, #213897, .T. ) ;
#206211 = EDGE_CURVE ( 'NONE', #61821, #142140, #242210, .T. ) ;
#206212 = DIRECTION ( 'NONE',  ( -0.000000000000000000, 1.000000000000000000, 6.982962677686266711E-15 ) ) ;
#206213 = ORIENTED_EDGE ( 'NONE', *, *, #211222, .F. ) ;
#206214 = DIRECTION ( 'NONE',  ( 0.000000000000000000, 0.8814952561688444987, -0.4721928772777320149 ) ) ;
#206215 = ORIENTED_EDGE ( 'NONE', *, *, #242833, .F. ) ;
#206216 = CARTESIAN_POINT ( 'NONE',  ( 21.05000000000000071, 10.48443348965288635, -141.4568058014919245 ) ) ;
#206217 = CARTESIAN_POINT ( 'NONE',  ( -18.50000000000000000, 7.783179459866045313, -245.3643104511423303 ) ) ;
#206218 = VECTOR ( 'NONE', #248864, 1000.000000000000000 ) ;
#206219 =( BOUNDED_SURFACE ( )  B_SPLINE_SURFACE ( 3, 2, ( 
 ( #242134, #101290, #144295 ),
 ( #83031, #180894, #45225 ),
 ( #62229, #143017, #141749 ),
 ( #23120, #222557, #221277 ) ),
 .UNSPECIFIED., .F., .F., .F. ) 
 B_SPLINE_SURFACE_WITH_KNOTS ( ( 4, 4 ),
 ( 3, 3 ),
 ( 0.3000847527772371737, 0.5552748953338753068 ),
 ( 0.000000000000000000, 1.000000000000000000 ),
 .UNSPECIFIED. ) 
 GEOMETRIC_REPRESENTATION_ITEM ( )  RATIONAL_B_SPLINE_SURFACE ( (
 ( 1.000000000000000000, 0.9152888060719498453, 1.000000000000000000),
 ( 1.000000000000000000, 0.9104333467450272943, 1.000000000000000000),
 ( 1.000000000000000000, 0.9035312726220395829, 1.000000000000000000),
 ( 1.000000000000000000, 0.8946697475932223753, 1.000000000000000000) ) ) 
 REPRESENTATION_ITEM ( '' )  SURFACE ( )  );
#206220 = DIRECTION ( 'NONE',  ( 0.000000000000000000, 0.000000000000000000, -1.000000000000000000 ) ) ;
#206221 = ORIENTED_EDGE ( 'NONE', *, *, #120573, .F. ) ;
#206222 = EDGE_CURVE ( 'NONE', #242166, #159849, #254651, .T. ) ;
#206223 = EDGE_CURVE ( 'NONE', #96734, #198238, #54769, .T. ) ;
#206224 = DIRECTION ( 'NONE',  ( 0.000000000000000000, 0.000000000000000000, 1.000000000000000000 ) ) ;
#206225 = DIRECTION ( 'NONE',  ( -1.000000000000000000, 1.836970198721029934E-16, 1.282749433769087582E-30 ) ) ;
#206226 = CARTESIAN_POINT ( 'NONE',  ( 18.69999999999999929, -11.65000000000000036, 5.900000000000001243 ) ) ;
#206227 = CARTESIAN_POINT ( 'NONE',  ( 22.39999999999999503, 64.25000000001195133, -103.0231074845244024 ) ) ;
#206228 = DIRECTION ( 'NONE',  ( 1.000000000000000000, 0.000000000000000000, 0.000000000000000000 ) ) ;
#206229 = PRODUCT_DEFINITION ( 'UNKNOWN', '', #11353, #45242 ) ;
#206230 = DIRECTION ( 'NONE',  ( 0.000000000000000000, 0.000000000000000000, -1.000000000000000000 ) ) ;
#206231 = CARTESIAN_POINT ( 'NONE',  ( -21.05000000000000071, 74.16465844978715438, -57.96795619196135618 ) ) ;
#206232 = VERTEX_POINT ( 'NONE', #118672 ) ;
#206234 = CARTESIAN_POINT ( 'NONE',  ( 21.15000000000005187, 64.35000000001120668, -51.02310748452479316 ) ) ;
#206233 = DIRECTION ( 'NONE',  ( 0.000000000000000000, 0.000000000000000000, 1.000000000000000000 ) ) ;
#206235 = EDGE_LOOP ( 'NONE', ( #31589, #128770, #111047 ) ) ;
#206237 = VERTEX_POINT ( 'NONE', #36585 ) ;
#206236 = CARTESIAN_POINT ( 'NONE',  ( -23.15000000000000213, 1.925233644870972816, -113.2302435331261563 ) ) ;
#206238 = CIRCLE ( 'NONE', #222971, 0.09999999999999810429 ) ;
#206239 = VERTEX_POINT ( 'NONE', #216456 ) ;
#206240 = AXIS2_PLACEMENT_3D ( 'NONE', #246252, #224104, #221521 ) ;
#206241 = FACE_OUTER_BOUND ( 'NONE', #95252, .T. ) ;
#206242 = CARTESIAN_POINT ( 'NONE',  ( 18.51024323315077069, 10.31104185824064068, -72.52045169831059468 ) ) ;
#206243 = DIRECTION ( 'NONE',  ( -1.000000000000000000, 0.000000000000000000, 0.000000000000000000 ) ) ;
#206244 = EDGE_CURVE ( 'NONE', #14406, #72194, #54808, .T. ) ;
#206245 = LINE ( 'NONE', #27645, #216746 ) ;
#206246 = ORIENTED_EDGE ( 'NONE', *, *, #108673, .F. ) ;
#206247 = EDGE_CURVE ( 'NONE', #114996, #250305, #202660, .T. ) ;
#206248 = EDGE_CURVE ( 'NONE', #14606, #36355, #104625, .T. ) ;
#206249 = CARTESIAN_POINT ( 'NONE',  ( -16.81744102076749314, 66.05000000001157900, -56.87310748452438958 ) ) ;
#206250 = FACE_OUTER_BOUND ( 'NONE', #117097, .T. ) ;
#206251 = ORIENTED_EDGE ( 'NONE', *, *, #241049, .T. ) ;
#206252 = DIRECTION ( 'NONE',  ( 0.000000000000000000, 1.000000000000000000, 0.000000000000000000 ) ) ;
#206253 = ADVANCED_FACE ( 'NONE', ( #178660 ), #78227, .F. ) ;
#206255 = VECTOR ( 'NONE', #159226, 1000.000000000000114 ) ;
#206254 = CARTESIAN_POINT ( 'NONE',  ( 21.72449340488910607, 30.36402033568042569, -234.5126641304238149 ) ) ;
#206256 = EDGE_LOOP ( 'NONE', ( #239719, #94585, #149278, #52239, #25662 ) ) ;
#206258 = FACE_OUTER_BOUND ( 'NONE', #235041, .T. ) ;
#206257 = VECTOR ( 'NONE', #50690, 1000.000000000000000 ) ;
#206259 = AXIS2_PLACEMENT_3D ( 'NONE', #10842, #52511, #49951 ) ;
#206260 = CIRCLE ( 'NONE', #81314, 0.1000000000000021844 ) ;
#206261 = VERTEX_POINT ( 'NONE', #194366 ) ;
#206262 = CARTESIAN_POINT ( 'NONE',  ( 20.94999999999999574, -11.48912529307605901, -3.100000000000000533 ) ) ;
#206263 = VERTEX_POINT ( 'NONE', #113515 ) ;
#206264 = FACE_OUTER_BOUND ( 'NONE', #203439, .T. ) ;
#206265 = CARTESIAN_POINT ( 'NONE',  ( 22.50000000000000000, 7.750000000011162626, -33.39999999999999858 ) ) ;
#206266 = DIRECTION ( 'NONE',  ( 0.000000000000000000, -6.853228547068871147E-15, 1.000000000000000000 ) ) ;
#206267 = CARTESIAN_POINT ( 'NONE',  ( 18.39999999999998082, 64.52683809665015247, -194.2731074845244450 ) ) ;
#206268 = ADVANCED_FACE ( 'NONE', ( #15731 ), #155246, .F. ) ;
#206269 = CARTESIAN_POINT ( 'NONE',  ( 21.05000000000000071, 11.65000000001116298, -179.6499999999999773 ) ) ;
#206270 = CARTESIAN_POINT ( 'NONE',  ( -20.54999999999999716, 4.349999999999999645, -21.14999999999999858 ) ) ;
#206271 = CARTESIAN_POINT ( 'NONE',  ( -23.25000000000000000, 36.65892442174935439, -249.5511627012433848 ) ) ;
#206272 = VECTOR ( 'NONE', #6180, 1000.000000000000114 ) ;
#206273 = ORIENTED_EDGE ( 'NONE', *, *, #75300, .T. ) ;
#206275 = DIRECTION ( 'NONE',  ( 1.000000000000000000, 0.000000000000000000, 0.000000000000000000 ) ) ;
#206274 = CARTESIAN_POINT ( 'NONE',  ( 23.25000000000000000, -11.74999999998883560, -112.6500000000000341 ) ) ;
#206276 = TOROIDAL_SURFACE ( 'NONE', #81328, 0.2000000000000000111, 0.1000000000000000056 ) ;
#206277 = EDGE_LOOP ( 'NONE', ( #169533, #101188, #234928, #23513, #162312 ) ) ;
#206278 = CONICAL_SURFACE ( 'NONE', #222828, 6.250000000000005329, 0.7853981633974431720 ) ;
#206279 = DIRECTION ( 'NONE',  ( 1.000000000000000000, 0.000000000000000000, 0.000000000000000000 ) ) ;
#206280 = DIRECTION ( 'NONE',  ( 1.000000000000000000, 0.000000000000000000, 0.000000000000000000 ) ) ;
#206281 = ADVANCED_FACE ( 'NONE', ( #221573 ), #63138, .T. ) ;
#206282 = LINE ( 'NONE', #181597, #208199 ) ;
#206284 = ORIENTED_EDGE ( 'NONE', *, *, #182822, .T. ) ;
#206283 = LINE ( 'NONE', #134103, #17103 ) ;
#206286 = VERTEX_POINT ( 'NONE', #242435 ) ;
#206285 = FACE_OUTER_BOUND ( 'NONE', #3522, .T. ) ;
#206288 = DIRECTION ( 'NONE',  ( -3.265361837132813093E-16, 0.9770955615653316162, 0.2128009952263604232 ) ) ;
#206287 =( BOUNDED_CURVE ( )  B_SPLINE_CURVE ( 3, ( #4907, #140586, #222680, #123608 ),
 .UNSPECIFIED., .F., .F. ) 
 B_SPLINE_CURVE_WITH_KNOTS ( ( 4, 4 ),
 ( 5.731445031868799056, 5.983100554402348337 ),
 .UNSPECIFIED. ) 
 CURVE ( )  GEOMETRIC_REPRESENTATION_ITEM ( )  RATIONAL_B_SPLINE_CURVE ( ( 1.000000000000000000, 0.9947294176030464508, 0.9947294176030464508, 1.000000000000000000 ) ) 
 REPRESENTATION_ITEM ( '' )  );
#206289 = CIRCLE ( 'NONE', #202010, 4.099999999999992539 ) ;
#206290 = EDGE_CURVE ( 'NONE', #36195, #94008, #67242, .T. ) ;
#206291 = LINE ( 'NONE', #10660, #5337 ) ;
#206292 = CIRCLE ( 'NONE', #218724, 0.1000000000000000472 ) ;
#206293 = CIRCLE ( 'NONE', #97916, 0.09999999999999939493 ) ;
#206295 = ORIENTED_EDGE ( 'NONE', *, *, #60070, .T. ) ;
#206294 = CARTESIAN_POINT ( 'NONE',  ( 15.48841904831874849, 8.561580951692381092, -121.3500000000000369 ) ) ;
#206297 = EDGE_CURVE ( 'NONE', #168528, #134169, #83339, .T. ) ;
#206296 = DIRECTION ( 'NONE',  ( -0.000000000000000000, -0.8660254037844420383, 0.4999999999999943379 ) ) ;
#206298 = AXIS2_PLACEMENT_3D ( 'NONE', #189653, #252177, #11013 ) ;
#206299 = FACE_OUTER_BOUND ( 'NONE', #74674, .T. ) ;
#206301 = EDGE_CURVE ( 'NONE', #155916, #11015, #90899, .T. ) ;
#206300 = ORIENTED_EDGE ( 'NONE', *, *, #161059, .T. ) ;
#206302 = FACE_OUTER_BOUND ( 'NONE', #122562, .T. ) ;
#206303 = VERTEX_POINT ( 'NONE', #143340 ) ;
#206304 = CIRCLE ( 'NONE', #43977, 0.09999999999999997780 ) ;
#206305 = CARTESIAN_POINT ( 'NONE',  ( -18.47690164073607733, 85.46484453802364101, -29.32172654468814699 ) ) ;
#206306 = DIRECTION ( 'NONE',  ( 0.000000000000000000, 0.000000000000000000, 1.000000000000000000 ) ) ;
#206307 = VECTOR ( 'NONE', #70577, 1000.000000000000000 ) ;
#206309 = ORIENTED_EDGE ( 'NONE', *, *, #30565, .F. ) ;
#206308 = CIRCLE ( 'NONE', #218750, 0.5000000000000022204 ) ;
#206310 = DIRECTION ( 'NONE',  ( 1.000000000000000000, 0.000000000000000000, -0.000000000000000000 ) ) ;
#206311 = FACE_OUTER_BOUND ( 'NONE', #184372, .T. ) ;
#206312 = EDGE_LOOP ( 'NONE', ( #128811, #139937, #113274, #116273 ) ) ;
#206314 = ADVANCED_FACE ( 'NONE', ( #222874 ), #25566, .F. ) ;
#206313 = FACE_OUTER_BOUND ( 'NONE', #226873, .T. ) ;
#206315 = ADVANCED_FACE ( 'NONE', ( #44261 ), #108929, .T. ) ;
#206316 =( BOUNDED_CURVE ( )  B_SPLINE_CURVE ( 3, ( #33513, #89574, #169161, #111721 ),
 .UNSPECIFIED., .F., .F. ) 
 B_SPLINE_CURVE_WITH_KNOTS ( ( 4, 4 ),
 ( 3.141592653589778461, 4.712388980384684345 ),
 .UNSPECIFIED. ) 
 CURVE ( )  GEOMETRIC_REPRESENTATION_ITEM ( )  RATIONAL_B_SPLINE_CURVE ( ( 1.000000000000000000, 0.8047378541243628280, 0.8047378541243628280, 1.000000000000000000 ) ) 
 REPRESENTATION_ITEM ( '' )  );
#206317 = ORIENTED_EDGE ( 'NONE', *, *, #135607, .F. ) ;
#206318 = ORIENTED_EDGE ( 'NONE', *, *, #200035, .F. ) ;
#206319 = DIRECTION ( 'NONE',  ( 0.000000000000000000, -0.9651348961777157509, 0.2617529984165031243 ) ) ;
#206320 = VERTEX_POINT ( 'NONE', #239894 ) ;
#206321 = ADVANCED_FACE ( 'NONE', ( #5084 ), #146342, .F. ) ;
#206322 = CARTESIAN_POINT ( 'NONE',  ( -16.87683809663753465, 23.48945571633983675, -231.3055249780561837 ) ) ;
#206323 = ORIENTED_EDGE ( 'NONE', *, *, #190127, .F. ) ;
#206325 = VERTEX_POINT ( 'NONE', #84608 ) ;
#206324 = CARTESIAN_POINT ( 'NONE',  ( 23.15000000000000213, 88.41227409416215721, -173.1231074845242688 ) ) ;
#206326 = CARTESIAN_POINT ( 'NONE',  ( -21.00219873199074883, 11.60538868788787070, -73.91264742829459067 ) ) ;
#206327 = ORIENTED_EDGE ( 'NONE', *, *, #11332, .T. ) ;
#206328 = VECTOR ( 'NONE', #45613, 1000.000000000000000 ) ;
#206329 = DIRECTION ( 'NONE',  ( -0.000000000000000000, 0.000000000000000000, 1.000000000000000000 ) ) ;
#206331 = ORIENTED_EDGE ( 'NONE', *, *, #5405, .F. ) ;
#206330 = EDGE_CURVE ( 'NONE', #52663, #189844, #233846, .T. ) ;
#206332 = AXIS2_PLACEMENT_3D ( 'NONE', #32181, #89544, #230346 ) ;
#206335 = ORIENTED_EDGE ( 'NONE', *, *, #227671, .T. ) ;
#206334 = ORIENTED_EDGE ( 'NONE', *, *, #176347, .F. ) ;
#206333 = DIRECTION ( 'NONE',  ( 7.589415207398576792E-15, 1.000000000000000000, 6.982962677686266711E-15 ) ) ;
#206336 = CARTESIAN_POINT ( 'NONE',  ( -20.94999999999999929, -11.64999999998884483, -103.4000000000000341 ) ) ;
#206337 = CIRCLE ( 'NONE', #239651, 0.1999999999999987899 ) ;
#206338 = EDGE_CURVE ( 'NONE', #225338, #159302, #163133, .T. ) ;
#206339 = B_SPLINE_CURVE_WITH_KNOTS ( 'NONE', 3,
 ( #164145, #243665, #87147, #224092, #89713, #186274, #144553, #188828, #8913, #45467 ),
 .UNSPECIFIED., .F., .F.,
 ( 4, 2, 2, 2, 4 ),
 ( 0.000000000000000000, 0.0001660831991682338823, 0.0002491247987523630071, 0.0002906455985444138680, 0.0003321663983364646746 ),
 .UNSPECIFIED. ) ;
#206340 = ORIENTED_EDGE ( 'NONE', *, *, #226015, .F. ) ;
#206341 = AXIS2_PLACEMENT_3D ( 'NONE', #187744, #255339, #256620 ) ;
#206342 = AXIS2_PLACEMENT_3D ( 'NONE', #229547, #35223, #252935 ) ;
#206343 = VERTEX_POINT ( 'NONE', #144612 ) ;
#206344 = CARTESIAN_POINT ( 'NONE',  ( -21.05000000000000071, 69.45934304831145312, -203.5231074845243882 ) ) ;
#206345 = LINE ( 'NONE', #27740, #51631 ) ;
#206347 = ORIENTED_EDGE ( 'NONE', *, *, #98569, .T. ) ;
#206346 = LINE ( 'NONE', #189350, #120064 ) ;
#206348 = DIRECTION ( 'NONE',  ( 0.000000000000000000, 0.000000000000000000, 1.000000000000000000 ) ) ;
#206349 = ORIENTED_EDGE ( 'NONE', *, *, #17941, .T. ) ;
#206350 = ADVANCED_FACE ( 'NONE', ( #125082 ), #62532, .T. ) ;
#206352 = AXIS2_PLACEMENT_3D ( 'NONE', #107274, #202529, #46015 ) ;
#206351 = FACE_OUTER_BOUND ( 'NONE', #243605, .T. ) ;
#206353 = DIRECTION ( 'NONE',  ( 1.000000000000000000, 0.000000000000000000, 0.000000000000000000 ) ) ;
#206354 = ADVANCED_FACE ( 'NONE', ( #220330 ), #204593, .F. ) ;
#206355 = CIRCLE ( 'NONE', #6421, 0.8750000000000007772 ) ;
#206356 = ORIENTED_EDGE ( 'NONE', *, *, #114467, .F. ) ;
#206357 = CARTESIAN_POINT ( 'NONE',  ( 18.50000000000000711, 85.41920976342086647, -62.27533802176532163 ) ) ;
#206358 = CARTESIAN_POINT ( 'NONE',  ( -18.59999999999999787, 77.83585931145546510, -91.51866831572576189 ) ) ;
#206359 = CIRCLE ( 'NONE', #68999, 0.09999999999999971412 ) ;
#206360 = EDGE_LOOP ( 'NONE', ( #3571, #64701, #220651, #12300 ) ) ;
#206361 = DIRECTION ( 'NONE',  ( 0.000000000000000000, -6.982962677686266711E-15, 1.000000000000000000 ) ) ;
#206363 = ORIENTED_EDGE ( 'NONE', *, *, #66782, .T. ) ;
#206362 = ORIENTED_EDGE ( 'NONE', *, *, #71583, .T. ) ;
#206364 = ORIENTED_EDGE ( 'NONE', *, *, #204584, .F. ) ;
#206365 = CARTESIAN_POINT ( 'NONE',  ( -22.10000000000000142, -1.467286812112899463, 28.00000000000000000 ) ) ;
#206366 = VERTEX_POINT ( 'NONE', #85907 ) ;
#206367 = DIRECTION ( 'NONE',  ( 0.000000000000000000, 0.000000000000000000, 1.000000000000000000 ) ) ;
#206368 = VECTOR ( 'NONE', #185173, 1000.000000000000114 ) ;
#206369 = EDGE_LOOP ( 'NONE', ( #253829, #13485, #182650, #31228 ) ) ;
#206370 = DIRECTION ( 'NONE',  ( 0.000000000000000000, 2.891205793294679805E-16, -1.000000000000000000 ) ) ;
#206371 = DIRECTION ( 'NONE',  ( -1.000000000000000000, 0.000000000000000000, -0.000000000000000000 ) ) ;
#206372 = ORIENTED_EDGE ( 'NONE', *, *, #1928, .T. ) ;
#206373 = ORIENTED_EDGE ( 'NONE', *, *, #116810, .F. ) ;
#206374 = ORIENTED_EDGE ( 'NONE', *, *, #44148, .F. ) ;
#206375 = VECTOR ( 'NONE', #65671, 1000.000000000000000 ) ;
#206376 = AXIS2_PLACEMENT_3D ( 'NONE', #245218, #66578, #142247 ) ;
#206377 = EDGE_CURVE ( 'NONE', #177234, #195444, #205896, .T. ) ;
#206378 = AXIS2_PLACEMENT_3D ( 'NONE', #198542, #44614, #201113 ) ;
#206379 = FACE_OUTER_BOUND ( 'NONE', #213166, .T. ) ;
#206380 = ORIENTED_EDGE ( 'NONE', *, *, #176940, .F. ) ;
#206381 = CARTESIAN_POINT ( 'NONE',  ( -21.05000000000000071, 14.05000000000000071, -5.513695070760990191 ) ) ;
#206383 = VERTEX_POINT ( 'NONE', #82054 ) ;
#206382 = FACE_OUTER_BOUND ( 'NONE', #31574, .T. ) ;
#206384 = CARTESIAN_POINT ( 'NONE',  ( -18.50000000000000000, 23.34004772283015328, -229.2004250369967338 ) ) ;
#206385 = CARTESIAN_POINT ( 'NONE',  ( -23.25000000000000355, 23.82801463864234037, -229.3483719500187306 ) ) ;
#206386 = DIRECTION ( 'NONE',  ( 0.000000000000000000, 0.000000000000000000, 1.000000000000000000 ) ) ;
#206387 = CARTESIAN_POINT ( 'NONE',  ( -17.01473183483380680, 9.949999999999983302, -20.75000000000000000 ) ) ;
#206388 = CARTESIAN_POINT ( 'NONE',  ( 23.25000000000000000, -9.600000000000001421, -23.60603087734755690 ) ) ;
#206390 = DIRECTION ( 'NONE',  ( 0.000000000000000000, 1.000000000000000000, 6.982962677686266711E-15 ) ) ;
#206389 = FACE_OUTER_BOUND ( 'NONE', #31247, .T. ) ;
#206391 = CARTESIAN_POINT ( 'NONE',  ( 18.39999999999999858, -9.599999999988845900, -140.7001893912220680 ) ) ;
#206392 = FACE_OUTER_BOUND ( 'NONE', #57167, .T. ) ;
#206393 = EDGE_CURVE ( 'NONE', #10735, #93242, #204608, .T. ) ;
#206394 = CIRCLE ( 'NONE', #177389, 2.000000000000001776 ) ;
#206395 = ORIENTED_EDGE ( 'NONE', *, *, #174018, .T. ) ;
#206396 = ORIENTED_EDGE ( 'NONE', *, *, #99999, .F. ) ;
#206397 = AXIS2_PLACEMENT_3D ( 'NONE', #137872, #160052, #17939 ) ;
#206399 = EDGE_LOOP ( 'NONE', ( #14586, #194026, #56365, #101696 ) ) ;
#206398 = CARTESIAN_POINT ( 'NONE',  ( 20.95512820512820440, 11.25838014693916378, -210.9828572391344039 ) ) ;
#206400 = VERTEX_POINT ( 'NONE', #187628 ) ;
#206401 = CARTESIAN_POINT ( 'NONE',  ( 18.69999999999999929, -9.749999999999998224, 31.39999999999999858 ) ) ;
#206402 = CARTESIAN_POINT ( 'NONE',  ( 20.22894356738451194, 9.278498222849622223, -142.2685229062465169 ) ) ;
#206403 = CARTESIAN_POINT ( 'NONE',  ( 20.44999100639886080, 39.47177588848037999, -236.8516082872442610 ) ) ;
#206404 = VERTEX_POINT ( 'NONE', #95862 ) ;
#206405 = CARTESIAN_POINT ( 'NONE',  ( 18.43473516226069009, -9.494942282747068418, -40.54589868334937108 ) ) ;
#206406 = CARTESIAN_POINT ( 'NONE',  ( 21.04999999999999716, 65.61001066310818430, -241.9764486272661372 ) ) ;
#206407 = ORIENTED_EDGE ( 'NONE', *, *, #142246, .T. ) ;
#206409 = LINE ( 'NONE', #207712, #33978 ) ;
#206408 = CIRCLE ( 'NONE', #235624, 3.899999999999987033 ) ;
#206410 = CIRCLE ( 'NONE', #180904, 0.1000000000000033362 ) ;
#206411 = DIRECTION ( 'NONE',  ( 0.000000000000000000, 1.000000000000000000, 2.775557561562888827E-14 ) ) ;
#206412 = DIRECTION ( 'NONE',  ( 0.000000000000000000, -1.000000000000000000, 0.000000000000000000 ) ) ;
#206413 = FACE_OUTER_BOUND ( 'NONE', #27418, .T. ) ;
#206414 = CARTESIAN_POINT ( 'NONE',  ( -12.25000000000000178, 12.70026017068886404, -215.3766613508543628 ) ) ;
#206416 = ORIENTED_EDGE ( 'NONE', *, *, #122454, .F. ) ;
#206415 = DIRECTION ( 'NONE',  ( 0.000000000000000000, 0.000000000000000000, -1.000000000000000000 ) ) ;
#206417 = CARTESIAN_POINT ( 'NONE',  ( 20.94999999999999929, 64.35000000001141984, -36.02310748452440237 ) ) ;
#206418 = CARTESIAN_POINT ( 'NONE',  ( -21.05000000000000071, -11.64999999998884483, -70.00000000000004263 ) ) ;
#206419 = DIRECTION ( 'NONE',  ( 1.000000000000000000, 0.000000000000000000, 0.000000000000000000 ) ) ;
#206420 = CARTESIAN_POINT ( 'NONE',  ( -20.85000000000000142, 67.85909929089923764, -227.8797997985275856 ) ) ;
#206421 = ORIENTED_EDGE ( 'NONE', *, *, #255911, .F. ) ;
#206422 = DIRECTION ( 'NONE',  ( 1.000000000000000000, 0.000000000000000000, 0.000000000000000000 ) ) ;
#206423 = DIRECTION ( 'NONE',  ( 0.7071359030027966064, 0.6824253222083512815, -0.1850796971394955137 ) ) ;
#206424 = SPHERICAL_SURFACE ( 'NONE', #199157, 0.1000000000000000056 ) ;
#206425 = DIRECTION ( 'NONE',  ( -0.000000000000000000, -0.000000000000000000, 1.000000000000000000 ) ) ;
#206427 = EDGE_CURVE ( 'NONE', #9803, #257751, #50657, .T. ) ;
#206426 = CARTESIAN_POINT ( 'NONE',  ( -17.01473183483382101, 23.06621698515930063, -230.9822826988503834 ) ) ;
#206428 = TOROIDAL_SURFACE ( 'NONE', #56549, 11.90000000000000213, 0.1000000000000000056 ) ;
#206429 = CARTESIAN_POINT ( 'NONE',  ( -20.85000000000000142, 77.16412189325330928, -128.6082593989527254 ) ) ;
#206430 = CARTESIAN_POINT ( 'NONE',  ( -16.78270389226383230, 66.05262738339450834, -48.68190044761291801 ) ) ;
#206431 = CARTESIAN_POINT ( 'NONE',  ( 18.60000000000001563, 85.36423601037887465, -129.3428530837995822 ) ) ;
#206432 = AXIS2_PLACEMENT_3D ( 'NONE', #41445, #63542, #101338 ) ;
#206433 = DIRECTION ( 'NONE',  ( -0.000000000000000000, 0.8660254037844411501, 0.4999999999999956701 ) ) ;
#206434 = TOROIDAL_SURFACE ( 'NONE', #139773, 0.2000000000000000111, 0.1000000000000000056 ) ;
#206435 = EDGE_LOOP ( 'NONE', ( #133387, #219896, #153943, #232456 ) ) ;
#206436 = AXIS2_PLACEMENT_3D ( 'NONE', #80918, #245154, #103049 ) ;
#206437 = VERTEX_POINT ( 'NONE', #54174 ) ;
#206438 = VERTEX_POINT ( 'NONE', #126346 ) ;
#206439 = ADVANCED_FACE ( 'NONE', ( #214535 ), #228023, .T. ) ;
#206440 = CARTESIAN_POINT ( 'NONE',  ( 20.12518398540832010, 66.02491127934419524, -95.02643923205445731 ) ) ;
#206441 = LINE ( 'NONE', #83877, #156982 ) ;
#206442 = EDGE_LOOP ( 'NONE', ( #160760, #237489, #31694, #26757 ) ) ;
#206443 = ADVANCED_FACE ( 'NONE', ( #49388 ), #92179, .T. ) ;
#206444 = ORIENTED_EDGE ( 'NONE', *, *, #214145, .T. ) ;
#206445 = ADVANCED_FACE ( 'NONE', ( #253653 ), #145900, .T. ) ;
#206446 = ORIENTED_EDGE ( 'NONE', *, *, #216856, .T. ) ;
#206447 = CARTESIAN_POINT ( 'NONE',  ( -23.25000000000000000, 64.25000000001190870, -103.0231074845243882 ) ) ;
#206448 = CIRCLE ( 'NONE', #60679, 0.9000000000000014655 ) ;
#206449 = ORIENTED_EDGE ( 'NONE', *, *, #103107, .F. ) ;
#206450 = PRESENTATION_LAYER_ASSIGNMENT (  '', '', ( #60681 ) ) ;
#206451 = CARTESIAN_POINT ( 'NONE',  ( -17.11825945287481332, 9.950000000011138823, -54.25000000000000711 ) ) ;
#206452 = CARTESIAN_POINT ( 'NONE',  ( -20.94999999999999929, 79.23417978893665747, -236.1056577391152587 ) ) ;
#206453 = AXIS2_PLACEMENT_3D ( 'NONE', #51992, #190254, #106839 ) ;
#206454 = CARTESIAN_POINT ( 'NONE',  ( 18.59999999999999787, 0.6869237119019839799, -212.7787591058053067 ) ) ;
#206455 = DIRECTION ( 'NONE',  ( 0.000000000000000000, 7.116814260417668513E-15, -1.000000000000000000 ) ) ;
#206456 = CARTESIAN_POINT ( 'NONE',  ( -16.94226253665225457, 29.94475842175044988, -234.6669290423084249 ) ) ;
#206457 = CARTESIAN_POINT ( 'NONE',  ( 21.05000000000000071, 85.00000000001251976, -179.9170766071767389 ) ) ;
#206460 = VERTEX_POINT ( 'NONE', #169375 ) ;
#206459 = CARTESIAN_POINT ( 'NONE',  ( 21.12400222705945652, 44.24938628123909012, -236.5315751477832578 ) ) ;
#206458 = AXIS2_PLACEMENT_3D ( 'NONE', #320, #2879, #18612 ) ;
#206462 = CARTESIAN_POINT ( 'NONE',  ( 22.60000000000000142, 64.05844819680034163, -247.1686437718134073 ) ) ;
#206461 = CARTESIAN_POINT ( 'NONE',  ( 20.94560253601876809, 11.75000000000000355, -26.51008351251537576 ) ) ;
#206463 = ADVANCED_FACE ( 'NONE', ( #128929 ), #195004, .F. ) ;
#206464 = CARTESIAN_POINT ( 'NONE',  ( -18.59999999999999787, 11.75000000000000000, -33.50000000000000000 ) ) ;
#206465 = VERTEX_POINT ( 'NONE', #148492 ) ;
#206466 = DIRECTION ( 'NONE',  ( -0.7071067811865474617, 0.7071067811865474617, 0.000000000000000000 ) ) ;
#206467 = CIRCLE ( 'NONE', #94028, 0.1000000000000066946 ) ;
#206468 = CARTESIAN_POINT ( 'NONE',  ( -15.15766958671844122, 9.410538608540022665, -115.9326879971409312 ) ) ;
#206469 = DIRECTION ( 'NONE',  ( -0.000000000000000000, -6.982962677686266711E-15, 1.000000000000000000 ) ) ;
#206470 = AXIS2_PLACEMENT_3D ( 'NONE', #128017, #70635, #144984 ) ;
#206472 = ORIENTED_EDGE ( 'NONE', *, *, #77688, .F. ) ;
#206471 = VECTOR ( 'NONE', #112410, 999.9999999999998863 ) ;
#206473 = CARTESIAN_POINT ( 'NONE',  ( -21.00000000000000000, -0.04453801223857078301, -0.3305886640091971196 ) ) ;
#206474 = CARTESIAN_POINT ( 'NONE',  ( -16.85722902420155478, 66.05000000001183480, -82.28865495829489873 ) ) ;
#206475 = VERTEX_POINT ( 'NONE', #248874 ) ;
#206476 = TOROIDAL_SURFACE ( 'NONE', #123268, 0.2000000000000000111, 0.1000000000000000056 ) ;
#206477 = CARTESIAN_POINT ( 'NONE',  ( 22.59999999999999787, 64.35042919246758686, -170.1231074845244393 ) ) ;
#206478 = CARTESIAN_POINT ( 'NONE',  ( -21.05000000000000071, 86.52890073500824997, -209.5906233940697234 ) ) ;
#206479 = VECTOR ( 'NONE', #44558, 1000.000000000000000 ) ;
#206480 = LINE ( 'NONE', #27878, #153348 ) ;
#206481 = CARTESIAN_POINT ( 'NONE',  ( -22.39999999999999858, 1.115486826172573664E-11, -122.3504291924552234 ) ) ;
#206482 = VERTEX_POINT ( 'NONE', #208480 ) ;
#206483 = VECTOR ( 'NONE', #148496, 1000.000000000000000 ) ;
#206484 = VECTOR ( 'NONE', #110065, 1000.000000000000000 ) ;
#206485 = VERTEX_POINT ( 'NONE', #254890 ) ;
#206486 = DIRECTION ( 'NONE',  ( 1.000000000000000000, 0.000000000000000000, 0.000000000000000000 ) ) ;
#206487 = DIRECTION ( 'NONE',  ( 1.000000000000000000, 0.000000000000000000, 0.000000000000000000 ) ) ;
#206488 = DIRECTION ( 'NONE',  ( 1.000000000000000000, 0.000000000000000000, 0.000000000000000000 ) ) ;
#206489 = CYLINDRICAL_SURFACE ( 'NONE', #65465, 0.09999999999998898659 ) ;
#206490 = CARTESIAN_POINT ( 'NONE',  ( 21.05000000000000071, 74.83729825007431202, -162.1231074845243540 ) ) ;
#206491 = DIRECTION ( 'NONE',  ( 0.7071067811865475727, 0.7071067811865475727, 2.044391222244500083E-16 ) ) ;
#206492 = ORIENTED_EDGE ( 'NONE', *, *, #107575, .F. ) ;
#206493 = CARTESIAN_POINT ( 'NONE',  ( 20.94999999999999929, 67.22371710472005191, -182.2731074845244166 ) ) ;
#206494 = ADVANCED_FACE ( 'NONE', ( #29849 ), #133715, .T. ) ;
#206496 = VERTEX_POINT ( 'NONE', #46796 ) ;
#206495 = CARTESIAN_POINT ( 'NONE',  ( 21.05000000000000071, 76.00000000001216449, -140.8231074845243143 ) ) ;
#206497 = CARTESIAN_POINT ( 'NONE',  ( 20.94999999999999929, 1.115600667400684642E-11, -167.5000000000000284 ) ) ;
#206498 = DIRECTION ( 'NONE',  ( -1.073024830501117725E-15, -0.000000000000000000, -1.000000000000000000 ) ) ;
#206499 = DIRECTION ( 'NONE',  ( -1.000000000000000000, -8.673617379884087537E-15, 0.000000000000000000 ) ) ;
#206500 = CARTESIAN_POINT ( 'NONE',  ( -23.25000000000000000, 1.115600667400684642E-11, -71.15000000000004832 ) ) ;
#206502 = ORIENTED_EDGE ( 'NONE', *, *, #180946, .T. ) ;
#206501 = CARTESIAN_POINT ( 'NONE',  ( -23.15000000000000213, 8.674677285224309031, -220.8588764535527957 ) ) ;
#206503 = DIRECTION ( 'NONE',  ( 1.000000000000000000, -0.000000000000000000, -0.000000000000000000 ) ) ;
#206504 = FACE_OUTER_BOUND ( 'NONE', #210601, .T. ) ;
#206505 = CARTESIAN_POINT ( 'NONE',  ( 21.05000000000000071, -11.39257802169451139, -197.9260504201680249 ) ) ;
#206506 = CARTESIAN_POINT ( 'NONE',  ( -23.15000000000000213, 86.43238724539048690, -209.5644480942280836 ) ) ;
#206507 = EDGE_CURVE ( 'NONE', #103997, #67043, #87204, .T. ) ;
#206508 = ORIENTED_EDGE ( 'NONE', *, *, #38577, .F. ) ;
#206509 = CARTESIAN_POINT ( 'NONE',  ( -22.39999999999999858, 1.115600667400684642E-11, -33.50000000000000000 ) ) ;
#206510 = CIRCLE ( 'NONE', #244095, 0.09999999999999939493 ) ;
#206511 = CARTESIAN_POINT ( 'NONE',  ( -16.79270642812295833, 66.05375578307382511, -115.6841742059614688 ) ) ;
#206513 = CIRCLE ( 'NONE', #256315, 12.87499999999999822 ) ;
#206512 = LINE ( 'NONE', #54802, #162835 ) ;
#206515 = EDGE_CURVE ( 'NONE', #195188, #74473, #167240, .T. ) ;
#206514 = AXIS2_PLACEMENT_3D ( 'NONE', #233372, #194244, #115977 ) ;
#206516 = AXIS2_PLACEMENT_3D ( 'NONE', #184477, #30577, #187081 ) ;
#206517 = CARTESIAN_POINT ( 'NONE',  ( -20.95000000000000284, 11.64999999999999680, -26.48519422934605316 ) ) ;
#206518 = ORIENTED_EDGE ( 'NONE', *, *, #72317, .F. ) ;
#206519 = CARTESIAN_POINT ( 'NONE',  ( -16.80621392010910498, 9.942202577518919782, -87.81040803458310506 ) ) ;
#206520 = VERTEX_POINT ( 'NONE', #15070 ) ;
#206521 = VECTOR ( 'NONE', #177178, 1000.000000000000114 ) ;
#206522 = DIRECTION ( 'NONE',  ( 1.000000000000000000, 0.000000000000000000, 0.000000000000000000 ) ) ;
#206523 = CARTESIAN_POINT ( 'NONE',  ( 20.94999999999999929, 85.00000000001197975, -112.9170766071766820 ) ) ;
#206524 = EDGE_CURVE ( 'NONE', #189844, #255259, #217246, .T. ) ;
#206525 = DIRECTION ( 'NONE',  ( 0.000000000000000000, -1.000000000000000000, -6.860497997771532351E-15 ) ) ;
#206526 = VERTEX_POINT ( 'NONE', #55433 ) ;
#206527 = VECTOR ( 'NONE', #185238, 1000.000000000000000 ) ;
#206528 = VECTOR ( 'NONE', #30728, 1000.000000000000000 ) ;
#206529 = ADVANCED_FACE ( 'NONE', ( #10270 ), #89778, .T. ) ;
#206531 = ADVANCED_FACE ( 'NONE', ( #94586 ), #185681, .T. ) ;
#206530 = FACE_OUTER_BOUND ( 'NONE', #19066, .T. ) ;
#206532 = CARTESIAN_POINT ( 'NONE',  ( -20.54999999999999716, 2.000000000011154189, -87.67537807723795140 ) ) ;
#206533 = CARTESIAN_POINT ( 'NONE',  ( -33.72168855820452649, 64.52683809664949877, -112.2731074845243739 ) ) ;
#206534 = CARTESIAN_POINT ( 'NONE',  ( 20.94999999999999574, 11.62071067812981795, -160.6315833476590456 ) ) ;
#206535 = CARTESIAN_POINT ( 'NONE',  ( -22.39999999999999858, 64.25000000001195133, -103.1231074845243825 ) ) ;
#206536 = VERTEX_POINT ( 'NONE', #102263 ) ;
#206538 = ORIENTED_EDGE ( 'NONE', *, *, #212159, .T. ) ;
#206537 = CARTESIAN_POINT ( 'NONE',  ( -21.00023020733438273, 6.390869245278866018, -167.4999999999999432 ) ) ;
#206539 = EDGE_CURVE ( 'NONE', #73105, #63327, #71363, .T. ) ;
#206540 = VERTEX_POINT ( 'NONE', #81423 ) ;
#206541 = ORIENTED_EDGE ( 'NONE', *, *, #48843, .T. ) ;
#206542 = CARTESIAN_POINT ( 'NONE',  ( 21.12769345151713196, 65.28071232307149785, -124.2756271383268967 ) ) ;
#206543 = DIRECTION ( 'NONE',  ( 1.000000000000000000, -0.000000000000000000, -0.000000000000000000 ) ) ;
#206544 = DIRECTION ( 'NONE',  ( -1.000000000000000000, -3.265361837132813093E-16, 0.000000000000000000 ) ) ;
#206545 = ORIENTED_EDGE ( 'NONE', *, *, #91997, .T. ) ;
#206546 = ADVANCED_FACE ( 'NONE', ( #22797 ), #604, .T. ) ;
#206547 = EDGE_CURVE ( 'NONE', #66884, #170116, #8987, .T. ) ;
#206548 = CARTESIAN_POINT ( 'NONE',  ( -23.15000000000000213, 2.000000000011154189, -180.2246219227620543 ) ) ;
#206549 = DIRECTION ( 'NONE',  ( 0.000000000000000000, 0.9126074666063769270, 0.4088369013363280513 ) ) ;
#206550 = DIRECTION ( 'NONE',  ( -0.000000000000000000, 0.9651348961777156399, -0.2617529984165037349 ) ) ;
#206551 = ORIENTED_EDGE ( 'NONE', *, *, #10172, .T. ) ;
#206552 = CARTESIAN_POINT ( 'NONE',  ( -16.77683809663752257, 30.20632856012693424, -234.8070450048000737 ) ) ;
#206554 = EDGE_LOOP ( 'NONE', ( #56267, #173409, #229630, #257961 ) ) ;
#206553 = DIRECTION ( 'NONE',  ( -1.000000000000000000, 0.000000000000000000, 0.000000000000000000 ) ) ;
#206555 = DIRECTION ( 'NONE',  ( -0.000000000000000000, 1.000000000000000000, 1.734723475976807292E-15 ) ) ;
#206556 = CARTESIAN_POINT ( 'NONE',  ( 19.99999999999998934, 64.25000000001176659, -78.17310748452439384 ) ) ;
#206557 = CIRCLE ( 'NONE', #94116, 0.09999999999999939493 ) ;
#206558 = AXIS2_PLACEMENT_3D ( 'NONE', #193926, #55643, #136477 ) ;
#206559 = CIRCLE ( 'NONE', #27713, 0.1000000000000028644 ) ;
#206560 = VECTOR ( 'NONE', #33923, 1000.000000000000000 ) ;
#206561 = ORIENTED_EDGE ( 'NONE', *, *, #33260, .T. ) ;
#206562 = CARTESIAN_POINT ( 'NONE',  ( 21.05000000000000426, 69.74118280533089376, -170.0567402198580567 ) ) ;
#206563 = CARTESIAN_POINT ( 'NONE',  ( -12.29659703204452015, 66.64411154550947458, -120.2344645877463734 ) ) ;
#206564 = CARTESIAN_POINT ( 'NONE',  ( -18.50000000000000000, 21.17283678855158513, -243.7231193059830332 ) ) ;
#206565 = ORIENTED_EDGE ( 'NONE', *, *, #68958, .T. ) ;
#206566 = DIRECTION ( 'NONE',  ( 2.952720810173289112E-16, -1.000000000000000000, 0.000000000000000000 ) ) ;
#206567 = EDGE_CURVE ( 'NONE', #14224, #235594, #52989, .T. ) ;
#206568 = ADVANCED_FACE ( 'NONE', ( #56715 ), #77489, .T. ) ;
#206569 = CARTESIAN_POINT ( 'NONE',  ( -21.93642651522410247, 7.327166239336959208, -100.5000000000000284 ) ) ;
#206570 = VERTEX_POINT ( 'NONE', #42335 ) ;
#206571 = EDGE_CURVE ( 'NONE', #206286, #200486, #46378, .T. ) ;
#206572 = CIRCLE ( 'NONE', #40011, 1.500000000000001332 ) ;
#206573 = AXIS2_PLACEMENT_3D ( 'NONE', #105702, #41933, #60175 ) ;
#206574 = ORIENTED_EDGE ( 'NONE', *, *, #244384, .F. ) ;
#206575 = DIRECTION ( 'NONE',  ( 0.000000000000000000, 0.8700118002898322711, -0.4930308989875231140 ) ) ;
#206576 = VECTOR ( 'NONE', #254903, 1000.000000000000000 ) ;
#206577 = ORIENTED_EDGE ( 'NONE', *, *, #2659, .F. ) ;
#206578 = CARTESIAN_POINT ( 'NONE',  ( 18.53317502108576420, 10.32263460346244166, -39.06059579686719729 ) ) ;
#206579 = CARTESIAN_POINT ( 'NONE',  ( -16.97683809663752186, 66.05000000001255955, -183.4254715027207396 ) ) ;
#206581 = ORIENTED_EDGE ( 'NONE', *, *, #241631, .F. ) ;
#206580 = DIRECTION ( 'NONE',  ( 1.000000000000000000, 0.000000000000000000, 0.000000000000000000 ) ) ;
#206582 = DIRECTION ( 'NONE',  ( -1.000000000000000000, 0.000000000000000000, 0.000000000000000000 ) ) ;
#206583 = CARTESIAN_POINT ( 'NONE',  ( -23.15000000000000213, 1.115600667400684642E-11, -167.4999999999999716 ) ) ;
#206584 = DIRECTION ( 'NONE',  ( -1.000000000000000000, 0.000000000000000000, 0.000000000000000000 ) ) ;
#206585 = CARTESIAN_POINT ( 'NONE',  ( 21.10257677756355932, 75.97504925044370339, -75.92148922705705161 ) ) ;
#206586 = CARTESIAN_POINT ( 'NONE',  ( -18.50000000000000000, 66.85000000001186038, -90.67310748452436542 ) ) ;
#206587 = EDGE_CURVE ( 'NONE', #39562, #42519, #154753, .T. ) ;
#206588 = DIRECTION ( 'NONE',  ( 1.000000000000000000, 0.000000000000000000, 0.000000000000000000 ) ) ;
#206589 = CARTESIAN_POINT ( 'NONE',  ( -18.50000000000000355, -9.399999999988814636, -107.7972597596633335 ) ) ;
#206591 = EDGE_LOOP ( 'NONE', ( #12216, #134812, #96000, #86067 ) ) ;
#206590 = CARTESIAN_POINT ( 'NONE',  ( 21.72449340488909897, 10.28395627749112151, -20.84999999999999787 ) ) ;
#206592 = DIRECTION ( 'NONE',  ( -1.000000000000000000, -0.000000000000000000, 0.000000000000000000 ) ) ;
#206593 = ORIENTED_EDGE ( 'NONE', *, *, #83693, .T. ) ;
#206594 = EDGE_CURVE ( 'NONE', #163705, #138726, #225445, .T. ) ;
#206595 = CIRCLE ( 'NONE', #90060, 3.999999999999999112 ) ;
#206597 = EDGE_CURVE ( 'NONE', #231873, #252932, #1897, .T. ) ;
#206596 = FACE_OUTER_BOUND ( 'NONE', #165290, .T. ) ;
#206598 = CARTESIAN_POINT ( 'NONE',  ( 22.48970261584622321, 11.65000000001115588, -66.94463051178263413 ) ) ;
#206599 = ADVANCED_FACE ( 'NONE', ( #198830 ), #240534, .T. ) ;
#206600 = CARTESIAN_POINT ( 'NONE',  ( 20.94999999999999929, 77.83585931145570669, -125.0186683157258045 ) ) ;
#206601 = DIRECTION ( 'NONE',  ( -1.000000000000000000, 7.304098846218164250E-16, -4.217023435051628197E-16 ) ) ;
#206602 = EDGE_CURVE ( 'NONE', #253366, #124163, #250777, .T. ) ;
#206603 = ORIENTED_EDGE ( 'NONE', *, *, #56408, .T. ) ;
#206604 = CARTESIAN_POINT ( 'NONE',  ( 20.85000000000000142, 87.75000000001246292, -173.0231074845243029 ) ) ;
#206605 = FACE_OUTER_BOUND ( 'NONE', #119743, .T. ) ;
#206606 = AXIS2_PLACEMENT_3D ( 'NONE', #159372, #216754, #38143 ) ;
#206607 = ORIENTED_EDGE ( 'NONE', *, *, #110891, .T. ) ;
#206608 = AXIS2_PLACEMENT_3D ( 'NONE', #48710, #245640, #46148 ) ;
#206609 = VECTOR ( 'NONE', #251236, 1000.000000000000000 ) ;
#206611 = EDGE_CURVE ( 'NONE', #130418, #74897, #121626, .T. ) ;
#206610 = DIRECTION ( 'NONE',  ( -5.603264701231743991E-32, -7.172728831056617961E-15, 1.000000000000000000 ) ) ;
#206612 = EDGE_CURVE ( 'NONE', #156062, #115699, #188243, .T. ) ;
#206613 = DIRECTION ( 'NONE',  ( 0.000000000000000000, 0.000000000000000000, -1.000000000000000000 ) ) ;
#206614 = PRESENTATION_LAYER_ASSIGNMENT (  '', '', ( #115046 ) ) ;
#206615 = EDGE_LOOP ( 'NONE', ( #257390, #119604, #73298 ) ) ;
#206616 = CARTESIAN_POINT ( 'NONE',  ( 23.14999999999999503, 8.930358663153430854, -211.6945637661233377 ) ) ;
#206617 = ORIENTED_EDGE ( 'NONE', *, *, #83123, .T. ) ;
#206618 = EDGE_CURVE ( 'NONE', #183886, #140937, #30052, .T. ) ;
#206619 = CARTESIAN_POINT ( 'NONE',  ( -13.88555196119804158, 9.457431528860068326, -48.49991693789967684 ) ) ;
#206620 = VERTEX_POINT ( 'NONE', #164856 ) ;
#206621 = CARTESIAN_POINT ( 'NONE',  ( 21.05000000000000071, 11.65000000001116298, -112.6500000000000341 ) ) ;
#206622 = DIRECTION ( 'NONE',  ( -0.000000000000000000, 1.000000000000000000, -0.000000000000000000 ) ) ;
#206623 = ORIENTED_EDGE ( 'NONE', *, *, #233150, .T. ) ;
#206624 = VERTEX_POINT ( 'NONE', #24079 ) ;
#206625 = CARTESIAN_POINT ( 'NONE',  ( 18.54147908293604985, 85.46326165794013718, -129.4741585877683292 ) ) ;
#206627 = ORIENTED_EDGE ( 'NONE', *, *, #221486, .T. ) ;
#206626 = DIRECTION ( 'NONE',  ( -0.000000000000000000, -0.1350103645451876666, -0.9908441862701600211 ) ) ;
#206628 = EDGE_CURVE ( 'NONE', #106788, #103673, #25742, .T. ) ;
#206629 = DIRECTION ( 'NONE',  ( 0.000000000000000000, -0.8103668758649471560, 0.5859227990963360444 ) ) ;
#206631 = ORIENTED_EDGE ( 'NONE', *, *, #195629, .F. ) ;
#206630 = AXIS2_PLACEMENT_3D ( 'NONE', #111412, #90546, #190972 ) ;
#206632 =( BOUNDED_SURFACE ( )  B_SPLINE_SURFACE ( 3, 2, ( 
 ( #13884, #54274, #192522 ),
 ( #56818, #232952, #93404 ),
 ( #136354, #133819, #214632 ),
 ( #213346, #37311, #34755 ) ),
 .UNSPECIFIED., .F., .F., .T. ) 
 B_SPLINE_SURFACE_WITH_KNOTS ( ( 4, 4 ),
 ( 3, 3 ),
 ( -1.734723475976807094E-18, 0.001979672783031532438 ),
 ( 0.000000000000000000, 1.000000000000000000 ),
 .UNSPECIFIED. ) 
 GEOMETRIC_REPRESENTATION_ITEM ( )  RATIONAL_B_SPLINE_SURFACE ( (
 ( 1.000000000000000000, 0.7103081912008197829, 1.000000000000000000),
 ( 1.000000000000000000, 0.7104998333558695256, 1.000000000000000000),
 ( 1.000000000000000000, 0.7107238315755238789, 1.000000000000000000),
 ( 1.000000000000000000, 0.7110073749539377319, 1.000000000000000000) ) ) 
 REPRESENTATION_ITEM ( '' )  SURFACE ( )  );
#206633 = AXIS2_PLACEMENT_3D ( 'NONE', #11296, #32164, #68703 ) ;
#206634 = EDGE_CURVE ( 'NONE', #95314, #104861, #64471, .T. ) ;
#206635 = VERTEX_POINT ( 'NONE', #162296 ) ;
#206636 = TOROIDAL_SURFACE ( 'NONE', #81703, 11.65000000000000036, 0.1000000000000000056 ) ;
#206637 = DIRECTION ( 'NONE',  ( 1.000000000000000000, 7.304098846218134667E-16, 0.000000000000000000 ) ) ;
#206638 = LINE ( 'NONE', #166263, #201149 ) ;
#206640 = ADVANCED_FACE ( 'NONE', ( #146542 ), #194068, .T. ) ;
#206639 = FACE_OUTER_BOUND ( 'NONE', #24750, .T. ) ;
#206641 = AXIS2_PLACEMENT_3D ( 'NONE', #98777, #220053, #242175 ) ;
#206642 = DIRECTION ( 'NONE',  ( -1.000000000000000000, 0.000000000000000000, 0.000000000000000000 ) ) ;
#206643 = VECTOR ( 'NONE', #23609, 1000.000000000000114 ) ;
#206644 = FACE_OUTER_BOUND ( 'NONE', #161737, .T. ) ;
#206645 = EDGE_CURVE ( 'NONE', #18233, #153656, #74757, .T. ) ;
#206646 = DIRECTION ( 'NONE',  ( 1.000000000000000000, 0.000000000000000000, 0.000000000000000000 ) ) ;
#206647 = VERTEX_POINT ( 'NONE', #87851 ) ;
#206648 = CARTESIAN_POINT ( 'NONE',  ( 23.24999999999999289, 64.25000000001202238, -114.7731074845243882 ) ) ;
#206649 = CARTESIAN_POINT ( 'NONE',  ( 20.73486653747088937, 68.25000000001156764, -60.27310748452438105 ) ) ;
#206650 = DIRECTION ( 'NONE',  ( -0.000000000000000000, -0.000000000000000000, -1.000000000000000000 ) ) ;
#206651 = DIRECTION ( 'NONE',  ( 0.000000000000000000, 0.9651348961777157509, -0.2617529984165031243 ) ) ;
#206652 = ORIENTED_EDGE ( 'NONE', *, *, #11210, .T. ) ;
#206653 = CARTESIAN_POINT ( 'NONE',  ( 18.54148534481893762, 10.32532329027886853, -106.0699343018359997 ) ) ;
#206654 = ORIENTED_EDGE ( 'NONE', *, *, #185441, .T. ) ;
#206655 = DIRECTION ( 'NONE',  ( 1.000000000000000000, -6.239415780002328221E-16, -5.674754385112862884E-16 ) ) ;
#206656 = VERTEX_POINT ( 'NONE', #167444 ) ;
#206657 = CIRCLE ( 'NONE', #94220, 0.1000000000000001860 ) ;
#206658 = AXIS2_PLACEMENT_3D ( 'NONE', #114048, #171504, #192324 ) ;
#206659 = VECTOR ( 'NONE', #85562, 1000.000000000000000 ) ;
#206660 = DIRECTION ( 'NONE',  ( 0.000000000000000000, 1.000000000000000000, 6.982962677686266711E-15 ) ) ;
#206661 = PLANE ( 'NONE',  #256233 ) ;
#206662 = EDGE_LOOP ( 'NONE', ( #70454, #121714, #208925, #35075 ) ) ;
#206663 = VERTEX_POINT ( 'NONE', #68324 ) ;
#206665 = ORIENTED_EDGE ( 'NONE', *, *, #210333, .F. ) ;
#206664 = CYLINDRICAL_SURFACE ( 'NONE', #90465, 0.09999999999999911737 ) ;
#206666 = ADVANCED_FACE ( 'NONE', ( #147866 ), #227383, .F. ) ;
#206667 = DIRECTION ( 'NONE',  ( 1.000000000000000000, -0.000000000000000000, -0.000000000000000000 ) ) ;
#206668 = ORIENTED_EDGE ( 'NONE', *, *, #237721, .F. ) ;
#206669 = CIRCLE ( 'NONE', #11037, 0.09999999999998898659 ) ;
#206670 = LINE ( 'NONE', #106258, #147971 ) ;
#206672 = ORIENTED_EDGE ( 'NONE', *, *, #249621, .T. ) ;
#206671 = ADVANCED_FACE ( 'NONE', ( #192139 ), #211701, .T. ) ;
#206673 = DIRECTION ( 'NONE',  ( 1.000000000000000000, 0.000000000000000000, 0.000000000000000000 ) ) ;
#206674 = TOROIDAL_SURFACE ( 'NONE', #244643, 0.2000000000000000111, 0.1000000000000000056 ) ;
#206675 = DIRECTION ( 'NONE',  ( -0.000000000000000000, 0.000000000000000000, -1.000000000000000000 ) ) ;
#206676 = EDGE_LOOP ( 'NONE', ( #187850, #90930, #27135, #234957, #232959 ) ) ;
#206677 = DIRECTION ( 'NONE',  ( 1.734723475976817507E-14, -1.000000000000000000, 0.000000000000000000 ) ) ;
#206678 = EDGE_CURVE ( 'NONE', #146024, #185168, #104812, .T. ) ;
#206679 = CARTESIAN_POINT ( 'NONE',  ( -16.78055652883087134, 22.98605849593701578, -230.9430003731122554 ) ) ;
#206680 = SHAPE_REPRESENTATION ( 'Snap Open Cable Crossbars 6', ( #2425 ), #131439 ) ;
#206681 = CARTESIAN_POINT ( 'NONE',  ( -20.94999999999999929, -11.65000000000000036, -33.50000000000000000 ) ) ;
#206683 = VERTEX_POINT ( 'NONE', #51288 ) ;
#206682 = DIRECTION ( 'NONE',  ( 1.000000000000000000, 0.000000000000000000, 0.000000000000000000 ) ) ;
#206684 = AXIS2_PLACEMENT_3D ( 'NONE', #135075, #155974, #214622 ) ;
#206685 = DIRECTION ( 'NONE',  ( -1.000000000000000000, 2.952720810173289112E-16, 2.061873921506763405E-30 ) ) ;
#206686 = CARTESIAN_POINT ( 'NONE',  ( 18.49999999999999645, 48.14768554360777841, -246.4498133360871179 ) ) ;
#206687 = CIRCLE ( 'NONE', #152567, 0.2000000000000048683 ) ;
#206688 = CARTESIAN_POINT ( 'NONE',  ( -21.45000000000000284, 68.29142135624935861, -124.1731074845243512 ) ) ;
#206690 = DIRECTION ( 'NONE',  ( -1.000000000000000000, -7.304098846218134667E-16, 4.217023435051678980E-16 ) ) ;
#206689 = PLANE ( 'NONE',  #98417 ) ;
#206692 = CIRCLE ( 'NONE', #189942, 0.1000000000000028644 ) ;
#206691 = CARTESIAN_POINT ( 'NONE',  ( 21.05000000000000071, 10.72371710471868056, -108.1649135690876449 ) ) ;
#206693 = AXIS2_PLACEMENT_3D ( 'NONE', #253439, #12299, #250871 ) ;
#206694 = PLANE ( 'NONE',  #27828 ) ;
#206695 = DIRECTION ( 'NONE',  ( 0.000000000000000000, 0.2617529984164506107, 0.9651348961777299618 ) ) ;
#206696 = EDGE_CURVE ( 'NONE', #232157, #241950, #17522, .T. ) ;
#206697 = DIRECTION ( 'NONE',  ( 0.000000000000000000, -1.000000000000000000, 0.000000000000000000 ) ) ;
#206699 = ORIENTED_EDGE ( 'NONE', *, *, #175474, .F. ) ;
#206698 = CIRCLE ( 'NONE', #177701, 0.1000000000000028644 ) ;
#206700 = VERTEX_POINT ( 'NONE', #151738 ) ;
#206701 = ORIENTED_EDGE ( 'NONE', *, *, #233099, .F. ) ;
#206702 = DIRECTION ( 'NONE',  ( 1.000000000000000000, -0.000000000000000000, -0.000000000000000000 ) ) ;
#206703 = AXIS2_PLACEMENT_3D ( 'NONE', #218335, #80090, #202643 ) ;
#206704 = ORIENTED_EDGE ( 'NONE', *, *, #224177, .T. ) ;
#206705 = VECTOR ( 'NONE', #103204, 1000.000000000000000 ) ;
#206706 = CYLINDRICAL_SURFACE ( 'NONE', #32512, 0.09999999999999939493 ) ;
#206707 = DIRECTION ( 'NONE',  ( 0.000000000000000000, 6.982962677686266711E-15, -1.000000000000000000 ) ) ;
#206708 = ORIENTED_EDGE ( 'NONE', *, *, #39337, .F. ) ;
#206709 = CARTESIAN_POINT ( 'NONE',  ( -21.08479644141221598, 6.187248666789188611, -199.5925561729470701 ) ) ;
#206710 = ORIENTED_EDGE ( 'NONE', *, *, #92352, .F. ) ;
#206711 = VERTEX_POINT ( 'NONE', #250798 ) ;
#206712 = CARTESIAN_POINT ( 'NONE',  ( -16.94445028196807002, 66.00793639031378746, -48.63043766294283898 ) ) ;
#206713 = DIRECTION ( 'NONE',  ( 4.504528286903032433E-15, 0.3848449534832963370, 0.9229812358755945523 ) ) ;
#206714 = ORIENTED_EDGE ( 'NONE', *, *, #215351, .F. ) ;
#206715 = CIRCLE ( 'NONE', #111048, 0.09999999999999961697 ) ;
#206716 = DIRECTION ( 'NONE',  ( -1.000000000000000000, 0.000000000000000000, 0.000000000000000000 ) ) ;
#206718 = ORIENTED_EDGE ( 'NONE', *, *, #132986, .F. ) ;
#206717 = FACE_OUTER_BOUND ( 'NONE', #27022, .T. ) ;
#206719 = CARTESIAN_POINT ( 'NONE',  ( -23.15000000000000213, 85.00000000001251976, -179.9170766071767389 ) ) ;
#206720 = DIRECTION ( 'NONE',  ( 0.000000000000000000, 1.000000000000000000, 6.982962677686266711E-15 ) ) ;
#206722 = EDGE_LOOP ( 'NONE', ( #129727, #255484, #238804, #153029, #169494, #4817, #216594, #230319, #144841 ) ) ;
#206721 = CYLINDRICAL_SURFACE ( 'NONE', #18933, 2.000000000000003109 ) ;
#206723 = FACE_OUTER_BOUND ( 'NONE', #140347, .T. ) ;
#206724 = CARTESIAN_POINT ( 'NONE',  ( -22.16821283564876666, 33.56853718381600515, -242.6527871905703648 ) ) ;
#206725 = EDGE_CURVE ( 'NONE', #109819, #54257, #229937, .T. ) ;
#206726 = CARTESIAN_POINT ( 'NONE',  ( -21.45000000000000284, 12.03275902784684703, -220.0251779199349187 ) ) ;
#206728 = CARTESIAN_POINT ( 'NONE',  ( 20.97462148592277842, 8.874737576461731337, -179.7546443317309866 ) ) ;
#206727 = FACE_OUTER_BOUND ( 'NONE', #219144, .T. ) ;
#206729 = CARTESIAN_POINT ( 'NONE',  ( -23.15000000000000213, 4.350000000011156054, -179.8499999999999943 ) ) ;
#206730 = CARTESIAN_POINT ( 'NONE',  ( -18.59999999999999787, 0.6656436123793491033, -212.6810495496487476 ) ) ;
#206731 = AXIS2_PLACEMENT_3D ( 'NONE', #80046, #160926, #219583 ) ;
#206732 = VECTOR ( 'NONE', #183339, 1000.000000000000227 ) ;
#206733 = LINE ( 'NONE', #127202, #205716 ) ;
#206734 = CIRCLE ( 'NONE', #219198, 0.1000000000000033362 ) ;
#206736 = LINE ( 'NONE', #82900, #176115 ) ;
#206735 = AXIS2_PLACEMENT_3D ( 'NONE', #54400, #75281, #11447 ) ;
#206737 = VERTEX_POINT ( 'NONE', #231266 ) ;
#206738 = ORIENTED_EDGE ( 'NONE', *, *, #200506, .F. ) ;
#206739 = ORIENTED_EDGE ( 'NONE', *, *, #110923, .F. ) ;
#206740 = LINE ( 'NONE', #5948, #147299 ) ;
#206741 = ORIENTED_EDGE ( 'NONE', *, *, #1666, .T. ) ;
#206742 = CARTESIAN_POINT ( 'NONE',  ( -23.15000000000000213, -9.599999999988847676, -110.3939691226524786 ) ) ;
#206743 = ORIENTED_EDGE ( 'NONE', *, *, #47547, .F. ) ;
#206744 = EDGE_CURVE ( 'NONE', #72101, #109375, #21647, .T. ) ;
#206745 = DIRECTION ( 'NONE',  ( 0.000000000000000000, 0.2128009952263603954, -0.9770955615653315052 ) ) ;
#206746 = CARTESIAN_POINT ( 'NONE',  ( -18.44085059012131822, 16.40865159970219267, -222.2349014206415916 ) ) ;
#206747 = ADVANCED_FACE ( 'NONE', ( #90432 ), #134055, .T. ) ;
#206748 = ORIENTED_EDGE ( 'NONE', *, *, #177489, .T. ) ;
#206749 = AXIS2_PLACEMENT_3D ( 'NONE', #256105, #20144, #158396 ) ;
#206750 = CARTESIAN_POINT ( 'NONE',  ( -21.05000000000000071, 87.75000000001173817, -72.62310748452422615 ) ) ;
#206751 = AXIS2_PLACEMENT_3D ( 'NONE', #220259, #59856, #258036 ) ;
#206752 = AXIS2_PLACEMENT_3D ( 'NONE', #178751, #224242, #123882 ) ;
#206753 = EDGE_CURVE ( 'NONE', #227593, #86031, #238104, .T. ) ;
#206754 = EDGE_LOOP ( 'NONE', ( #12911, #15580, #31549, #136560, #114923, #152289, #10141, #173970, #100377, #30985, #87967, #153558 ) ) ;
#206755 = ORIENTED_EDGE ( 'NONE', *, *, #73778, .F. ) ;
#206756 = ORIENTED_EDGE ( 'NONE', *, *, #239243, .T. ) ;
#206757 = ADVANCED_FACE ( 'NONE', ( #89152 ), #35648, .T. ) ;
#206758 = CARTESIAN_POINT ( 'NONE',  ( 23.15000000000000213, -9.499999999988844479, -157.6060308773475640 ) ) ;
#206759 = FACE_OUTER_BOUND ( 'NONE', #155529, .T. ) ;
#206760 = CIRCLE ( 'NONE', #23819, 0.1000000000000002554 ) ;
#206761 = CARTESIAN_POINT ( 'NONE',  ( -23.15000000000000213, 5.900000000011162093, -123.7809002353436654 ) ) ;
#206763 = EDGE_CURVE ( 'NONE', #125626, #208807, #6343, .T. ) ;
#206762 = DIRECTION ( 'NONE',  ( 1.000000000000000000, 0.000000000000000000, 0.000000000000000000 ) ) ;
#206764 = DIRECTION ( 'NONE',  ( 0.000000000000000000, 0.000000000000000000, -1.000000000000000000 ) ) ;
#206765 = DIRECTION ( 'NONE',  ( 1.000000000000000000, 0.000000000000000000, 0.000000000000000000 ) ) ;
#206767 = PLANE ( 'NONE',  #145127 ) ;
#206766 = CARTESIAN_POINT ( 'NONE',  ( -22.47071067811865319, 76.00000000001213607, -136.5231074845242745 ) ) ;
#206768 = DIRECTION ( 'NONE',  ( 0.000000000000000000, 0.000000000000000000, 1.000000000000000000 ) ) ;
#206770 = ORIENTED_EDGE ( 'NONE', *, *, #121612, .T. ) ;
#206769 = CARTESIAN_POINT ( 'NONE',  ( -20.94999999999999929, 10.29270135741298731, -139.4573618871519614 ) ) ;
#206772 = DIRECTION ( 'NONE',  ( 1.000000000000000000, 0.000000000000000000, 0.000000000000000000 ) ) ;
#206771 = CARTESIAN_POINT ( 'NONE',  ( 20.84451136049631259, 10.62014191481791059, -74.49392455952968817 ) ) ;
#206773 = EDGE_CURVE ( 'NONE', #71417, #186223, #253369, .T. ) ;
#206774 = CARTESIAN_POINT ( 'NONE',  ( -20.64999999999999858, 85.00000000001232081, -160.1291383618718385 ) ) ;
#206775 = EDGE_LOOP ( 'NONE', ( #69940, #198013, #140171, #3672 ) ) ;
#206776 = CARTESIAN_POINT ( 'NONE',  ( 20.93284271247462414, 11.75000000001116085, -160.4851942293460638 ) ) ;
#206777 = DIRECTION ( 'NONE',  ( 0.7071359030027766224, -0.7070776581709024011, 0.000000000000000000 ) ) ;
#206778 = DIRECTION ( 'NONE',  ( 1.000000000000000000, 0.000000000000000000, 0.000000000000000000 ) ) ;
#206779 = ORIENTED_EDGE ( 'NONE', *, *, #68709, .F. ) ;
#206780 = EDGE_CURVE ( 'NONE', #197206, #18414, #85872, .T. ) ;
#206781 = CARTESIAN_POINT ( 'NONE',  ( -16.80468759584940486, 60.95740558621518090, -221.0051579303695917 ) ) ;
#206782 = CIRCLE ( 'NONE', #123574, 0.09999999999999986677 ) ;
#206783 = DIRECTION ( 'NONE',  ( 0.000000000000000000, 0.9667078373770138233, 0.2558827019434041783 ) ) ;
#206784 = DIRECTION ( 'NONE',  ( 0.000000000000000000, 1.000000000000000000, 6.853228547068871147E-15 ) ) ;
#206785 = ORIENTED_EDGE ( 'NONE', *, *, #225438, .T. ) ;
#206786 = EDGE_LOOP ( 'NONE', ( #228666, #152764, #231510, #145405 ) ) ;
#206787 = CARTESIAN_POINT ( 'NONE',  ( 22.60000000000000142, 11.74956712350054744, -133.8991416309013118 ) ) ;
#206788 = EDGE_LOOP ( 'NONE', ( #66842, #109183, #6571, #68845 ) ) ;
#206789 = CARTESIAN_POINT ( 'NONE',  ( -18.33682934331484304, -9.511185591082512047, -174.4056547686735428 ) ) ;
#206790 = CARTESIAN_POINT ( 'NONE',  ( 18.41416235934318379, 85.50000000001169553, -62.92291809330222208 ) ) ;
#206791 = CARTESIAN_POINT ( 'NONE',  ( -20.94999999999999929, 10.29288807859936661, -206.4580020160121592 ) ) ;
#206792 = ORIENTED_EDGE ( 'NONE', *, *, #227452, .T. ) ;
#206793 = CIRCLE ( 'NONE', #165688, 11.74999999999999467 ) ;
#206794 = EDGE_CURVE ( 'NONE', #45686, #65351, #73486, .T. ) ;
#206795 = CARTESIAN_POINT ( 'NONE',  ( -15.75000000000001066, 9.350000000011142731, -117.3642676076161706 ) ) ;
#206796 = DIRECTION ( 'NONE',  ( 1.000000000000000000, 0.000000000000000000, 0.000000000000000000 ) ) ;
#206797 = AXIS2_PLACEMENT_3D ( 'NONE', #116719, #55427, #33375 ) ;
#206798 = CARTESIAN_POINT ( 'NONE',  ( 18.59999999999999076, 10.49142135624846617, -192.2499999999999716 ) ) ;
#206799 = CARTESIAN_POINT ( 'NONE',  ( 21.05000000000000071, 8.776282895303632259, -42.05862899514094977 ) ) ;
#206800 = CIRCLE ( 'NONE', #177779, 0.09999999999999939493 ) ;
#206801 = CIRCLE ( 'NONE', #244193, 0.1000000000000028644 ) ;
#206802 = ORIENTED_EDGE ( 'NONE', *, *, #99311, .T. ) ;
#206803 = CARTESIAN_POINT ( 'NONE',  ( 20.85882249326303040, 10.33248238082519066, -39.09484654391314962 ) ) ;
#206804 = AXIS2_PLACEMENT_3D ( 'NONE', #227005, #245298, #125348 ) ;
#206805 = EDGE_CURVE ( 'NONE', #96904, #44045, #50840, .T. ) ;
#206807 = ORIENTED_EDGE ( 'NONE', *, *, #249604, .F. ) ;
#206806 = DIRECTION ( 'NONE',  ( -1.000000000000000000, 0.000000000000000000, -0.000000000000000000 ) ) ;
#206808 = FACE_OUTER_BOUND ( 'NONE', #181358, .T. ) ;
#206809 = CYLINDRICAL_SURFACE ( 'NONE', #159948, 0.09999999999998898659 ) ;
#206810 = DIRECTION ( 'NONE',  ( 0.000000000000000000, 0.4721928772780015771, 0.8814952561687000587 ) ) ;
#206811 = CARTESIAN_POINT ( 'NONE',  ( -20.54999999999999716, 2.400000000011155432, -57.10603087734755690 ) ) ;
#206812 = DIRECTION ( 'NONE',  ( 1.186688945009010077E-16, -1.000000000000000000, -0.000000000000000000 ) ) ;
#206813 = CARTESIAN_POINT ( 'NONE',  ( -23.15000000000000213, 54.36465331297785042, -236.8526523779771082 ) ) ;
#206814 = ORIENTED_EDGE ( 'NONE', *, *, #43737, .F. ) ;
#206815 = DIRECTION ( 'NONE',  ( 0.000000000000000000, 0.9908441862701420355, 0.1350103645453197554 ) ) ;
#206816 = CARTESIAN_POINT ( 'NONE',  ( 15.74999999999999645, 13.18880795147152618, -215.2702608532411830 ) ) ;
#206817 = CARTESIAN_POINT ( 'NONE',  ( -6.100000000000004086, -11.65000000000000036, 10.10000000000000142 ) ) ;
#206818 = EDGE_CURVE ( 'NONE', #106358, #91629, #154325, .T. ) ;
#206819 = AXIS2_PLACEMENT_3D ( 'NONE', #211632, #134626, #253303 ) ;
#206820 = DIRECTION ( 'NONE',  ( 1.000000000000000000, 0.000000000000000000, -0.000000000000000000 ) ) ;
#206821 = EDGE_CURVE ( 'NONE', #91602, #228089, #120328, .T. ) ;
#206822 = ORIENTED_EDGE ( 'NONE', *, *, #16825, .T. ) ;
#206823 = ORIENTED_EDGE ( 'NONE', *, *, #189432, .T. ) ;
#206824 = DIRECTION ( 'NONE',  ( 1.000000000000000000, 0.000000000000000000, 0.000000000000000000 ) ) ;
#206825 = CIRCLE ( 'NONE', #94378, 0.1000000000000012407 ) ;
#206826 = CARTESIAN_POINT ( 'NONE',  ( 22.00356870068456061, 9.582273870969723154E-12, -126.7457576382395388 ) ) ;
#206827 = VECTOR ( 'NONE', #36293, 1000.000000000000000 ) ;
#206828 = EDGE_CURVE ( 'NONE', #197443, #132227, #58993, .T. ) ;
#206829 = LINE ( 'NONE', #24363, #122416 ) ;
#206830 = CIRCLE ( 'NONE', #77614, 11.65000000000000036 ) ;
#206831 = AXIS2_PLACEMENT_3D ( 'NONE', #29388, #188415, #9777 ) ;
#206832 = CARTESIAN_POINT ( 'NONE',  ( -16.97683809663752186, 9.950000000011138823, -187.5976359818036485 ) ) ;
#206833 = EDGE_CURVE ( 'NONE', #226065, #154105, #109110, .T. ) ;
#206835 = EDGE_CURVE ( 'NONE', #130308, #149929, #225622, .T. ) ;
#206834 = CARTESIAN_POINT ( 'NONE',  ( -20.64999999999999858, 4.350000000011156054, -146.2500000000000284 ) ) ;
#206836 = CARTESIAN_POINT ( 'NONE',  ( 23.15000000000000213, 28.42524210734032408, -258.3567845160494585 ) ) ;
#206837 = CIRCLE ( 'NONE', #223569, 0.1000000000000002554 ) ;
#206838 = VECTOR ( 'NONE', #209011, 1000.000000000000000 ) ;
#206839 = ORIENTED_EDGE ( 'NONE', *, *, #171534, .F. ) ;
#206841 = DIRECTION ( 'NONE',  ( -0.000000000000000000, 6.982962677686266711E-15, -1.000000000000000000 ) ) ;
#206840 = AXIS2_PLACEMENT_3D ( 'NONE', #15068, #94583, #95859 ) ;
#206842 = EDGE_CURVE ( 'NONE', #21323, #214500, #113214, .T. ) ;
#206843 = ORIENTED_EDGE ( 'NONE', *, *, #172178, .F. ) ;
#206844 = FACE_OUTER_BOUND ( 'NONE', #158626, .T. ) ;
#206845 = LINE ( 'NONE', #103864, #99469 ) ;
#206846 = CARTESIAN_POINT ( 'NONE',  ( 21.07199075132371746, 8.774944999127242795, -79.21353216161290334 ) ) ;
#206847 = CARTESIAN_POINT ( 'NONE',  ( 21.00000000000000000, 9.750000000011153745, -146.3500000000000227 ) ) ;
#206848 = CARTESIAN_POINT ( 'NONE',  ( 18.49999999999999645, 1.115600667400684642E-11, -67.00000000000000000 ) ) ;
#206849 = CARTESIAN_POINT ( 'NONE',  ( -18.45037301276663300, -9.490200447541971229, -7.012674136414320358 ) ) ;
#206850 = CARTESIAN_POINT ( 'NONE',  ( -16.92209698673680052, 66.05000000001182059, -82.23374305157656750 ) ) ;
#206851 = ORIENTED_EDGE ( 'NONE', *, *, #207604, .T. ) ;
#206852 = CARTESIAN_POINT ( 'NONE',  ( -16.94309007106718212, 22.95903659219989024, -230.8769661811952290 ) ) ;
#206853 = DIRECTION ( 'NONE',  ( -1.000000000000000000, -0.000000000000000000, -0.000000000000000000 ) ) ;
#206854 = DIRECTION ( 'NONE',  ( 0.000000000000000000, -0.9126074666063660468, -0.4088369013363524762 ) ) ;
#206855 = AXIS2_PLACEMENT_3D ( 'NONE', #89602, #169187, #34809 ) ;
#206856 = DIRECTION ( 'NONE',  ( -1.000000000000000000, 0.000000000000000000, 0.000000000000000000 ) ) ;
#206857 = DIRECTION ( 'NONE',  ( 0.000000000000000000, 0.000000000000000000, -1.000000000000000000 ) ) ;
#206858 = CARTESIAN_POINT ( 'NONE',  ( 21.05000000000000071, 8.876614585098257848, -175.8850804788446567 ) ) ;
#206859 = ORIENTED_EDGE ( 'NONE', *, *, #216233, .T. ) ;
#206860 = DIRECTION ( 'NONE',  ( 0.000000000000000000, -6.608470384673580212E-15, 1.000000000000000000 ) ) ;
#206861 = CARTESIAN_POINT ( 'NONE',  ( -23.25000000000000000, 76.00000000001267608, -203.5231074845243597 ) ) ;
#206862 = ORIENTED_EDGE ( 'NONE', *, *, #15470, .T. ) ;
#206863 = EDGE_CURVE ( 'NONE', #239256, #248313, #159046, .T. ) ;
#206864 = ADVANCED_FACE ( 'NONE', ( #16080 ), #84119, .T. ) ;
#206865 = VERTEX_POINT ( 'NONE', #325 ) ;
#206866 = DIRECTION ( 'NONE',  ( 0.000000000000000000, 0.008583690987127625890, 0.9999631594459055250 ) ) ;
#206867 = FACE_OUTER_BOUND ( 'NONE', #142420, .T. ) ;
#206868 = AXIS2_PLACEMENT_3D ( 'NONE', #156953, #213043, #38273 ) ;
#206869 = CIRCLE ( 'NONE', #98485, 0.09999999999999939493 ) ;
#206870 = CARTESIAN_POINT ( 'NONE',  ( -20.94999999999999929, -11.64999999998884306, -70.10000000000005116 ) ) ;
#206871 = ORIENTED_EDGE ( 'NONE', *, *, #180210, .T. ) ;
#206873 = TOROIDAL_SURFACE ( 'NONE', #227704, 12.77500000000000036, 0.1000000000000000056 ) ;
#206872 = CARTESIAN_POINT ( 'NONE',  ( 18.43630871534866955, -9.679800874791860466, -174.1606320679840394 ) ) ;
#206874 = CARTESIAN_POINT ( 'NONE',  ( 23.25000000000000000, -9.599999999988849453, -21.75000000000000355 ) ) ;
#206875 = AXIS2_PLACEMENT_3D ( 'NONE', #181112, #201945, #218917 ) ;
#206876 = EDGE_CURVE ( 'NONE', #208477, #121217, #117505, .T. ) ;
#206877 = ORIENTED_EDGE ( 'NONE', *, *, #85558, .F. ) ;
#206878 = AXIS2_PLACEMENT_3D ( 'NONE', #180072, #58801, #137083 ) ;
#206879 = DIRECTION ( 'NONE',  ( 0.000000000000000000, 0.000000000000000000, 1.000000000000000000 ) ) ;
#206880 = ORIENTED_EDGE ( 'NONE', *, *, #145008, .F. ) ;
#206881 = CARTESIAN_POINT ( 'NONE',  ( 23.14999999999999503, 11.75000000001115552, -54.75000000000000000 ) ) ;
#206883 = AXIS2_PLACEMENT_3D ( 'NONE', #167325, #143867, #142577 ) ;
#206882 = CARTESIAN_POINT ( 'NONE',  ( -20.64999999999999858, 61.88149656937975607, -248.1136133839584090 ) ) ;
#206884 = DIRECTION ( 'NONE',  ( -0.000000000000000000, -1.000000000000000000, -0.000000000000000000 ) ) ;
#206886 = UNCERTAINTY_MEASURE_WITH_UNIT (LENGTH_MEASURE( 1.000000000000000082E-05 ), #169016, 'distance_accuracy_value', 'NONE');
#206885 = PLANE ( 'NONE',  #178435 ) ;
#206887 = DIRECTION ( 'NONE',  ( -1.836970198721029441E-16, 0.4721928772777346239, 0.8814952561688430555 ) ) ;
#206888 = VECTOR ( 'NONE', #249057, 1000.000000000000000 ) ;
#206889 = CARTESIAN_POINT ( 'NONE',  ( -23.15000000000000213, 76.00000000001229239, -157.2481074845243540 ) ) ;
#206890 = CARTESIAN_POINT ( 'NONE',  ( -16.79814274880124358, 66.05072745733529871, -190.8706744474764321 ) ) ;
#206891 = AXIS2_PLACEMENT_3D ( 'NONE', #194036, #153662, #171921 ) ;
#206892 = CARTESIAN_POINT ( 'NONE',  ( 18.79999999999999361, -11.75000000000000000, -15.00000000000000000 ) ) ;
#206893 = DIRECTION ( 'NONE',  ( 0.000000000000000000, 0.01562499999998609446, -0.9998779222360101304 ) ) ;
#206895 = ORIENTED_EDGE ( 'NONE', *, *, #158184, .T. ) ;
#206894 = DIRECTION ( 'NONE',  ( 0.000000000000000000, -7.116814260417668513E-15, 1.000000000000000000 ) ) ;
#206896 = ORIENTED_EDGE ( 'NONE', *, *, #192386, .T. ) ;
#206898 = CARTESIAN_POINT ( 'NONE',  ( -13.54036565897074773, 9.451541661396667848, -85.45387549883064082 ) ) ;
#206897 = DIRECTION ( 'NONE',  ( 0.000000000000000000, 0.000000000000000000, -1.000000000000000000 ) ) ;
#206900 = ORIENTED_EDGE ( 'NONE', *, *, #178964, .F. ) ;
#206899 = CARTESIAN_POINT ( 'NONE',  ( -18.50000000000000000, 0.000000000000000000, -33.50000000000000000 ) ) ;
#206901 = B_SPLINE_CURVE_WITH_KNOTS ( 'NONE', 3,
 ( #60096, #114952, #57524, #254434, #79654, #95389, #90560, #135782, #137082, #216614, #139623, #40590, #116253, #237469, #118819, #78379, #96637, #17159, #255697 ),
 .UNSPECIFIED., .F., .F.,
 ( 4, 3, 3, 3, 3, 3, 4 ),
 ( 0.0001624081864585664764, 0.0001685232196531825368, 0.0001764526673566942224, 0.0001916878551483208173, 0.0002009890782182613455, 0.0002238845907555189795, 0.0002283406619926576847 ),
 .UNSPECIFIED. ) ;
#206902 = EDGE_CURVE ( 'NONE', #6267, #221894, #18812, .T. ) ;
#206903 = ORIENTED_EDGE ( 'NONE', *, *, #85416, .T. ) ;
#206904 = DIRECTION ( 'NONE',  ( -0.000000000000000000, 0.000000000000000000, -1.000000000000000000 ) ) ;
#206905 = DIRECTION ( 'NONE',  ( -4.239556034732056743E-17, 0.1298341882520022694, 0.9915357197604853789 ) ) ;
#206906 = DIRECTION ( 'NONE',  ( 0.000000000000000000, -1.000000000000000000, 0.000000000000000000 ) ) ;
#206907 = EDGE_CURVE ( 'NONE', #102268, #132210, #192333, .T. ) ;
#206908 = DIRECTION ( 'NONE',  ( -1.000000000000000000, 0.000000000000000000, -0.000000000000000000 ) ) ;
#206909 = CARTESIAN_POINT ( 'NONE',  ( -17.11825945287482753, 44.09459801588531036, -235.2076708599468020 ) ) ;
#206910 = ADVANCED_FACE ( 'NONE', ( #76019 ), #56440, .F. ) ;
#206911 = DIRECTION ( 'NONE',  ( 0.000000000000000000, 0.9770955615653316162, 0.2128009952263604232 ) ) ;
#206912 = ORIENTED_EDGE ( 'NONE', *, *, #159758, .T. ) ;
#206913 = VERTEX_POINT ( 'NONE', #57725 ) ;
#206914 = EDGE_CURVE ( 'NONE', #171420, #21650, #79871, .T. ) ;
#206915 = CARTESIAN_POINT ( 'NONE',  ( -20.94999999999999929, 1.115600667400684642E-11, -67.00000000000000000 ) ) ;
#206916 = CIRCLE ( 'NONE', #131905, 11.65000000000000036 ) ;
#206917 = AXIS2_PLACEMENT_3D ( 'NONE', #57624, #175071, #74678 ) ;
#206918 = VERTEX_POINT ( 'NONE', #181562 ) ;
#206919 = VECTOR ( 'NONE', #80182, 1000.000000000000000 ) ;
#206921 = DIRECTION ( 'NONE',  ( 0.000000000000000000, 6.982962677686266711E-15, -1.000000000000000000 ) ) ;
#206920 = AXIS2_PLACEMENT_3D ( 'NONE', #202288, #103162, #242681 ) ;
#206922 = EDGE_LOOP ( 'NONE', ( #151066, #2558, #101804, #18088 ) ) ;
#206923 = CARTESIAN_POINT ( 'NONE',  ( 23.14999999999999503, 69.45000000001229523, -157.6731074845243938 ) ) ;
#206924 = EDGE_CURVE ( 'NONE', #6279, #116117, #213167, .T. ) ;
#206926 = ADVANCED_FACE ( 'NONE', ( #204936 ), #25062, .F. ) ;
#206925 = EDGE_CURVE ( 'NONE', #236242, #152148, #68009, .T. ) ;
#206927 = DIRECTION ( 'NONE',  ( -1.000000000000000000, 0.000000000000000000, -0.000000000000000000 ) ) ;
#206928 = DIRECTION ( 'NONE',  ( -1.000000000000000000, 0.000000000000000000, 0.000000000000000000 ) ) ;
#206929 = EDGE_LOOP ( 'NONE', ( #197775, #153985, #248631, #245912 ) ) ;
#206930 = LINE ( 'NONE', #184790, #242101 ) ;
#206931 = ORIENTED_EDGE ( 'NONE', *, *, #237462, .T. ) ;
#206932 = CARTESIAN_POINT ( 'NONE',  ( -20.54999999999999716, 4.389020526555173163, -221.1525959572864792 ) ) ;
#206933 = CARTESIAN_POINT ( 'NONE',  ( -20.85000000000000142, 77.83585931145546510, -91.51866831572576189 ) ) ;
#206934 = FACE_OUTER_BOUND ( 'NONE', #127205, .T. ) ;
#206935 = CYLINDRICAL_SURFACE ( 'NONE', #3266, 0.1000000000000028644 ) ;
#206936 = VERTEX_POINT ( 'NONE', #244071 ) ;
#206937 = AXIS2_PLACEMENT_3D ( 'NONE', #253909, #75318, #234351 ) ;
#206939 = DIRECTION ( 'NONE',  ( -2.940209281316620030E-16, -0.9651348961777150848, 0.2617529984165054002 ) ) ;
#206938 = AXIS2_PLACEMENT_3D ( 'NONE', #26587, #89101, #248188 ) ;
#206940 = ORIENTED_EDGE ( 'NONE', *, *, #119763, .F. ) ;
#206943 = ORIENTED_EDGE ( 'NONE', *, *, #90782, .T. ) ;
#206942 = SPHERICAL_SURFACE ( 'NONE', #13947, 0.1000000000000000056 ) ;
#206941 = CARTESIAN_POINT ( 'NONE',  ( 18.39999999999998792, 46.93054509580814226, -255.3593361228639367 ) ) ;
#206944 = EDGE_CURVE ( 'NONE', #13609, #117897, #200715, .T. ) ;
#206945 = CARTESIAN_POINT ( 'NONE',  ( -20.94999999999999929, -11.64999999998884483, -134.0000000000000284 ) ) ;
#206946 = EDGE_CURVE ( 'NONE', #25682, #206663, #55116, .T. ) ;
#206947 = ORIENTED_EDGE ( 'NONE', *, *, #153466, .F. ) ;
#206948 = DIRECTION ( 'NONE',  ( 0.000000000000000000, 6.982962677686266711E-15, -1.000000000000000000 ) ) ;
#206949 = AXIS2_PLACEMENT_3D ( 'NONE', #120656, #241857, #41120 ) ;
#206950 = VERTEX_POINT ( 'NONE', #26328 ) ;
#206951 = EDGE_CURVE ( 'NONE', #87151, #20839, #200885, .T. ) ;
#206952 = CARTESIAN_POINT ( 'NONE',  ( 20.85000000000000142, 6.846123162352588665, -37.23772626684986164 ) ) ;
#206953 = CARTESIAN_POINT ( 'NONE',  ( 20.94999999999999929, 36.65892442174935439, -249.5511627012433848 ) ) ;
#206954 = DIRECTION ( 'NONE',  ( 0.000000000000000000, 0.000000000000000000, 1.000000000000000000 ) ) ;
#206955 = EDGE_CURVE ( 'NONE', #7750, #3198, #159218, .T. ) ;
#206956 = EDGE_LOOP ( 'NONE', ( #230344, #123361, #235686, #200220 ) ) ;
#206958 = EDGE_CURVE ( 'NONE', #137562, #187441, #134238, .T. ) ;
#206957 = DIRECTION ( 'NONE',  ( -1.000000000000000000, 0.000000000000000000, -0.000000000000000000 ) ) ;
#206959 = CARTESIAN_POINT ( 'NONE',  ( -16.87372397896795917, 13.98494438218169655, -218.7820011785657925 ) ) ;
#206960 = FACE_OUTER_BOUND ( 'NONE', #192287, .T. ) ;
#206961 = ORIENTED_EDGE ( 'NONE', *, *, #192488, .F. ) ;
#206962 = DIRECTION ( 'NONE',  ( 1.000000000000000000, -0.000000000000000000, -0.000000000000000000 ) ) ;
#206963 = EDGE_LOOP ( 'NONE', ( #153354, #231469, #150361, #203259, #105443, #204599 ) ) ;
#206964 = CARTESIAN_POINT ( 'NONE',  ( 21.07946286933444924, 30.85164652312839451, -252.0687244592667469 ) ) ;
#206965 = DIRECTION ( 'NONE',  ( -1.000000000000000000, 0.000000000000000000, -0.000000000000000000 ) ) ;
#206966 = CARTESIAN_POINT ( 'NONE',  ( -21.00000000000000000, 8.000000000000000000, -1.212568896937008089 ) ) ;
#206968 = ORIENTED_EDGE ( 'NONE', *, *, #228149, .T. ) ;
#206967 = CARTESIAN_POINT ( 'NONE',  ( -16.79270642812330294, 44.14711678134324302, -235.2978346781722223 ) ) ;
#206969 = EDGE_CURVE ( 'NONE', #214712, #41600, #43323, .T. ) ;
#206970 = CARTESIAN_POINT ( 'NONE',  ( -18.50000000000000000, 11.65000000001115232, -88.35000000000003695 ) ) ;
#206971 = VECTOR ( 'NONE', #190787, 1000.000000000000000 ) ;
#206972 = CARTESIAN_POINT ( 'NONE',  ( -23.15000000000000213, 1.115650265596050101E-11, -163.4499999999999886 ) ) ;
#206973 = CARTESIAN_POINT ( 'NONE',  ( -23.25000000000000000, 54.36465331297785042, -236.8526523779771082 ) ) ;
#206974 = ORIENTED_EDGE ( 'NONE', *, *, #135049, .T. ) ;
#206975 = CIRCLE ( 'NONE', #44670, 0.1000000000000076245 ) ;
#206976 = ADVANCED_FACE ( 'NONE', ( #42050 ), #143690, .F. ) ;
#206977 = DIRECTION ( 'NONE',  ( 0.000000000000000000, 1.000000000000000000, 0.000000000000000000 ) ) ;
#206978 = DIRECTION ( 'NONE',  ( -0.000000000000000000, 1.000000000000000000, 6.352154140967427193E-15 ) ) ;
#206979 = ORIENTED_EDGE ( 'NONE', *, *, #127447, .T. ) ;
#206980 = CARTESIAN_POINT ( 'NONE',  ( 20.94999999999999929, 20.02733907826963033, -235.1395327601354666 ) ) ;
#206981 = VECTOR ( 'NONE', #105650, 999.9999999999998863 ) ;
#206982 = CIRCLE ( 'NONE', #223530, 0.09999999999999939493 ) ;
#206983 = ORIENTED_EDGE ( 'NONE', *, *, #47606, .T. ) ;
#206984 = AXIS2_PLACEMENT_3D ( 'NONE', #79765, #178936, #156799 ) ;
#206985 = DIRECTION ( 'NONE',  ( 0.000000000000000000, -0.9651348961777157509, 0.2617529984165032353 ) ) ;
#206988 = ORIENTED_EDGE ( 'NONE', *, *, #125434, .F. ) ;
#206987 = CARTESIAN_POINT ( 'NONE',  ( -22.59999999999999787, 64.05844819680034163, -247.1686437718134073 ) ) ;
#206986 = VECTOR ( 'NONE', #144766, 1000.000000000000000 ) ;
#206989 = EDGE_CURVE ( 'NONE', #76432, #89464, #64166, .T. ) ;
#206990 = AXIS2_PLACEMENT_3D ( 'NONE', #77839, #37461, #175691 ) ;
#206993 = ORIENTED_EDGE ( 'NONE', *, *, #244258, .F. ) ;
#206992 = VERTEX_POINT ( 'NONE', #4176 ) ;
#206991 = DIRECTION ( 'NONE',  ( -1.073024830501117725E-15, 6.982962677686266711E-15, -1.000000000000000000 ) ) ;
#206994 = CARTESIAN_POINT ( 'NONE',  ( 20.94999999999999574, -10.56629024491939894, -206.4738935375009703 ) ) ;
#206995 = CARTESIAN_POINT ( 'NONE',  ( -21.14999999999999858, 44.10931966560507789, -259.0886734199950183 ) ) ;
#206996 = LINE ( 'NONE', #109158, #106557 ) ;
#206998 = DIRECTION ( 'NONE',  ( -1.000000000000000000, 0.000000000000000000, 0.000000000000000000 ) ) ;
#206997 = CARTESIAN_POINT ( 'NONE',  ( 22.47809213839789066, 0.03753706763967752658, -88.85002666521222636 ) ) ;
#206999 = LINE ( 'NONE', #165301, #215422 ) ;
#207000 = TOROIDAL_SURFACE ( 'NONE', #77991, 11.65000000000000036, 0.1000000000000000056 ) ;
#207001 = CARTESIAN_POINT ( 'NONE',  ( -20.94999999999999929, 68.97833521811179480, -99.38954208262707368 ) ) ;
#207002 = CARTESIAN_POINT ( 'NONE',  ( 0.8999999999999993561, -8.250000000000005329, 23.40000000000000568 ) ) ;
#207003 = AXIS2_PLACEMENT_3D ( 'NONE', #67447, #251208, #226502 ) ;
#207004 = ORIENTED_EDGE ( 'NONE', *, *, #55725, .F. ) ;
#207005 = ORIENTED_EDGE ( 'NONE', *, *, #222088, .T. ) ;
#207007 = CARTESIAN_POINT ( 'NONE',  ( -21.04999999999999716, 64.25000000001175238, -76.36470817442145176 ) ) ;
#207006 = VECTOR ( 'NONE', #118838, 1000.000000000000000 ) ;
#207009 = ORIENTED_EDGE ( 'NONE', *, *, #251336, .F. ) ;
#207008 = CARTESIAN_POINT ( 'NONE',  ( -20.64999999999999858, 74.07476635515199348, -82.25335101765045920 ) ) ;
#207010 = CIRCLE ( 'NONE', #73762, 0.1000000000000024342 ) ;
#207011 = ORIENTED_EDGE ( 'NONE', *, *, #83660, .T. ) ;
#207012 = CARTESIAN_POINT ( 'NONE',  ( 23.14999999999999503, 11.65000000001116298, -188.8499999999999659 ) ) ;
#207013 =( BOUNDED_CURVE ( )  B_SPLINE_CURVE ( 3, ( #198483, #137226, #257125, #160677 ),
 .UNSPECIFIED., .F., .F. ) 
 B_SPLINE_CURVE_WITH_KNOTS ( ( 4, 4 ),
 ( 0.000000000000000000, 1.570796326794908992 ),
 .UNSPECIFIED. ) 
 CURVE ( )  GEOMETRIC_REPRESENTATION_ITEM ( )  RATIONAL_B_SPLINE_CURVE ( ( 1.000000000000000000, 0.8047378541243619399, 0.8047378541243619399, 1.000000000000000000 ) ) 
 REPRESENTATION_ITEM ( '' )  );
#207014 = ORIENTED_EDGE ( 'NONE', *, *, #115068, .T. ) ;
#207015 = CARTESIAN_POINT ( 'NONE',  ( -21.05000000000000071, 69.52192177891714664, -136.4231075492198784 ) ) ;
#207016 = AXIS2_PLACEMENT_3D ( 'NONE', #63902, #24810, #143432 ) ;
#207017 = VECTOR ( 'NONE', #104686, 1000.000000000000000 ) ;
#207018 = ORIENTED_EDGE ( 'NONE', *, *, #234562, .F. ) ;
#207019 = DIRECTION ( 'NONE',  ( 0.000000000000000000, 0.000000000000000000, -1.000000000000000000 ) ) ;
#207020 = DIRECTION ( 'NONE',  ( 0.000000000000000000, 0.9651348961777118651, -0.2617529984165174461 ) ) ;
#207023 = ORIENTED_EDGE ( 'NONE', *, *, #104114, .T. ) ;
#207022 = EDGE_LOOP ( 'NONE', ( #248918, #6848, #144524, #163941 ) ) ;
#207021 = CIRCLE ( 'NONE', #127926, 0.1000000000000054040 ) ;
#207024 = ORIENTED_EDGE ( 'NONE', *, *, #34965, .T. ) ;
#207025 = CARTESIAN_POINT ( 'NONE',  ( 20.94999999999999929, 36.65892442174935439, -249.5511627012433848 ) ) ;
#207026 = VECTOR ( 'NONE', #233110, 1000.000000000000000 ) ;
#207027 = ORIENTED_EDGE ( 'NONE', *, *, #11529, .F. ) ;
#207028 = ORIENTED_EDGE ( 'NONE', *, *, #24279, .T. ) ;
#207029 = CARTESIAN_POINT ( 'NONE',  ( 18.49999999999999645, 67.23127455305835554, -235.8551265064784559 ) ) ;
#207030 = CARTESIAN_POINT ( 'NONE',  ( -21.65000000000000213, 63.05955705323258798, -213.2241350765465882 ) ) ;
#207031 = CARTESIAN_POINT ( 'NONE',  ( -23.39999999999994529, 74.94272479589878344, -8.023107484524793165 ) ) ;
#207033 = ORIENTED_EDGE ( 'NONE', *, *, #166745, .T. ) ;
#207032 = DIRECTION ( 'NONE',  ( 0.000000000000000000, -0.8814952561688437216, 0.4721928772777334582 ) ) ;
#207034 = DIRECTION ( 'NONE',  ( -1.000000000000000000, 0.000000000000000000, 0.000000000000000000 ) ) ;
#207035 = CARTESIAN_POINT ( 'NONE',  ( 20.94999999999999574, 10.47338541492405994, -108.0786544642485865 ) ) ;
#207037 = ORIENTED_EDGE ( 'NONE', *, *, #145410, .T. ) ;
#207036 = DIRECTION ( 'NONE',  ( 0.000000000000000000, 0.9394191166662618775, 0.3427706569150580362 ) ) ;
#207038 = CYLINDRICAL_SURFACE ( 'NONE', #176018, 11.75000000000000000 ) ;
#207039 = ORIENTED_EDGE ( 'NONE', *, *, #26652, .F. ) ;
#207040 = LINE ( 'NONE', #105324, #11920 ) ;
#207041 = ORIENTED_EDGE ( 'NONE', *, *, #253248, .T. ) ;
#207042 = CARTESIAN_POINT ( 'NONE',  ( 21.95218792049437795, 68.79849243876572018, -170.1221359243243114 ) ) ;
#207043 = PLANE ( 'NONE',  #253882 ) ;
#207044 = EDGE_CURVE ( 'NONE', #118980, #187404, #230105, .T. ) ;
#207045 = AXIS2_PLACEMENT_3D ( 'NONE', #35782, #237812, #116582 ) ;
#207046 = VERTEX_POINT ( 'NONE', #165848 ) ;
#207048 = CARTESIAN_POINT ( 'NONE',  ( -33.72168855820452649, 40.40989152675300033, -235.2989281452919954 ) ) ;
#207047 = CARTESIAN_POINT ( 'NONE',  ( 23.14999999999999503, 31.36165455396662693, -233.4973802202241018 ) ) ;
#207049 = LINE ( 'NONE', #79698, #55732 ) ;
#207050 = CARTESIAN_POINT ( 'NONE',  ( 18.59999999999999076, 14.86477715130881272, -235.7932433709592601 ) ) ;
#207051 = CARTESIAN_POINT ( 'NONE',  ( -20.94999999999999929, 87.65000000001163016, -66.52310748452423184 ) ) ;
#207052 = VERTEX_POINT ( 'NONE', #105826 ) ;
#207053 = ORIENTED_EDGE ( 'NONE', *, *, #220098, .T. ) ;
#207054 = AXIS2_PLACEMENT_3D ( 'NONE', #249976, #192571, #154747 ) ;
#207055 = DIRECTION ( 'NONE',  ( 0.000000000000000000, 0.000000000000000000, -1.000000000000000000 ) ) ;
#207056 = DIRECTION ( 'NONE',  ( 0.000000000000000000, 1.000000000000000000, 6.853228547068871147E-15 ) ) ;
#207057 = ORIENTED_EDGE ( 'NONE', *, *, #35893, .F. ) ;
#207058 = DIRECTION ( 'NONE',  ( 1.000000000000000000, 0.000000000000000000, 0.000000000000000000 ) ) ;
#207059 = ORIENTED_EDGE ( 'NONE', *, *, #17698, .F. ) ;
#207060 = DIRECTION ( 'NONE',  ( 1.000000000000000000, 0.000000000000000000, 0.000000000000000000 ) ) ;
#207061 = ORIENTED_EDGE ( 'NONE', *, *, #81555, .T. ) ;
#207062 = CARTESIAN_POINT ( 'NONE',  ( -20.54999999999999716, 68.75000000001179501, -81.87310748452436826 ) ) ;
#207063 = AXIS2_PLACEMENT_3D ( 'NONE', #80580, #97575, #237123 ) ;
#207064 = ADVANCED_FACE ( 'NONE', ( #163276, #242786 ), #124152, .T. ) ;
#207065 = DIRECTION ( 'NONE',  ( -0.000000000000000000, -6.982962677686266711E-15, 1.000000000000000000 ) ) ;
#207066 = CIRCLE ( 'NONE', #169695, 0.2000000000000057288 ) ;
#207067 = AXIS2_PLACEMENT_3D ( 'NONE', #71766, #131717, #148727 ) ;
#207068 = AXIS2_PLACEMENT_3D ( 'NONE', #179827, #1145, #80684 ) ;
#207069 = ORIENTED_EDGE ( 'NONE', *, *, #205823, .T. ) ;
#207070 = CARTESIAN_POINT ( 'NONE',  ( -16.77732147262506146, 63.08608884956520768, -213.1417150269271303 ) ) ;
#207071 = AXIS2_PLACEMENT_3D ( 'NONE', #138039, #160219, #175930 ) ;
#207072 = ORIENTED_EDGE ( 'NONE', *, *, #178633, .F. ) ;
#207073 = ORIENTED_EDGE ( 'NONE', *, *, #27128, .F. ) ;
#207074 = ORIENTED_EDGE ( 'NONE', *, *, #131821, .F. ) ;
#207075 = EDGE_CURVE ( 'NONE', #3284, #126100, #77933, .T. ) ;
#207076 = DIRECTION ( 'NONE',  ( 0.000000000000000000, -1.000000000000000000, 0.000000000000000000 ) ) ;
#207077 = LINE ( 'NONE', #29752, #207239 ) ;
#207078 = DIRECTION ( 'NONE',  ( -1.000000000000000000, 0.000000000000000000, 0.000000000000000000 ) ) ;
#207080 = EDGE_CURVE ( 'NONE', #235459, #98712, #180471, .T. ) ;
#207079 = FACE_OUTER_BOUND ( 'NONE', #226556, .T. ) ;
#207081 = SPHERICAL_SURFACE ( 'NONE', #209258, 0.1000000000000000056 ) ;
#207083 = CARTESIAN_POINT ( 'NONE',  ( 21.05000000000000071, 0.000000000000000000, -12.87500000000000000 ) ) ;
#207082 = CARTESIAN_POINT ( 'NONE',  ( -20.00857864376270001, 61.63293978347611812, -221.5406706031726003 ) ) ;
#207085 = ORIENTED_EDGE ( 'NONE', *, *, #25541, .T. ) ;
#207084 = CARTESIAN_POINT ( 'NONE',  ( -21.05000000000000426, 61.12960278649826762, -234.1614078874438860 ) ) ;
#207086 = DIRECTION ( 'NONE',  ( -1.000000000000000000, 0.000000000000000000, 0.000000000000000000 ) ) ;
#207087 = ORIENTED_EDGE ( 'NONE', *, *, #161626, .T. ) ;
#207088 = EDGE_CURVE ( 'NONE', #218279, #222610, #230345, .T. ) ;
#207089 = DIRECTION ( 'NONE',  ( -0.000000000000000000, -0.000000000000000000, -1.000000000000000000 ) ) ;
#207090 = VECTOR ( 'NONE', #67842, 1000.000000000000000 ) ;
#207091 = EDGE_LOOP ( 'NONE', ( #105175, #233892, #181652, #199643 ) ) ;
#207092 = ORIENTED_EDGE ( 'NONE', *, *, #23594, .T. ) ;
#207093 = DIRECTION ( 'NONE',  ( 0.000000000000000000, -1.000000000000000000, -6.982962677686266711E-15 ) ) ;
#207094 = TOROIDAL_SURFACE ( 'NONE', #7144, 11.65000000000000036, 0.1000000000000000056 ) ;
#207095 = FACE_OUTER_BOUND ( 'NONE', #95130, .T. ) ;
#207096 = CARTESIAN_POINT ( 'NONE',  ( -16.91776028072577631, 66.03659960638177040, -48.64808346982226794 ) ) ;
#207097 = DIRECTION ( 'NONE',  ( 0.000000000000000000, 0.000000000000000000, 1.000000000000000000 ) ) ;
#207098 = ADVANCED_FACE ( 'NONE', ( #211381 ), #34334, .T. ) ;
#207099 = AXIS2_PLACEMENT_3D ( 'NONE', #146540, #110000, #145263 ) ;
#207100 = CARTESIAN_POINT ( 'NONE',  ( -18.50000000000000000, 66.85000000001275566, -215.2731074845244166 ) ) ;
#207101 = ORIENTED_EDGE ( 'NONE', *, *, #237452, .T. ) ;
#207103 = ORIENTED_EDGE ( 'NONE', *, *, #75747, .F. ) ;
#207102 = EDGE_CURVE ( 'NONE', #233466, #229059, #49730, .T. ) ;
#207104 = DIRECTION ( 'NONE',  ( 0.7071067811865456854, 0.7071067811865493491, 4.937700262164544098E-15 ) ) ;
#207105 = VERTEX_POINT ( 'NONE', #92698 ) ;
#207106 = CARTESIAN_POINT ( 'NONE',  ( -20.85000000000000142, 11.75000000001115197, -127.2161343370219413 ) ) ;
#207107 = CARTESIAN_POINT ( 'NONE',  ( -23.15000000000000213, 64.25000000001246292, -181.7731074845244450 ) ) ;
#207108 = VERTEX_POINT ( 'NONE', #129274 ) ;
#207109 = FACE_OUTER_BOUND ( 'NONE', #101504, .T. ) ;
#207110 = LINE ( 'NONE', #165415, #171202 ) ;
#207111 = DIRECTION ( 'NONE',  ( 1.000000000000000000, 0.000000000000000000, 0.000000000000000000 ) ) ;
#207112 = FACE_OUTER_BOUND ( 'NONE', #208516, .T. ) ;
#207113 = ORIENTED_EDGE ( 'NONE', *, *, #200050, .F. ) ;
#207114 = DIRECTION ( 'NONE',  ( 0.000000000000000000, -0.2617529984165030132, -0.9651348961777157509 ) ) ;
#207115 = DIRECTION ( 'NONE',  ( 0.000000000000000000, -0.9916376685811618685, 0.1290532225514649800 ) ) ;
#207116 = DIRECTION ( 'NONE',  ( 1.000000000000000000, 0.000000000000000000, 0.000000000000000000 ) ) ;
#207117 = EDGE_CURVE ( 'NONE', #94765, #243170, #172296, .T. ) ;
#207118 = DIRECTION ( 'NONE',  ( 0.000000000000000000, 0.4721928772776973204, 0.8814952561688629284 ) ) ;
#207119 = CARTESIAN_POINT ( 'NONE',  ( 20.95000000000005258, 65.25000000001119815, -3.023107484524792277 ) ) ;
#207120 = AXIS2_PLACEMENT_3D ( 'NONE', #45488, #165450, #148453 ) ;
#207122 = VECTOR ( 'NONE', #193968, 1000.000000000000000 ) ;
#207121 = DIRECTION ( 'NONE',  ( 0.000000000000000000, 0.1332476588733448597, 0.9910827722268067408 ) ) ;
#207123 = AXIS2_PLACEMENT_3D ( 'NONE', #102020, #162047, #62926 ) ;
#207124 = CIRCLE ( 'NONE', #144727, 11.80000000000000426 ) ;
#207125 = ORIENTED_EDGE ( 'NONE', *, *, #192932, .T. ) ;
#207126 =( BOUNDED_SURFACE ( )  B_SPLINE_SURFACE ( 3, 2, ( 
 ( #141142, #79846, #144965 ),
 ( #223221, #26329, #326 ),
 ( #60297, #42051, #159427 ),
 ( #201102, #238960, #139833 ),
 ( #22492, #219372, #101972 ),
 ( #181563, #2885, #82408 ) ),
 .UNSPECIFIED., .F., .F., .T. ) 
 B_SPLINE_SURFACE_WITH_KNOTS ( ( 4, 2, 4 ),
 ( 3, 3 ),
 ( 0.0001342700090130087912, 0.0002909192928057473108, 0.0004475685765984858304 ),
 ( 0.000000000000000000, 1.000000000000000000 ),
 .UNSPECIFIED. ) 
 GEOMETRIC_REPRESENTATION_ITEM ( )  RATIONAL_B_SPLINE_SURFACE ( (
 ( 1.000000000000000000, 0.7250110520819882387, 1.000000000000000000),
 ( 1.000000000000000000, 0.7257599279127958658, 1.000000000000000000),
 ( 1.000000000000000000, 0.7137594617292875032, 1.000000000000000000),
 ( 1.000000000000000000, 0.6959270178801479911, 1.000000000000000000),
 ( 1.000000000000000000, 0.6919879549344875036, 1.000000000000000000),
 ( 1.000000000000000000, 0.7071067811866664776, 1.000000000000000000) ) ) 
 REPRESENTATION_ITEM ( '' )  SURFACE ( )  );
#207127 = LINE ( 'NONE', #28527, #199607 ) ;
#207128 = ORIENTED_EDGE ( 'NONE', *, *, #239136, .F. ) ;
#207129 = DIRECTION ( 'NONE',  ( 1.000000000000000000, 2.952720810173289112E-16, -0.000000000000000000 ) ) ;
#207130 = CARTESIAN_POINT ( 'NONE',  ( -23.25000000000000000, -8.999999999988844479, -90.60603087734760663 ) ) ;
#207131 = LINE ( 'NONE', #28533, #243824 ) ;
#207132 = CARTESIAN_POINT ( 'NONE',  ( 20.94999999999999574, 77.83534155023598089, -57.86795619196132634 ) ) ;
#207133 = VERTEX_POINT ( 'NONE', #193105 ) ;
#207134 = CARTESIAN_POINT ( 'NONE',  ( -23.25000000000000000, 31.36165455396662693, -233.4973802202241302 ) ) ;
#207135 = CARTESIAN_POINT ( 'NONE',  ( -21.64999999999999858, 65.95000000001159890, -56.87310748452438958 ) ) ;
#207136 = VECTOR ( 'NONE', #48469, 1000.000000000000114 ) ;
#207137 = DIRECTION ( 'NONE',  ( 1.000000000000000000, 0.000000000000000000, 0.000000000000000000 ) ) ;
#207138 = DIRECTION ( 'NONE',  ( 0.000000000000000000, 0.000000000000000000, 1.000000000000000000 ) ) ;
#207139 = CIRCLE ( 'NONE', #194694, 0.1000000000000041550 ) ;
#207140 = CARTESIAN_POINT ( 'NONE',  ( 22.41477678272288188, 75.99917613424950957, -181.6726927690397417 ) ) ;
#207141 = ADVANCED_FACE ( 'NONE', ( #189252 ), #38575, .T. ) ;
#207142 = CIRCLE ( 'NONE', #240446, 0.09999999999998898659 ) ;
#207143 = ORIENTED_EDGE ( 'NONE', *, *, #47232, .T. ) ;
#207144 = ORIENTED_EDGE ( 'NONE', *, *, #43457, .T. ) ;
#207145 = CARTESIAN_POINT ( 'NONE',  ( -20.85000000000000142, 76.00000000001126921, -203.5231074845248997 ) ) ;
#207146 = CARTESIAN_POINT ( 'NONE',  ( -21.05000000000000071, 74.83729825007388570, -94.92310748452432279 ) ) ;
#207147 = DIRECTION ( 'NONE',  ( -1.000000000000000000, -0.000000000000000000, -0.000000000000000000 ) ) ;
#207148 = LINE ( 'NONE', #108044, #118453 ) ;
#207149 = CARTESIAN_POINT ( 'NONE',  ( 22.60000000000000142, 11.74956712350054744, -33.39914163090129762 ) ) ;
#207150 = EDGE_CURVE ( 'NONE', #89904, #152124, #213343, .T. ) ;
#207151 = EDGE_CURVE ( 'NONE', #90926, #72361, #215225, .T. ) ;
#207152 = ORIENTED_EDGE ( 'NONE', *, *, #70388, .T. ) ;
#207153 = DIRECTION ( 'NONE',  ( -1.000000000000000000, -2.952720810173289112E-16, 0.000000000000000000 ) ) ;
#207154 = DIRECTION ( 'NONE',  ( 0.000000000000000000, 0.8741572761215393728, -0.4856429311786291669 ) ) ;
#207155 = ADVANCED_FACE ( 'NONE', ( #116138 ), #250937, .F. ) ;
#207156 = ORIENTED_EDGE ( 'NONE', *, *, #112829, .F. ) ;
#207157 = LINE ( 'NONE', #168066, #25430 ) ;
#207158 = ADVANCED_FACE ( 'NONE', ( #20904 ), #154021, .F. ) ;
#207159 = AXIS2_PLACEMENT_3D ( 'NONE', #205093, #185554, #222076 ) ;
#207160 = EDGE_CURVE ( 'NONE', #187556, #206536, #142602, .T. ) ;
#207161 = EDGE_LOOP ( 'NONE', ( #156635, #17780, #43130, #257595 ) ) ;
#207162 = EDGE_LOOP ( 'NONE', ( #94886, #240584, #97188, #172313 ) ) ;
#207163 = ADVANCED_FACE ( 'NONE', ( #156573 ), #254327, .F. ) ;
#207164 = VERTEX_POINT ( 'NONE', #57414 ) ;
#207165 = CARTESIAN_POINT ( 'NONE',  ( 21.04999999999999716, 10.54375127550682301, -74.55638780866505044 ) ) ;
#207166 = CARTESIAN_POINT ( 'NONE',  ( -20.65000000000000568, 5.650000000011139001, -76.25000000000004263 ) ) ;
#207167 = AXIS2_PLACEMENT_3D ( 'NONE', #41346, #98677, #257739 ) ;
#207168 = DIRECTION ( 'NONE',  ( 1.000000000000000000, 0.000000000000000000, 0.000000000000000000 ) ) ;
#207169 = CARTESIAN_POINT ( 'NONE',  ( 18.49505816908823874, -9.437872553199978753, -140.7776572016709054 ) ) ;
#207170 = CYLINDRICAL_SURFACE ( 'NONE', #152771, 0.09999999999999933942 ) ;
#207171 = ADVANCED_FACE ( 'NONE', ( #17041 ), #97810, .F. ) ;
#207172 = DIRECTION ( 'NONE',  ( 1.000000000000000000, 0.000000000000000000, 0.000000000000000000 ) ) ;
#207173 = DIRECTION ( 'NONE',  ( 0.000000000000000000, -0.2128009952263603677, 0.9770955615653313941 ) ) ;
#207176 = CARTESIAN_POINT ( 'NONE',  ( -22.47071067811865319, 1.115600667400684642E-11, -67.00000000000004263 ) ) ;
#207175 = CIRCLE ( 'NONE', #61231, 0.9000000000000014655 ) ;
#207174 = LINE ( 'NONE', #231883, #253493 ) ;
#207177 = DIRECTION ( 'NONE',  ( 0.000000000000000000, 0.8814952561688476074, -0.4721928772777262417 ) ) ;
#207179 = EDGE_CURVE ( 'NONE', #139562, #62001, #37894, .T. ) ;
#207178 = DIRECTION ( 'NONE',  ( -1.000000000000000000, -8.673617379884087537E-15, 0.000000000000000000 ) ) ;
#207180 = DIRECTION ( 'NONE',  ( -0.000000000000000000, -1.000000000000000000, -6.982962677686266711E-15 ) ) ;
#207181 = CARTESIAN_POINT ( 'NONE',  ( 18.39999999999999503, 11.75000000001113953, -180.1499999999999773 ) ) ;
#207182 = AXIS2_PLACEMENT_3D ( 'NONE', #163937, #229050, #50373 ) ;
#207183 = EDGE_LOOP ( 'NONE', ( #58387, #72078, #157549, #59731 ) ) ;
#207184 = CIRCLE ( 'NONE', #161387, 0.1000000000000028644 ) ;
#207185 = EDGE_LOOP ( 'NONE', ( #166739, #85807, #106047, #47820 ) ) ;
#207186 = CARTESIAN_POINT ( 'NONE',  ( -18.50000000000000000, -9.499999999988849808, -108.6000000000000227 ) ) ;
#207187 = CARTESIAN_POINT ( 'NONE',  ( -18.59999999999999787, -1.851617760457748618, -112.1031897196037050 ) ) ;
#207189 = CARTESIAN_POINT ( 'NONE',  ( -14.45422546970484312, 13.15902077901803224, -217.0103513519800060 ) ) ;
#207188 = CARTESIAN_POINT ( 'NONE',  ( -16.91049119928363353, 9.950000000011137047, -154.8817203931908182 ) ) ;
#207190 = ADVANCED_FACE ( 'NONE', ( #28421 ), #167921, .T. ) ;
#207191 = ADVANCED_FACE ( 'NONE', ( #35344 ), #194404, .F. ) ;
#207192 = DIRECTION ( 'NONE',  ( 0.000000000000000000, 6.938893903907222067E-15, -1.000000000000000000 ) ) ;
#207193 = DIRECTION ( 'NONE',  ( 1.000000000000000000, 0.000000000000000000, 0.000000000000000000 ) ) ;
#207194 = AXIS2_PLACEMENT_3D ( 'NONE', #71133, #134903, #189775 ) ;
#207195 = DIRECTION ( 'NONE',  ( 0.000000000000000000, 0.8814952561688429444, -0.4721928772777348460 ) ) ;
#207196 = EDGE_CURVE ( 'NONE', #233154, #59508, #155286, .T. ) ;
#207197 = EDGE_CURVE ( 'NONE', #195237, #106096, #163474, .T. ) ;
#207198 = ORIENTED_EDGE ( 'NONE', *, *, #71790, .F. ) ;
#207199 = ORIENTED_EDGE ( 'NONE', *, *, #81130, .T. ) ;
#207200 = DIRECTION ( 'NONE',  ( -2.952720810173289112E-16, -1.000000000000000000, -6.982962677686266711E-15 ) ) ;
#207201 = ORIENTED_EDGE ( 'NONE', *, *, #84988, .F. ) ;
#207202 = LINE ( 'NONE', #28607, #218142 ) ;
#207203 = AXIS2_PLACEMENT_3D ( 'NONE', #258092, #182477, #101594 ) ;
#207204 = AXIS2_PLACEMENT_3D ( 'NONE', #200242, #84086, #120730 ) ;
#207205 = LINE ( 'NONE', #65106, #117265 ) ;
#207206 = B_SPLINE_CURVE_WITH_KNOTS ( 'NONE', 3,
 ( #32856, #253130, #112363, #95355, #233591, #229727, #54920, #131912 ),
 .UNSPECIFIED., .F., .F.,
 ( 4, 2, 2, 4 ),
 ( 0.000000000000000000, 0.0002114466876442108679, 0.0003171700314663126563, 0.0004228933752884144175 ),
 .UNSPECIFIED. ) ;
#207207 = AXIS2_PLACEMENT_3D ( 'NONE', #36433, #76806, #59786 ) ;
#207209 = VERTEX_POINT ( 'NONE', #159131 ) ;
#207208 = VECTOR ( 'NONE', #17081, 1000.000000000000000 ) ;
#207210 = LINE ( 'NONE', #92369, #68558 ) ;
#207211 = ORIENTED_EDGE ( 'NONE', *, *, #226737, .F. ) ;
#207212 = VECTOR ( 'NONE', #102682, 1000.000000000000000 ) ;
#207213 = CARTESIAN_POINT ( 'NONE',  ( -0.8999999999999993561, -8.350000000000004974, 26.00000000000000355 ) ) ;
#207214 = DIRECTION ( 'NONE',  ( 0.000000000000000000, -1.000000000000000000, 0.000000000000000000 ) ) ;
#207215 = CYLINDRICAL_SURFACE ( 'NONE', #203351, 0.1000000000000028644 ) ;
#207216 = CARTESIAN_POINT ( 'NONE',  ( 18.50000000000000000, -9.399999999988823518, -141.2972597596632909 ) ) ;
#207217 = DIRECTION ( 'NONE',  ( 0.000000000000000000, -1.000000000000000000, -8.717686153663073805E-15 ) ) ;
#207218 = FACE_OUTER_BOUND ( 'NONE', #239701, .T. ) ;
#207219 = DIRECTION ( 'NONE',  ( 0.000000000000000000, -0.000000000000000000, -1.000000000000000000 ) ) ;
#207221 = ORIENTED_EDGE ( 'NONE', *, *, #88720, .T. ) ;
#207220 = DIRECTION ( 'NONE',  ( 0.000000000000000000, 0.9126074666063848095, 0.4088369013363106763 ) ) ;
#207223 = LINE ( 'NONE', #50673, #39397 ) ;
#207222 = FACE_OUTER_BOUND ( 'NONE', #208958, .T. ) ;
#207224 = ORIENTED_EDGE ( 'NONE', *, *, #93260, .T. ) ;
#207226 = ORIENTED_EDGE ( 'NONE', *, *, #170481, .F. ) ;
#207225 = DIRECTION ( 'NONE',  ( 1.000000000000000000, 0.000000000000000000, 0.000000000000000000 ) ) ;
#207227 = VECTOR ( 'NONE', #156417, 1000.000000000000000 ) ;
#207228 = ORIENTED_EDGE ( 'NONE', *, *, #39947, .F. ) ;
#207229 = CARTESIAN_POINT ( 'NONE',  ( 20.94999999999999574, -1.835341550213255957, -179.1551512925629197 ) ) ;
#207230 = VECTOR ( 'NONE', #138759, 1000.000000000000000 ) ;
#207231 = CARTESIAN_POINT ( 'NONE',  ( -18.38639463286148867, 11.48019957384713230, -143.2500000000000284 ) ) ;
#207232 = CARTESIAN_POINT ( 'NONE',  ( -22.39999999999999858, 0.2612980822699374484, -230.0539506776466681 ) ) ;
#207233 = DIRECTION ( 'NONE',  ( 0.000000000000000000, -0.9770955615653316162, -0.2128009952263604232 ) ) ;
#207234 = CYLINDRICAL_SURFACE ( 'NONE', #2444, 0.09999999999999939493 ) ;
#207235 = DIRECTION ( 'NONE',  ( 2.659396599871503635E-15, 0.6132151058540549204, -0.7899159663865520375 ) ) ;
#207236 = DIRECTION ( 'NONE',  ( -1.020425574104004196E-15, 6.982962677686266711E-15, -1.000000000000000000 ) ) ;
#207237 = CARTESIAN_POINT ( 'NONE',  ( 20.94999999999999574, -11.41227409413852989, -36.39999999999999858 ) ) ;
#207238 = B_SPLINE_CURVE_WITH_KNOTS ( 'NONE', 3,
 ( #125303, #126583, #69202, #204815, #124024, #185274, #182719, #108308, #228261, #187860 ),
 .UNSPECIFIED., .F., .F.,
 ( 4, 3, 3, 4 ),
 ( 4.504661056180557620E-18, 0.0002000000000002871876, 0.001000000000045109336, 0.001967863649472136479 ),
 .UNSPECIFIED. ) ;
#207239 = VECTOR ( 'NONE', #149689, 1000.000000000000000 ) ;
#207240 = EDGE_CURVE ( 'NONE', #138184, #183886, #117689, .T. ) ;
#207241 = CIRCLE ( 'NONE', #53092, 0.2000000000000057288 ) ;
#207242 = FACE_OUTER_BOUND ( 'NONE', #125532, .T. ) ;
#207243 = ORIENTED_EDGE ( 'NONE', *, *, #67735, .T. ) ;
#207244 = VERTEX_POINT ( 'NONE', #96533 ) ;
#207245 = ADVANCED_FACE ( 'NONE', ( #120009 ), #212348, .F. ) ;
#207246 = CARTESIAN_POINT ( 'NONE',  ( -20.54999999999999716, 7.150000000000000355, -21.15000000000000213 ) ) ;
#207247 = AXIS2_PLACEMENT_3D ( 'NONE', #86517, #85228, #47407 ) ;
#207248 = VERTEX_POINT ( 'NONE', #178702 ) ;
#207249 = DIRECTION ( 'NONE',  ( 0.000000000000000000, 0.8814952561688430555, -0.4721928772777346239 ) ) ;
#207250 = ORIENTED_EDGE ( 'NONE', *, *, #24452, .T. ) ;
#207251 = DIRECTION ( 'NONE',  ( 1.000000000000000000, 0.000000000000000000, 0.000000000000000000 ) ) ;
#207252 = CIRCLE ( 'NONE', #28199, 0.1000000000000012546 ) ;
#207253 = EDGE_CURVE ( 'NONE', #82701, #71184, #42663, .T. ) ;
#207254 = ADVANCED_FACE ( 'NONE', ( #241223 ), #175976, .F. ) ;
#207255 = FACE_OUTER_BOUND ( 'NONE', #119734, .T. ) ;
#207256 = LINE ( 'NONE', #92411, #247592 ) ;
#207257 = CARTESIAN_POINT ( 'NONE',  ( 21.14999999999999858, -11.64999999998883595, -33.50000000000000000 ) ) ;
#207258 = DIRECTION ( 'NONE',  ( 1.000000000000000000, 0.000000000000000000, 0.000000000000000000 ) ) ;
#207259 = ORIENTED_EDGE ( 'NONE', *, *, #38628, .F. ) ;
#207260 = CIRCLE ( 'NONE', #15738, 0.09999999999998708533 ) ;
#207261 = FACE_OUTER_BOUND ( 'NONE', #93977, .T. ) ;
#207262 = AXIS2_PLACEMENT_3D ( 'NONE', #221501, #45450, #63727 ) ;
#207263 = AXIS2_PLACEMENT_3D ( 'NONE', #59512, #41301, #161227 ) ;
#207264 = CARTESIAN_POINT ( 'NONE',  ( -16.89268316805465986, 66.04827818677036078, -182.6673550059788909 ) ) ;
#207265 = VECTOR ( 'NONE', #232895, 1000.000000000000000 ) ;
#207266 = CARTESIAN_POINT ( 'NONE',  ( 18.43579564894470835, 85.51932753530414288, -62.55013084066395379 ) ) ;
#207267 = DIRECTION ( 'NONE',  ( -0.000000000000000000, 1.000000000000000000, 6.352154140967427193E-15 ) ) ;
#207268 = VERTEX_POINT ( 'NONE', #62575 ) ;
#207270 = DIRECTION ( 'NONE',  ( 0.000000000000000000, 1.776356839400254803E-15, -1.000000000000000000 ) ) ;
#207269 = CARTESIAN_POINT ( 'NONE',  ( 21.08134388332232234, 61.09760743966705832, -234.2701803535934459 ) ) ;
#207271 = ORIENTED_EDGE ( 'NONE', *, *, #150347, .T. ) ;
#207274 = ORIENTED_EDGE ( 'NONE', *, *, #79863, .T. ) ;
#207273 = CARTESIAN_POINT ( 'NONE',  ( -16.81453563122430950, 51.56697356313223679, -231.9816583874184346 ) ) ;
#207272 = DIRECTION ( 'NONE',  ( 0.000000000000000000, 7.147358527629762208E-15, -1.000000000000000000 ) ) ;
#207275 = TOROIDAL_SURFACE ( 'NONE', #248962, 4.149999999999999467, 0.1000000000000000056 ) ;
#207276 = EDGE_LOOP ( 'NONE', ( #72369, #31896, #10033, #59746 ) ) ;
#207277 = DIRECTION ( 'NONE',  ( -0.000000000000000000, 0.8660254037844424824, 0.4999999999999934497 ) ) ;
#207278 = EDGE_CURVE ( 'NONE', #227337, #150102, #64975, .T. ) ;
#207279 = CARTESIAN_POINT ( 'NONE',  ( -20.64999999999999858, 27.82649702422227733, -239.8850763025288870 ) ) ;
#207280 = DIRECTION ( 'NONE',  ( -0.000000000000000000, -0.000000000000000000, 1.000000000000000000 ) ) ;
#207281 = ORIENTED_EDGE ( 'NONE', *, *, #214199, .F. ) ;
#207282 = CARTESIAN_POINT ( 'NONE',  ( 20.95000000000000284, 64.40000000001248281, -176.9513107147999449 ) ) ;
#207283 = SPHERICAL_SURFACE ( 'NONE', #28165, 0.1000000000000000056 ) ;
#207285 = DIRECTION ( 'NONE',  ( 1.000000000000000000, -0.000000000000000000, -0.000000000000000000 ) ) ;
#207284 = CARTESIAN_POINT ( 'NONE',  ( -22.59066674512250472, 11.75000000000000000, 0.03050412363058079002 ) ) ;
#207287 = VERTEX_POINT ( 'NONE', #26022 ) ;
#207286 = PLANE ( 'NONE',  #118278 ) ;
#207288 = VECTOR ( 'NONE', #191158, 1000.000000000000000 ) ;
#207289 = EDGE_CURVE ( 'NONE', #65351, #39843, #144660, .T. ) ;
#207290 = ORIENTED_EDGE ( 'NONE', *, *, #62331, .T. ) ;
#207292 = ADVANCED_FACE ( 'NONE', ( #221616 ), #84655, .F. ) ;
#207291 = FACE_OUTER_BOUND ( 'NONE', #226109, .T. ) ;
#207293 = DIRECTION ( 'NONE',  ( -0.8660254037844653530, 0.000000000000000000, -0.4999999999999539257 ) ) ;
#207294 = AXIS2_PLACEMENT_3D ( 'NONE', #216803, #119011, #198529 ) ;
#207295 = DIRECTION ( 'NONE',  ( 0.000000000000000000, 0.9893560106964510714, -0.1455152366551481502 ) ) ;
#207296 = ORIENTED_EDGE ( 'NONE', *, *, #242727, .T. ) ;
#207297 = CARTESIAN_POINT ( 'NONE',  ( 18.49999999999999289, 64.35000000001197407, -111.6731074845243796 ) ) ;
#207298 = DIRECTION ( 'NONE',  ( 1.000000000000000000, 0.000000000000000000, 0.000000000000000000 ) ) ;
#207299 = DIRECTION ( 'NONE',  ( 1.000000000000000000, 0.000000000000000000, 0.000000000000000000 ) ) ;
#207300 = ORIENTED_EDGE ( 'NONE', *, *, #182822, .F. ) ;
#207301 = EDGE_CURVE ( 'NONE', #219183, #75451, #76000, .T. ) ;
#207302 = CARTESIAN_POINT ( 'NONE',  ( 23.14999999999999858, 65.71172719659838890, -223.0701118083454446 ) ) ;
#207303 = EDGE_CURVE ( 'NONE', #57548, #53632, #196783, .T. ) ;
#207304 = ORIENTED_EDGE ( 'NONE', *, *, #242156, .T. ) ;
#207305 = EDGE_CURVE ( 'NONE', #252337, #53762, #5225, .T. ) ;
#207306 = CIRCLE ( 'NONE', #182357, 0.09999999999999939493 ) ;
#207307 = DIRECTION ( 'NONE',  ( -1.000000000000000000, -3.265361837132813093E-16, 0.000000000000000000 ) ) ;
#207308 = DIRECTION ( 'NONE',  ( -1.000000000000000000, -0.000000000000000000, -0.000000000000000000 ) ) ;
#207309 = CIRCLE ( 'NONE', #161519, 11.64999999999999325 ) ;
#207310 = VERTEX_POINT ( 'NONE', #225469 ) ;
#207311 = ORIENTED_EDGE ( 'NONE', *, *, #44445, .F. ) ;
#207312 = LINE ( 'NONE', #169493, #154213 ) ;
#207313 = ORIENTED_EDGE ( 'NONE', *, *, #182391, .F. ) ;
#207315 = ORIENTED_EDGE ( 'NONE', *, *, #117563, .F. ) ;
#207314 = CARTESIAN_POINT ( 'NONE',  ( -22.45354308602431814, 2.198887230422068235E-07, -155.7495671095381624 ) ) ;
#207316 = ADVANCED_FACE ( 'NONE', ( #6438 ), #44303, .T. ) ;
#207317 = VERTEX_POINT ( 'NONE', #126389 ) ;
#207319 = ORIENTED_EDGE ( 'NONE', *, *, #200475, .F. ) ;
#207318 = EDGE_LOOP ( 'NONE', ( #143211, #166939, #254052, #162826 ) ) ;
#207320 = EDGE_CURVE ( 'NONE', #216000, #253186, #165537, .T. ) ;
#207321 = CONICAL_SURFACE ( 'NONE', #153178, 4.299999999999956302, 0.7853981633974466137 ) ;
#207322 = DIRECTION ( 'NONE',  ( 1.000000000000000000, 0.000000000000000000, 0.000000000000000000 ) ) ;
#207323 = AXIS2_PLACEMENT_3D ( 'NONE', #227376, #26636, #189554 ) ;
#207324 = ORIENTED_EDGE ( 'NONE', *, *, #158525, .F. ) ;
#207325 = CARTESIAN_POINT ( 'NONE',  ( -20.64999999999999858, 71.65000000001187175, -90.67310748452433700 ) ) ;
#207326 = CARTESIAN_POINT ( 'NONE',  ( 20.94999999999999929, 43.08613539620618837, -254.3146655184800409 ) ) ;
#207327 = DIRECTION ( 'NONE',  ( 1.000000000000000000, 0.000000000000000000, 0.000000000000000000 ) ) ;
#207328 = AXIS2_PLACEMENT_3D ( 'NONE', #189066, #174687, #32600 ) ;
#207329 = CARTESIAN_POINT ( 'NONE',  ( -18.40000000000000213, 11.47316190337362940, -146.6085786437627121 ) ) ;
#207330 = ORIENTED_EDGE ( 'NONE', *, *, #104156, .T. ) ;
#207331 = ORIENTED_EDGE ( 'NONE', *, *, #205577, .F. ) ;
#207332 = DIRECTION ( 'NONE',  ( 0.000000000000000000, 0.000000000000000000, 1.000000000000000000 ) ) ;
#207334 = EDGE_LOOP ( 'NONE', ( #146698, #241073, #85510, #114095 ) ) ;
#207333 = CARTESIAN_POINT ( 'NONE',  ( 18.49999999999999289, 63.82873662800449210, -209.2836886274109247 ) ) ;
#207335 = CARTESIAN_POINT ( 'NONE',  ( 20.85000000000000142, 31.15787740146373963, -259.8205824356103903 ) ) ;
#207337 = VERTEX_POINT ( 'NONE', #66423 ) ;
#207336 = DIRECTION ( 'NONE',  ( -0.000000000000000000, -0.000000000000000000, -1.000000000000000000 ) ) ;
#207338 = VERTEX_POINT ( 'NONE', #203368 ) ;
#207339 = DIRECTION ( 'NONE',  ( 0.000000000000000000, 1.000000000000000000, 0.000000000000000000 ) ) ;
#207340 = ORIENTED_EDGE ( 'NONE', *, *, #135818, .T. ) ;
#207341 = DIRECTION ( 'NONE',  ( 0.000000000000000000, 0.000000000000000000, -1.000000000000000000 ) ) ;
#207342 = CARTESIAN_POINT ( 'NONE',  ( -21.05000000000000071, -0.09999996528895159498, -161.0224478175061904 ) ) ;
#207343 = AXIS2_PLACEMENT_3D ( 'NONE', #115006, #257037, #194576 ) ;
#207344 = VECTOR ( 'NONE', #105924, 1000.000000000000000 ) ;
#207346 = ORIENTED_EDGE ( 'NONE', *, *, #75773, .T. ) ;
#207345 = ORIENTED_EDGE ( 'NONE', *, *, #62854, .T. ) ;
#207347 = EDGE_LOOP ( 'NONE', ( #111842, #171465, #115044, #82223 ) ) ;
#207348 = CARTESIAN_POINT ( 'NONE',  ( 21.05000000000000071, 6.257814610487280937, -33.40220970869120265 ) ) ;
#207349 = ORIENTED_EDGE ( 'NONE', *, *, #79922, .F. ) ;
#207350 = VERTEX_POINT ( 'NONE', #3878 ) ;
#207351 = CARTESIAN_POINT ( 'NONE',  ( 20.12500000000000000, 66.25000000001161027, -61.41133620241011215 ) ) ;
#207353 = EDGE_LOOP ( 'NONE', ( #157176, #155695, #235309, #80913 ) ) ;
#207352 = DIRECTION ( 'NONE',  ( -1.000000000000000000, -0.000000000000000000, -0.000000000000000000 ) ) ;
#207354 = DIRECTION ( 'NONE',  ( 0.000000000000000000, -0.9915357197604982575, 0.1298341882519033486 ) ) ;
#207355 = CIRCLE ( 'NONE', #94895, 0.2000000000000150546 ) ;
#207357 = DIRECTION ( 'NONE',  ( 0.000000000000000000, 1.000000000000000000, 6.982962677686266711E-15 ) ) ;
#207356 = CARTESIAN_POINT ( 'NONE',  ( 19.75857864376268935, 11.65000000001115943, -192.2499999999999716 ) ) ;
#207358 = CARTESIAN_POINT ( 'NONE',  ( 18.43579564894469414, 85.51932753530516607, -196.5501308406639680 ) ) ;
#207359 = CARTESIAN_POINT ( 'NONE',  ( -12.84409460144754078, 62.18784473894375964, -218.4987171750604773 ) ) ;
#207360 = VERTEX_POINT ( 'NONE', #2579 ) ;
#207361 = EDGE_LOOP ( 'NONE', ( #16811, #10654, #69820 ) ) ;
#207362 = AXIS2_PLACEMENT_3D ( 'NONE', #199524, #119998, #255570 ) ;
#207363 = DIRECTION ( 'NONE',  ( 0.000000000000000000, -0.8700118002898359348, 0.4930308989875165082 ) ) ;
#207364 = CARTESIAN_POINT ( 'NONE',  ( -18.40000000000000213, 64.51332499825382172, -45.27310748452440947 ) ) ;
#207365 = EDGE_CURVE ( 'NONE', #123327, #54036, #204964, .T. ) ;
#207366 = VERTEX_POINT ( 'NONE', #204630 ) ;
#207367 = CIRCLE ( 'NONE', #19932, 12.87499999999999822 ) ;
#207368 = AXIS2_PLACEMENT_3D ( 'NONE', #124327, #164735, #241699 ) ;
#207369 = PLANE ( 'NONE',  #21892 ) ;
#207370 = ORIENTED_EDGE ( 'NONE', *, *, #154504, .T. ) ;
#207371 = ORIENTED_EDGE ( 'NONE', *, *, #87040, .F. ) ;
#207372 = DIRECTION ( 'NONE',  ( -1.000000000000000000, -7.304098846218135653E-16, -4.639676173203994055E-30 ) ) ;
#207373 = EDGE_CURVE ( 'NONE', #202760, #3198, #125856, .T. ) ;
#207374 = CARTESIAN_POINT ( 'NONE',  ( -18.38639463286148867, 64.51980042617610422, -127.2731074845243882 ) ) ;
#207375 = ORIENTED_EDGE ( 'NONE', *, *, #181479, .F. ) ;
#207376 = CARTESIAN_POINT ( 'NONE',  ( -18.59999999999999787, 76.00000000001244871, -170.0231074845243597 ) ) ;
#207377 = CARTESIAN_POINT ( 'NONE',  ( 21.06600267594171783, 8.775166069211060460, -112.7042627823747694 ) ) ;
#207379 = ORIENTED_EDGE ( 'NONE', *, *, #69772, .F. ) ;
#207378 = APPLICATION_CONTEXT ( 'automotive_design' ) ;
#207380 = DIRECTION ( 'NONE',  ( 0.000000000000000000, 0.000000000000000000, 1.000000000000000000 ) ) ;
#207381 = CARTESIAN_POINT ( 'NONE',  ( -16.87036670365549895, 10.08494996326643189, -46.04999999999999716 ) ) ;
#207383 = CARTESIAN_POINT ( 'NONE',  ( 23.14999999999998437, 71.14007088257814360, -236.9152261500652514 ) ) ;
#207382 = DIRECTION ( 'NONE',  ( 0.000000000000000000, 0.2128009952263485993, -0.9770955615653341697 ) ) ;
#207384 = CARTESIAN_POINT ( 'NONE',  ( 19.97071067811865674, 11.72071067812981937, -91.65000000000004832 ) ) ;
#207385 = EDGE_CURVE ( 'NONE', #164329, #151038, #933, .T. ) ;
#207387 = EDGE_CURVE ( 'NONE', #24784, #148073, #80040, .T. ) ;
#207386 = FACE_OUTER_BOUND ( 'NONE', #61147, .T. ) ;
#207388 = DIRECTION ( 'NONE',  ( 0.000000000000000000, -0.01283462868041981321, -0.9999176327611367654 ) ) ;
#207389 = DIRECTION ( 'NONE',  ( 0.000000000000000000, 0.2617529984166090395, 0.9651348961776869961 ) ) ;
#207390 = CIRCLE ( 'NONE', #94924, 2.100000000000004530 ) ;
#207391 = ORIENTED_EDGE ( 'NONE', *, *, #203593, .T. ) ;
#207392 = VECTOR ( 'NONE', #241630, 1000.000000000000114 ) ;
#207395 = ORIENTED_EDGE ( 'NONE', *, *, #55144, .T. ) ;
#207394 = VERTEX_POINT ( 'NONE', #22179 ) ;
#207393 = AXIS2_PLACEMENT_3D ( 'NONE', #135483, #1097, #215040 ) ;
#207396 = ORIENTED_EDGE ( 'NONE', *, *, #84983, .F. ) ;
#207397 = VECTOR ( 'NONE', #194820, 1000.000000000000000 ) ;
#207398 = VECTOR ( 'NONE', #156298, 1000.000000000000000 ) ;
#207399 = ADVANCED_FACE ( 'NONE', ( #181254 ), #82102, .F. ) ;
#207400 = DIRECTION ( 'NONE',  ( 0.000000000000000000, 1.000000000000000000, 0.000000000000000000 ) ) ;
#207401 = CARTESIAN_POINT ( 'NONE',  ( 20.04142135623730070, 54.39174857302370469, -228.8414560973406822 ) ) ;
#207402 = CIRCLE ( 'NONE', #53259, 0.1000000000000028644 ) ;
#207404 = CARTESIAN_POINT ( 'NONE',  ( -18.59999999999999787, 1.115600667400684642E-11, -200.9999999999999432 ) ) ;
#207403 = DIRECTION ( 'NONE',  ( 0.000000000000000000, 0.000000000000000000, 1.000000000000000000 ) ) ;
#207405 = FACE_OUTER_BOUND ( 'NONE', #169732, .T. ) ;
#207406 = VERTEX_POINT ( 'NONE', #67702 ) ;
#207407 = DIRECTION ( 'NONE',  ( 0.000000000000000000, 6.982962677686267499E-15, -1.000000000000000000 ) ) ;
#207408 = CARTESIAN_POINT ( 'NONE',  ( -23.15000000000000213, 87.48912529308852015, -173.1231074845242688 ) ) ;
#207409 = DIRECTION ( 'NONE',  ( -4.239556034732056743E-17, 0.1298341882520022694, 0.9915357197604853789 ) ) ;
#207410 = FACE_OUTER_BOUND ( 'NONE', #22216, .T. ) ;
#207411 = ORIENTED_EDGE ( 'NONE', *, *, #37662, .F. ) ;
#207412 = VECTOR ( 'NONE', #136141, 1000.000000000000000 ) ;
#207413 = VECTOR ( 'NONE', #246705, 1000.000000000000114 ) ;
#207414 = CARTESIAN_POINT ( 'NONE',  ( 21.33487959338958362, 6.725558151922348848, -134.0000000000000000 ) ) ;
#207415 = CARTESIAN_POINT ( 'NONE',  ( 23.14999999999999858, 5.900000000000005684, -23.28090023534362629 ) ) ;
#207416 = EDGE_LOOP ( 'NONE', ( #138438, #62186, #56350, #106251 ) ) ;
#207418 = EDGE_LOOP ( 'NONE', ( #93699, #251346, #177495, #213425 ) ) ;
#207417 = EDGE_CURVE ( 'NONE', #60194, #782, #59378, .T. ) ;
#207419 = LINE ( 'NONE', #69201, #33292 ) ;
#207420 = DIRECTION ( 'NONE',  ( 0.000000000000000000, 0.9126074666063660468, 0.4088369013363524762 ) ) ;
#207421 = CARTESIAN_POINT ( 'NONE',  ( -21.05000000000000071, 70.15000000001211333, -126.3906102602463619 ) ) ;
#207422 = CARTESIAN_POINT ( 'NONE',  ( -21.44999999999999929, 7.350000000011155166, -45.85000000000000142 ) ) ;
#207423 = CYLINDRICAL_SURFACE ( 'NONE', #23450, 0.09999999999999990841 ) ;
#207424 = CARTESIAN_POINT ( 'NONE',  ( 22.50000000000000000, 76.00000000001165290, -69.52310748452431710 ) ) ;
#207425 = EDGE_LOOP ( 'NONE', ( #54505, #227008, #71576, #55947 ) ) ;
#207426 = CARTESIAN_POINT ( 'NONE',  ( -20.94999999999999929, 2.838478681111047841, -208.5693404029859437 ) ) ;
#207427 = CARTESIAN_POINT ( 'NONE',  ( 18.39999999999999858, 86.99291436658650412, -199.6658631664729739 ) ) ;
#207428 = CIRCLE ( 'NONE', #128312, 0.09999999999999491240 ) ;
#207430 = DIRECTION ( 'NONE',  ( -4.408576920032447355E-17, -0.1350103645451945777, 0.9908441862701589109 ) ) ;
#207429 = CARTESIAN_POINT ( 'NONE',  ( -21.05000000000000071, 4.348235979057646361, -245.2768893876484810 ) ) ;
#207431 = CARTESIAN_POINT ( 'NONE',  ( -23.15000000000000213, 67.23127455305835554, -235.8551265064784559 ) ) ;
#207432 = AXIS2_PLACEMENT_3D ( 'NONE', #106648, #124963, #246190 ) ;
#207433 = EDGE_CURVE ( 'NONE', #97734, #232002, #1135, .T. ) ;
#207434 = CARTESIAN_POINT ( 'NONE',  ( 20.85000000000000142, 64.35000000001141984, -36.02310748452440237 ) ) ;
#207435 = DIRECTION ( 'NONE',  ( 1.000000000000000000, 0.000000000000000000, -0.000000000000000000 ) ) ;
#207437 = CYLINDRICAL_SURFACE ( 'NONE', #198195, 0.09999999999999939493 ) ;
#207436 = AXIS2_PLACEMENT_3D ( 'NONE', #26283, #206197, #223177 ) ;
#207439 = ORIENTED_EDGE ( 'NONE', *, *, #191258, .T. ) ;
#207438 = FACE_OUTER_BOUND ( 'NONE', #125322, .T. ) ;
#207440 = CIRCLE ( 'NONE', #169872, 0.09999999999999935330 ) ;
#207441 = CIRCLE ( 'NONE', #82489, 0.09999999999999939493 ) ;
#207442 = CIRCLE ( 'NONE', #103169, 0.1000000000000008937 ) ;
#207443 = DIRECTION ( 'NONE',  ( 0.000000000000000000, -1.000000000000000000, 0.000000000000000000 ) ) ;
#207444 = AXIS2_PLACEMENT_3D ( 'NONE', #15678, #112201, #208728 ) ;
#207445 = DIRECTION ( 'NONE',  ( 1.000000000000000000, 0.000000000000000000, 0.000000000000000000 ) ) ;
#207446 = ORIENTED_EDGE ( 'NONE', *, *, #92123, .F. ) ;
#207447 = VECTOR ( 'NONE', #227835, 999.9999999999998863 ) ;
#207448 = CYLINDRICAL_SURFACE ( 'NONE', #222164, 0.09999999999999939493 ) ;
#207449 = CARTESIAN_POINT ( 'NONE',  ( -21.14999999999999858, 37.99340787088039662, -236.0781345613907547 ) ) ;
#207450 = FACE_OUTER_BOUND ( 'NONE', #77622, .T. ) ;
#207451 = EDGE_CURVE ( 'NONE', #146658, #108916, #132826, .T. ) ;
#207452 = ADVANCED_FACE ( 'NONE', ( #246343 ), #212368, .T. ) ;
#207453 = ORIENTED_EDGE ( 'NONE', *, *, #192106, .T. ) ;
#207454 = CARTESIAN_POINT ( 'NONE',  ( -23.15000000000000213, 1.148907358139439339E-11, -201.0000000000015064 ) ) ;
#207456 = ORIENTED_EDGE ( 'NONE', *, *, #127973, .F. ) ;
#207455 = CARTESIAN_POINT ( 'NONE',  ( -20.85000000000000142, 77.83585931145498193, -24.51866831572578675 ) ) ;
#207457 = CARTESIAN_POINT ( 'NONE',  ( -21.05000000000000071, 13.54362637910787370, -238.4879411198429580 ) ) ;
#207459 = EDGE_CURVE ( 'NONE', #229115, #89242, #159400, .T. ) ;
#207458 = DIRECTION ( 'NONE',  ( 1.000000000000000000, 0.000000000000000000, 0.000000000000000000 ) ) ;
#207460 = EDGE_CURVE ( 'NONE', #225834, #110138, #46927, .T. ) ;
#207461 = ORIENTED_EDGE ( 'NONE', *, *, #232144, .T. ) ;
#207462 = CARTESIAN_POINT ( 'NONE',  ( -16.89935556175704789, 66.05000000001261640, -190.3834311216385515 ) ) ;
#207463 = CIRCLE ( 'NONE', #161676, 12.97499999999999254 ) ;
#207464 = DIRECTION ( 'NONE',  ( 1.000000000000000000, 0.000000000000000000, 0.000000000000000000 ) ) ;
#207465 = CARTESIAN_POINT ( 'NONE',  ( 21.14999999999998082, 87.75000000001165290, -69.52310748452424605 ) ) ;
#207466 = DIRECTION ( 'NONE',  ( -0.000000000000000000, -0.000000000000000000, 1.000000000000000000 ) ) ;
#207467 = CARTESIAN_POINT ( 'NONE',  ( -18.50000000000000000, 76.00000000001244871, -170.0231074845243597 ) ) ;
#207468 = EDGE_CURVE ( 'NONE', #10935, #120254, #205143, .T. ) ;
#207469 = ORIENTED_EDGE ( 'NONE', *, *, #109384, .F. ) ;
#207470 = CARTESIAN_POINT ( 'NONE',  ( -23.15000000000000213, 71.65000000001259650, -191.2731074845243882 ) ) ;
#207471 = DIRECTION ( 'NONE',  ( 0.000000000000000000, -5.204170427930272346E-14, 1.000000000000000000 ) ) ;
#207472 = EDGE_CURVE ( 'NONE', #41443, #193457, #228072, .T. ) ;
#207474 = EDGE_CURVE ( 'NONE', #23667, #88823, #161539, .T. ) ;
#207473 = EDGE_CURVE ( 'NONE', #211151, #147787, #209787, .T. ) ;
#207475 = LINE ( 'NONE', #211315, #91053 ) ;
#207476 = VERTEX_POINT ( 'NONE', #108119 ) ;
#207477 = EDGE_CURVE ( 'NONE', #180058, #182048, #72873, .T. ) ;
#207478 = ORIENTED_EDGE ( 'NONE', *, *, #31639, .T. ) ;
#207479 = CARTESIAN_POINT ( 'NONE',  ( 21.05000000000003979, 74.83745509109094485, -43.92310748452479885 ) ) ;
#207480 = DIRECTION ( 'NONE',  ( -1.000000000000000000, -0.000000000000000000, -0.000000000000000000 ) ) ;
#207481 = DIRECTION ( 'NONE',  ( 0.000000000000000000, -7.086529944415886769E-15, 1.000000000000000000 ) ) ;
#207482 = ADVANCED_FACE ( 'NONE', ( #111981 ), #191533, .F. ) ;
#207483 = FACE_OUTER_BOUND ( 'NONE', #23939, .T. ) ;
#207484 = DIRECTION ( 'NONE',  ( 2.840903330521631775E-16, 0.8700118002898354908, -0.4930308989875170078 ) ) ;
#207486 = FILL_AREA_STYLE ('',( #64110 ) ) ;
#207485 = CARTESIAN_POINT ( 'NONE',  ( -20.54999999999999716, 68.75000000001185185, -90.77310748452435973 ) ) ;
#207487 = VECTOR ( 'NONE', #165811, 1000.000000000000227 ) ;
#207488 = AXIS2_PLACEMENT_3D ( 'NONE', #10853, #149092, #47384 ) ;
#207489 = AXIS2_PLACEMENT_3D ( 'NONE', #13935, #256313, #252517 ) ;
#207491 = ADVANCED_FACE ( 'NONE', ( #89817 ), #91115, .T. ) ;
#207490 = DIRECTION ( 'NONE',  ( 0.000000000000000000, -0.2128009952263604232, 0.9770955615653316162 ) ) ;
#207492 = AXIS2_PLACEMENT_3D ( 'NONE', #49000, #123413, #208100 ) ;
#207494 = ADVANCED_FACE ( 'NONE', ( #168136 ), #49425, .F. ) ;
#207493 = CARTESIAN_POINT ( 'NONE',  ( -22.49533356619861735, 64.34999999370803891, -136.5882300648471244 ) ) ;
#207495 = DIRECTION ( 'NONE',  ( 0.000000000000000000, 7.026728003956683390E-15, -1.000000000000000000 ) ) ;
#207497 = ORIENTED_EDGE ( 'NONE', *, *, #205819, .F. ) ;
#207496 = CARTESIAN_POINT ( 'NONE',  ( 13.99999999999999822, 66.15000000001185754, -86.27310748452437394 ) ) ;
#207498 = DIRECTION ( 'NONE',  ( 0.000000000000000000, 5.329070518200751394E-15, 1.000000000000000000 ) ) ;
#207499 = DIRECTION ( 'NONE',  ( -1.000000000000000000, -0.000000000000000000, 0.000000000000000000 ) ) ;
#207501 = DIRECTION ( 'NONE',  ( -2.840903330521632269E-16, 0.8454177738465993297, 0.5341055959866553016 ) ) ;
#207500 = DIRECTION ( 'NONE',  ( 4.408576920032446739E-17, 0.1350103645451945777, -0.9908441862701590219 ) ) ;
#207502 = EDGE_CURVE ( 'NONE', #15628, #86491, #113590, .T. ) ;
#207503 = ORIENTED_EDGE ( 'NONE', *, *, #110919, .F. ) ;
#207504 = CARTESIAN_POINT ( 'NONE',  ( -16.87331047859649757, 66.05000000001201954, -115.6731074845243796 ) ) ;
#207505 = DIRECTION ( 'NONE',  ( 0.000000000000000000, 0.2617529984165031243, 0.9651348961777157509 ) ) ;
#207506 = CYLINDRICAL_SURFACE ( 'NONE', #105467, 0.09999999999999939493 ) ;
#207507 = DIRECTION ( 'NONE',  ( 1.000000000000000000, 0.000000000000000000, 0.000000000000000000 ) ) ;
#207508 = ORIENTED_EDGE ( 'NONE', *, *, #201764, .T. ) ;
#207509 = ADVANCED_FACE ( 'NONE', ( #175808 ), #94957, .T. ) ;
#207510 = ORIENTED_EDGE ( 'NONE', *, *, #243476, .T. ) ;
#207511 = VECTOR ( 'NONE', #222169, 1000.000000000000000 ) ;
#207512 = EDGE_CURVE ( 'NONE', #7857, #63242, #38767, .T. ) ;
#207514 = AXIS2_PLACEMENT_3D ( 'NONE', #70603, #66728, #150131 ) ;
#207513 = FACE_OUTER_BOUND ( 'NONE', #18075, .T. ) ;
#207515 = VERTEX_POINT ( 'NONE', #157554 ) ;
#207516 = ORIENTED_EDGE ( 'NONE', *, *, #103315, .T. ) ;
#207518 = DIRECTION ( 'NONE',  ( 1.000000000000000000, -0.000000000000000000, -0.000000000000000000 ) ) ;
#207517 = AXIS2_PLACEMENT_3D ( 'NONE', #200616, #101460, #127495 ) ;
#207519 = DIRECTION ( 'NONE',  ( 0.000000000000000000, 0.000000000000000000, 1.000000000000000000 ) ) ;
#207520 = CARTESIAN_POINT ( 'NONE',  ( -20.96077737575326339, 62.98594959644117353, -207.1005776826179954 ) ) ;
#207521 = ORIENTED_EDGE ( 'NONE', *, *, #81122, .F. ) ;
#207522 = EDGE_CURVE ( 'NONE', #118763, #27421, #36298, .T. ) ;
#207523 = CARTESIAN_POINT ( 'NONE',  ( -21.05000000000000071, 11.65000000001115232, -134.1000000000000227 ) ) ;
#207524 = CARTESIAN_POINT ( 'NONE',  ( -18.51024323315077424, 68.05374558910872906, -224.1882283518532120 ) ) ;
#207525 = CARTESIAN_POINT ( 'NONE',  ( 23.40000000000005542, 87.50449464844290048, -34.18759587077607165 ) ) ;
#207526 = DIRECTION ( 'NONE',  ( -0.000000000000000000, -6.982962677686266711E-15, 1.000000000000000000 ) ) ;
#207527 = LINE ( 'NONE', #28925, #20662 ) ;
#207528 = LINE ( 'NONE', #4167, #248861 ) ;
#207529 = AXIS2_PLACEMENT_3D ( 'NONE', #235609, #256399, #153572 ) ;
#207530 = ORIENTED_EDGE ( 'NONE', *, *, #19975, .T. ) ;
#207531 = CARTESIAN_POINT ( 'NONE',  ( -16.90137573187933384, 9.950000000011137047, -180.2884174240968775 ) ) ;
#207533 = ORIENTED_EDGE ( 'NONE', *, *, #54355, .T. ) ;
#207532 = AXIS2_PLACEMENT_3D ( 'NONE', #77090, #36721, #75816 ) ;
#207534 = ORIENTED_EDGE ( 'NONE', *, *, #22397, .T. ) ;
#207535 = AXIS2_PLACEMENT_3D ( 'NONE', #234405, #55742, #135301 ) ;
#207536 = ORIENTED_EDGE ( 'NONE', *, *, #116099, .F. ) ;
#207537 = CARTESIAN_POINT ( 'NONE',  ( -23.15000000000000213, 64.35000000001150511, -48.27310748452440237 ) ) ;
#207538 = CARTESIAN_POINT ( 'NONE',  ( 15.51872946208853499, 66.62341902196831711, -152.3961612375124730 ) ) ;
#207539 = DIRECTION ( 'NONE',  ( 1.000000000000000000, 0.000000000000000000, 0.000000000000000000 ) ) ;
#207540 = CARTESIAN_POINT ( 'NONE',  ( -18.59999999999999787, -1.835859311432484375, -145.5044391687985694 ) ) ;
#207541 = ORIENTED_EDGE ( 'NONE', *, *, #162397, .T. ) ;
#207542 = CARTESIAN_POINT ( 'NONE',  ( 18.59999999999999076, 69.35000000001222986, -148.8731074845244109 ) ) ;
#207543 = AXIS2_PLACEMENT_3D ( 'NONE', #255857, #101936, #237636 ) ;
#207544 = DIRECTION ( 'NONE',  ( -1.000000000000000000, 2.952720810173289112E-16, 2.061873921506763405E-30 ) ) ;
#207545 = EDGE_LOOP ( 'NONE', ( #179373, #80028, #211454, #165533 ) ) ;
#207546 = FACE_OUTER_BOUND ( 'NONE', #16154, .T. ) ;
#207547 = ADVANCED_FACE ( 'NONE', ( #178382 ), #174563, .F. ) ;
#207548 = CARTESIAN_POINT ( 'NONE',  ( 21.05000000000000071, 4.813084112149524252, -11.94151775652382419 ) ) ;
#207549 = AXIS2_PLACEMENT_3D ( 'NONE', #233580, #74541, #172361 ) ;
#207550 = ORIENTED_EDGE ( 'NONE', *, *, #214391, .T. ) ;
#207551 = AXIS2_PLACEMENT_3D ( 'NONE', #155485, #36817, #116333 ) ;
#207552 = EDGE_CURVE ( 'NONE', #127380, #67166, #13635, .T. ) ;
#207553 = CARTESIAN_POINT ( 'NONE',  ( -16.87036670365548474, 9.989418819312801290, -188.4795601173020145 ) ) ;
#207554 = CIRCLE ( 'NONE', #211644, 11.80000000000000426 ) ;
#207555 = ORIENTED_EDGE ( 'NONE', *, *, #7513, .T. ) ;
#207556 = CARTESIAN_POINT ( 'NONE',  ( 18.56579813702275317, 65.66974365629664590, -97.43601455626048846 ) ) ;
#207558 = ORIENTED_EDGE ( 'NONE', *, *, #26038, .T. ) ;
#207557 = AXIS2_PLACEMENT_3D ( 'NONE', #98056, #21158, #57664 ) ;
#207559 = SPHERICAL_SURFACE ( 'NONE', #216990, 0.1000000000000000056 ) ;
#207560 = EDGE_CURVE ( 'NONE', #203476, #200641, #72093, .T. ) ;
#207561 = EDGE_CURVE ( 'NONE', #192523, #201210, #201076, .T. ) ;
#207562 = LINE ( 'NONE', #148871, #227309 ) ;
#207563 = DIRECTION ( 'NONE',  ( 0.000000000000000000, 0.4930308989875230585, 0.8700118002898322711 ) ) ;
#207564 = CARTESIAN_POINT ( 'NONE',  ( -21.00023020733438273, 6.244489974106951280, -199.6400166642470140 ) ) ;
#207565 = ADVANCED_FACE ( 'NONE', ( #74157 ), #238318, .F. ) ;
#207566 = VECTOR ( 'NONE', #44550, 1000.000000000000000 ) ;
#207567 = VECTOR ( 'NONE', #57395, 1000.000000000000000 ) ;
#207568 = FACE_OUTER_BOUND ( 'NONE', #230925, .T. ) ;
#207569 = CARTESIAN_POINT ( 'NONE',  ( -20.54999999999999716, 74.07476635515241981, -149.2533510176504876 ) ) ;
#207570 = ORIENTED_EDGE ( 'NONE', *, *, #210197, .F. ) ;
#207572 = CARTESIAN_POINT ( 'NONE',  ( -22.94999999999999929, -1.885425182446134107, -11.59641995933507808 ) ) ;
#207571 = AXIS2_PLACEMENT_3D ( 'NONE', #95083, #92507, #130347 ) ;
#207573 = ORIENTED_EDGE ( 'NONE', *, *, #158316, .F. ) ;
#207575 = CARTESIAN_POINT ( 'NONE',  ( -18.59999999999999787, 77.68707439010432836, -216.3376804510660065 ) ) ;
#207574 = DIRECTION ( 'NONE',  ( -1.646408749285562691E-14, -1.000000000000000000, -6.982962677686266711E-15 ) ) ;
#207576 = EDGE_CURVE ( 'NONE', #188768, #319, #153718, .T. ) ;
#207577 = AXIS2_PLACEMENT_3D ( 'NONE', #238126, #179471, #80313 ) ;
#207578 = ORIENTED_EDGE ( 'NONE', *, *, #142939, .T. ) ;
#207579 = CIRCLE ( 'NONE', #186730, 0.09999999999999939493 ) ;
#207580 = DIRECTION ( 'NONE',  ( -1.000000000000000000, 2.952720810173289112E-16, 2.061873921506763405E-30 ) ) ;
#207581 = CARTESIAN_POINT ( 'NONE',  ( -18.59999999999999787, 66.85000000001245724, -181.7731074845244166 ) ) ;
#207582 = CARTESIAN_POINT ( 'NONE',  ( 20.95378194480896639, 59.04383896832029421, -225.7962839547865883 ) ) ;
#207583 = ORIENTED_EDGE ( 'NONE', *, *, #247380, .T. ) ;
#207585 = ORIENTED_EDGE ( 'NONE', *, *, #131238, .T. ) ;
#207584 = CARTESIAN_POINT ( 'NONE',  ( -23.15000000000000213, 23.68770167995059595, -252.8127582590406348 ) ) ;
#207586 = AXIS2_PLACEMENT_3D ( 'NONE', #60265, #220638, #201067 ) ;
#207587 = DIRECTION ( 'NONE',  ( 0.000000000000000000, 0.000000000000000000, -1.000000000000000000 ) ) ;
#207588 = DIRECTION ( 'NONE',  ( -1.000000000000000000, 0.000000000000000000, 0.000000000000000000 ) ) ;
#207590 = ORIENTED_EDGE ( 'NONE', *, *, #230616, .F. ) ;
#207589 = DIRECTION ( 'NONE',  ( -1.000000000000000000, 0.000000000000000000, 0.000000000000000000 ) ) ;
#207591 = PRODUCT_DEFINITION_SHAPE ( 'NONE', 'NONE',  #155341 ) ;
#207592 = ORIENTED_EDGE ( 'NONE', *, *, #87285, .F. ) ;
#207593 = EDGE_CURVE ( 'NONE', #98647, #49064, #213533, .T. ) ;
#207594 = VECTOR ( 'NONE', #18556, 1000.000000000000000 ) ;
#207595 = CARTESIAN_POINT ( 'NONE',  ( 21.05000000000000071, 1.115600667400684642E-11, -67.00000000000004263 ) ) ;
#207597 = CLOSED_SHELL ( 'NONE', ( #131433, #71555, #95605, #16428, #211587, #195795, #77335, #190843, #160075, #83431, #80503, #83455, #9041, #243092, #98261, #119910, #181955, #11295, #185599, #251865, #17065, #214277, #148683, #84015, #51445, #41666, #33220, #27957, #131560, #68807, #91736, #107053, #233685, #25315, #130884, #62177, #40383, #207158, #95347, #41332, #175133, #7636, #25348, #149248, #219880, #34917, #41348, #36003, #41894, #154871, #120909, #195430, #111728 ) ) ;
#207596 = CARTESIAN_POINT ( 'NONE',  ( 23.14999999999999503, 64.25000000001259082, -191.3731074845244393 ) ) ;
#207598 = EDGE_LOOP ( 'NONE', ( #142790, #175992, #94368, #149239 ) ) ;
#207599 = DIRECTION ( 'NONE',  ( 1.000000000000000000, 3.265361837132813093E-16, -0.000000000000000000 ) ) ;
#207600 = ORIENTED_EDGE ( 'NONE', *, *, #199990, .F. ) ;
#207601 = LINE ( 'NONE', #124208, #36692 ) ;
#207602 = DIRECTION ( 'NONE',  ( 1.000000000000000000, 0.000000000000000000, 0.000000000000000000 ) ) ;
#207603 = VERTEX_POINT ( 'NONE', #139199 ) ;
#207604 = EDGE_CURVE ( 'NONE', #205178, #50106, #184487, .T. ) ;
#207605 = FACE_OUTER_BOUND ( 'NONE', #7242, .T. ) ;
#207606 = AXIS2_PLACEMENT_3D ( 'NONE', #4386, #104745, #170919 ) ;
#207607 = EDGE_CURVE ( 'NONE', #90674, #225961, #59566, .T. ) ;
#207609 = ORIENTED_EDGE ( 'NONE', *, *, #2228, .T. ) ;
#207608 = AXIS2_PLACEMENT_3D ( 'NONE', #182494, #165492, #101609 ) ;
#207610 = CARTESIAN_POINT ( 'NONE',  ( -16.89268316805465986, 66.04827818676933759, -48.66735500597884823 ) ) ;
#207611 = AXIS2_PLACEMENT_3D ( 'NONE', #93833, #246491, #209954 ) ;
#207612 = ADVANCED_FACE ( 'NONE', ( #234464 ), #87420, .T. ) ;
#207613 = ORIENTED_EDGE ( 'NONE', *, *, #252166, .F. ) ;
#207614 = ORIENTED_EDGE ( 'NONE', *, *, #172760, .F. ) ;
#207615 = CARTESIAN_POINT ( 'NONE',  ( -22.59999999999999787, 64.08545097430041437, -247.0723585184913986 ) ) ;
#207616 = VERTEX_POINT ( 'NONE', #2261 ) ;
#207617 = CARTESIAN_POINT ( 'NONE',  ( -17.11825945287481332, 65.95000000001225260, -149.1731074845244223 ) ) ;
#207618 = VERTEX_POINT ( 'NONE', #23155 ) ;
#207620 = ORIENTED_EDGE ( 'NONE', *, *, #162551, .T. ) ;
#207619 = DIRECTION ( 'NONE',  ( 0.000000000000000000, 0.2128009952263485993, -0.9770955615653341697 ) ) ;
#207621 = EDGE_CURVE ( 'NONE', #72558, #70690, #167779, .T. ) ;
#207622 = EDGE_CURVE ( 'NONE', #152046, #70458, #34505, .T. ) ;
#207623 = DIRECTION ( 'NONE',  ( -1.000000000000000000, 0.000000000000000000, 0.000000000000000000 ) ) ;
#207624 = VERTEX_POINT ( 'NONE', #163931 ) ;
#207625 = CARTESIAN_POINT ( 'NONE',  ( 23.24999999999999645, 76.00000000001142553, -36.02310748452432421 ) ) ;
#207626 = AXIS2_PLACEMENT_3D ( 'NONE', #93246, #37153, #115376 ) ;
#207627 = AXIS2_PLACEMENT_3D ( 'NONE', #152630, #206152, #71796 ) ;
#207628 = EDGE_LOOP ( 'NONE', ( #169038, #229147, #89661, #40459 ) ) ;
#207631 = VERTEX_POINT ( 'NONE', #119678 ) ;
#207630 = ORIENTED_EDGE ( 'NONE', *, *, #201985, .T. ) ;
#207629 = CARTESIAN_POINT ( 'NONE',  ( -23.15000000000000213, 1.115600667400684642E-11, -200.9999999999999432 ) ) ;
#207632 = DIRECTION ( 'NONE',  ( -0.000000000000000000, 0.9770955615653316162, 0.2128009952263603122 ) ) ;
#207633 = EDGE_CURVE ( 'NONE', #32735, #218469, #62258, .T. ) ;
#207634 = AXIS2_PLACEMENT_3D ( 'NONE', #191751, #74374, #153926 ) ;
#207635 = FACE_OUTER_BOUND ( 'NONE', #205138, .T. ) ;
#207636 = ORIENTED_EDGE ( 'NONE', *, *, #10949, .T. ) ;
#207637 = AXIS2_PLACEMENT_3D ( 'NONE', #15230, #150869, #193859 ) ;
#207638 = ORIENTED_EDGE ( 'NONE', *, *, #24179, .F. ) ;
#207639 = DIRECTION ( 'NONE',  ( 0.000000000000000000, 0.000000000000000000, 1.000000000000000000 ) ) ;
#207640 = ADVANCED_FACE ( 'NONE', ( #242172 ), #20584, .F. ) ;
#207641 = DIRECTION ( 'NONE',  ( -1.000000000000000000, 3.151514657663852580E-16, -8.547182517843351137E-17 ) ) ;
#207643 = VERTEX_POINT ( 'NONE', #124806 ) ;
#207642 = CARTESIAN_POINT ( 'NONE',  ( -33.72168855820452649, 64.52683809665015247, -194.2731074845244450 ) ) ;
#207644 = LINE ( 'NONE', #68116, #231267 ) ;
#207645 = EDGE_LOOP ( 'NONE', ( #91844, #54647, #162544, #29540 ) ) ;
#207646 = DIRECTION ( 'NONE',  ( -0.000000000000000000, -0.000000000000000000, -1.000000000000000000 ) ) ;
#207647 = DIRECTION ( 'NONE',  ( 0.000000000000000000, -6.652207440891569552E-15, 1.000000000000000000 ) ) ;
#207648 = VECTOR ( 'NONE', #71563, 1000.000000000000000 ) ;
#207649 = ORIENTED_EDGE ( 'NONE', *, *, #77470, .F. ) ;
#207650 = DIRECTION ( 'NONE',  ( -1.000000000000000000, -2.952720810173289112E-16, 0.000000000000000000 ) ) ;
#207651 = FACE_OUTER_BOUND ( 'NONE', #42798, .T. ) ;
#207652 = ORIENTED_EDGE ( 'NONE', *, *, #84236, .F. ) ;
#207654 = VERTEX_POINT ( 'NONE', #102633 ) ;
#207653 = CARTESIAN_POINT ( 'NONE',  ( 5.551115123125782702E-14, 64.35000000001120668, -3.023107484524792277 ) ) ;
#207655 = CARTESIAN_POINT ( 'NONE',  ( -16.91256925476569606, 14.21894878281401198, -219.3624168839846789 ) ) ;
#207657 = ORIENTED_EDGE ( 'NONE', *, *, #246573, .F. ) ;
#207656 = VERTEX_POINT ( 'NONE', #24443 ) ;
#207658 = ORIENTED_EDGE ( 'NONE', *, *, #134158, .F. ) ;
#207659 = DIRECTION ( 'NONE',  ( 0.000000000000000000, 0.8814952561688431665, -0.4721928772777345129 ) ) ;
#207660 = VERTEX_POINT ( 'NONE', #141781 ) ;
#207661 = CARTESIAN_POINT ( 'NONE',  ( 20.85000000000000142, 67.85125148167622910, -227.9794913823769491 ) ) ;
#207662 = ORIENTED_EDGE ( 'NONE', *, *, #15219, .F. ) ;
#207663 = CARTESIAN_POINT ( 'NONE',  ( -21.05000000000000071, 1.115600667400684642E-11, -37.79999999999996163 ) ) ;
#207664 = CARTESIAN_POINT ( 'NONE',  ( 21.87500000000000355, 52.06567329910104291, -231.9654557484363409 ) ) ;
#207665 = ORIENTED_EDGE ( 'NONE', *, *, #19151, .F. ) ;
#207666 = EDGE_LOOP ( 'NONE', ( #15889, #67869, #141159 ) ) ;
#207667 = AXIS2_PLACEMENT_3D ( 'NONE', #65398, #224464, #47097 ) ;
#207668 = AXIS2_PLACEMENT_3D ( 'NONE', #193551, #57857, #94428 ) ;
#207669 = AXIS2_PLACEMENT_3D ( 'NONE', #132086, #14734, #227329 ) ;
#207670 = EDGE_LOOP ( 'NONE', ( #209311, #48098, #124298 ) ) ;
#207671 = EDGE_CURVE ( 'NONE', #50639, #124804, #51194, .T. ) ;
#207672 = AXIS2_PLACEMENT_3D ( 'NONE', #5657, #25271, #146464 ) ;
#207673 = CARTESIAN_POINT ( 'NONE',  ( -20.94999999999999929, -11.64999999998884483, -131.0000000000000284 ) ) ;
#207674 = EDGE_LOOP ( 'NONE', ( #65068, #128371 ) ) ;
#207675 = EDGE_CURVE ( 'NONE', #247506, #6846, #172070, .T. ) ;
#207677 = VERTEX_POINT ( 'NONE', #239619 ) ;
#207676 = DIRECTION ( 'NONE',  ( -1.000000000000000000, -3.265361837132813093E-16, 0.000000000000000000 ) ) ;
#207678 = CARTESIAN_POINT ( 'NONE',  ( -20.94999999999999929, -11.48912529307605546, -30.59999999999999432 ) ) ;
#207679 = CYLINDRICAL_SURFACE ( 'NONE', #26804, 0.1000000000000028644 ) ;
#207680 = DIRECTION ( 'NONE',  ( 0.000000000000000000, -1.000000000000000000, -0.000000000000000000 ) ) ;
#207681 = CARTESIAN_POINT ( 'NONE',  ( -16.92507428761700083, 9.949999999999983302, -20.78660254037844624 ) ) ;
#207682 = CARTESIAN_POINT ( 'NONE',  ( 20.85000000000000142, 77.85161776048096272, -124.9199177649206689 ) ) ;
#207683 = EDGE_CURVE ( 'NONE', #130981, #160723, #55287, .T. ) ;
#207686 = DIRECTION ( 'NONE',  ( 0.000000000000000000, 1.000000000000000000, 0.000000000000000000 ) ) ;
#207685 = AXIS2_PLACEMENT_3D ( 'NONE', #1705, #121691, #159526 ) ;
#207684 = DIRECTION ( 'NONE',  ( 0.000000000000000000, -0.9651348961777158619, 0.2617529984165031243 ) ) ;
#207689 = ADVANCED_FACE ( 'NONE', ( #25702 ), #64815, .T. ) ;
#207688 = CARTESIAN_POINT ( 'NONE',  ( 21.07928932188134397, 10.02993822722304351, -228.1074463178677263 ) ) ;
#207687 = AXIS2_PLACEMENT_3D ( 'NONE', #97981, #257034, #237531 ) ;
#207690 = CARTESIAN_POINT ( 'NONE',  ( 18.46163235739464881, 38.05111684352567636, -261.0515469419265742 ) ) ;
#207691 = AXIS2_PLACEMENT_3D ( 'NONE', #127361, #201753, #204311 ) ;
#207692 = CARTESIAN_POINT ( 'NONE',  ( -20.85000000000000142, 10.33248238083635151, -72.59484654391314962 ) ) ;
#207693 = EDGE_LOOP ( 'NONE', ( #212085, #245385 ) ) ;
#207694 = CIRCLE ( 'NONE', #257679, 0.09999999999999939493 ) ;
#207695 = ORIENTED_EDGE ( 'NONE', *, *, #14009, .T. ) ;
#207697 = ORIENTED_EDGE ( 'NONE', *, *, #256490, .T. ) ;
#207696 = DIRECTION ( 'NONE',  ( 0.000000000000000000, -0.4999999999999689138, -0.8660254037844565822 ) ) ;
#207698 = VERTEX_POINT ( 'NONE', #41434 ) ;
#207699 = EDGE_CURVE ( 'NONE', #231927, #214748, #42857, .T. ) ;
#207700 = DIRECTION ( 'NONE',  ( 0.000000000000000000, -0.9856811345164800953, -0.1686199900910462790 ) ) ;
#207701 = CARTESIAN_POINT ( 'NONE',  ( 20.97107704358301916, 8.875478152032441059, -142.5589732293892951 ) ) ;
#207703 = CARTESIAN_POINT ( 'NONE',  ( 20.94999999999999574, -1.835341550213255957, -145.5551512925629822 ) ) ;
#207702 = CARTESIAN_POINT ( 'NONE',  ( 20.96937028524355640, 39.15198068096341899, -236.7924211901758156 ) ) ;
#207704 = ORIENTED_EDGE ( 'NONE', *, *, #146748, .F. ) ;
#207705 = ORIENTED_EDGE ( 'NONE', *, *, #224833, .F. ) ;
#207706 = DIRECTION ( 'NONE',  ( -0.7071067811865475727, -0.7071067811865475727, -0.000000000000000000 ) ) ;
#207707 = AXIS2_PLACEMENT_3D ( 'NONE', #55659, #195243, #136497 ) ;
#207708 = CARTESIAN_POINT ( 'NONE',  ( 20.94999999999999929, 85.00000000001261924, -193.6291383618718385 ) ) ;
#207709 = VERTEX_POINT ( 'NONE', #3556 ) ;
#207710 = AXIS2_PLACEMENT_3D ( 'NONE', #97603, #64916, #147014 ) ;
#207711 = AXIS2_PLACEMENT_3D ( 'NONE', #145574, #225095, #46467 ) ;
#207712 = CARTESIAN_POINT ( 'NONE',  ( 22.50000000000000000, 68.25000000001267608, -203.6231074845244109 ) ) ;
#207713 = DIRECTION ( 'NONE',  ( 1.000000000000000000, 0.000000000000000000, 0.000000000000000000 ) ) ;
#207714 = DIRECTION ( 'NONE',  ( 0.000000000000000000, 3.208737065390628822E-15, 1.000000000000000000 ) ) ;
#207715 = CARTESIAN_POINT ( 'NONE',  ( -18.59999999999999787, 7.128833340094563376, -233.7327013124401276 ) ) ;
#207716 = EDGE_CURVE ( 'NONE', #246680, #242521, #200488, .T. ) ;
#207717 = FACE_OUTER_BOUND ( 'NONE', #227707, .T. ) ;
#207719 = ORIENTED_EDGE ( 'NONE', *, *, #50951, .T. ) ;
#207718 = DIRECTION ( 'NONE',  ( -0.000000000000000000, -0.8700118002898356018, 0.4930308989875170078 ) ) ;
#207720 = EDGE_CURVE ( 'NONE', #35577, #6603, #240902, .T. ) ;
#207721 = CIRCLE ( 'NONE', #211814, 0.5000000000000004441 ) ;
#207722 = CARTESIAN_POINT ( 'NONE',  ( -20.65000000000000568, 5.650000000011139001, -154.8500000000000227 ) ) ;
#207723 = CYLINDRICAL_SURFACE ( 'NONE', #169017, 0.1000000000000028644 ) ;
#207724 = CARTESIAN_POINT ( 'NONE',  ( -23.15000000000000213, 8.980461154494397746, -187.0187154576991304 ) ) ;
#207725 = CARTESIAN_POINT ( 'NONE',  ( 18.51565452909439813, 85.35285933885081988, -95.82819816328898810 ) ) ;
#207726 = EDGE_LOOP ( 'NONE', ( #31877, #188904, #36605, #145391 ) ) ;
#207727 = CARTESIAN_POINT ( 'NONE',  ( -16.77683809663752257, 60.94702803318471496, -221.0293550571836647 ) ) ;
#207728 = DIRECTION ( 'NONE',  ( 0.7071067811865474617, -0.7071067811865474617, -4.937700262164531476E-15 ) ) ;
#207729 = B_SPLINE_CURVE_WITH_KNOTS ( 'NONE', 3,
 ( #186015, #245996, #85589, #227694, #183457, #88163, #4779, #203003, #165168, #24397 ),
 .UNSPECIFIED., .F., .F.,
 ( 4, 2, 2, 2, 4 ),
 ( 0.000000000000000000, 0.0001660831991682657036, 0.0002491247987523985690, 0.0002906455985444294263, 0.0003321663983364602293 ),
 .UNSPECIFIED. ) ;
#207731 = DIRECTION ( 'NONE',  ( 0.000000000000000000, 0.000000000000000000, -1.000000000000000000 ) ) ;
#207730 = DIRECTION ( 'NONE',  ( 0.000000000000000000, 0.000000000000000000, -1.000000000000000000 ) ) ;
#207732 = CYLINDRICAL_SURFACE ( 'NONE', #149734, 11.74999999999999645 ) ;
#207733 = DIRECTION ( 'NONE',  ( 0.000000000000000000, -0.2128009952263604232, 0.9770955615653316162 ) ) ;
#207734 = EDGE_CURVE ( 'NONE', #144818, #97476, #150781, .T. ) ;
#207735 = CARTESIAN_POINT ( 'NONE',  ( -20.94999999999999929, -11.48912529306489994, -164.4000000000000057 ) ) ;
#207736 = CARTESIAN_POINT ( 'NONE',  ( -16.79363873026997922, 66.05114977059308501, -48.67695370307892233 ) ) ;
#207737 = TOROIDAL_SURFACE ( 'NONE', #111869, 0.9750000000000019762, 0.1000000000000000056 ) ;
#207738 = AXIS2_PLACEMENT_3D ( 'NONE', #223755, #46403, #20783 ) ;
#207739 = CARTESIAN_POINT ( 'NONE',  ( 20.04142135623730070, 11.65000000001115943, -88.35000000000003695 ) ) ;
#207740 = CARTESIAN_POINT ( 'NONE',  ( 23.14999999999999503, 11.65000000001116298, -127.0851942293460866 ) ) ;
#207741 = AXIS2_PLACEMENT_3D ( 'NONE', #22205, #242513, #102988 ) ;
#207742 = ORIENTED_EDGE ( 'NONE', *, *, #180829, .T. ) ;
#207743 = ORIENTED_EDGE ( 'NONE', *, *, #91028, .F. ) ;
#207744 = ORIENTED_EDGE ( 'NONE', *, *, #256337, .T. ) ;
#207745 = CARTESIAN_POINT ( 'NONE',  ( 20.12481660106788439, 66.47365600773694894, -94.79696581543133505 ) ) ;
#207746 = DIRECTION ( 'NONE',  ( 2.889348024582214003E-16, -0.1332476588733650935, -0.9910827722268042983 ) ) ;
#207747 = VERTEX_POINT ( 'NONE', #29583 ) ;
#207748 = AXIS2_PLACEMENT_3D ( 'NONE', #112480, #66912, #128179 ) ;
#207749 = AXIS2_PLACEMENT_3D ( 'NONE', #92340, #171925, #113193 ) ;
#207751 = EDGE_CURVE ( 'NONE', #250150, #74197, #24852, .T. ) ;
#207750 = VERTEX_POINT ( 'NONE', #92084 ) ;
#207752 = AXIS2_PLACEMENT_3D ( 'NONE', #196606, #114512, #152385 ) ;
#207753 = ORIENTED_EDGE ( 'NONE', *, *, #76395, .F. ) ;
#207754 = CARTESIAN_POINT ( 'NONE',  ( 21.05000000000000071, 11.60058429089262333, -246.3380203656811887 ) ) ;
#207755 = ORIENTED_EDGE ( 'NONE', *, *, #98706, .T. ) ;
#207757 = CARTESIAN_POINT ( 'NONE',  ( -23.15000000000000213, 64.35000000001222986, -148.2731074845243882 ) ) ;
#207756 = AXIS2_PLACEMENT_3D ( 'NONE', #147410, #7917, #246504 ) ;
#207758 = CARTESIAN_POINT ( 'NONE',  ( -16.79363873026997922, 66.05114977059336923, -82.17695370307890812 ) ) ;
#207759 = CIRCLE ( 'NONE', #166077, 12.97499999999998721 ) ;
#207760 = AXIS2_PLACEMENT_3D ( 'NONE', #184924, #114036, #252262 ) ;
#207761 = CARTESIAN_POINT ( 'NONE',  ( -18.59999999999999787, 64.35000000001161879, -62.50830171387039513 ) ) ;
#207762 = CARTESIAN_POINT ( 'NONE',  ( 23.14999999999998437, 1.115600667400684642E-11, -33.50000000000000000 ) ) ;
#207763 = EDGE_CURVE ( 'NONE', #67597, #225539, #196964, .T. ) ;
#207764 =( BOUNDED_CURVE ( )  B_SPLINE_CURVE ( 3, ( #188525, #108976, #189818, #93269 ),
 .UNSPECIFIED., .F., .F. ) 
 B_SPLINE_CURVE_WITH_KNOTS ( ( 4, 4 ),
 ( 0.000000000000000000, 1.570796326794908992 ),
 .UNSPECIFIED. ) 
 CURVE ( )  GEOMETRIC_REPRESENTATION_ITEM ( )  RATIONAL_B_SPLINE_CURVE ( ( 1.000000000000000000, 0.8047378541243619399, 0.8047378541243619399, 1.000000000000000000 ) ) 
 REPRESENTATION_ITEM ( '' )  );
#207765 = CARTESIAN_POINT ( 'NONE',  ( -23.15000000000000213, 1.115600667400684642E-11, -200.9999999999999432 ) ) ;
#207766 = DIRECTION ( 'NONE',  ( 0.000000000000000000, 0.000000000000000000, -1.000000000000000000 ) ) ;
#207768 = EDGE_LOOP ( 'NONE', ( #123771, #86036, #242347, #124194 ) ) ;
#207767 = DIRECTION ( 'NONE',  ( 1.000000000000000000, 0.000000000000000000, 0.000000000000000000 ) ) ;
#207770 = CARTESIAN_POINT ( 'NONE',  ( 21.14999999999999858, 8.786607556611267356, -79.25000000000004263 ) ) ;
#207769 = LINE ( 'NONE', #6970, #13010 ) ;
#207771 = CIRCLE ( 'NONE', #82796, 7.720710678118662962 ) ;
#207772 = DIRECTION ( 'NONE',  ( 0.000000000000000000, 0.000000000000000000, -1.000000000000000000 ) ) ;
#207773 = ORIENTED_EDGE ( 'NONE', *, *, #43348, .T. ) ;
#207774 = CARTESIAN_POINT ( 'NONE',  ( 12.84233041328156588, 66.58946139148318366, -121.0904194873834854 ) ) ;
#207775 = CARTESIAN_POINT ( 'NONE',  ( -22.39999999999999858, -0.1008583690875579364, -155.7504328765105868 ) ) ;
#207777 = ADVANCED_FACE ( 'NONE', ( #152088 ), #7405, .T. ) ;
#207776 = DIRECTION ( 'NONE',  ( -1.000000000000000000, 0.000000000000000000, 0.000000000000000000 ) ) ;
#207778 = EDGE_CURVE ( 'NONE', #24117, #193233, #222066, .T. ) ;
#207779 = ORIENTED_EDGE ( 'NONE', *, *, #78503, .F. ) ;
#207780 = CARTESIAN_POINT ( 'NONE',  ( -18.59999999999999787, 7.250000000011155521, -88.35000000000003695 ) ) ;
#207781 = CARTESIAN_POINT ( 'NONE',  ( -16.92280123533721792, 66.05000000001182059, -82.37373979860946349 ) ) ;
#207782 = VECTOR ( 'NONE', #43723, 1000.000000000000000 ) ;
#207784 = EDGE_LOOP ( 'NONE', ( #224058, #67697, #101536, #214628 ) ) ;
#207783 = CIRCLE ( 'NONE', #182846, 7.800000000000001599 ) ;
#207785 = EDGE_CURVE ( 'NONE', #46619, #14082, #209632, .T. ) ;
#207786 = CARTESIAN_POINT ( 'NONE',  ( -21.05000000000000071, -0.2561057920810652089, -66.96510355832775474 ) ) ;
#207787 = AXIS2_PLACEMENT_3D ( 'NONE', #220380, #221622, #3885 ) ;
#207789 = ADVANCED_FACE ( 'NONE', ( #230308 ), #248595, .T. ) ;
#207788 = CARTESIAN_POINT ( 'NONE',  ( -18.59999999999999787, 9.250000000011157297, -112.8500000000000369 ) ) ;
#207790 = DIRECTION ( 'NONE',  ( -1.646408749285562691E-14, 1.000000000000000000, 0.000000000000000000 ) ) ;
#207791 = CARTESIAN_POINT ( 'NONE',  ( -20.05000000000000426, 66.75000000001151079, -48.27310748452438816 ) ) ;
#207792 = VERTEX_POINT ( 'NONE', #247300 ) ;
#207793 = EDGE_CURVE ( 'NONE', #222093, #101654, #251310, .T. ) ;
#207794 = VERTEX_POINT ( 'NONE', #68682 ) ;
#207795 = AXIS2_PLACEMENT_3D ( 'NONE', #234365, #76579, #151000 ) ;
#207796 = CIRCLE ( 'NONE', #78588, 0.1000000000000000472 ) ;
#207797 = DIRECTION ( 'NONE',  ( -0.000000000000000000, 0.1298341882520022694, 0.9915357197604853789 ) ) ;
#207798 = CYLINDRICAL_SURFACE ( 'NONE', #77340, 0.09999999999999970024 ) ;
#207799 = EDGE_CURVE ( 'NONE', #82729, #248843, #9707, .T. ) ;
#207800 = CARTESIAN_POINT ( 'NONE',  ( 21.30000000000002558, 32.96286418198890544, -251.2069521516576174 ) ) ;
#207801 = DIRECTION ( 'NONE',  ( 1.000000000000000000, 0.000000000000000000, 0.000000000000000000 ) ) ;
#207802 = AXIS2_PLACEMENT_3D ( 'NONE', #223832, #203000, #915 ) ;
#207803 = DIRECTION ( 'NONE',  ( 1.000000000000000000, 0.000000000000000000, 0.000000000000000000 ) ) ;
#207804 = DIRECTION ( 'NONE',  ( 0.000000000000000000, 0.000000000000000000, -1.000000000000000000 ) ) ;
#207806 = EDGE_CURVE ( 'NONE', #255801, #211746, #251140, .T. ) ;
#207805 = DIRECTION ( 'NONE',  ( -0.000000000000000000, -1.000000000000000000, 6.308085367188393199E-16 ) ) ;
#207808 = EDGE_CURVE ( 'NONE', #110056, #179549, #1325, .T. ) ;
#207807 = DIRECTION ( 'NONE',  ( 1.000000000000000000, 0.000000000000000000, 0.000000000000000000 ) ) ;
#207809 = EDGE_LOOP ( 'NONE', ( #195992, #58803, #18282, #166069 ) ) ;
#207810 = FACE_OUTER_BOUND ( 'NONE', #233795, .T. ) ;
#207811 = CIRCLE ( 'NONE', #24657, 7.800000000000001599 ) ;
#207813 = ORIENTED_EDGE ( 'NONE', *, *, #236939, .F. ) ;
#207812 = DIRECTION ( 'NONE',  ( 0.000000000000000000, 1.000000000000000000, 1.156482317317873105E-15 ) ) ;
#207814 = DIRECTION ( 'NONE',  ( -0.000000000000000000, 0.1332476588733589318, 0.9910827722268049644 ) ) ;
#207815 = LINE ( 'NONE', #253321, #232376 ) ;
#207816 = DIRECTION ( 'NONE',  ( 0.000000000000000000, 0.2617529984165046231, 0.9651348961777154178 ) ) ;
#207817 = CARTESIAN_POINT ( 'NONE',  ( -16.80891096016329911, 66.05000000001207638, -123.8907702917925064 ) ) ;
#207818 = EDGE_CURVE ( 'NONE', #16570, #221411, #191222, .T. ) ;
#207819 = DIRECTION ( 'NONE',  ( 0.000000000000000000, 0.000000000000000000, -1.000000000000000000 ) ) ;
#207821 = ORIENTED_EDGE ( 'NONE', *, *, #23538, .F. ) ;
#207820 = CARTESIAN_POINT ( 'NONE',  ( 19.90000000000000924, 1.350000000000000089, 21.90000000000000213 ) ) ;
#207822 = DIRECTION ( 'NONE',  ( 1.000000000000000000, 0.000000000000000000, 0.000000000000000000 ) ) ;
#207823 = DIRECTION ( 'NONE',  ( 1.000000000000000000, 0.000000000000000000, 0.000000000000000000 ) ) ;
#207824 = CARTESIAN_POINT ( 'NONE',  ( -18.59999999999999787, 77.44184265367995579, -241.6694879557322508 ) ) ;
#207825 = CARTESIAN_POINT ( 'NONE',  ( 23.14999999999998437, 1.115600667400684642E-11, -71.05000000000003979 ) ) ;
#207826 = ORIENTED_EDGE ( 'NONE', *, *, #87017, .T. ) ;
#207827 = CARTESIAN_POINT ( 'NONE',  ( -23.25000000000000000, 68.78821595027156377, -214.2597350192734211 ) ) ;
#207828 = ADVANCED_FACE ( 'NONE', ( #109074 ), #170399, .F. ) ;
#207829 = CARTESIAN_POINT ( 'NONE',  ( -16.84793658983450726, 66.05000000001203375, -115.7567541623343743 ) ) ;
#207831 = ORIENTED_EDGE ( 'NONE', *, *, #11855, .T. ) ;
#207830 = CIRCLE ( 'NONE', #116231, 0.1000000000000028644 ) ;
#207832 = CIRCLE ( 'NONE', #220284, 0.1999999999999987899 ) ;
#207833 = EDGE_CURVE ( 'NONE', #151026, #87941, #130515, .T. ) ;
#207834 = LINE ( 'NONE', #152666, #63022 ) ;
#207835 = TOROIDAL_SURFACE ( 'NONE', #116235, 0.2000000000000000111, 0.1000000000000000056 ) ;
#207836 = EDGE_CURVE ( 'NONE', #40541, #100962, #12579, .T. ) ;
#207837 = CARTESIAN_POINT ( 'NONE',  ( -23.15000000000000213, 1.910280373842930812, -188.3686321448010403 ) ) ;
#207838 = EDGE_LOOP ( 'NONE', ( #79995, #188917, #226940, #33595, #247620 ) ) ;
#207839 = CARTESIAN_POINT ( 'NONE',  ( 18.59999999999999076, 10.20857864377385127, -192.2499999999999716 ) ) ;
#207840 = ORIENTED_EDGE ( 'NONE', *, *, #18790, .F. ) ;
#207841 = DIRECTION ( 'NONE',  ( 0.000000000000000000, 0.1298341882519953583, 0.9915357197604861561 ) ) ;
#207842 = DIRECTION ( 'NONE',  ( -1.000000000000000000, 0.000000000000000000, 0.000000000000000000 ) ) ;
#207843 = LINE ( 'NONE', #103549, #139313 ) ;
#207844 = ORIENTED_EDGE ( 'NONE', *, *, #125412, .T. ) ;
#207845 = EDGE_CURVE ( 'NONE', #55613, #101037, #197147, .T. ) ;
#207846 =( BOUNDED_CURVE ( )  B_SPLINE_CURVE ( 3, ( #419, #103366, #182946, #220771 ),
 .UNSPECIFIED., .F., .F. ) 
 B_SPLINE_CURVE_WITH_KNOTS ( ( 4, 4 ),
 ( 5.733388419619901200, 5.983100554402347449 ),
 .UNSPECIFIED. ) 
 CURVE ( )  GEOMETRIC_REPRESENTATION_ITEM ( )  RATIONAL_B_SPLINE_CURVE ( ( 1.000000000000000000, 0.9948104011409417691, 0.9948104011409417691, 1.000000000000000000 ) ) 
 REPRESENTATION_ITEM ( '' )  );
#207847 = EDGE_CURVE ( 'NONE', #15440, #253585, #80410, .T. ) ;
#207848 = DIRECTION ( 'NONE',  ( 1.000000000000000000, 0.000000000000000000, 0.000000000000000000 ) ) ;
#207849 = DIRECTION ( 'NONE',  ( 1.186688945009010077E-16, 1.000000000000000000, 6.982962677686266711E-15 ) ) ;
#207850 = CARTESIAN_POINT ( 'NONE',  ( 15.74999999999999289, 9.349999999999985434, -16.86574316727392286 ) ) ;
#207851 = FACE_OUTER_BOUND ( 'NONE', #2371, .T. ) ;
#207852 = ORIENTED_EDGE ( 'NONE', *, *, #207303, .T. ) ;
#207854 = VERTEX_POINT ( 'NONE', #93365 ) ;
#207853 = CARTESIAN_POINT ( 'NONE',  ( 20.94403535211772294, 10.30632246271647467, -106.0041836778896283 ) ) ;
#207855 = VERTEX_POINT ( 'NONE', #132504 ) ;
#207856 = LINE ( 'NONE', #205237, #19660 ) ;
#207857 = ORIENTED_EDGE ( 'NONE', *, *, #231528, .T. ) ;
#207858 = DIRECTION ( 'NONE',  ( -1.000000000000000000, 0.000000000000000000, 0.000000000000000000 ) ) ;
#207859 = CARTESIAN_POINT ( 'NONE',  ( 20.94999999999999929, 10.72371710471867701, -141.6649135690876165 ) ) ;
#207860 = ORIENTED_EDGE ( 'NONE', *, *, #29389, .F. ) ;
#207861 = DIRECTION ( 'NONE',  ( 0.000000000000000000, -0.1335171055202901413, -0.9910465087640860649 ) ) ;
#207862 = CARTESIAN_POINT ( 'NONE',  ( -23.25000000000000000, 87.65000000001144542, -39.12310748452424747 ) ) ;
#207863 = CARTESIAN_POINT ( 'NONE',  ( 18.54286124688534088, -9.623917578786652882, -140.7412023318627234 ) ) ;
#207864 = ORIENTED_EDGE ( 'NONE', *, *, #90833, .F. ) ;
#207865 = DIRECTION ( 'NONE',  ( 0.000000000000000000, -0.1298341882520079038, -0.9915357197604846018 ) ) ;
#207866 = ORIENTED_EDGE ( 'NONE', *, *, #206076, .F. ) ;
#207867 = DIRECTION ( 'NONE',  ( 1.000000000000000000, 0.000000000000000000, -1.020425574104004196E-15 ) ) ;
#207868 = DIRECTION ( 'NONE',  ( 0.000000000000000000, -0.9908441862701596881, -0.1350103645451904977 ) ) ;
#207869 = CIRCLE ( 'NONE', #141198, 0.09999999999999062417 ) ;
#207870 = EDGE_CURVE ( 'NONE', #67694, #1155, #101245, .T. ) ;
#207871 = AXIS2_PLACEMENT_3D ( 'NONE', #220518, #40630, #197076 ) ;
#207872 = VECTOR ( 'NONE', #15065, 1000.000000000000227 ) ;
#207873 = CIRCLE ( 'NONE', #78811, 0.09999999999999939493 ) ;
#207874 = EDGE_CURVE ( 'NONE', #41050, #239914, #34680, .T. ) ;
#207875 = ORIENTED_EDGE ( 'NONE', *, *, #164339, .T. ) ;
#207876 =( BOUNDED_SURFACE ( )  B_SPLINE_SURFACE ( 3, 2, ( 
 ( #37897, #217767, #178704 ),
 ( #79543, #254329, #75729 ),
 ( #18, #177415, #162631 ),
 ( #114841, #135671, #213944 ) ),
 .UNSPECIFIED., .F., .F., .F. ) 
 B_SPLINE_SURFACE_WITH_KNOTS ( ( 4, 4 ),
 ( 3, 3 ),
 ( 5.727910411845712702, 5.983100554402349225 ),
 ( 0.000000000000000000, 1.000000000000000000 ),
 .UNSPECIFIED. ) 
 GEOMETRIC_REPRESENTATION_ITEM ( )  RATIONAL_B_SPLINE_SURFACE ( (
 ( 1.000000000000000000, 0.8946697475932277044, 1.000000000000000000),
 ( 1.000000000000000000, 0.9035312726220163793, 1.000000000000000000),
 ( 1.000000000000000000, 0.9104333467450778095, 1.000000000000000000),
 ( 1.000000000000000000, 0.9152888060719297503, 1.000000000000000000) ) ) 
 REPRESENTATION_ITEM ( '' )  SURFACE ( )  );
#207877 = DIRECTION ( 'NONE',  ( -1.000000000000000000, -0.000000000000000000, -0.000000000000000000 ) ) ;
#207878 = CARTESIAN_POINT ( 'NONE',  ( 21.00000000000000000, 9.750000000011153745, -54.65000000000000568 ) ) ;
#207879 = TOROIDAL_SURFACE ( 'NONE', #187027, 0.2000000000000000111, 0.1000000000000000056 ) ;
#207880 = DIRECTION ( 'NONE',  ( 1.000000000000000000, 0.000000000000000000, -0.000000000000000000 ) ) ;
#207881 = ORIENTED_EDGE ( 'NONE', *, *, #192484, .T. ) ;
#207882 = CARTESIAN_POINT ( 'NONE',  ( -23.25000000000000000, 64.25000000001249134, -177.0379132551784096 ) ) ;
#207883 = CARTESIAN_POINT ( 'NONE',  ( -21.14999999999999858, 87.75000000001236344, -167.1231074845242688 ) ) ;
#207884 = EDGE_LOOP ( 'NONE', ( #97265, #68356, #219698, #112464 ) ) ;
#207885 = AXIS2_PLACEMENT_3D ( 'NONE', #122322, #184849, #201853 ) ;
#207886 = AXIS2_PLACEMENT_3D ( 'NONE', #135565, #75632, #114739 ) ;
#207887 = EDGE_CURVE ( 'NONE', #126780, #157985, #76327, .T. ) ;
#207888 = VECTOR ( 'NONE', #214128, 1000.000000000000114 ) ;
#207889 = ORIENTED_EDGE ( 'NONE', *, *, #249193, .T. ) ;
#207890 = DIRECTION ( 'NONE',  ( 0.000000000000000000, 0.000000000000000000, -1.000000000000000000 ) ) ;
#207891 = ORIENTED_EDGE ( 'NONE', *, *, #229824, .F. ) ;
#207892 = CARTESIAN_POINT ( 'NONE',  ( -18.54118089899632693, -9.463537631836951292, -174.5485775978680749 ) ) ;
#207893 = DIRECTION ( 'NONE',  ( 0.000000000000000000, -0.07847809223012357227, -0.9969158384938622275 ) ) ;
#207895 = ORIENTED_EDGE ( 'NONE', *, *, #230927, .T. ) ;
#207894 = DIRECTION ( 'NONE',  ( 0.000000000000000000, 0.9651348961777157509, -0.2617529984165031243 ) ) ;
#207896 = CARTESIAN_POINT ( 'NONE',  ( -20.64999999999999858, 7.150000000011155876, -179.8499999999999943 ) ) ;
#207897 = LINE ( 'NONE', #70963, #20007 ) ;
#207898 = DIRECTION ( 'NONE',  ( 0.000000000000000000, 0.000000000000000000, -1.000000000000000000 ) ) ;
#207899 = DIRECTION ( 'NONE',  ( 0.000000000000000000, 0.2617529984165044565, 0.9651348961777151958 ) ) ;
#207900 = DIRECTION ( 'NONE',  ( -1.000000000000000000, -2.952720810173289112E-16, 0.000000000000000000 ) ) ;
#207901 = CARTESIAN_POINT ( 'NONE',  ( -17.11825945287482753, 9.950000000011140600, -79.65000000000006253 ) ) ;
#207902 = CARTESIAN_POINT ( 'NONE',  ( -18.43473496883416729, -9.494952410988140912, -107.5458715722282648 ) ) ;
#207904 = ORIENTED_EDGE ( 'NONE', *, *, #81735, .T. ) ;
#207903 = DIRECTION ( 'NONE',  ( 0.000000000000000000, 0.000000000000000000, -1.000000000000000000 ) ) ;
#207905 = DIRECTION ( 'NONE',  ( 0.000000000000000000, 0.8814952561688429444, -0.4721928772777348460 ) ) ;
#207906 = TOROIDAL_SURFACE ( 'NONE', #249588, 0.4000000000000009104, 0.1000000000000000056 ) ;
#207907 = DIRECTION ( 'NONE',  ( 0.000000000000000000, -6.982962677686266711E-15, 1.000000000000000000 ) ) ;
#207908 = CARTESIAN_POINT ( 'NONE',  ( 21.05000000000000071, -8.730841121484171907, -43.09807471898433562 ) ) ;
#207909 = VECTOR ( 'NONE', #215674, 1000.000000000000000 ) ;
#207910 = DIRECTION ( 'NONE',  ( -1.000000000000000000, -0.000000000000000000, -0.000000000000000000 ) ) ;
#207911 = DIRECTION ( 'NONE',  ( 0.000000000000000000, 0.1350103645451876666, -0.9908441862701600211 ) ) ;
#207912 = VERTEX_POINT ( 'NONE', #13842 ) ;
#207913 = EDGE_CURVE ( 'NONE', #90293, #113629, #184676, .T. ) ;
#207914 = DIRECTION ( 'NONE',  ( -1.000000000000000000, -1.186688945009010077E-16, -0.000000000000000000 ) ) ;
#207915 = DIRECTION ( 'NONE',  ( -1.000000000000000000, -0.000000000000000000, -0.000000000000000000 ) ) ;
#207916 = EDGE_CURVE ( 'NONE', #82519, #66786, #122155, .T. ) ;
#207917 = AXIS2_PLACEMENT_3D ( 'NONE', #131087, #50251, #192354 ) ;
#207918 = VERTEX_POINT ( 'NONE', #215864 ) ;
#207919 = LINE ( 'NONE', #146614, #243556 ) ;
#207920 = CIRCLE ( 'NONE', #124518, 0.1000000000000000472 ) ;
#207921 = DIRECTION ( 'NONE',  ( -0.000000000000000000, 1.000000000000000000, 6.982962677686266711E-15 ) ) ;
#207922 = ADVANCED_FACE ( 'NONE', ( #175502 ), #133777, .T. ) ;
#207923 = ORIENTED_EDGE ( 'NONE', *, *, #154865, .T. ) ;
#207924 = FACE_OUTER_BOUND ( 'NONE', #84370, .T. ) ;
#207925 = VERTEX_POINT ( 'NONE', #114220 ) ;
#207926 = CARTESIAN_POINT ( 'NONE',  ( 23.14999999999999858, 7.128833340093095217, -233.7327013124392749 ) ) ;
#207927 = EDGE_LOOP ( 'NONE', ( #43744, #199775, #208173, #142839 ) ) ;
#207928 = EDGE_CURVE ( 'NONE', #182327, #220374, #34708, .T. ) ;
#207929 = VECTOR ( 'NONE', #107742, 1000.000000000000000 ) ;
#207930 = DIRECTION ( 'NONE',  ( 0.000000000000000000, 0.5000000000000144329, 0.8660254037844302699 ) ) ;
#207931 = CARTESIAN_POINT ( 'NONE',  ( 18.59999999999999432, 77.63717271298195044, -57.94095411905229298 ) ) ;
#207932 = EDGE_LOOP ( 'NONE', ( #212205, #220781, #214047, #149837, #52591 ) ) ;
#207933 = ORIENTED_EDGE ( 'NONE', *, *, #215047, .F. ) ;
#207934 = DIRECTION ( 'NONE',  ( 1.000000000000000000, 0.000000000000000000, 0.000000000000000000 ) ) ;
#207935 = EDGE_CURVE ( 'NONE', #135828, #74892, #18084, .T. ) ;
#207937 = ORIENTED_EDGE ( 'NONE', *, *, #119630, .T. ) ;
#207936 = CARTESIAN_POINT ( 'NONE',  ( 13.88302573338719093, 9.457410944778569473, -48.50008397379001934 ) ) ;
#207938 = CARTESIAN_POINT ( 'NONE',  ( 18.52928932188133970, 30.80256426056735108, -234.7528744682934700 ) ) ;
#207939 = ORIENTED_EDGE ( 'NONE', *, *, #168326, .F. ) ;
#207940 = CIRCLE ( 'NONE', #70585, 0.09999999999998882005 ) ;
#207941 = AXIS2_PLACEMENT_3D ( 'NONE', #1236, #194354, #178645 ) ;
#207942 =( GEOMETRIC_REPRESENTATION_CONTEXT ( 3 ) GLOBAL_UNCERTAINTY_ASSIGNED_CONTEXT ( ( #57145 ) ) GLOBAL_UNIT_ASSIGNED_CONTEXT ( ( #185580, #123049, #220848 ) ) REPRESENTATION_CONTEXT ( 'NONE', 'WORKASPACE' ) );
#207943 = AXIS2_PLACEMENT_3D ( 'NONE', #208346, #248738, #29718 ) ;
#207944 = EDGE_LOOP ( 'NONE', ( #105278, #139810, #169651 ) ) ;
#207946 = VECTOR ( 'NONE', #32285, 1000.000000000000000 ) ;
#207945 = CARTESIAN_POINT ( 'NONE',  ( -18.40000000000000213, 11.47316190336247210, -12.60857864376269255 ) ) ;
#207947 = EDGE_CURVE ( 'NONE', #104211, #107411, #205520, .T. ) ;
#207948 = PLANE ( 'NONE',  #184561 ) ;
#207949 = FACE_OUTER_BOUND ( 'NONE', #186709, .T. ) ;
#207950 = CARTESIAN_POINT ( 'NONE',  ( 20.85000000000000142, 43.27008861172207332, -245.2265230569236110 ) ) ;
#207951 = DIRECTION ( 'NONE',  ( 0.000000000000000000, 0.9654727137038715545, 0.2605042016806676242 ) ) ;
#207952 = DIRECTION ( 'NONE',  ( 7.304098846218134667E-16, 0.9651348961777158619, -0.2617529984165031243 ) ) ;
#207953 = VERTEX_POINT ( 'NONE', #193760 ) ;
#207954 = CARTESIAN_POINT ( 'NONE',  ( -20.00857864376270001, 9.350000000000001421, -21.15000000000000213 ) ) ;
#207955 = SPHERICAL_SURFACE ( 'NONE', #210978, 0.1000000000000000056 ) ;
#207956 = CARTESIAN_POINT ( 'NONE',  ( 21.05000000000000071, 70.50000000001223555, -148.9283735034374843 ) ) ;
#207957 = DIRECTION ( 'NONE',  ( 1.000000000000000000, 0.000000000000000000, 0.000000000000000000 ) ) ;
#207958 = ORIENTED_EDGE ( 'NONE', *, *, #188131, .F. ) ;
#207959 = CARTESIAN_POINT ( 'NONE',  ( 22.40000000000010516, 1.020945751984553285E-11, -55.35042919245493209 ) ) ;
#207960 = ORIENTED_EDGE ( 'NONE', *, *, #225427, .T. ) ;
#207962 = VECTOR ( 'NONE', #224784, 1000.000000000000000 ) ;
#207961 = DIRECTION ( 'NONE',  ( 0.000000000000000000, 0.000000000000000000, -1.000000000000000000 ) ) ;
#207963 = ORIENTED_EDGE ( 'NONE', *, *, #158866, .F. ) ;
#207964 = DIRECTION ( 'NONE',  ( -3.265361837132813093E-16, 1.000000000000000000, 0.000000000000000000 ) ) ;
#207965 = CARTESIAN_POINT ( 'NONE',  ( -20.54999999999999716, 76.00000000001170974, -69.52310748452431710 ) ) ;
#207966 = ORIENTED_EDGE ( 'NONE', *, *, #132365, .T. ) ;
#207967 = ORIENTED_EDGE ( 'NONE', *, *, #60005, .F. ) ;
#207969 = ORIENTED_EDGE ( 'NONE', *, *, #233623, .F. ) ;
#207968 = DIRECTION ( 'NONE',  ( -7.304098846218134667E-16, 1.000000000000000000, 6.982962677686266711E-15 ) ) ;
#207970 = DIRECTION ( 'NONE',  ( 1.000000000000000000, 0.000000000000000000, 0.000000000000000000 ) ) ;
#207971 = ORIENTED_EDGE ( 'NONE', *, *, #102652, .F. ) ;
#207972 = DIRECTION ( 'NONE',  ( 1.000000000000000000, 0.000000000000000000, 0.000000000000000000 ) ) ;
#207973 = DIRECTION ( 'NONE',  ( 0.000000000000000000, 0.000000000000000000, -1.000000000000000000 ) ) ;
#207974 = AXIS2_PLACEMENT_3D ( 'NONE', #152431, #31214, #50699 ) ;
#207975 = VERTEX_POINT ( 'NONE', #75125 ) ;
#207976 = DIRECTION ( 'NONE',  ( 0.000000000000000000, 1.000000000000000000, 6.938893903907222067E-15 ) ) ;
#207977 = AXIS2_PLACEMENT_3D ( 'NONE', #218076, #174198, #193720 ) ;
#207978 = CARTESIAN_POINT ( 'NONE',  ( 21.05000000000000071, 76.00000000001126921, -203.5231074845248997 ) ) ;
#207979 = ORIENTED_EDGE ( 'NONE', *, *, #138189, .F. ) ;
#207980 = ADVANCED_FACE ( 'NONE', ( #112943 ), #255359, .T. ) ;
#207981 = FACE_OUTER_BOUND ( 'NONE', #248237, .T. ) ;
#207982 = DIRECTION ( 'NONE',  ( 1.000000000000000000, 0.000000000000000000, -0.000000000000000000 ) ) ;
#207983 = EDGE_CURVE ( 'NONE', #200289, #168569, #15129, .T. ) ;
#207984 = CARTESIAN_POINT ( 'NONE',  ( -21.07946286933444568, 6.329037319018858021, -66.92331615674363832 ) ) ;
#207986 = ORIENTED_EDGE ( 'NONE', *, *, #80160, .T. ) ;
#207985 = CARTESIAN_POINT ( 'NONE',  ( 22.60000000000000142, 1.148907358139439339E-11, -201.0000000000015064 ) ) ;
#207987 = FACE_OUTER_BOUND ( 'NONE', #148035, .T. ) ;
#207988 = AXIS2_PLACEMENT_3D ( 'NONE', #212291, #214829, #255187 ) ;
#207989 = DIRECTION ( 'NONE',  ( 0.000000000000000000, 0.000000000000000000, -1.000000000000000000 ) ) ;
#207990 = CARTESIAN_POINT ( 'NONE',  ( -20.64999999999999858, 54.80101577392981937, -239.2322065708440846 ) ) ;
#207991 = TOROIDAL_SURFACE ( 'NONE', #170625, 0.6000000000000009770, 0.1000000000000000056 ) ;
#207992 = EDGE_CURVE ( 'NONE', #10935, #156135, #154662, .T. ) ;
#207994 = LINE ( 'NONE', #112728, #149320 ) ;
#207993 = CARTESIAN_POINT ( 'NONE',  ( 18.59999999999999076, 10.20857864377385127, -188.8499999999999659 ) ) ;
#207996 = EDGE_CURVE ( 'NONE', #182942, #147164, #142965, .T. ) ;
#207995 = CARTESIAN_POINT ( 'NONE',  ( 21.05000000000000071, 10.72371681401022592, -108.0943992358844525 ) ) ;
#207997 = CYLINDRICAL_SURFACE ( 'NONE', #156994, 0.1000000000000028644 ) ;
#207998 = DIRECTION ( 'NONE',  ( -7.304098846218134667E-16, 1.000000000000000000, -0.000000000000000000 ) ) ;
#207999 = DIRECTION ( 'NONE',  ( 0.000000000000000000, 0.000000000000000000, 1.000000000000000000 ) ) ;
#208000 = CIRCLE ( 'NONE', #57930, 0.09999999999999939493 ) ;
#208001 = ORIENTED_EDGE ( 'NONE', *, *, #48487, .F. ) ;
#208002 = VERTEX_POINT ( 'NONE', #77632 ) ;
#208003 = EDGE_LOOP ( 'NONE', ( #51457, #2474, #35726, #54859 ) ) ;
#208004 = EDGE_CURVE ( 'NONE', #235258, #1091, #192478, .T. ) ;
#208005 = CARTESIAN_POINT ( 'NONE',  ( 20.85000000000000142, 70.37092869010230345, -198.1237041667535550 ) ) ;
#208006 = ADVANCED_FACE ( 'NONE', ( #157228 ), #84691, .F. ) ;
#208007 = CARTESIAN_POINT ( 'NONE',  ( 20.95520789717937404, 65.42306940062736942, -162.4428745106495739 ) ) ;
#208008 = ORIENTED_EDGE ( 'NONE', *, *, #209794, .F. ) ;
#208009 = DIRECTION ( 'NONE',  ( -5.603264701231743991E-32, 1.897661533703520143E-16, -1.000000000000000000 ) ) ;
#208011 = LINE ( 'NONE', #107598, #233142 ) ;
#208010 = TOROIDAL_SURFACE ( 'NONE', #124609, 0.2000000000000000111, 0.1000000000000000056 ) ;
#208012 = CARTESIAN_POINT ( 'NONE',  ( 20.94999999999999929, -1.835341550213257733, -45.05515129256298223 ) ) ;
#208013 = EDGE_LOOP ( 'NONE', ( #127744, #106599, #56832, #52960 ) ) ;
#208014 = VERTEX_POINT ( 'NONE', #137611 ) ;
#208015 = DIRECTION ( 'NONE',  ( 1.000000000000000000, 0.000000000000000000, 0.000000000000000000 ) ) ;
#208016 = CARTESIAN_POINT ( 'NONE',  ( -18.59999999999999787, 77.83585931145498193, -24.41866831572578533 ) ) ;
#208017 = ORIENTED_EDGE ( 'NONE', *, *, #242589, .T. ) ;
#208018 = ADVANCED_FACE ( 'NONE', ( #217144 ), #197598, .F. ) ;
#208019 = EDGE_CURVE ( 'NONE', #132343, #1155, #185431, .T. ) ;
#208020 = CARTESIAN_POINT ( 'NONE',  ( -20.00857864376270001, 13.56015509305096778, -219.7948714774209691 ) ) ;
#208022 = ORIENTED_EDGE ( 'NONE', *, *, #207699, .T. ) ;
#208021 = DIRECTION ( 'NONE',  ( 0.000000000000000000, -0.9126074666063772600, -0.4088369013363276627 ) ) ;
#208023 = CARTESIAN_POINT ( 'NONE',  ( -23.25000000000000000, 74.00000000001186606, -89.79848556176222019 ) ) ;
#208024 = EDGE_CURVE ( 'NONE', #225548, #236288, #87590, .T. ) ;
#208025 = DIRECTION ( 'NONE',  ( 1.000000000000000000, 0.000000000000000000, 0.000000000000000000 ) ) ;
#208027 = VERTEX_POINT ( 'NONE', #27682 ) ;
#208026 = CARTESIAN_POINT ( 'NONE',  ( 23.25000000000000355, 98.45632476063481420, -96.22920903679255389 ) ) ;
#208028 = CARTESIAN_POINT ( 'NONE',  ( -18.50596464788227635, 10.30632246271647112, -72.50418367788957141 ) ) ;
#208029 = CARTESIAN_POINT ( 'NONE',  ( -16.89021194854740315, 9.950000000011137047, -87.74256813160438639 ) ) ;
#208030 = DIRECTION ( 'NONE',  ( -1.000000000000000000, 0.000000000000000000, 0.000000000000000000 ) ) ;
#208031 = CARTESIAN_POINT ( 'NONE',  ( -16.81744102076749314, 12.41403342719998726, -211.2428889513006993 ) ) ;
#208032 = AXIS2_PLACEMENT_3D ( 'NONE', #102266, #226074, #224807 ) ;
#208035 = CARTESIAN_POINT ( 'NONE',  ( 20.86036036209908318, 10.62104277658211693, -108.1663484185050237 ) ) ;
#208034 = AXIS2_PLACEMENT_3D ( 'NONE', #209286, #69802, #228861 ) ;
#208033 = LINE ( 'NONE', #107621, #115769 ) ;
#208036 = FACE_OUTER_BOUND ( 'NONE', #105925, .T. ) ;
#208037 = AXIS2_PLACEMENT_3D ( 'NONE', #226058, #186993, #241801 ) ;
#208038 = AXIS2_PLACEMENT_3D ( 'NONE', #97678, #178562, #134248 ) ;
#208039 = DIRECTION ( 'NONE',  ( 1.000000000000000000, 3.469446951953704435E-14, -2.003086131649669752E-14 ) ) ;
#208040 = CYLINDRICAL_SURFACE ( 'NONE', #234343, 0.09999999999998898659 ) ;
#208041 = ORIENTED_EDGE ( 'NONE', *, *, #82060, .F. ) ;
#208042 = ORIENTED_EDGE ( 'NONE', *, *, #18768, .T. ) ;
#208043 = DIRECTION ( 'NONE',  ( -1.000000000000000000, 0.000000000000000000, 0.000000000000000000 ) ) ;
#208044 = CIRCLE ( 'NONE', #179031, 0.9750000000000036415 ) ;
#208046 = VERTEX_POINT ( 'NONE', #99764 ) ;
#208045 = EDGE_CURVE ( 'NONE', #119088, #178023, #147586, .T. ) ;
#208047 = CARTESIAN_POINT ( 'NONE',  ( -23.15000000000000213, 11.65000000001115588, -146.1500000000000341 ) ) ;
#208048 = ORIENTED_EDGE ( 'NONE', *, *, #170138, .F. ) ;
#208049 = DIRECTION ( 'NONE',  ( 1.000000000000000000, 0.000000000000000000, 0.000000000000000000 ) ) ;
#208050 = DIRECTION ( 'NONE',  ( 0.000000000000000000, 0.000000000000000000, -1.000000000000000000 ) ) ;
#208051 = AXIS2_PLACEMENT_3D ( 'NONE', #59426, #217234, #93445 ) ;
#208052 = CIRCLE ( 'NONE', #95607, 0.2000000000000057288 ) ;
#208054 = EDGE_CURVE ( 'NONE', #106227, #91860, #38954, .T. ) ;
#208053 = ORIENTED_EDGE ( 'NONE', *, *, #56463, .F. ) ;
#208055 = AXIS2_PLACEMENT_3D ( 'NONE', #202118, #41783, #120040 ) ;
#208056 = DIRECTION ( 'NONE',  ( 0.000000000000000000, 0.1298341882519953583, 0.9915357197604862671 ) ) ;
#208057 =( LENGTH_UNIT ( ) NAMED_UNIT ( * ) SI_UNIT ( .MILLI., .METRE. ) );
#208058 = VERTEX_POINT ( 'NONE', #105862 ) ;
#208059 = CIRCLE ( 'NONE', #103962, 0.09999999999999939493 ) ;
#208060 = ORIENTED_EDGE ( 'NONE', *, *, #44965, .F. ) ;
#208061 = ORIENTED_EDGE ( 'NONE', *, *, #31813, .T. ) ;
#208062 = DIRECTION ( 'NONE',  ( 0.000000000000000000, -1.000000000000000000, 0.000000000000000000 ) ) ;
#208063 = FILL_AREA_STYLE ('',( #242028 ) ) ;
#208064 = LINE ( 'NONE', #90646, #1032 ) ;
#208065 = FACE_BOUND ( 'NONE', #54393, .T. ) ;
#208066 = CARTESIAN_POINT ( 'NONE',  ( 21.05000000000000071, 79.07891399537199106, -236.0635483022085452 ) ) ;
#208067 = EDGE_CURVE ( 'NONE', #239085, #21068, #55226, .T. ) ;
#208069 = CARTESIAN_POINT ( 'NONE',  ( 21.00000000000000000, 66.25000000001151079, -48.27310748452438816 ) ) ;
#208068 = DIRECTION ( 'NONE',  ( 0.000000000000000000, -6.938893903907222067E-15, 1.000000000000000000 ) ) ;
#208070 = DIRECTION ( 'NONE',  ( 0.000000000000000000, -6.853228547068871147E-15, 1.000000000000000000 ) ) ;
#208072 = VERTEX_POINT ( 'NONE', #179351 ) ;
#208071 = CARTESIAN_POINT ( 'NONE',  ( 20.94999999999999574, -10.51247937907010410, -206.3598299697285654 ) ) ;
#208074 = CARTESIAN_POINT ( 'NONE',  ( -16.87036670365548474, 65.91505003675652574, -82.07310748452438531 ) ) ;
#208073 = DIRECTION ( 'NONE',  ( 0.000000000000000000, 0.000000000000000000, 1.000000000000000000 ) ) ;
#208075 = CARTESIAN_POINT ( 'NONE',  ( 23.14999999999999503, 11.65000000000000746, -12.15000000000000036 ) ) ;
#208076 = EDGE_LOOP ( 'NONE', ( #111119, #117084, #219050 ) ) ;
#208077 = CARTESIAN_POINT ( 'NONE',  ( 20.95545211741311320, 10.58641331155510379, -74.58614685958833945 ) ) ;
#208078 = CARTESIAN_POINT ( 'NONE',  ( -21.05000000000000071, 1.115600667400684642E-11, -196.8999999999999773 ) ) ;
#208080 = ADVANCED_FACE ( 'NONE', ( #120666 ), #227110, .F. ) ;
#208079 = CARTESIAN_POINT ( 'NONE',  ( -21.65000000000000213, 7.708578643762696636, -12.34999999999999964 ) ) ;
#208081 = ORIENTED_EDGE ( 'NONE', *, *, #80473, .F. ) ;
#208082 = CARTESIAN_POINT ( 'NONE',  ( -21.59142135623730852, 7.850000000011158718, -54.75000000000000000 ) ) ;
#208083 = ADVANCED_FACE ( 'NONE', ( #48478 ), #140178, .F. ) ;
#208084 = AXIS2_PLACEMENT_3D ( 'NONE', #200776, #39160, #236048 ) ;
#208085 = CARTESIAN_POINT ( 'NONE',  ( 22.39999999999999503, 76.10085836911045476, -81.27267460801371612 ) ) ;
#208086 = DIRECTION ( 'NONE',  ( 1.000000000000000000, -2.952720810173289112E-16, -2.061873921506763405E-30 ) ) ;
#208087 = EDGE_LOOP ( 'NONE', ( #109995, #210670, #13 ) ) ;
#208088 = VERTEX_POINT ( 'NONE', #159775 ) ;
#208089 = EDGE_CURVE ( 'NONE', #25020, #17722, #238673, .T. ) ;
#208091 = EDGE_CURVE ( 'NONE', #139720, #171702, #218432, .T. ) ;
#208090 = DIRECTION ( 'NONE',  ( 0.000000000000000000, 0.000000000000000000, 1.000000000000000000 ) ) ;
#208093 = CARTESIAN_POINT ( 'NONE',  ( -17.78241384945270909, 65.14442424721120517, -159.7740698120441891 ) ) ;
#208092 = CIRCLE ( 'NONE', #78865, 0.1000000000000028644 ) ;
#208094 = CARTESIAN_POINT ( 'NONE',  ( 20.85000000000000142, 64.35000000001195986, -109.8069731475024753 ) ) ;
#208095 = CARTESIAN_POINT ( 'NONE',  ( 23.25000000000000000, 87.65000000001245439, -181.7731074845242745 ) ) ;
#208096 = VERTEX_POINT ( 'NONE', #9347 ) ;
#208097 = DIRECTION ( 'NONE',  ( -1.000000000000000000, -0.000000000000000000, 0.000000000000000000 ) ) ;
#208098 = CYLINDRICAL_SURFACE ( 'NONE', #170870, 0.5000000000000004441 ) ;
#208099 = DIRECTION ( 'NONE',  ( 0.000000000000000000, 0.000000000000000000, -1.000000000000000000 ) ) ;
#208100 = DIRECTION ( 'NONE',  ( 0.000000000000000000, -6.982962677686266711E-15, 1.000000000000000000 ) ) ;
#208101 = TOROIDAL_SURFACE ( 'NONE', #66437, 3.899999999999999467, 0.1000000000000000056 ) ;
#208102 = EDGE_CURVE ( 'NONE', #187156, #135372, #13811, .T. ) ;
#208103 = ORIENTED_EDGE ( 'NONE', *, *, #161270, .T. ) ;
#208106 = EDGE_CURVE ( 'NONE', #227798, #217285, #122330, .T. ) ;
#208105 = CARTESIAN_POINT ( 'NONE',  ( 20.94999999999999929, 10.29288807858821286, -38.95800201601217339 ) ) ;
#208104 = AXIS2_PLACEMENT_3D ( 'NONE', #244058, #107119, #44594 ) ;
#208108 = ORIENTED_EDGE ( 'NONE', *, *, #233925, .F. ) ;
#208107 = CARTESIAN_POINT ( 'NONE',  ( -23.25000000000000000, 77.73670573947940454, -91.50568489690056140 ) ) ;
#208109 = CARTESIAN_POINT ( 'NONE',  ( -16.94132844910801694, 9.992436755191500097, -121.3962017559823607 ) ) ;
#208110 = LINE ( 'NONE', #106395, #43406 ) ;
#208111 = CARTESIAN_POINT ( 'NONE',  ( 20.04142135623730070, 11.65000000001115943, -55.25000000000004974 ) ) ;
#208112 = ADVANCED_FACE ( 'NONE', ( #165888 ), #88990, .T. ) ;
#208113 = CARTESIAN_POINT ( 'NONE',  ( 21.05000000000000071, 67.12338541492553645, -195.1380270056797599 ) ) ;
#208114 = FACE_OUTER_BOUND ( 'NONE', #177219, .T. ) ;
#208115 = CIRCLE ( 'NONE', #153986, 0.1999999999999987899 ) ;
#208116 = DIRECTION ( 'NONE',  ( 0.000000000000000000, 0.000000000000000000, 1.000000000000000000 ) ) ;
#208117 = DIRECTION ( 'NONE',  ( 0.000000000000000000, 0.000000000000000000, -1.000000000000000000 ) ) ;
#208118 = TOROIDAL_SURFACE ( 'NONE', #241427, 11.65000000000000036, 0.1000000000000000056 ) ;
#208119 = ORIENTED_EDGE ( 'NONE', *, *, #43109, .T. ) ;
#208120 = DIRECTION ( 'NONE',  ( 0.000000000000000000, 0.4721928772776973204, 0.8814952561688629284 ) ) ;
#208121 = CARTESIAN_POINT ( 'NONE',  ( 23.04999999999999716, 65.06382255409391746, -210.1412732845728897 ) ) ;
#208122 = CARTESIAN_POINT ( 'NONE',  ( 22.39999999999999858, 0.1000000000111554016, -59.20922040162665922 ) ) ;
#208123 = DIRECTION ( 'NONE',  ( -1.000000000000000000, 0.000000000000000000, 0.000000000000000000 ) ) ;
#208124 = EDGE_CURVE ( 'NONE', #152543, #229766, #255552, .T. ) ;
#208125 = DIRECTION ( 'NONE',  ( 0.000000000000000000, 0.000000000000000000, -1.000000000000000000 ) ) ;
#208127 = DIRECTION ( 'NONE',  ( 0.000000000000000000, 0.000000000000000000, 1.000000000000000000 ) ) ;
#208126 = AXIS2_PLACEMENT_3D ( 'NONE', #64679, #125926, #81643 ) ;
#208128 = AXIS2_PLACEMENT_3D ( 'NONE', #136589, #36251, #96180 ) ;
#208130 = ORIENTED_EDGE ( 'NONE', *, *, #173962, .T. ) ;
#208129 = VECTOR ( 'NONE', #92892, 1000.000000000000114 ) ;
#208131 = ORIENTED_EDGE ( 'NONE', *, *, #14498, .F. ) ;
#208132 = VECTOR ( 'NONE', #98772, 1000.000000000000000 ) ;
#208133 = CARTESIAN_POINT ( 'NONE',  ( 21.05000000000000071, 87.75000000001142553, -38.92310748452424463 ) ) ;
#208134 = EDGE_CURVE ( 'NONE', #183417, #168131, #86297, .T. ) ;
#208135 = CARTESIAN_POINT ( 'NONE',  ( 20.94999999999999929, -3.770473190032740174, -225.9805569534692324 ) ) ;
#208136 = AXIS2_PLACEMENT_3D ( 'NONE', #2094, #141617, #106319 ) ;
#208137 = DIRECTION ( 'NONE',  ( 0.000000000000000000, 0.000000000000000000, 1.000000000000000000 ) ) ;
#208138 = EDGE_CURVE ( 'NONE', #129130, #182530, #238994, .T. ) ;
#208139 = CARTESIAN_POINT ( 'NONE',  ( 18.49999999999998934, 6.450000000011156587, -110.5170271704400591 ) ) ;
#208140 = DIRECTION ( 'NONE',  ( 0.000000000000000000, 0.000000000000000000, -1.000000000000000000 ) ) ;
#208141 = CARTESIAN_POINT ( 'NONE',  ( 21.14999999999999503, 11.75000000001115552, -33.50000000000000000 ) ) ;
#208142 = CARTESIAN_POINT ( 'NONE',  ( 20.95512820512820440, 40.84069494668059264, -237.9516373772122222 ) ) ;
#208143 = EDGE_LOOP ( 'NONE', ( #77881, #222184, #34878, #40673 ) ) ;
#208144 = LINE ( 'NONE', #166463, #19217 ) ;
#208145 = VERTEX_POINT ( 'NONE', #1954 ) ;
#208146 = EDGE_CURVE ( 'NONE', #168221, #84927, #90158, .T. ) ;
#208147 = DIRECTION ( 'NONE',  ( 0.000000000000000000, 6.982962677686266711E-15, -1.000000000000000000 ) ) ;
#208148 = CARTESIAN_POINT ( 'NONE',  ( 21.05000000000000071, -0.08561306080396914597, 6.413759733810287855 ) ) ;
#208149 = DIRECTION ( 'NONE',  ( 0.000000000000000000, 6.982962677686266711E-15, -1.000000000000000000 ) ) ;
#208150 = DIRECTION ( 'NONE',  ( 1.000000000000000000, -7.304098846218135653E-16, 0.000000000000000000 ) ) ;
#208151 = SURFACE_SIDE_STYLE ('',( #249829 ) ) ;
#208152 = CARTESIAN_POINT ( 'NONE',  ( 20.85000000000000142, 76.00000000001136868, -28.12310748452432208 ) ) ;
#208153 = DIRECTION ( 'NONE',  ( 0.000000000000000000, 6.982962677686266711E-15, -1.000000000000000000 ) ) ;
#208155 = VERTEX_POINT ( 'NONE', #194443 ) ;
#208154 = AXIS2_PLACEMENT_3D ( 'NONE', #254669, #73546, #232615 ) ;
#208156 = LINE ( 'NONE', #109018, #158085 ) ;
#208157 = CARTESIAN_POINT ( 'NONE',  ( 23.24999999999999645, 5.000000000011153745, -79.40526601891313874 ) ) ;
#208158 = CIRCLE ( 'NONE', #170778, 0.09999999999999939493 ) ;
#208159 = DIRECTION ( 'NONE',  ( 1.000000000000000000, 0.000000000000000000, 0.000000000000000000 ) ) ;
#208160 = DIRECTION ( 'NONE',  ( 0.000000000000000000, 0.8700118002898356018, -0.4930308989875170078 ) ) ;
#208161 = CARTESIAN_POINT ( 'NONE',  ( -22.50000000000000000, 11.64987090377452361, -167.4174801091270126 ) ) ;
#208162 = VERTEX_POINT ( 'NONE', #133165 ) ;
#208163 = CARTESIAN_POINT ( 'NONE',  ( -23.15000000000000213, 40.09675592080784412, -251.3927149226265385 ) ) ;
#208164 = FACE_OUTER_BOUND ( 'NONE', #88812, .T. ) ;
#208165 = EDGE_CURVE ( 'NONE', #27052, #19071, #13232, .T. ) ;
#208166 = VERTEX_POINT ( 'NONE', #113597 ) ;
#208167 = ORIENTED_EDGE ( 'NONE', *, *, #212210, .T. ) ;
#208168 = DIRECTION ( 'NONE',  ( -0.000000000000000000, -2.891205793294679805E-16, 1.000000000000000000 ) ) ;
#208169 = CARTESIAN_POINT ( 'NONE',  ( 20.94999999999999574, 47.92640890138473253, -246.4059919526569900 ) ) ;
#208170 = AXIS2_PLACEMENT_3D ( 'NONE', #61881, #103548, #218356 ) ;
#208171 = DIRECTION ( 'NONE',  ( 1.000000000000000000, 0.000000000000000000, 0.000000000000000000 ) ) ;
#208172 = CIRCLE ( 'NONE', #87335, 0.1000000000000013933 ) ;
#208173 = ORIENTED_EDGE ( 'NONE', *, *, #195603, .F. ) ;
#208174 = DIRECTION ( 'NONE',  ( 0.000000000000000000, -0.6728971962616697722, 0.7397360091702875895 ) ) ;
#208175 = DIRECTION ( 'NONE',  ( -0.000000000000000000, 0.000000000000000000, -1.000000000000000000 ) ) ;
#208176 = ADVANCED_FACE ( 'NONE', ( #88871 ), #190588, .F. ) ;
#208177 = EDGE_LOOP ( 'NONE', ( #173398, #203336, #87311, #17944 ) ) ;
#208178 = AXIS2_PLACEMENT_3D ( 'NONE', #213123, #38352, #175317 ) ;
#208179 =( BOUNDED_SURFACE ( )  B_SPLINE_SURFACE ( 3, 2, ( 
 ( #234519, #115867, #235799 ),
 ( #134125, #213679, #35085 ),
 ( #137970, #195424, #38908 ),
 ( #178432, #57144, #177149 ) ),
 .UNSPECIFIED., .F., .F., .T. ) 
 B_SPLINE_SURFACE_WITH_KNOTS ( ( 4, 4 ),
 ( 3, 3 ),
 ( 4.712388980384689674, 5.765869716888459173 ),
 ( 0.000000000000000000, 1.000000000000000000 ),
 .UNSPECIFIED. ) 
 GEOMETRIC_REPRESENTATION_ITEM ( )  RATIONAL_B_SPLINE_SURFACE ( (
 ( 1.000000000000000000, 0.7071067811865475727, 1.000000000000000000),
 ( 1.000000000000000000, 0.7953136715913138310, 1.000000000000000000),
 ( 1.000000000000000000, 0.8646876308615499829, 1.000000000000000000),
 ( 1.000000000000000000, 0.8984936768950558816, 1.000000000000000000) ) ) 
 REPRESENTATION_ITEM ( '' )  SURFACE ( )  );
#208180 = CARTESIAN_POINT ( 'NONE',  ( -18.59999999999999787, -9.849999999999996092, 31.39999999999999858 ) ) ;
#208181 = ORIENTED_EDGE ( 'NONE', *, *, #232485, .T. ) ;
#208182 = DIRECTION ( 'NONE',  ( 0.000000000000000000, 0.4721928772777551075, 0.8814952561688320642 ) ) ;
#208183 = FACE_OUTER_BOUND ( 'NONE', #1438, .T. ) ;
#208185 = ORIENTED_EDGE ( 'NONE', *, *, #181974, .T. ) ;
#208184 = LINE ( 'NONE', #192457, #241563 ) ;
#208186 = DIRECTION ( 'NONE',  ( 0.000000000000000000, 0.000000000000000000, 1.000000000000000000 ) ) ;
#208187 = CARTESIAN_POINT ( 'NONE',  ( -21.44999999999999929, 7.250000000011155521, -146.3500000000000227 ) ) ;
#208188 = FACE_OUTER_BOUND ( 'NONE', #154219, .T. ) ;
#208189 = CARTESIAN_POINT ( 'NONE',  ( -23.15000000000000213, -11.64999999998884483, -164.4000000000000057 ) ) ;
#208190 = CARTESIAN_POINT ( 'NONE',  ( -23.15000000000000213, 70.85002333954264486, -215.2140597723681879 ) ) ;
#208191 = DIRECTION ( 'NONE',  ( 1.000000000000000000, 0.000000000000000000, 0.000000000000000000 ) ) ;
#208192 = DIRECTION ( 'NONE',  ( 0.000000000000000000, -0.4999999999999949485, 0.8660254037844415942 ) ) ;
#208194 = EDGE_LOOP ( 'NONE', ( #12045, #166630, #196428, #113696 ) ) ;
#208193 = CARTESIAN_POINT ( 'NONE',  ( 18.54271179734040587, 87.05300735455581673, -199.5362999912227053 ) ) ;
#208195 = ORIENTED_EDGE ( 'NONE', *, *, #161070, .F. ) ;
#208198 = CARTESIAN_POINT ( 'NONE',  ( -23.15000000000000213, 11.65000000001115588, -188.8499999999999659 ) ) ;
#208197 = DIRECTION ( 'NONE',  ( 1.000000000000000000, -0.000000000000000000, -0.000000000000000000 ) ) ;
#208196 = AXIS2_PLACEMENT_3D ( 'NONE', #180291, #142436, #1629 ) ;
#208199 = VECTOR ( 'NONE', #107169, 1000.000000000000000 ) ;
#208201 = ORIENTED_EDGE ( 'NONE', *, *, #73826, .F. ) ;
#208200 = CARTESIAN_POINT ( 'NONE',  ( -20.64999999999999858, -9.000000000000001776, -23.60603087734756045 ) ) ;
#208202 = ORIENTED_EDGE ( 'NONE', *, *, #204752, .T. ) ;
#208203 = LINE ( 'NONE', #169098, #99922 ) ;
#208204 = DIRECTION ( 'NONE',  ( 0.000000000000000000, 0.000000000000000000, -1.000000000000000000 ) ) ;
#208205 = CARTESIAN_POINT ( 'NONE',  ( 23.15000000000000213, 88.41227409416143246, -72.62310748452421194 ) ) ;
#208206 = CARTESIAN_POINT ( 'NONE',  ( 23.14999999999999858, 76.00000000001213607, -136.5231074845243313 ) ) ;
#208207 = FACE_OUTER_BOUND ( 'NONE', #5361, .T. ) ;
#208208 = CARTESIAN_POINT ( 'NONE',  ( 18.49999999999999645, 1.115600667400684642E-11, -167.5000000000000284 ) ) ;
#208209 = ADVANCED_FACE ( 'NONE', ( #31529 ), #72463, .T. ) ;
#208210 = DIRECTION ( 'NONE',  ( 1.000000000000000000, 1.186688945009009831E-16, 0.000000000000000000 ) ) ;
#208211 = AXIS2_PLACEMENT_3D ( 'NONE', #176431, #177724, #120331 ) ;
#208212 = ORIENTED_EDGE ( 'NONE', *, *, #78798, .T. ) ;
#208213 = VERTEX_POINT ( 'NONE', #249266 ) ;
#208214 = CARTESIAN_POINT ( 'NONE',  ( -18.59999999999999787, 1.250000000011155299, -75.00000000000004263 ) ) ;
#208215 = CIRCLE ( 'NONE', #95750, 11.89999999999999325 ) ;
#208216 = CIRCLE ( 'NONE', #237430, 0.09999999999999939493 ) ;
#208217 = ORIENTED_EDGE ( 'NONE', *, *, #47847, .F. ) ;
#208218 = DIRECTION ( 'NONE',  ( 0.000000000000000000, -6.853228547068871147E-15, 1.000000000000000000 ) ) ;
#208219 = ORIENTED_EDGE ( 'NONE', *, *, #45419, .T. ) ;
#208220 = CYLINDRICAL_SURFACE ( 'NONE', #85062, 4.049999999999998046 ) ;
#208221 = AXIS2_PLACEMENT_3D ( 'NONE', #6353, #31104, #28549 ) ;
#208222 = LINE ( 'NONE', #243475, #221970 ) ;
#208223 = EDGE_CURVE ( 'NONE', #176, #148199, #9894, .T. ) ;
#208224 = DIRECTION ( 'NONE',  ( 1.000000000000000000, -0.000000000000000000, -0.000000000000000000 ) ) ;
#208225 = DIRECTION ( 'NONE',  ( 1.000000000000000000, 0.000000000000000000, 0.000000000000000000 ) ) ;
#208226 = ORIENTED_EDGE ( 'NONE', *, *, #255381, .T. ) ;
#208228 = CARTESIAN_POINT ( 'NONE',  ( -23.25000000000000000, 11.65000000001115588, -155.2500000000000284 ) ) ;
#208227 =( BOUNDED_SURFACE ( )  B_SPLINE_SURFACE ( 3, 2, ( 
 ( #6805, #86310, #165907 ),
 ( #245432, #66784, #233574 ),
 ( #77043, #56185, #133181 ),
 ( #254379, #92752, #156632 ) ),
 .UNSPECIFIED., .F., .F., .F. ) 
 B_SPLINE_SURFACE_WITH_KNOTS ( ( 4, 4 ),
 ( 3, 3 ),
 ( 0.0006461284895273780972, 0.0007503702773985887866 ),
 ( 0.000000000000000000, 1.000000000000000000 ),
 .UNSPECIFIED. ) 
 GEOMETRIC_REPRESENTATION_ITEM ( )  RATIONAL_B_SPLINE_SURFACE ( (
 ( 1.000000000000000000, 0.7071067811865475727, 1.000000000000000000),
 ( 1.000000000000000000, 0.7076476444649502096, 1.000000000000000000),
 ( 1.000000000000000000, 0.7075727925191112044, 1.000000000000000000),
 ( 1.000000000000000000, 0.7071067811865475727, 1.000000000000000000) ) ) 
 REPRESENTATION_ITEM ( '' )  SURFACE ( )  );
#208229 = ORIENTED_EDGE ( 'NONE', *, *, #55642, .F. ) ;
#208230 = EDGE_CURVE ( 'NONE', #65772, #101606, #155684, .T. ) ;
#208231 = FACE_OUTER_BOUND ( 'NONE', #257488, .T. ) ;
#208232 = TOROIDAL_SURFACE ( 'NONE', #233192, 0.6000000000000009770, 0.1000000000000000056 ) ;
#208233 = CARTESIAN_POINT ( 'NONE',  ( 20.12500000000000000, 66.25000000001209344, -128.4113362024100979 ) ) ;
#208235 = AXIS2_PLACEMENT_3D ( 'NONE', #182027, #3362, #67208 ) ;
#208234 = CARTESIAN_POINT ( 'NONE',  ( 21.05000000000000071, 8.776282648982402179, -108.9875923785189258 ) ) ;
#208236 = EDGE_LOOP ( 'NONE', ( #213748, #81502, #160478, #62927 ) ) ;
#208237 = CARTESIAN_POINT ( 'NONE',  ( -0.8999999999999435119, 66.35000000001119247, -12.62310748452479281 ) ) ;
#208238 = EDGE_CURVE ( 'NONE', #32586, #19570, #64064, .T. ) ;
#208239 = VERTEX_POINT ( 'NONE', #172338 ) ;
#208242 = ORIENTED_EDGE ( 'NONE', *, *, #70623, .T. ) ;
#208241 = CARTESIAN_POINT ( 'NONE',  ( 18.54148534481893762, 46.44433919924418319, -243.0795225066946159 ) ) ;
#208240 = DIRECTION ( 'NONE',  ( 0.000000000000000000, 0.2617529984165031243, 0.9651348961777157509 ) ) ;
#208243 = CARTESIAN_POINT ( 'NONE',  ( -22.39999999999999858, 68.20922040163854660, -103.1231074845243540 ) ) ;
#208244 = ORIENTED_EDGE ( 'NONE', *, *, #113552, .F. ) ;
#208245 = CARTESIAN_POINT ( 'NONE',  ( 18.59999999999997655, 76.00000000001165290, -61.62310748452430431 ) ) ;
#208246 = EDGE_LOOP ( 'NONE', ( #74216, #35032, #154846 ) ) ;
#208247 = CARTESIAN_POINT ( 'NONE',  ( 0.9000000000000000222, -12.25000000000000355, 26.00000000000000355 ) ) ;
#208248 = EDGE_CURVE ( 'NONE', #241028, #124696, #93283, .T. ) ;
#208249 = DIRECTION ( 'NONE',  ( 1.000000000000000000, -0.000000000000000000, -0.000000000000000000 ) ) ;
#208250 = DIRECTION ( 'NONE',  ( 1.000000000000000000, 2.986185139342070877E-16, -6.665775143889692774E-16 ) ) ;
#208251 = DIRECTION ( 'NONE',  ( 0.000000000000000000, -1.000000000000000000, -6.860497997771531562E-15 ) ) ;
#208252 = EDGE_CURVE ( 'NONE', #245204, #225390, #134417, .T. ) ;
#208253 = ORIENTED_EDGE ( 'NONE', *, *, #25852, .T. ) ;
#208254 = DIRECTION ( 'NONE',  ( 1.836970198721029934E-16, 1.000000000000000000, 6.982962677686266711E-15 ) ) ;
#208255 = CARTESIAN_POINT ( 'NONE',  ( -16.78493211734303259, 14.15196434607596387, -219.2423291894721729 ) ) ;
#208256 = CARTESIAN_POINT ( 'NONE',  ( -22.39999999999999858, 29.54900078958453236, -252.7363208912387051 ) ) ;
#208257 = AXIS2_PLACEMENT_3D ( 'NONE', #17964, #59634, #58355 ) ;
#208258 = ORIENTED_EDGE ( 'NONE', *, *, #39592, .F. ) ;
#208259 = CARTESIAN_POINT ( 'NONE',  ( -20.85000000000000142, 64.25000000001176659, -76.30697314750248950 ) ) ;
#208260 = ORIENTED_EDGE ( 'NONE', *, *, #220655, .F. ) ;
#208261 = CARTESIAN_POINT ( 'NONE',  ( -21.12642695952773764, 33.96205950053516176, -243.7731231636842608 ) ) ;
#208262 = ORIENTED_EDGE ( 'NONE', *, *, #238893, .F. ) ;
#208263 = CARTESIAN_POINT ( 'NONE',  ( -20.85000000000000142, -1.149570369575693807, -41.31591248450196474 ) ) ;
#208264 = CARTESIAN_POINT ( 'NONE',  ( -23.15000000000000213, 76.52350599684427834, -201.5928376921694678 ) ) ;
#208265 = AXIS2_PLACEMENT_3D ( 'NONE', #100255, #105379, #1162 ) ;
#208267 = ORIENTED_EDGE ( 'NONE', *, *, #224165, .F. ) ;
#208266 = CARTESIAN_POINT ( 'NONE',  ( -16.77431908686106965, 44.15011970405063835, -235.2969698559747656 ) ) ;
#208268 = DIRECTION ( 'NONE',  ( 1.000000000000000000, 0.000000000000000000, 0.000000000000000000 ) ) ;
#208269 = ADVANCED_FACE ( 'NONE', ( #250533 ), #114882, .F. ) ;
#208270 = CARTESIAN_POINT ( 'NONE',  ( -12.42749937872396160, 62.77489950700472576, -216.4869172218852214 ) ) ;
#208271 = DIRECTION ( 'NONE',  ( 0.000000000000000000, 0.8660254037844482555, 0.4999999999999837907 ) ) ;
#208272 = ORIENTED_EDGE ( 'NONE', *, *, #196165, .F. ) ;
#208273 = CARTESIAN_POINT ( 'NONE',  ( 21.00023020733438273, 69.60913075474496736, -203.5231074845244166 ) ) ;
#208274 = CARTESIAN_POINT ( 'NONE',  ( 18.54116936837189655, 85.46356419838478757, -162.9745649936360223 ) ) ;
#208275 = ORIENTED_EDGE ( 'NONE', *, *, #230034, .F. ) ;
#208276 = CARTESIAN_POINT ( 'NONE',  ( 21.05000000000000426, 1.372128392831997390, -230.7624356707774496 ) ) ;
#208277 = CIRCLE ( 'NONE', #70931, 0.1000000000000028644 ) ;
#208278 = CIRCLE ( 'NONE', #195822, 0.2000000000000057288 ) ;
#208279 = ORIENTED_EDGE ( 'NONE', *, *, #154139, .F. ) ;
#208280 = EDGE_CURVE ( 'NONE', #7516, #64282, #131876, .T. ) ;
#208281 = CARTESIAN_POINT ( 'NONE',  ( 23.14999999999998437, 1.115600667400684642E-11, -167.4999999999999716 ) ) ;
#208282 = FACE_OUTER_BOUND ( 'NONE', #60640, .T. ) ;
#208283 = VECTOR ( 'NONE', #151662, 1000.000000000000000 ) ;
#208284 = AXIS2_PLACEMENT_3D ( 'NONE', #105397, #125013, #207115 ) ;
#208286 = EDGE_CURVE ( 'NONE', #86047, #213499, #130579, .T. ) ;
#208285 = AXIS2_PLACEMENT_3D ( 'NONE', #39166, #24745, #59961 ) ;
#208289 = VERTEX_POINT ( 'NONE', #49768 ) ;
#208288 = ORIENTED_EDGE ( 'NONE', *, *, #221990, .T. ) ;
#208287 = CARTESIAN_POINT ( 'NONE',  ( -16.87683809663752399, 66.15000000001187175, -89.62074346632807931 ) ) ;
#208290 = DIRECTION ( 'NONE',  ( 0.000000000000000000, 0.9126074666063769270, 0.4088369013363280513 ) ) ;
#208291 = CYLINDRICAL_SURFACE ( 'NONE', #43976, 0.1000000000000028644 ) ;
#208292 = CARTESIAN_POINT ( 'NONE',  ( -23.25000000000000000, -11.74999999998884448, -167.4999999999999432 ) ) ;
#208294 = CARTESIAN_POINT ( 'NONE',  ( -14.22969084473441725, 66.54399267394222761, -51.03447399037762722 ) ) ;
#208293 = CARTESIAN_POINT ( 'NONE',  ( 22.49806830649814060, 0.07746431633666320260, -88.85011034516095663 ) ) ;
#208296 = EDGE_CURVE ( 'NONE', #19688, #62457, #67736, .T. ) ;
#208295 = DIRECTION ( 'NONE',  ( 1.000000000000000000, 0.000000000000000000, 0.000000000000000000 ) ) ;
#208297 = PLANE ( 'NONE',  #119773 ) ;
#208298 = CARTESIAN_POINT ( 'NONE',  ( -23.25000000000000000, -11.74999999998884448, -97.40000000000004832 ) ) ;
#208299 = ADVANCED_FACE ( 'NONE', ( #94019 ), #104165, .T. ) ;
#208300 = CIRCLE ( 'NONE', #79268, 12.77499999999999503 ) ;
#208301 = CARTESIAN_POINT ( 'NONE',  ( 20.94999999999999574, -1.835341550213255957, -179.0551512925629538 ) ) ;
#208302 = CIRCLE ( 'NONE', #216473, 0.1999999999999987899 ) ;
#208303 = AXIS2_PLACEMENT_3D ( 'NONE', #156467, #92588, #153914 ) ;
#208304 = ORIENTED_EDGE ( 'NONE', *, *, #136753, .F. ) ;
#208305 = VECTOR ( 'NONE', #208985, 1000.000000000000227 ) ;
#208307 = ORIENTED_EDGE ( 'NONE', *, *, #230905, .T. ) ;
#208306 = CIRCLE ( 'NONE', #91769, 0.09999999999999939493 ) ;
#208308 = DIRECTION ( 'NONE',  ( -0.5932847527679298016, -0.7769265190100954621, 0.2107092456252268875 ) ) ;
#208310 = ORIENTED_EDGE ( 'NONE', *, *, #79922, .T. ) ;
#208309 = CARTESIAN_POINT ( 'NONE',  ( -21.05000000000000071, -0.2576658302507160991, -201.0204024091695487 ) ) ;
#208311 = EDGE_LOOP ( 'NONE', ( #169739, #251247, #191570, #233815 ) ) ;
#208312 = DIRECTION ( 'NONE',  ( 0.000000000000000000, 0.000000000000000000, -1.000000000000000000 ) ) ;
#208313 = ADVANCED_FACE ( 'NONE', ( #79581 ), #43227, .T. ) ;
#208314 = ORIENTED_EDGE ( 'NONE', *, *, #107403, .F. ) ;
#208315 = CARTESIAN_POINT ( 'NONE',  ( -20.64999999999999858, 7.150000000011155876, -188.6499999999999488 ) ) ;
#208316 = ADVANCED_FACE ( 'NONE', ( #174914 ), #239038, .F. ) ;
#208317 = ADVANCED_FACE ( 'NONE', ( #157913 ), #156617, .T. ) ;
#208318 = VECTOR ( 'NONE', #212117, 1000.000000000000000 ) ;
#208319 = ORIENTED_EDGE ( 'NONE', *, *, #49825, .F. ) ;
#208320 = CARTESIAN_POINT ( 'NONE',  ( 20.94999999999999929, 5.400000000011154988, -88.09473398108696074 ) ) ;
#208321 = DIRECTION ( 'NONE',  ( 1.000000000000000000, -0.000000000000000000, 0.000000000000000000 ) ) ;
#208323 = VERTEX_POINT ( 'NONE', #238679 ) ;
#208322 = ORIENTED_EDGE ( 'NONE', *, *, #207916, .F. ) ;
#208324 = ORIENTED_EDGE ( 'NONE', *, *, #149868, .T. ) ;
#208325 = DIRECTION ( 'NONE',  ( 0.000000000000000000, 0.000000000000000000, 1.000000000000000000 ) ) ;
#208326 = ORIENTED_EDGE ( 'NONE', *, *, #91159, .T. ) ;
#208327 = VERTEX_POINT ( 'NONE', #19643 ) ;
#208328 = ADVANCED_FACE ( 'NONE', ( #39223 ), #76525, .T. ) ;
#208329 = DIRECTION ( 'NONE',  ( 1.000000000000000000, 0.000000000000000000, 0.000000000000000000 ) ) ;
#208330 = DIRECTION ( 'NONE',  ( -1.000000000000000000, 0.000000000000000000, -0.000000000000000000 ) ) ;
#208331 = DIRECTION ( 'NONE',  ( 1.000000000000000000, -0.000000000000000000, -0.000000000000000000 ) ) ;
#208333 = ORIENTED_EDGE ( 'NONE', *, *, #201421, .T. ) ;
#208332 = DIRECTION ( 'NONE',  ( 1.000000000000000000, 0.000000000000000000, 0.000000000000000000 ) ) ;
#208334 = DIRECTION ( 'NONE',  ( 0.000000000000000000, 0.000000000000000000, 1.000000000000000000 ) ) ;
#208335 = EDGE_CURVE ( 'NONE', #121432, #188354, #139559, .T. ) ;
#208336 = CARTESIAN_POINT ( 'NONE',  ( 23.14999999999999858, 11.65000000001116298, -160.4851942293460922 ) ) ;
#208338 = ORIENTED_EDGE ( 'NONE', *, *, #232009, .T. ) ;
#208337 = DIRECTION ( 'NONE',  ( 0.000000000000000000, -0.9916376685811618685, 0.1290532225514649800 ) ) ;
#208339 = LINE ( 'NONE', #27150, #151050 ) ;
#208341 = EDGE_CURVE ( 'NONE', #98712, #235459, #226609, .T. ) ;
#208340 = VERTEX_POINT ( 'NONE', #199584 ) ;
#208342 = DIRECTION ( 'NONE',  ( -1.000000000000000000, 0.000000000000000000, 0.000000000000000000 ) ) ;
#208343 = AXIS2_PLACEMENT_3D ( 'NONE', #231028, #71940, #150198 ) ;
#208344 = ORIENTED_EDGE ( 'NONE', *, *, #82573, .F. ) ;
#208345 = CARTESIAN_POINT ( 'NONE',  ( -21.00250684356849362, 18.86061765621301234, -226.6874733719499488 ) ) ;
#208346 = CARTESIAN_POINT ( 'NONE',  ( 20.85000000000000142, 77.16412189325360771, -162.1082593989527254 ) ) ;
#208347 = AXIS2_PLACEMENT_3D ( 'NONE', #79311, #158895, #238406 ) ;
#208348 = ORIENTED_EDGE ( 'NONE', *, *, #152137, .T. ) ;
#208350 = DIRECTION ( 'NONE',  ( -1.000000000000000000, -0.000000000000000000, 0.000000000000000000 ) ) ;
#208349 = DIRECTION ( 'NONE',  ( 0.000000000000000000, 0.9126074666063545004, 0.4088369013363783999 ) ) ;
#208351 = FACE_OUTER_BOUND ( 'NONE', #225805, .T. ) ;
#208352 = DIRECTION ( 'NONE',  ( -1.000000000000000000, -0.000000000000000000, -0.000000000000000000 ) ) ;
#208353 = DIRECTION ( 'NONE',  ( -0.000000000000000000, -0.000000000000000000, 1.000000000000000000 ) ) ;
#208354 = VERTEX_POINT ( 'NONE', #212268 ) ;
#208355 = ORIENTED_EDGE ( 'NONE', *, *, #98572, .F. ) ;
#208356 = DIRECTION ( 'NONE',  ( 0.000000000000000000, -0.000000000000000000, -1.000000000000000000 ) ) ;
#208357 = CARTESIAN_POINT ( 'NONE',  ( 20.94999999999999929, 67.23127455305841238, -235.8551265064783991 ) ) ;
#208359 = ORIENTED_EDGE ( 'NONE', *, *, #179068, .F. ) ;
#208358 = ADVANCED_FACE ( 'NONE', ( #93587 ), #16632, .T. ) ;
#208360 = DIRECTION ( 'NONE',  ( 0.000000000000000000, -0.1350103645451945777, 0.9908441862701590219 ) ) ;
#208361 = ORIENTED_EDGE ( 'NONE', *, *, #237466, .F. ) ;
#208362 = EDGE_CURVE ( 'NONE', #180293, #35579, #1512, .T. ) ;
#208363 = DIRECTION ( 'NONE',  ( 1.000000000000000000, 0.000000000000000000, 0.000000000000000000 ) ) ;
#208364 = CARTESIAN_POINT ( 'NONE',  ( 20.27550659511089037, 9.216043722520002035, -180.1499999999999773 ) ) ;
#208365 = AXIS2_PLACEMENT_3D ( 'NONE', #199728, #41937, #21097 ) ;
#208366 = CARTESIAN_POINT ( 'NONE',  ( -18.50000000000000000, -1.637172712959223952, -78.58215336547205254 ) ) ;
#208367 = AXIS2_PLACEMENT_3D ( 'NONE', #96027, #196417, #116891 ) ;
#208369 = ADVANCED_FACE ( 'NONE', ( #31087 ), #231829, .F. ) ;
#208368 = ORIENTED_EDGE ( 'NONE', *, *, #239855, .T. ) ;
#208370 = CARTESIAN_POINT ( 'NONE',  ( 23.15000000000000213, 88.41227409416161720, -106.1231074845242262 ) ) ;
#208371 = AXIS2_PLACEMENT_3D ( 'NONE', #214117, #236239, #175040 ) ;
#208373 = ORIENTED_EDGE ( 'NONE', *, *, #74477, .F. ) ;
#208372 = CIRCLE ( 'NONE', #8442, 0.09999999999999939493 ) ;
#208374 = ORIENTED_EDGE ( 'NONE', *, *, #87635, .F. ) ;
#208375 = ORIENTED_EDGE ( 'NONE', *, *, #94418, .F. ) ;
#208376 = LINE ( 'NONE', #124975, #73979 ) ;
#208377 = PLANE ( 'NONE',  #233933 ) ;
#208378 = DIRECTION ( 'NONE',  ( -1.000000000000000000, 0.000000000000000000, 0.000000000000000000 ) ) ;
#208379 = DIRECTION ( 'NONE',  ( 0.000000000000000000, 0.000000000000000000, -1.000000000000000000 ) ) ;
#208381 = CARTESIAN_POINT ( 'NONE',  ( 21.07964655665547582, 8.774889614978558683, -12.22191658296405592 ) ) ;
#208380 = DIRECTION ( 'NONE',  ( -1.000000000000000000, 0.000000000000000000, 0.000000000000000000 ) ) ;
#208383 = ORIENTED_EDGE ( 'NONE', *, *, #200877, .T. ) ;
#208382 = DIRECTION ( 'NONE',  ( 0.000000000000000000, 0.5000000000000078826, -0.8660254037844340447 ) ) ;
#208384 = CARTESIAN_POINT ( 'NONE',  ( -21.17356465864818205, 10.07444543872610154, -228.0243256418613385 ) ) ;
#208385 = VERTEX_POINT ( 'NONE', #149738 ) ;
#208386 = DIRECTION ( 'NONE',  ( -1.000000000000000000, 0.000000000000000000, 0.000000000000000000 ) ) ;
#208387 = VERTEX_POINT ( 'NONE', #213519 ) ;
#208388 = ORIENTED_EDGE ( 'NONE', *, *, #131123, .F. ) ;
#208389 = CARTESIAN_POINT ( 'NONE',  ( -23.15000000000000213, -9.599999999988847676, -177.3939691226524076 ) ) ;
#208390 = DIRECTION ( 'NONE',  ( 1.000000000000000000, -2.952720810173289112E-16, -2.061873921506763405E-30 ) ) ;
#208392 = EDGE_CURVE ( 'NONE', #22954, #241306, #130694, .T. ) ;
#208391 = CARTESIAN_POINT ( 'NONE',  ( -21.13422380239133958, 76.00000000001273293, -210.0164339993299620 ) ) ;
#208393 = CARTESIAN_POINT ( 'NONE',  ( -23.25000000000000355, 10.05000000001113847, -154.7500000000000284 ) ) ;
#208394 = CIRCLE ( 'NONE', #16843, 0.1999999999999987899 ) ;
#208395 = VECTOR ( 'NONE', #108464, 1000.000000000000000 ) ;
#208396 = EDGE_CURVE ( 'NONE', #155941, #87320, #229261, .T. ) ;
#208397 = CARTESIAN_POINT ( 'NONE',  ( 21.05000000000000071, 24.04029978241812771, -253.0016354099517457 ) ) ;
#208398 = VERTEX_POINT ( 'NONE', #132729 ) ;
#208399 = ORIENTED_EDGE ( 'NONE', *, *, #117763, .T. ) ;
#208401 = EDGE_CURVE ( 'NONE', #191564, #9869, #110579, .T. ) ;
#208400 = CARTESIAN_POINT ( 'NONE',  ( -23.25000000000000000, -1.851617760457748618, -212.6031897196036198 ) ) ;
#208402 = VERTEX_POINT ( 'NONE', #190132 ) ;
#208403 = DIRECTION ( 'NONE',  ( 2.557131231893036492E-16, -0.9525900758537790836, 0.3042567129660269099 ) ) ;
#208404 = ORIENTED_EDGE ( 'NONE', *, *, #181837, .T. ) ;
#208405 = CARTESIAN_POINT ( 'NONE',  ( -20.64999999999999858, 74.00000000001199396, -115.8477294072864083 ) ) ;
#208406 = CARTESIAN_POINT ( 'NONE',  ( 21.59780538579342135, -1.360356060411589185, -194.2886754741613231 ) ) ;
#208407 = CARTESIAN_POINT ( 'NONE',  ( 20.94999999999997442, -1.263275465206102233, -74.90186466674640542 ) ) ;
#208408 = CARTESIAN_POINT ( 'NONE',  ( 21.05000000000000071, -1.835341550213257733, -112.0551512925630249 ) ) ;
#208409 = VERTEX_POINT ( 'NONE', #130136 ) ;
#208410 = DIRECTION ( 'NONE',  ( 0.000000000000000000, -1.000000000000000000, 0.000000000000000000 ) ) ;
#208411 = EDGE_CURVE ( 'NONE', #183734, #146084, #153612, .T. ) ;
#208412 = CARTESIAN_POINT ( 'NONE',  ( -23.15000000000000213, 76.00000000001142553, -36.02310748452432421 ) ) ;
#208413 = DIRECTION ( 'NONE',  ( 0.000000000000000000, 1.000000000000000000, -3.469446951953635015E-14 ) ) ;
#208414 = CIRCLE ( 'NONE', #154264, 4.000000000000003553 ) ;
#208415 = AXIS2_PLACEMENT_3D ( 'NONE', #152904, #92882, #211567 ) ;
#208417 = ADVANCED_FACE ( 'NONE', ( #11501, #92293 ), #91018, .T. ) ;
#208416 = CARTESIAN_POINT ( 'NONE',  ( -18.46902351632713746, 85.50947011869274661, -96.03665355026690520 ) ) ;
#208418 = AXIS2_PLACEMENT_3D ( 'NONE', #257382, #13697, #213177 ) ;
#208419 = CARTESIAN_POINT ( 'NONE',  ( 20.04142135623731136, 64.25000000001196554, -111.7559501969989952 ) ) ;
#208420 = ADVANCED_FACE ( 'NONE', ( #113148 ), #133987, .F. ) ;
#208421 = ORIENTED_EDGE ( 'NONE', *, *, #187229, .F. ) ;
#208422 = CIRCLE ( 'NONE', #133555, 7.791421356237310469 ) ;
#208424 = ADVANCED_FACE ( 'NONE', ( #193989 ), #159745, .F. ) ;
#208423 = EDGE_CURVE ( 'NONE', #189844, #84325, #222250, .T. ) ;
#208425 = CARTESIAN_POINT ( 'NONE',  ( 21.05000000000000071, 10.72371710470752149, -12.15000000000000036 ) ) ;
#208426 = VERTEX_POINT ( 'NONE', #54453 ) ;
#208427 = CARTESIAN_POINT ( 'NONE',  ( -18.40000000000000213, 11.33174054713633261, -121.3500000000000369 ) ) ;
#208428 = LINE ( 'NONE', #91022, #256162 ) ;
#208429 = CARTESIAN_POINT ( 'NONE',  ( -21.05000000000000071, -11.48912529307605546, -30.39999999999999503 ) ) ;
#208430 = VECTOR ( 'NONE', #124080, 1000.000000000000114 ) ;
#208431 = ORIENTED_EDGE ( 'NONE', *, *, #109677, .T. ) ;
#208432 = DIRECTION ( 'NONE',  ( 0.000000000000000000, -7.429790795770644761E-15, 1.000000000000000000 ) ) ;
#208433 = CARTESIAN_POINT ( 'NONE',  ( 18.59999999999999076, 74.16465844978715438, -57.96795619196135618 ) ) ;
#208434 = FACE_OUTER_BOUND ( 'NONE', #220879, .T. ) ;
#208435 = DIRECTION ( 'NONE',  ( 1.000000000000000000, 6.938893903907222067E-15, 0.000000000000000000 ) ) ;
#208436 = EDGE_CURVE ( 'NONE', #76307, #144523, #55696, .T. ) ;
#208437 = EDGE_CURVE ( 'NONE', #112448, #123398, #41340, .T. ) ;
#208438 = CARTESIAN_POINT ( 'NONE',  ( -23.25000000000000000, 46.01276039807270024, -256.6622985126337539 ) ) ;
#208439 = ORIENTED_EDGE ( 'NONE', *, *, #241667, .F. ) ;
#208440 = EDGE_LOOP ( 'NONE', ( #229880, #137329, #94946, #55713 ) ) ;
#208441 = CARTESIAN_POINT ( 'NONE',  ( 21.05000000000000071, 86.45856254523212669, -209.4679346046102921 ) ) ;
#208442 = FACE_OUTER_BOUND ( 'NONE', #163053, .T. ) ;
#208443 = CARTESIAN_POINT ( 'NONE',  ( 22.49999999999999645, 0.1000000000111554016, -122.3504291924552092 ) ) ;
#208445 = EDGE_CURVE ( 'NONE', #134186, #66864, #240804, .T. ) ;
#208444 = DIRECTION ( 'NONE',  ( 1.000000000000000000, 0.000000000000000000, 0.000000000000000000 ) ) ;
#208446 = CARTESIAN_POINT ( 'NONE',  ( -16.87368910959167678, 44.09664347368151738, -235.3039772434659085 ) ) ;
#208447 = EDGE_LOOP ( 'NONE', ( #9633, #92696, #237526, #31370 ) ) ;
#208449 = EDGE_CURVE ( 'NONE', #45489, #48315, #68163, .T. ) ;
#208448 = CARTESIAN_POINT ( 'NONE',  ( 22.48660254037844552, 11.75000000001115730, -33.45000000000000995 ) ) ;
#208450 = CONTEXT_DEPENDENT_SHAPE_REPRESENTATION ( #189086, #78732 ) ;
#208451 = EDGE_CURVE ( 'NONE', #13912, #56045, #22395, .T. ) ;
#208452 = DIRECTION ( 'NONE',  ( -1.000000000000000000, 0.000000000000000000, 0.000000000000000000 ) ) ;
#208453 = ORIENTED_EDGE ( 'NONE', *, *, #20595, .F. ) ;
#208454 = CARTESIAN_POINT ( 'NONE',  ( 13.40000000000000036, -11.65000000000000036, 17.60000000000000497 ) ) ;
#208455 = AXIS2_PLACEMENT_3D ( 'NONE', #364, #137303, #196023 ) ;
#208456 = B_SPLINE_CURVE_WITH_KNOTS ( 'NONE', 3,
 ( #81737, #101281, #43930, #201719, #80448, #160056, #23108, #162609 ),
 .UNSPECIFIED., .F., .F.,
 ( 4, 2, 2, 4 ),
 ( 0.000000000000000000, 9.550056980125310032E-05, 0.0001910011396025062006, 0.0003820022792049910425 ),
 .UNSPECIFIED. ) ;
#208457 = ORIENTED_EDGE ( 'NONE', *, *, #182059, .F. ) ;
#208458 = ORIENTED_EDGE ( 'NONE', *, *, #40261, .T. ) ;
#208459 = AXIS2_PLACEMENT_3D ( 'NONE', #253901, #55671, #36170 ) ;
#208460 = ORIENTED_EDGE ( 'NONE', *, *, #95597, .F. ) ;
#208461 = ADVANCED_FACE ( 'NONE', ( #99968 ), #97398, .F. ) ;
#208462 = DIRECTION ( 'NONE',  ( 1.000000000000000000, 0.000000000000000000, 0.000000000000000000 ) ) ;
#208463 = LINE ( 'NONE', #48074, #159060 ) ;
#208464 = CARTESIAN_POINT ( 'NONE',  ( 21.04999999999999716, 10.62872031401550466, -112.6500000000000199 ) ) ;
#208465 = LINE ( 'NONE', #128911, #48950 ) ;
#208466 = DIRECTION ( 'NONE',  ( 0.000000000000000000, 0.000000000000000000, 1.000000000000000000 ) ) ;
#208467 = CARTESIAN_POINT ( 'NONE',  ( -20.85000000000000142, 1.115600667400684642E-11, -100.5000000000000426 ) ) ;
#208468 = DIRECTION ( 'NONE',  ( 0.000000000000000000, 0.9651348961777157509, -0.2617529984165031243 ) ) ;
#208470 = FACE_OUTER_BOUND ( 'NONE', #141951, .T. ) ;
#208469 = CARTESIAN_POINT ( 'NONE',  ( 20.95496329884391784, 65.43256679391885200, -95.44879755223956863 ) ) ;
#208471 = ADVANCED_FACE ( 'NONE', ( #23060 ), #59551, .T. ) ;
#208472 = LINE ( 'NONE', #109327, #206218 ) ;
#208473 = FACE_OUTER_BOUND ( 'NONE', #103568, .T. ) ;
#208474 = CYLINDRICAL_SURFACE ( 'NONE', #219573, 0.09999999999998304689 ) ;
#208475 = AXIS2_PLACEMENT_3D ( 'NONE', #124767, #225117, #24398 ) ;
#208476 = ORIENTED_EDGE ( 'NONE', *, *, #202472, .F. ) ;
#208477 = VERTEX_POINT ( 'NONE', #2164 ) ;
#208478 = CARTESIAN_POINT ( 'NONE',  ( -20.94560253601877164, 11.75000000001115197, -93.51008351251550721 ) ) ;
#208479 = AXIS2_PLACEMENT_3D ( 'NONE', #161360, #122223, #84310 ) ;
#208481 = CARTESIAN_POINT ( 'NONE',  ( -15.69373346032659455, 12.80368220771249632, -215.8196253896158794 ) ) ;
#208480 = CARTESIAN_POINT ( 'NONE',  ( 23.14999999999999503, 59.19392724319016708, -220.9828015967491126 ) ) ;
#208482 = CIRCLE ( 'NONE', #71102, 0.1000000000000028644 ) ;
#208483 = DIRECTION ( 'NONE',  ( 1.000000000000000000, 0.000000000000000000, 0.000000000000000000 ) ) ;
#208484 = EDGE_CURVE ( 'NONE', #71383, #117652, #7455, .T. ) ;
#208485 = CARTESIAN_POINT ( 'NONE',  ( 18.59999999999997655, 77.16412189325286874, -61.60825939895269698 ) ) ;
#208486 = TOROIDAL_SURFACE ( 'NONE', #204161, 0.2000000000000000111, 0.1000000000000000056 ) ;
#208487 = ORIENTED_EDGE ( 'NONE', *, *, #139836, .F. ) ;
#208488 = AXIS2_PLACEMENT_3D ( 'NONE', #25687, #127350, #105167 ) ;
#208489 = ORIENTED_EDGE ( 'NONE', *, *, #39419, .T. ) ;
#208490 = DIRECTION ( 'NONE',  ( 0.000000000000000000, 6.982962677686266711E-15, -1.000000000000000000 ) ) ;
#208491 = ORIENTED_EDGE ( 'NONE', *, *, #92891, .F. ) ;
#208492 = FACE_OUTER_BOUND ( 'NONE', #49406, .T. ) ;
#208493 = EDGE_CURVE ( 'NONE', #98813, #100166, #230678, .T. ) ;
#208494 = AXIS2_PLACEMENT_3D ( 'NONE', #149739, #252642, #74059 ) ;
#208495 = AXIS2_PLACEMENT_3D ( 'NONE', #73431, #134630, #214201 ) ;
#208496 = TOROIDAL_SURFACE ( 'NONE', #150229, 0.2000000000000000111, 0.1000000000000000056 ) ;
#208497 = CIRCLE ( 'NONE', #75411, 0.1000000000000011158 ) ;
#208498 = TOROIDAL_SURFACE ( 'NONE', #359, 7.800000000000000711, 0.1000000000000000056 ) ;
#208499 = ORIENTED_EDGE ( 'NONE', *, *, #63774, .T. ) ;
#208500 = CARTESIAN_POINT ( 'NONE',  ( -18.59999999999999787, 18.41524492703432614, -237.0006385043383546 ) ) ;
#208501 = ORIENTED_EDGE ( 'NONE', *, *, #164841, .T. ) ;
#208502 = CARTESIAN_POINT ( 'NONE',  ( -23.15000000000000213, 7.128833340093095217, -233.7327013124392749 ) ) ;
#208503 = LINE ( 'NONE', #92372, #161973 ) ;
#208504 = LINE ( 'NONE', #166823, #3420 ) ;
#208505 = CARTESIAN_POINT ( 'NONE',  ( -23.25000000000000000, 30.38404434817536881, -239.4399867032565794 ) ) ;
#208506 = DIRECTION ( 'NONE',  ( -1.000000000000000000, 0.000000000000000000, -0.000000000000000000 ) ) ;
#208507 = CIRCLE ( 'NONE', #16971, 0.09999999999999939493 ) ;
#208508 = LINE ( 'NONE', #169402, #8369 ) ;
#208509 = DIRECTION ( 'NONE',  ( 0.000000000000000000, 2.891205793294679805E-16, -1.000000000000000000 ) ) ;
#208511 = ORIENTED_EDGE ( 'NONE', *, *, #232990, .F. ) ;
#208510 = CARTESIAN_POINT ( 'NONE',  ( -20.94999999999999929, 77.16412189325305349, -95.10825939895268277 ) ) ;
#208513 = CARTESIAN_POINT ( 'NONE',  ( 18.59999999999999432, -1.162701749926853712, -75.10000000000003695 ) ) ;
#208512 = DIRECTION ( 'NONE',  ( 1.000000000000000000, 0.000000000000000000, 0.000000000000000000 ) ) ;
#208514 = VERTEX_POINT ( 'NONE', #122140 ) ;
#208516 = EDGE_LOOP ( 'NONE', ( #135470, #213365, #26854, #245412 ) ) ;
#208515 = DIRECTION ( 'NONE',  ( 0.000000000000000000, 1.000000000000000000, 0.000000000000000000 ) ) ;
#208517 = ORIENTED_EDGE ( 'NONE', *, *, #251587, .T. ) ;
#208518 = LINE ( 'NONE', #96236, #162330 ) ;
#208519 = DIRECTION ( 'NONE',  ( -1.000000000000000000, 0.000000000000000000, 0.000000000000000000 ) ) ;
#208520 = CARTESIAN_POINT ( 'NONE',  ( 22.49806830649814060, 75.92253568368623462, -81.17299713936340311 ) ) ;
#208521 = DIRECTION ( 'NONE',  ( 0.000000000000000000, 0.000000000000000000, 1.000000000000000000 ) ) ;
#208522 = CYLINDRICAL_SURFACE ( 'NONE', #77274, 0.09999999999999543976 ) ;
#208523 = DIRECTION ( 'NONE',  ( -0.000000000000000000, -0.000000000000000000, 1.000000000000000000 ) ) ;
#208524 = DIRECTION ( 'NONE',  ( 1.000000000000000000, 0.000000000000000000, 0.000000000000000000 ) ) ;
#208525 = AXIS2_PLACEMENT_3D ( 'NONE', #105579, #126458, #224269 ) ;
#208526 = CARTESIAN_POINT ( 'NONE',  ( 20.85000000000000142, -1.362429037193307435, -41.38888124792119783 ) ) ;
#208527 = ADVANCED_FACE ( 'NONE', ( #20486 ), #197513, .F. ) ;
#208528 = CARTESIAN_POINT ( 'NONE',  ( 18.49999999999999289, 65.70729864260954400, -30.56574559737245877 ) ) ;
#208529 = VERTEX_POINT ( 'NONE', #256437 ) ;
#208530 = ORIENTED_EDGE ( 'NONE', *, *, #114716, .T. ) ;
#208531 = VECTOR ( 'NONE', #108819, 1000.000000000000000 ) ;
#208532 = ORIENTED_EDGE ( 'NONE', *, *, #188927, .T. ) ;
#208533 = DIRECTION ( 'NONE',  ( 1.000000000000000000, 0.000000000000000000, 0.000000000000000000 ) ) ;
#208534 = ORIENTED_EDGE ( 'NONE', *, *, #131697, .T. ) ;
#208535 = CYLINDRICAL_SURFACE ( 'NONE', #155168, 0.1000000000000106498 ) ;
#208536 = AXIS2_PLACEMENT_3D ( 'NONE', #27185, #49273, #150951 ) ;
#208537 = DIRECTION ( 'NONE',  ( 0.000000000000000000, -0.000000000000000000, 1.000000000000000000 ) ) ;
#208538 = CARTESIAN_POINT ( 'NONE',  ( -21.00023020733438628, 69.60913075474422840, -103.0231074845243597 ) ) ;
#208539 = ADVANCED_FACE ( 'NONE', ( #235650 ), #101626, .T. ) ;
#208540 = DIRECTION ( 'NONE',  ( 0.000000000000000000, 0.4999999999999478195, -0.8660254037844686836 ) ) ;
#208541 = PLANE ( 'NONE',  #207974 ) ;
#208542 = EDGE_LOOP ( 'NONE', ( #151905, #124673, #9230, #200465 ) ) ;
#208543 = EDGE_CURVE ( 'NONE', #16536, #101606, #161277, .T. ) ;
#208544 = CARTESIAN_POINT ( 'NONE',  ( -23.39999999999994529, 77.26165318615413469, -44.00978271863746016 ) ) ;
#208545 = AXIS2_PLACEMENT_3D ( 'NONE', #2719, #118851, #220513 ) ;
#208546 = DIRECTION ( 'NONE',  ( 1.000000000000000000, 0.000000000000000000, 0.000000000000000000 ) ) ;
#208547 = CARTESIAN_POINT ( 'NONE',  ( 21.05000000000000071, 1.115600667400684642E-11, -100.5000000000000284 ) ) ;
#208548 = DIRECTION ( 'NONE',  ( 0.000000000000000000, -0.7035695228903323661, -0.7106264324241465813 ) ) ;
#208549 = DIRECTION ( 'NONE',  ( 0.000000000000000000, 0.000000000000000000, -1.000000000000000000 ) ) ;
#208550 = ORIENTED_EDGE ( 'NONE', *, *, #164606, .F. ) ;
#208553 = DIRECTION ( 'NONE',  ( 0.000000000000000000, 6.982962677686266711E-15, -1.000000000000000000 ) ) ;
#208552 = CARTESIAN_POINT ( 'NONE',  ( 21.07933241753356768, 61.09883511494023622, -234.2887083548779685 ) ) ;
#208551 = CIRCLE ( 'NONE', #220983, 0.1000000000000028644 ) ;
#208554 = EDGE_CURVE ( 'NONE', #3601, #154962, #80162, .T. ) ;
#208555 = ORIENTED_EDGE ( 'NONE', *, *, #212527, .T. ) ;
#208557 = VERTEX_POINT ( 'NONE', #56991 ) ;
#208556 = CARTESIAN_POINT ( 'NONE',  ( 20.94999999999999574, 67.07338541492521244, -161.5514244653012952 ) ) ;
#208558 = AXIS2_PLACEMENT_3D ( 'NONE', #45411, #87086, #188770 ) ;
#208559 = CARTESIAN_POINT ( 'NONE',  ( -16.91049119928364064, 9.950000000011138823, -113.1182796068092102 ) ) ;
#208560 = AXIS2_PLACEMENT_3D ( 'NONE', #169196, #253817, #248703 ) ;
#208561 = FACE_OUTER_BOUND ( 'NONE', #223919, .T. ) ;
#208562 = ADVANCED_FACE ( 'NONE', ( #870 ), #60864, .T. ) ;
#208563 = CARTESIAN_POINT ( 'NONE',  ( -20.64999999999999858, 1.115600667400684642E-11, -200.9999999999999432 ) ) ;
#208564 = ORIENTED_EDGE ( 'NONE', *, *, #10542, .T. ) ;
#208565 = DIRECTION ( 'NONE',  ( -0.000000000000000000, -1.000000000000000000, 0.000000000000000000 ) ) ;
#208566 = EDGE_CURVE ( 'NONE', #221781, #166364, #205895, .T. ) ;
#208568 = DIRECTION ( 'NONE',  ( 1.000000000000000000, 0.000000000000000000, -0.000000000000000000 ) ) ;
#208567 =( BOUNDED_SURFACE ( )  B_SPLINE_SURFACE ( 3, 2, ( 
 ( #203804, #104669, #5580 ),
 ( #185535, #120456, #121726 ),
 ( #85106, #201231, #242928 ),
 ( #199972, #164690, #241650 ),
 ( #22627, #4308, #102109 ),
 ( #181688, #83816, #3019 ) ),
 .UNSPECIFIED., .F., .F., .F. ) 
 B_SPLINE_SURFACE_WITH_KNOTS ( ( 4, 2, 4 ),
 ( 3, 3 ),
 ( 1.570796326794897668, 2.356194490192346169, 3.141592653589794448 ),
 ( 0.000000000000000000, 1.000000000000000000 ),
 .UNSPECIFIED. ) 
 GEOMETRIC_REPRESENTATION_ITEM ( )  RATIONAL_B_SPLINE_SURFACE ( (
 ( 1.000000000000000000, 0.7071067811865719976, 1.000000000000000000),
 ( 1.000000000000000000, 0.6611148371783983624, 1.000000000000000000),
 ( 1.000000000000000000, 0.6092287576689580098, 1.000000000000000000),
 ( 1.000000000000000000, 0.5278258667064269494, 1.000000000000000000),
 ( 1.000000000000000000, 0.4993418825329443700, 1.000000000000000000),
 ( 1.000000000000000000, 0.5000000000000260902, 1.000000000000000000) ) ) 
 REPRESENTATION_ITEM ( '' )  SURFACE ( )  );
#208569 = ADVANCED_FACE ( 'NONE', ( #141685 ), #142951, .T. ) ;
#208571 = DIRECTION ( 'NONE',  ( 0.000000000000000000, 0.000000000000000000, 1.000000000000000000 ) ) ;
#208570 = CARTESIAN_POINT ( 'NONE',  ( 22.20000000000000284, 3.362550747017869490, 28.82623795144604983 ) ) ;
#208573 = ORIENTED_EDGE ( 'NONE', *, *, #69963, .T. ) ;
#208572 = CARTESIAN_POINT ( 'NONE',  ( -18.58671080940898790, 47.00638226075548687, -255.2233826300025044 ) ) ;
#208574 = ADVANCED_FACE ( 'NONE', ( #127270 ), #7316, .F. ) ;
#208575 = AXIS2_PLACEMENT_3D ( 'NONE', #214954, #114579, #118438 ) ;
#208576 = ORIENTED_EDGE ( 'NONE', *, *, #72860, .F. ) ;
#208577 = CARTESIAN_POINT ( 'NONE',  ( -20.94999999999999929, 14.85285025691667293, -236.4388300032497057 ) ) ;
#208578 = DIRECTION ( 'NONE',  ( 0.000000000000000000, 1.000000000000000000, 0.000000000000000000 ) ) ;
#208579 = DIRECTION ( 'NONE',  ( 1.000000000000000000, 0.000000000000000000, 0.000000000000000000 ) ) ;
#208580 = VERTEX_POINT ( 'NONE', #84228 ) ;
#208581 = CARTESIAN_POINT ( 'NONE',  ( -16.79140778683509438, 9.944941598865719712, -188.3297372337707714 ) ) ;
#208582 = DIRECTION ( 'NONE',  ( 1.000000000000000000, 0.000000000000000000, 0.000000000000000000 ) ) ;
#208583 = CARTESIAN_POINT ( 'NONE',  ( 18.43565242384934066, -9.519327731081286714, -140.9729763765593589 ) ) ;
#208584 = EDGE_CURVE ( 'NONE', #45271, #12116, #105917, .T. ) ;
#208585 = EDGE_LOOP ( 'NONE', ( #246717, #61084, #66313, #182026 ) ) ;
#208586 = CARTESIAN_POINT ( 'NONE',  ( 20.12481660106788439, 60.19028478040584673, -225.4222410168123929 ) ) ;
#208587 = EDGE_CURVE ( 'NONE', #1731, #117008, #247205, .T. ) ;
#208588 = AXIS2_PLACEMENT_3D ( 'NONE', #152066, #252404, #93344 ) ;
#208589 = AXIS2_PLACEMENT_3D ( 'NONE', #211262, #32668, #232123 ) ;
#208590 = VERTEX_POINT ( 'NONE', #68587 ) ;
#208591 = AXIS2_PLACEMENT_3D ( 'NONE', #217987, #39412, #237587 ) ;
#208592 = CARTESIAN_POINT ( 'NONE',  ( -23.25000000000000000, 61.88149656937975607, -248.1136133839584090 ) ) ;
#208593 = CARTESIAN_POINT ( 'NONE',  ( 20.95512820512820440, 8.876151316299271343, -146.1500000000000341 ) ) ;
#208594 = EDGE_LOOP ( 'NONE', ( #222851, #48671, #153133 ) ) ;
#208595 = ORIENTED_EDGE ( 'NONE', *, *, #84352, .F. ) ;
#208596 = EDGE_CURVE ( 'NONE', #41988, #118767, #107699, .T. ) ;
#208597 = CARTESIAN_POINT ( 'NONE',  ( 20.94999999999999574, 43.57568952063339651, -245.1784935019914826 ) ) ;
#208598 = VERTEX_POINT ( 'NONE', #123420 ) ;
#208600 = VERTEX_POINT ( 'NONE', #163835 ) ;
#208599 = CARTESIAN_POINT ( 'NONE',  ( 22.49999999999999645, 25.98655542988603173, -254.2226763854395983 ) ) ;
#208601 = EDGE_LOOP ( 'NONE', ( #129518, #246064, #192224, #198582, #4758, #89719, #202004, #129801, #21269, #206021, #155052, #113323, #154672, #95020, #87473, #111104 ) ) ;
#208602 = AXIS2_PLACEMENT_3D ( 'NONE', #157800, #237294, #58629 ) ;
#208605 = ORIENTED_EDGE ( 'NONE', *, *, #180532, .T. ) ;
#208604 = VERTEX_POINT ( 'NONE', #184663 ) ;
#208603 = LINE ( 'NONE', #170794, #246974 ) ;
#208606 = CARTESIAN_POINT ( 'NONE',  ( -18.43634282235122868, -9.679787199916756180, -107.1606518854540440 ) ) ;
#208607 = ORIENTED_EDGE ( 'NONE', *, *, #209470, .F. ) ;
#208608 = CARTESIAN_POINT ( 'NONE',  ( -20.85000000000000142, -1.835859311432481045, -78.50443916879852679 ) ) ;
#208609 = CARTESIAN_POINT ( 'NONE',  ( 18.49999999999998934, 6.650000000011155876, -179.8499999999999943 ) ) ;
#208610 = DIRECTION ( 'NONE',  ( -0.000000000000000000, 1.000000000000000000, -0.000000000000000000 ) ) ;
#208611 = EDGE_CURVE ( 'NONE', #65335, #98906, #85061, .T. ) ;
#208612 = CARTESIAN_POINT ( 'NONE',  ( -17.22361732159832215, 65.65484434140915937, -58.15232295865727252 ) ) ;
#208613 = ORIENTED_EDGE ( 'NONE', *, *, #15510, .F. ) ;
#208614 = ORIENTED_EDGE ( 'NONE', *, *, #84462, .F. ) ;
#208615 = LINE ( 'NONE', #29992, #129056 ) ;
#208617 = ORIENTED_EDGE ( 'NONE', *, *, #245643, .F. ) ;
#208616 = DIRECTION ( 'NONE',  ( -2.952720810173288619E-16, 0.4721928772777346239, 0.8814952561688430555 ) ) ;
#208618 = DIRECTION ( 'NONE',  ( 1.000000000000000000, 3.265361837132813093E-16, -0.000000000000000000 ) ) ;
#208620 = EDGE_LOOP ( 'NONE', ( #49556, #137665 ) ) ;
#208619 = CARTESIAN_POINT ( 'NONE',  ( 22.88900146558018989, 8.703904791123973084, -109.7500000000000426 ) ) ;
#208621 = CIRCLE ( 'NONE', #96154, 0.9750000000000036415 ) ;
#208622 = ADVANCED_FACE ( 'NONE', ( #182115 ), #206809, .T. ) ;
#208623 = ORIENTED_EDGE ( 'NONE', *, *, #45849, .T. ) ;
#208624 = CARTESIAN_POINT ( 'NONE',  ( -18.50000000000000000, 7.021664781911246322, -104.3335654018973315 ) ) ;
#208625 = CIRCLE ( 'NONE', #166952, 11.65000000000000036 ) ;
#208626 = EDGE_CURVE ( 'NONE', #136054, #220667, #230869, .T. ) ;
#208627 = EDGE_CURVE ( 'NONE', #63775, #185172, #128555, .T. ) ;
#208628 = ORIENTED_EDGE ( 'NONE', *, *, #73264, .F. ) ;
#208629 = CARTESIAN_POINT ( 'NONE',  ( -18.59999999999999787, 66.75000000001230660, -157.7731074845244166 ) ) ;
#208630 = DIRECTION ( 'NONE',  ( 1.000000000000000000, 0.000000000000000000, 0.000000000000000000 ) ) ;
#208631 = EDGE_CURVE ( 'NONE', #143070, #182666, #24338, .T. ) ;
#208633 = EDGE_LOOP ( 'NONE', ( #91257, #120948, #239302, #225490 ) ) ;
#208632 = ORIENTED_EDGE ( 'NONE', *, *, #113216, .F. ) ;
#208634 = ORIENTED_EDGE ( 'NONE', *, *, #54873, .F. ) ;
#208635 = CARTESIAN_POINT ( 'NONE',  ( -18.40000000000000213, 13.19198836721619017, -207.5937580722650466 ) ) ;
#208636 = ORIENTED_EDGE ( 'NONE', *, *, #251052, .T. ) ;
#208637 = ORIENTED_EDGE ( 'NONE', *, *, #138131, .F. ) ;
#208638 = EDGE_CURVE ( 'NONE', #56738, #162791, #160135, .T. ) ;
#208639 = DIRECTION ( 'NONE',  ( -1.000000000000000000, -0.000000000000000000, 0.000000000000000000 ) ) ;
#208640 = AXIS2_PLACEMENT_3D ( 'NONE', #154230, #228595, #209018 ) ;
#208642 = ORIENTED_EDGE ( 'NONE', *, *, #172704, .T. ) ;
#208641 = LINE ( 'NONE', #91250, #139150 ) ;
#208643 = DIRECTION ( 'NONE',  ( 0.000000000000000000, -1.000000000000000000, 0.000000000000000000 ) ) ;
#208645 = DIRECTION ( 'NONE',  ( 0.000000000000000000, 0.000000000000000000, 1.000000000000000000 ) ) ;
#208644 = DIRECTION ( 'NONE',  ( 0.000000000000000000, -1.000000000000000000, 6.308085367188393199E-16 ) ) ;
#208646 = LINE ( 'NONE', #50808, #99144 ) ;
#208647 = DIRECTION ( 'NONE',  ( -1.000000000000000000, 0.000000000000000000, 0.000000000000000000 ) ) ;
#208648 = ORIENTED_EDGE ( 'NONE', *, *, #170007, .T. ) ;
#208649 = ORIENTED_EDGE ( 'NONE', *, *, #156724, .T. ) ;
#208650 = CARTESIAN_POINT ( 'NONE',  ( 21.05000000000000071, 2.449293598294710852E-16, -31.50000000000000000 ) ) ;
#208652 = ORIENTED_EDGE ( 'NONE', *, *, #6457, .T. ) ;
#208651 = AXIS2_PLACEMENT_3D ( 'NONE', #78880, #18923, #16386 ) ;
#208653 = VECTOR ( 'NONE', #96561, 1000.000000000000000 ) ;
#208654 = EDGE_CURVE ( 'NONE', #94515, #69727, #130879, .T. ) ;
#208655 = AXIS2_PLACEMENT_3D ( 'NONE', #211722, #35668, #134712 ) ;
#208656 = LINE ( 'NONE', #144791, #9404 ) ;
#208657 = ORIENTED_EDGE ( 'NONE', *, *, #20944, .F. ) ;
#208658 = VERTEX_POINT ( 'NONE', #82967 ) ;
#208659 =( BOUNDED_CURVE ( )  B_SPLINE_CURVE ( 3, ( #133383, #34303, #212914, #209058 ),
 .UNSPECIFIED., .F., .T. ) 
 B_SPLINE_CURVE_WITH_KNOTS ( ( 4, 4 ),
 ( 1.570796326794896558, 3.141592653589793116 ),
 .UNSPECIFIED. ) 
 CURVE ( )  GEOMETRIC_REPRESENTATION_ITEM ( )  RATIONAL_B_SPLINE_CURVE ( ( 1.000000000000000000, 0.8047378541243649375, 0.8047378541243649375, 1.000000000000000000 ) ) 
 REPRESENTATION_ITEM ( '' )  );
#208660 = CARTESIAN_POINT ( 'NONE',  ( 21.30000000000002558, 76.00000000001195133, -103.0231074845243171 ) ) ;
#208661 = LINE ( 'NONE', #87396, #232041 ) ;
#208663 = ORIENTED_EDGE ( 'NONE', *, *, #39020, .F. ) ;
#208662 = EDGE_CURVE ( 'NONE', #44347, #10713, #208110, .T. ) ;
#208664 = CARTESIAN_POINT ( 'NONE',  ( -21.14999999893415250, 11.75000000001115197, -107.3444953435264040 ) ) ;
#208665 = CARTESIAN_POINT ( 'NONE',  ( 20.94999999999999929, -11.29603075032412995, -70.04789915966391334 ) ) ;
#208666 = ORIENTED_EDGE ( 'NONE', *, *, #12510, .F. ) ;
#208667 = EDGE_CURVE ( 'NONE', #39957, #55352, #64254, .T. ) ;
#208668 = AXIS2_PLACEMENT_3D ( 'NONE', #64904, #164025, #244826 ) ;
#208669 = CARTESIAN_POINT ( 'NONE',  ( 18.59999999999999787, 77.83534155023598089, -57.86795619196132634 ) ) ;
#208671 = VECTOR ( 'NONE', #177760, 1000.000000000000000 ) ;
#208670 = DIRECTION ( 'NONE',  ( 0.000000000000000000, 1.000000000000000000, 0.000000000000000000 ) ) ;
#208673 = CARTESIAN_POINT ( 'NONE',  ( -23.25000000000000000, 1.115600667400684642E-11, -100.5000000000000284 ) ) ;
#208672 = DIRECTION ( 'NONE',  ( -1.000000000000000000, 0.000000000000000000, 0.000000000000000000 ) ) ;
#208674 = DIRECTION ( 'NONE',  ( 1.000000000000000000, -0.000000000000000000, -0.000000000000000000 ) ) ;
#208675 = CARTESIAN_POINT ( 'NONE',  ( 20.85000000000000142, 64.25000000001146816, -42.80697314750249660 ) ) ;
#208676 = CARTESIAN_POINT ( 'NONE',  ( 19.75857864376268935, 62.49201502323811752, -208.8221019049098857 ) ) ;
#208677 = CARTESIAN_POINT ( 'NONE',  ( -20.64999999999999858, 82.57900542960499024, -215.5587758314583482 ) ) ;
#208678 = EDGE_CURVE ( 'NONE', #54689, #205939, #166429, .T. ) ;
#208679 = EDGE_LOOP ( 'NONE', ( #83914, #128807, #202445, #168525 ) ) ;
#208680 = VECTOR ( 'NONE', #12478, 1000.000000000000000 ) ;
#208681 = AXIS2_PLACEMENT_3D ( 'NONE', #229695, #113593, #247957 ) ;
#208682 = AXIS2_PLACEMENT_3D ( 'NONE', #238206, #218637, #119577 ) ;
#208683 = CIRCLE ( 'NONE', #129562, 2.000000000000002220 ) ;
#208684 = CIRCLE ( 'NONE', #13056, 0.09999999999998898659 ) ;
#208686 = ORIENTED_EDGE ( 'NONE', *, *, #127846, .T. ) ;
#208685 = EDGE_LOOP ( 'NONE', ( #220539, #103773, #167989, #173447 ) ) ;
#208687 = VERTEX_POINT ( 'NONE', #28204 ) ;
#208688 = FACE_OUTER_BOUND ( 'NONE', #121497, .T. ) ;
#208689 = DIRECTION ( 'NONE',  ( 1.000000000000000000, 0.000000000000000000, 0.000000000000000000 ) ) ;
#208691 = DIRECTION ( 'NONE',  ( 0.000000000000000000, -0.4999999999999608646, 0.8660254037844612451 ) ) ;
#208690 = DIRECTION ( 'NONE',  ( 0.000000000000000000, -0.9654421110809058293, -0.2606175937108693996 ) ) ;
#208692 = DIRECTION ( 'NONE',  ( 0.000000000000000000, 0.8700118002898393765, -0.4930308989875104575 ) ) ;
#208693 = ORIENTED_EDGE ( 'NONE', *, *, #200141, .F. ) ;
#208694 = CARTESIAN_POINT ( 'NONE',  ( 20.94999999999999929, 70.60000000001251408, -179.9170766071768526 ) ) ;
#208695 = AXIS2_PLACEMENT_3D ( 'NONE', #156368, #241012, #78068 ) ;
#208697 = EDGE_CURVE ( 'NONE', #41142, #133931, #76708, .T. ) ;
#208696 = VERTEX_POINT ( 'NONE', #245941 ) ;
#208698 = CARTESIAN_POINT ( 'NONE',  ( -18.50000000000000000, 64.35000000001214460, -136.5231074845244166 ) ) ;
#208699 = DIRECTION ( 'NONE',  ( 0.000000000000000000, -0.4105728183244014562, -0.9118278131605539460 ) ) ;
#208700 = CARTESIAN_POINT ( 'NONE',  ( 17.74533788810831325, 65.18150020854182003, -193.2094848095768782 ) ) ;
#208701 = VERTEX_POINT ( 'NONE', #47713 ) ;
#208702 = DIRECTION ( 'NONE',  ( -3.787827842127534447E-15, -0.7397360091702729346, -0.6728971962616859814 ) ) ;
#208703 = LINE ( 'NONE', #209978, #46502 ) ;
#208704 = VERTEX_POINT ( 'NONE', #187261 ) ;
#208705 = ORIENTED_EDGE ( 'NONE', *, *, #75017, .T. ) ;
#208706 = CARTESIAN_POINT ( 'NONE',  ( -23.15000000000000213, 1.115600667400684642E-11, -134.0000000000000284 ) ) ;
#208707 = CYLINDRICAL_SURFACE ( 'NONE', #35597, 0.1000000000000024342 ) ;
#208708 = CYLINDRICAL_SURFACE ( 'NONE', #161289, 0.1000000000000028644 ) ;
#208709 = CARTESIAN_POINT ( 'NONE',  ( -23.15000000000000213, 74.00000000001229239, -156.7984855617622770 ) ) ;
#208710 = CARTESIAN_POINT ( 'NONE',  ( -18.50000000000000000, 70.47363787294415260, -228.3418745167492432 ) ) ;
#208711 = CARTESIAN_POINT ( 'NONE',  ( -21.14999999999999858, 64.25000000001215028, -136.4231074845243938 ) ) ;
#208712 = VERTEX_POINT ( 'NONE', #8610 ) ;
#208713 = CARTESIAN_POINT ( 'NONE',  ( -6.000000000000003553, -11.34999999999999964, 10.10000000000000142 ) ) ;
#208714 = TOROIDAL_SURFACE ( 'NONE', #229552, 11.89999999999999858, 0.1000000000000000056 ) ;
#208715 = EDGE_CURVE ( 'NONE', #239420, #240431, #239218, .T. ) ;
#208717 = CARTESIAN_POINT ( 'NONE',  ( -21.14999999893415250, 11.75000000001115197, -174.3444953435266598 ) ) ;
#208716 = CARTESIAN_POINT ( 'NONE',  ( 18.59999999999999787, -9.849999999999990763, 31.50000000000000000 ) ) ;
#208718 = CARTESIAN_POINT ( 'NONE',  ( 19.75857864376268935, 11.65000000001115943, -91.75000000000005684 ) ) ;
#208719 = CARTESIAN_POINT ( 'NONE',  ( 23.24999999999999289, 64.25000000001276135, -215.2731074845244450 ) ) ;
#208721 = EDGE_CURVE ( 'NONE', #119770, #201185, #97532, .T. ) ;
#208720 = CARTESIAN_POINT ( 'NONE',  ( -21.64999999999999858, 10.05000000001113847, -87.75000000000005684 ) ) ;
#208722 = CARTESIAN_POINT ( 'NONE',  ( 20.94403535211772294, 10.30632246271647467, -139.5041836778896140 ) ) ;
#208724 = ORIENTED_EDGE ( 'NONE', *, *, #117240, .T. ) ;
#208723 = FACE_OUTER_BOUND ( 'NONE', #177971, .T. ) ;
#208725 = EDGE_CURVE ( 'NONE', #60383, #242024, #222429, .T. ) ;
#208726 = CIRCLE ( 'NONE', #33778, 0.1000000000000028644 ) ;
#208727 = EDGE_CURVE ( 'NONE', #111851, #199002, #86165, .T. ) ;
#208728 = DIRECTION ( 'NONE',  ( 0.000000000000000000, 0.000000000000000000, -1.000000000000000000 ) ) ;
#208729 = DIRECTION ( 'NONE',  ( -1.000000000000000000, 0.000000000000000000, 0.000000000000000000 ) ) ;
#208730 = CARTESIAN_POINT ( 'NONE',  ( 23.24999999999999289, 64.35000000001204512, -124.3731074845243825 ) ) ;
#208731 = AXIS2_PLACEMENT_3D ( 'NONE', #111844, #32329, #251329 ) ;
#208732 = VERTEX_POINT ( 'NONE', #16864 ) ;
#208733 = VECTOR ( 'NONE', #127180, 1000.000000000000000 ) ;
#208734 = EDGE_CURVE ( 'NONE', #174146, #223676, #1694, .T. ) ;
#208735 = FACE_OUTER_BOUND ( 'NONE', #51528, .T. ) ;
#208736 = ADVANCED_FACE ( 'NONE', ( #192930 ), #180780, .T. ) ;
#208737 = DIRECTION ( 'NONE',  ( 0.000000000000000000, 0.000000000000000000, 1.000000000000000000 ) ) ;
#208739 = DIRECTION ( 'NONE',  ( -1.000000000000000000, 0.000000000000000000, 0.000000000000000000 ) ) ;
#208738 = AXIS2_PLACEMENT_3D ( 'NONE', #108125, #187679, #188946 ) ;
#208740 = ORIENTED_EDGE ( 'NONE', *, *, #33816, .T. ) ;
#208741 = CARTESIAN_POINT ( 'NONE',  ( 21.05000000000000071, 78.08573236070779444, -228.9307947190811774 ) ) ;
#208743 = ORIENTED_EDGE ( 'NONE', *, *, #226223, .T. ) ;
#208742 = CARTESIAN_POINT ( 'NONE',  ( 21.05000000000000071, 87.48912529308779540, -72.52310748452423184 ) ) ;
#208744 = CARTESIAN_POINT ( 'NONE',  ( 21.07928932188134397, -1.250084634896337255, -194.7953894783290423 ) ) ;
#208745 = DIRECTION ( 'NONE',  ( 0.000000000000000000, -7.056502275159890043E-15, 1.000000000000000000 ) ) ;
#208746 = VERTEX_POINT ( 'NONE', #93808 ) ;
#208747 = CARTESIAN_POINT ( 'NONE',  ( -16.84981964351500139, 66.08268176591401755, -190.6535058705039773 ) ) ;
#208748 = APPLICATION_PROTOCOL_DEFINITION ( 'draft international standard', 'automotive_design', 1998, #235521 ) ;
#208749 = DIRECTION ( 'NONE',  ( 0.000000000000000000, -0.1568667991644693838, -0.9876197685951279004 ) ) ;
#208750 = EDGE_CURVE ( 'NONE', #246278, #4741, #243297, .T. ) ;
#208751 = CYLINDRICAL_SURFACE ( 'NONE', #110621, 0.8750000000000007772 ) ;
#208752 = CIRCLE ( 'NONE', #426, 11.74999999999999645 ) ;
#208753 = VERTEX_POINT ( 'NONE', #115960 ) ;
#208754 = DIRECTION ( 'NONE',  ( 1.000000000000000000, -0.000000000000000000, -0.000000000000000000 ) ) ;
#208755 = CARTESIAN_POINT ( 'NONE',  ( -20.54999999999999716, 71.75000000001186606, -90.77310748452434552 ) ) ;
#208756 = EDGE_CURVE ( 'NONE', #100676, #18989, #5961, .T. ) ;
#208757 = DIRECTION ( 'NONE',  ( 1.652117596168391306E-15, 0.9770955615653313941, 0.2128009952263603677 ) ) ;
#208758 = ORIENTED_EDGE ( 'NONE', *, *, #108863, .T. ) ;
#208759 = EDGE_LOOP ( 'NONE', ( #2276, #190354, #80761, #135913 ) ) ;
#208760 = EDGE_CURVE ( 'NONE', #44981, #200910, #247395, .T. ) ;
#208761 = CARTESIAN_POINT ( 'NONE',  ( 18.45139536634708577, 85.48608172029307184, -96.38259586671357226 ) ) ;
#208763 = CARTESIAN_POINT ( 'NONE',  ( 21.13461538461538680, 8.885417037985614996, -146.3500000000000227 ) ) ;
#208762 = AXIS2_PLACEMENT_3D ( 'NONE', #12774, #92276, #53158 ) ;
#208764 = AXIS2_PLACEMENT_3D ( 'NONE', #7379, #8673, #208174 ) ;
#208767 = CARTESIAN_POINT ( 'NONE',  ( 22.41477678272288188, -2.478238346927450930, -189.6170666049704323 ) ) ;
#208766 = AXIS2_PLACEMENT_3D ( 'NONE', #2168, #41343, #102532 ) ;
#208765 = FACE_OUTER_BOUND ( 'NONE', #244588, .T. ) ;
#208768 = EDGE_CURVE ( 'NONE', #39159, #121769, #33896, .T. ) ;
#208769 = DIRECTION ( 'NONE',  ( 0.000000000000000000, -0.000000000000000000, 1.000000000000000000 ) ) ;
#208770 = CYLINDRICAL_SURFACE ( 'NONE', #214395, 0.9000000000000014655 ) ;
#208771 = CARTESIAN_POINT ( 'NONE',  ( -18.42609945526357862, 46.93054533616035684, -255.3593356979593239 ) ) ;
#208773 = ORIENTED_EDGE ( 'NONE', *, *, #122032, .T. ) ;
#208772 = DIRECTION ( 'NONE',  ( 0.000000000000000000, 0.4088369013363783999, -0.9126074666063545004 ) ) ;
#208774 = DIRECTION ( 'NONE',  ( 0.000000000000000000, 0.000000000000000000, 1.000000000000000000 ) ) ;
#208775 = DIRECTION ( 'NONE',  ( 0.000000000000000000, 0.9126074666063844765, 0.4088369013363114535 ) ) ;
#208777 = DIRECTION ( 'NONE',  ( -4.701977403289178058E-30, 1.734723475976807094E-14, -1.000000000000000000 ) ) ;
#208776 = CARTESIAN_POINT ( 'NONE',  ( 23.14999999999999858, 1.115649653272650466E-11, -63.00000000000000000 ) ) ;
#208778 = ORIENTED_EDGE ( 'NONE', *, *, #124433, .T. ) ;
#208779 = LINE ( 'NONE', #11878, #18472 ) ;
#208780 = DIRECTION ( 'NONE',  ( -1.000000000000000000, 0.000000000000000000, 0.000000000000000000 ) ) ;
#208781 = EDGE_CURVE ( 'NONE', #181475, #132493, #96362, .T. ) ;
#208782 = DIRECTION ( 'NONE',  ( 0.000000000000000000, 0.000000000000000000, -1.000000000000000000 ) ) ;
#208783 = DIRECTION ( 'NONE',  ( 0.000000000000000000, 6.982962677686267499E-15, -1.000000000000000000 ) ) ;
#208784 = VERTEX_POINT ( 'NONE', #54685 ) ;
#208786 = VERTEX_POINT ( 'NONE', #254157 ) ;
#208785 = AXIS2_PLACEMENT_3D ( 'NONE', #111913, #213552, #153647 ) ;
#208787 = CARTESIAN_POINT ( 'NONE',  ( 18.39999999999999858, 38.26833061496694199, -261.1904200532067648 ) ) ;
#208788 = ORIENTED_EDGE ( 'NONE', *, *, #30258, .T. ) ;
#208789 = CARTESIAN_POINT ( 'NONE',  ( -21.05000000000000071, 12.81615072508355802, -205.2382006284440763 ) ) ;
#208790 = ORIENTED_EDGE ( 'NONE', *, *, #222456, .T. ) ;
#208791 = DIRECTION ( 'NONE',  ( 0.000000000000000000, 0.4999999999999649170, -0.8660254037844589137 ) ) ;
#208792 = CYLINDRICAL_SURFACE ( 'NONE', #64976, 0.09999999999998898659 ) ;
#208793 = DIRECTION ( 'NONE',  ( 0.000000000000000000, 0.000000000000000000, -1.000000000000000000 ) ) ;
#208794 = VERTEX_POINT ( 'NONE', #11736 ) ;
#208795 = AXIS2_PLACEMENT_3D ( 'NONE', #36579, #58643, #57364 ) ;
#208796 = DIRECTION ( 'NONE',  ( -1.000000000000000000, 1.652117596168391700E-15, 0.000000000000000000 ) ) ;
#208797 = LINE ( 'NONE', #8037, #249253 ) ;
#208798 = AXIS2_PLACEMENT_3D ( 'NONE', #229914, #31749, #209066 ) ;
#208799 = DIRECTION ( 'NONE',  ( -1.000000000000000000, -0.000000000000000000, -0.000000000000000000 ) ) ;
#208800 = DIRECTION ( 'NONE',  ( -0.000000000000000000, -0.2128009952263607285, 0.9770955615653316162 ) ) ;
#208801 = CYLINDRICAL_SURFACE ( 'NONE', #170546, 0.1000000000000028644 ) ;
#208803 = DIRECTION ( 'NONE',  ( 0.000000000000000000, 0.4999999999999956701, -0.8660254037844411501 ) ) ;
#208802 = VECTOR ( 'NONE', #16452, 1000.000000000000000 ) ;
#208804 = ORIENTED_EDGE ( 'NONE', *, *, #254777, .T. ) ;
#208805 = EDGE_LOOP ( 'NONE', ( #236155, #196189, #210024, #130756 ) ) ;
#208807 = VERTEX_POINT ( 'NONE', #35171 ) ;
#208806 = DIRECTION ( 'NONE',  ( 0.000000000000000000, 0.000000000000000000, -1.000000000000000000 ) ) ;
#208808 = ORIENTED_EDGE ( 'NONE', *, *, #92437, .T. ) ;
#208809 = DIRECTION ( 'NONE',  ( 0.000000000000000000, 6.982962677686266711E-15, -1.000000000000000000 ) ) ;
#208810 = TOROIDAL_SURFACE ( 'NONE', #100438, 0.4000000000000015210, 0.1000000000000000056 ) ;
#208811 = CARTESIAN_POINT ( 'NONE',  ( 12.68104795156995479, 66.60346600605836898, -152.1171677053511360 ) ) ;
#208812 = DIRECTION ( 'NONE',  ( 0.000000000000000000, -0.4930308989875248349, -0.8700118002898312719 ) ) ;
#208813 = AXIS2_PLACEMENT_3D ( 'NONE', #72786, #92304, #53185 ) ;
#208814 = ORIENTED_EDGE ( 'NONE', *, *, #235454, .F. ) ;
#208815 = CARTESIAN_POINT ( 'NONE',  ( 21.05000000000000071, 82.48249193998721296, -215.5326005316167084 ) ) ;
#208816 = DIRECTION ( 'NONE',  ( 0.000000000000000000, 0.2128009952263688886, -0.9770955615653297288 ) ) ;
#208817 = ORIENTED_EDGE ( 'NONE', *, *, #184356, .F. ) ;
#208818 = TOROIDAL_SURFACE ( 'NONE', #79783, 3.899999999999999467, 0.1000000000000000056 ) ;
#208819 = CARTESIAN_POINT ( 'NONE',  ( 18.46082813848010673, -9.480749650896242997, -174.5843701027156385 ) ) ;
#208820 = EDGE_CURVE ( 'NONE', #154033, #210105, #194232, .T. ) ;
#208821 = FACE_OUTER_BOUND ( 'NONE', #57676, .T. ) ;
#208822 = AXIS2_PLACEMENT_3D ( 'NONE', #123840, #186385, #5129 ) ;
#208823 = ORIENTED_EDGE ( 'NONE', *, *, #221324, .T. ) ;
#208824 = FACE_OUTER_BOUND ( 'NONE', #149585, .T. ) ;
#208825 = VECTOR ( 'NONE', #96262, 1000.000000000000000 ) ;
#208826 = VERTEX_POINT ( 'NONE', #195516 ) ;
#208827 = DIRECTION ( 'NONE',  ( 1.000000000000000000, 0.000000000000000000, 0.000000000000000000 ) ) ;
#208828 = ORIENTED_EDGE ( 'NONE', *, *, #31471, .T. ) ;
#208829 = DIRECTION ( 'NONE',  ( 0.000000000000000000, -0.9999631594459056361, -0.008583690987124413183 ) ) ;
#208830 = AXIS2_PLACEMENT_3D ( 'NONE', #38447, #196229, #175422 ) ;
#208831 = ADVANCED_FACE ( 'NONE', ( #211197 ), #13026, .T. ) ;
#208832 = SPHERICAL_SURFACE ( 'NONE', #134949, 0.1000000000000000056 ) ;
#208833 = CIRCLE ( 'NONE', #154874, 0.9000000000000014655 ) ;
#208834 = CARTESIAN_POINT ( 'NONE',  ( 18.49999999999999289, 7.021664781911246322, -137.8335654018973457 ) ) ;
#208835 = ADVANCED_FACE ( 'NONE', ( #172119 ), #31316, .F. ) ;
#208836 = DIRECTION ( 'NONE',  ( 1.000000000000000000, 0.000000000000000000, 0.000000000000000000 ) ) ;
#208837 = CYLINDRICAL_SURFACE ( 'NONE', #176407, 0.09999999999999939493 ) ;
#208838 = AXIS2_PLACEMENT_3D ( 'NONE', #161670, #78244, #156544 ) ;
#208839 = ORIENTED_EDGE ( 'NONE', *, *, #87723, .F. ) ;
#208840 = DIRECTION ( 'NONE',  ( 0.000000000000000000, 0.9916376685811618685, -0.1290532225514649800 ) ) ;
#208841 = AXIS2_PLACEMENT_3D ( 'NONE', #35275, #114773, #95208 ) ;
#208842 = VERTEX_POINT ( 'NONE', #92521 ) ;
#208844 = FACE_OUTER_BOUND ( 'NONE', #35936, .T. ) ;
#208843 = CARTESIAN_POINT ( 'NONE',  ( 20.94999999999999929, 1.115624548013267999E-11, -98.60000000000005116 ) ) ;
#208845 = AXIS2_PLACEMENT_3D ( 'NONE', #221260, #218692, #165161 ) ;
#208846 = VERTEX_POINT ( 'NONE', #152546 ) ;
#208847 = CARTESIAN_POINT ( 'NONE',  ( 21.05000000000000071, -0.01454569055837845459, -60.50298221356805328 ) ) ;
#208848 = CARTESIAN_POINT ( 'NONE',  ( 18.59999999999999432, 68.22930980752001062, -227.7331931781284879 ) ) ;
#208849 = ADVANCED_FACE ( 'NONE', ( #232065 ), #80795, .T. ) ;
#208850 = CARTESIAN_POINT ( 'NONE',  ( 20.95556889135987788, 58.98008573395630805, -225.6988595695161166 ) ) ;
#208851 = EDGE_LOOP ( 'NONE', ( #234492, #240243, #213423, #149801 ) ) ;
#208853 = VERTEX_POINT ( 'NONE', #41574 ) ;
#208852 = DIRECTION ( 'NONE',  ( 0.000000000000000000, -0.4721928772777346239, -0.8814952561688430555 ) ) ;
#208854 = EDGE_CURVE ( 'NONE', #97109, #56847, #26861, .T. ) ;
#208855 = DIRECTION ( 'NONE',  ( 1.000000000000000000, 0.000000000000000000, 0.000000000000000000 ) ) ;
#208856 = EDGE_CURVE ( 'NONE', #247, #220817, #61104, .T. ) ;
#208858 = FACE_OUTER_BOUND ( 'NONE', #221549, .T. ) ;
#208857 = DIRECTION ( 'NONE',  ( 0.000000000000000000, -1.000000000000000000, -6.982962677686265922E-15 ) ) ;
#208860 = ORIENTED_EDGE ( 'NONE', *, *, #113805, .F. ) ;
#208859 = LINE ( 'NONE', #90170, #215473 ) ;
#208861 = ORIENTED_EDGE ( 'NONE', *, *, #186320, .T. ) ;
#208862 = CARTESIAN_POINT ( 'NONE',  ( 18.59999999999999076, 6.450000000011156587, -188.6499999999999488 ) ) ;
#208863 = CARTESIAN_POINT ( 'NONE',  ( 21.04999999999999716, 67.12791932463410660, -94.50206006569311512 ) ) ;
#208864 = ORIENTED_EDGE ( 'NONE', *, *, #41030, .F. ) ;
#208865 = DIRECTION ( 'NONE',  ( -1.000000000000000000, -3.469446951953635015E-14, -2.422701857770461054E-28 ) ) ;
#208866 = EDGE_CURVE ( 'NONE', #132867, #228310, #130837, .T. ) ;
#208867 = ORIENTED_EDGE ( 'NONE', *, *, #152497, .F. ) ;
#208868 = FACE_OUTER_BOUND ( 'NONE', #226765, .T. ) ;
#208869 = DIRECTION ( 'NONE',  ( 0.000000000000000000, 0.000000000000000000, 1.000000000000000000 ) ) ;
#208870 = ORIENTED_EDGE ( 'NONE', *, *, #254699, .T. ) ;
#208871 = CARTESIAN_POINT ( 'NONE',  ( -23.15000000000000213, 2.739812813550878801, -213.5801053551551547 ) ) ;
#208872 = AXIS2_PLACEMENT_3D ( 'NONE', #102387, #45021, #121992 ) ;
#208873 = ADVANCED_FACE ( 'NONE', ( #238462 ), #121116, .F. ) ;
#208874 = ORIENTED_EDGE ( 'NONE', *, *, #142931, .F. ) ;
#208875 = CARTESIAN_POINT ( 'NONE',  ( -22.94999999999999929, 6.223900101154156594, 12.09999999999999964 ) ) ;
#208877 = VERTEX_POINT ( 'NONE', #200625 ) ;
#208876 = AXIS2_PLACEMENT_3D ( 'NONE', #91940, #171515, #250993 ) ;
#208878 = EDGE_LOOP ( 'NONE', ( #84071, #45619, #14650, #162844 ) ) ;
#208879 = CARTESIAN_POINT ( 'NONE',  ( -21.05000000000000071, 61.18226735070197009, -234.2477531894260494 ) ) ;
#208880 = VERTEX_POINT ( 'NONE', #1106 ) ;
#208881 = CARTESIAN_POINT ( 'NONE',  ( 23.14999999999999858, 76.00000000001229239, -157.1481074845243882 ) ) ;
#208882 = VERTEX_POINT ( 'NONE', #161513 ) ;
#208884 = VERTEX_POINT ( 'NONE', #80650 ) ;
#208883 = CARTESIAN_POINT ( 'NONE',  ( 21.14999999999999858, 76.00000000001276135, -215.1726782920691505 ) ) ;
#208885 = APPLICATION_CONTEXT ( 'automotive_design' ) ;
#208886 = ORIENTED_EDGE ( 'NONE', *, *, #51045, .F. ) ;
#208887 = CARTESIAN_POINT ( 'NONE',  ( -18.59999999999999787, -10.84999999999999076, -15.00000000000000000 ) ) ;
#208888 = EDGE_LOOP ( 'NONE', ( #202490, #41559, #187857, #86009 ) ) ;
#208890 = EDGE_LOOP ( 'NONE', ( #15268, #114704, #217544, #53980 ) ) ;
#208889 = ORIENTED_EDGE ( 'NONE', *, *, #126277, .F. ) ;
#208891 = CYLINDRICAL_SURFACE ( 'NONE', #240377, 2.000000000000001776 ) ;
#208892 = CARTESIAN_POINT ( 'NONE',  ( -21.05000000000000071, 76.00000000001213607, -136.5231074845242745 ) ) ;
#208893 = AXIS2_PLACEMENT_3D ( 'NONE', #200359, #63395, #242041 ) ;
#208894 = ORIENTED_EDGE ( 'NONE', *, *, #127346, .F. ) ;
#208895 = TOROIDAL_SURFACE ( 'NONE', #92366, 3.900000000000000355, 0.1000000000000000056 ) ;
#208896 = AXIS2_PLACEMENT_3D ( 'NONE', #18268, #97767, #256816 ) ;
#208897 = EDGE_CURVE ( 'NONE', #185478, #161501, #160239, .T. ) ;
#208898 = EDGE_CURVE ( 'NONE', #27038, #86618, #35072, .T. ) ;
#208899 = ORIENTED_EDGE ( 'NONE', *, *, #253038, .T. ) ;
#208900 = DIRECTION ( 'NONE',  ( 0.000000000000000000, 1.000000000000000000, 1.734723475976807292E-15 ) ) ;
#208902 = VERTEX_POINT ( 'NONE', #218880 ) ;
#208901 = DIRECTION ( 'NONE',  ( -1.000000000000000000, 0.000000000000000000, 0.000000000000000000 ) ) ;
#208903 = CARTESIAN_POINT ( 'NONE',  ( 23.14999999999999858, 5.000000000011153745, -112.9052660189131245 ) ) ;
#208904 = EDGE_LOOP ( 'NONE', ( #20335, #245470, #103322 ) ) ;
#208905 = EDGE_CURVE ( 'NONE', #189963, #53606, #251063, .T. ) ;
#208907 = EDGE_CURVE ( 'NONE', #47690, #63666, #139338, .T. ) ;
#208906 = FACE_OUTER_BOUND ( 'NONE', #228151, .T. ) ;
#208908 = DIRECTION ( 'NONE',  ( 0.000000000000000000, 0.1568667991644863147, 0.9876197685951252359 ) ) ;
#208909 = ORIENTED_EDGE ( 'NONE', *, *, #111455, .F. ) ;
#208910 = CARTESIAN_POINT ( 'NONE',  ( 18.49505832270841310, 85.43802806279451545, -62.32463430963041162 ) ) ;
#208911 = CARTESIAN_POINT ( 'NONE',  ( 18.55807992284871588, 18.40923646582965745, -236.9894833875398206 ) ) ;
#208912 = CIRCLE ( 'NONE', #96465, 0.09999999999999749367 ) ;
#208913 = ADVANCED_FACE ( 'NONE', ( #196757 ), #3692, .T. ) ;
#208914 = ORIENTED_EDGE ( 'NONE', *, *, #93755, .F. ) ;
#208915 = ORIENTED_EDGE ( 'NONE', *, *, #24728, .T. ) ;
#208917 = EDGE_CURVE ( 'NONE', #14506, #82047, #18068, .T. ) ;
#208916 = CARTESIAN_POINT ( 'NONE',  ( 18.59999999999999787, 43.57281345108133053, -239.9888335660389487 ) ) ;
#208919 = ADVANCED_FACE ( 'NONE', ( #42833 ), #214283, .T. ) ;
#208918 = EDGE_CURVE ( 'NONE', #202918, #108079, #156035, .T. ) ;
#208921 = EDGE_LOOP ( 'NONE', ( #164796, #243206, #115275, #18592 ) ) ;
#208920 = ORIENTED_EDGE ( 'NONE', *, *, #218512, .T. ) ;
#208922 = ORIENTED_EDGE ( 'NONE', *, *, #146931, .T. ) ;
#208923 = CARTESIAN_POINT ( 'NONE',  ( 18.79999999999999716, 11.50977166988710820, -1.786320531569725478 ) ) ;
#208924 = EDGE_LOOP ( 'NONE', ( #171129, #70365, #254330, #178285 ) ) ;
#208925 = ORIENTED_EDGE ( 'NONE', *, *, #91019, .F. ) ;
#208926 = DIRECTION ( 'NONE',  ( -1.836970198721029934E-16, 1.000000000000000000, 0.000000000000000000 ) ) ;
#208927 = ORIENTED_EDGE ( 'NONE', *, *, #247502, .T. ) ;
#208928 = DIRECTION ( 'NONE',  ( 1.000000000000000000, -0.000000000000000000, 0.000000000000000000 ) ) ;
#208929 = CARTESIAN_POINT ( 'NONE',  ( -20.64999999999999858, 68.85000000001200249, -115.3731074845243540 ) ) ;
#208930 = ORIENTED_EDGE ( 'NONE', *, *, #184736, .F. ) ;
#208931 = ADVANCED_FACE ( 'NONE', ( #122374 ), #243596, .T. ) ;
#208932 = CIRCLE ( 'NONE', #250614, 0.1999999999999987899 ) ;
#208933 = CIRCLE ( 'NONE', #254671, 0.09999999999999939493 ) ;
#208934 = ORIENTED_EDGE ( 'NONE', *, *, #37561, .F. ) ;
#208935 = VECTOR ( 'NONE', #51251, 1000.000000000000000 ) ;
#208936 = DIRECTION ( 'NONE',  ( -1.000000000000000000, 0.000000000000000000, 0.000000000000000000 ) ) ;
#208937 = EDGE_CURVE ( 'NONE', #250411, #168984, #193447, .T. ) ;
#208938 = ADVANCED_FACE ( 'NONE', ( #25843 ), #66248, .F. ) ;
#208939 = EDGE_LOOP ( 'NONE', ( #45551, #205236, #149477, #124644 ) ) ;
#208940 = EDGE_CURVE ( 'NONE', #44364, #160821, #241837, .T. ) ;
#208941 = FACE_OUTER_BOUND ( 'NONE', #46138, .T. ) ;
#208942 = ORIENTED_EDGE ( 'NONE', *, *, #69183, .T. ) ;
#208944 = ORIENTED_EDGE ( 'NONE', *, *, #92457, .T. ) ;
#208943 = CARTESIAN_POINT ( 'NONE',  ( 18.60000000000000497, 1.115600667400684642E-11, -67.00000000000004263 ) ) ;
#208945 = FACE_OUTER_BOUND ( 'NONE', #184098, .T. ) ;
#208946 = DIRECTION ( 'NONE',  ( 0.000000000000000000, -0.3738317757009718689, 0.9274965247785342815 ) ) ;
#208947 = ADVANCED_FACE ( 'NONE', ( #145763 ), #222622, .F. ) ;
#208948 = DIRECTION ( 'NONE',  ( 0.000000000000000000, 0.9126074666063545004, 0.4088369013363783999 ) ) ;
#208949 = VECTOR ( 'NONE', #25631, 1000.000000000000000 ) ;
#208950 = CARTESIAN_POINT ( 'NONE',  ( -21.08479644141222664, 6.345038657743036659, -133.9414455574358556 ) ) ;
#208951 = CARTESIAN_POINT ( 'NONE',  ( -22.39999999999999858, 0.1000000000111554016, -92.70922040162662370 ) ) ;
#208952 = CARTESIAN_POINT ( 'NONE',  ( -21.44999999999999929, 68.85000000001186038, -90.67310748452435121 ) ) ;
#208953 = CARTESIAN_POINT ( 'NONE',  ( 18.60000000000000142, 85.40000000001258229, -196.2258477248609836 ) ) ;
#208954 = CARTESIAN_POINT ( 'NONE',  ( 18.39999999999999858, 37.95493834378066822, -261.2294694241335264 ) ) ;
#208955 = DIRECTION ( 'NONE',  ( 0.000000000000000000, -0.1332476588733589040, 0.9910827722268048534 ) ) ;
#208956 = B_SPLINE_CURVE_WITH_KNOTS ( 'NONE', 3,
 ( #250652, #8219, #172464, #225932, #47305, #14653 ),
 .UNSPECIFIED., .F., .F.,
 ( 4, 2, 4 ),
 ( 0.000000000000000000, 0.0001496588209255844779, 0.0002993176418511689558 ),
 .UNSPECIFIED. ) ;
#208957 = ORIENTED_EDGE ( 'NONE', *, *, #16643, .T. ) ;
#208958 = EDGE_LOOP ( 'NONE', ( #137972, #129481, #186138, #150413, #25880, #100320, #152858, #223726, #110461, #157347, #157035, #94068, #84455, #255153, #144057, #196497, #54000, #252786, #239818, #242200, #129340, #257541, #237317, #62646, #37253 ) ) ;
#208960 = ORIENTED_EDGE ( 'NONE', *, *, #257784, .T. ) ;
#208959 = DIRECTION ( 'NONE',  ( 0.000000000000000000, 0.000000000000000000, -1.000000000000000000 ) ) ;
#208961 = ORIENTED_EDGE ( 'NONE', *, *, #113779, .T. ) ;
#208962 = CARTESIAN_POINT ( 'NONE',  ( -16.91256925476571027, 66.01426884188369115, -90.49074997352965966 ) ) ;
#208963 = VECTOR ( 'NONE', #74575, 1000.000000000000000 ) ;
#208964 = CARTESIAN_POINT ( 'NONE',  ( 21.14999999999999858, 6.540656951712400691, -100.5000000000000284 ) ) ;
#208966 = CARTESIAN_POINT ( 'NONE',  ( 21.12230431290519661, 1.438979023680419633, -230.6788918746589161 ) ) ;
#208965 = DIRECTION ( 'NONE',  ( 1.000000000000000000, 0.000000000000000000, 0.000000000000000000 ) ) ;
#208967 = ORIENTED_EDGE ( 'NONE', *, *, #183862, .F. ) ;
#208968 = ORIENTED_EDGE ( 'NONE', *, *, #226538, .T. ) ;
#208969 = AXIS2_PLACEMENT_3D ( 'NONE', #65323, #50871, #243960 ) ;
#208970 = CARTESIAN_POINT ( 'NONE',  ( 18.58703555225022797, -9.406336740777579308, -40.62494464124684157 ) ) ;
#208971 = CIRCLE ( 'NONE', #104883, 0.6000000000000033085 ) ;
#208972 = DIRECTION ( 'NONE',  ( 0.000000000000000000, -0.4721928772777346239, -0.8814952561688430555 ) ) ;
#208973 = ORIENTED_EDGE ( 'NONE', *, *, #103269, .F. ) ;
#208974 = EDGE_LOOP ( 'NONE', ( #241782, #159892, #143769, #61710 ) ) ;
#208975 = CARTESIAN_POINT ( 'NONE',  ( -11.59999999999994458, 67.75000000001118394, -21.02310748452479316 ) ) ;
#208976 = FACE_OUTER_BOUND ( 'NONE', #164999, .T. ) ;
#208977 = CARTESIAN_POINT ( 'NONE',  ( -23.15000000000000213, -9.599999999988844124, -55.25000000000004974 ) ) ;
#208978 = DIRECTION ( 'NONE',  ( -1.000000000000000000, -0.000000000000000000, -0.000000000000000000 ) ) ;
#208979 = AXIS2_PLACEMENT_3D ( 'NONE', #67302, #225070, #69899 ) ;
#208980 = CYLINDRICAL_SURFACE ( 'NONE', #78842, 0.1000000000000028644 ) ;
#208982 = ORIENTED_EDGE ( 'NONE', *, *, #27910, .T. ) ;
#208981 = DIRECTION ( 'NONE',  ( 0.000000000000000000, 0.9654727137038715545, 0.2605042016806676242 ) ) ;
#208983 = CARTESIAN_POINT ( 'NONE',  ( -18.39999999999999858, 87.01908966642815813, -199.5693496768551825 ) ) ;
#208984 = DIRECTION ( 'NONE',  ( 0.000000000000000000, 1.000000000000000000, 0.000000000000000000 ) ) ;
#208985 = DIRECTION ( 'NONE',  ( -0.000000000000000000, -0.2128009952263603677, 0.9770955615653313941 ) ) ;
#208987 = AXIS2_PLACEMENT_3D ( 'NONE', #92872, #134556, #13357 ) ;
#208986 = DIRECTION ( 'NONE',  ( 0.000000000000000000, 0.000000000000000000, -1.000000000000000000 ) ) ;
#208988 = EDGE_LOOP ( 'NONE', ( #151178, #143995, #99688, #68908 ) ) ;
#208989 = CARTESIAN_POINT ( 'NONE',  ( 15.73863059295127798, 66.64859682587018597, -86.04357704768588633 ) ) ;
#208990 = DIRECTION ( 'NONE',  ( 0.000000000000000000, 0.000000000000000000, 1.000000000000000000 ) ) ;
#208991 = CIRCLE ( 'NONE', #179789, 0.1000000000000000472 ) ;
#208992 = EDGE_CURVE ( 'NONE', #184295, #49052, #131060, .T. ) ;
#208994 = DIRECTION ( 'NONE',  ( 1.000000000000000000, -0.000000000000000000, 0.000000000000000000 ) ) ;
#208993 = CARTESIAN_POINT ( 'NONE',  ( -20.94999999999999929, 77.85102823015243700, -57.86919421510181394 ) ) ;
#208995 = CARTESIAN_POINT ( 'NONE',  ( 20.95512820512820440, 43.40368376489742275, -234.8883907171572787 ) ) ;
#208996 = CARTESIAN_POINT ( 'NONE',  ( -16.85722902420154412, 9.950000000011138823, -54.23445252622962443 ) ) ;
#208998 = DIRECTION ( 'NONE',  ( 0.000000000000000000, 0.9126074666063777041, 0.4088369013363267745 ) ) ;
#208997 = CIRCLE ( 'NONE', #75738, 0.09999999999999986677 ) ;
#208999 = FACE_OUTER_BOUND ( 'NONE', #188453, .T. ) ;
#209001 = EDGE_CURVE ( 'NONE', #169538, #94099, #89641, .T. ) ;
#209000 = CARTESIAN_POINT ( 'NONE',  ( -5.899999999999938183, 64.65000000001120384, -25.92310748452479174 ) ) ;
#209002 = CARTESIAN_POINT ( 'NONE',  ( -18.40000000000000213, 33.92901942162173157, -235.0579290632217067 ) ) ;
#209003 = CIRCLE ( 'NONE', #96550, 0.09999999999999892308 ) ;
#209004 = ORIENTED_EDGE ( 'NONE', *, *, #150503, .F. ) ;
#209005 = VERTEX_POINT ( 'NONE', #24573 ) ;
#209006 = CIRCLE ( 'NONE', #246422, 11.90000000000000746 ) ;
#209007 = ORIENTED_EDGE ( 'NONE', *, *, #32463, .T. ) ;
#209008 = ADVANCED_FACE ( 'NONE', ( #45393 ), #143537, .F. ) ;
#209009 = CARTESIAN_POINT ( 'NONE',  ( 20.50589344625387156, 65.51681206853663753, -95.45011250585221774 ) ) ;
#209010 = ADVANCED_FACE ( 'NONE', ( #44117 ), #47653, .T. ) ;
#209011 = DIRECTION ( 'NONE',  ( 1.000000000000000000, -0.000000000000000000, 0.000000000000000000 ) ) ;
#209012 = ORIENTED_EDGE ( 'NONE', *, *, #35193, .T. ) ;
#209013 = AXIS2_PLACEMENT_3D ( 'NONE', #126089, #45288, #88234 ) ;
#209014 = ORIENTED_EDGE ( 'NONE', *, *, #30014, .T. ) ;
#209015 =( LENGTH_UNIT ( ) NAMED_UNIT ( * ) SI_UNIT ( .MILLI., .METRE. ) );
#209017 = VERTEX_POINT ( 'NONE', #126204 ) ;
#209016 = VECTOR ( 'NONE', #85300, 1000.000000000000000 ) ;
#209018 = DIRECTION ( 'NONE',  ( 1.000000000000000000, 0.000000000000000000, 0.000000000000000000 ) ) ;
#209019 = TOROIDAL_SURFACE ( 'NONE', #154887, 0.9750000000000019762, 0.1000000000000000056 ) ;
#209020 = EDGE_LOOP ( 'NONE', ( #139036, #124781, #222163, #63972 ) ) ;
#209021 = AXIS2_PLACEMENT_3D ( 'NONE', #158465, #219680, #220963 ) ;
#209022 = ADVANCED_FACE ( 'NONE', ( #49240 ), #60750, .T. ) ;
#209023 = DIRECTION ( 'NONE',  ( -1.836970198721029934E-16, -0.9651348961777157509, 0.2617529984165031243 ) ) ;
#209024 = ADVANCED_FACE ( 'NONE', ( #96057 ), #85245, .T. ) ;
#209025 = DIRECTION ( 'NONE',  ( -1.000000000000000000, 0.000000000000000000, 0.000000000000000000 ) ) ;
#209026 = CARTESIAN_POINT ( 'NONE',  ( -21.14250536705909411, 1.383095487280965763, -230.6548668376462672 ) ) ;
#209027 = CARTESIAN_POINT ( 'NONE',  ( -16.92989507731675758, 30.00137997040565097, -234.6972596558748023 ) ) ;
#209028 = CYLINDRICAL_SURFACE ( 'NONE', #224579, 0.1000000000000065836 ) ;
#209030 = EDGE_LOOP ( 'NONE', ( #54158, #25693, #77611, #246072 ) ) ;
#209029 = DIRECTION ( 'NONE',  ( 1.000000000000000000, 0.000000000000000000, 0.000000000000000000 ) ) ;
#209032 = CARTESIAN_POINT ( 'NONE',  ( -23.15000000000000213, 10.71906255309368383, -222.4921384173655383 ) ) ;
#209031 = CARTESIAN_POINT ( 'NONE',  ( 20.85000000106584750, 11.75000000000000355, -26.65550465647362088 ) ) ;
#209033 = CARTESIAN_POINT ( 'NONE',  ( 21.05000000000000071, -11.64999999998883595, -33.50000000000000000 ) ) ;
#209034 = ORIENTED_EDGE ( 'NONE', *, *, #211512, .F. ) ;
#209035 = CARTESIAN_POINT ( 'NONE',  ( 13.22261339317535978, 66.56344716000761252, -121.3451520117640570 ) ) ;
#209036 = CARTESIAN_POINT ( 'NONE',  ( 23.24999999999999289, 69.35000000001254250, -182.1731074845243938 ) ) ;
#209037 = CARTESIAN_POINT ( 'NONE',  ( -23.39999999999994529, 64.35000000001120668, -3.123107484524795474 ) ) ;
#209038 = ORIENTED_EDGE ( 'NONE', *, *, #163487, .T. ) ;
#209039 = CYLINDRICAL_SURFACE ( 'NONE', #175197, 0.1000000000000054040 ) ;
#209040 = EDGE_CURVE ( 'NONE', #40550, #14005, #18644, .T. ) ;
#209041 = CARTESIAN_POINT ( 'NONE',  ( -16.87401514999234209, 66.05000000001182059, -82.24308949199205188 ) ) ;
#209042 = EDGE_CURVE ( 'NONE', #122635, #104512, #234289, .T. ) ;
#209043 = AXIS2_PLACEMENT_3D ( 'NONE', #90607, #137145, #78442 ) ;
#209044 = ORIENTED_EDGE ( 'NONE', *, *, #57839, .T. ) ;
#209045 = DIRECTION ( 'NONE',  ( -1.000000000000000000, -0.000000000000000000, -0.000000000000000000 ) ) ;
#209046 = DIRECTION ( 'NONE',  ( 0.000000000000000000, -1.000000000000000000, -1.734723475976807292E-15 ) ) ;
#209047 = DIRECTION ( 'NONE',  ( 0.000000000000000000, -1.000000000000000000, 0.000000000000000000 ) ) ;
#209048 = DIRECTION ( 'NONE',  ( -1.000000000000000000, 0.000000000000000000, -0.000000000000000000 ) ) ;
#209049 = ORIENTED_EDGE ( 'NONE', *, *, #243211, .F. ) ;
#209050 = ORIENTED_EDGE ( 'NONE', *, *, #30961, .T. ) ;
#209051 = EDGE_CURVE ( 'NONE', #133509, #185627, #164403, .T. ) ;
#209052 = ADVANCED_FACE ( 'NONE', ( #152229 ), #197135, .T. ) ;
#209053 = CARTESIAN_POINT ( 'NONE',  ( -20.85000000000000142, -1.249999999988843369, -208.8004807544150481 ) ) ;
#209054 = FACE_OUTER_BOUND ( 'NONE', #167084, .T. ) ;
#209055 = DIRECTION ( 'NONE',  ( -0.000000000000000000, -6.982962677686266711E-15, 1.000000000000000000 ) ) ;
#209056 = LINE ( 'NONE', #130795, #132121 ) ;
#209058 = CARTESIAN_POINT ( 'NONE',  ( 18.49999999999999289, 10.20857864377385127, -158.6500000000000057 ) ) ;
#209057 = FACE_OUTER_BOUND ( 'NONE', #191401, .T. ) ;
#209059 = EDGE_CURVE ( 'NONE', #81005, #6871, #201793, .T. ) ;
#209060 = CARTESIAN_POINT ( 'NONE',  ( -23.39999999999994529, 83.97335046823651794, -37.38386894789040582 ) ) ;
#209061 = DIRECTION ( 'NONE',  ( 0.000000000000000000, 0.000000000000000000, -1.000000000000000000 ) ) ;
#209062 = DIRECTION ( 'NONE',  ( -1.000000000000000000, 0.000000000000000000, 0.000000000000000000 ) ) ;
#209063 = ORIENTED_EDGE ( 'NONE', *, *, #29093, .F. ) ;
#209064 = LINE ( 'NONE', #5694, #195109 ) ;
#209065 = VECTOR ( 'NONE', #109627, 999.9999999999998863 ) ;
#209067 = ORIENTED_EDGE ( 'NONE', *, *, #54675, .T. ) ;
#209066 = DIRECTION ( 'NONE',  ( 0.000000000000000000, 0.8814952561688437216, -0.4721928772777331806 ) ) ;
#209068 = CARTESIAN_POINT ( 'NONE',  ( 21.00023020733438273, 69.60913075474465472, -170.0231074845244166 ) ) ;
#209069 = DIRECTION ( 'NONE',  ( 0.000000000000000000, 0.000000000000000000, 1.000000000000000000 ) ) ;
#209070 = CARTESIAN_POINT ( 'NONE',  ( -23.25000000000000000, 3.558777552609281525, -231.8203201594644725 ) ) ;
#209071 = CARTESIAN_POINT ( 'NONE',  ( -16.93710578446424009, 66.05000000001207638, -123.6043035007249671 ) ) ;
#209072 = CARTESIAN_POINT ( 'NONE',  ( 20.94999999999999929, 11.63687328911501773, -194.1782407866753886 ) ) ;
#209074 = ORIENTED_EDGE ( 'NONE', *, *, #223839, .F. ) ;
#209073 = CARTESIAN_POINT ( 'NONE',  ( -20.00857864376270001, 63.76951449014745066, -212.8986194275075832 ) ) ;
#209075 = LINE ( 'NONE', #190833, #208935 ) ;
#209076 = CARTESIAN_POINT ( 'NONE',  ( -16.97048361161166596, 51.17066711795111900, -232.1472552184704341 ) ) ;
#209077 = ADVANCED_FACE ( 'NONE', ( #54374 ), #197689, .T. ) ;
#209078 = DIRECTION ( 'NONE',  ( 1.000000000000000000, 0.000000000000000000, 0.000000000000000000 ) ) ;
#209079 = CARTESIAN_POINT ( 'NONE',  ( 18.79999999999999716, -10.84999999999999076, 33.00000000000000000 ) ) ;
#209080 = ORIENTED_EDGE ( 'NONE', *, *, #230940, .T. ) ;
#209081 = DIRECTION ( 'NONE',  ( -1.000000000000000000, -0.000000000000000000, -0.000000000000000000 ) ) ;
#209082 = EDGE_LOOP ( 'NONE', ( #106811, #28649, #223294, #247703 ) ) ;
#209083 = ADVANCED_FACE ( 'NONE', ( #248737 ), #170535, .F. ) ;
#209084 = CIRCLE ( 'NONE', #79869, 0.1000000000000052097 ) ;
#209085 = ORIENTED_EDGE ( 'NONE', *, *, #31454, .F. ) ;
#209087 = DIRECTION ( 'NONE',  ( 0.000000000000000000, 0.000000000000000000, 1.000000000000000000 ) ) ;
#209086 = B_SPLINE_CURVE_WITH_KNOTS ( 'NONE', 3,
 ( #7153, #125822, #4583, #144089, #167557, #185802, #86673, #45012, #222331, #244488, #63281, #106244, #104945, #247047, #142798, #243199, #65851, #227488, #224915, #245786, #123265, #202797, #68435, #223625, #67143, #84081 ),
 .UNSPECIFIED., .F., .F.,
 ( 4, 2, 2, 2, 2, 2, 2, 2, 2, 2, 2, 2, 4 ),
 ( 0.005476422646581343041, 0.006160811967703572201, 0.006845201288825802227, 0.007187395949386904230, 0.007529590609948006233, 0.007871785270509109103, 0.008213979931070210239, 0.008556174591631313109, 0.008898369252192414244, 0.009240563912753517115, 0.009582758573314618250, 0.01026714789443682399, 0.01095153721555902800 ),
 .UNSPECIFIED. ) ;
#209088 = EDGE_LOOP ( 'NONE', ( #53405, #148652, #59174, #233144 ) ) ;
#209089 = DIRECTION ( 'NONE',  ( 0.000000000000000000, 0.000000000000000000, -1.000000000000000000 ) ) ;
#209090 = CARTESIAN_POINT ( 'NONE',  ( 21.05000000000000071, 76.00000000001192291, -98.72310748452429152 ) ) ;
#209091 = EDGE_CURVE ( 'NONE', #207953, #117519, #93655, .T. ) ;
#209092 = DIRECTION ( 'NONE',  ( -0.000000000000000000, -6.982962677686266711E-15, 1.000000000000000000 ) ) ;
#209093 = VERTEX_POINT ( 'NONE', #11417 ) ;
#209094 = CARTESIAN_POINT ( 'NONE',  ( -16.85697194749127803, 9.908543714123608126, -12.93500426761395872 ) ) ;
#209095 = CARTESIAN_POINT ( 'NONE',  ( 23.24999999999999645, 76.00000000001190870, -103.0231074845243029 ) ) ;
#209096 = VECTOR ( 'NONE', #118171, 1000.000000000000000 ) ;
#209097 = CARTESIAN_POINT ( 'NONE',  ( -23.15000000000000213, 2.000000000011154189, -80.22462192276213955 ) ) ;
#209098 = CARTESIAN_POINT ( 'NONE',  ( -21.64999999999999858, 68.65000000001222702, -148.8731074845244109 ) ) ;
#209099 = SPHERICAL_SURFACE ( 'NONE', #82376, 0.1000000000000000056 ) ;
#209100 = ORIENTED_EDGE ( 'NONE', *, *, #66168, .T. ) ;
#209102 = ORIENTED_EDGE ( 'NONE', *, *, #65515, .F. ) ;
#209101 = CARTESIAN_POINT ( 'NONE',  ( -22.47071067811865674, 7.720074744509219045, -167.4009075452973434 ) ) ;
#209103 = VERTEX_POINT ( 'NONE', #15274 ) ;
#209104 = DIRECTION ( 'NONE',  ( 0.000000000000000000, -6.454785026890406770E-15, 1.000000000000000000 ) ) ;
#209105 = ORIENTED_EDGE ( 'NONE', *, *, #174402, .F. ) ;
#209106 = DIRECTION ( 'NONE',  ( -0.8660254037844653530, 0.000000000000000000, -0.4999999999999539257 ) ) ;
#209107 = CARTESIAN_POINT ( 'NONE',  ( 23.24999999999999289, 11.65000000000000746, -12.15000000000000036 ) ) ;
#209108 = ORIENTED_EDGE ( 'NONE', *, *, #95944, .F. ) ;
#209109 = DIRECTION ( 'NONE',  ( 0.000000000000000000, 0.000000000000000000, 1.000000000000000000 ) ) ;
#209110 = DIRECTION ( 'NONE',  ( 0.000000000000000000, -0.2617529984165031243, -0.9651348961777157509 ) ) ;
#209111 = DIRECTION ( 'NONE',  ( -1.000000000000000000, 0.000000000000000000, -0.000000000000000000 ) ) ;
#209112 = ORIENTED_EDGE ( 'NONE', *, *, #154989, .T. ) ;
#209114 = VERTEX_POINT ( 'NONE', #75256 ) ;
#209113 = DIRECTION ( 'NONE',  ( 0.000000000000000000, 0.2128009952263602844, -0.9770955615653315052 ) ) ;
#209115 = TOROIDAL_SURFACE ( 'NONE', #966, 7.800000000000000711, 0.1000000000000000056 ) ;
#209116 = AXIS2_PLACEMENT_3D ( 'NONE', #94265, #138500, #135952 ) ;
#209117 = DIRECTION ( 'NONE',  ( 1.000000000000000000, 0.000000000000000000, 0.000000000000000000 ) ) ;
#209118 = DIRECTION ( 'NONE',  ( -1.000000000000000000, -3.265361837132813093E-16, 0.000000000000000000 ) ) ;
#209119 = AXIS2_PLACEMENT_3D ( 'NONE', #147829, #95541, #132111 ) ;
#209120 = VERTEX_POINT ( 'NONE', #212187 ) ;
#209121 = CARTESIAN_POINT ( 'NONE',  ( -5.899999999999938183, 64.35000000001120668, -25.92310748452479174 ) ) ;
#209122 = CARTESIAN_POINT ( 'NONE',  ( -15.39946565075090312, 66.61046543766534000, -120.8482981801344067 ) ) ;
#209123 = CARTESIAN_POINT ( 'NONE',  ( -20.94999675878240808, 18.34775554461856828, -236.8759397601555179 ) ) ;
#209124 = ORIENTED_EDGE ( 'NONE', *, *, #43999, .T. ) ;
#209125 = CARTESIAN_POINT ( 'NONE',  ( 20.94999999999999929, 23.68770167995059239, -252.8127582590406348 ) ) ;
#209126 = EDGE_CURVE ( 'NONE', #76756, #81287, #153533, .T. ) ;
#209127 = LINE ( 'NONE', #30521, #243121 ) ;
#209128 = VECTOR ( 'NONE', #206225, 1000.000000000000000 ) ;
#209129 = EDGE_CURVE ( 'NONE', #217199, #214190, #111795, .T. ) ;
#209130 = ORIENTED_EDGE ( 'NONE', *, *, #41732, .T. ) ;
#209131 = EDGE_CURVE ( 'NONE', #219794, #19019, #154792, .T. ) ;
#209132 = CIRCLE ( 'NONE', #255453, 0.09999999999999031886 ) ;
#209133 = VERTEX_POINT ( 'NONE', #135183 ) ;
#209134 = DIRECTION ( 'NONE',  ( -1.000000000000000000, 0.000000000000000000, 0.000000000000000000 ) ) ;
#209135 = VERTEX_POINT ( 'NONE', #213447 ) ;
#209136 = DIRECTION ( 'NONE',  ( 0.000000000000000000, 7.086529944415886769E-15, -1.000000000000000000 ) ) ;
#209137 = EDGE_CURVE ( 'NONE', #86042, #225349, #195204, .T. ) ;
#209138 = DIRECTION ( 'NONE',  ( 1.000000000000000000, -0.000000000000000000, 0.000000000000000000 ) ) ;
#209139 = VECTOR ( 'NONE', #27440, 1000.000000000000000 ) ;
#209141 = ORIENTED_EDGE ( 'NONE', *, *, #21353, .T. ) ;
#209140 = DIRECTION ( 'NONE',  ( 0.000000000000000000, -0.000000000000000000, 1.000000000000000000 ) ) ;
#209142 = DIRECTION ( 'NONE',  ( 1.000000000000000000, -0.000000000000000000, -0.000000000000000000 ) ) ;
#209143 = CARTESIAN_POINT ( 'NONE',  ( 21.05933563467872460, 65.27547528793024867, -57.32945973556844876 ) ) ;
#209144 = CARTESIAN_POINT ( 'NONE',  ( -21.14999999999999858, 1.115600667400684642E-11, -67.00000000000004263 ) ) ;
#209145 = CARTESIAN_POINT ( 'NONE',  ( -20.54999999999999716, -8.999999999988846255, -110.3939691226524786 ) ) ;
#209146 = LINE ( 'NONE', #110050, #247657 ) ;
#209147 = VECTOR ( 'NONE', #213827, 1000.000000000000000 ) ;
#209148 = DIRECTION ( 'NONE',  ( -1.000000000000000000, 0.000000000000000000, 0.000000000000000000 ) ) ;
#209149 = CARTESIAN_POINT ( 'NONE',  ( -18.49719636458538830, -9.446365359216949642, -107.5716138698836062 ) ) ;
#209151 = VERTEX_POINT ( 'NONE', #193906 ) ;
#209150 = DIRECTION ( 'NONE',  ( 1.000000000000000000, 0.000000000000000000, 0.000000000000000000 ) ) ;
#209152 = CIRCLE ( 'NONE', #100778, 0.1999999999999893807 ) ;
#209153 = AXIS2_PLACEMENT_3D ( 'NONE', #51068, #113647, #172392 ) ;
#209154 = AXIS2_PLACEMENT_3D ( 'NONE', #163391, #29051, #31608 ) ;
#209155 = CIRCLE ( 'NONE', #63406, 0.1000000000000141609 ) ;
#209156 = FACE_OUTER_BOUND ( 'NONE', #257178, .T. ) ;
#209157 = CARTESIAN_POINT ( 'NONE',  ( 20.94999999999999929, -11.64999999999999147, -33.50000000000000000 ) ) ;
#209158 = EDGE_CURVE ( 'NONE', #208884, #75744, #39526, .T. ) ;
#209159 = EDGE_CURVE ( 'NONE', #20493, #178795, #209607, .T. ) ;
#209160 = CARTESIAN_POINT ( 'NONE',  ( -23.15000000000000213, 1.115600667400684642E-11, -100.5000000000000284 ) ) ;
#209161 = CARTESIAN_POINT ( 'NONE',  ( -20.54999999999999716, 84.66355140188075268, -59.99900636645695329 ) ) ;
#209162 = B_SPLINE_CURVE_WITH_KNOTS ( 'NONE', 3,
 ( #128894, #230561, #247549, #130155, #209707, #31106, #171899, #12810 ),
 .UNSPECIFIED., .F., .F.,
 ( 4, 2, 2, 4 ),
 ( 0.000000000000000000, 0.0001049670497870067789, 0.0002099340995740135577, 0.0004198681991479925294 ),
 .UNSPECIFIED. ) ;
#209163 = AXIS2_PLACEMENT_3D ( 'NONE', #102488, #43842, #123378 ) ;
#209164 = ORIENTED_EDGE ( 'NONE', *, *, #227514, .T. ) ;
#209165 = CARTESIAN_POINT ( 'NONE',  ( 20.94999999999999929, 70.60000000001149090, -45.91707660717680284 ) ) ;
#209166 = TOROIDAL_SURFACE ( 'NONE', #167506, 0.2000000000000000111, 0.1000000000000000056 ) ;
#209167 = LINE ( 'NONE', #164912, #231565 ) ;
#209169 = EDGE_CURVE ( 'NONE', #198528, #44180, #10286, .T. ) ;
#209168 = DIRECTION ( 'NONE',  ( 0.000000000000000000, 0.1298341882520022694, 0.9915357197604852679 ) ) ;
#209170 = VECTOR ( 'NONE', #238007, 1000.000000000000000 ) ;
#209171 = VECTOR ( 'NONE', #207372, 1000.000000000000000 ) ;
#209172 = ORIENTED_EDGE ( 'NONE', *, *, #112642, .F. ) ;
#209173 = VECTOR ( 'NONE', #228643, 1000.000000000000000 ) ;
#209174 = FACE_OUTER_BOUND ( 'NONE', #127653, .T. ) ;
#209175 = VECTOR ( 'NONE', #177968, 1000.000000000000000 ) ;
#209176 = DIRECTION ( 'NONE',  ( 0.000000000000000000, 0.000000000000000000, -1.000000000000000000 ) ) ;
#209177 = ORIENTED_EDGE ( 'NONE', *, *, #96771, .F. ) ;
#209178 = CARTESIAN_POINT ( 'NONE',  ( -21.05000000000000071, 6.299230910103438497, -66.90156249999972715 ) ) ;
#209179 = VERTEX_POINT ( 'NONE', #32279 ) ;
#209181 = AXIS2_PLACEMENT_3D ( 'NONE', #47830, #248620, #226466 ) ;
#209180 = LINE ( 'NONE', #48823, #225517 ) ;
#209183 = ORIENTED_EDGE ( 'NONE', *, *, #26787, .F. ) ;
#209182 = LINE ( 'NONE', #150508, #234702 ) ;
#209184 = DIRECTION ( 'NONE',  ( 1.000000000000000000, 0.000000000000000000, 0.000000000000000000 ) ) ;
#209185 = ADVANCED_FACE ( 'NONE', ( #39982 ), #176881, .T. ) ;
#209186 = ORIENTED_EDGE ( 'NONE', *, *, #14294, .T. ) ;
#209187 = DIRECTION ( 'NONE',  ( 0.000000000000000000, -0.4088369013363280513, 0.9126074666063769270 ) ) ;
#209188 = ORIENTED_EDGE ( 'NONE', *, *, #187203, .F. ) ;
#209189 = ORIENTED_EDGE ( 'NONE', *, *, #6282, .F. ) ;
#209190 = CARTESIAN_POINT ( 'NONE',  ( 18.51997666896875572, 85.39233213153090674, -129.3797012970411231 ) ) ;
#209191 = ORIENTED_EDGE ( 'NONE', *, *, #17523, .T. ) ;
#209192 = FACE_OUTER_BOUND ( 'NONE', #20250, .T. ) ;
#209194 = ORIENTED_EDGE ( 'NONE', *, *, #108665, .T. ) ;
#209193 = AXIS2_PLACEMENT_3D ( 'NONE', #55423, #234084, #54165 ) ;
#209195 = AXIS2_PLACEMENT_3D ( 'NONE', #124684, #47689, #166405 ) ;
#209196 = EDGE_CURVE ( 'NONE', #181442, #133901, #72843, .T. ) ;
#209197 = ORIENTED_EDGE ( 'NONE', *, *, #149542, .T. ) ;
#209198 = CARTESIAN_POINT ( 'NONE',  ( -18.69999999999999929, -9.849999999999942801, -15.00000000000000178 ) ) ;
#209199 = CARTESIAN_POINT ( 'NONE',  ( -23.15000000000000213, 8.555687629545136730, -220.7824469969188783 ) ) ;
#209200 = CARTESIAN_POINT ( 'NONE',  ( 21.14999999999999503, 87.65000000001163016, -66.62310748452424036 ) ) ;
#209201 = ORIENTED_EDGE ( 'NONE', *, *, #29941, .T. ) ;
#209202 = EDGE_CURVE ( 'NONE', #71875, #154018, #255914, .T. ) ;
#209204 = EDGE_CURVE ( 'NONE', #110542, #55978, #77771, .T. ) ;
#209203 = CARTESIAN_POINT ( 'NONE',  ( -16.78805706634180694, 9.948252493071178648, -20.84415320803185523 ) ) ;
#209205 = DIRECTION ( 'NONE',  ( 0.000000000000000000, 0.000000000000000000, -1.000000000000000000 ) ) ;
#209206 = ORIENTED_EDGE ( 'NONE', *, *, #186460, .F. ) ;
#209207 = CARTESIAN_POINT ( 'NONE',  ( -20.54999999999999716, 76.00000000001170974, -69.52310748452431710 ) ) ;
#209208 = DIRECTION ( 'NONE',  ( -0.000000000000000000, 0.1350103645451876666, 0.9908441862701600211 ) ) ;
#209209 = LINE ( 'NONE', #113961, #220251 ) ;
#209210 = CARTESIAN_POINT ( 'NONE',  ( -20.54999999999999716, -11.75000000000000000, -21.15000000000000213 ) ) ;
#209211 = ORIENTED_EDGE ( 'NONE', *, *, #49664, .F. ) ;
#209213 = CARTESIAN_POINT ( 'NONE',  ( -18.59999999999999787, 5.900000000011102586, -43.71909976465641989 ) ) ;
#209212 = AXIS2_PLACEMENT_3D ( 'NONE', #53453, #211241, #213806 ) ;
#209214 = VERTEX_POINT ( 'NONE', #81603 ) ;
#209215 = CARTESIAN_POINT ( 'NONE',  ( -18.34374000495060386, 64.52683809664961245, -127.2731074845243882 ) ) ;
#209216 = ORIENTED_EDGE ( 'NONE', *, *, #74804, .F. ) ;
#209217 = EDGE_CURVE ( 'NONE', #86372, #52350, #251863, .T. ) ;
#209218 = EDGE_CURVE ( 'NONE', #214434, #246557, #98592, .T. ) ;
#209219 = CARTESIAN_POINT ( 'NONE',  ( -23.15000000000000213, 1.115600667400684642E-11, -46.37500000000000000 ) ) ;
#209220 = CARTESIAN_POINT ( 'NONE',  ( 11.60000000000000320, -8.279289321881350361, 11.02928932188135036 ) ) ;
#209221 = EDGE_LOOP ( 'NONE', ( #74264, #132443, #122075, #73214 ) ) ;
#209222 = ORIENTED_EDGE ( 'NONE', *, *, #187038, .T. ) ;
#209224 = EDGE_LOOP ( 'NONE', ( #105596, #163013, #44407, #221917 ) ) ;
#209223 = FACE_OUTER_BOUND ( 'NONE', #207932, .T. ) ;
#209225 = CARTESIAN_POINT ( 'NONE',  ( -23.15000000000000213, 23.42819724844703444, -229.2476443247244902 ) ) ;
#209226 = ORIENTED_EDGE ( 'NONE', *, *, #207716, .T. ) ;
#209227 = EDGE_CURVE ( 'NONE', #14872, #257751, #58206, .T. ) ;
#209228 = CARTESIAN_POINT ( 'NONE',  ( 22.50000000000000000, 7.591056067193225232, -199.2444047917219052 ) ) ;
#209229 = PRESENTATION_STYLE_ASSIGNMENT (( #90558 ) ) ;
#209230 = VERTEX_POINT ( 'NONE', #201581 ) ;
#209231 = EDGE_CURVE ( 'NONE', #89290, #60411, #180963, .T. ) ;
#209232 = FACE_OUTER_BOUND ( 'NONE', #186091, .T. ) ;
#209233 = ADVANCED_FACE ( 'NONE', ( #256362 ), #168539, .F. ) ;
#209234 = EDGE_CURVE ( 'NONE', #53701, #200289, #97331, .T. ) ;
#209235 = ORIENTED_EDGE ( 'NONE', *, *, #56358, .F. ) ;
#209236 = CIRCLE ( 'NONE', #250918, 11.80000000000000426 ) ;
#209237 = LINE ( 'NONE', #11045, #168271 ) ;
#209238 = EDGE_CURVE ( 'NONE', #143070, #135750, #255536, .T. ) ;
#209239 = CARTESIAN_POINT ( 'NONE',  ( -20.54999999999999361, 64.35000000001180354, -81.67310748452439384 ) ) ;
#209240 = DIRECTION ( 'NONE',  ( -1.000000000000000000, -0.000000000000000000, 0.000000000000000000 ) ) ;
#209242 = EDGE_LOOP ( 'NONE', ( #246976, #193821, #101988, #25031 ) ) ;
#209241 = LINE ( 'NONE', #249668, #30907 ) ;
#209243 = EDGE_CURVE ( 'NONE', #99799, #205134, #180578, .T. ) ;
#209244 = DIRECTION ( 'NONE',  ( 1.000000000000000000, 0.000000000000000000, 0.000000000000000000 ) ) ;
#209245 = LINE ( 'NONE', #232687, #239990 ) ;
#209246 = EDGE_CURVE ( 'NONE', #61013, #48194, #130678, .T. ) ;
#209247 = CARTESIAN_POINT ( 'NONE',  ( 18.49999999999999289, 65.79142135624927334, -111.8731074845243683 ) ) ;
#209249 = CARTESIAN_POINT ( 'NONE',  ( 21.07928932188134397, 69.67148334361864670, -103.1220026301787414 ) ) ;
#209248 = CARTESIAN_POINT ( 'NONE',  ( -18.59999999999999787, -9.480686695267820596, -140.9411151687578752 ) ) ;
#209250 = DIRECTION ( 'NONE',  ( -0.000000000000000000, -0.8814952561688430555, 0.4721928772777344574 ) ) ;
#209252 = EDGE_CURVE ( 'NONE', #252130, #129596, #143134, .T. ) ;
#209251 = CARTESIAN_POINT ( 'NONE',  ( 21.30000000000002558, 76.00000000001195133, -103.0231074845243171 ) ) ;
#209253 = AXIS2_PLACEMENT_3D ( 'NONE', #23068, #98682, #161287 ) ;
#209254 = DIRECTION ( 'NONE',  ( 1.000000000000000000, 0.000000000000000000, 0.000000000000000000 ) ) ;
#209255 = DIRECTION ( 'NONE',  ( -1.836970198721029441E-16, 0.4721928772777346239, 0.8814952561688430555 ) ) ;
#209256 = AXIS2_PLACEMENT_3D ( 'NONE', #167149, #125429, #144964 ) ;
#209257 = ORIENTED_EDGE ( 'NONE', *, *, #225868, .T. ) ;
#209259 = ORIENTED_EDGE ( 'NONE', *, *, #50934, .F. ) ;
#209258 = AXIS2_PLACEMENT_3D ( 'NONE', #149693, #33622, #50536 ) ;
#209260 =( BOUNDED_CURVE ( )  B_SPLINE_CURVE ( 3, ( #168437, #31470, #186675, #133111 ),
 .UNSPECIFIED., .F., .F. ) 
 B_SPLINE_CURVE_WITH_KNOTS ( ( 4, 4 ),
 ( 0.000000000000000000, 1.570796326794916320 ),
 .UNSPECIFIED. ) 
 CURVE ( )  GEOMETRIC_REPRESENTATION_ITEM ( )  RATIONAL_B_SPLINE_CURVE ( ( 1.000000000000000000, 0.8047378541243603856, 0.8047378541243603856, 1.000000000000000000 ) ) 
 REPRESENTATION_ITEM ( '' )  );
#209261 = ORIENTED_EDGE ( 'NONE', *, *, #77999, .T. ) ;
#209262 = EDGE_CURVE ( 'NONE', #68386, #55997, #157367, .T. ) ;
#209263 = DIRECTION ( 'NONE',  ( 0.000000000000000000, 0.000000000000000000, 1.000000000000000000 ) ) ;
#209264 = FACE_BOUND ( 'NONE', #66296, .T. ) ;
#209265 = ORIENTED_EDGE ( 'NONE', *, *, #43173, .F. ) ;
#209266 = AXIS2_PLACEMENT_3D ( 'NONE', #76736, #139258, #18050 ) ;
#209267 = CARTESIAN_POINT ( 'NONE',  ( 18.39999999999999503, 20.94763808724815846, -234.7254930126486556 ) ) ;
#209268 = B_SPLINE_CURVE_WITH_KNOTS ( 'NONE', 3,
 ( #40177, #156277, #117122, #18004, #196642, #59678, #139216 ),
 .UNSPECIFIED., .F., .F.,
 ( 4, 3, 4 ),
 ( 0.000000000000000000, 1.860045280646152724E-05, 5.251155757305309607E-05 ),
 .UNSPECIFIED. ) ;
#209269 = CARTESIAN_POINT ( 'NONE',  ( 20.90851465518105812, 10.32532329027886320, -206.5699343018359002 ) ) ;
#209270 = DIRECTION ( 'NONE',  ( 1.000000000000000000, -2.952720810173289112E-16, -2.061873921506763405E-30 ) ) ;
#209271 = ORIENTED_EDGE ( 'NONE', *, *, #26652, .T. ) ;
#209272 = VERTEX_POINT ( 'NONE', #236858 ) ;
#209273 = CARTESIAN_POINT ( 'NONE',  ( 18.39999999999999503, 70.35000000001261355, -190.8731074845244109 ) ) ;
#209274 = FACE_OUTER_BOUND ( 'NONE', #170356, .T. ) ;
#209275 = VERTEX_POINT ( 'NONE', #217278 ) ;
#209276 = VECTOR ( 'NONE', #77010, 1000.000000000000114 ) ;
#209277 = DIRECTION ( 'NONE',  ( 0.000000000000000000, 0.1568667991644355497, -0.9876197685951332295 ) ) ;
#209278 = ORIENTED_EDGE ( 'NONE', *, *, #164841, .F. ) ;
#209279 = DIRECTION ( 'NONE',  ( 0.000000000000000000, -1.000000000000000000, 0.000000000000000000 ) ) ;
#209280 = DIRECTION ( 'NONE',  ( 1.000000000000000000, 0.000000000000000000, 0.000000000000000000 ) ) ;
#209282 = VERTEX_POINT ( 'NONE', #197735 ) ;
#209281 = CARTESIAN_POINT ( 'NONE',  ( -21.05000000000000071, 5.850000000011108092, -144.1324972242779836 ) ) ;
#209283 = AXIS2_PLACEMENT_3D ( 'NONE', #13730, #172857, #252326 ) ;
#209284 = CARTESIAN_POINT ( 'NONE',  ( -21.70464131381649509, 33.75808023539804736, -243.0758859948899726 ) ) ;
#209286 = CARTESIAN_POINT ( 'NONE',  ( -23.15000000000000213, 25.94586868676353575, -241.5435999122864530 ) ) ;
#209285 = AXIS2_PLACEMENT_3D ( 'NONE', #20600, #173294, #178399 ) ;
#209287 = LINE ( 'NONE', #74947, #161037 ) ;
#209288 = DIRECTION ( 'NONE',  ( 1.000000000000000000, -7.510212038922846022E-17, 1.676432719286211941E-16 ) ) ;
#209289 = VECTOR ( 'NONE', #141915, 1000.000000000000000 ) ;
#209290 = EDGE_CURVE ( 'NONE', #89936, #147651, #88971, .T. ) ;
#209292 = CARTESIAN_POINT ( 'NONE',  ( 20.94999999999999574, 87.48912529308871910, -200.4231074845242802 ) ) ;
#209291 = DIRECTION ( 'NONE',  ( 1.000000000000000000, -0.000000000000000000, 0.000000000000000000 ) ) ;
#209293 = CARTESIAN_POINT ( 'NONE',  ( -15.75000000000000355, 9.850000000011133849, -50.25000000000000711 ) ) ;
#209294 = CARTESIAN_POINT ( 'NONE',  ( -18.50000000000000000, 85.42129027953541254, -163.1992253054984587 ) ) ;
#209295 = EDGE_CURVE ( 'NONE', #95688, #228463, #122313, .T. ) ;
#209296 = CARTESIAN_POINT ( 'NONE',  ( -22.50000000000000000, 68.20922040163927136, -203.6231074845244109 ) ) ;
#209297 = LINE ( 'NONE', #50210, #105121 ) ;
#209298 = ORIENTED_EDGE ( 'NONE', *, *, #140664, .F. ) ;
#209299 = CARTESIAN_POINT ( 'NONE',  ( -18.41431012584569160, 11.48747202921932242, -76.22676398689837640 ) ) ;
#209300 = EDGE_LOOP ( 'NONE', ( #39322, #1376, #19081, #14691 ) ) ;
#209301 = DIRECTION ( 'NONE',  ( 0.000000000000000000, -0.2128009952263603954, 0.9770955615653315052 ) ) ;
#209302 = ORIENTED_EDGE ( 'NONE', *, *, #193040, .T. ) ;
#209303 = LINE ( 'NONE', #88048, #156890 ) ;
#209304 = LINE ( 'NONE', #110200, #94222 ) ;
#209305 = ORIENTED_EDGE ( 'NONE', *, *, #27877, .F. ) ;
#209306 = CARTESIAN_POINT ( 'NONE',  ( 23.24999999999999645, 76.00000000001190870, -103.0231074845243029 ) ) ;
#209307 = EDGE_CURVE ( 'NONE', #235134, #50332, #234746, .T. ) ;
#209308 = AXIS2_PLACEMENT_3D ( 'NONE', #218535, #55599, #56885 ) ;
#209309 = VECTOR ( 'NONE', #71714, 1000.000000000000000 ) ;
#209310 = VERTEX_POINT ( 'NONE', #101151 ) ;
#209311 = ORIENTED_EDGE ( 'NONE', *, *, #89630, .T. ) ;
#209312 = ORIENTED_EDGE ( 'NONE', *, *, #22922, .T. ) ;
#209313 = CARTESIAN_POINT ( 'NONE',  ( 20.94999999999999929, 84.66355140188105111, -93.49900636645693908 ) ) ;
#209314 = CARTESIAN_POINT ( 'NONE',  ( -22.39999999999999858, 7.790779598384560245, -33.39999999999999858 ) ) ;
#209315 = CARTESIAN_POINT ( 'NONE',  ( 18.59999999999999787, 70.10000000001213039, -126.3040077198679398 ) ) ;
#209316 = CARTESIAN_POINT ( 'NONE',  ( 18.59999999999999076, 70.08587962373171365, -198.1273832143211848 ) ) ;
#209317 = DIRECTION ( 'NONE',  ( 1.000000000000000000, 2.952720810173289112E-16, -0.000000000000000000 ) ) ;
#209318 = AXIS2_PLACEMENT_3D ( 'NONE', #228824, #90570, #167579 ) ;
#209320 = CARTESIAN_POINT ( 'NONE',  ( -23.25000000000000000, -1.249999999988843369, -141.8004807544151333 ) ) ;
#209319 = DIRECTION ( 'NONE',  ( -1.000000000000000000, -0.000000000000000000, -0.000000000000000000 ) ) ;
#209321 = CARTESIAN_POINT ( 'NONE',  ( 18.49999999999999289, 10.25000000001115730, -58.14999999999999858 ) ) ;
#209323 = ORIENTED_EDGE ( 'NONE', *, *, #78590, .T. ) ;
#209322 = CARTESIAN_POINT ( 'NONE',  ( -16.77683809663752257, 23.65833333334447985, -50.25000000000000000 ) ) ;
#209325 = DIRECTION ( 'NONE',  ( 0.000000000000000000, 0.9916376685811618685, -0.1290532225514649800 ) ) ;
#209324 = LINE ( 'NONE', #90657, #163400 ) ;
#209326 = CARTESIAN_POINT ( 'NONE',  ( 18.59999999999998366, 43.35377423437995503, -245.1717807829448930 ) ) ;
#209327 =( BOUNDED_SURFACE ( )  B_SPLINE_SURFACE ( 3, 2, ( 
 ( #141269, #64301, #21350 ),
 ( #20054, #181689, #100810 ),
 ( #143820, #42182, #138662 ),
 ( #223360, #59126, #3021 ),
 ( #43454, #121727, #162138 ),
 ( #182981, #39637, #78704 ) ),
 .UNSPECIFIED., .F., .F., .F. ) 
 B_SPLINE_SURFACE_WITH_KNOTS ( ( 4, 2, 4 ),
 ( 3, 3 ),
 ( 6.719893378901192380E-05, 0.0002757154632485820170, 0.0004842319927081520695 ),
 ( 0.000000000000000000, 1.000000000000000000 ),
 .UNSPECIFIED. ) 
 GEOMETRIC_REPRESENTATION_ITEM ( )  RATIONAL_B_SPLINE_SURFACE ( (
 ( 1.000000000000000000, 0.7250110520819756932, 1.000000000000000000),
 ( 1.000000000000000000, 0.7277932058358641543, 1.000000000000000000),
 ( 1.000000000000000000, 0.7278452872618367264, 1.000000000000000000),
 ( 1.000000000000000000, 0.7221445671548437639, 1.000000000000000000),
 ( 1.000000000000000000, 0.7163662143780165081, 1.000000000000000000),
 ( 1.000000000000000000, 0.7071067811865475727, 1.000000000000000000) ) ) 
 REPRESENTATION_ITEM ( '' )  SURFACE ( )  );
#209328 = VERTEX_POINT ( 'NONE', #142871 ) ;
#209329 = CARTESIAN_POINT ( 'NONE',  ( 20.95203847575071521, 10.50106053928516303, -74.56707134862361386 ) ) ;
#209330 = CIRCLE ( 'NONE', #96871, 0.09999999999999938105 ) ;
#209331 = FACE_OUTER_BOUND ( 'NONE', #78859, .T. ) ;
#209332 = CARTESIAN_POINT ( 'NONE',  ( 20.04999999999999716, 67.25000000001186606, -93.77310748452437394 ) ) ;
#209333 = ORIENTED_EDGE ( 'NONE', *, *, #234152, .T. ) ;
#209334 = AXIS2_PLACEMENT_3D ( 'NONE', #61011, #160149, #84374 ) ;
#209336 = CARTESIAN_POINT ( 'NONE',  ( -16.85939591225059431, 61.06373154741859111, -220.7541896542538780 ) ) ;
#209335 = AXIS2_PLACEMENT_3D ( 'NONE', #146672, #29369, #68462 ) ;
#209337 = VECTOR ( 'NONE', #99225, 1000.000000000000000 ) ;
#209338 = PLANE ( 'NONE',  #144357 ) ;
#209339 = CARTESIAN_POINT ( 'NONE',  ( 12.93225390519045170, 66.58234804117083172, -87.66432009208394049 ) ) ;
#209340 = VECTOR ( 'NONE', #77876, 1000.000000000000000 ) ;
#209341 = ORIENTED_EDGE ( 'NONE', *, *, #56813, .F. ) ;
#209342 = ORIENTED_EDGE ( 'NONE', *, *, #39602, .F. ) ;
#209343 = TOROIDAL_SURFACE ( 'NONE', #96880, 12.97499999999999787, 0.1000000000000000056 ) ;
#209344 = CARTESIAN_POINT ( 'NONE',  ( -21.05000000000000071, -1.360870587180885716, -75.07299792709100927 ) ) ;
#209345 = CARTESIAN_POINT ( 'NONE',  ( 23.14999999999999858, -3.899999999988843502, -167.5000000000000284 ) ) ;
#209346 = CARTESIAN_POINT ( 'NONE',  ( 21.72449340488910607, 10.28395627749112151, -9.250000000000001776 ) ) ;
#209347 = DIRECTION ( 'NONE',  ( 0.000000000000000000, -6.938893903907222067E-15, 1.000000000000000000 ) ) ;
#209348 = ORIENTED_EDGE ( 'NONE', *, *, #107306, .T. ) ;
#209349 = AXIS2_PLACEMENT_3D ( 'NONE', #141343, #181759, #22708 ) ;
#209350 = EDGE_CURVE ( 'NONE', #56882, #186477, #123344, .T. ) ;
#209352 = CIRCLE ( 'NONE', #88535, 0.1000000000000028644 ) ;
#209351 = CARTESIAN_POINT ( 'NONE',  ( 20.94999999999999929, 76.00000000001190870, -103.0231074845243029 ) ) ;
#209353 = FACE_OUTER_BOUND ( 'NONE', #223453, .T. ) ;
#209354 = EDGE_CURVE ( 'NONE', #3192, #95067, #238845, .T. ) ;
#209355 = CARTESIAN_POINT ( 'NONE',  ( 18.59999999999999076, 77.16412189325305349, -95.10825939895268277 ) ) ;
#209356 = DIRECTION ( 'NONE',  ( 1.000000000000000000, 0.000000000000000000, 0.000000000000000000 ) ) ;
#209357 = EDGE_LOOP ( 'NONE', ( #24933, #187689 ) ) ;
#209358 = FACE_OUTER_BOUND ( 'NONE', #241896, .T. ) ;
#209359 = CIRCLE ( 'NONE', #5335, 0.1000000000000028644 ) ;
#209361 =( BOUNDED_CURVE ( )  B_SPLINE_CURVE ( 3, ( #127525, #89659, #147065, #205765 ),
 .UNSPECIFIED., .F., .F. ) 
 B_SPLINE_CURVE_WITH_KNOTS ( ( 4, 4 ),
 ( 3.141592653589793116, 4.712388980384647041 ),
 .UNSPECIFIED. ) 
 CURVE ( )  GEOMETRIC_REPRESENTATION_ITEM ( )  RATIONAL_B_SPLINE_CURVE ( ( 1.000000000000000000, 0.8047378541243750405, 0.8047378541243750405, 1.000000000000000000 ) ) 
 REPRESENTATION_ITEM ( '' )  );
#209360 = CIRCLE ( 'NONE', #180331, 11.75000000000001066 ) ;
#209362 = AXIS2_PLACEMENT_3D ( 'NONE', #22228, #65, #198272 ) ;
#209363 = ADVANCED_FACE ( 'NONE', ( #206723 ), #222401, .F. ) ;
#209365 = ORIENTED_EDGE ( 'NONE', *, *, #140023, .T. ) ;
#209364 = DIRECTION ( 'NONE',  ( -1.000000000000000000, -3.265361837132813093E-16, 0.000000000000000000 ) ) ;
#209366 = CIRCLE ( 'NONE', #51122, 0.09999999999999939493 ) ;
#209367 = CARTESIAN_POINT ( 'NONE',  ( 22.48660254037844197, 31.85034414784619017, -238.9397275603479898 ) ) ;
#209368 = DIRECTION ( 'NONE',  ( 0.000000000000000000, 0.000000000000000000, 1.000000000000000000 ) ) ;
#209369 = DIRECTION ( 'NONE',  ( 0.000000000000000000, 0.000000000000000000, 1.000000000000000000 ) ) ;
#209370 = LINE ( 'NONE', #49011, #208680 ) ;
#209371 = ADVANCED_FACE ( 'NONE', ( #182033 ), #231134, .T. ) ;
#209372 = DIRECTION ( 'NONE',  ( -1.000000000000000000, -0.000000000000000000, -0.000000000000000000 ) ) ;
#209373 = EDGE_CURVE ( 'NONE', #140569, #83407, #213457, .T. ) ;
#209374 = CARTESIAN_POINT ( 'NONE',  ( 21.10000000000000142, 0.000000000000000000, 0.000000000000000000 ) ) ;
#209375 = CARTESIAN_POINT ( 'NONE',  ( 21.14999999999999858, 6.540656951712400691, -100.6000000000000369 ) ) ;
#209376 = ORIENTED_EDGE ( 'NONE', *, *, #10195, .T. ) ;
#209377 = CARTESIAN_POINT ( 'NONE',  ( 20.84999999999999432, 67.85909929089923764, -227.8797997985275856 ) ) ;
#209378 = LINE ( 'NONE', #88115, #231567 ) ;
#209379 = DIRECTION ( 'NONE',  ( 1.000000000000000000, 0.000000000000000000, 0.000000000000000000 ) ) ;
#209380 = CARTESIAN_POINT ( 'NONE',  ( 18.49999999999999645, 1.736257131608553550, -78.56865232901755292 ) ) ;
#209381 = EDGE_CURVE ( 'NONE', #75529, #33291, #226336, .T. ) ;
#209382 = CARTESIAN_POINT ( 'NONE',  ( 21.11833042828123652, 6.445644693866282360, -167.4928994909405731 ) ) ;
#209383 = VECTOR ( 'NONE', #114886, 1000.000000000000000 ) ;
#209384 = VECTOR ( 'NONE', #101313, 1000.000000000000000 ) ;
#209385 = DIRECTION ( 'NONE',  ( -0.000000000000000000, 1.000000000000000000, -0.000000000000000000 ) ) ;
#209386 = AXIS2_PLACEMENT_3D ( 'NONE', #31272, #191623, #229437 ) ;
#209387 = EDGE_LOOP ( 'NONE', ( #107511, #165529, #244586, #198922 ) ) ;
#209388 = ORIENTED_EDGE ( 'NONE', *, *, #142385, .T. ) ;
#209389 = DIRECTION ( 'NONE',  ( -1.000000000000000000, 0.000000000000000000, 0.000000000000000000 ) ) ;
#209390 = DIRECTION ( 'NONE',  ( -1.000000000000000000, 0.000000000000000000, 0.000000000000000000 ) ) ;
#209391 = ADVANCED_FACE ( 'NONE', ( #64642 ), #166349, .T. ) ;
#209392 = CARTESIAN_POINT ( 'NONE',  ( -20.94999999999999929, 38.23914636435921466, -236.1324109481172968 ) ) ;
#209393 = CARTESIAN_POINT ( 'NONE',  ( -17.11825945287482753, 66.05000000001157900, -56.77310748452439526 ) ) ;
#209394 = CARTESIAN_POINT ( 'NONE',  ( 22.32929514600007792, 7.578647565376482653, 0.09907567811391973511 ) ) ;
#209395 = CARTESIAN_POINT ( 'NONE',  ( 23.24999999999999645, 1.115600667400684642E-11, -134.0000000000000284 ) ) ;
#209396 = DIRECTION ( 'NONE',  ( 0.000000000000000000, 0.000000000000000000, -1.000000000000000000 ) ) ;
#209397 = TOROIDAL_SURFACE ( 'NONE', #126004, 1.900000000000002576, 0.1000000000000000056 ) ;
#209398 = CARTESIAN_POINT ( 'NONE',  ( -20.85000000000000142, 77.16412189325258453, -28.30825939895270693 ) ) ;
#209399 = ORIENTED_EDGE ( 'NONE', *, *, #139898, .F. ) ;
#209400 = CARTESIAN_POINT ( 'NONE',  ( -18.69999999999999929, -1.467286812112899463, 28.00000000000000000 ) ) ;
#209401 = AXIS2_PLACEMENT_3D ( 'NONE', #107085, #186648, #8010 ) ;
#209402 = ORIENTED_EDGE ( 'NONE', *, *, #80637, .F. ) ;
#209403 = CYLINDRICAL_SURFACE ( 'NONE', #247043, 0.09999999999999939493 ) ;
#209404 = CARTESIAN_POINT ( 'NONE',  ( 21.04999999999951399, 10.50253167712597779, -7.558829817074861346 ) ) ;
#209405 = CARTESIAN_POINT ( 'NONE',  ( -20.64999999999999858, 29.28400589394459530, -237.3759593473670293 ) ) ;
#209406 = DIRECTION ( 'NONE',  ( 0.000000000000000000, 1.000000000000000000, 0.000000000000000000 ) ) ;
#209407 = CARTESIAN_POINT ( 'NONE',  ( 21.12802099929860589, 22.07166910013054917, -231.7761939280465526 ) ) ;
#209408 = DIRECTION ( 'NONE',  ( -1.000000000000000000, 0.000000000000000000, 0.000000000000000000 ) ) ;
#209409 = DIRECTION ( 'NONE',  ( 0.000000000000000000, 1.000000000000000000, -3.469446951953635015E-14 ) ) ;
#209410 = VERTEX_POINT ( 'NONE', #245855 ) ;
#209411 = CARTESIAN_POINT ( 'NONE',  ( 18.59999999999999432, 71.84303044094815505, -225.1053209871248271 ) ) ;
#209412 = DIRECTION ( 'NONE',  ( 1.000000000000000000, 0.000000000000000000, 0.000000000000000000 ) ) ;
#209413 = DIRECTION ( 'NONE',  ( 1.000000000000000000, 0.000000000000000000, 0.000000000000000000 ) ) ;
#209414 = CARTESIAN_POINT ( 'NONE',  ( -18.50000000000000000, 1.866714910068465239, -45.25267524628200988 ) ) ;
#209415 = CARTESIAN_POINT ( 'NONE',  ( 18.54286124688534798, 85.62391757880969578, -96.28190515266155103 ) ) ;
#209416 = EDGE_CURVE ( 'NONE', #207624, #205292, #67213, .T. ) ;
#209417 = AXIS2_PLACEMENT_3D ( 'NONE', #147842, #190844, #31771 ) ;
#209418 = ORIENTED_EDGE ( 'NONE', *, *, #172323, .F. ) ;
#209419 = CARTESIAN_POINT ( 'NONE',  ( 20.73486653747088937, 68.25000000001185185, -93.77310748452435973 ) ) ;
#209420 = CARTESIAN_POINT ( 'NONE',  ( 23.14999999999999858, 5.000000000011153745, -122.0947339810869465 ) ) ;
#209421 = ORIENTED_EDGE ( 'NONE', *, *, #146931, .F. ) ;
#209422 = ADVANCED_FACE ( 'NONE', ( #226258 ), #72046, .F. ) ;
#209423 = ORIENTED_EDGE ( 'NONE', *, *, #231666, .F. ) ;
#209424 = CARTESIAN_POINT ( 'NONE',  ( -16.90128866880175806, 51.62887945800996192, -231.9378224694952166 ) ) ;
#209425 = CARTESIAN_POINT ( 'NONE',  ( 21.05000005001206276, 11.25956737883785941, -211.0112013901115517 ) ) ;
#209426 = B_SPLINE_CURVE_WITH_KNOTS ( 'NONE', 3,
 ( #202334, #81084, #120271, #23734, #181508, #39445, #2831, #142354, #100631, #160674 ),
 .UNSPECIFIED., .F., .F.,
 ( 4, 2, 2, 2, 4 ),
 ( 0.000000000000000000, 0.0001660831991682438027, 0.0002491247987523657176, 0.0002906455985444088264, 0.0003321663983364519894 ),
 .UNSPECIFIED. ) ;
#209427 = EDGE_CURVE ( 'NONE', #50377, #217484, #30758, .T. ) ;
#209428 = ORIENTED_EDGE ( 'NONE', *, *, #184171, .T. ) ;
#209430 = EDGE_CURVE ( 'NONE', #46223, #42536, #146719, .T. ) ;
#209429 = CARTESIAN_POINT ( 'NONE',  ( 20.85000000106584750, 64.25000000001146816, -42.86760282805085609 ) ) ;
#209431 = CARTESIAN_POINT ( 'NONE',  ( -20.54999999999999716, -3.685352791942193562, -226.3713951780953550 ) ) ;
#209432 = CIRCLE ( 'NONE', #230277, 0.09999999999998951394 ) ;
#209433 = ORIENTED_EDGE ( 'NONE', *, *, #243122, .T. ) ;
#209434 = AXIS2_PLACEMENT_3D ( 'NONE', #203041, #43974, #100069 ) ;
#209435 = CARTESIAN_POINT ( 'NONE',  ( 18.39999999999999858, -9.682403433465241349, -174.1568433774127982 ) ) ;
#209436 = CIRCLE ( 'NONE', #205327, 0.1000000000000087624 ) ;
#209437 = ORIENTED_EDGE ( 'NONE', *, *, #204497, .T. ) ;
#209438 = CARTESIAN_POINT ( 'NONE',  ( 21.08489834409762764, 10.62232389474667293, -79.35000000000005116 ) ) ;
#209439 = EDGE_CURVE ( 'NONE', #238178, #70035, #101408, .T. ) ;
#209440 = DIRECTION ( 'NONE',  ( 1.000000000000000000, 0.000000000000000000, 0.000000000000000000 ) ) ;
#209442 = ORIENTED_EDGE ( 'NONE', *, *, #117042, .F. ) ;
#209441 = LINE ( 'NONE', #131185, #99867 ) ;
#209443 = CARTESIAN_POINT ( 'NONE',  ( 21.87500000000000355, 9.750000000011153745, -79.35000000000005116 ) ) ;
#209445 = DIRECTION ( 'NONE',  ( 0.000000000000000000, 0.000000000000000000, -1.000000000000000000 ) ) ;
#209444 = UNCERTAINTY_MEASURE_WITH_UNIT (LENGTH_MEASURE( 1.000000000000000082E-05 ), #178879, 'distance_accuracy_value', 'NONE');
#209446 = EDGE_CURVE ( 'NONE', #235545, #122770, #224977, .T. ) ;
#209447 = CARTESIAN_POINT ( 'NONE',  ( -21.05000000000000071, 1.250000000011155299, -175.4999999999999716 ) ) ;
#209448 = CARTESIAN_POINT ( 'NONE',  ( -20.85000000000000142, 6.846123162352588665, -37.23772626684986164 ) ) ;
#209449 = CARTESIAN_POINT ( 'NONE',  ( -16.77902162784673479, 66.05358074280475478, -190.8611162404550896 ) ) ;
#209450 = AXIS2_PLACEMENT_3D ( 'NONE', #164075, #19430, #243601 ) ;
#209451 = DIRECTION ( 'NONE',  ( -1.000000000000000000, 0.000000000000000000, -0.000000000000000000 ) ) ;
#209453 = DIRECTION ( 'NONE',  ( -1.690361071372200435E-14, 0.1332476588733650935, -0.9910827722268042983 ) ) ;
#209452 = AXIS2_PLACEMENT_3D ( 'NONE', #133835, #255000, #95978 ) ;
#209455 = ORIENTED_EDGE ( 'NONE', *, *, #198684, .F. ) ;
#209454 = CARTESIAN_POINT ( 'NONE',  ( 18.79999999999999716, 1.350000000000000089, 22.00000000000000355 ) ) ;
#209457 = ORIENTED_EDGE ( 'NONE', *, *, #7426, .F. ) ;
#209456 = PRODUCT_RELATED_PRODUCT_CATEGORY ( 'part', '', ( #49357 ) ) ;
#209459 = CARTESIAN_POINT ( 'NONE',  ( -15.73854595235692244, 9.351413679112546617, -83.98034356754902774 ) ) ;
#209458 = DIRECTION ( 'NONE',  ( 1.000000000000000000, 0.000000000000000000, 0.000000000000000000 ) ) ;
#209461 = ORIENTED_EDGE ( 'NONE', *, *, #85503, .T. ) ;
#209460 = CARTESIAN_POINT ( 'NONE',  ( -20.64999999999999858, 2.500000000011154633, -187.7753780772378889 ) ) ;
#209462 = EDGE_LOOP ( 'NONE', ( #18369, #90281, #247829, #12935 ) ) ;
#209463 = CARTESIAN_POINT ( 'NONE',  ( 18.59999999999999076, 6.450000000011156587, -144.0170271704400307 ) ) ;
#209464 = CARTESIAN_POINT ( 'NONE',  ( 18.59999999999999432, 74.36282728704168221, -124.9409541190522930 ) ) ;
#209466 = EDGE_CURVE ( 'NONE', #13430, #257702, #254492, .T. ) ;
#209465 = CARTESIAN_POINT ( 'NONE',  ( 21.05000000000000071, 76.00000000001142553, -36.02310748452432421 ) ) ;
#209467 = AXIS2_PLACEMENT_3D ( 'NONE', #24586, #70138, #166672 ) ;
#209468 = CARTESIAN_POINT ( 'NONE',  ( -20.91682497891422798, 10.32263460347359363, -173.0605957968672328 ) ) ;
#209469 = EDGE_CURVE ( 'NONE', #114401, #176027, #184660, .T. ) ;
#209470 = EDGE_CURVE ( 'NONE', #115707, #97104, #84863, .T. ) ;
#209471 = FACE_OUTER_BOUND ( 'NONE', #169931, .T. ) ;
#209472 = DIRECTION ( 'NONE',  ( 1.000000000000000000, 0.000000000000000000, 0.000000000000000000 ) ) ;
#209473 = CIRCLE ( 'NONE', #84536, 0.1000000000000028644 ) ;
#209474 = CIRCLE ( 'NONE', #221928, 0.09999999999999895084 ) ;
#209475 = AXIS2_PLACEMENT_3D ( 'NONE', #35316, #54819, #19573 ) ;
#209477 = AXIS2_PLACEMENT_3D ( 'NONE', #188523, #111561, #107700 ) ;
#209476 = CARTESIAN_POINT ( 'NONE',  ( -23.15000000000000213, 13.96869538424788360, -210.3925794786331949 ) ) ;
#209478 = EDGE_LOOP ( 'NONE', ( #214935, #79966, #146575, #62573 ) ) ;
#209479 = VERTEX_POINT ( 'NONE', #232418 ) ;
#209480 = DIRECTION ( 'NONE',  ( 0.000000000000000000, 0.000000000000000000, -1.000000000000000000 ) ) ;
#209481 = ORIENTED_EDGE ( 'NONE', *, *, #119519, .T. ) ;
#209482 = CARTESIAN_POINT ( 'NONE',  ( -20.54999999999999716, 23.45160524131172508, -253.2535058871250726 ) ) ;
#209483 = ORIENTED_EDGE ( 'NONE', *, *, #174472, .F. ) ;
#209484 = DIRECTION ( 'NONE',  ( 0.000000000000000000, 0.4930308989874980785, 0.8700118002898462599 ) ) ;
#209485 = CARTESIAN_POINT ( 'NONE',  ( -23.15000000000000213, 73.50000000001259082, -190.2984855617622770 ) ) ;
#209486 = CARTESIAN_POINT ( 'NONE',  ( -20.94999999999999929, 76.00000000001170974, -69.52310748452431710 ) ) ;
#209487 = ORIENTED_EDGE ( 'NONE', *, *, #38448, .T. ) ;
#209488 = CARTESIAN_POINT ( 'NONE',  ( 23.14999999999999858, 2.100000000000002309, -33.50000000000000000 ) ) ;
#209489 = ORIENTED_EDGE ( 'NONE', *, *, #137203, .F. ) ;
#209490 = LINE ( 'NONE', #229072, #181414 ) ;
#209491 = EDGE_CURVE ( 'NONE', #252057, #122792, #18267, .T. ) ;
#209492 = DIRECTION ( 'NONE',  ( 0.000000000000000000, 0.000000000000000000, -1.000000000000000000 ) ) ;
#209493 = VECTOR ( 'NONE', #176706, 1000.000000000000000 ) ;
#209494 = VERTEX_POINT ( 'NONE', #138397 ) ;
#209495 = AXIS2_PLACEMENT_3D ( 'NONE', #57891, #219538, #123032 ) ;
#209496 = CARTESIAN_POINT ( 'NONE',  ( -20.94999999999999929, 76.00000000001247713, -174.0231074845243882 ) ) ;
#209497 = ORIENTED_EDGE ( 'NONE', *, *, #133171, .T. ) ;
#209500 = ORIENTED_EDGE ( 'NONE', *, *, #69170, .T. ) ;
#209499 = DIRECTION ( 'NONE',  ( 0.000000000000000000, -0.9121259477928120862, 0.4099100576505341209 ) ) ;
#209498 = CARTESIAN_POINT ( 'NONE',  ( 23.14999999999998437, 1.148907358139439339E-11, -201.0000000000015064 ) ) ;
#209501 = FACE_OUTER_BOUND ( 'NONE', #176356, .T. ) ;
#209502 = ORIENTED_EDGE ( 'NONE', *, *, #198687, .F. ) ;
#209503 = DIRECTION ( 'NONE',  ( 0.000000000000000000, 1.000000000000000000, 0.000000000000000000 ) ) ;
#209504 = EDGE_LOOP ( 'NONE', ( #114916, #220610, #93217, #101779, #247074 ) ) ;
#209505 = VECTOR ( 'NONE', #212651, 1000.000000000000000 ) ;
#209506 = EDGE_CURVE ( 'NONE', #112737, #196929, #216680, .T. ) ;
#209507 = CIRCLE ( 'NONE', #97036, 11.69999999999998863 ) ;
#209508 = CARTESIAN_POINT ( 'NONE',  ( 23.14999999999999503, 64.35000000001150511, -48.17310748452440095 ) ) ;
#209509 = EDGE_LOOP ( 'NONE', ( #240771, #178622, #75657, #247685 ) ) ;
#209510 = DIRECTION ( 'NONE',  ( 0.000000000000000000, -0.2617529984165078982, -0.9651348961777145297 ) ) ;
#209511 = DIRECTION ( 'NONE',  ( -1.836970198721029934E-16, -1.000000000000000000, -6.982962677686266711E-15 ) ) ;
#209512 = DIRECTION ( 'NONE',  ( 0.000000000000000000, -0.000000000000000000, 1.000000000000000000 ) ) ;
#209513 = CIRCLE ( 'NONE', #109553, 0.09999999999999993616 ) ;
#209514 = EDGE_CURVE ( 'NONE', #192577, #22307, #79501, .T. ) ;
#209515 = CARTESIAN_POINT ( 'NONE',  ( -16.94878442675512886, 66.00827089702106321, -123.9113270601622503 ) ) ;
#209516 = AXIS2_PLACEMENT_3D ( 'NONE', #110408, #106539, #27059 ) ;
#209517 = ORIENTED_EDGE ( 'NONE', *, *, #163025, .F. ) ;
#209518 = AXIS2_PLACEMENT_3D ( 'NONE', #116569, #254744, #17461 ) ;
#209519 = EDGE_CURVE ( 'NONE', #44233, #67154, #217968, .T. ) ;
#209520 = AXIS2_PLACEMENT_3D ( 'NONE', #188736, #110482, #10110 ) ;
#209521 = DIRECTION ( 'NONE',  ( 1.000000000000000000, 0.000000000000000000, 0.000000000000000000 ) ) ;
#209522 = CARTESIAN_POINT ( 'NONE',  ( 18.39999999999999503, 11.47316190337363828, -46.15000000000000568 ) ) ;
#209523 = CARTESIAN_POINT ( 'NONE',  ( 18.51024323315077069, 10.31104185824064068, -139.5204516983106089 ) ) ;
#209524 = ORIENTED_EDGE ( 'NONE', *, *, #83740, .T. ) ;
#209525 = FACE_OUTER_BOUND ( 'NONE', #90587, .T. ) ;
#209526 = EDGE_LOOP ( 'NONE', ( #113475, #255041, #75772, #254706 ) ) ;
#209527 = CARTESIAN_POINT ( 'NONE',  ( -18.39999999999999858, 64.25000000001264766, -194.2731074845244450 ) ) ;
#209529 = ORIENTED_EDGE ( 'NONE', *, *, #173040, .T. ) ;
#209528 = AXIS2_PLACEMENT_3D ( 'NONE', #106206, #104903, #164919 ) ;
#209530 = EDGE_CURVE ( 'NONE', #55402, #253110, #134552, .T. ) ;
#209531 = EDGE_CURVE ( 'NONE', #207515, #183971, #193066, .T. ) ;
#209532 = CARTESIAN_POINT ( 'NONE',  ( -20.85000000000000142, 7.021664781911246322, -70.73356540189729458 ) ) ;
#209533 = DIRECTION ( 'NONE',  ( 1.000000000000000000, 0.000000000000000000, -3.469446951953635015E-14 ) ) ;
#209535 = ORIENTED_EDGE ( 'NONE', *, *, #40528, .F. ) ;
#209534 = CARTESIAN_POINT ( 'NONE',  ( -16.87401514999234564, 44.19934780856234369, -235.2703203795249749 ) ) ;
#209536 = CARTESIAN_POINT ( 'NONE',  ( -18.59999999999999787, 1.835341550235567887, -112.0551512925630249 ) ) ;
#209537 = ORIENTED_EDGE ( 'NONE', *, *, #180633, .F. ) ;
#209538 = VECTOR ( 'NONE', #164462, 1000.000000000000000 ) ;
#209539 = DIRECTION ( 'NONE',  ( 0.000000000000000000, -6.853228547068871147E-15, 1.000000000000000000 ) ) ;
#209540 = CARTESIAN_POINT ( 'NONE',  ( -16.87683809663750978, 9.950000000011137047, -113.9023640181965220 ) ) ;
#209541 = EDGE_LOOP ( 'NONE', ( #114586, #126869, #231716, #147434 ) ) ;
#209542 = CIRCLE ( 'NONE', #30510, 2.000000000000012879 ) ;
#209543 = DIRECTION ( 'NONE',  ( 0.000000000000000000, 1.000000000000000000, -6.308085367188393199E-16 ) ) ;
#209544 = CARTESIAN_POINT ( 'NONE',  ( -22.39999999999999858, 64.25000000001195133, -103.0231074845244024 ) ) ;
#209545 = ORIENTED_EDGE ( 'NONE', *, *, #70547, .T. ) ;
#209546 = CARTESIAN_POINT ( 'NONE',  ( -21.00000000000000000, -1.212568896937008089, -7.900000000000000355 ) ) ;
#209547 = EDGE_CURVE ( 'NONE', #61112, #175899, #48574, .T. ) ;
#209548 = EDGE_CURVE ( 'NONE', #166706, #8100, #251294, .T. ) ;
#209549 = VECTOR ( 'NONE', #51732, 1000.000000000000000 ) ;
#209550 = ORIENTED_EDGE ( 'NONE', *, *, #208024, .T. ) ;
#209551 = TOROIDAL_SURFACE ( 'NONE', #47212, 11.70000000000000107, 0.1000000000000000056 ) ;
#209552 = CIRCLE ( 'NONE', #184602, 0.2000000000000057288 ) ;
#209553 = CARTESIAN_POINT ( 'NONE',  ( 22.50000000000000000, 11.64957080755595520, -100.4000000000000483 ) ) ;
#209554 = AXIS2_PLACEMENT_3D ( 'NONE', #236305, #34293, #155525 ) ;
#209555 = LINE ( 'NONE', #195151, #47211 ) ;
#209556 = ADVANCED_FACE ( 'NONE', ( #15946 ), #147255, .F. ) ;
#209559 = EDGE_LOOP ( 'NONE', ( #578, #205593, #134078, #149577 ) ) ;
#209558 = ORIENTED_EDGE ( 'NONE', *, *, #139144, .F. ) ;
#209557 = DIRECTION ( 'NONE',  ( 0.000000000000000000, -7.109473446599835262E-15, 1.000000000000000000 ) ) ;
#209560 = CARTESIAN_POINT ( 'NONE',  ( 21.14999999999999858, 23.34004772283015328, -229.2004250369967338 ) ) ;
#209561 = FACE_OUTER_BOUND ( 'NONE', #205613, .T. ) ;
#209562 = ADVANCED_FACE ( 'NONE', ( #212840 ), #195860, .F. ) ;
#209563 = CARTESIAN_POINT ( 'NONE',  ( -16.93860193097148326, 9.993107767329243885, -20.90013836730685526 ) ) ;
#209565 = FACE_OUTER_BOUND ( 'NONE', #44725, .T. ) ;
#209564 = FACE_OUTER_BOUND ( 'NONE', #169160, .T. ) ;
#209566 = LINE ( 'NONE', #133871, #219499 ) ;
#209568 = EDGE_CURVE ( 'NONE', #9700, #245573, #32951, .T. ) ;
#209567 = DIRECTION ( 'NONE',  ( 0.000000000000000000, 0.1568667991644863147, 0.9876197685951252359 ) ) ;
#209569 = CARTESIAN_POINT ( 'NONE',  ( -22.94999999999999929, 0.000000000000000000, 0.000000000000000000 ) ) ;
#209570 = CIRCLE ( 'NONE', #168110, 11.80000000000000604 ) ;
#209571 = CARTESIAN_POINT ( 'NONE',  ( -18.59999999999999787, 38.29773864426885410, -236.0513742605307925 ) ) ;
#209572 = AXIS2_PLACEMENT_3D ( 'NONE', #95958, #12614, #215897 ) ;
#209573 = AXIS2_PLACEMENT_3D ( 'NONE', #230401, #131294, #210841 ) ;
#209574 = ORIENTED_EDGE ( 'NONE', *, *, #66187, .F. ) ;
#209575 = VERTEX_POINT ( 'NONE', #117582 ) ;
#209576 = ADVANCED_FACE ( 'NONE', ( #133297 ), #158041, .T. ) ;
#209577 = CARTESIAN_POINT ( 'NONE',  ( -22.57320508075687115, 11.75000000001115552, -33.50000000000000000 ) ) ;
#209579 = ORIENTED_EDGE ( 'NONE', *, *, #19889, .T. ) ;
#209578 = DIRECTION ( 'NONE',  ( 1.000000000000000000, 0.000000000000000000, 0.000000000000000000 ) ) ;
#209580 = ORIENTED_EDGE ( 'NONE', *, *, #204653, .T. ) ;
#209581 = DIRECTION ( 'NONE',  ( 0.000000000000000000, 1.000000000000000000, 0.000000000000000000 ) ) ;
#209582 = ORIENTED_EDGE ( 'NONE', *, *, #201935, .F. ) ;
#209583 = DIRECTION ( 'NONE',  ( -0.000000000000000000, -1.000000000000000000, 6.308085367188393199E-16 ) ) ;
#209584 = EDGE_CURVE ( 'NONE', #58661, #183838, #257041, .T. ) ;
#209585 = EDGE_CURVE ( 'NONE', #43859, #29044, #47271, .T. ) ;
#209586 = ORIENTED_EDGE ( 'NONE', *, *, #86502, .T. ) ;
#209587 = DIRECTION ( 'NONE',  ( 0.000000000000000000, -1.000000000000000000, -6.982962677686266711E-15 ) ) ;
#209588 = CARTESIAN_POINT ( 'NONE',  ( -20.85000000000000142, 79.16909458115067366, -196.2854372848902926 ) ) ;
#209590 = ORIENTED_EDGE ( 'NONE', *, *, #73536, .F. ) ;
#209589 = ORIENTED_EDGE ( 'NONE', *, *, #79309, .F. ) ;
#209591 = ORIENTED_EDGE ( 'NONE', *, *, #63131, .T. ) ;
#209592 = ORIENTED_EDGE ( 'NONE', *, *, #162166, .F. ) ;
#209593 = ORIENTED_EDGE ( 'NONE', *, *, #68755, .F. ) ;
#209594 = CARTESIAN_POINT ( 'NONE',  ( -20.10000000000000142, 4.625944962820097039, 22.03401928653448749 ) ) ;
#209595 = DIRECTION ( 'NONE',  ( -1.000000000000000000, 0.000000000000000000, 0.000000000000000000 ) ) ;
#209596 = DIRECTION ( 'NONE',  ( 0.000000000000000000, 0.9126074666063771490, 0.4088369013363281623 ) ) ;
#209598 = EDGE_LOOP ( 'NONE', ( #231805, #117478, #123219, #244061, #26208 ) ) ;
#209597 = DIRECTION ( 'NONE',  ( -1.000000000000000000, 0.000000000000000000, 0.000000000000000000 ) ) ;
#209599 = FACE_OUTER_BOUND ( 'NONE', #238437, .T. ) ;
#209600 = DIRECTION ( 'NONE',  ( 0.000000000000000000, -1.265107689135680095E-16, 1.000000000000000000 ) ) ;
#209602 = ORIENTED_EDGE ( 'NONE', *, *, #110975, .T. ) ;
#209601 = DIRECTION ( 'NONE',  ( -1.000000000000000000, -0.000000000000000000, 0.000000000000000000 ) ) ;
#209603 = DIRECTION ( 'NONE',  ( 0.000000000000000000, 0.000000000000000000, -1.000000000000000000 ) ) ;
#209604 = VERTEX_POINT ( 'NONE', #217942 ) ;
#209605 = FACE_OUTER_BOUND ( 'NONE', #121425, .T. ) ;
#209606 = ORIENTED_EDGE ( 'NONE', *, *, #6896, .T. ) ;
#209607 = LINE ( 'NONE', #150917, #1866 ) ;
#209608 = DIRECTION ( 'NONE',  ( 1.000000000000000000, -0.000000000000000000, -0.000000000000000000 ) ) ;
#209609 = VERTEX_POINT ( 'NONE', #120193 ) ;
#209611 = CYLINDRICAL_SURFACE ( 'NONE', #195668, 0.09999999999998898659 ) ;
#209610 = CARTESIAN_POINT ( 'NONE',  ( -21.00023020733502932, 76.00000000001273293, -209.9139767297926937 ) ) ;
#209612 = CARTESIAN_POINT ( 'NONE',  ( 23.15000000000000213, 69.47678708576792417, -248.4500549165069856 ) ) ;
#209613 = EDGE_CURVE ( 'NONE', #242161, #35701, #199713, .T. ) ;
#209614 = VECTOR ( 'NONE', #151393, 1000.000000000000000 ) ;
#209615 = LINE ( 'NONE', #27161, #222078 ) ;
#209616 = DIRECTION ( 'NONE',  ( -1.000000000000000000, 0.000000000000000000, 0.000000000000000000 ) ) ;
#209617 = EDGE_LOOP ( 'NONE', ( #205028, #228625, #159241, #158450, #156471, #152341, #94371, #151756, #255635, #183660, #131219 ) ) ;
#209618 = ORIENTED_EDGE ( 'NONE', *, *, #62086, .F. ) ;
#209619 = CARTESIAN_POINT ( 'NONE',  ( 21.05000000000000071, 8.815201804566768828, -8.420537496683621725 ) ) ;
#209620 = CARTESIAN_POINT ( 'NONE',  ( 18.59999999999999076, 69.55000000001207638, -126.5060803140843291 ) ) ;
#209621 = ORIENTED_EDGE ( 'NONE', *, *, #228724, .F. ) ;
#209622 = CARTESIAN_POINT ( 'NONE',  ( -23.25000000000000000, 21.17283678855157802, -243.7231193059830332 ) ) ;
#209623 = ORIENTED_EDGE ( 'NONE', *, *, #161700, .T. ) ;
#209624 = DIRECTION ( 'NONE',  ( 0.000000000000000000, -1.000000000000000000, 0.000000000000000000 ) ) ;
#209625 = DIRECTION ( 'NONE',  ( 0.000000000000000000, 0.8814952561688476074, -0.4721928772777262417 ) ) ;
#209626 = FACE_OUTER_BOUND ( 'NONE', #12083, .T. ) ;
#209627 = ORIENTED_EDGE ( 'NONE', *, *, #52212, .F. ) ;
#209628 = VECTOR ( 'NONE', #132116, 1000.000000000000227 ) ;
#209629 = CARTESIAN_POINT ( 'NONE',  ( -16.87683809663752399, 66.15000000001259650, -190.1207434663281219 ) ) ;
#209630 =( NAMED_UNIT ( * ) PLANE_ANGLE_UNIT ( ) SI_UNIT ( $, .RADIAN. ) );
#209631 = EDGE_CURVE ( 'NONE', #251832, #14729, #68145, .T. ) ;
#209632 = CIRCLE ( 'NONE', #242939, 0.1000000000000028644 ) ;
#209633 = ORIENTED_EDGE ( 'NONE', *, *, #34592, .T. ) ;
#209634 = ORIENTED_EDGE ( 'NONE', *, *, #95248, .F. ) ;
#209635 = ORIENTED_EDGE ( 'NONE', *, *, #202755, .T. ) ;
#209636 = AXIS2_PLACEMENT_3D ( 'NONE', #220120, #200547, #63603 ) ;
#209637 = LINE ( 'NONE', #31036, #34152 ) ;
#209638 = CARTESIAN_POINT ( 'NONE',  ( -23.15000000000000213, 76.00000000001165290, -69.52310748452431710 ) ) ;
#209639 = DIRECTION ( 'NONE',  ( 0.000000000000000000, 0.8814952561688476074, -0.4721928772777262417 ) ) ;
#209640 = DIRECTION ( 'NONE',  ( 0.000000000000000000, -0.8814952561685545085, 0.4721928772782730821 ) ) ;
#209641 = CARTESIAN_POINT ( 'NONE',  ( -16.87786941232801041, 9.958154714144969333, -20.87718579979400957 ) ) ;
#209643 = DIRECTION ( 'NONE',  ( 0.000000000000000000, 0.3488585713686273571, 0.9371753822965264158 ) ) ;
#209642 = CARTESIAN_POINT ( 'NONE',  ( 22.49806830649814060, -3.103911027125945132, -228.1634219689893825 ) ) ;
#209645 = EDGE_LOOP ( 'NONE', ( #217854, #239300, #160221, #31659, #37712 ) ) ;
#209644 = DIRECTION ( 'NONE',  ( 1.000000000000000000, 0.000000000000000000, 0.000000000000000000 ) ) ;
#209646 = CARTESIAN_POINT ( 'NONE',  ( 16.87683809663750267, 9.950000000011138823, -46.15000000000000568 ) ) ;
#209647 = ORIENTED_EDGE ( 'NONE', *, *, #156567, .F. ) ;
#209648 = DIRECTION ( 'NONE',  ( 0.000000000000000000, 0.2617529984165152257, 0.9651348961777124202 ) ) ;
#209649 = EDGE_LOOP ( 'NONE', ( #115154, #190679, #210382, #232319 ) ) ;
#209650 = VERTEX_POINT ( 'NONE', #61462 ) ;
#209651 = DIRECTION ( 'NONE',  ( 0.000000000000000000, 1.000000000000000000, 6.938893903907222067E-15 ) ) ;
#209653 = CIRCLE ( 'NONE', #217994, 0.09999999999999939493 ) ;
#209652 = CARTESIAN_POINT ( 'NONE',  ( 21.05000000000000071, 85.00000000001222134, -146.4170766071767389 ) ) ;
#209654 = CARTESIAN_POINT ( 'NONE',  ( -16.86757978335471719, 66.03434962097729510, -56.92510283135688098 ) ) ;
#209655 = AXIS2_PLACEMENT_3D ( 'NONE', #253471, #176537, #134795 ) ;
#209656 = CARTESIAN_POINT ( 'NONE',  ( 18.49999999999998934, 69.55000000001207638, -126.5060803140843291 ) ) ;
#209657 = VECTOR ( 'NONE', #19917, 1000.000000000000000 ) ;
#209658 = CARTESIAN_POINT ( 'NONE',  ( -21.05000000000000071, 7.128833340093095217, -233.7327013124392749 ) ) ;
#209659 = VERTEX_POINT ( 'NONE', #139693 ) ;
#209660 = EDGE_LOOP ( 'NONE', ( #188026, #64591 ) ) ;
#209661 = AXIS2_PLACEMENT_3D ( 'NONE', #144178, #3385, #163773 ) ;
#209662 = CARTESIAN_POINT ( 'NONE',  ( 20.04142135623730070, 64.25000000001253397, -182.1731074845244507 ) ) ;
#209663 = EDGE_LOOP ( 'NONE', ( #25548, #213076, #25014, #7060, #159452 ) ) ;
#209664 = CARTESIAN_POINT ( 'NONE',  ( 18.79999999999999716, -1.786320531569725478, -11.50977166988710820 ) ) ;
#209665 = DIRECTION ( 'NONE',  ( -0.000000000000000000, -0.000000000000000000, -1.000000000000000000 ) ) ;
#209666 = ORIENTED_EDGE ( 'NONE', *, *, #34547, .T. ) ;
#209667 = CARTESIAN_POINT ( 'NONE',  ( 23.50000000000005684, 82.72707916847673459, -26.51159310135756897 ) ) ;
#209668 = CARTESIAN_POINT ( 'NONE',  ( -23.25000000000000000, -11.74999999998884448, -33.50000000000000000 ) ) ;
#209669 = CARTESIAN_POINT ( 'NONE',  ( -18.54270223418608410, -9.624105502871737272, -207.7409350504073586 ) ) ;
#209670 = CARTESIAN_POINT ( 'NONE',  ( -21.05000000000000071, 4.252251777740764460, -211.8999245327126744 ) ) ;
#209671 = EDGE_LOOP ( 'NONE', ( #1795, #143980, #150506, #28058, #178270, #253183 ) ) ;
#209672 = DIRECTION ( 'NONE',  ( 1.000000000000000000, 0.000000000000000000, 0.000000000000000000 ) ) ;
#209673 = AXIS2_PLACEMENT_3D ( 'NONE', #114793, #229611, #70563 ) ;
#209675 = DIRECTION ( 'NONE',  ( 0.000000000000000000, 1.000000000000000000, 0.000000000000000000 ) ) ;
#209674 = VECTOR ( 'NONE', #133182, 1000.000000000000000 ) ;
#209676 = AXIS2_PLACEMENT_3D ( 'NONE', #173901, #85594, #225125 ) ;
#209677 = AXIS2_PLACEMENT_3D ( 'NONE', #173213, #54489, #213560 ) ;
#209678 = DIRECTION ( 'NONE',  ( 0.000000000000000000, 1.000000000000000000, -6.308085367188393199E-16 ) ) ;
#209679 = DIRECTION ( 'NONE',  ( 0.000000000000000000, 0.1332476588733589040, -0.9910827722268048534 ) ) ;
#209680 = EDGE_CURVE ( 'NONE', #245594, #163086, #81002, .T. ) ;
#209681 = DIRECTION ( 'NONE',  ( 0.000000000000000000, 0.000000000000000000, 1.000000000000000000 ) ) ;
#209682 = ORIENTED_EDGE ( 'NONE', *, *, #128684, .T. ) ;
#209683 = EDGE_CURVE ( 'NONE', #228476, #238440, #234931, .T. ) ;
#209684 = DIRECTION ( 'NONE',  ( 0.000000000000000000, 0.000000000000000000, -1.000000000000000000 ) ) ;
#209685 = ORIENTED_EDGE ( 'NONE', *, *, #63070, .T. ) ;
#209686 = DIRECTION ( 'NONE',  ( -1.000000000000000000, -0.000000000000000000, -0.000000000000000000 ) ) ;
#209687 = DIRECTION ( 'NONE',  ( -1.462545276649569224E-15, 0.1686199900910448357, -0.9856811345164804283 ) ) ;
#209688 = ADVANCED_FACE ( 'NONE', ( #5303 ), #219238, .F. ) ;
#209689 = DIRECTION ( 'NONE',  ( -1.000000000000000000, 0.000000000000000000, 0.000000000000000000 ) ) ;
#209690 = DIRECTION ( 'NONE',  ( 1.000000000000000000, -0.000000000000000000, -0.000000000000000000 ) ) ;
#209691 = CARTESIAN_POINT ( 'NONE',  ( 20.96937028524355284, 65.37553062838564699, -162.5316813833548508 ) ) ;
#209692 = VERTEX_POINT ( 'NONE', #118885 ) ;
#209693 = FACE_OUTER_BOUND ( 'NONE', #247726, .T. ) ;
#209694 = AXIS2_PLACEMENT_3D ( 'NONE', #107110, #124129, #82385 ) ;
#209695 = DIRECTION ( 'NONE',  ( 0.000000000000000000, 0.000000000000000000, -1.000000000000000000 ) ) ;
#209697 = AXIS2_PLACEMENT_3D ( 'NONE', #186566, #28811, #185267 ) ;
#209696 = DIRECTION ( 'NONE',  ( 0.000000000000000000, 0.000000000000000000, -1.000000000000000000 ) ) ;
#209698 = EDGE_CURVE ( 'NONE', #77369, #19542, #30947, .T. ) ;
#209699 = CIRCLE ( 'NONE', #168045, 0.09999999999998898659 ) ;
#209700 = DIRECTION ( 'NONE',  ( 0.000000000000000000, 0.000000000000000000, -1.000000000000000000 ) ) ;
#209701 =( BOUNDED_SURFACE ( )  B_SPLINE_SURFACE ( 3, 2, ( 
 ( #232426, #133308, #34234 ),
 ( #173770, #194591, #15956 ),
 ( #96707, #62440, #204493 ),
 ( #222771, #201950, #3737 ),
 ( #22038, #254502, #161553 ),
 ( #24621, #243632, #164108 ),
 ( #23337, #42871, #121158 ),
 ( #116323, #224057, #141959 ),
 ( #45436, #156749, #144516 ),
 ( #64990, #44164, #102815 ) ),
 .UNSPECIFIED., .F., .F., .T. ) 
 B_SPLINE_SURFACE_WITH_KNOTS ( ( 4, 2, 2, 2, 4 ),
 ( 3, 3 ),
 ( 0.0001701955120502381136, 0.0002247052511886090949, 0.0002792149903269800491, 0.0003882344686037219575, 0.0006062734251572058286 ),
 ( 0.000000000000000000, 1.000000000000000000 ),
 .UNSPECIFIED. ) 
 GEOMETRIC_REPRESENTATION_ITEM ( )  RATIONAL_B_SPLINE_SURFACE ( (
 ( 1.000000000000000000, 0.2966190024561997651, 1.000000000000000000),
 ( 1.000000000000000000, 0.2964522492692210909, 1.000000000000000000),
 ( 1.000000000000000000, 0.3059923531906453276, 1.000000000000000000),
 ( 1.000000000000000000, 0.3355751146923415251, 1.000000000000000000),
 ( 1.000000000000000000, 0.3550672384958439287, 1.000000000000000000),
 ( 1.000000000000000000, 0.4157034672187444047, 1.000000000000000000),
 ( 1.000000000000000000, 0.4588031877661047919, 1.000000000000000000),
 ( 1.000000000000000000, 0.5771441759645236091, 1.000000000000000000),
 ( 1.000000000000000000, 0.6469377121783427276, 1.000000000000000000),
 ( 1.000000000000000000, 0.7071067811865475727, 1.000000000000000000) ) ) 
 REPRESENTATION_ITEM ( '' )  SURFACE ( )  );
#209702 = EDGE_LOOP ( 'NONE', ( #245066, #165622, #39840, #236770 ) ) ;
#209703 = ORIENTED_EDGE ( 'NONE', *, *, #163982, .T. ) ;
#209704 = FACE_OUTER_BOUND ( 'NONE', #6558, .T. ) ;
#209705 = AXIS2_PLACEMENT_3D ( 'NONE', #88861, #91463, #193135 ) ;
#209706 = DIRECTION ( 'NONE',  ( 1.000000000000000000, -0.000000000000000000, -0.000000000000000000 ) ) ;
#209707 = CARTESIAN_POINT ( 'NONE',  ( -18.54118089899632693, -9.463537631836942410, -107.5485775978681602 ) ) ;
#209708 = AXIS2_PLACEMENT_3D ( 'NONE', #66575, #5274, #125260 ) ;
#209709 = CARTESIAN_POINT ( 'NONE',  ( -21.07094088545304444, 69.67983277809588571, -170.1220011870766200 ) ) ;
#209710 = EDGE_CURVE ( 'NONE', #157096, #148469, #43384, .T. ) ;
#209711 = ORIENTED_EDGE ( 'NONE', *, *, #162242, .T. ) ;
#209712 = FACE_OUTER_BOUND ( 'NONE', #427, .T. ) ;
#209713 = ITEM_DEFINED_TRANSFORMATION ( 'NONE', 'NONE', #15288,  #2425 ) ;
#209715 = CIRCLE ( 'NONE', #122224, 0.09999999999999939493 ) ;
#209714 = CARTESIAN_POINT ( 'NONE',  ( 23.24999999999999289, 71.85000000001194564, -103.0231074845243455 ) ) ;
#209716 = ORIENTED_EDGE ( 'NONE', *, *, #168329, .T. ) ;
#209717 = CARTESIAN_POINT ( 'NONE',  ( -18.50000000000000000, 1.835341550235567887, -179.0551512925629538 ) ) ;
#209718 = CIRCLE ( 'NONE', #43123, 2.000000000000001776 ) ;
#209719 = AXIS2_PLACEMENT_3D ( 'NONE', #26481, #105976, #151584 ) ;
#209720 = PRODUCT ( 'Injection Molded Chain Links 4', 'Injection Molded Chain Links 4', '', ( #151348 ) ) ;
#209721 = CIRCLE ( 'NONE', #97236, 3.970710678118657189 ) ;
#209722 = VERTEX_POINT ( 'NONE', #2753 ) ;
#209723 = VERTEX_POINT ( 'NONE', #99281 ) ;
#209724 = ORIENTED_EDGE ( 'NONE', *, *, #16576, .T. ) ;
#209725 = CARTESIAN_POINT ( 'NONE',  ( -16.94226253665225812, 9.950000000011138823, -154.5532654043842626 ) ) ;
#209726 = FACE_OUTER_BOUND ( 'NONE', #159051, .T. ) ;
#209728 = AXIS2_PLACEMENT_3D ( 'NONE', #215138, #37809, #36533 ) ;
#209727 = CARTESIAN_POINT ( 'NONE',  ( -18.50000000000000000, 1.115600667400684642E-11, -200.9999999999999432 ) ) ;
#209729 = EDGE_CURVE ( 'NONE', #40263, #108305, #203543, .T. ) ;
#209730 = DIRECTION ( 'NONE',  ( -1.000000000000000000, -0.000000000000000000, -0.000000000000000000 ) ) ;
#209731 = DIRECTION ( 'NONE',  ( -1.000000000000000000, 0.000000000000000000, -0.000000000000000000 ) ) ;
#209732 = CARTESIAN_POINT ( 'NONE',  ( 21.05000000000005400, 83.80000000001119531, -34.86056257560453986 ) ) ;
#209733 = DIRECTION ( 'NONE',  ( 0.000000000000000000, 0.2617529984165152257, 0.9651348961777124202 ) ) ;
#209735 = DIRECTION ( 'NONE',  ( 1.000000000000000000, 0.000000000000000000, 0.000000000000000000 ) ) ;
#209734 = DIRECTION ( 'NONE',  ( -1.000000000000000000, 0.000000000000000000, -0.000000000000000000 ) ) ;
#209736 = AXIS2_PLACEMENT_3D ( 'NONE', #12673, #110459, #28403 ) ;
#209737 = DIRECTION ( 'NONE',  ( 1.186688945009009831E-16, 1.000000000000000000, 6.982962677686266711E-15 ) ) ;
#209738 = CARTESIAN_POINT ( 'NONE',  ( -21.44999999999999929, 29.19585636832770703, -237.3287400596392445 ) ) ;
#209739 = CARTESIAN_POINT ( 'NONE',  ( 20.94999999999999929, 33.13294339707397995, -247.6623911921324463 ) ) ;
#209740 = DIRECTION ( 'NONE',  ( 0.000000000000000000, 1.000000000000000000, 6.982962677686266711E-15 ) ) ;
#209741 = ORIENTED_EDGE ( 'NONE', *, *, #247748, .F. ) ;
#209742 = ORIENTED_EDGE ( 'NONE', *, *, #25169, .T. ) ;
#209743 = FACE_OUTER_BOUND ( 'NONE', #19984, .T. ) ;
#209744 = CIRCLE ( 'NONE', #214020, 0.09999999999999986677 ) ;
#209745 = LINE ( 'NONE', #251432, #20355 ) ;
#209746 = DIRECTION ( 'NONE',  ( 0.000000000000000000, -0.000000000000000000, -1.000000000000000000 ) ) ;
#209747 = VECTOR ( 'NONE', #180345, 1000.000000000000000 ) ;
#209748 = ADVANCED_FACE ( 'NONE', ( #41925 ), #1671, .T. ) ;
#209749 = CARTESIAN_POINT ( 'NONE',  ( -20.94999999999999929, 79.10508929521364507, -235.9670348125907537 ) ) ;
#209750 = SPHERICAL_SURFACE ( 'NONE', #58592, 0.1000000000000000056 ) ;
#209751 = CARTESIAN_POINT ( 'NONE',  ( 12.25000000000000000, 62.10905854918434699, -217.1108499610991203 ) ) ;
#209752 = EDGE_LOOP ( 'NONE', ( #108057, #146466, #5575, #59895 ) ) ;
#209753 = EDGE_CURVE ( 'NONE', #13712, #42440, #180765, .T. ) ;
#209754 = ORIENTED_EDGE ( 'NONE', *, *, #230150, .T. ) ;
#209755 = CARTESIAN_POINT ( 'NONE',  ( -20.94999999999999929, 87.48912529308779540, -72.52310748452423184 ) ) ;
#209756 = ORIENTED_EDGE ( 'NONE', *, *, #150279, .T. ) ;
#209757 = EDGE_CURVE ( 'NONE', #54789, #107177, #22550, .T. ) ;
#209758 = CARTESIAN_POINT ( 'NONE',  ( -23.15000000000000213, 71.65000000001259650, -191.1731074845243654 ) ) ;
#209759 = CIRCLE ( 'NONE', #146806, 0.1000000000000016431 ) ;
#209760 = VECTOR ( 'NONE', #143736, 1000.000000000000000 ) ;
#209761 = AXIS2_PLACEMENT_3D ( 'NONE', #211779, #193504, #14874 ) ;
#209762 = VECTOR ( 'NONE', #229123, 1000.000000000000000 ) ;
#209763 = VERTEX_POINT ( 'NONE', #101842 ) ;
#209764 = CARTESIAN_POINT ( 'NONE',  ( 33.30000000000001137, 3.332938107839120701, -347.0000000000001137 ) ) ;
#209765 = EDGE_CURVE ( 'NONE', #67305, #20901, #24926, .T. ) ;
#209766 = ORIENTED_EDGE ( 'NONE', *, *, #209765, .F. ) ;
#209767 = CARTESIAN_POINT ( 'NONE',  ( 23.14999999999999503, 64.35000000001186038, -90.87310748452438247 ) ) ;
#209768 = DIRECTION ( 'NONE',  ( 0.000000000000000000, 1.000000000000000000, 0.000000000000000000 ) ) ;
#209769 = DIRECTION ( 'NONE',  ( -0.000000000000000000, -0.2617529984165031243, -0.9651348961777157509 ) ) ;
#209770 = EDGE_CURVE ( 'NONE', #207394, #222651, #184840, .T. ) ;
#209771 = CARTESIAN_POINT ( 'NONE',  ( 18.43473516226068298, -9.494942282747075524, -141.0458986833495203 ) ) ;
#209772 = EDGE_CURVE ( 'NONE', #35900, #183385, #4047, .T. ) ;
#209773 = DIRECTION ( 'NONE',  ( -1.000000000000000000, 7.492892343619937423E-30, -1.073024830501117725E-15 ) ) ;
#209774 = DIRECTION ( 'NONE',  ( 0.000000000000000000, -7.026728003956695223E-15, 1.000000000000000000 ) ) ;
#209775 = DIRECTION ( 'NONE',  ( 1.000000000000000000, 0.000000000000000000, 0.000000000000000000 ) ) ;
#209776 = FACE_OUTER_BOUND ( 'NONE', #130627, .T. ) ;
#209778 = ORIENTED_EDGE ( 'NONE', *, *, #38500, .T. ) ;
#209777 = FACE_OUTER_BOUND ( 'NONE', #233922, .T. ) ;
#209780 = CARTESIAN_POINT ( 'NONE',  ( 21.14999999999999858, 76.00000000001242029, -176.5637644362255969 ) ) ;
#209779 = DIRECTION ( 'NONE',  ( 1.186688945009009831E-16, -1.000000000000000000, 0.000000000000000000 ) ) ;
#209782 = ORIENTED_EDGE ( 'NONE', *, *, #210388, .T. ) ;
#209781 = B_SPLINE_CURVE_WITH_KNOTS ( 'NONE', 3,
 ( #160732, #240248, #61596, #201103, #101973, #2886, #70615, #148850, #108429, #110994 ),
 .UNSPECIFIED., .F., .F.,
 ( 4, 3, 3, 4 ),
 ( 0.000000000000000000, 0.0002000000000008546862, 0.001000000000082975097, 0.001967863649483340624 ),
 .UNSPECIFIED. ) ;
#209784 = ORIENTED_EDGE ( 'NONE', *, *, #217702, .F. ) ;
#209783 = CARTESIAN_POINT ( 'NONE',  ( 21.05000000000000071, 1.148907358139439339E-11, -201.0000000000015064 ) ) ;
#209785 = ORIENTED_EDGE ( 'NONE', *, *, #243745, .F. ) ;
#209786 = CARTESIAN_POINT ( 'NONE',  ( 20.04142135623730070, 15.92646454033040015, -219.3818586450342423 ) ) ;
#209787 = LINE ( 'NONE', #33760, #130324 ) ;
#209788 = EDGE_CURVE ( 'NONE', #225448, #17815, #85965, .T. ) ;
#209789 = AXIS2_PLACEMENT_3D ( 'NONE', #68015, #230967, #251785 ) ;
#209790 = CARTESIAN_POINT ( 'NONE',  ( 20.99780126800947144, 62.98982820228305002, -207.1569994557046073 ) ) ;
#209791 = CARTESIAN_POINT ( 'NONE',  ( -18.59999999999999787, -9.480686695267820596, -107.4411151687578894 ) ) ;
#209792 = DIRECTION ( 'NONE',  ( 1.000000000000000000, 3.265361837132813093E-16, -0.000000000000000000 ) ) ;
#209793 = ADVANCED_FACE ( 'NONE', ( #7923 ), #5944, .T. ) ;
#209794 = EDGE_CURVE ( 'NONE', #90690, #224002, #105720, .T. ) ;
#209795 = DIRECTION ( 'NONE',  ( 0.000000000000000000, 0.000000000000000000, -1.000000000000000000 ) ) ;
#209796 = CARTESIAN_POINT ( 'NONE',  ( -18.50000000000000000, 9.150000000011157653, -21.75000000000000355 ) ) ;
#209797 = DIRECTION ( 'NONE',  ( 2.978066053179067751E-16, -0.9770955615653316162, -0.2128009952263596738 ) ) ;
#209798 = CARTESIAN_POINT ( 'NONE',  ( 20.85000000000000142, 76.00000000001126921, -203.5231074845248997 ) ) ;
#209799 = ORIENTED_EDGE ( 'NONE', *, *, #100041, .T. ) ;
#209800 = ORIENTED_EDGE ( 'NONE', *, *, #88043, .F. ) ;
#209801 = DIRECTION ( 'NONE',  ( 0.000000000000000000, 0.1350103645451807555, 0.9908441862701609093 ) ) ;
#209802 = AXIS2_PLACEMENT_3D ( 'NONE', #5097, #242445, #63830 ) ;
#209803 = ORIENTED_EDGE ( 'NONE', *, *, #37965, .T. ) ;
#209804 = DIRECTION ( 'NONE',  ( -0.000000000000000000, -0.8814952561688430555, 0.4721928772777346239 ) ) ;
#209805 = ORIENTED_EDGE ( 'NONE', *, *, #253149, .T. ) ;
#209806 = CARTESIAN_POINT ( 'NONE',  ( 22.49999999999999645, 11.64976291804307884, -33.41119002361307366 ) ) ;
#209807 = AXIS2_PLACEMENT_3D ( 'NONE', #97991, #192006, #13351 ) ;
#209808 = EDGE_CURVE ( 'NONE', #133447, #29429, #189143, .T. ) ;
#209809 = CARTESIAN_POINT ( 'NONE',  ( 21.14999999999999503, 87.65000000001192859, -100.1231074845242262 ) ) ;
#209810 = CARTESIAN_POINT ( 'NONE',  ( -22.49072729836729678, -2.423945104021340224, -189.6048092360547059 ) ) ;
#209811 = EDGE_CURVE ( 'NONE', #147021, #216194, #85040, .T. ) ;
#209812 = FACE_OUTER_BOUND ( 'NONE', #134151, .T. ) ;
#209813 = CARTESIAN_POINT ( 'NONE',  ( 21.07928932188134397, 75.90110485435833709, -209.8516241409176928 ) ) ;
#209814 = ORIENTED_EDGE ( 'NONE', *, *, #15096, .F. ) ;
#209815 = DIRECTION ( 'NONE',  ( 0.000000000000000000, 0.3042567129660163627, 0.9525900758537824142 ) ) ;
#209816 = DIRECTION ( 'NONE',  ( 0.000000000000000000, -0.2617529984165152257, -0.9651348961777124202 ) ) ;
#209817 = ADVANCED_FACE ( 'NONE', ( #86123 ), #251484, .F. ) ;
#209819 = AXIS2_PLACEMENT_3D ( 'NONE', #203699, #220695, #180286 ) ;
#209818 = DIRECTION ( 'NONE',  ( 0.000000000000000000, 0.9770955615653313941, 0.2128009952263603677 ) ) ;
#209820 = CARTESIAN_POINT ( 'NONE',  ( -21.05000000000000426, 6.477046381801004671, -134.1000000000000227 ) ) ;
#209821 = CARTESIAN_POINT ( 'NONE',  ( -23.15000000000000213, 56.18374508921711197, -227.9290876000915205 ) ) ;
#209822 = ORIENTED_EDGE ( 'NONE', *, *, #78839, .T. ) ;
#209824 = LINE ( 'NONE', #49461, #123300 ) ;
#209823 = DIRECTION ( 'NONE',  ( 0.000000000000000000, 0.9126074666063770380, 0.4088369013363281068 ) ) ;
#209826 = VERTEX_POINT ( 'NONE', #206108 ) ;
#209825 = VECTOR ( 'NONE', #251818, 1000.000000000000114 ) ;
#209829 = EDGE_LOOP ( 'NONE', ( #19893, #108555, #45325, #58260 ) ) ;
#209828 = CARTESIAN_POINT ( 'NONE',  ( -18.40000000000000213, 11.47316190337364183, -57.67405393319205587 ) ) ;
#209827 = DIRECTION ( 'NONE',  ( 1.000000000000000000, 0.000000000000000000, -0.000000000000000000 ) ) ;
#209830 = CARTESIAN_POINT ( 'NONE',  ( -23.25000000000000000, 1.115600667400684642E-11, -167.5000000000000284 ) ) ;
#209831 = TOROIDAL_SURFACE ( 'NONE', #188980, 0.2000000000000000111, 0.1000000000000000056 ) ;
#209833 = LINE ( 'NONE', #168179, #32175 ) ;
#209832 = VECTOR ( 'NONE', #110745, 1000.000000000000000 ) ;
#209834 = CARTESIAN_POINT ( 'NONE',  ( -18.39999999999999858, 20.76715588789282307, -228.0228088279911560 ) ) ;
#209835 = VERTEX_POINT ( 'NONE', #88700 ) ;
#209836 = CARTESIAN_POINT ( 'NONE',  ( -20.54999999999999716, 52.13794731297493712, -232.3713824252124880 ) ) ;
#209837 = DIRECTION ( 'NONE',  ( 0.000000000000000000, 0.000000000000000000, 1.000000000000000000 ) ) ;
#209839 = CARTESIAN_POINT ( 'NONE',  ( -20.94999999999999929, -1.835341550213255957, -45.15515129256298366 ) ) ;
#209838 = LINE ( 'NONE', #31241, #26405 ) ;
#209841 = ORIENTED_EDGE ( 'NONE', *, *, #152175, .T. ) ;
#209840 = CARTESIAN_POINT ( 'NONE',  ( -18.52139480978225450, 46.94591656517138745, -255.3320236366652409 ) ) ;
#209842 = VECTOR ( 'NONE', #154500, 1000.000000000000000 ) ;
#209843 = EDGE_CURVE ( 'NONE', #21693, #72588, #35054, .T. ) ;
#209844 = CIRCLE ( 'NONE', #184874, 0.1000000000000028644 ) ;
#209845 = B_SPLINE_CURVE_WITH_KNOTS ( 'NONE', 3,
 ( #153289, #214496, #16328, #95818, #15041, #175410 ),
 .UNSPECIFIED., .F., .F.,
 ( 4, 2, 4 ),
 ( 0.000000000000000000, 0.0001568709654583421050, 0.0003137419309166842099 ),
 .UNSPECIFIED. ) ;
#209846 = AXIS2_PLACEMENT_3D ( 'NONE', #170372, #93343, #50343 ) ;
#209847 = ORIENTED_EDGE ( 'NONE', *, *, #458, .F. ) ;
#209848 = ADVANCED_FACE ( 'NONE', ( #69194 ), #110858, .F. ) ;
#209849 = CARTESIAN_POINT ( 'NONE',  ( 23.25000000000000000, 85.00000000001222134, -146.4170766071767389 ) ) ;
#209850 = CIRCLE ( 'NONE', #97371, 0.09999999999999939493 ) ;
#209851 = CARTESIAN_POINT ( 'NONE',  ( 20.94999999999999929, 70.15000000001266756, -193.3906102602464330 ) ) ;
#209852 = DIRECTION ( 'NONE',  ( 0.000000000000000000, 1.000000000000000000, 0.000000000000000000 ) ) ;
#209853 = ORIENTED_EDGE ( 'NONE', *, *, #217050, .F. ) ;
#209854 = CARTESIAN_POINT ( 'NONE',  ( 18.69999999999998153, 7.986648289447971116, 1.311673547813416718 ) ) ;
#209855 = CIRCLE ( 'NONE', #180812, 0.09999999999999892308 ) ;
#209856 = EDGE_CURVE ( 'NONE', #66925, #110195, #151566, .T. ) ;
#209857 = DIRECTION ( 'NONE',  ( 0.000000000000000000, -6.982962677686266711E-15, 1.000000000000000000 ) ) ;
#209858 = DIRECTION ( 'NONE',  ( 1.000000000000000000, -3.265361837132813093E-16, -2.280189983783949500E-30 ) ) ;
#209859 = ORIENTED_EDGE ( 'NONE', *, *, #9887, .F. ) ;
#209860 = DIRECTION ( 'NONE',  ( 1.000000000000000000, 0.000000000000000000, 0.000000000000000000 ) ) ;
#209861 = AXIS2_PLACEMENT_3D ( 'NONE', #122615, #104292, #182587 ) ;
#209862 = EDGE_CURVE ( 'NONE', #20649, #208696, #239017, .T. ) ;
#209863 = AXIS2_PLACEMENT_3D ( 'NONE', #38210, #198543, #135986 ) ;
#209864 = AXIS2_PLACEMENT_3D ( 'NONE', #33700, #151040, #212305 ) ;
#209865 = ORIENTED_EDGE ( 'NONE', *, *, #31425, .T. ) ;
#209866 = DIRECTION ( 'NONE',  ( 1.000000000000000000, -0.000000000000000000, -0.000000000000000000 ) ) ;
#209867 = DIRECTION ( 'NONE',  ( 0.000000000000000000, 0.9126074666063769270, 0.4088369013363282733 ) ) ;
#209868 = ADVANCED_FACE ( 'NONE', ( #245245 ), #114104, .F. ) ;
#209869 = ORIENTED_EDGE ( 'NONE', *, *, #130214, .T. ) ;
#209870 = ORIENTED_EDGE ( 'NONE', *, *, #180447, .F. ) ;
#209871 = EDGE_CURVE ( 'NONE', #157348, #133253, #14195, .T. ) ;
#209872 = DIRECTION ( 'NONE',  ( 0.000000000000000000, 1.000000000000000000, -8.673617379884042375E-16 ) ) ;
#209873 = ORIENTED_EDGE ( 'NONE', *, *, #85416, .F. ) ;
#209875 = EDGE_LOOP ( 'NONE', ( #52783, #243972, #7402, #10921 ) ) ;
#209874 = CARTESIAN_POINT ( 'NONE',  ( -21.17356465864818205, 6.422803126241717564, 0.09891124101387023526 ) ) ;
#209876 = EDGE_CURVE ( 'NONE', #178487, #93087, #76692, .T. ) ;
#209877 = VERTEX_POINT ( 'NONE', #126574 ) ;
#209880 = ORIENTED_EDGE ( 'NONE', *, *, #113389, .F. ) ;
#209879 = EDGE_LOOP ( 'NONE', ( #97637, #17618, #163498, #153255 ) ) ;
#209878 = DIRECTION ( 'NONE',  ( 0.000000000000000000, -1.000000000000000000, 6.308085367188393199E-16 ) ) ;
#209881 = VECTOR ( 'NONE', #183461, 1000.000000000000000 ) ;
#209882 = VECTOR ( 'NONE', #142748, 1000.000000000000000 ) ;
#209883 = DIRECTION ( 'NONE',  ( -0.000000000000000000, -6.982962677686266711E-15, 1.000000000000000000 ) ) ;
#209884 = ORIENTED_EDGE ( 'NONE', *, *, #88180, .T. ) ;
#209885 = CARTESIAN_POINT ( 'NONE',  ( 20.94999999999999929, 76.00000000001244871, -170.0231074845243597 ) ) ;
#209886 = DIRECTION ( 'NONE',  ( 0.000000000000000000, 0.000000000000000000, -1.000000000000000000 ) ) ;
#209887 = AXIS2_PLACEMENT_3D ( 'NONE', #183788, #62561, #1277 ) ;
#209888 = EDGE_CURVE ( 'NONE', #35113, #12130, #186556, .T. ) ;
#209889 = EDGE_CURVE ( 'NONE', #16939, #111732, #148716, .T. ) ;
#209890 = CARTESIAN_POINT ( 'NONE',  ( 23.24999999999999645, 5.650000000011139001, -188.3499999999999659 ) ) ;
#209891 = CARTESIAN_POINT ( 'NONE',  ( 22.39999999999999503, -0.1008583690875579364, -21.75043287651061164 ) ) ;
#209892 = ORIENTED_EDGE ( 'NONE', *, *, #27039, .T. ) ;
#209893 = VERTEX_POINT ( 'NONE', #28804 ) ;
#209894 = EDGE_LOOP ( 'NONE', ( #227518, #46949, #105122, #89612 ) ) ;
#209895 = EDGE_CURVE ( 'NONE', #109956, #74961, #97947, .T. ) ;
#209896 = CARTESIAN_POINT ( 'NONE',  ( 20.95512820512820440, 8.876151316299271343, -146.1500000000000341 ) ) ;
#209897 = CIRCLE ( 'NONE', #5844, 4.049999999999998934 ) ;
#209899 = ORIENTED_EDGE ( 'NONE', *, *, #138632, .T. ) ;
#209898 = DIRECTION ( 'NONE',  ( -0.000000000000000000, -6.982962677686266711E-15, 1.000000000000000000 ) ) ;
#209900 = FACE_OUTER_BOUND ( 'NONE', #129996, .T. ) ;
#209902 = VERTEX_POINT ( 'NONE', #194280 ) ;
#209901 = DIRECTION ( 'NONE',  ( -1.000000000000000000, 0.000000000000000000, -0.000000000000000000 ) ) ;
#209903 = VERTEX_POINT ( 'NONE', #136832 ) ;
#209904 = EDGE_CURVE ( 'NONE', #105777, #138550, #39137, .T. ) ;
#209905 = CARTESIAN_POINT ( 'NONE',  ( -18.44448725179914916, -0.7332340351039789983, -242.2293278273956787 ) ) ;
#209906 = EDGE_CURVE ( 'NONE', #42311, #184620, #80780, .T. ) ;
#209907 = AXIS2_PLACEMENT_3D ( 'NONE', #150908, #75248, #136448 ) ;
#209908 = CIRCLE ( 'NONE', #89082, 14.30833333333333890 ) ;
#209909 = ORIENTED_EDGE ( 'NONE', *, *, #222378, .F. ) ;
#209910 = VECTOR ( 'NONE', #202240, 1000.000000000000000 ) ;
#209911 = CARTESIAN_POINT ( 'NONE',  ( -20.54999999999999716, 25.30967299857549691, -243.4716794062925374 ) ) ;
#209912 = CARTESIAN_POINT ( 'NONE',  ( -21.05000000000000071, 69.45934304831143891, -203.4231074845244223 ) ) ;
#209914 = ORIENTED_EDGE ( 'NONE', *, *, #165233, .F. ) ;
#209913 = ORIENTED_EDGE ( 'NONE', *, *, #121618, .T. ) ;
#209915 = ORIENTED_EDGE ( 'NONE', *, *, #90270, .T. ) ;
#209916 = CARTESIAN_POINT ( 'NONE',  ( 20.85000000000000142, 1.115600667400684642E-11, -108.3000000000000540 ) ) ;
#209917 = ORIENTED_EDGE ( 'NONE', *, *, #210093, .F. ) ;
#209918 = ORIENTED_EDGE ( 'NONE', *, *, #160358, .F. ) ;
#209919 = DIRECTION ( 'NONE',  ( 0.000000000000000000, 0.000000000000000000, -1.000000000000000000 ) ) ;
#209921 = ORIENTED_EDGE ( 'NONE', *, *, #47205, .F. ) ;
#209920 = CARTESIAN_POINT ( 'NONE',  ( -21.05000000000000071, 67.23127455305835554, -235.8551265064784559 ) ) ;
#209922 = EDGE_CURVE ( 'NONE', #52116, #150942, #247376, .T. ) ;
#209923 = DIRECTION ( 'NONE',  ( 0.000000000000000000, 0.000000000000000000, -1.000000000000000000 ) ) ;
#209924 = VECTOR ( 'NONE', #126296, 1000.000000000000000 ) ;
#209926 = DIRECTION ( 'NONE',  ( -0.000000000000000000, 0.9126074666063770380, 0.4088369013363281068 ) ) ;
#209925 = FACE_BOUND ( 'NONE', #34159, .T. ) ;
#209927 = DIRECTION ( 'NONE',  ( -1.000000000000000000, -0.000000000000000000, -0.000000000000000000 ) ) ;
#209928 = CARTESIAN_POINT ( 'NONE',  ( -14.11697426661281973, 62.02991417940919661, -218.9025163457276335 ) ) ;
#209929 = EDGE_LOOP ( 'NONE', ( #159543, #57544, #231671, #153363 ) ) ;
#209930 = ORIENTED_EDGE ( 'NONE', *, *, #130024, .F. ) ;
#209931 = EDGE_CURVE ( 'NONE', #30344, #228338, #89169, .T. ) ;
#209932 = AXIS2_PLACEMENT_3D ( 'NONE', #184546, #219826, #41229 ) ;
#209933 = CARTESIAN_POINT ( 'NONE',  ( -18.59999999999999787, 70.22659352830977753, -197.9852579278363578 ) ) ;
#209934 = CARTESIAN_POINT ( 'NONE',  ( 18.39999999999997371, 64.52683809664949877, -112.2731074845243739 ) ) ;
#209935 = EDGE_LOOP ( 'NONE', ( #85348, #209418, #131749, #75832 ) ) ;
#209936 = AXIS2_PLACEMENT_3D ( 'NONE', #249050, #225586, #70433 ) ;
#209937 = TOROIDAL_SURFACE ( 'NONE', #55956, 2.100000000000002309, 0.1000000000000000056 ) ;
#209938 = FACE_OUTER_BOUND ( 'NONE', #36138, .T. ) ;
#209939 = TOROIDAL_SURFACE ( 'NONE', #72386, 4.099999999999999645, 0.1000000000000000056 ) ;
#209940 = CARTESIAN_POINT ( 'NONE',  ( -21.14999999999999858, 76.10000000001276987, -215.1726782920691505 ) ) ;
#209941 = ORIENTED_EDGE ( 'NONE', *, *, #98227, .F. ) ;
#209942 = ORIENTED_EDGE ( 'NONE', *, *, #57217, .T. ) ;
#209943 = FACE_OUTER_BOUND ( 'NONE', #247918, .T. ) ;
#209944 = EDGE_CURVE ( 'NONE', #183282, #13885, #112168, .T. ) ;
#209945 = DIRECTION ( 'NONE',  ( 0.000000000000000000, 0.8660254037844352659, -0.5000000000000058842 ) ) ;
#209946 = VERTEX_POINT ( 'NONE', #191715 ) ;
#209947 = DIRECTION ( 'NONE',  ( 1.000000000000000000, -0.000000000000000000, -0.000000000000000000 ) ) ;
#209948 = ORIENTED_EDGE ( 'NONE', *, *, #169063, .T. ) ;
#209949 = DIRECTION ( 'NONE',  ( 0.000000000000000000, 0.000000000000000000, 1.000000000000000000 ) ) ;
#209950 = DIRECTION ( 'NONE',  ( -1.000000000000000000, 0.000000000000000000, 0.000000000000000000 ) ) ;
#209952 = CYLINDRICAL_SURFACE ( 'NONE', #215903, 0.1000000000000028644 ) ;
#209951 = CARTESIAN_POINT ( 'NONE',  ( 21.14999999999999858, 59.07123845373075000, -221.0531397865252075 ) ) ;
#209953 = CARTESIAN_POINT ( 'NONE',  ( 19.97071067695831559, 11.72071067696947644, -91.67625343280374750 ) ) ;
#209954 = DIRECTION ( 'NONE',  ( 0.000000000000000000, 0.000000000000000000, 1.000000000000000000 ) ) ;
#209955 = CARTESIAN_POINT ( 'NONE',  ( -21.05000000000000071, 1.115600667400684642E-11, -129.9000000000000341 ) ) ;
#209956 = FACE_OUTER_BOUND ( 'NONE', #106056, .T. ) ;
#209959 = VERTEX_POINT ( 'NONE', #212547 ) ;
#209958 = AXIS2_PLACEMENT_3D ( 'NONE', #17096, #77037, #250539 ) ;
#209957 = CARTESIAN_POINT ( 'NONE',  ( -22.94999999999999929, 1.885425182446134107, -11.59641995933507808 ) ) ;
#209960 = ADVANCED_FACE ( 'NONE', ( #35214 ), #95148, .T. ) ;
#209961 = CIRCLE ( 'NONE', #155796, 0.5000000000000004441 ) ;
#209962 = VECTOR ( 'NONE', #112722, 1000.000000000000000 ) ;
#209964 = ORIENTED_EDGE ( 'NONE', *, *, #107918, .T. ) ;
#209963 = ORIENTED_EDGE ( 'NONE', *, *, #242814, .T. ) ;
#209965 = ORIENTED_EDGE ( 'NONE', *, *, #35005, .T. ) ;
#209966 = DIRECTION ( 'NONE',  ( -0.7071067811865487940, -0.7071067811865463515, -4.216150419019404490E-15 ) ) ;
#209967 = CARTESIAN_POINT ( 'NONE',  ( 21.30000000000002558, 1.148907358139439339E-11, -201.0000000000015064 ) ) ;
#209968 = CARTESIAN_POINT ( 'NONE',  ( -20.85000000000000142, 77.83585931145600512, -158.5186683157258187 ) ) ;
#209969 = ORIENTED_EDGE ( 'NONE', *, *, #233973, .T. ) ;
#209970 = CARTESIAN_POINT ( 'NONE',  ( 22.60000000000000142, 75.89914163091303578, -81.27267460801371612 ) ) ;
#209971 = VERTEX_POINT ( 'NONE', #18178 ) ;
#209972 = LINE ( 'NONE', #246508, #225071 ) ;
#209973 = CARTESIAN_POINT ( 'NONE',  ( 18.59999999999997655, 7.675662554762638479, -241.7139905447625381 ) ) ;
#209974 = CARTESIAN_POINT ( 'NONE',  ( -21.07954763557448175, 1.580699497018342559, -230.6859858789673297 ) ) ;
#209975 = ORIENTED_EDGE ( 'NONE', *, *, #184151, .F. ) ;
#209976 = DIRECTION ( 'NONE',  ( 0.000000000000000000, 1.000000000000000000, 0.000000000000000000 ) ) ;
#209977 = AXIS2_PLACEMENT_3D ( 'NONE', #114843, #196940, #215231 ) ;
#209978 = CARTESIAN_POINT ( 'NONE',  ( 20.94999999999999574, 6.550000000011159784, -110.3438220896831581 ) ) ;
#209979 = EDGE_LOOP ( 'NONE', ( #209799, #207439, #30411, #65828 ) ) ;
#209980 = EDGE_LOOP ( 'NONE', ( #148303, #137209, #110616, #12710 ) ) ;
#209981 = CYLINDRICAL_SURFACE ( 'NONE', #4033, 0.5000000000000004441 ) ;
#209982 = CARTESIAN_POINT ( 'NONE',  ( 20.94999999999999929, 4.252251777740766236, -211.8999245327126744 ) ) ;
#209983 = CARTESIAN_POINT ( 'NONE',  ( 18.49999999999999289, 15.37733547974377402, -223.0834978222773657 ) ) ;
#209984 = CARTESIAN_POINT ( 'NONE',  ( 23.15000000000000213, 85.00000000001251976, -179.4170766071767389 ) ) ;
#209985 = CYLINDRICAL_SURFACE ( 'NONE', #40192, 12.87499999999999822 ) ;
#209986 = DIRECTION ( 'NONE',  ( 0.000000000000000000, 0.000000000000000000, -1.000000000000000000 ) ) ;
#209987 = ORIENTED_EDGE ( 'NONE', *, *, #67122, .F. ) ;
#209988 = CARTESIAN_POINT ( 'NONE',  ( 23.14999999999999503, 3.801854678198143933, -188.1465607323988252 ) ) ;
#209989 = CARTESIAN_POINT ( 'NONE',  ( 18.59999999999999076, 1.250000000000011546, -8.000000000000000000 ) ) ;
#209991 = CARTESIAN_POINT ( 'NONE',  ( -23.15000000000000213, 76.00000000001213607, -136.5231074845242745 ) ) ;
#209990 = DIRECTION ( 'NONE',  ( -1.836970198721029934E-16, 0.9770955615653316162, 0.2128009952263604232 ) ) ;
#209993 = ADVANCED_FACE ( 'NONE', ( #16908 ), #36488, .F. ) ;
#209992 = DIRECTION ( 'NONE',  ( -1.000000000000000000, -0.000000000000000000, -0.000000000000000000 ) ) ;
#209994 = CARTESIAN_POINT ( 'NONE',  ( -18.39999999999999858, -9.500000000000005329, -7.032069396699667685 ) ) ;
#209995 = DIRECTION ( 'NONE',  ( 1.000000000000000000, 0.000000000000000000, 0.000000000000000000 ) ) ;
#209996 = DIRECTION ( 'NONE',  ( 0.000000000000000000, 0.1568667991644355497, -0.9876197685951332295 ) ) ;
#209997 = TOROIDAL_SURFACE ( 'NONE', #22547, 14.20833333333334103, 0.1000000000000000056 ) ;
#209999 = VERTEX_POINT ( 'NONE', #71751 ) ;
#209998 = DIRECTION ( 'NONE',  ( -1.000000000000000000, -0.000000000000000000, 0.000000000000000000 ) ) ;
#210000 = AXIS2_PLACEMENT_3D ( 'NONE', #11245, #106454, #204289 ) ;
#210001 = AXIS2_PLACEMENT_3D ( 'NONE', #1475, #121467, #200970 ) ;
#210002 = AXIS2_PLACEMENT_3D ( 'NONE', #150926, #12726, #51799 ) ;
#210003 = ADVANCED_FACE ( 'NONE', ( #52154 ), #37766, .T. ) ;
#210004 = DIRECTION ( 'NONE',  ( 1.000000000000000000, 0.000000000000000000, 0.000000000000000000 ) ) ;
#210005 = EDGE_CURVE ( 'NONE', #257831, #215317, #172164, .T. ) ;
#210006 = CARTESIAN_POINT ( 'NONE',  ( -22.49533356619863156, 64.34999999370783996, -103.0882300648471528 ) ) ;
#210008 = PLANE ( 'NONE',  #84114 ) ;
#210007 = AXIS2_PLACEMENT_3D ( 'NONE', #44628, #224534, #241536 ) ;
#210009 = CARTESIAN_POINT ( 'NONE',  ( 20.94999999999999929, 55.49311008795314137, -234.6486875357297492 ) ) ;
#210010 = ADVANCED_FACE ( 'NONE', ( #251654, #73060 ), #232110, .T. ) ;
#210011 = ORIENTED_EDGE ( 'NONE', *, *, #58392, .T. ) ;
#210012 = VECTOR ( 'NONE', #223783, 1000.000000000000000 ) ;
#210013 = DIRECTION ( 'NONE',  ( -1.000000000000000000, 0.000000000000000000, 0.000000000000000000 ) ) ;
#210014 = AXIS2_PLACEMENT_3D ( 'NONE', #27700, #86313, #66787 ) ;
#210015 = CARTESIAN_POINT ( 'NONE',  ( -20.94999999999999929, 5.900000000011102586, -77.21909976465646253 ) ) ;
#210016 = LINE ( 'NONE', #75653, #11491 ) ;
#210017 = AXIS2_PLACEMENT_3D ( 'NONE', #19357, #98850, #257906 ) ;
#210018 = EDGE_CURVE ( 'NONE', #31477, #27216, #143339, .T. ) ;
#210019 = AXIS2_PLACEMENT_3D ( 'NONE', #156835, #131133, #16038 ) ;
#210021 = ORIENTED_EDGE ( 'NONE', *, *, #241049, .F. ) ;
#210020 = EDGE_CURVE ( 'NONE', #117081, #125245, #243280, .T. ) ;
#210022 = DIRECTION ( 'NONE',  ( -3.265361837132813093E-16, 1.000000000000000000, 0.000000000000000000 ) ) ;
#210024 = ORIENTED_EDGE ( 'NONE', *, *, #230952, .F. ) ;
#210023 = CARTESIAN_POINT ( 'NONE',  ( -18.39999999999999858, -9.499999999988849808, -74.03206939669971121 ) ) ;
#210025 = DIRECTION ( 'NONE',  ( 0.000000000000000000, -0.8814952561688437216, 0.4721928772777331806 ) ) ;
#210026 = EDGE_CURVE ( 'NONE', #208807, #178117, #235932, .T. ) ;
#210027 = CARTESIAN_POINT ( 'NONE',  ( 21.05000000000000071, 87.29603075034741266, -133.4752083248603469 ) ) ;
#210028 = ORIENTED_EDGE ( 'NONE', *, *, #133779, .T. ) ;
#210029 = LINE ( 'NONE', #229586, #59444 ) ;
#210030 = AXIS2_PLACEMENT_3D ( 'NONE', #205124, #107326, #147751 ) ;
#210031 = DIRECTION ( 'NONE',  ( 0.000000000000000000, 0.000000000000000000, 1.000000000000000000 ) ) ;
#210033 = DIRECTION ( 'NONE',  ( -1.000000000000000000, -3.265361837132813093E-16, 0.000000000000000000 ) ) ;
#210032 = AXIS2_PLACEMENT_3D ( 'NONE', #178027, #188279, #205261 ) ;
#210035 = AXIS2_PLACEMENT_3D ( 'NONE', #7083, #65780, #202717 ) ;
#210034 = DIRECTION ( 'NONE',  ( 1.000000000000000000, 0.000000000000000000, 0.000000000000000000 ) ) ;
#210037 = EDGE_CURVE ( 'NONE', #242320, #95060, #164381, .T. ) ;
#210036 = FACE_OUTER_BOUND ( 'NONE', #122537, .T. ) ;
#210038 = VERTEX_POINT ( 'NONE', #217633 ) ;
#210039 = DIRECTION ( 'NONE',  ( 1.000000000000000000, 0.000000000000000000, 0.000000000000000000 ) ) ;
#210040 = DIRECTION ( 'NONE',  ( 1.000000000000000000, 0.000000000000000000, 0.000000000000000000 ) ) ;
#210041 = AXIS2_PLACEMENT_3D ( 'NONE', #98165, #115201, #55189 ) ;
#210042 = AXIS2_PLACEMENT_3D ( 'NONE', #176822, #257561, #132551 ) ;
#210043 = CARTESIAN_POINT ( 'NONE',  ( -21.05000000000000071, 1.115600667400684642E-11, -200.9999999999999432 ) ) ;
#210044 = EDGE_LOOP ( 'NONE', ( #41852, #19967, #68754, #149162 ) ) ;
#210045 = VERTEX_POINT ( 'NONE', #101528 ) ;
#210046 = VECTOR ( 'NONE', #212418, 1000.000000000000000 ) ;
#210047 = CARTESIAN_POINT ( 'NONE',  ( -23.15000000000000213, -11.64999999998884483, -164.4000000000000057 ) ) ;
#210048 = AXIS2_PLACEMENT_3D ( 'NONE', #209798, #211076, #69018 ) ;
#210049 = ADVANCED_FACE ( 'NONE', ( #39046 ), #100251, .T. ) ;
#210050 = DIRECTION ( 'NONE',  ( 0.000000000000000000, 0.2617529984165031243, 0.9651348961777157509 ) ) ;
#210051 = DIRECTION ( 'NONE',  ( 1.000000000000000000, -1.836970198721029934E-16, -1.282749433769087582E-30 ) ) ;
#210052 = LINE ( 'NONE', #31435, #128433 ) ;
#210054 = CARTESIAN_POINT ( 'NONE',  ( 22.49806830649814060, -2.403418073154200307, -189.6004600419238102 ) ) ;
#210053 = DIRECTION ( 'NONE',  ( 1.000000000000000000, 0.000000000000000000, 0.000000000000000000 ) ) ;
#210055 = CARTESIAN_POINT ( 'NONE',  ( -21.07971444708686093, 75.91217656369460087, -176.3528995661508816 ) ) ;
#210056 = CARTESIAN_POINT ( 'NONE',  ( -17.78241384941120629, 65.14442424719840119, -113.2721451569643278 ) ) ;
#210057 = CARTESIAN_POINT ( 'NONE',  ( -21.64999999999999858, 9.788464569039593499, -211.4053333142630891 ) ) ;
#210058 = ORIENTED_EDGE ( 'NONE', *, *, #159570, .T. ) ;
#210060 = ORIENTED_EDGE ( 'NONE', *, *, #140570, .F. ) ;
#210059 = CARTESIAN_POINT ( 'NONE',  ( -23.15000000000000213, 1.115600667400684642E-11, -200.9999999999999432 ) ) ;
#210061 = DIRECTION ( 'NONE',  ( 1.000000000000000000, 0.000000000000000000, 0.000000000000000000 ) ) ;
#210062 = CARTESIAN_POINT ( 'NONE',  ( -21.11101077989000174, -1.352031336145134821, -194.7201934363683904 ) ) ;
#210063 = CARTESIAN_POINT ( 'NONE',  ( -18.50000000000000000, 102.4393534156134962, -185.3815988770167280 ) ) ;
#210064 = EDGE_CURVE ( 'NONE', #182665, #170158, #41619, .T. ) ;
#210065 = ORIENTED_EDGE ( 'NONE', *, *, #148272, .T. ) ;
#210066 = CARTESIAN_POINT ( 'NONE',  ( -16.88005004766534967, 66.04989949669095495, -115.6727713725756104 ) ) ;
#210067 = CARTESIAN_POINT ( 'NONE',  ( 21.13736287352038445, 8.046642376395153562, -154.8500000000000227 ) ) ;
#210068 = DIRECTION ( 'NONE',  ( 0.000000000000000000, 0.2128009952263568427, -0.9770955615653323934 ) ) ;
#210069 = ORIENTED_EDGE ( 'NONE', *, *, #174193, .T. ) ;
#210070 = EDGE_LOOP ( 'NONE', ( #165205, #40519, #73904, #130263 ) ) ;
#210071 = VECTOR ( 'NONE', #53770, 1000.000000000000000 ) ;
#210072 = CIRCLE ( 'NONE', #181027, 0.1000000000000028644 ) ;
#210073 = DIRECTION ( 'NONE',  ( 0.000000000000000000, 0.000000000000000000, -1.000000000000000000 ) ) ;
#210074 = ORIENTED_EDGE ( 'NONE', *, *, #56654, .T. ) ;
#210075 = CARTESIAN_POINT ( 'NONE',  ( 20.12500000000000000, 59.94448977088796937, -225.4740812377367263 ) ) ;
#210076 = CIRCLE ( 'NONE', #172516, 0.09999999999999918676 ) ;
#210077 = ADVANCED_FACE ( 'NONE', ( #20767 ), #200673, .T. ) ;
#210078 = CARTESIAN_POINT ( 'NONE',  ( 21.05000000000000071, 10.72371710471867701, -141.6649135690876165 ) ) ;
#210079 = CARTESIAN_POINT ( 'NONE',  ( 21.05000000000000071, 8.815201804577958100, -142.4205374966838633 ) ) ;
#210080 = VECTOR ( 'NONE', #243802, 1000.000000000000000 ) ;
#210081 = AXIS2_PLACEMENT_3D ( 'NONE', #179501, #238154, #256382 ) ;
#210082 = CARTESIAN_POINT ( 'NONE',  ( 21.00000000000000000, 6.258114003436813455, 11.90000000000000036 ) ) ;
#210083 = ORIENTED_EDGE ( 'NONE', *, *, #230098, .T. ) ;
#210084 = DIRECTION ( 'NONE',  ( 0.000000000000000000, 0.000000000000000000, -1.000000000000000000 ) ) ;
#210086 = EDGE_CURVE ( 'NONE', #83940, #13313, #19472, .T. ) ;
#210085 =( BOUNDED_CURVE ( )  B_SPLINE_CURVE ( 3, ( #231758, #53098, #33594, #13992 ),
 .UNSPECIFIED., .F., .F. ) 
 B_SPLINE_CURVE_WITH_KNOTS ( ( 4, 4 ),
 ( 4.712388980384689674, 6.231880751915386263 ),
 .UNSPECIFIED. ) 
 CURVE ( )  GEOMETRIC_REPRESENTATION_ITEM ( )  RATIONAL_B_SPLINE_CURVE ( ( 1.000000000000000000, 0.8166740347213228279, 0.8166740347213228279, 1.000000000000000000 ) ) 
 REPRESENTATION_ITEM ( '' )  );
#210087 = AXIS2_PLACEMENT_3D ( 'NONE', #130838, #151723, #74762 ) ;
#210088 = CARTESIAN_POINT ( 'NONE',  ( -20.85000000000000142, -1.135018845899022466, -108.2169768834323662 ) ) ;
#210090 = AXIS2_PLACEMENT_3D ( 'NONE', #11092, #71079, #115312 ) ;
#210089 = CARTESIAN_POINT ( 'NONE',  ( -18.50000324121759121, 68.00468331834514402, -224.2298952291173464 ) ) ;
#210091 = ADVANCED_FACE ( 'NONE', ( #3748 ), #123708, .T. ) ;
#210092 = DIRECTION ( 'NONE',  ( 1.000000000000000000, 0.000000000000000000, 0.000000000000000000 ) ) ;
#210093 = EDGE_CURVE ( 'NONE', #203266, #235855, #1158, .T. ) ;
#210095 = AXIS2_PLACEMENT_3D ( 'NONE', #62210, #218689, #242115 ) ;
#210094 = CARTESIAN_POINT ( 'NONE',  ( -23.15000000000000213, 11.75000000001115552, -79.25000000000004263 ) ) ;
#210096 = DIRECTION ( 'NONE',  ( -1.000000000000000000, 0.000000000000000000, 0.000000000000000000 ) ) ;
#210097 = TOROIDAL_SURFACE ( 'NONE', #39422, 0.2000000000000000111, 0.1000000000000000056 ) ;
#210098 = CARTESIAN_POINT ( 'NONE',  ( -16.85722902420161518, 66.05000000001224691, -149.2886549582941882 ) ) ;
#210099 = ORIENTED_EDGE ( 'NONE', *, *, #92914, .T. ) ;
#210101 = CARTESIAN_POINT ( 'NONE',  ( 21.14999999999999858, 69.45000000001205365, -124.1731074845243370 ) ) ;
#210100 = DIRECTION ( 'NONE',  ( -0.000000000000000000, 0.4721928772777345684, 0.8814952561688429444 ) ) ;
#210102 = ORIENTED_EDGE ( 'NONE', *, *, #46101, .T. ) ;
#210104 = VERTEX_POINT ( 'NONE', #42879 ) ;
#210103 = CARTESIAN_POINT ( 'NONE',  ( -18.69999999999999929, 1.350000000000000089, 16.50000000000000000 ) ) ;
#210105 = VERTEX_POINT ( 'NONE', #83255 ) ;
#210106 = CARTESIAN_POINT ( 'NONE',  ( 22.59999999999999432, 12.61936297652653138, -223.3443501630868298 ) ) ;
#210107 = CARTESIAN_POINT ( 'NONE',  ( -18.39999999999999858, 11.47316190337363828, -176.7998292484659544 ) ) ;
#210108 = FACE_OUTER_BOUND ( 'NONE', #26325, .T. ) ;
#210109 = EDGE_CURVE ( 'NONE', #92384, #103375, #23347, .T. ) ;
#210110 = CARTESIAN_POINT ( 'NONE',  ( 20.95595012432474391, 65.39582078693574374, -128.9273381543061134 ) ) ;
#210111 = ORIENTED_EDGE ( 'NONE', *, *, #163657, .T. ) ;
#210112 = DIRECTION ( 'NONE',  ( 1.000000000000000000, 0.000000000000000000, 0.000000000000000000 ) ) ;
#210114 = DIRECTION ( 'NONE',  ( -1.000000000000000000, 0.000000000000000000, 0.000000000000000000 ) ) ;
#210113 = CIRCLE ( 'NONE', #110128, 0.1000000000000028644 ) ;
#210115 = VERTEX_POINT ( 'NONE', #238505 ) ;
#210116 = CARTESIAN_POINT ( 'NONE',  ( 18.39999999999999858, -9.682403433465241349, -73.65684337741279819 ) ) ;
#210117 = TOROIDAL_SURFACE ( 'NONE', #126893, 0.2000000000000000111, 0.1000000000000000056 ) ;
#210118 = CARTESIAN_POINT ( 'NONE',  ( -23.25000000000000000, 84.59626168225486254, -93.57297996737396772 ) ) ;
#210119 = VERTEX_POINT ( 'NONE', #138105 ) ;
#210120 = CARTESIAN_POINT ( 'NONE',  ( -23.25000000000000000, 64.25000000001199396, -115.1731074845243938 ) ) ;
#210121 = VECTOR ( 'NONE', #255391, 1000.000000000000114 ) ;
#210122 = AXIS2_PLACEMENT_3D ( 'NONE', #207012, #28414, #32248 ) ;
#210123 = EDGE_LOOP ( 'NONE', ( #12928, #161832, #128840, #91437 ) ) ;
#210124 = DIRECTION ( 'NONE',  ( 1.000000000000000000, 0.000000000000000000, 0.000000000000000000 ) ) ;
#210125 = ORIENTED_EDGE ( 'NONE', *, *, #224833, .T. ) ;
#210126 = CARTESIAN_POINT ( 'NONE',  ( -20.64999999999999858, 9.712035112405693837, -211.5243229699422614 ) ) ;
#210127 = EDGE_CURVE ( 'NONE', #116639, #192753, #61156, .T. ) ;
#210128 = CYLINDRICAL_SURFACE ( 'NONE', #94032, 0.1000000000000028644 ) ;
#210129 = LINE ( 'NONE', #53610, #110034 ) ;
#210130 = EDGE_CURVE ( 'NONE', #157985, #105911, #42120, .T. ) ;
#210131 = DIRECTION ( 'NONE',  ( -2.952720810173289112E-16, 1.000000000000000000, -0.000000000000000000 ) ) ;
#210132 = EDGE_CURVE ( 'NONE', #233325, #24291, #39517, .T. ) ;
#210133 = DIRECTION ( 'NONE',  ( 0.000000000000000000, 6.982962677686266711E-15, -1.000000000000000000 ) ) ;
#210134 = LINE ( 'NONE', #172327, #223663 ) ;
#210135 = CARTESIAN_POINT ( 'NONE',  ( -21.04999999999999716, -7.883686024897174072, -209.9138933503092233 ) ) ;
#210136 = ORIENTED_EDGE ( 'NONE', *, *, #54620, .F. ) ;
#210137 = TOROIDAL_SURFACE ( 'NONE', #5905, 0.2000000000000000111, 0.1000000000000000056 ) ;
#210138 = DIRECTION ( 'NONE',  ( 1.652117596168391700E-15, -1.000000000000000000, -6.982962677686266711E-15 ) ) ;
#210139 = EDGE_LOOP ( 'NONE', ( #216868, #198507, #94092 ) ) ;
#210140 = DIRECTION ( 'NONE',  ( -1.073024830501117725E-15, 0.000000000000000000, -1.000000000000000000 ) ) ;
#210141 = ORIENTED_EDGE ( 'NONE', *, *, #229381, .T. ) ;
#210142 = CARTESIAN_POINT ( 'NONE',  ( 23.24999999999999645, 64.25000000001182343, -82.17310748452440805 ) ) ;
#210143 = CARTESIAN_POINT ( 'NONE',  ( -21.07946286933445279, 6.329037319007698947, 0.07668384325640564825 ) ) ;
#210144 = DIRECTION ( 'NONE',  ( 1.000000000000000000, 0.000000000000000000, 0.000000000000000000 ) ) ;
#210145 = DIRECTION ( 'NONE',  ( -1.000000000000000000, -0.000000000000000000, 0.000000000000000000 ) ) ;
#210146 = VECTOR ( 'NONE', #48385, 1000.000000000000114 ) ;
#210147 = VERTEX_POINT ( 'NONE', #78134 ) ;
#210149 = ORIENTED_EDGE ( 'NONE', *, *, #83939, .F. ) ;
#210148 = CYLINDRICAL_SURFACE ( 'NONE', #103711, 0.09999999999999939493 ) ;
#210151 = CARTESIAN_POINT ( 'NONE',  ( -20.64999999999999858, 4.350000000011156054, -54.75000000000000000 ) ) ;
#210150 = CARTESIAN_POINT ( 'NONE',  ( -33.72168855820451938, 22.97806745954237684, -230.9350634111225986 ) ) ;
#210153 = ORIENTED_EDGE ( 'NONE', *, *, #131242, .F. ) ;
#210152 = DIRECTION ( 'NONE',  ( 0.000000000000000000, -1.000000000000000000, -0.000000000000000000 ) ) ;
#210154 = EDGE_LOOP ( 'NONE', ( #217091, #206251, #93680, #130336 ) ) ;
#210155 = EDGE_CURVE ( 'NONE', #110447, #79096, #118610, .T. ) ;
#210156 = DIRECTION ( 'NONE',  ( 1.000000000000000000, 0.000000000000000000, 0.000000000000000000 ) ) ;
#210157 = TOROIDAL_SURFACE ( 'NONE', #198233, 0.2000000000000000111, 0.1000000000000000056 ) ;
#210158 = AXIS2_PLACEMENT_3D ( 'NONE', #90480, #30539, #228738 ) ;
#210159 = DIRECTION ( 'NONE',  ( 1.000000000000000000, -7.304098846218135653E-16, -2.111765289898286048E-31 ) ) ;
#210160 = ORIENTED_EDGE ( 'NONE', *, *, #58741, .T. ) ;
#210161 = CARTESIAN_POINT ( 'NONE',  ( 20.99999999999999645, 66.25000000001256240, -182.6731074845244223 ) ) ;
#210162 = EDGE_LOOP ( 'NONE', ( #254533, #189084, #26041, #50136 ) ) ;
#210163 = ADVANCED_FACE ( 'NONE', ( #218934 ), #239807, .T. ) ;
#210164 = DIRECTION ( 'NONE',  ( -3.265361837132813093E-16, -0.4088369013363283844, 0.9126074666063769270 ) ) ;
#210165 = DIRECTION ( 'NONE',  ( 0.000000000000000000, 0.000000000000000000, -1.000000000000000000 ) ) ;
#210166 = ORIENTED_EDGE ( 'NONE', *, *, #168381, .F. ) ;
#210167 = FACE_OUTER_BOUND ( 'NONE', #232303, .T. ) ;
#210168 = ADVANCED_FACE ( 'NONE', ( #80697 ), #160288, .F. ) ;
#210169 = EDGE_CURVE ( 'NONE', #104858, #113005, #180944, .T. ) ;
#210170 = ORIENTED_EDGE ( 'NONE', *, *, #191610, .T. ) ;
#210171 = AXIS2_PLACEMENT_3D ( 'NONE', #103983, #239680, #41495 ) ;
#210172 = CARTESIAN_POINT ( 'NONE',  ( -21.64999999999999858, 7.250000000011148416, -155.1500000000000057 ) ) ;
#210173 = CIRCLE ( 'NONE', #97710, 0.1000000000000028644 ) ;
#210174 = CIRCLE ( 'NONE', #39315, 2.000000000000001776 ) ;
#210175 = AXIS2_PLACEMENT_3D ( 'NONE', #111616, #191174, #193724 ) ;
#210176 = ADVANCED_FACE ( 'NONE', ( #27201 ), #88393, .F. ) ;
#210177 = VERTEX_POINT ( 'NONE', #165400 ) ;
#210178 = VERTEX_POINT ( 'NONE', #6302 ) ;
#210181 = EDGE_CURVE ( 'NONE', #197069, #163468, #45444, .T. ) ;
#210180 = EDGE_CURVE ( 'NONE', #68928, #162856, #204504, .T. ) ;
#210179 = CARTESIAN_POINT ( 'NONE',  ( 20.22483756094572271, 18.79053017939081016, -229.2002498143492346 ) ) ;
#210182 = ORIENTED_EDGE ( 'NONE', *, *, #197262, .T. ) ;
#210183 = DIRECTION ( 'NONE',  ( 0.000000000000000000, -1.000000000000000000, 0.000000000000000000 ) ) ;
#210184 = ORIENTED_EDGE ( 'NONE', *, *, #230553, .F. ) ;
#210186 = ORIENTED_EDGE ( 'NONE', *, *, #106408, .T. ) ;
#210185 = DIRECTION ( 'NONE',  ( -2.940209281316618057E-16, 0.4721928772777342354, 0.8814952561688433885 ) ) ;
#210187 = ORIENTED_EDGE ( 'NONE', *, *, #68702, .T. ) ;
#210188 = CARTESIAN_POINT ( 'NONE',  ( 18.49999999999999645, 1.637172712970381694, -11.58215336547201879 ) ) ;
#210189 = EDGE_LOOP ( 'NONE', ( #236894, #197136, #4505, #70842 ) ) ;
#210192 = VERTEX_POINT ( 'NONE', #229227 ) ;
#210191 = ORIENTED_EDGE ( 'NONE', *, *, #207734, .T. ) ;
#210190 = DIRECTION ( 'NONE',  ( 0.000000000000000000, 0.000000000000000000, -1.000000000000000000 ) ) ;
#210193 = DIRECTION ( 'NONE',  ( 0.000000000000000000, -7.056502275159890043E-15, 1.000000000000000000 ) ) ;
#210194 = ORIENTED_EDGE ( 'NONE', *, *, #204201, .T. ) ;
#210195 = AXIS2_PLACEMENT_3D ( 'NONE', #162792, #138061, #118541 ) ;
#210196 = ADVANCED_FACE ( 'NONE', ( #107987, #147093, #126252 ), #188799, .F. ) ;
#210197 = EDGE_CURVE ( 'NONE', #99817, #110542, #205880, .T. ) ;
#210198 = AXIS2_PLACEMENT_3D ( 'NONE', #101723, #19665, #180025 ) ;
#210199 = CIRCLE ( 'NONE', #147642, 0.6000000000000033085 ) ;
#210200 = DIRECTION ( 'NONE',  ( 1.000000000000000000, -2.849773892568378313E-16, 7.728835255496647986E-17 ) ) ;
#210201 = CIRCLE ( 'NONE', #214287, 0.1000000000000053069 ) ;
#210202 = ORIENTED_EDGE ( 'NONE', *, *, #112127, .F. ) ;
#210203 = EDGE_CURVE ( 'NONE', #61669, #134771, #66298, .T. ) ;
#210204 = CARTESIAN_POINT ( 'NONE',  ( -16.94445028196807002, 9.992063609708893068, -154.8926698215815634 ) ) ;
#210206 = ORIENTED_EDGE ( 'NONE', *, *, #1964, .F. ) ;
#210205 = CARTESIAN_POINT ( 'NONE',  ( 23.14999999999999858, 72.10000000001214460, -136.5231074845243597 ) ) ;
#210207 = DIRECTION ( 'NONE',  ( 0.000000000000000000, 0.000000000000000000, -1.000000000000000000 ) ) ;
#210208 = ORIENTED_EDGE ( 'NONE', *, *, #221025, .F. ) ;
#210209 = CARTESIAN_POINT ( 'NONE',  ( 21.05000000000000071, 61.88149656937974896, -248.1136133839584090 ) ) ;
#210210 = DIRECTION ( 'NONE',  ( 1.000000000000000000, 0.000000000000000000, 0.000000000000000000 ) ) ;
#210211 = ORIENTED_EDGE ( 'NONE', *, *, #171698, .F. ) ;
#210212 = AXIS2_PLACEMENT_3D ( 'NONE', #14152, #152380, #134057 ) ;
#210214 = EDGE_CURVE ( 'NONE', #227883, #163431, #210174, .T. ) ;
#210213 = FACE_OUTER_BOUND ( 'NONE', #39585, .T. ) ;
#210215 = CARTESIAN_POINT ( 'NONE',  ( 18.39999999999999503, 56.47972699439914379, -234.4806356575134885 ) ) ;
#210216 = AXIS2_PLACEMENT_3D ( 'NONE', #28975, #148885, #108462 ) ;
#210217 = ORIENTED_EDGE ( 'NONE', *, *, #234766, .T. ) ;
#210218 = ADVANCED_FACE ( 'NONE', ( #68877 ), #164119, .F. ) ;
#210220 = VERTEX_POINT ( 'NONE', #243640 ) ;
#210219 = CARTESIAN_POINT ( 'NONE',  ( 20.00000000000000000, 54.35086488289007889, -228.7501953506800589 ) ) ;
#210221 = AXIS2_PLACEMENT_3D ( 'NONE', #27697, #49782, #47195 ) ;
#210222 = CARTESIAN_POINT ( 'NONE',  ( -23.15000000000000213, 11.65000000001115588, -93.48519422934610645 ) ) ;
#210225 = ORIENTED_EDGE ( 'NONE', *, *, #146693, .T. ) ;
#210224 = ORIENTED_EDGE ( 'NONE', *, *, #249421, .F. ) ;
#210223 = CIRCLE ( 'NONE', #164428, 0.09999999999999395484 ) ;
#210226 = ORIENTED_EDGE ( 'NONE', *, *, #131211, .T. ) ;
#210227 = DIRECTION ( 'NONE',  ( 1.000000000000000000, -0.000000000000000000, -0.000000000000000000 ) ) ;
#210228 = ORIENTED_EDGE ( 'NONE', *, *, #106334, .F. ) ;
#210229 = ORIENTED_EDGE ( 'NONE', *, *, #100628, .F. ) ;
#210230 = CARTESIAN_POINT ( 'NONE',  ( -20.94999999999999929, 18.18127959618848877, -237.5711165786817389 ) ) ;
#210231 = EDGE_LOOP ( 'NONE', ( #92266, #169848, #57844, #106850 ) ) ;
#210232 = EDGE_CURVE ( 'NONE', #207855, #121700, #166709, .T. ) ;
#210233 = CARTESIAN_POINT ( 'NONE',  ( 23.24999999999999289, 45.02833974712562792, -238.5149546970766892 ) ) ;
#210234 = TOROIDAL_SURFACE ( 'NONE', #189377, 4.099999999999999645, 0.1000000000000000056 ) ;
#210235 = VECTOR ( 'NONE', #106497, 1000.000000000000000 ) ;
#210236 = DIRECTION ( 'NONE',  ( -1.000000000000000000, -0.000000000000000000, -0.000000000000000000 ) ) ;
#210237 = ORIENTED_EDGE ( 'NONE', *, *, #29430, .T. ) ;
#210238 = EDGE_LOOP ( 'NONE', ( #214545, #251221, #187478, #195797 ) ) ;
#210239 = EDGE_CURVE ( 'NONE', #235746, #30238, #151752, .T. ) ;
#210240 = DIRECTION ( 'NONE',  ( 1.186688945009009831E-16, -1.000000000000000000, 0.000000000000000000 ) ) ;
#210241 = ORIENTED_EDGE ( 'NONE', *, *, #72850, .F. ) ;
#210242 = DIRECTION ( 'NONE',  ( 0.000000000000000000, 0.000000000000000000, -1.000000000000000000 ) ) ;
#210243 = EDGE_LOOP ( 'NONE', ( #209302, #17696, #35476, #227064, #57134, #37282, #216235, #132945, #130881, #138890 ) ) ;
#210244 = ADVANCED_FACE ( 'NONE', ( #207095 ), #239198, .T. ) ;
#210246 = VERTEX_POINT ( 'NONE', #167995 ) ;
#210245 = CARTESIAN_POINT ( 'NONE',  ( -21.04999999999999716, -9.599999999988844124, -141.0320693966996828 ) ) ;
#210247 = CARTESIAN_POINT ( 'NONE',  ( 21.07928932188134397, 0.09889514566555242248, -127.6714833436067238 ) ) ;
#210248 = LINE ( 'NONE', #51128, #189284 ) ;
#210249 = LINE ( 'NONE', #113700, #27160 ) ;
#210250 = CARTESIAN_POINT ( 'NONE',  ( -20.85000000000000142, -1.835859311432481045, -145.5044391687985694 ) ) ;
#210251 = LINE ( 'NONE', #131978, #77831 ) ;
#210252 = CARTESIAN_POINT ( 'NONE',  ( -16.87435696428308063, 66.04999753708007404, -157.3731157193578554 ) ) ;
#210253 = FACE_OUTER_BOUND ( 'NONE', #168451, .T. ) ;
#210254 = CARTESIAN_POINT ( 'NONE',  ( -23.15000000000000213, 73.50000000001156764, -56.29848556176223440 ) ) ;
#210255 = FACE_OUTER_BOUND ( 'NONE', #219298, .T. ) ;
#210256 = AXIS2_PLACEMENT_3D ( 'NONE', #212407, #254069, #155011 ) ;
#210257 = DIRECTION ( 'NONE',  ( 4.026293107431335996E-15, 0.8700118002898393765, -0.4930308989875104575 ) ) ;
#210258 = TOROIDAL_SURFACE ( 'NONE', #231114, 0.4000000000000003553, 0.1000000000000000056 ) ;
#210259 = ORIENTED_EDGE ( 'NONE', *, *, #42406, .F. ) ;
#210260 = AXIS2_PLACEMENT_3D ( 'NONE', #52659, #132211, #194779 ) ;
#210261 = EDGE_LOOP ( 'NONE', ( #240438, #25735, #88641, #133628 ) ) ;
#210262 = CIRCLE ( 'NONE', #118688, 11.74999999999999645 ) ;
#210264 = EDGE_LOOP ( 'NONE', ( #240338, #163680, #151816, #241098 ) ) ;
#210263 = CARTESIAN_POINT ( 'NONE',  ( 20.99999999999999645, 9.749999999999982236, -12.65000000000000568 ) ) ;
#210265 = ORIENTED_EDGE ( 'NONE', *, *, #54254, .F. ) ;
#210266 = CARTESIAN_POINT ( 'NONE',  ( -16.89268316805465986, 9.951721813253337601, -87.85575247854558256 ) ) ;
#210267 = CARTESIAN_POINT ( 'NONE',  ( 20.97565083910961548, 10.47461740128996510, -141.5779431765885477 ) ) ;
#210269 = DIRECTION ( 'NONE',  ( 1.000000000000000000, 0.000000000000000000, 0.000000000000000000 ) ) ;
#210268 = DIRECTION ( 'NONE',  ( 1.000000000000000000, 0.000000000000000000, 0.000000000000000000 ) ) ;
#210270 = VERTEX_POINT ( 'NONE', #49288 ) ;
#210272 = ORIENTED_EDGE ( 'NONE', *, *, #65909, .F. ) ;
#210271 = VECTOR ( 'NONE', #147733, 1000.000000000000000 ) ;
#210273 = CARTESIAN_POINT ( 'NONE',  ( -22.39999999999999858, 0.1000000000111554016, -25.70922040162659883 ) ) ;
#210274 = AXIS2_PLACEMENT_3D ( 'NONE', #103018, #185142, #224256 ) ;
#210275 = DIRECTION ( 'NONE',  ( 0.000000000000000000, 0.000000000000000000, 1.000000000000000000 ) ) ;
#210276 = VERTEX_POINT ( 'NONE', #244923 ) ;
#210277 = ORIENTED_EDGE ( 'NONE', *, *, #13793, .T. ) ;
#210278 = CARTESIAN_POINT ( 'NONE',  ( -20.95000000000000284, 11.65000000001115232, -160.4851942293460638 ) ) ;
#210279 = CARTESIAN_POINT ( 'NONE',  ( 23.25000000000000000, -7.274670914976375968, -212.7102428701827250 ) ) ;
#210280 = DIRECTION ( 'NONE',  ( 1.000000000000000000, 0.000000000000000000, 0.000000000000000000 ) ) ;
#210281 = FACE_OUTER_BOUND ( 'NONE', #157020, .T. ) ;
#210283 = EDGE_LOOP ( 'NONE', ( #376, #124999, #51193, #180869 ) ) ;
#210282 = DIRECTION ( 'NONE',  ( -3.440080580676165868E-14, 0.1298341882520054891, 0.9915357197604850459 ) ) ;
#210284 = CIRCLE ( 'NONE', #247868, 11.75000000000000000 ) ;
#210285 = DIRECTION ( 'NONE',  ( 0.000000000000000000, -0.8660254037844343777, 0.5000000000000074385 ) ) ;
#210286 = DIRECTION ( 'NONE',  ( 0.000000000000000000, -0.3116596277708331142, -0.9501938099239259916 ) ) ;
#210287 = CARTESIAN_POINT ( 'NONE',  ( -18.59999999999999787, 77.16412189325258453, -28.20825939895270551 ) ) ;
#210288 = CARTESIAN_POINT ( 'NONE',  ( 18.43473516226078956, 85.49494228277008290, -95.97720880117476838 ) ) ;
#210289 = ORIENTED_EDGE ( 'NONE', *, *, #216011, .F. ) ;
#210290 = LINE ( 'NONE', #31672, #69652 ) ;
#210291 = DIRECTION ( 'NONE',  ( 0.000000000000000000, -1.000000000000000000, -2.891205793294679805E-16 ) ) ;
#210293 = DIRECTION ( 'NONE',  ( 0.000000000000000000, -0.000000000000000000, 1.000000000000000000 ) ) ;
#210292 = LINE ( 'NONE', #107316, #161766 ) ;
#210295 = ADVANCED_FACE ( 'NONE', ( #128843 ), #122700, .F. ) ;
#210294 = DIRECTION ( 'NONE',  ( 1.000000000000000000, 0.000000000000000000, 0.000000000000000000 ) ) ;
#210296 = CARTESIAN_POINT ( 'NONE',  ( -16.89935556175728237, 9.950000000011009149, -53.86032363711485971 ) ) ;
#210297 = CARTESIAN_POINT ( 'NONE',  ( -16.94445028196807002, 9.992063609708893068, -121.3926698215815918 ) ) ;
#210298 = CARTESIAN_POINT ( 'NONE',  ( -23.15000000000000213, 85.60000000001203091, -114.7731074845242460 ) ) ;
#210299 = CYLINDRICAL_SURFACE ( 'NONE', #113256, 4.049999999999998934 ) ;
#210300 = LINE ( 'NONE', #90322, #189172 ) ;
#210302 = ORIENTED_EDGE ( 'NONE', *, *, #87822, .T. ) ;
#210301 = TOROIDAL_SURFACE ( 'NONE', #160432, 0.2000000000000000111, 0.1000000000000000056 ) ;
#210303 = AXIS2_PLACEMENT_3D ( 'NONE', #191818, #32754, #112266 ) ;
#210304 = ORIENTED_EDGE ( 'NONE', *, *, #122609, .F. ) ;
#210305 = ORIENTED_EDGE ( 'NONE', *, *, #200378, .F. ) ;
#210306 = CARTESIAN_POINT ( 'NONE',  ( 20.96937028524354929, 65.37553062838524909, -95.53168138335472293 ) ) ;
#210307 = CARTESIAN_POINT ( 'NONE',  ( 21.05000000000000071, 20.97908333644147660, -233.6079013178409411 ) ) ;
#210308 = VERTEX_POINT ( 'NONE', #70170 ) ;
#210309 = EDGE_CURVE ( 'NONE', #182530, #73622, #163110, .T. ) ;
#210310 = EDGE_CURVE ( 'NONE', #215160, #96910, #222603, .T. ) ;
#210311 = EDGE_LOOP ( 'NONE', ( #3609, #220764, #172896, #239415 ) ) ;
#210312 =( NAMED_UNIT ( * ) SI_UNIT ( $, .STERADIAN. ) SOLID_ANGLE_UNIT ( ) );
#210313 = EDGE_LOOP ( 'NONE', ( #52245, #226972, #235553, #26060 ) ) ;
#210314 = CARTESIAN_POINT ( 'NONE',  ( -21.65000000000000213, 7.249999999999984013, -12.65000000000000213 ) ) ;
#210315 = AXIS2_PLACEMENT_3D ( 'NONE', #140311, #179481, #55621 ) ;
#210316 = ORIENTED_EDGE ( 'NONE', *, *, #249016, .F. ) ;
#210317 = CARTESIAN_POINT ( 'NONE',  ( 23.24999999999999289, 11.65000000001116298, -188.8499999999999659 ) ) ;
#210318 = CARTESIAN_POINT ( 'NONE',  ( -16.77683809663752257, 30.19206623356022234, -234.8041291499450551 ) ) ;
#210319 = DIRECTION ( 'NONE',  ( 0.000000000000000000, 0.2128009952263606452, -0.9770955615653313941 ) ) ;
#210320 = ADVANCED_FACE ( 'NONE', ( #191406 ), #234338, .T. ) ;
#210321 = VECTOR ( 'NONE', #152358, 1000.000000000000000 ) ;
#210322 = CARTESIAN_POINT ( 'NONE',  ( -21.14999999999999858, 6.540656951712397138, -67.00000000000004263 ) ) ;
#210323 = EDGE_CURVE ( 'NONE', #45147, #160776, #255902, .T. ) ;
#210324 = DIRECTION ( 'NONE',  ( 1.000000000000000000, -0.000000000000000000, -0.000000000000000000 ) ) ;
#210326 = ORIENTED_EDGE ( 'NONE', *, *, #102024, .F. ) ;
#210325 = FACE_OUTER_BOUND ( 'NONE', #157326, .T. ) ;
#210328 = CARTESIAN_POINT ( 'NONE',  ( 20.04142135623730070, 64.35000000001150511, -48.27310748452440237 ) ) ;
#210327 = CARTESIAN_POINT ( 'NONE',  ( -18.40000000000000213, 11.48667500176882328, -42.75000000000000000 ) ) ;
#210329 = CARTESIAN_POINT ( 'NONE',  ( -17.11825945287482043, 9.949999999999983302, -20.84999999999999787 ) ) ;
#210330 = ORIENTED_EDGE ( 'NONE', *, *, #181630, .T. ) ;
#210331 = CARTESIAN_POINT ( 'NONE',  ( 15.70340296795548518, 66.64411154550946037, -120.2344645877463591 ) ) ;
#210333 = EDGE_CURVE ( 'NONE', #193751, #225850, #10269, .T. ) ;
#210332 = CARTESIAN_POINT ( 'NONE',  ( 21.05000000000000071, 65.65271564877468791, -222.5736063831752176 ) ) ;
#210334 = CARTESIAN_POINT ( 'NONE',  ( -20.90000000000000213, 6.783826713665066066, 9.593862367105556288 ) ) ;
#210335 = ORIENTED_EDGE ( 'NONE', *, *, #134734, .T. ) ;
#210336 = ADVANCED_FACE ( 'NONE', ( #71447 ), #152272, .F. ) ;
#210337 = CARTESIAN_POINT ( 'NONE',  ( -20.94999999999999929, 71.93512633425886804, -225.1442869522136334 ) ) ;
#210338 = ORIENTED_EDGE ( 'NONE', *, *, #137173, .T. ) ;
#210339 = AXIS2_PLACEMENT_3D ( 'NONE', #227809, #89578, #106563 ) ;
#210340 = DIRECTION ( 'NONE',  ( -0.000000000000000000, 0.1350103645451876666, 0.9908441862701600211 ) ) ;
#210341 = EDGE_CURVE ( 'NONE', #10632, #8831, #33633, .T. ) ;
#210342 = CARTESIAN_POINT ( 'NONE',  ( 21.05000000000000071, -11.64999999998883595, -67.00000000000004263 ) ) ;
#210343 = CARTESIAN_POINT ( 'NONE',  ( 18.49999999999999289, 16.76897757977918957, -222.7804130109902871 ) ) ;
#210344 = ORIENTED_EDGE ( 'NONE', *, *, #1645, .F. ) ;
#210345 = EDGE_LOOP ( 'NONE', ( #153697, #202886, #151451, #238704 ) ) ;
#210346 = EDGE_CURVE ( 'NONE', #235498, #146255, #1844, .T. ) ;
#210347 = DIRECTION ( 'NONE',  ( -1.000000000000000000, 0.000000000000000000, 0.000000000000000000 ) ) ;
#210348 = SPHERICAL_SURFACE ( 'NONE', #181608, 0.1000000000000000056 ) ;
#210349 = CARTESIAN_POINT ( 'NONE',  ( 20.93975676684922504, 65.68895814178293335, -164.5026557862138645 ) ) ;
#210350 = PLANE ( 'NONE',  #98744 ) ;
#210353 = SPHERICAL_SURFACE ( 'NONE', #208495, 0.1000000000000000056 ) ;
#210352 = CIRCLE ( 'NONE', #14550, 12.77499999999999503 ) ;
#210351 = DIRECTION ( 'NONE',  ( 0.000000000000000000, 0.9126074666063771490, 0.4088369013363281623 ) ) ;
#210354 = DIRECTION ( 'NONE',  ( -0.000000000000000000, 0.8814952561688430555, -0.4721928772777346239 ) ) ;
#210355 = VECTOR ( 'NONE', #179978, 999.9999999999998863 ) ;
#210356 = CARTESIAN_POINT ( 'NONE',  ( 20.94999999999999929, -11.48912529306489994, -97.40000000000004832 ) ) ;
#210357 = DIRECTION ( 'NONE',  ( 0.000000000000000000, -0.9126074666063660468, -0.4088369013363524762 ) ) ;
#210359 = ORIENTED_EDGE ( 'NONE', *, *, #42886, .F. ) ;
#210358 = AXIS2_PLACEMENT_3D ( 'NONE', #238184, #161244, #23032 ) ;
#210360 = AXIS2_PLACEMENT_3D ( 'NONE', #91752, #252101, #171342 ) ;
#210362 = VERTEX_POINT ( 'NONE', #192667 ) ;
#210361 = DIRECTION ( 'NONE',  ( 0.000000000000000000, -1.000000000000000000, -6.982962677686266711E-15 ) ) ;
#210363 = CYLINDRICAL_SURFACE ( 'NONE', #1959, 12.87499999999999822 ) ;
#210364 = FACE_OUTER_BOUND ( 'NONE', #200701, .T. ) ;
#210365 = CARTESIAN_POINT ( 'NONE',  ( -15.55912972643741199, 8.490870273573719373, -180.0499999999999545 ) ) ;
#210366 = CARTESIAN_POINT ( 'NONE',  ( -16.77180007708460963, 66.05000000001207638, -123.8874933655695543 ) ) ;
#210367 = CARTESIAN_POINT ( 'NONE',  ( 21.02374657821588855, 11.60000000083178406, -194.0717967701982616 ) ) ;
#210369 = ORIENTED_EDGE ( 'NONE', *, *, #197470, .F. ) ;
#210368 = FACE_OUTER_BOUND ( 'NONE', #250793, .T. ) ;
#210370 = CARTESIAN_POINT ( 'NONE',  ( 18.59999999999999076, 76.00000000001213607, -136.5231074845243313 ) ) ;
#210372 = B_SPLINE_CURVE_WITH_KNOTS ( 'NONE', 3,
 ( #12464, #73727, #68577, #168994, #252320, #91974, #34596, #167697, #50267, #110254 ),
 .UNSPECIFIED., .F., .F.,
 ( 4, 3, 3, 4 ),
 ( 0.000000000000000000, 0.0002000000000008733344, 0.001000000000082982470, 0.001967863649483324578 ),
 .UNSPECIFIED. ) ;
#210371 = CARTESIAN_POINT ( 'NONE',  ( -16.86133551771148475, 51.57445858725908749, -231.9663616150992027 ) ) ;
#210373 = DIRECTION ( 'NONE',  ( 0.000000000000000000, 0.000000000000000000, -1.000000000000000000 ) ) ;
#210374 = CARTESIAN_POINT ( 'NONE',  ( 21.05000000000000071, -9.000000000000001776, -9.893969122652443104 ) ) ;
#210375 = EDGE_LOOP ( 'NONE', ( #154894, #56333, #103242, #236777 ) ) ;
#210376 = FACE_OUTER_BOUND ( 'NONE', #93444, .T. ) ;
#210377 = ORIENTED_EDGE ( 'NONE', *, *, #91235, .T. ) ;
#210378 = FACE_OUTER_BOUND ( 'NONE', #102642, .T. ) ;
#210379 = ORIENTED_EDGE ( 'NONE', *, *, #72461, .T. ) ;
#210380 = DIRECTION ( 'NONE',  ( 1.000000000000000000, -0.000000000000000000, -0.000000000000000000 ) ) ;
#210381 = CIRCLE ( 'NONE', #97899, 0.1999999999999987899 ) ;
#210382 = ORIENTED_EDGE ( 'NONE', *, *, #16877, .T. ) ;
#210383 = AXIS2_PLACEMENT_3D ( 'NONE', #218858, #122352, #161492 ) ;
#210384 = ADVANCED_FACE ( 'NONE', ( #14032 ), #220707, .T. ) ;
#210385 = CARTESIAN_POINT ( 'NONE',  ( -23.25000000000000000, -1.835859311432481045, -212.5044391687984842 ) ) ;
#210388 = EDGE_CURVE ( 'NONE', #55134, #197715, #101795, .T. ) ;
#210387 = PLANE ( 'NONE',  #79141 ) ;
#210386 = AXIS2_PLACEMENT_3D ( 'NONE', #249841, #35946, #11233 ) ;
#210389 = SPHERICAL_SURFACE ( 'NONE', #210087, 0.1000000000000000056 ) ;
#210390 = EDGE_LOOP ( 'NONE', ( #93843, #170826, #187346, #168466 ) ) ;
#210391 = EDGE_CURVE ( 'NONE', #120125, #64517, #239494, .T. ) ;
#210392 = EDGE_CURVE ( 'NONE', #155813, #124582, #143518, .T. ) ;
#210393 = AXIS2_PLACEMENT_3D ( 'NONE', #70925, #112595, #150449 ) ;
#210394 = AXIS2_PLACEMENT_3D ( 'NONE', #6092, #247272, #167780 ) ;
#210396 = CARTESIAN_POINT ( 'NONE',  ( 20.27550659511089037, 9.216043722520002035, -54.35000000000000142 ) ) ;
#210395 = AXIS2_PLACEMENT_3D ( 'NONE', #99526, #179130, #1725 ) ;
#210397 = CARTESIAN_POINT ( 'NONE',  ( 20.95512820512820440, 65.37615131630072085, -191.3731074845244393 ) ) ;
#210398 = ADVANCED_FACE ( 'NONE', ( #256409 ), #20457, .F. ) ;
#210399 = CARTESIAN_POINT ( 'NONE',  ( -22.47071067811865319, 7.522163794833024220, -199.2603376134758832 ) ) ;
#210400 = CARTESIAN_POINT ( 'NONE',  ( 12.26145404764308289, 9.351413679101387544, -16.98034356754895668 ) ) ;
#210401 = DIRECTION ( 'NONE',  ( 1.000000000000000000, -1.335000415235278971E-16, 2.979993593738921214E-16 ) ) ;
#210402 = EDGE_CURVE ( 'NONE', #90553, #21197, #131046, .T. ) ;
#210403 = ORIENTED_EDGE ( 'NONE', *, *, #233099, .T. ) ;
#210405 = ADVANCED_FACE ( 'NONE', ( #141661 ), #77827, .T. ) ;
#210404 = LINE ( 'NONE', #186997, #7579 ) ;
#210406 = ORIENTED_EDGE ( 'NONE', *, *, #165950, .F. ) ;
#210408 = ORIENTED_EDGE ( 'NONE', *, *, #149364, .T. ) ;
#210407 = CARTESIAN_POINT ( 'NONE',  ( -21.53699400381685436, 6.787711793192194420, -167.4999999999999432 ) ) ;
#210409 = VECTOR ( 'NONE', #245484, 1000.000000000000000 ) ;
#210410 = ORIENTED_EDGE ( 'NONE', *, *, #115386, .T. ) ;
#210411 = FACE_OUTER_BOUND ( 'NONE', #172053, .T. ) ;
#210412 = ORIENTED_EDGE ( 'NONE', *, *, #117155, .F. ) ;
#210413 = DIRECTION ( 'NONE',  ( -1.000000000000000000, -2.952720810173289112E-16, 0.000000000000000000 ) ) ;
#210414 = AXIS2_PLACEMENT_3D ( 'NONE', #146348, #128092, #107235 ) ;
#210415 = CARTESIAN_POINT ( 'NONE',  ( -20.95000000000000284, 11.65000000001115232, -193.9851942293460070 ) ) ;
#210416 = EDGE_CURVE ( 'NONE', #93396, #209151, #113686, .T. ) ;
#210417 = CARTESIAN_POINT ( 'NONE',  ( -22.60000000000094289, 75.89914163091323474, -81.27267460801374455 ) ) ;
#210418 = ORIENTED_EDGE ( 'NONE', *, *, #57913, .F. ) ;
#210419 = CARTESIAN_POINT ( 'NONE',  ( -16.89268316805465986, 66.04827818676933759, -48.66735500597884823 ) ) ;
#210420 = DIRECTION ( 'NONE',  ( 0.000000000000000000, 0.000000000000000000, -1.000000000000000000 ) ) ;
#210421 = CIRCLE ( 'NONE', #123106, 0.09999999999999363565 ) ;
#210422 = EDGE_LOOP ( 'NONE', ( #161937, #210359, #112500, #180085 ) ) ;
#210423 = EDGE_CURVE ( 'NONE', #13384, #118720, #236910, .T. ) ;
#210425 = ORIENTED_EDGE ( 'NONE', *, *, #213915, .T. ) ;
#210424 = DIRECTION ( 'NONE',  ( -1.000000000000000000, -0.000000000000000000, -0.000000000000000000 ) ) ;
#210426 = CARTESIAN_POINT ( 'NONE',  ( 21.05000000000000071, 6.703231349641842307, -231.7785101893094577 ) ) ;
#210427 = CARTESIAN_POINT ( 'NONE',  ( -21.05000000000000071, 77.83534155023670564, -158.4679561919613491 ) ) ;
#210428 = EDGE_CURVE ( 'NONE', #135352, #233834, #64585, .T. ) ;
#210429 = EDGE_CURVE ( 'NONE', #197715, #213407, #72828, .T. ) ;
#210430 = ORIENTED_EDGE ( 'NONE', *, *, #231455, .T. ) ;
#210431 = CARTESIAN_POINT ( 'NONE',  ( 20.85000000000000142, -1.362429037182151470, -108.3888812479212476 ) ) ;
#210433 = ADVANCED_FACE ( 'NONE', ( #840 ), #19148, .T. ) ;
#210432 = CARTESIAN_POINT ( 'NONE',  ( -15.06774609480955363, 66.58234804117103067, -121.1643200920839121 ) ) ;
#210434 = DIRECTION ( 'NONE',  ( -1.000000000000000000, 0.000000000000000000, 0.000000000000000000 ) ) ;
#210435 = ORIENTED_EDGE ( 'NONE', *, *, #4449, .T. ) ;
#210436 = DIRECTION ( 'NONE',  ( 1.000000000000000000, 0.000000000000000000, 0.000000000000000000 ) ) ;
#210437 = ADVANCED_FACE ( 'NONE', ( #139058 ), #242042, .F. ) ;
#210438 = FACE_OUTER_BOUND ( 'NONE', #160767, .T. ) ;
#210439 = EDGE_CURVE ( 'NONE', #237280, #35927, #2035, .T. ) ;
#210440 = AXIS2_PLACEMENT_3D ( 'NONE', #123512, #4814, #84321 ) ;
#210442 = B_SPLINE_CURVE_WITH_KNOTS ( 'NONE', 3,
 ( #163496, #243020, #203895, #184327, #125645, #112517, #29165, #128225 ),
 .UNSPECIFIED., .F., .F.,
 ( 4, 2, 2, 4 ),
 ( 0.000000000000000000, 6.534141206311912362E-05, 0.0001306828241262382472, 0.0002613656482524788255 ),
 .UNSPECIFIED. ) ;
#210441 = AXIS2_PLACEMENT_3D ( 'NONE', #78949, #99795, #175540 ) ;
#210443 = AXIS2_PLACEMENT_3D ( 'NONE', #184143, #83727, #71605 ) ;
#210444 = ORIENTED_EDGE ( 'NONE', *, *, #127687, .T. ) ;
#210445 = CARTESIAN_POINT ( 'NONE',  ( 21.08479644141222664, 0.05855444257529220792, -94.15496134226816594 ) ) ;
#210446 = CIRCLE ( 'NONE', #72915, 0.1000000000000028644 ) ;
#210447 = CIRCLE ( 'NONE', #68784, 0.09999999999999939493 ) ;
#210448 = VERTEX_POINT ( 'NONE', #200360 ) ;
#210449 = CARTESIAN_POINT ( 'NONE',  ( -18.59999999999999787, -9.321008403350132809, -174.7359382490778614 ) ) ;
#210450 = DIRECTION ( 'NONE',  ( 1.000000000000000000, 0.000000000000000000, 0.000000000000000000 ) ) ;
#210452 = ORIENTED_EDGE ( 'NONE', *, *, #20342, .F. ) ;
#210451 = CARTESIAN_POINT ( 'NONE',  ( 21.97500000000000497, 63.35728523183471594, -212.8904317177587870 ) ) ;
#210453 = CARTESIAN_POINT ( 'NONE',  ( -37.88850191057539973, -10.74999999999999289, 31.59999999999999787 ) ) ;
#210454 = DIRECTION ( 'NONE',  ( 0.7071067811865493491, 0.7071067811865456854, 0.000000000000000000 ) ) ;
#210455 = CARTESIAN_POINT ( 'NONE',  ( -23.25000000000000000, 64.25000000001246292, -181.7731074845244450 ) ) ;
#210457 = CARTESIAN_POINT ( 'NONE',  ( -23.25000000000000000, 64.35000000001205933, -124.3731074845243825 ) ) ;
#210456 = CIRCLE ( 'NONE', #73108, 0.09999999999998898659 ) ;
#210458 = CIRCLE ( 'NONE', #23031, 0.1000000000000012407 ) ;
#210459 = CARTESIAN_POINT ( 'NONE',  ( 20.94999999999999929, 71.99422445362657186, -246.4870034924427671 ) ) ;
#210460 = LINE ( 'NONE', #110054, #44814 ) ;
#210461 = VERTEX_POINT ( 'NONE', #97366 ) ;
#210462 = CARTESIAN_POINT ( 'NONE',  ( -23.15000000000000213, 87.65000000001204228, -114.7731074845242318 ) ) ;
#210463 = DIRECTION ( 'NONE',  ( 1.000000000000000000, -7.304098846218134667E-16, 4.607487905232622991E-31 ) ) ;
#210464 = VECTOR ( 'NONE', #37024, 1000.000000000000000 ) ;
#210465 = CARTESIAN_POINT ( 'NONE',  ( -18.50000000000000000, 85.42129027953507148, -62.69922530549790451 ) ) ;
#210466 = ORIENTED_EDGE ( 'NONE', *, *, #1643, .F. ) ;
#210467 = EDGE_CURVE ( 'NONE', #128224, #88400, #239389, .T. ) ;
#210468 = DIRECTION ( 'NONE',  ( -1.000000000000000000, -0.000000000000000000, -0.000000000000000000 ) ) ;
#210469 = DIRECTION ( 'NONE',  ( -1.000000000000000000, 0.000000000000000000, -0.000000000000000000 ) ) ;
#210470 = ADVANCED_FACE ( 'NONE', ( #178258 ), #257699, .F. ) ;
#210471 = ORIENTED_EDGE ( 'NONE', *, *, #23448, .T. ) ;
#210472 = AXIS2_PLACEMENT_3D ( 'NONE', #122714, #125264, #204777 ) ;
#210473 = DIRECTION ( 'NONE',  ( -0.000000000000000000, -6.982962677686266711E-15, 1.000000000000000000 ) ) ;
#210474 = CIRCLE ( 'NONE', #127076, 0.09999999999999939493 ) ;
#210475 = CARTESIAN_POINT ( 'NONE',  ( -20.64999999999999858, 36.65892442174935439, -249.5511627012433848 ) ) ;
#210476 = EDGE_CURVE ( 'NONE', #83171, #180198, #214427, .T. ) ;
#210477 = ORIENTED_EDGE ( 'NONE', *, *, #188524, .F. ) ;
#210479 = ADVANCED_FACE ( 'NONE', ( #146770 ), #107667, .T. ) ;
#210478 = CARTESIAN_POINT ( 'NONE',  ( -16.87845715379269507, 66.04214188611558711, -190.8993068334655447 ) ) ;
#210480 = ORIENTED_EDGE ( 'NONE', *, *, #41995, .F. ) ;
#210481 = SPHERICAL_SURFACE ( 'NONE', #29944, 0.1000000000000000056 ) ;
#210483 = VERTEX_POINT ( 'NONE', #4699 ) ;
#210482 = DIRECTION ( 'NONE',  ( 1.000000000000000000, 0.000000000000000000, -0.000000000000000000 ) ) ;
#210484 = DIRECTION ( 'NONE',  ( 0.000000000000000000, 1.000000000000000000, 0.000000000000000000 ) ) ;
#210485 = VERTEX_POINT ( 'NONE', #145507 ) ;
#210486 = CARTESIAN_POINT ( 'NONE',  ( 18.59999999999999787, -11.65000000000000036, 30.09999999999999787 ) ) ;
#210487 = EDGE_LOOP ( 'NONE', ( #94676, #233388, #39145, #142697 ) ) ;
#210489 = ORIENTED_EDGE ( 'NONE', *, *, #102572, .T. ) ;
#210488 = ORIENTED_EDGE ( 'NONE', *, *, #45395, .T. ) ;
#210490 = CARTESIAN_POINT ( 'NONE',  ( 18.59999999999999787, 85.32100840337339775, -129.2871692354463562 ) ) ;
#210492 = EDGE_LOOP ( 'NONE', ( #123949, #70487, #45981, #10568 ) ) ;
#210491 = CARTESIAN_POINT ( 'NONE',  ( -20.00857864376270001, 9.250000000000001776, -21.25000000000000000 ) ) ;
#210493 = CARTESIAN_POINT ( 'NONE',  ( 20.94403535211772294, 65.69367753730635684, -64.01892380663480253 ) ) ;
#210494 = ORIENTED_EDGE ( 'NONE', *, *, #156896, .T. ) ;
#210495 = EDGE_CURVE ( 'NONE', #102722, #73021, #97882, .T. ) ;
#210496 = ORIENTED_EDGE ( 'NONE', *, *, #229452, .F. ) ;
#210497 = FACE_OUTER_BOUND ( 'NONE', #158363, .T. ) ;
#210498 = DIRECTION ( 'NONE',  ( -0.000000000000000000, 1.000000000000000000, -0.000000000000000000 ) ) ;
#210499 = DIRECTION ( 'NONE',  ( 1.000000000000000000, 0.000000000000000000, -0.000000000000000000 ) ) ;
#210500 = EDGE_LOOP ( 'NONE', ( #44940, #34017, #81422 ) ) ;
#210501 = DIRECTION ( 'NONE',  ( -0.000000000000000000, 0.2128009952263603677, -0.9770955615653313941 ) ) ;
#210502 = CARTESIAN_POINT ( 'NONE',  ( 21.06089410995830491, 65.27470446788798597, -57.32072675348123880 ) ) ;
#210503 = EDGE_LOOP ( 'NONE', ( #172881, #33631, #164938, #229951 ) ) ;
#210505 = EDGE_CURVE ( 'NONE', #254324, #8739, #123392, .T. ) ;
#210504 = CARTESIAN_POINT ( 'NONE',  ( 21.05000000000000071, 71.00000000001223555, -148.4283735034374843 ) ) ;
#210506 = DIRECTION ( 'NONE',  ( 1.000000000000000000, 0.000000000000000000, 0.000000000000000000 ) ) ;
#210507 = CYLINDRICAL_SURFACE ( 'NONE', #142875, 0.09999999999999804878 ) ;
#210508 = ORIENTED_EDGE ( 'NONE', *, *, #170066, .F. ) ;
#210509 = EDGE_CURVE ( 'NONE', #51098, #145748, #181147, .T. ) ;
#210510 = CARTESIAN_POINT ( 'NONE',  ( -20.00857864376270001, 9.350000000000001421, -21.25000000000000000 ) ) ;
#210511 = EDGE_LOOP ( 'NONE', ( #250496, #158583, #244415, #85081 ) ) ;
#210512 = CARTESIAN_POINT ( 'NONE',  ( -18.48550754432010379, -7.746656446482333536, -209.9011620725964633 ) ) ;
#210513 = EDGE_LOOP ( 'NONE', ( #5227, #16526, #146520, #62869, #35169, #5168, #86863, #54602, #51964, #40238 ) ) ;
#210514 = AXIS2_PLACEMENT_3D ( 'NONE', #205365, #67158, #167569 ) ;
#210515 = AXIS2_PLACEMENT_3D ( 'NONE', #157777, #79451, #244956 ) ;
#210516 = DIRECTION ( 'NONE',  ( 0.000000000000000000, -1.000000000000000000, 0.000000000000000000 ) ) ;
#210517 = DIRECTION ( 'NONE',  ( 0.000000000000000000, 0.000000000000000000, 1.000000000000000000 ) ) ;
#210518 = ORIENTED_EDGE ( 'NONE', *, *, #135594, .F. ) ;
#210519 = ORIENTED_EDGE ( 'NONE', *, *, #237094, .T. ) ;
#210520 = CARTESIAN_POINT ( 'NONE',  ( -22.50000000000000000, 0.000000000000000000, 11.64957080754479968 ) ) ;
#210521 = DIRECTION ( 'NONE',  ( -1.000000000000000000, 0.000000000000000000, 0.000000000000000000 ) ) ;
#210522 = ORIENTED_EDGE ( 'NONE', *, *, #177473, .T. ) ;
#210523 = ADVANCED_FACE ( 'NONE', ( #64691 ), #24310, .T. ) ;
#210524 = FACE_OUTER_BOUND ( 'NONE', #203729, .T. ) ;
#210525 =( NAMED_UNIT ( * ) PLANE_ANGLE_UNIT ( ) SI_UNIT ( $, .RADIAN. ) );
#210526 = EDGE_CURVE ( 'NONE', #179646, #88490, #243667, .T. ) ;
#210527 = EDGE_LOOP ( 'NONE', ( #231496, #65477, #225283, #131131 ) ) ;
#210528 = CIRCLE ( 'NONE', #6507, 0.1000000000000024342 ) ;
#210529 = ADVANCED_FACE ( 'NONE', ( #103795 ), #248471, .T. ) ;
#210530 = AXIS2_PLACEMENT_3D ( 'NONE', #43987, #200499, #83070 ) ;
#210531 = ORIENTED_EDGE ( 'NONE', *, *, #185293, .T. ) ;
#210532 = AXIS2_PLACEMENT_3D ( 'NONE', #63093, #108649, #142618 ) ;
#210533 = DIRECTION ( 'NONE',  ( 0.000000000000000000, 0.000000000000000000, 1.000000000000000000 ) ) ;
#210534 =( GEOMETRIC_REPRESENTATION_CONTEXT ( 3 ) GLOBAL_UNCERTAINTY_ASSIGNED_CONTEXT ( ( #74137 ) ) GLOBAL_UNIT_ASSIGNED_CONTEXT ( ( #63371, #242020, #144189 ) ) REPRESENTATION_CONTEXT ( 'NONE', 'WORKASPACE' ) );
#210535 = DIRECTION ( 'NONE',  ( 0.000000000000000000, -0.2128009952263604232, 0.9770955615653316162 ) ) ;
#210536 = EDGE_CURVE ( 'NONE', #218583, #168057, #177055, .T. ) ;
#210537 = LINE ( 'NONE', #52728, #225862 ) ;
#210539 = EDGE_LOOP ( 'NONE', ( #184021, #147466, #125282, #35665, #117171 ) ) ;
#210538 = DIRECTION ( 'NONE',  ( 0.000000000000000000, -6.608470384673558123E-15, 1.000000000000000000 ) ) ;
#210540 = DIRECTION ( 'NONE',  ( -1.000000000000000000, 0.000000000000000000, 0.000000000000000000 ) ) ;
#210541 = FACE_OUTER_BOUND ( 'NONE', #71855, .T. ) ;
#210542 = LINE ( 'NONE', #193553, #64687 ) ;
#210543 = ADVANCED_FACE ( 'NONE', ( #28169 ), #157530, .T. ) ;
#210545 = CARTESIAN_POINT ( 'NONE',  ( -17.29838795459677314, 60.20407299469992068, -222.1423803938182289 ) ) ;
#210544 = CARTESIAN_POINT ( 'NONE',  ( 20.85000000000000142, 7.783179459866048866, -245.3643104511423303 ) ) ;
#210546 = LINE ( 'NONE', #252221, #82303 ) ;
#210547 = CARTESIAN_POINT ( 'NONE',  ( -20.95000000000000284, 64.35000000001220144, -143.5379132551784096 ) ) ;
#210548 = DIRECTION ( 'NONE',  ( 0.000000000000000000, 0.000000000000000000, -1.000000000000000000 ) ) ;
#210549 = CARTESIAN_POINT ( 'NONE',  ( -21.05000000000000071, 76.01771943332080639, -176.4641921729960643 ) ) ;
#210550 = AXIS2_PLACEMENT_3D ( 'NONE', #214651, #174305, #115554 ) ;
#210551 = VERTEX_POINT ( 'NONE', #5987 ) ;
#210552 = TOROIDAL_SURFACE ( 'NONE', #206453, 0.2000000000000000111, 0.1000000000000000056 ) ;
#210553 = ORIENTED_EDGE ( 'NONE', *, *, #56336, .F. ) ;
#210554 = ORIENTED_EDGE ( 'NONE', *, *, #116198, .F. ) ;
#210555 = AXIS2_PLACEMENT_3D ( 'NONE', #150438, #229952, #74775 ) ;
#210556 = DIRECTION ( 'NONE',  ( 1.000000000000000000, 0.000000000000000000, 0.000000000000000000 ) ) ;
#210557 = CIRCLE ( 'NONE', #118995, 3.999999999999999112 ) ;
#210558 = AXIS2_PLACEMENT_3D ( 'NONE', #68032, #5462, #246660 ) ;
#210559 = AXIS2_PLACEMENT_3D ( 'NONE', #53702, #133246, #92819 ) ;
#210560 = LINE ( 'NONE', #193569, #115200 ) ;
#210561 = ORIENTED_EDGE ( 'NONE', *, *, #218716, .T. ) ;
#210562 =( NAMED_UNIT ( * ) SI_UNIT ( $, .STERADIAN. ) SOLID_ANGLE_UNIT ( ) );
#210563 = DIRECTION ( 'NONE',  ( -1.000000000000000000, 7.304098846218134667E-16, -4.217023435051678980E-16 ) ) ;
#210564 = CYLINDRICAL_SURFACE ( 'NONE', #29147, 11.80000000000000426 ) ;
#210565 = SPHERICAL_SURFACE ( 'NONE', #74658, 0.1000000000000000056 ) ;
#210566 = ORIENTED_EDGE ( 'NONE', *, *, #37378, .F. ) ;
#210567 = EDGE_LOOP ( 'NONE', ( #118772, #6246, #203432, #164688 ) ) ;
#210569 = CARTESIAN_POINT ( 'NONE',  ( 20.94999999999999929, -4.756823075239758225, -233.1486023682345490 ) ) ;
#210568 = AXIS2_PLACEMENT_3D ( 'NONE', #70714, #165961, #111093 ) ;
#210570 = LINE ( 'NONE', #11087, #67157 ) ;
#210571 = EDGE_LOOP ( 'NONE', ( #240651, #217185, #32431, #12610 ) ) ;
#210572 = CARTESIAN_POINT ( 'NONE',  ( -23.25000000000000000, 77.25000000001165290, -61.72262673010922640 ) ) ;
#210574 = VERTEX_POINT ( 'NONE', #148089 ) ;
#210573 = DIRECTION ( 'NONE',  ( 0.000000000000000000, 0.000000000000000000, -1.000000000000000000 ) ) ;
#210575 = DIRECTION ( 'NONE',  ( 0.000000000000000000, 0.000000000000000000, -1.000000000000000000 ) ) ;
#210576 = VECTOR ( 'NONE', #16972, 1000.000000000000000 ) ;
#210578 = ORIENTED_EDGE ( 'NONE', *, *, #128919, .T. ) ;
#210577 = DIRECTION ( 'NONE',  ( 1.000000000000000000, -7.304098846218134667E-16, -5.100424963727255829E-30 ) ) ;
#210579 = DIRECTION ( 'NONE',  ( 0.000000000000000000, 0.000000000000000000, -1.000000000000000000 ) ) ;
#210580 = CARTESIAN_POINT ( 'NONE',  ( -16.90138253750127006, 9.950000000011137047, -87.71156270790466181 ) ) ;
#210581 = DIRECTION ( 'NONE',  ( 0.000000000000000000, 1.000000000000000000, 0.000000000000000000 ) ) ;
#210583 = CARTESIAN_POINT ( 'NONE',  ( 20.77766267348356166, 10.44904239063021123, -108.0927089158775374 ) ) ;
#210582 = DIRECTION ( 'NONE',  ( -1.000000000000000000, -5.603460673774840016E-17, -1.046060675573451769E-16 ) ) ;
#210585 = EDGE_CURVE ( 'NONE', #65541, #183861, #23171, .T. ) ;
#210584 = DIRECTION ( 'NONE',  ( 0.000000000000000000, -0.2128009952263603677, 0.9770955615653313941 ) ) ;
#210586 = DIRECTION ( 'NONE',  ( -1.000000000000000000, 0.000000000000000000, 0.000000000000000000 ) ) ;
#210587 = CARTESIAN_POINT ( 'NONE',  ( -18.59999999999999787, 1.115600667400684642E-11, -200.9999999999999432 ) ) ;
#210588 = FACE_OUTER_BOUND ( 'NONE', #129612, .T. ) ;
#210589 = ORIENTED_EDGE ( 'NONE', *, *, #173958, .F. ) ;
#210590 = DIRECTION ( 'NONE',  ( 1.000000000000000000, 0.000000000000000000, 0.000000000000000000 ) ) ;
#210591 = ORIENTED_EDGE ( 'NONE', *, *, #195755, .T. ) ;
#210592 = DIRECTION ( 'NONE',  ( -0.000000000000000000, 0.2617529984165031243, 0.9651348961777157509 ) ) ;
#210593 = ORIENTED_EDGE ( 'NONE', *, *, #158782, .T. ) ;
#210594 = LINE ( 'NONE', #230157, #135988 ) ;
#210595 = ADVANCED_FACE ( 'NONE', ( #202920 ), #128524, .T. ) ;
#210596 = FACE_OUTER_BOUND ( 'NONE', #29994, .T. ) ;
#210597 = AXIS2_PLACEMENT_3D ( 'NONE', #139552, #234822, #217798 ) ;
#210598 = EDGE_CURVE ( 'NONE', #220769, #239144, #27031, .T. ) ;
#210599 = EDGE_CURVE ( 'NONE', #78967, #197038, #118776, .T. ) ;
#210600 = AXIS2_PLACEMENT_3D ( 'NONE', #250579, #151516, #109781 ) ;
#210601 = EDGE_LOOP ( 'NONE', ( #93158, #25975, #142874, #247408 ) ) ;
#210602 = DIRECTION ( 'NONE',  ( -1.000000000000000000, 1.335000415235278971E-16, -2.979993593738921214E-16 ) ) ;
#210603 = AXIS2_PLACEMENT_3D ( 'NONE', #160128, #80530, #179680 ) ;
#210604 = VERTEX_POINT ( 'NONE', #106366 ) ;
#210605 = EDGE_LOOP ( 'NONE', ( #257900, #62379, #224710, #84934 ) ) ;
#210606 = CIRCLE ( 'NONE', #60572, 1.500000000000001332 ) ;
#210607 = DIRECTION ( 'NONE',  ( 0.000000000000000000, 0.000000000000000000, -1.000000000000000000 ) ) ;
#210608 = CARTESIAN_POINT ( 'NONE',  ( 21.05000000000000071, 10.42338541492406101, -40.99205192387010044 ) ) ;
#210609 = CARTESIAN_POINT ( 'NONE',  ( -20.65000000000000568, 5.649999999999983480, -9.250000000000001776 ) ) ;
#210610 = CARTESIAN_POINT ( 'NONE',  ( 18.59999999999999787, 77.83534155023700407, -191.8679561919613832 ) ) ;
#210611 = EDGE_CURVE ( 'NONE', #226150, #45344, #152108, .T. ) ;
#210613 = CARTESIAN_POINT ( 'NONE',  ( -18.40000000000000213, 11.48667500176882861, -57.75000000000000000 ) ) ;
#210612 = DIRECTION ( 'NONE',  ( 1.000000000000000000, 0.000000000000000000, 0.000000000000000000 ) ) ;
#210614 = PLANE ( 'NONE',  #136928 ) ;
#210616 = ORIENTED_EDGE ( 'NONE', *, *, #255932, .F. ) ;
#210615 = LINE ( 'NONE', #214453, #204878 ) ;
#210618 = CARTESIAN_POINT ( 'NONE',  ( -22.59999999999999787, 11.74987124438766273, -100.4345704089863602 ) ) ;
#210617 = FACE_OUTER_BOUND ( 'NONE', #21266, .T. ) ;
#210619 = FACE_OUTER_BOUND ( 'NONE', #8603, .T. ) ;
#210620 = AXIS2_PLACEMENT_3D ( 'NONE', #156719, #80979, #1449 ) ;
#210621 = ORIENTED_EDGE ( 'NONE', *, *, #128232, .F. ) ;
#210622 = DIRECTION ( 'NONE',  ( 1.000000000000000000, -0.000000000000000000, 0.000000000000000000 ) ) ;
#210623 = VECTOR ( 'NONE', #142915, 1000.000000000000000 ) ;
#210624 = DIRECTION ( 'NONE',  ( 0.000000000000000000, -0.01562499999999307672, 0.9998779222360100194 ) ) ;
#210625 = CARTESIAN_POINT ( 'NONE',  ( 20.94999999999999574, 1.835341550235567887, -179.0551512925629538 ) ) ;
#210626 = EDGE_LOOP ( 'NONE', ( #107173, #245234, #253020, #217881 ) ) ;
#210627 = CIRCLE ( 'NONE', #110668, 0.5000000000000004441 ) ;
#210628 = DIRECTION ( 'NONE',  ( 0.000000000000000000, 0.000000000000000000, -1.000000000000000000 ) ) ;
#210629 = PLANE ( 'NONE',  #73513 ) ;
#210630 = LINE ( 'NONE', #12452, #9470 ) ;
#210631 = VERTEX_POINT ( 'NONE', #151962 ) ;
#210632 = ORIENTED_EDGE ( 'NONE', *, *, #66275, .T. ) ;
#210633 = CARTESIAN_POINT ( 'NONE',  ( 22.40000000000010516, 64.18196446391901588, -247.0985338183336353 ) ) ;
#210634 = EDGE_CURVE ( 'NONE', #26951, #156138, #193600, .T. ) ;
#210635 = ADVANCED_FACE ( 'NONE', ( #90663 ), #175380, .F. ) ;
#210636 = CARTESIAN_POINT ( 'NONE',  ( -21.05000000000000071, 67.63082410804655353, -211.8415745842588649 ) ) ;
#210637 = AXIS2_PLACEMENT_3D ( 'NONE', #131300, #111747, #231706 ) ;
#210638 = DIRECTION ( 'NONE',  ( -0.000000000000000000, 0.5474227397873200340, -0.8368562265788217491 ) ) ;
#210639 = CARTESIAN_POINT ( 'NONE',  ( 18.39999999999999503, 61.34848953995435039, -212.6564661897791098 ) ) ;
#210640 = ORIENTED_EDGE ( 'NONE', *, *, #117411, .F. ) ;
#210641 = CARTESIAN_POINT ( 'NONE',  ( -20.05000000000000426, 9.250000000011157297, -155.1500000000000057 ) ) ;
#210642 = EDGE_CURVE ( 'NONE', #176131, #232311, #249754, .T. ) ;
#210643 = DIRECTION ( 'NONE',  ( 1.000000000000000000, 0.000000000000000000, 0.000000000000000000 ) ) ;
#210644 = DIRECTION ( 'NONE',  ( -1.000000000000000000, 0.000000000000000000, 0.000000000000000000 ) ) ;
#210645 = AXIS2_PLACEMENT_3D ( 'NONE', #43844, #82928, #141649 ) ;
#210646 = CIRCLE ( 'NONE', #119074, 0.1000000000000028644 ) ;
#210647 = VERTEX_POINT ( 'NONE', #111527 ) ;
#210648 = AXIS2_PLACEMENT_3D ( 'NONE', #185714, #72200, #8367 ) ;
#210649 = CIRCLE ( 'NONE', #131542, 11.80000000000000426 ) ;
#210650 = CARTESIAN_POINT ( 'NONE',  ( 21.05000000000000071, 0.000000000000000000, -33.50000000000000000 ) ) ;
#210652 = ORIENTED_EDGE ( 'NONE', *, *, #230034, .T. ) ;
#210651 = CARTESIAN_POINT ( 'NONE',  ( -16.93211319090181632, 66.00001321885433470, -82.10060198525131625 ) ) ;
#210653 = DIRECTION ( 'NONE',  ( 0.000000000000000000, -0.5907332058517320572, 0.8068669527896995541 ) ) ;
#210654 = CARTESIAN_POINT ( 'NONE',  ( 23.25000000000000000, 86.52890073500824997, -209.5906233940697234 ) ) ;
#210655 = DIRECTION ( 'NONE',  ( -1.000000000000000000, -0.000000000000000000, -0.000000000000000000 ) ) ;
#210656 = CARTESIAN_POINT ( 'NONE',  ( -23.24999999999999645, 85.60000000001186038, -96.42291809330220076 ) ) ;
#210657 = DIRECTION ( 'NONE',  ( 0.000000000000000000, -1.000000000000000000, -6.982962677686266711E-15 ) ) ;
#210658 = ORIENTED_EDGE ( 'NONE', *, *, #141336, .T. ) ;
#210659 = CARTESIAN_POINT ( 'NONE',  ( 21.13461538461538680, 8.885417037974457699, -12.34999999999999964 ) ) ;
#210660 = DIRECTION ( 'NONE',  ( 0.000000000000000000, 0.000000000000000000, -1.000000000000000000 ) ) ;
#210661 = CARTESIAN_POINT ( 'NONE',  ( -23.25000000000000000, 76.00000000001186606, -90.24810748452431142 ) ) ;
#210662 = EDGE_LOOP ( 'NONE', ( #206331, #191896, #158659, #73380, #25698, #51347, #52272, #143113, #208217, #135603, #216271, #45252 ) ) ;
#210663 = DIRECTION ( 'NONE',  ( 0.000000000000000000, 0.000000000000000000, 1.000000000000000000 ) ) ;
#210664 = DIRECTION ( 'NONE',  ( 0.000000000000000000, -0.9770955615653313941, -0.2128009952263603677 ) ) ;
#210665 = CARTESIAN_POINT ( 'NONE',  ( -18.50000000000000000, 64.35000000001205933, -124.3731074845243825 ) ) ;
#210666 = CARTESIAN_POINT ( 'NONE',  ( 19.58285714285715073, 18.80841834337416074, -229.7621925467414883 ) ) ;
#210667 = CIRCLE ( 'NONE', #239713, 2.000000000000001776 ) ;
#210668 = DIRECTION ( 'NONE',  ( 1.000000000000000000, 0.000000000000000000, 0.000000000000000000 ) ) ;
#210669 = CARTESIAN_POINT ( 'NONE',  ( -23.15000000000000213, 74.08971962618008433, -90.39173962932538586 ) ) ;
#210670 = ORIENTED_EDGE ( 'NONE', *, *, #184925, .F. ) ;
#210671 = VERTEX_POINT ( 'NONE', #150654 ) ;
#210672 = ADVANCED_FACE ( 'NONE', ( #16301 ), #194932, .T. ) ;
#210674 = FACE_OUTER_BOUND ( 'NONE', #111973, .T. ) ;
#210673 = AXIS2_PLACEMENT_3D ( 'NONE', #217101, #97131, #239265 ) ;
#210676 = EDGE_CURVE ( 'NONE', #55258, #240571, #56201, .T. ) ;
#210675 = DIRECTION ( 'NONE',  ( 1.000000000000000000, 4.095934188116521533E-15, 3.985178720521109717E-14 ) ) ;
#210677 = CARTESIAN_POINT ( 'NONE',  ( -21.05000000000000071, 38.08698097766499302, -236.1457910985472779 ) ) ;
#210678 = FACE_OUTER_BOUND ( 'NONE', #149823, .T. ) ;
#210679 = ADVANCED_FACE ( 'NONE', ( #93234 ), #11145, .T. ) ;
#210680 = EDGE_CURVE ( 'NONE', #224814, #190621, #89525, .T. ) ;
#210681 = LINE ( 'NONE', #187289, #121912 ) ;
#210682 = FACE_OUTER_BOUND ( 'NONE', #7864, .T. ) ;
#210683 = CARTESIAN_POINT ( 'NONE',  ( -16.93909480342659890, 9.993078364812696179, -113.1003470166723588 ) ) ;
#210684 = ADVANCED_FACE ( 'NONE', ( #134905 ), #172832, .F. ) ;
#210685 = AXIS2_PLACEMENT_3D ( 'NONE', #220789, #186816, #203790 ) ;
#210687 = EDGE_CURVE ( 'NONE', #107334, #245093, #122879, .T. ) ;
#210686 = ADVANCED_FACE ( 'NONE', ( #209331 ), #235274, .T. ) ;
#210688 = ORIENTED_EDGE ( 'NONE', *, *, #242810, .T. ) ;
#210689 = DIRECTION ( 'NONE',  ( 1.000000000000000000, 0.000000000000000000, 0.000000000000000000 ) ) ;
#210690 = EDGE_LOOP ( 'NONE', ( #197915, #125608, #81999, #246724 ) ) ;
#210691 = DIRECTION ( 'NONE',  ( 0.000000000000000000, 0.000000000000000000, 1.000000000000000000 ) ) ;
#210692 = CARTESIAN_POINT ( 'NONE',  ( 23.24999999999999289, 69.35000000001186038, -90.87310748452435405 ) ) ;
#210694 = EDGE_CURVE ( 'NONE', #91733, #15173, #253123, .T. ) ;
#210693 = CARTESIAN_POINT ( 'NONE',  ( -22.50000000000000000, 76.00000000001237765, -170.1231074845243540 ) ) ;
#210695 = CARTESIAN_POINT ( 'NONE',  ( -22.59999999999999787, -3.180729737797944434, -228.0957332317254895 ) ) ;
#210696 = CARTESIAN_POINT ( 'NONE',  ( 23.25000000000000000, 23.68770167995059239, -252.8127582590406348 ) ) ;
#210697 = DIRECTION ( 'NONE',  ( 0.000000000000000000, -1.000000000000000000, 0.000000000000000000 ) ) ;
#210698 = FACE_OUTER_BOUND ( 'NONE', #221881, .T. ) ;
#210699 = VERTEX_POINT ( 'NONE', #55358 ) ;
#210700 = CARTESIAN_POINT ( 'NONE',  ( -16.94445028196808778, 22.96031635112858282, -230.8778361528912058 ) ) ;
#210701 = EDGE_CURVE ( 'NONE', #172111, #39830, #119201, .T. ) ;
#210702 = CYLINDRICAL_SURFACE ( 'NONE', #54886, 0.1000000000000124262 ) ;
#210703 = DIRECTION ( 'NONE',  ( -1.000000000000000000, -0.000000000000000000, -0.000000000000000000 ) ) ;
#210704 = CARTESIAN_POINT ( 'NONE',  ( -18.50000000000000711, 64.35000000001161879, -62.50830171387040934 ) ) ;
#210705 = AXIS2_PLACEMENT_3D ( 'NONE', #129071, #92497, #169520 ) ;
#210706 = AXIS2_PLACEMENT_3D ( 'NONE', #185759, #70979, #7107 ) ;
#210707 = ADVANCED_FACE ( 'NONE', ( #39718 ), #237885, .F. ) ;
#210708 = EDGE_CURVE ( 'NONE', #173939, #160204, #14553, .T. ) ;
#210709 = VECTOR ( 'NONE', #174470, 1000.000000000000000 ) ;
#210710 = AXIS2_PLACEMENT_3D ( 'NONE', #248691, #72641, #29672 ) ;
#210711 = ORIENTED_EDGE ( 'NONE', *, *, #83809, .T. ) ;
#210713 = CARTESIAN_POINT ( 'NONE',  ( 18.39999999999999503, 11.47316190337363828, -154.8500000000000227 ) ) ;
#210712 = COLOUR_RGB ( '', 0.40784314, 0.44705882, 0.49803922) ;
#210715 = ADVANCED_FACE ( 'NONE', ( #81347 ), #47822, .T. ) ;
#210714 = DIRECTION ( 'NONE',  ( 1.000000000000000000, 0.000000000000000000, 0.000000000000000000 ) ) ;
#210716 = VERTEX_POINT ( 'NONE', #37143 ) ;
#210717 = ORIENTED_EDGE ( 'NONE', *, *, #177318, .F. ) ;
#210718 = FACE_OUTER_BOUND ( 'NONE', #53692, .T. ) ;
#210719 = DIRECTION ( 'NONE',  ( -0.000000000000000000, -0.000000000000000000, -1.000000000000000000 ) ) ;
#210720 = EDGE_CURVE ( 'NONE', #137100, #251749, #106707, .T. ) ;
#210721 = ORIENTED_EDGE ( 'NONE', *, *, #249562, .F. ) ;
#210722 = CARTESIAN_POINT ( 'NONE',  ( 18.54271179734065456, -9.624084290087184357, -174.2409648527008983 ) ) ;
#210723 = DIRECTION ( 'NONE',  ( 0.000000000000000000, 0.000000000000000000, 1.000000000000000000 ) ) ;
#210724 = ADVANCED_FACE ( 'NONE', ( #138744 ), #218298, .T. ) ;
#210725 = EDGE_LOOP ( 'NONE', ( #161123, #114252, #64374, #237859, #216080 ) ) ;
#210726 = CIRCLE ( 'NONE', #223193, 0.5000000000000004441 ) ;
#210727 = CIRCLE ( 'NONE', #44153, 4.000000000000003553 ) ;
#210728 = CARTESIAN_POINT ( 'NONE',  ( 21.00000000000000000, 66.25000000001158185, -57.17310748452438673 ) ) ;
#210729 = VERTEX_POINT ( 'NONE', #119238 ) ;
#210730 = AXIS2_PLACEMENT_3D ( 'NONE', #80821, #142091, #118707 ) ;
#210731 = CARTESIAN_POINT ( 'NONE',  ( -20.00857864376270001, 22.24771505525269788, -231.4513824651465939 ) ) ;
#210732 = EDGE_CURVE ( 'NONE', #254141, #13152, #147815, .T. ) ;
#210733 = DIRECTION ( 'NONE',  ( -4.336808689941751890E-15, -0.9667078373770149335, -0.2558827019434000150 ) ) ;
#210735 = ORIENTED_EDGE ( 'NONE', *, *, #245952, .F. ) ;
#210734 = DIRECTION ( 'NONE',  ( -1.000000000000000000, 0.000000000000000000, 0.000000000000000000 ) ) ;
#210736 = CARTESIAN_POINT ( 'NONE',  ( 23.40000000000005187, 76.00000000001119815, -36.02310748452479316 ) ) ;
#210737 = DIRECTION ( 'NONE',  ( -0.000000000000000000, -2.891205793294679805E-16, 1.000000000000000000 ) ) ;
#210738 = LINE ( 'NONE', #112924, #33726 ) ;
#210739 = AXIS2_PLACEMENT_3D ( 'NONE', #108247, #187793, #229479 ) ;
#210740 = DIRECTION ( 'NONE',  ( 0.000000000000000000, 0.000000000000000000, 1.000000000000000000 ) ) ;
#210741 = DIRECTION ( 'NONE',  ( 1.000000000000000000, 0.000000000000000000, 0.000000000000000000 ) ) ;
#210742 = CARTESIAN_POINT ( 'NONE',  ( -16.81744102076749314, 66.05000000001230376, -157.3731074845244393 ) ) ;
#210744 = ORIENTED_EDGE ( 'NONE', *, *, #132986, .T. ) ;
#210743 = DIRECTION ( 'NONE',  ( 0.000000000000000000, 0.000000000000000000, 1.000000000000000000 ) ) ;
#210745 = ORIENTED_EDGE ( 'NONE', *, *, #51760, .F. ) ;
#210747 = DIRECTION ( 'NONE',  ( 0.000000000000000000, 0.000000000000000000, 1.000000000000000000 ) ) ;
#210746 = CARTESIAN_POINT ( 'NONE',  ( -21.14999999999999858, 69.45934304831041572, -69.52310748452435973 ) ) ;
#210749 = VERTEX_POINT ( 'NONE', #198753 ) ;
#210748 = DIRECTION ( 'NONE',  ( 0.000000000000000000, 0.000000000000000000, 1.000000000000000000 ) ) ;
#210750 = ORIENTED_EDGE ( 'NONE', *, *, #31110, .T. ) ;
#210751 = CARTESIAN_POINT ( 'NONE',  ( -22.39999999999999503, 0.2612980822699338401, -230.0539506776466681 ) ) ;
#210752 = DIRECTION ( 'NONE',  ( -0.000000000000000000, 0.2617529984165037349, 0.9651348961777156399 ) ) ;
#210753 = AXIS2_PLACEMENT_3D ( 'NONE', #213099, #192274, #211833 ) ;
#210754 = DIRECTION ( 'NONE',  ( 1.000000000000000000, 0.000000000000000000, 0.000000000000000000 ) ) ;
#210755 = CARTESIAN_POINT ( 'NONE',  ( 18.59999999999999076, 52.91185528119410009, -244.1460391050142675 ) ) ;
#210756 = CARTESIAN_POINT ( 'NONE',  ( -18.50000324121759121, 67.49461024981998492, -195.5605382655040216 ) ) ;
#210757 = CIRCLE ( 'NONE', #177486, 11.74999999999999645 ) ;
#210758 = DIRECTION ( 'NONE',  ( 0.8049926720990051576, 0.5932847527679298016, -0.000000000000000000 ) ) ;
#210759 = DIRECTION ( 'NONE',  ( 1.000000000000000000, 0.000000000000000000, 0.000000000000000000 ) ) ;
#210761 = ORIENTED_EDGE ( 'NONE', *, *, #169271, .F. ) ;
#210760 = ADVANCED_FACE ( 'NONE', ( #102191 ), #20139, .T. ) ;
#210762 = ORIENTED_EDGE ( 'NONE', *, *, #105577, .F. ) ;
#210763 = DIRECTION ( 'NONE',  ( -0.000000000000000000, 1.000000000000000000, -1.224646799147352961E-16 ) ) ;
#210764 = VECTOR ( 'NONE', #178812, 1000.000000000000000 ) ;
#210765 = EDGE_CURVE ( 'NONE', #214123, #202965, #180490, .T. ) ;
#210766 = ORIENTED_EDGE ( 'NONE', *, *, #196851, .F. ) ;
#210767 = FACE_OUTER_BOUND ( 'NONE', #211895, .T. ) ;
#210768 = ORIENTED_EDGE ( 'NONE', *, *, #182245, .T. ) ;
#210769 = CARTESIAN_POINT ( 'NONE',  ( -21.14999999999999858, 65.69183180257304855, -241.9133949074307566 ) ) ;
#210770 = DIRECTION ( 'NONE',  ( -0.7071067811865463515, -0.7071067811865487940, 7.587431340288849180E-16 ) ) ;
#210771 = EDGE_CURVE ( 'NONE', #91470, #203708, #157085, .T. ) ;
#210773 = EDGE_CURVE ( 'NONE', #20729, #46619, #114672, .T. ) ;
#210772 = CARTESIAN_POINT ( 'NONE',  ( 18.59999999999997655, 64.25000000001142553, -36.02310748452440237 ) ) ;
#210774 = EDGE_LOOP ( 'NONE', ( #96010, #175734, #465, #151735, #187838, #99380, #8296, #16915 ) ) ;
#210775 =( REPRESENTATION_RELATIONSHIP ('NONE','NONE', #36900, #106899 ) REPRESENTATION_RELATIONSHIP_WITH_TRANSFORMATION ( #23404 )SHAPE_REPRESENTATION_RELATIONSHIP( ) );
#210776 = DIRECTION ( 'NONE',  ( 1.000000000000000000, 3.265361837132813093E-16, -0.000000000000000000 ) ) ;
#210777 = ORIENTED_EDGE ( 'NONE', *, *, #164913, .F. ) ;
#210778 = VECTOR ( 'NONE', #44010, 1000.000000000000000 ) ;
#210779 = LINE ( 'NONE', #146935, #156483 ) ;
#210780 = AXIS2_PLACEMENT_3D ( 'NONE', #245010, #28590, #108080 ) ;
#210781 = CARTESIAN_POINT ( 'NONE',  ( 21.05000000000000071, 8.876614585098257848, -108.8850804788447135 ) ) ;
#210782 = AXIS2_PLACEMENT_3D ( 'NONE', #166674, #231763, #17821 ) ;
#210783 = CIRCLE ( 'NONE', #214882, 0.1999999999999987899 ) ;
#210784 = VERTEX_POINT ( 'NONE', #197467 ) ;
#210785 = DIRECTION ( 'NONE',  ( 1.000000000000000000, 0.000000000000000000, 0.000000000000000000 ) ) ;
#210786 = VERTEX_POINT ( 'NONE', #18834 ) ;
#210789 = ORIENTED_EDGE ( 'NONE', *, *, #1803, .T. ) ;
#210788 = CARTESIAN_POINT ( 'NONE',  ( 23.25000000000000000, -8.596261682231828516, -91.04987248284976431 ) ) ;
#210787 = DIRECTION ( 'NONE',  ( 0.000000000000000000, 0.7216758089626587047, -0.6922311945860948335 ) ) ;
#210790 = DIRECTION ( 'NONE',  ( 0.000000000000000000, 0.000000000000000000, -1.000000000000000000 ) ) ;
#210791 = ORIENTED_EDGE ( 'NONE', *, *, #42279, .T. ) ;
#210792 = AXIS2_PLACEMENT_3D ( 'NONE', #54622, #134154, #75504 ) ;
#210793 = ADVANCED_FACE ( 'NONE', ( #98330 ), #83902, .T. ) ;
#210794 = ORIENTED_EDGE ( 'NONE', *, *, #15605, .F. ) ;
#210796 = FACE_OUTER_BOUND ( 'NONE', #112494, .T. ) ;
#210795 =( BOUNDED_SURFACE ( )  B_SPLINE_SURFACE ( 3, 2, ( 
 ( #47419, #184367, #24043 ),
 ( #103538, #183109, #106098 ),
 ( #64438, #5713, #85241 ),
 ( #164825, #86531, #4445 ),
 ( #244341, #186978, #223489 ),
 ( #8330, #83942, #124417 ),
 ( #185667, #207829, #27908 ),
 ( #126976, #65714, #66999 ),
 ( #206511, #87820, #167411 ),
 ( #68294, #147835, #227352 ) ),
 .UNSPECIFIED., .F., .F., .F. ) 
 B_SPLINE_SURFACE_WITH_KNOTS ( ( 4, 2, 2, 2, 4 ),
 ( 3, 3 ),
 ( 0.002161241639767248670, 0.002579950749615824400, 0.002789305304540112482, 0.002893982582002256523, 0.002998659859464400564 ),
 ( 0.000000000000000000, 1.000000000000000000 ),
 .UNSPECIFIED. ) 
 GEOMETRIC_REPRESENTATION_ITEM ( )  RATIONAL_B_SPLINE_SURFACE ( (
 ( 1.000000000000000000, 0.7071067811865475727, 1.000000000000000000),
 ( 1.000000000000000000, 0.7632447400665458570, 1.000000000000000000),
 ( 1.000000000000000000, 0.8158073005108548159, 1.000000000000000000),
 ( 1.000000000000000000, 0.8906973462396701180, 1.000000000000000000),
 ( 1.000000000000000000, 0.9149408947804109626, 1.000000000000000000),
 ( 1.000000000000000000, 0.9493368785273814670, 1.000000000000000000),
 ( 1.000000000000000000, 0.9605194247155539600, 1.000000000000000000),
 ( 1.000000000000000000, 0.9803630264782379200, 1.000000000000000000),
 ( 1.000000000000000000, 0.9900844824270240707, 1.000000000000000000),
 ( 1.000000000000000000, 0.9894588281429241849, 1.000000000000000000) ) ) 
 REPRESENTATION_ITEM ( '' )  SURFACE ( )  );
#210797 = ORIENTED_EDGE ( 'NONE', *, *, #255539, .T. ) ;
#210798 = DIRECTION ( 'NONE',  ( 0.000000000000000000, 0.2617529984165032908, 0.9651348961777156399 ) ) ;
#210799 = CARTESIAN_POINT ( 'NONE',  ( -23.24999999999999645, -9.599999999988845900, -174.2001893912220680 ) ) ;
#210800 = VECTOR ( 'NONE', #199030, 1000.000000000000000 ) ;
#210801 = DIRECTION ( 'NONE',  ( 0.000000000000000000, 0.8700118002898356018, -0.4930308989875170078 ) ) ;
#210802 = AXIS2_PLACEMENT_3D ( 'NONE', #203930, #49997, #169995 ) ;
#210803 = DIRECTION ( 'NONE',  ( -0.000000000000000000, 1.000000000000000000, -0.000000000000000000 ) ) ;
#210804 = AXIS2_PLACEMENT_3D ( 'NONE', #251727, #250435, #71823 ) ;
#210805 = ORIENTED_EDGE ( 'NONE', *, *, #121668, .T. ) ;
#210806 = DIRECTION ( 'NONE',  ( 0.000000000000000000, -0.3738317757009718689, 0.9274965247785342815 ) ) ;
#210807 = CARTESIAN_POINT ( 'NONE',  ( -21.29999999999995808, 1.115600667400684642E-11, -67.00000000000004263 ) ) ;
#210808 = CARTESIAN_POINT ( 'NONE',  ( 21.13498764882293557, 6.495618143485025975, -33.49834360526865851 ) ) ;
#210809 = ORIENTED_EDGE ( 'NONE', *, *, #24637, .F. ) ;
#210810 = EDGE_CURVE ( 'NONE', #210784, #230912, #60483, .T. ) ;
#210811 = DIRECTION ( 'NONE',  ( 1.000000000000000000, 0.000000000000000000, 0.000000000000000000 ) ) ;
#210812 = ORIENTED_EDGE ( 'NONE', *, *, #88795, .T. ) ;
#210813 = DIRECTION ( 'NONE',  ( -1.000000000000000000, 0.000000000000000000, 0.000000000000000000 ) ) ;
#210814 = VERTEX_POINT ( 'NONE', #185623 ) ;
#210815 = DIRECTION ( 'NONE',  ( 0.000000000000000000, 0.1350103645451974088, -0.9908441862701587999 ) ) ;
#210816 = CARTESIAN_POINT ( 'NONE',  ( -22.50047199487426752, 75.95509394809670312, -181.7731549034402008 ) ) ;
#210817 = AXIS2_PLACEMENT_3D ( 'NONE', #193856, #12668, #210846 ) ;
#210819 = ORIENTED_EDGE ( 'NONE', *, *, #28276, .T. ) ;
#210818 = CARTESIAN_POINT ( 'NONE',  ( -16.80621392010893445, 44.17480150332616518, -235.2898609361353124 ) ) ;
#210820 = FACE_OUTER_BOUND ( 'NONE', #103595, .T. ) ;
#210821 = VERTEX_POINT ( 'NONE', #143914 ) ;
#210822 = EDGE_CURVE ( 'NONE', #142573, #140921, #163490, .T. ) ;
#210823 = PLANE ( 'NONE',  #98285 ) ;
#210824 = CARTESIAN_POINT ( 'NONE',  ( -16.79270642812322478, 9.946244216949072126, -113.1610667214380044 ) ) ;
#210825 = EDGE_CURVE ( 'NONE', #15255, #168103, #85194, .T. ) ;
#210826 = ORIENTED_EDGE ( 'NONE', *, *, #145300, .T. ) ;
#210827 = CARTESIAN_POINT ( 'NONE',  ( -18.59999999999999787, 74.36282728704168221, -124.9409541190522930 ) ) ;
#210828 = CARTESIAN_POINT ( 'NONE',  ( -20.00857864376270001, 9.250000000011157297, -79.35000000000005116 ) ) ;
#210829 = ORIENTED_EDGE ( 'NONE', *, *, #235136, .T. ) ;
#210830 = DIRECTION ( 'NONE',  ( 0.000000000000000000, 6.982962677686266711E-15, -1.000000000000000000 ) ) ;
#210831 = AXIS2_PLACEMENT_3D ( 'NONE', #168668, #66940, #108638 ) ;
#210832 = CIRCLE ( 'NONE', #244132, 3.900000000000000799 ) ;
#210833 = VECTOR ( 'NONE', #255590, 1000.000000000000000 ) ;
#210834 = VECTOR ( 'NONE', #40331, 1000.000000000000000 ) ;
#210835 = ORIENTED_EDGE ( 'NONE', *, *, #3112, .T. ) ;
#210836 = EDGE_CURVE ( 'NONE', #237818, #113968, #64772, .T. ) ;
#210837 = DIRECTION ( 'NONE',  ( 1.000000000000000000, 0.000000000000000000, -0.000000000000000000 ) ) ;
#210838 = CARTESIAN_POINT ( 'NONE',  ( -22.59999999999999787, 64.25043287652299284, -170.1239658536231616 ) ) ;
#210839 = EDGE_CURVE ( 'NONE', #218130, #227674, #5667, .T. ) ;
#210840 = ADVANCED_FACE ( 'NONE', ( #103491 ), #125643, .F. ) ;
#210843 = ORIENTED_EDGE ( 'NONE', *, *, #169672, .F. ) ;
#210842 = EDGE_LOOP ( 'NONE', ( #200670, #209333, #88368, #818 ) ) ;
#210841 = DIRECTION ( 'NONE',  ( 0.000000000000000000, 0.000000000000000000, -1.000000000000000000 ) ) ;
#210844 = CARTESIAN_POINT ( 'NONE',  ( 18.59999999999998366, 68.97833521811233481, -166.1895420826271277 ) ) ;
#210845 = DIRECTION ( 'NONE',  ( -1.000000000000000000, 0.000000000000000000, 0.000000000000000000 ) ) ;
#210846 = DIRECTION ( 'NONE',  ( -1.020425574104004196E-15, -1.210927747993693964E-31, 1.000000000000000000 ) ) ;
#210847 = ADVANCED_FACE ( 'NONE', ( #106054 ), #164777, .F. ) ;
#210848 = AXIS2_PLACEMENT_3D ( 'NONE', #224400, #184000, #185290 ) ;
#210850 = LINE ( 'NONE', #171752, #42076 ) ;
#210849 = CARTESIAN_POINT ( 'NONE',  ( -18.50000000000000000, 11.75000000001115197, -54.85000000000000142 ) ) ;
#210851 = DIRECTION ( 'NONE',  ( 1.000000000000000000, 0.000000000000000000, 0.000000000000000000 ) ) ;
#210852 = DIRECTION ( 'NONE',  ( 1.000000000000000000, -0.000000000000000000, -0.000000000000000000 ) ) ;
#210853 = AXIS2_PLACEMENT_3D ( 'NONE', #23664, #180151, #160605 ) ;
#210854 = CARTESIAN_POINT ( 'NONE',  ( -23.15000000000000213, 68.63171270270233038, -223.0506438513196770 ) ) ;
#210855 = ORIENTED_EDGE ( 'NONE', *, *, #102262, .F. ) ;
#210856 = ORIENTED_EDGE ( 'NONE', *, *, #146774, .F. ) ;
#210857 = DIRECTION ( 'NONE',  ( 0.000000000000000000, 0.000000000000000000, 1.000000000000000000 ) ) ;
#210858 = VECTOR ( 'NONE', #196274, 1000.000000000000000 ) ;
#210860 = ORIENTED_EDGE ( 'NONE', *, *, #69423, .T. ) ;
#210859 = CARTESIAN_POINT ( 'NONE',  ( -20.64999999999999858, -6.688413578037177842, -212.5825622730469036 ) ) ;
#210861 = ORIENTED_EDGE ( 'NONE', *, *, #115411, .T. ) ;
#210862 = EDGE_CURVE ( 'NONE', #120061, #53606, #218699, .T. ) ;
#210863 = CARTESIAN_POINT ( 'NONE',  ( -16.77683809663752257, 12.41293291551535916, -211.2574046339461233 ) ) ;
#210864 = ORIENTED_EDGE ( 'NONE', *, *, #20650, .T. ) ;
#210865 = VERTEX_POINT ( 'NONE', #245600 ) ;
#210866 = SPHERICAL_SURFACE ( 'NONE', #18996, 0.1000000000000000056 ) ;
#210867 = DIRECTION ( 'NONE',  ( 0.7071067811865475727, 0.7071067811865475727, 2.044391222244500083E-16 ) ) ;
#210869 = ORIENTED_EDGE ( 'NONE', *, *, #64847, .F. ) ;
#210868 = ORIENTED_EDGE ( 'NONE', *, *, #195307, .F. ) ;
#210870 = EDGE_LOOP ( 'NONE', ( #53410, #56319, #127325, #231581 ) ) ;
#210871 = ORIENTED_EDGE ( 'NONE', *, *, #138232, .F. ) ;
#210872 = VERTEX_POINT ( 'NONE', #207775 ) ;
#210873 = FACE_OUTER_BOUND ( 'NONE', #56492, .T. ) ;
#210874 = CARTESIAN_POINT ( 'NONE',  ( 21.05000000000000071, 43.36285386911620776, -234.7972500504784534 ) ) ;
#210875 = CARTESIAN_POINT ( 'NONE',  ( -21.05000000000000071, 64.21185867012613357, -224.4479740254296303 ) ) ;
#210877 = ORIENTED_EDGE ( 'NONE', *, *, #147658, .T. ) ;
#210876 = DIRECTION ( 'NONE',  ( 0.000000000000000000, 0.000000000000000000, 1.000000000000000000 ) ) ;
#210878 = FACE_OUTER_BOUND ( 'NONE', #97548, .T. ) ;
#210879 = CARTESIAN_POINT ( 'NONE',  ( -20.94999999999999929, 13.66123737402873495, -238.6633470470287648 ) ) ;
#210881 = EDGE_LOOP ( 'NONE', ( #155912, #33049, #30225, #147621 ) ) ;
#210880 = DIRECTION ( 'NONE',  ( 0.000000000000000000, 0.000000000000000000, -1.000000000000000000 ) ) ;
#210882 = CARTESIAN_POINT ( 'NONE',  ( 19.99999999999998934, 11.75000000001115552, -88.35000000000003695 ) ) ;
#210883 = VERTEX_POINT ( 'NONE', #244295 ) ;
#210884 = AXIS2_PLACEMENT_3D ( 'NONE', #170264, #249751, #211922 ) ;
#210885 = ORIENTED_EDGE ( 'NONE', *, *, #193254, .F. ) ;
#210886 = DIRECTION ( 'NONE',  ( 0.000000000000000000, 0.2617529984165152257, 0.9651348961777124202 ) ) ;
#210887 = CARTESIAN_POINT ( 'NONE',  ( -21.05000000000000071, 74.25000000001186606, -91.35359592662267403 ) ) ;
#210888 = AXIS2_PLACEMENT_3D ( 'NONE', #246586, #28884, #204885 ) ;
#210889 = ORIENTED_EDGE ( 'NONE', *, *, #197856, .T. ) ;
#210891 = DIRECTION ( 'NONE',  ( 0.000000000000000000, 0.000000000000000000, -1.000000000000000000 ) ) ;
#210890 = DIRECTION ( 'NONE',  ( 0.000000000000000000, 0.000000000000000000, -1.000000000000000000 ) ) ;
#210892 = CYLINDRICAL_SURFACE ( 'NONE', #60043, 0.09999999999999939493 ) ;
#210893 = TOROIDAL_SURFACE ( 'NONE', #256623, 12.97499999999999787, 0.1000000000000000056 ) ;
#210894 = AXIS2_PLACEMENT_3D ( 'NONE', #210544, #30643, #107576 ) ;
#210895 = EDGE_CURVE ( 'NONE', #71835, #243532, #177244, .T. ) ;
#210896 = LINE ( 'NONE', #94792, #97160 ) ;
#210897 = CARTESIAN_POINT ( 'NONE',  ( -23.39999999999994529, 87.60324567546805952, -34.17184040628037422 ) ) ;
#210898 = VERTEX_POINT ( 'NONE', #65664 ) ;
#210899 = ORIENTED_EDGE ( 'NONE', *, *, #207847, .T. ) ;
#210900 =( BOUNDED_CURVE ( )  B_SPLINE_CURVE ( 3, ( #230197, #189795, #187245, #52832 ),
 .UNSPECIFIED., .F., .F. ) 
 B_SPLINE_CURVE_WITH_KNOTS ( ( 4, 4 ),
 ( 5.731445031868799056, 5.983100554402348337 ),
 .UNSPECIFIED. ) 
 CURVE ( )  GEOMETRIC_REPRESENTATION_ITEM ( )  RATIONAL_B_SPLINE_CURVE ( ( 1.000000000000000000, 0.9947294176030464508, 0.9947294176030464508, 1.000000000000000000 ) ) 
 REPRESENTATION_ITEM ( '' )  );
#210901 = DIRECTION ( 'NONE',  ( -3.265361837132813093E-16, -0.9651348961777157509, 0.2617529984165031243 ) ) ;
#210902 = DIRECTION ( 'NONE',  ( 0.000000000000000000, 0.000000000000000000, -1.000000000000000000 ) ) ;
#210903 = ORIENTED_EDGE ( 'NONE', *, *, #208750, .T. ) ;
#210904 = CARTESIAN_POINT ( 'NONE',  ( -22.59999999999999787, 55.87393739788256397, -232.8427108587849261 ) ) ;
#210905 = VERTEX_POINT ( 'NONE', #44826 ) ;
#210906 = CARTESIAN_POINT ( 'NONE',  ( 23.24999999999999645, 72.10000000001244302, -170.0231074845243882 ) ) ;
#210907 = EDGE_CURVE ( 'NONE', #177021, #121663, #52289, .T. ) ;
#210908 = DIRECTION ( 'NONE',  ( 0.000000000000000000, -0.1350103645451904977, 0.9908441862701596881 ) ) ;
#210909 = CARTESIAN_POINT ( 'NONE',  ( -18.59999999999999787, 85.50000000001259082, -191.3731074845242972 ) ) ;
#210910 = EDGE_CURVE ( 'NONE', #66847, #163406, #247937, .T. ) ;
#210911 = EDGE_CURVE ( 'NONE', #46965, #109416, #4401, .T. ) ;
#210912 = EDGE_LOOP ( 'NONE', ( #183935, #50779, #42445 ) ) ;
#210913 = LINE ( 'NONE', #92236, #6823 ) ;
#210914 = SURFACE_STYLE_FILL_AREA ( #188777 ) ;
#210915 = VECTOR ( 'NONE', #207797, 999.9999999999998863 ) ;
#210916 = ORIENTED_EDGE ( 'NONE', *, *, #181461, .F. ) ;
#210917 = ORIENTED_EDGE ( 'NONE', *, *, #8340, .F. ) ;
#210918 = AXIS2_PLACEMENT_3D ( 'NONE', #13564, #213029, #193488 ) ;
#210919 = ORIENTED_EDGE ( 'NONE', *, *, #50924, .F. ) ;
#210920 = DIRECTION ( 'NONE',  ( 1.000000000000000000, 0.000000000000000000, 0.000000000000000000 ) ) ;
#210921 = LINE ( 'NONE', #11453, #49176 ) ;
#210922 = CARTESIAN_POINT ( 'NONE',  ( -21.12757541349819590, 0.005161215820883788274, -127.5266194287484609 ) ) ;
#210923 = CARTESIAN_POINT ( 'NONE',  ( 20.94999999999999929, 1.115600667400684642E-11, -167.5000000000000284 ) ) ;
#210924 = AXIS2_PLACEMENT_3D ( 'NONE', #24754, #106810, #186377 ) ;
#210925 = EDGE_CURVE ( 'NONE', #181223, #44121, #249897, .T. ) ;
#210927 = CARTESIAN_POINT ( 'NONE',  ( -21.05000000000000071, 35.94660524813657076, -234.4748257877825495 ) ) ;
#210926 = CARTESIAN_POINT ( 'NONE',  ( -18.59999999999999787, 7.128833340094563376, -233.7327013124401276 ) ) ;
#210929 = EDGE_LOOP ( 'NONE', ( #22182, #116979, #81895, #19118, #125345 ) ) ;
#210928 = CARTESIAN_POINT ( 'NONE',  ( -20.00857864376270001, 9.150000000011157653, -54.65000000000000568 ) ) ;
#210930 = CARTESIAN_POINT ( 'NONE',  ( -23.49999999999994316, 82.78482233730476025, -26.42994920107286916 ) ) ;
#210931 = ORIENTED_EDGE ( 'NONE', *, *, #63703, .F. ) ;
#210932 = AXIS2_PLACEMENT_3D ( 'NONE', #178069, #97176, #138877 ) ;
#210933 = EDGE_CURVE ( 'NONE', #142313, #201052, #252035, .T. ) ;
#210934 = DIRECTION ( 'NONE',  ( 1.000000000000000000, 0.000000000000000000, 0.000000000000000000 ) ) ;
#210935 = AXIS2_PLACEMENT_3D ( 'NONE', #111452, #249687, #93163 ) ;
#210936 = ORIENTED_EDGE ( 'NONE', *, *, #215986, .T. ) ;
#210937 = ORIENTED_EDGE ( 'NONE', *, *, #173127, .F. ) ;
#210938 = CARTESIAN_POINT ( 'NONE',  ( -16.93658211146644987, 66.00589133767032024, -48.61881241456871550 ) ) ;
#210939 = DIRECTION ( 'NONE',  ( 1.000000000000000000, -2.952720810173289112E-16, -2.061873921506763405E-30 ) ) ;
#210940 = CARTESIAN_POINT ( 'NONE',  ( -23.15000000000000213, 70.60814576644823148, -215.7631455941064189 ) ) ;
#210941 = DIRECTION ( 'NONE',  ( 0.000000000000000000, 0.000000000000000000, 1.000000000000000000 ) ) ;
#210942 = AXIS2_PLACEMENT_3D ( 'NONE', #124289, #85108, #43455 ) ;
#210943 = CARTESIAN_POINT ( 'NONE',  ( 22.57320508075687115, 55.89093952297024970, -232.7795287750844579 ) ) ;
#210945 = ORIENTED_EDGE ( 'NONE', *, *, #99702, .F. ) ;
#210944 =( GEOMETRIC_REPRESENTATION_CONTEXT ( 3 ) GLOBAL_UNCERTAINTY_ASSIGNED_CONTEXT ( ( #85677 ) ) GLOBAL_UNIT_ASSIGNED_CONTEXT ( ( #111500, #93207, #89347 ) ) REPRESENTATION_CONTEXT ( 'NONE', 'WORKASPACE' ) );
#210946 = ORIENTED_EDGE ( 'NONE', *, *, #98074, .T. ) ;
#210947 = CIRCLE ( 'NONE', #65194, 0.09999999999999767408 ) ;
#210948 = ADVANCED_FACE ( 'NONE', ( #94210 ), #53812, .T. ) ;
#210949 = DIRECTION ( 'NONE',  ( -1.000000000000000000, -2.952720810173289112E-16, 0.000000000000000000 ) ) ;
#210951 = ORIENTED_EDGE ( 'NONE', *, *, #78408, .F. ) ;
#210950 = EDGE_CURVE ( 'NONE', #160550, #58185, #9539, .T. ) ;
#210952 = DIRECTION ( 'NONE',  ( -1.000000000000000000, 3.265361837132813093E-16, 2.280189983783949500E-30 ) ) ;
#210953 = CARTESIAN_POINT ( 'NONE',  ( -21.05000000000000426, 11.60000000000000320, -6.928203230275554958 ) ) ;
#210954 = VERTEX_POINT ( 'NONE', #209036 ) ;
#210955 = EDGE_CURVE ( 'NONE', #37312, #192475, #227087, .T. ) ;
#210956 = DIRECTION ( 'NONE',  ( 0.000000000000000000, -0.2868887416115947775, 0.9579639084728169829 ) ) ;
#210957 = DIRECTION ( 'NONE',  ( -2.952720810173288619E-16, 1.000000000000000000, 0.000000000000000000 ) ) ;
#210958 = CARTESIAN_POINT ( 'NONE',  ( -18.52328366898032996, -9.642321089030088999, -207.7148193375699918 ) ) ;
#210959 = CARTESIAN_POINT ( 'NONE',  ( 18.39999999999999858, 85.50000000001189449, -95.99103808782457747 ) ) ;
#210960 = ORIENTED_EDGE ( 'NONE', *, *, #228413, .F. ) ;
#210961 = CARTESIAN_POINT ( 'NONE',  ( 22.60000000000000142, 75.95218160930696172, -81.27312990357155797 ) ) ;
#210962 = CARTESIAN_POINT ( 'NONE',  ( -23.25000000000000000, 2.600000000011156054, -120.7753780772379315 ) ) ;
#210963 = DIRECTION ( 'NONE',  ( 0.000000000000000000, 6.982962677686266711E-15, -1.000000000000000000 ) ) ;
#210964 = CARTESIAN_POINT ( 'NONE',  ( -21.05000000000000071, 87.75000000001143974, -39.02310748452423894 ) ) ;
#210965 = AXIS2_PLACEMENT_3D ( 'NONE', #39941, #115592, #135139 ) ;
#210966 = EDGE_CURVE ( 'NONE', #10053, #189338, #147378, .T. ) ;
#210967 = CARTESIAN_POINT ( 'NONE',  ( 20.85000000000000142, -11.74999999999999112, -30.59999999999999432 ) ) ;
#210968 = ORIENTED_EDGE ( 'NONE', *, *, #119904, .F. ) ;
#210969 = CARTESIAN_POINT ( 'NONE',  ( 21.05000000000000071, -0.09999999998884510910, -161.0229536182100958 ) ) ;
#210970 = EDGE_LOOP ( 'NONE', ( #223334, #82319, #84566, #158194, #97397, #98075, #80111, #54317, #98167 ) ) ;
#210971 = CARTESIAN_POINT ( 'NONE',  ( 20.94999999999999929, 61.95000000001218154, -142.0368025552853624 ) ) ;
#210972 = CARTESIAN_POINT ( 'NONE',  ( -16.93294127766158752, 14.22806568586737264, -219.3218115319804156 ) ) ;
#210973 = CYLINDRICAL_SURFACE ( 'NONE', #154444, 0.09999999999999568956 ) ;
#210975 = AXIS2_PLACEMENT_3D ( 'NONE', #39876, #158541, #138906 ) ;
#210974 = DIRECTION ( 'NONE',  ( -1.000000000000000000, 0.000000000000000000, -0.000000000000000000 ) ) ;
#210976 = CARTESIAN_POINT ( 'NONE',  ( 23.24999999999999645, 3.318160649989770672, -234.5626251938229245 ) ) ;
#210977 = DIRECTION ( 'NONE',  ( 1.000000000000000000, 0.000000000000000000, 0.000000000000000000 ) ) ;
#210979 = ORIENTED_EDGE ( 'NONE', *, *, #808, .T. ) ;
#210978 = AXIS2_PLACEMENT_3D ( 'NONE', #69723, #172712, #29335 ) ;
#210980 = EDGE_CURVE ( 'NONE', #161314, #177537, #73409, .T. ) ;
#210981 = CARTESIAN_POINT ( 'NONE',  ( 20.94999999999999929, 5.850000000011160495, -123.8675027757221017 ) ) ;
#210982 = CARTESIAN_POINT ( 'NONE',  ( 21.13920837816993270, 67.21675294989213967, -124.2731074845243597 ) ) ;
#210983 = AXIS2_PLACEMENT_3D ( 'NONE', #181723, #203839, #25231 ) ;
#210984 = DIRECTION ( 'NONE',  ( 1.000000000000000000, -7.136802563874200093E-16, -1.554319503706932210E-16 ) ) ;
#210985 = CARTESIAN_POINT ( 'NONE',  ( -23.15000000000000213, 64.35000000001205933, -124.2731074845243882 ) ) ;
#210986 = LINE ( 'NONE', #10228, #136532 ) ;
#210987 = VECTOR ( 'NONE', #193841, 1000.000000000000000 ) ;
#210988 = ORIENTED_EDGE ( 'NONE', *, *, #251912, .F. ) ;
#210989 = ORIENTED_EDGE ( 'NONE', *, *, #201049, .F. ) ;
#210990 = DIRECTION ( 'NONE',  ( -1.000000000000000000, 0.000000000000000000, -0.000000000000000000 ) ) ;
#210991 = DIRECTION ( 'NONE',  ( 0.000000000000000000, 0.000000000000000000, 1.000000000000000000 ) ) ;
#210993 = EDGE_CURVE ( 'NONE', #75171, #229678, #127136, .T. ) ;
#210992 = CARTESIAN_POINT ( 'NONE',  ( 18.49999999999999289, 10.32573593129922607, -91.85000000000003695 ) ) ;
#210994 = CARTESIAN_POINT ( 'NONE',  ( 18.59999999999999432, 43.57568952063339651, -245.1784935019914826 ) ) ;
#210995 = CARTESIAN_POINT ( 'NONE',  ( -23.15000000000000213, -9.499999999988846255, -57.10603087734755690 ) ) ;
#210996 = AXIS2_PLACEMENT_3D ( 'NONE', #183025, #203847, #25237 ) ;
#210997 = ORIENTED_EDGE ( 'NONE', *, *, #62259, .F. ) ;
#210998 = CARTESIAN_POINT ( 'NONE',  ( 22.94999999999999929, -11.64999999999999858, 11.99999999999999645 ) ) ;
#210999 = ADVANCED_FACE ( 'NONE', ( #152950 ), #232472, .F. ) ;
#211000 = CIRCLE ( 'NONE', #165194, 11.75000000000000000 ) ;
#211001 = CARTESIAN_POINT ( 'NONE',  ( -23.25000000000000355, 64.25000000001179501, -78.77310748452440237 ) ) ;
#211002 = AXIS2_PLACEMENT_3D ( 'NONE', #221555, #105451, #147179 ) ;
#211003 = ORIENTED_EDGE ( 'NONE', *, *, #94958, .F. ) ;
#211004 = CARTESIAN_POINT ( 'NONE',  ( 23.15000000000000213, 85.00000000001261924, -193.6291383618718385 ) ) ;
#211005 = EDGE_CURVE ( 'NONE', #174802, #248032, #98063, .T. ) ;
#211006 = EDGE_CURVE ( 'NONE', #241107, #42365, #113777, .T. ) ;
#211007 = EDGE_LOOP ( 'NONE', ( #153273, #169282, #218898, #202562 ) ) ;
#211008 = EDGE_LOOP ( 'NONE', ( #241301, #101416, #329, #139113 ) ) ;
#211009 = CIRCLE ( 'NONE', #244125, 0.09999999999999609201 ) ;
#211010 = ORIENTED_EDGE ( 'NONE', *, *, #95176, .F. ) ;
#211011 = DIRECTION ( 'NONE',  ( -1.000000000000000000, -2.952720810173289112E-16, 0.000000000000000000 ) ) ;
#211012 = DIRECTION ( 'NONE',  ( -1.000000000000000000, 0.000000000000000000, 0.000000000000000000 ) ) ;
#211013 = CARTESIAN_POINT ( 'NONE',  ( 21.14999999999999858, 10.71339244341104013, -112.7500000000000284 ) ) ;
#211014 = DIRECTION ( 'NONE',  ( 0.000000000000000000, -1.000000000000000000, 0.000000000000000000 ) ) ;
#211015 = CYLINDRICAL_SURFACE ( 'NONE', #186247, 0.09999999999999939493 ) ;
#211016 = CARTESIAN_POINT ( 'NONE',  ( 21.05000000000000071, 87.75000000001192291, -106.1231074845242262 ) ) ;
#211017 = DIRECTION ( 'NONE',  ( -0.000000000000000000, 0.9126074666063770380, 0.4088369013363281068 ) ) ;
#211018 = DIRECTION ( 'NONE',  ( -0.5932847527679299127, 0.8049926720990051576, 6.366092712777055223E-16 ) ) ;
#211019 = EDGE_CURVE ( 'NONE', #55818, #177471, #243839, .T. ) ;
#211020 = CARTESIAN_POINT ( 'NONE',  ( 18.49999999999999289, 67.84340367245323478, -228.0791829662263410 ) ) ;
#211021 = CARTESIAN_POINT ( 'NONE',  ( 21.04999999999997229, 22.02795578261032716, -231.6498538120116280 ) ) ;
#211022 = CARTESIAN_POINT ( 'NONE',  ( -20.00857864376270001, 9.150000000011157653, -155.1500000000000057 ) ) ;
#211023 = CARTESIAN_POINT ( 'NONE',  ( 20.95520789717937404, 18.80512403970892166, -227.9885191826238895 ) ) ;
#211024 = AXIS2_PLACEMENT_3D ( 'NONE', #234708, #215140, #56034 ) ;
#211025 = ORIENTED_EDGE ( 'NONE', *, *, #246962, .F. ) ;
#211026 = AXIS2_PLACEMENT_3D ( 'NONE', #129626, #228744, #110055 ) ;
#211027 = FACE_OUTER_BOUND ( 'NONE', #103827, .T. ) ;
#211028 = CIRCLE ( 'NONE', #127826, 4.000000000000003553 ) ;
#211029 = EDGE_CURVE ( 'NONE', #183881, #14506, #33019, .T. ) ;
#211030 = CARTESIAN_POINT ( 'NONE',  ( 18.59999999999999787, 76.00000000001195133, -103.0231074845243171 ) ) ;
#211031 = DIRECTION ( 'NONE',  ( 0.000000000000000000, 0.000000000000000000, 1.000000000000000000 ) ) ;
#211032 = DIRECTION ( 'NONE',  ( 0.000000000000000000, 0.000000000000000000, -1.000000000000000000 ) ) ;
#211034 = EDGE_CURVE ( 'NONE', #91128, #87157, #81312, .T. ) ;
#211033 = CARTESIAN_POINT ( 'NONE',  ( 18.59999999999999432, 65.87552587769046397, -245.8195358697090001 ) ) ;
#211035 = CARTESIAN_POINT ( 'NONE',  ( -20.65000000000000568, 42.13647595316535188, -239.1530172309881834 ) ) ;
#211036 = VERTEX_POINT ( 'NONE', #116368 ) ;
#211037 = VERTEX_POINT ( 'NONE', #215447 ) ;
#211038 = EDGE_CURVE ( 'NONE', #1286, #245188, #84558, .T. ) ;
#211039 = DIRECTION ( 'NONE',  ( -0.000000000000000000, -1.000000000000000000, -1.734723475976807292E-15 ) ) ;
#211040 = AXIS2_PLACEMENT_3D ( 'NONE', #235319, #213184, #72425 ) ;
#211041 = ORIENTED_EDGE ( 'NONE', *, *, #240835, .T. ) ;
#211042 = CARTESIAN_POINT ( 'NONE',  ( -21.05000000000000071, 87.65000000001235492, -167.1231074845242688 ) ) ;
#211043 = DIRECTION ( 'NONE',  ( 0.000000000000000000, 0.000000000000000000, 1.000000000000000000 ) ) ;
#211044 = ADVANCED_FACE ( 'NONE', ( #102859 ), #102161, .T. ) ;
#211045 = CIRCLE ( 'NONE', #119464, 11.80000000000000782 ) ;
#211046 = VECTOR ( 'NONE', #237401, 1000.000000000000000 ) ;
#211047 = CIRCLE ( 'NONE', #160986, 0.09999999999999939493 ) ;
#211048 = ORIENTED_EDGE ( 'NONE', *, *, #111400, .F. ) ;
#211049 = FACE_OUTER_BOUND ( 'NONE', #24739, .T. ) ;
#211050 = ORIENTED_EDGE ( 'NONE', *, *, #51930, .F. ) ;
#211051 = EDGE_CURVE ( 'NONE', #85452, #158852, #63756, .T. ) ;
#211052 = CARTESIAN_POINT ( 'NONE',  ( -21.44999999999999929, 68.65000000001205649, -124.1731074845243512 ) ) ;
#211053 = ADVANCED_FACE ( 'NONE', ( #156794 ), #143292, .T. ) ;
#211054 = DIRECTION ( 'NONE',  ( -0.000000000000000000, 0.8814952561688430555, -0.4721928772777346239 ) ) ;
#211055 = LINE ( 'NONE', #53264, #132618 ) ;
#211056 = DIRECTION ( 'NONE',  ( -0.000000000000000000, -0.000000000000000000, 1.000000000000000000 ) ) ;
#211057 = LINE ( 'NONE', #71569, #225916 ) ;
#211058 = LINE ( 'NONE', #70294, #74769 ) ;
#211060 = ORIENTED_EDGE ( 'NONE', *, *, #119316, .F. ) ;
#211059 = CARTESIAN_POINT ( 'NONE',  ( -18.45068461519105796, -9.486506529077932015, -40.56877716890470964 ) ) ;
#211062 = CARTESIAN_POINT ( 'NONE',  ( -20.64999999999999858, -8.663551401858001100, -57.47589888193270014 ) ) ;
#211061 = DIRECTION ( 'NONE',  ( -0.000000000000000000, -0.9126074666063770380, -0.4088369013363281068 ) ) ;
#211063 = ORIENTED_EDGE ( 'NONE', *, *, #189917, .T. ) ;
#211065 = ORIENTED_EDGE ( 'NONE', *, *, #89183, .T. ) ;
#211064 = DIRECTION ( 'NONE',  ( 1.000000000000000000, 0.000000000000000000, 0.000000000000000000 ) ) ;
#211066 = AXIS2_PLACEMENT_3D ( 'NONE', #50179, #11073, #14941 ) ;
#211067 = VERTEX_POINT ( 'NONE', #24669 ) ;
#211068 = DIRECTION ( 'NONE',  ( 1.000000000000000000, 0.000000000000000000, 0.000000000000000000 ) ) ;
#211069 = CARTESIAN_POINT ( 'NONE',  ( 20.02499999999999858, 9.749999999999998224, -21.15000000000000213 ) ) ;
#211070 = LINE ( 'NONE', #15451, #217160 ) ;
#211071 = LINE ( 'NONE', #225471, #214057 ) ;
#211072 = FACE_OUTER_BOUND ( 'NONE', #158595, .T. ) ;
#211074 = DIRECTION ( 'NONE',  ( 0.000000000000000000, -0.8814952561688430555, 0.4721928772777346239 ) ) ;
#211073 = CIRCLE ( 'NONE', #119494, 0.09999999999999609201 ) ;
#211075 = DIRECTION ( 'NONE',  ( -1.000000000000000000, 0.000000000000000000, -0.000000000000000000 ) ) ;
#211077 = AXIS2_PLACEMENT_3D ( 'NONE', #202672, #200117, #142686 ) ;
#211076 = DIRECTION ( 'NONE',  ( -1.000000000000000000, -0.000000000000000000, -0.000000000000000000 ) ) ;
#211078 = VERTEX_POINT ( 'NONE', #182442 ) ;
#211079 = ORIENTED_EDGE ( 'NONE', *, *, #204308, .F. ) ;
#211080 = DIRECTION ( 'NONE',  ( -0.7071067811865474617, -0.6909108974501236844, -0.1504730267678055788 ) ) ;
#211081 = TOROIDAL_SURFACE ( 'NONE', #127703, 0.2000000000000000111, 0.1000000000000000056 ) ;
#211082 = TOROIDAL_SURFACE ( 'NONE', #102907, 0.2000000000000000111, 0.1000000000000000056 ) ;
#211083 = ADVANCED_FACE ( 'NONE', ( #243682 ), #158097, .T. ) ;
#211084 = ORIENTED_EDGE ( 'NONE', *, *, #69222, .T. ) ;
#211085 = DIRECTION ( 'NONE',  ( 1.000000000000000000, 0.000000000000000000, 0.000000000000000000 ) ) ;
#211086 = ORIENTED_EDGE ( 'NONE', *, *, #125661, .F. ) ;
#211087 = CARTESIAN_POINT ( 'NONE',  ( 18.31325810956328937, -9.536388476007093828, -40.36844020630490348 ) ) ;
#211088 = DIRECTION ( 'NONE',  ( 0.000000000000000000, 0.000000000000000000, 1.000000000000000000 ) ) ;
#211089 = DIRECTION ( 'NONE',  ( 1.000000000000000000, -0.000000000000000000, -0.000000000000000000 ) ) ;
#211090 = AXIS2_PLACEMENT_3D ( 'NONE', #248801, #53153, #212248 ) ;
#211091 = CARTESIAN_POINT ( 'NONE',  ( 20.85000000000000142, 0.000000000000000000, -33.50000000000000000 ) ) ;
#211092 = DIRECTION ( 'NONE',  ( 1.000000000000000000, 0.000000000000000000, 0.000000000000000000 ) ) ;
#211093 = ORIENTED_EDGE ( 'NONE', *, *, #184921, .F. ) ;
#211094 = CARTESIAN_POINT ( 'NONE',  ( -18.52309608778520911, -9.642476320044041316, -207.7145963411695959 ) ) ;
#211095 = DIRECTION ( 'NONE',  ( -1.000000000000000000, 2.952720810173289112E-16, 2.061873921506763405E-30 ) ) ;
#211096 = DIRECTION ( 'NONE',  ( 0.000000000000000000, -1.000000000000000000, 0.000000000000000000 ) ) ;
#211097 = DIRECTION ( 'NONE',  ( 1.000000000000000000, 3.816239940179503281E-14, -1.218904804407150903E-14 ) ) ;
#211098 = CARTESIAN_POINT ( 'NONE',  ( 20.04142135623730070, 11.75000000001115907, -125.1500000000000341 ) ) ;
#211100 = ADVANCED_FACE ( 'NONE', ( #164155 ), #38116, .T. ) ;
#211099 = CYLINDRICAL_SURFACE ( 'NONE', #226813, 0.1000000000000028644 ) ;
#211101 = ORIENTED_EDGE ( 'NONE', *, *, #133824, .T. ) ;
#211103 = CARTESIAN_POINT ( 'NONE',  ( -18.50000000000000000, 85.40000000001138858, -29.14106563635158764 ) ) ;
#211102 = CARTESIAN_POINT ( 'NONE',  ( -16.97092634996741722, 60.88504535834231035, -221.0475723052460069 ) ) ;
#211104 = ORIENTED_EDGE ( 'NONE', *, *, #72564, .F. ) ;
#211107 = VERTEX_POINT ( 'NONE', #235026 ) ;
#211106 = CARTESIAN_POINT ( 'NONE',  ( -18.59999999999999787, 68.97833521811131163, -32.18954208262707795 ) ) ;
#211105 = CARTESIAN_POINT ( 'NONE',  ( 20.94999999999999929, 5.000000000011153745, -88.09473398108696074 ) ) ;
#211108 = DIRECTION ( 'NONE',  ( 1.000000000000000000, 0.000000000000000000, -0.000000000000000000 ) ) ;
#211109 = AXIS2_PLACEMENT_3D ( 'NONE', #82477, #62948, #142474 ) ;
#211110 = VECTOR ( 'NONE', #202276, 1000.000000000000000 ) ;
#211111 = CARTESIAN_POINT ( 'NONE',  ( 18.59999999999999076, 11.65000000001115943, -134.0000000000000284 ) ) ;
#211112 = ORIENTED_EDGE ( 'NONE', *, *, #144761, .F. ) ;
#211113 = FACE_OUTER_BOUND ( 'NONE', #166253, .T. ) ;
#211114 = AXIS2_PLACEMENT_3D ( 'NONE', #44636, #82438, #62909 ) ;
#211115 = DIRECTION ( 'NONE',  ( -0.000000000000000000, 0.000000000000000000, 1.000000000000000000 ) ) ;
#211116 = CIRCLE ( 'NONE', #127915, 0.1999999999999987899 ) ;
#211118 = LINE ( 'NONE', #147287, #105236 ) ;
#211117 = CARTESIAN_POINT ( 'NONE',  ( 21.00000000000000000, 9.750000000011153745, -54.65000000000000568 ) ) ;
#211119 = CIRCLE ( 'NONE', #131999, 0.2000000000000057288 ) ;
#211121 = VERTEX_POINT ( 'NONE', #222819 ) ;
#211120 = CARTESIAN_POINT ( 'NONE',  ( -20.64999999999999858, 68.85000000001205933, -124.2731074845243455 ) ) ;
#211122 = ORIENTED_EDGE ( 'NONE', *, *, #104602, .F. ) ;
#211123 = DIRECTION ( 'NONE',  ( 0.000000000000000000, -0.9915357197604792727, 0.1298341882520473722 ) ) ;
#211124 = CARTESIAN_POINT ( 'NONE',  ( 18.43579564894474387, -9.519327535281719932, -73.97297664385990856 ) ) ;
#211125 = CARTESIAN_POINT ( 'NONE',  ( -23.15000000000000213, 82.22731448072437388, -214.9453318841612486 ) ) ;
#211126 = ORIENTED_EDGE ( 'NONE', *, *, #157312, .F. ) ;
#211128 = AXIS2_PLACEMENT_3D ( 'NONE', #86460, #143889, #181745 ) ;
#211127 = DIRECTION ( 'NONE',  ( -1.000000000000000000, -0.000000000000000000, -0.000000000000000000 ) ) ;
#211129 = DIRECTION ( 'NONE',  ( 1.000000000000000000, 2.885090398161910739E-16, 6.283419270304611573E-17 ) ) ;
#211130 = CARTESIAN_POINT ( 'NONE',  ( -21.14999999999999858, 64.35000000001214460, -136.4231074845243938 ) ) ;
#211131 = ORIENTED_EDGE ( 'NONE', *, *, #94548, .F. ) ;
#211132 = CARTESIAN_POINT ( 'NONE',  ( 20.77526135991770317, 60.82735416649695281, -225.3438353432380552 ) ) ;
#211133 = CARTESIAN_POINT ( 'NONE',  ( 21.05000000000000071, 1.115600667400684642E-11, -67.00000000000004263 ) ) ;
#211134 = ADVANCED_FACE ( 'NONE', ( #44211 ), #15872, .T. ) ;
#211135 = TOROIDAL_SURFACE ( 'NONE', #73793, 0.2000000000000000111, 0.1000000000000000056 ) ;
#211136 = ORIENTED_EDGE ( 'NONE', *, *, #86201, .T. ) ;
#211137 = DIRECTION ( 'NONE',  ( 0.000000000000000000, 0.000000000000000000, 1.000000000000000000 ) ) ;
#211138 = DIRECTION ( 'NONE',  ( 0.000000000000000000, 0.8814952561688429444, -0.4721928772777347350 ) ) ;
#211139 = ORIENTED_EDGE ( 'NONE', *, *, #153683, .F. ) ;
#211140 = VERTEX_POINT ( 'NONE', #95500 ) ;
#211141 = EDGE_CURVE ( 'NONE', #62395, #9358, #159864, .T. ) ;
#211142 = CARTESIAN_POINT ( 'NONE',  ( -20.85000000000000142, 87.24382154048164750, -206.5725299160771726 ) ) ;
#211143 = ORIENTED_EDGE ( 'NONE', *, *, #17389, .F. ) ;
#211145 = ORIENTED_EDGE ( 'NONE', *, *, #222663, .F. ) ;
#211144 = CARTESIAN_POINT ( 'NONE',  ( -21.44999999999999929, 7.350000000011155166, -45.85000000000000142 ) ) ;
#211146 = ADVANCED_FACE ( 'NONE', ( #197160 ), #118938, .T. ) ;
#211147 = ORIENTED_EDGE ( 'NONE', *, *, #8333, .T. ) ;
#211148 = VECTOR ( 'NONE', #20028, 1000.000000000000000 ) ;
#211151 = VERTEX_POINT ( 'NONE', #138453 ) ;
#211150 = ORIENTED_EDGE ( 'NONE', *, *, #217480, .T. ) ;
#211149 = DIRECTION ( 'NONE',  ( 1.000000000000000000, 0.000000000000000000, -0.000000000000000000 ) ) ;
#211152 = AXIS2_PLACEMENT_3D ( 'NONE', #156750, #154199, #237544 ) ;
#211153 = CIRCLE ( 'NONE', #169697, 0.1000000000000028644 ) ;
#211154 = DIRECTION ( 'NONE',  ( -1.000000000000000000, 0.000000000000000000, 0.000000000000000000 ) ) ;
#211156 = EDGE_CURVE ( 'NONE', #175543, #52387, #77239, .T. ) ;
#211155 = ORIENTED_EDGE ( 'NONE', *, *, #104544, .T. ) ;
#211157 = DIRECTION ( 'NONE',  ( -1.000000000000000000, -0.000000000000000000, -0.000000000000000000 ) ) ;
#211158 = CARTESIAN_POINT ( 'NONE',  ( -18.34374000495060386, 11.47316190337362585, -42.74999999999999289 ) ) ;
#211159 = CARTESIAN_POINT ( 'NONE',  ( -23.15000000000000213, 59.09741375357241111, -220.9566262969074444 ) ) ;
#211160 = AXIS2_PLACEMENT_3D ( 'NONE', #148654, #53386, #172094 ) ;
#211161 = DIRECTION ( 'NONE',  ( 0.000000000000000000, 0.000000000000000000, 1.000000000000000000 ) ) ;
#211162 = CARTESIAN_POINT ( 'NONE',  ( 21.14999999999999858, 11.75000000001116263, -179.6499999999999773 ) ) ;
#211163 = ORIENTED_EDGE ( 'NONE', *, *, #107470, .F. ) ;
#211164 = ORIENTED_EDGE ( 'NONE', *, *, #137930, .F. ) ;
#211165 = ORIENTED_EDGE ( 'NONE', *, *, #13213, .T. ) ;
#211166 = CARTESIAN_POINT ( 'NONE',  ( 23.14999999999999858, 4.813084112160680661, -45.44151775652382952 ) ) ;
#211168 = ORIENTED_EDGE ( 'NONE', *, *, #116727, .T. ) ;
#211167 = CARTESIAN_POINT ( 'NONE',  ( -16.93521499325732194, 66.00521388020901270, -182.6159989434308955 ) ) ;
#211169 = CARTESIAN_POINT ( 'NONE',  ( -21.37071067811865532, 8.070710678129811910, -45.75000000000000000 ) ) ;
#211171 = VERTEX_POINT ( 'NONE', #125033 ) ;
#211170 = DIRECTION ( 'NONE',  ( 1.000000000000000000, -3.265361837132813093E-16, -2.280189983783949500E-30 ) ) ;
#211172 = EDGE_CURVE ( 'NONE', #140599, #59542, #222987, .T. ) ;
#211173 = ORIENTED_EDGE ( 'NONE', *, *, #145877, .T. ) ;
#211174 = CARTESIAN_POINT ( 'NONE',  ( -20.00857864376270001, 9.150000000011157653, -45.85000000000000142 ) ) ;
#211175 = AXIS2_PLACEMENT_3D ( 'NONE', #50822, #70457, #126541 ) ;
#211176 = VECTOR ( 'NONE', #136585, 1000.000000000000000 ) ;
#211177 = ORIENTED_EDGE ( 'NONE', *, *, #83450, .T. ) ;
#211178 = CARTESIAN_POINT ( 'NONE',  ( -21.04999999999994387, 67.75000000001118394, -5.923107484524791744 ) ) ;
#211179 = CARTESIAN_POINT ( 'NONE',  ( -21.05000000000000071, 75.96636726467876599, -176.2819246792058152 ) ) ;
#211180 = B_SPLINE_CURVE_WITH_KNOTS ( 'NONE', 3,
 ( #146988, #44061, #244811, #203127, #27095, #145707, #227822, #187432, #109148, #188699, #225234, #148298, #46599, #126144 ),
 .UNSPECIFIED., .F., .F.,
 ( 4, 2, 2, 2, 2, 2, 4 ),
 ( 0.000000000000000000, 2.389617747641528420E-05, 4.779235495283056841E-05, 9.558470990567925654E-05, 0.0001911694198113798448, 0.0003823388396228040876, 0.0007646776792456565306 ),
 .UNSPECIFIED. ) ;
#211182 = ORIENTED_EDGE ( 'NONE', *, *, #252491, .T. ) ;
#211181 = EDGE_LOOP ( 'NONE', ( #99136, #21709, #138712, #225256 ) ) ;
#211183 = VERTEX_POINT ( 'NONE', #10224 ) ;
#211184 = EDGE_LOOP ( 'NONE', ( #123205, #147795, #52483, #136475 ) ) ;
#211185 = ORIENTED_EDGE ( 'NONE', *, *, #178228, .T. ) ;
#211186 = DIRECTION ( 'NONE',  ( -1.000000000000000000, -0.000000000000000000, -0.000000000000000000 ) ) ;
#211188 = EDGE_LOOP ( 'NONE', ( #233037, #35392, #3076, #162999, #120403, #210750, #225620, #50309, #250230, #68425, #102450, #87287, #34820, #45022, #104548, #177162 ) ) ;
#211187 = CARTESIAN_POINT ( 'NONE',  ( -21.14999999999999858, 18.77629512215284535, -226.6423040988329092 ) ) ;
#211189 = CARTESIAN_POINT ( 'NONE',  ( -16.27683809663750480, 9.350000000011133849, -42.75000000000000000 ) ) ;
#211191 = DIRECTION ( 'NONE',  ( -0.000000000000000000, 0.000000000000000000, -1.000000000000000000 ) ) ;
#211190 = FACE_OUTER_BOUND ( 'NONE', #73501, .T. ) ;
#211192 = DIRECTION ( 'NONE',  ( 1.000000000000000000, 0.000000000000000000, 0.000000000000000000 ) ) ;
#211193 = CARTESIAN_POINT ( 'NONE',  ( 20.94999999999999929, 5.000000000011153745, -88.09473398108696074 ) ) ;
#211194 = ORIENTED_EDGE ( 'NONE', *, *, #214189, .F. ) ;
#211195 = ORIENTED_EDGE ( 'NONE', *, *, #203920, .F. ) ;
#211196 = FACE_OUTER_BOUND ( 'NONE', #49366, .T. ) ;
#211197 = FACE_OUTER_BOUND ( 'NONE', #17497, .T. ) ;
#211198 = CARTESIAN_POINT ( 'NONE',  ( -18.38204789744325396, 64.52049896284640340, -45.27310748452440947 ) ) ;
#211199 = VERTEX_POINT ( 'NONE', #68921 ) ;
#211200 = CIRCLE ( 'NONE', #86275, 0.09999999999999609201 ) ;
#211201 = CIRCLE ( 'NONE', #98728, 0.5000000000000002220 ) ;
#211202 = CIRCLE ( 'NONE', #244507, 14.30833333333333890 ) ;
#211203 = AXIS2_PLACEMENT_3D ( 'NONE', #186590, #228278, #7950 ) ;
#211204 = ADVANCED_FACE ( 'NONE', ( #25930 ), #85582, .F. ) ;
#211205 = CARTESIAN_POINT ( 'NONE',  ( -16.93344882324368683, 51.65733344460321064, -231.8781845289940691 ) ) ;
#211206 = CARTESIAN_POINT ( 'NONE',  ( 21.14999999999999503, 12.67709964810648238, -223.3751320524553705 ) ) ;
#211207 = ORIENTED_EDGE ( 'NONE', *, *, #121490, .F. ) ;
#211208 = ORIENTED_EDGE ( 'NONE', *, *, #94182, .T. ) ;
#211209 = DIRECTION ( 'NONE',  ( 0.000000000000000000, -1.000000000000000000, 0.000000000000000000 ) ) ;
#211210 = CARTESIAN_POINT ( 'NONE',  ( 21.14999999999999858, 69.45000000001157048, -57.17310748452436542 ) ) ;
#211211 = ORIENTED_EDGE ( 'NONE', *, *, #65345, .T. ) ;
#211212 = CARTESIAN_POINT ( 'NONE',  ( -18.44362607810620602, -9.490496158073669974, -174.5579538668471855 ) ) ;
#211213 = ORIENTED_EDGE ( 'NONE', *, *, #153951, .T. ) ;
#211214 = CARTESIAN_POINT ( 'NONE',  ( 18.48413544395661745, -9.664304033616602396, -140.6831049930383131 ) ) ;
#211216 = EDGE_CURVE ( 'NONE', #239961, #235074, #225383, .T. ) ;
#211215 = FACE_OUTER_BOUND ( 'NONE', #231721, .T. ) ;
#211218 = DIRECTION ( 'NONE',  ( -1.000000000000000000, 0.000000000000000000, 0.000000000000000000 ) ) ;
#211217 = CARTESIAN_POINT ( 'NONE',  ( -20.64999999999999858, 36.65892442174935439, -249.5511627012433848 ) ) ;
#211219 = DIRECTION ( 'NONE',  ( 1.000000000000000000, 0.000000000000000000, 0.000000000000000000 ) ) ;
#211220 = CARTESIAN_POINT ( 'NONE',  ( 18.45068634130096186, -9.486506073331606004, -174.5687784311680844 ) ) ;
#211221 = FACE_OUTER_BOUND ( 'NONE', #59649, .T. ) ;
#211222 = EDGE_CURVE ( 'NONE', #96638, #247235, #64954, .T. ) ;
#211223 = VECTOR ( 'NONE', #69039, 1000.000000000000000 ) ;
#211224 = ADVANCED_FACE ( 'NONE', ( #8927 ), #128884, .T. ) ;
#211225 = AXIS2_PLACEMENT_3D ( 'NONE', #45160, #242069, #162565 ) ;
#211227 = ORIENTED_EDGE ( 'NONE', *, *, #163647, .F. ) ;
#211226 = LINE ( 'NONE', #32628, #23433 ) ;
#211229 = ORIENTED_EDGE ( 'NONE', *, *, #43894, .T. ) ;
#211228 = VERTEX_POINT ( 'NONE', #207135 ) ;
#211230 = TOROIDAL_SURFACE ( 'NONE', #132125, 0.4000000000000003553, 0.1000000000000000056 ) ;
#211231 = ORIENTED_EDGE ( 'NONE', *, *, #33807, .F. ) ;
#211232 = CARTESIAN_POINT ( 'NONE',  ( -16.78569801330229438, 60.94316146603833317, -221.0355967009543292 ) ) ;
#211233 = EDGE_CURVE ( 'NONE', #6556, #241989, #88427, .T. ) ;
#211234 = DIRECTION ( 'NONE',  ( 0.000000000000000000, 1.000000000000000000, 0.000000000000000000 ) ) ;
#211235 = EDGE_CURVE ( 'NONE', #152832, #42819, #169056, .T. ) ;
#211237 = FACE_OUTER_BOUND ( 'NONE', #213137, .T. ) ;
#211236 = CYLINDRICAL_SURFACE ( 'NONE', #103653, 7.900000000000003908 ) ;
#211238 = LINE ( 'NONE', #53450, #153920 ) ;
#211239 = ORIENTED_EDGE ( 'NONE', *, *, #66649, .F. ) ;
#211240 = EDGE_CURVE ( 'NONE', #160655, #106067, #56551, .T. ) ;
#211241 = DIRECTION ( 'NONE',  ( -0.000000000000000000, -1.000000000000000000, -0.000000000000000000 ) ) ;
#211242 = VERTEX_POINT ( 'NONE', #169327 ) ;
#211243 = ORIENTED_EDGE ( 'NONE', *, *, #223332, .F. ) ;
#211244 = CARTESIAN_POINT ( 'NONE',  ( -21.05000000000000071, -0.1000000000000007688, 6.540656951701240729 ) ) ;
#211245 = DIRECTION ( 'NONE',  ( -1.000000000000000000, 0.000000000000000000, 0.000000000000000000 ) ) ;
#211246 = LINE ( 'NONE', #112169, #8357 ) ;
#211247 = VERTEX_POINT ( 'NONE', #27241 ) ;
#211248 = CIRCLE ( 'NONE', #153023, 11.74999999999999645 ) ;
#211249 = DIRECTION ( 'NONE',  ( 0.000000000000000000, -0.000000000000000000, 1.000000000000000000 ) ) ;
#211250 = ADVANCED_FACE ( 'NONE', ( #168041 ), #206434, .T. ) ;
#211251 = VERTEX_POINT ( 'NONE', #7647 ) ;
#211252 = ORIENTED_EDGE ( 'NONE', *, *, #166745, .F. ) ;
#211253 = DIRECTION ( 'NONE',  ( 0.000000000000000000, 0.000000000000000000, -1.000000000000000000 ) ) ;
#211254 = DIRECTION ( 'NONE',  ( 0.000000000000000000, 0.1568667991644863147, -0.9876197685951252359 ) ) ;
#211255 = EDGE_CURVE ( 'NONE', #146084, #100999, #147142, .T. ) ;
#211256 = DIRECTION ( 'NONE',  ( 0.000000000000000000, 0.8814952561688476074, -0.4721928772777262417 ) ) ;
#211257 = ADVANCED_FACE ( 'NONE', ( #130143 ), #244019, .T. ) ;
#211258 = FACE_OUTER_BOUND ( 'NONE', #106477, .T. ) ;
#211259 = DIRECTION ( 'NONE',  ( -1.000000000000000000, -0.000000000000000000, -0.000000000000000000 ) ) ;
#211260 = EDGE_CURVE ( 'NONE', #15770, #246137, #6340, .T. ) ;
#211261 = AXIS2_PLACEMENT_3D ( 'NONE', #133690, #72454, #249791 ) ;
#211262 = CARTESIAN_POINT ( 'NONE',  ( -20.15000000000000568, 11.70669885886984751, -211.0899064736586013 ) ) ;
#211263 = ORIENTED_EDGE ( 'NONE', *, *, #150912, .F. ) ;
#211264 = CARTESIAN_POINT ( 'NONE',  ( -21.05000000000000071, -0.09999999998884338825, -155.8504291924551808 ) ) ;
#211265 = CARTESIAN_POINT ( 'NONE',  ( 18.49999999999999645, 77.13501884592203339, -95.30613060109196510 ) ) ;
#211267 = DIRECTION ( 'NONE',  ( 0.000000000000000000, -0.9856811345164800953, -0.1686199900910462790 ) ) ;
#211266 = CARTESIAN_POINT ( 'NONE',  ( -18.39999999999999858, 85.68240343348850274, -129.8662641071115047 ) ) ;
#211268 = CARTESIAN_POINT ( 'NONE',  ( 21.56666275994539816, 1.115600667400684642E-11, -26.54263159310668030 ) ) ;
#211269 = AXIS2_PLACEMENT_3D ( 'NONE', #255878, #17333, #35639 ) ;
#211270 = DIRECTION ( 'NONE',  ( 0.000000000000000000, 0.000000000000000000, -1.000000000000000000 ) ) ;
#211271 = CARTESIAN_POINT ( 'NONE',  ( 18.69999999999999929, 0.000000000000000000, 0.000000000000000000 ) ) ;
#211272 = DIRECTION ( 'NONE',  ( 0.000000000000000000, 0.000000000000000000, -1.000000000000000000 ) ) ;
#211273 = VECTOR ( 'NONE', #153723, 1000.000000000000000 ) ;
#211275 = ORIENTED_EDGE ( 'NONE', *, *, #221043, .T. ) ;
#211274 = DIRECTION ( 'NONE',  ( 0.000000000000000000, 1.000000000000000000, 6.688090509790097607E-15 ) ) ;
#211276 = AXIS2_PLACEMENT_3D ( 'NONE', #183320, #125895, #63352 ) ;
#211277 = PRODUCT_DEFINITION_FORMATION_WITH_SPECIFIED_SOURCE ( 'ANY', '', #249281, .NOT_KNOWN. ) ;
#211278 = EDGE_CURVE ( 'NONE', #245692, #51036, #23300, .T. ) ;
#211279 = EDGE_CURVE ( 'NONE', #142411, #28813, #105415, .T. ) ;
#211280 = FACE_OUTER_BOUND ( 'NONE', #32399, .T. ) ;
#211281 = AXIS2_PLACEMENT_3D ( 'NONE', #8576, #167667, #46395 ) ;
#211282 = CARTESIAN_POINT ( 'NONE',  ( 20.94999999999999574, 16.50669723772569952, -240.7258389668962479 ) ) ;
#211283 = EDGE_CURVE ( 'NONE', #125644, #164289, #110748, .T. ) ;
#211284 = CARTESIAN_POINT ( 'NONE',  ( -21.07928932188134041, 6.328516656404449492, -33.40110485434561127 ) ) ;
#211285 = DIRECTION ( 'NONE',  ( -0.7071067811865431318, -0.6824534298469886462, 0.1850873201764167419 ) ) ;
#211286 = FACE_OUTER_BOUND ( 'NONE', #155435, .T. ) ;
#211287 = AXIS2_PLACEMENT_3D ( 'NONE', #153661, #171920, #174509 ) ;
#211288 = DIRECTION ( 'NONE',  ( 0.000000000000000000, 0.000000000000000000, -1.000000000000000000 ) ) ;
#211289 = VECTOR ( 'NONE', #205358, 1000.000000000000000 ) ;
#211290 = DIRECTION ( 'NONE',  ( -0.7071067811865460184, -0.6824534298470606997, 0.1850873201761399356 ) ) ;
#211291 = DIRECTION ( 'NONE',  ( 1.000000000000000000, 0.000000000000000000, 0.000000000000000000 ) ) ;
#211292 = AXIS2_PLACEMENT_3D ( 'NONE', #134205, #71701, #112113 ) ;
#211293 = VERTEX_POINT ( 'NONE', #246256 ) ;
#211294 = DIRECTION ( 'NONE',  ( 1.000000000000000000, 0.000000000000000000, 0.000000000000000000 ) ) ;
#211296 = EDGE_LOOP ( 'NONE', ( #45018, #69094, #161053 ) ) ;
#211295 = AXIS2_PLACEMENT_3D ( 'NONE', #237396, #180000, #222949 ) ;
#211297 = CARTESIAN_POINT ( 'NONE',  ( 20.94999999999999574, 1.250000000011155299, -41.40000000000000568 ) ) ;
#211298 = CIRCLE ( 'NONE', #157151, 14.30833333333333890 ) ;
#211299 = FACE_OUTER_BOUND ( 'NONE', #246060, .T. ) ;
#211300 = VERTEX_POINT ( 'NONE', #67607 ) ;
#211301 = CARTESIAN_POINT ( 'NONE',  ( -21.05000000000000071, 11.62071067811865177, -6.868416652341032602 ) ) ;
#211302 = ADVANCED_FACE ( 'NONE', ( #152316 ), #34942, .T. ) ;
#211303 = SHAPE_DEFINITION_REPRESENTATION ( #88892, #196772 ) ;
#211304 = CARTESIAN_POINT ( 'NONE',  ( -21.14999999999999858, 64.35000000001268461, -203.4231074845244507 ) ) ;
#211305 = FACE_OUTER_BOUND ( 'NONE', #197357, .T. ) ;
#211306 = VERTEX_POINT ( 'NONE', #97406 ) ;
#211308 = EDGE_CURVE ( 'NONE', #230747, #215461, #113158, .T. ) ;
#211307 = CARTESIAN_POINT ( 'NONE',  ( 21.05000000000000071, -0.09999999998884338825, -55.35042919245524473 ) ) ;
#211309 = DIRECTION ( 'NONE',  ( 0.000000000000000000, -1.000000000000000000, 0.000000000000000000 ) ) ;
#211310 = AXIS2_PLACEMENT_3D ( 'NONE', #213784, #233379, #55969 ) ;
#211311 = CONICAL_SURFACE ( 'NONE', #19788, 6.250000000000005329, 0.7853981633974431720 ) ;
#211312 = AXIS2_PLACEMENT_3D ( 'NONE', #46728, #126267, #227949 ) ;
#211313 = EDGE_CURVE ( 'NONE', #155989, #24275, #106632, .T. ) ;
#211314 = EDGE_CURVE ( 'NONE', #34828, #153574, #75790, .T. ) ;
#211315 = CARTESIAN_POINT ( 'NONE',  ( 21.05000000000000071, 76.00000000001260503, -191.3731074845243540 ) ) ;
#211316 = ORIENTED_EDGE ( 'NONE', *, *, #116250, .T. ) ;
#211317 = ORIENTED_EDGE ( 'NONE', *, *, #3230, .F. ) ;
#211318 = ADVANCED_FACE ( 'NONE', ( #57002 ), #93994, .T. ) ;
#211319 = CARTESIAN_POINT ( 'NONE',  ( 20.94999999999999929, 69.45000000001158469, -59.50608031408435039 ) ) ;
#211320 = CARTESIAN_POINT ( 'NONE',  ( 18.47688499308724985, 85.46485595029596993, -96.32175973138681968 ) ) ;
#211322 = TOROIDAL_SURFACE ( 'NONE', #69685, 11.65000000000000036, 0.1000000000000000056 ) ;
#211321 = FACE_OUTER_BOUND ( 'NONE', #130085, .T. ) ;
#211323 = DIRECTION ( 'NONE',  ( -0.4999999999999799050, 0.000000000000000000, -0.8660254037844502539 ) ) ;
#211324 = TOROIDAL_SURFACE ( 'NONE', #132206, 7.800000000000000711, 0.1000000000000000056 ) ;
#211326 = DIRECTION ( 'NONE',  ( 0.000000000000000000, -0.8814952561688476074, 0.4721928772777262417 ) ) ;
#211325 = FACE_OUTER_BOUND ( 'NONE', #112997, .T. ) ;
#211327 = CYLINDRICAL_SURFACE ( 'NONE', #23490, 0.09999999999999520384 ) ;
#211328 = DIRECTION ( 'NONE',  ( 0.000000000000000000, 0.000000000000000000, -1.000000000000000000 ) ) ;
#211329 = DIRECTION ( 'NONE',  ( 0.000000000000000000, 0.000000000000000000, -1.000000000000000000 ) ) ;
#211330 = EDGE_LOOP ( 'NONE', ( #209433, #116969, #220566, #103417 ) ) ;
#211331 = EDGE_CURVE ( 'NONE', #7658, #102511, #122448, .T. ) ;
#211333 = ORIENTED_EDGE ( 'NONE', *, *, #91830, .F. ) ;
#211332 = CARTESIAN_POINT ( 'NONE',  ( -16.87331047859651179, 12.41403342719998726, -211.2428889513006993 ) ) ;
#211334 = FACE_OUTER_BOUND ( 'NONE', #128014, .T. ) ;
#211335 = EDGE_CURVE ( 'NONE', #239535, #17340, #114444, .T. ) ;
#211336 = CARTESIAN_POINT ( 'NONE',  ( 21.05000000000000071, 76.00000000001237765, -170.0231074845243597 ) ) ;
#211337 = FACE_OUTER_BOUND ( 'NONE', #129345, .T. ) ;
#211338 = AXIS2_PLACEMENT_3D ( 'NONE', #186840, #26478, #63012 ) ;
#211339 = ORIENTED_EDGE ( 'NONE', *, *, #171635, .T. ) ;
#211340 = DIRECTION ( 'NONE',  ( 1.000000000000000000, 0.000000000000000000, 0.000000000000000000 ) ) ;
#211342 = EDGE_CURVE ( 'NONE', #225002, #190519, #191452, .T. ) ;
#211341 = CARTESIAN_POINT ( 'NONE',  ( -16.87036670365549895, 66.01058118071041747, -124.0026676018264169 ) ) ;
#211343 = CARTESIAN_POINT ( 'NONE',  ( 22.49806830649814060, 11.64988965485023620, -133.9225356836745107 ) ) ;
#211344 = FACE_OUTER_BOUND ( 'NONE', #121014, .T. ) ;
#211345 = ORIENTED_EDGE ( 'NONE', *, *, #84650, .T. ) ;
#211346 = CIRCLE ( 'NONE', #202949, 7.791421356237310469 ) ;
#211347 = ORIENTED_EDGE ( 'NONE', *, *, #57878, .F. ) ;
#211348 = AXIS2_PLACEMENT_3D ( 'NONE', #214048, #152825, #172401 ) ;
#211349 = AXIS2_PLACEMENT_3D ( 'NONE', #254211, #198105, #116021 ) ;
#211350 = AXIS2_PLACEMENT_3D ( 'NONE', #178242, #257685, #79087 ) ;
#211351 = DIRECTION ( 'NONE',  ( 1.000000000000000000, 0.000000000000000000, 0.000000000000000000 ) ) ;
#211352 = CIRCLE ( 'NONE', #82312, 0.1000000000000028644 ) ;
#211353 = EDGE_LOOP ( 'NONE', ( #21975, #4670, #150261, #63965, #37739 ) ) ;
#211354 = DIRECTION ( 'NONE',  ( 1.000000000000000000, 0.000000000000000000, 0.000000000000000000 ) ) ;
#211355 = EDGE_CURVE ( 'NONE', #16105, #184497, #76591, .T. ) ;
#211356 = AXIS2_PLACEMENT_3D ( 'NONE', #85744, #87039, #207020 ) ;
#211357 = B_SPLINE_CURVE_WITH_KNOTS ( 'NONE', 3,
 ( #113907, #229999, #153081, #171364, #231306, #250833, #69664, #72231, #151777, #52638 ),
 .UNSPECIFIED., .F., .F.,
 ( 4, 3, 3, 4 ),
 ( 1.960480067105092529E-15, 8.145022132831457041E-06, 1.905645951092260382E-05, 2.061107371225662837E-05 ),
 .UNSPECIFIED. ) ;
#211358 = SPHERICAL_SURFACE ( 'NONE', #85346, 0.1000000000000000056 ) ;
#211359 = CARTESIAN_POINT ( 'NONE',  ( -18.50000000000000000, 85.50000000001175238, -81.27310748452426026 ) ) ;
#211360 = EDGE_CURVE ( 'NONE', #86653, #123093, #85771, .T. ) ;
#211361 = FACE_OUTER_BOUND ( 'NONE', #3802, .T. ) ;
#211362 = ORIENTED_EDGE ( 'NONE', *, *, #194540, .F. ) ;
#211363 = LINE ( 'NONE', #112272, #209505 ) ;
#211364 = EDGE_CURVE ( 'NONE', #131148, #153971, #212278, .T. ) ;
#211365 = LINE ( 'NONE', #229639, #16358 ) ;
#211366 = ADVANCED_FACE ( 'NONE', ( #93595 ), #173170, .F. ) ;
#211367 = DIRECTION ( 'NONE',  ( 0.000000000000000000, 0.008583690987124100932, -0.9999631594459055250 ) ) ;
#211368 = AXIS2_PLACEMENT_3D ( 'NONE', #166173, #145271, #223520 ) ;
#211369 = CARTESIAN_POINT ( 'NONE',  ( -21.05000000000000071, 66.10573665986746050, -240.0052065600425237 ) ) ;
#211370 = CARTESIAN_POINT ( 'NONE',  ( 20.94999999999999929, 11.46684968301824625, -245.9610388612851750 ) ) ;
#211371 = DIRECTION ( 'NONE',  ( 0.000000000000000000, 0.8660254037844383745, -0.5000000000000003331 ) ) ;
#211372 = DIRECTION ( 'NONE',  ( 0.000000000000000000, 0.2128009952263603677, -0.9770955615653313941 ) ) ;
#211373 = ORIENTED_EDGE ( 'NONE', *, *, #73082, .T. ) ;
#211374 = CARTESIAN_POINT ( 'NONE',  ( 20.94999999999999574, 74.15091558138485084, -91.36709696307720208 ) ) ;
#211375 = ORIENTED_EDGE ( 'NONE', *, *, #186209, .F. ) ;
#211377 = ORIENTED_EDGE ( 'NONE', *, *, #221529, .F. ) ;
#211376 = CARTESIAN_POINT ( 'NONE',  ( -18.39999999999999858, -9.499999999988849808, -141.0320693966996828 ) ) ;
#211378 = VECTOR ( 'NONE', #142406, 1000.000000000000000 ) ;
#211379 = ORIENTED_EDGE ( 'NONE', *, *, #12080, .F. ) ;
#211380 = DIRECTION ( 'NONE',  ( 0.000000000000000000, 0.000000000000000000, -1.000000000000000000 ) ) ;
#211381 = FACE_OUTER_BOUND ( 'NONE', #17729, .T. ) ;
#211382 = DIRECTION ( 'NONE',  ( 0.000000000000000000, 0.000000000000000000, -1.000000000000000000 ) ) ;
#211383 = DIRECTION ( 'NONE',  ( 1.000000000000000000, 0.000000000000000000, 0.000000000000000000 ) ) ;
#211384 = ORIENTED_EDGE ( 'NONE', *, *, #161602, .T. ) ;
#211385 = EDGE_CURVE ( 'NONE', #172291, #43551, #117010, .T. ) ;
#211386 = CARTESIAN_POINT ( 'NONE',  ( -18.50000000000000000, -9.399999999988850163, -174.4146583429696875 ) ) ;
#211387 = DIRECTION ( 'NONE',  ( 0.000000000000000000, 0.000000000000000000, 1.000000000000000000 ) ) ;
#211388 = ORIENTED_EDGE ( 'NONE', *, *, #112335, .F. ) ;
#211389 = CARTESIAN_POINT ( 'NONE',  ( -20.94999999999999929, 11.64999999999999680, -26.71613433702190576 ) ) ;
#211390 = DIRECTION ( 'NONE',  ( 1.000000000000000000, 3.190570557967288949E-16, 6.948722487160392945E-17 ) ) ;
#211391 = AXIS2_PLACEMENT_3D ( 'NONE', #57681, #33053, #95537 ) ;
#211392 = ORIENTED_EDGE ( 'NONE', *, *, #36718, .F. ) ;
#211393 = DIRECTION ( 'NONE',  ( 0.000000000000000000, 0.8814952561688430555, -0.4721928772777346239 ) ) ;
#211394 = ORIENTED_EDGE ( 'NONE', *, *, #54389, .T. ) ;
#211395 = CARTESIAN_POINT ( 'NONE',  ( 18.50000000000000000, -9.399999999988843058, -141.2972597596633193 ) ) ;
#211396 = ORIENTED_EDGE ( 'NONE', *, *, #151209, .T. ) ;
#211397 = CARTESIAN_POINT ( 'NONE',  ( 20.09999999999999787, 9.750000000011137757, -188.3499999999999659 ) ) ;
#211398 = EDGE_CURVE ( 'NONE', #96922, #174796, #89891, .T. ) ;
#211399 = CYLINDRICAL_SURFACE ( 'NONE', #239802, 0.5000000000000008882 ) ;
#211400 = CARTESIAN_POINT ( 'NONE',  ( 20.85000000000000142, -1.835859311432481045, -179.0044391687985410 ) ) ;
#211401 = CARTESIAN_POINT ( 'NONE',  ( 18.59999999999999787, 77.83534155023627932, -91.46795619196132066 ) ) ;
#211402 = AXIS2_PLACEMENT_3D ( 'NONE', #176674, #22741, #159668 ) ;
#211404 = AXIS2_PLACEMENT_3D ( 'NONE', #148483, #182488, #28587 ) ;
#211403 = DIRECTION ( 'NONE',  ( -1.000000000000000000, 1.836970198721029934E-16, 1.601412966608202925E-30 ) ) ;
#211405 = FACE_OUTER_BOUND ( 'NONE', #219773, .T. ) ;
#211407 = EDGE_CURVE ( 'NONE', #49823, #138780, #98238, .T. ) ;
#211406 = CARTESIAN_POINT ( 'NONE',  ( -20.54999999999999716, -8.999999999988844479, -157.6060308773475924 ) ) ;
#211408 = ORIENTED_EDGE ( 'NONE', *, *, #248042, .T. ) ;
#211409 = CARTESIAN_POINT ( 'NONE',  ( 20.84999999999999432, 7.021664781911246322, -171.3335654018973173 ) ) ;
#211410 = ORIENTED_EDGE ( 'NONE', *, *, #202196, .F. ) ;
#211413 = VERTEX_POINT ( 'NONE', #219957 ) ;
#211412 = CARTESIAN_POINT ( 'NONE',  ( 20.12500000000000000, 66.25000000001257661, -182.3731074845244393 ) ) ;
#211411 = DIRECTION ( 'NONE',  ( -0.000000000000000000, -0.01283462868040327436, 0.9999176327611370985 ) ) ;
#211414 = ORIENTED_EDGE ( 'NONE', *, *, #221640, .F. ) ;
#211415 = CIRCLE ( 'NONE', #48900, 0.1999999999999987899 ) ;
#211416 = CARTESIAN_POINT ( 'NONE',  ( -18.59999999999999787, -11.65000000000000036, 6.100000000000002309 ) ) ;
#211417 = CARTESIAN_POINT ( 'NONE',  ( 21.15000000000005187, 79.88763423575340994, -7.282924647898262549 ) ) ;
#211418 = LINE ( 'NONE', #47176, #194318 ) ;
#211419 = CARTESIAN_POINT ( 'NONE',  ( 20.95496329884391784, 59.01487433854230602, -225.7788383491038360 ) ) ;
#211420 = ORIENTED_EDGE ( 'NONE', *, *, #128190, .F. ) ;
#211422 = ORIENTED_EDGE ( 'NONE', *, *, #56454, .T. ) ;
#211421 = CARTESIAN_POINT ( 'NONE',  ( 20.94999999999999929, 6.550000000011156231, -45.74999999999999289 ) ) ;
#211424 = CARTESIAN_POINT ( 'NONE',  ( -16.86445178670597045, 66.03778837089667775, -190.9138849226415005 ) ) ;
#211423 = DIRECTION ( 'NONE',  ( 1.000000000000000000, -0.000000000000000000, 0.000000000000000000 ) ) ;
#211426 = VERTEX_POINT ( 'NONE', #62178 ) ;
#211425 = CARTESIAN_POINT ( 'NONE',  ( -16.88328101497759448, 9.950352834230013599, -154.8511795149292993 ) ) ;
#211427 = ORIENTED_EDGE ( 'NONE', *, *, #3190, .T. ) ;
#211428 = AXIS2_PLACEMENT_3D ( 'NONE', #168306, #247790, #69186 ) ;
#211429 = AXIS2_PLACEMENT_3D ( 'NONE', #235198, #116538, #197336 ) ;
#211430 = FACE_OUTER_BOUND ( 'NONE', #240013, .T. ) ;
#211431 = DIRECTION ( 'NONE',  ( 0.000000000000000000, 0.000000000000000000, 1.000000000000000000 ) ) ;
#211432 = ORIENTED_EDGE ( 'NONE', *, *, #103701, .T. ) ;
#211433 = DIRECTION ( 'NONE',  ( 0.000000000000000000, 0.8814952561688430555, -0.4721928772777346239 ) ) ;
#211434 = VERTEX_POINT ( 'NONE', #80405 ) ;
#211435 = CARTESIAN_POINT ( 'NONE',  ( -18.50000000000000000, -9.399999999988850163, -107.3820418481727046 ) ) ;
#211436 = CARTESIAN_POINT ( 'NONE',  ( -20.64999999999999858, 7.250000000011155521, -121.6500000000000341 ) ) ;
#211437 = VECTOR ( 'NONE', #243058, 1000.000000000000000 ) ;
#211438 = ORIENTED_EDGE ( 'NONE', *, *, #164619, .T. ) ;
#211439 = DIRECTION ( 'NONE',  ( -1.000000000000000000, -0.000000000000000000, -0.000000000000000000 ) ) ;
#211440 = EDGE_CURVE ( 'NONE', #59289, #1366, #150631, .T. ) ;
#211441 = AXIS2_PLACEMENT_3D ( 'NONE', #164241, #105497, #83372 ) ;
#211442 = CIRCLE ( 'NONE', #98986, 0.1000000000000028644 ) ;
#211443 = TOROIDAL_SURFACE ( 'NONE', #78162, 12.97499999999999787, 0.1000000000000000056 ) ;
#211444 = CARTESIAN_POINT ( 'NONE',  ( 23.14999999999999858, 87.75000000001276135, -215.2731074845242745 ) ) ;
#211445 = AXIS2_PLACEMENT_3D ( 'NONE', #148189, #150764, #51624 ) ;
#211446 = VERTEX_POINT ( 'NONE', #222498 ) ;
#211447 = EDGE_LOOP ( 'NONE', ( #19420, #51876, #39472, #146741 ) ) ;
#211449 = CARTESIAN_POINT ( 'NONE',  ( -18.40000000000000213, -9.499999999988851584, -73.60018939122203108 ) ) ;
#211448 = AXIS2_PLACEMENT_3D ( 'NONE', #79994, #201247, #43472 ) ;
#211450 = VERTEX_POINT ( 'NONE', #182124 ) ;
#211451 = EDGE_CURVE ( 'NONE', #177874, #86629, #239530, .T. ) ;
#211452 = CARTESIAN_POINT ( 'NONE',  ( 18.59999999999999076, 1.835341550235567887, -145.6551512925629766 ) ) ;
#211453 = AXIS2_PLACEMENT_3D ( 'NONE', #172826, #35854, #252295 ) ;
#211454 = ORIENTED_EDGE ( 'NONE', *, *, #117572, .F. ) ;
#211456 = EDGE_LOOP ( 'NONE', ( #168171, #216640, #120899, #11966 ) ) ;
#211455 = DIRECTION ( 'NONE',  ( 0.000000000000000000, -0.4930308989874653269, -0.8700118002898649117 ) ) ;
#211457 = EDGE_CURVE ( 'NONE', #226150, #31765, #177431, .T. ) ;
#211458 = ORIENTED_EDGE ( 'NONE', *, *, #172631, .T. ) ;
#211459 = DIRECTION ( 'NONE',  ( 0.9880948137434723000, 0.1503223940869687913, 0.03273861465020814349 ) ) ;
#211460 = ORIENTED_EDGE ( 'NONE', *, *, #185689, .T. ) ;
#211463 = EDGE_LOOP ( 'NONE', ( #74236, #144246, #108361, #177681 ) ) ;
#211462 = VERTEX_POINT ( 'NONE', #160010 ) ;
#211461 = DIRECTION ( 'NONE',  ( 0.000000000000000000, 1.000000000000000000, 0.000000000000000000 ) ) ;
#211464 = DIRECTION ( 'NONE',  ( 1.000000000000000000, 0.000000000000000000, 0.000000000000000000 ) ) ;
#211467 = EDGE_CURVE ( 'NONE', #43683, #196290, #131597, .T. ) ;
#211466 = ORIENTED_EDGE ( 'NONE', *, *, #157825, .T. ) ;
#211465 = AXIS2_PLACEMENT_3D ( 'NONE', #132132, #219358, #115137 ) ;
#211468 = CIRCLE ( 'NONE', #70022, 0.09999999999998898659 ) ;
#211469 = AXIS2_PLACEMENT_3D ( 'NONE', #182346, #222724, #183623 ) ;
#211470 = CARTESIAN_POINT ( 'NONE',  ( 21.06600267594171783, 8.775166069211060460, -45.70426278237474094 ) ) ;
#211471 = AXIS2_PLACEMENT_3D ( 'NONE', #122971, #44717, #202497 ) ;
#211472 = ORIENTED_EDGE ( 'NONE', *, *, #156023, .F. ) ;
#211473 = TOROIDAL_SURFACE ( 'NONE', #190851, 6.258578643762700899, 0.1000000000000000056 ) ;
#211474 = DIRECTION ( 'NONE',  ( 1.000000000000000000, 0.000000000000000000, 0.000000000000000000 ) ) ;
#211476 = ORIENTED_EDGE ( 'NONE', *, *, #49658, .T. ) ;
#211475 = CARTESIAN_POINT ( 'NONE',  ( 23.14999999999999147, 36.65892442174472876, -249.5511627012454596 ) ) ;
#211477 = DIRECTION ( 'NONE',  ( -0.000000000000000000, -0.9126074666063770380, -0.4088369013363281068 ) ) ;
#211478 = EDGE_LOOP ( 'NONE', ( #190554, #95701, #208373, #81402, #138456, #150206 ) ) ;
#211479 = VECTOR ( 'NONE', #46571, 1000.000000000000000 ) ;
#211480 = ADVANCED_FACE ( 'NONE', ( #38763 ), #4736, .F. ) ;
#211481 = CARTESIAN_POINT ( 'NONE',  ( -20.64999999999999858, 74.00000000001223555, -149.7477294072864709 ) ) ;
#211482 = DIRECTION ( 'NONE',  ( 1.000000000000000000, -0.000000000000000000, 0.000000000000000000 ) ) ;
#211483 = ORIENTED_EDGE ( 'NONE', *, *, #76039, .T. ) ;
#211484 = CARTESIAN_POINT ( 'NONE',  ( 21.14999999999999503, 26.06832281015329755, -254.4051978787608732 ) ) ;
#211485 = DIRECTION ( 'NONE',  ( 1.000000000000000000, 0.000000000000000000, 0.000000000000000000 ) ) ;
#211486 = ADVANCED_FACE ( 'NONE', ( #257743 ), #137836, .T. ) ;
#211487 = ORIENTED_EDGE ( 'NONE', *, *, #122009, .T. ) ;
#211489 = ORIENTED_EDGE ( 'NONE', *, *, #14862, .F. ) ;
#211488 = CARTESIAN_POINT ( 'NONE',  ( -22.40000000000000213, 76.00000000001222134, -148.2735403769829077 ) ) ;
#211490 = SPHERICAL_SURFACE ( 'NONE', #106726, 0.1000000000000000056 ) ;
#211491 = CIRCLE ( 'NONE', #119338, 0.4000000000000114575 ) ;
#211492 = AXIS2_PLACEMENT_3D ( 'NONE', #38742, #197795, #19163 ) ;
#211494 = ORIENTED_EDGE ( 'NONE', *, *, #125657, .T. ) ;
#211493 = EDGE_LOOP ( 'NONE', ( #6771, #33931, #137776, #170017 ) ) ;
#211495 = EDGE_LOOP ( 'NONE', ( #9431, #221112, #63449, #39272 ) ) ;
#211496 = DIRECTION ( 'NONE',  ( 1.000000000000000000, 0.000000000000000000, 0.000000000000000000 ) ) ;
#211497 = VERTEX_POINT ( 'NONE', #21773 ) ;
#211498 = EDGE_LOOP ( 'NONE', ( #189103, #143072 ) ) ;
#211499 = CARTESIAN_POINT ( 'NONE',  ( -18.40000000000000568, 30.89789434349017938, -233.5160218091985200 ) ) ;
#211500 = ORIENTED_EDGE ( 'NONE', *, *, #239391, .F. ) ;
#211501 = FACE_OUTER_BOUND ( 'NONE', #207276, .T. ) ;
#211502 = CARTESIAN_POINT ( 'NONE',  ( -18.59999999999999787, -1.164121893230052995, -74.91484808557160591 ) ) ;
#211503 = ADVANCED_FACE ( 'NONE', ( #119597 ), #44124, .F. ) ;
#211504 = ORIENTED_EDGE ( 'NONE', *, *, #257033, .F. ) ;
#211505 = AXIS2_PLACEMENT_3D ( 'NONE', #49274, #204486, #246200 ) ;
#211506 = CIRCLE ( 'NONE', #32476, 12.87499999999999822 ) ;
#211507 = ORIENTED_EDGE ( 'NONE', *, *, #147958, .T. ) ;
#211508 = FACE_OUTER_BOUND ( 'NONE', #256107, .T. ) ;
#211509 = AXIS2_PLACEMENT_3D ( 'NONE', #14751, #52547, #172565 ) ;
#211510 = VERTEX_POINT ( 'NONE', #3465 ) ;
#211511 = AXIS2_PLACEMENT_3D ( 'NONE', #181409, #241373, #142252 ) ;
#211512 = EDGE_CURVE ( 'NONE', #42862, #247233, #240812, .T. ) ;
#211513 = CYLINDRICAL_SURFACE ( 'NONE', #54996, 0.1999999999999987899 ) ;
#211514 = ORIENTED_EDGE ( 'NONE', *, *, #18240, .T. ) ;
#211515 = ORIENTED_EDGE ( 'NONE', *, *, #73638, .F. ) ;
#211516 = CARTESIAN_POINT ( 'NONE',  ( 20.95512820512820440, 8.876151316299271343, -121.7500000000000426 ) ) ;
#211518 = ORIENTED_EDGE ( 'NONE', *, *, #174221, .T. ) ;
#211517 = CARTESIAN_POINT ( 'NONE',  ( 18.59999999999999787, 85.32100840337362513, -162.7871692354464130 ) ) ;
#211519 = CARTESIAN_POINT ( 'NONE',  ( 21.05000000000000071, 36.65892442174472876, -249.5511627012454596 ) ) ;
#211520 = CARTESIAN_POINT ( 'NONE',  ( -21.14999999999999858, 36.65892442174472876, -249.5511627012454596 ) ) ;
#211521 = CIRCLE ( 'NONE', #99063, 0.1000000000000028644 ) ;
#211522 = LINE ( 'NONE', #12057, #197803 ) ;
#211524 = EDGE_CURVE ( 'NONE', #164969, #48358, #242079, .T. ) ;
#211523 = CARTESIAN_POINT ( 'NONE',  ( 20.94999999999999574, 68.09270462032664284, -227.9033695786537805 ) ) ;
#211525 = PLANE ( 'NONE',  #236063 ) ;
#211526 = DIRECTION ( 'NONE',  ( 0.000000000000000000, 0.000000000000000000, -1.000000000000000000 ) ) ;
#211527 = SPHERICAL_SURFACE ( 'NONE', #191395, 0.1000000000000000056 ) ;
#211529 = CIRCLE ( 'NONE', #219889, 0.1000000000000028644 ) ;
#211528 = CARTESIAN_POINT ( 'NONE',  ( 22.42357213249528769, 10.66459267205035388, -226.9222596543260977 ) ) ;
#211530 = AXIS2_PLACEMENT_3D ( 'NONE', #152937, #69532, #232462 ) ;
#211531 = CARTESIAN_POINT ( 'NONE',  ( 18.44208962362734638, 38.17972036805543468, -261.2023309164682701 ) ) ;
#211533 = CARTESIAN_POINT ( 'NONE',  ( 18.49999999999999289, 33.90972941529384599, -236.3646070729083988 ) ) ;
#211532 = TOROIDAL_SURFACE ( 'NONE', #70079, 0.2000000000000000111, 0.1000000000000000056 ) ;
#211534 = EDGE_CURVE ( 'NONE', #77128, #129272, #217370, .T. ) ;
#211536 = ORIENTED_EDGE ( 'NONE', *, *, #164843, .F. ) ;
#211535 = AXIS2_PLACEMENT_3D ( 'NONE', #187471, #167922, #68799 ) ;
#211537 = ADVANCED_FACE ( 'NONE', ( #20495 ), #123429, .T. ) ;
#211539 = ORIENTED_EDGE ( 'NONE', *, *, #155095, .F. ) ;
#211538 = ORIENTED_EDGE ( 'NONE', *, *, #160251, .T. ) ;
#211540 = ORIENTED_EDGE ( 'NONE', *, *, #242309, .T. ) ;
#211541 = DIRECTION ( 'NONE',  ( -1.000000000000000000, 0.000000000000000000, 0.000000000000000000 ) ) ;
#211542 = ADVANCED_FACE ( 'NONE', ( #124717 ), #187272, .F. ) ;
#211543 = CARTESIAN_POINT ( 'NONE',  ( -18.50000000000000000, 85.50000000001233502, -161.9231074845242802 ) ) ;
#211545 = FACE_OUTER_BOUND ( 'NONE', #170142, .T. ) ;
#211544 = DIRECTION ( 'NONE',  ( -1.073024830501117725E-15, -0.000000000000000000, -1.000000000000000000 ) ) ;
#211546 = ORIENTED_EDGE ( 'NONE', *, *, #215668, .F. ) ;
#211547 = ORIENTED_EDGE ( 'NONE', *, *, #101395, .F. ) ;
#211548 = CIRCLE ( 'NONE', #128350, 0.6000000000000064171 ) ;
#211549 = EDGE_CURVE ( 'NONE', #239741, #67400, #209378, .T. ) ;
#211550 = EDGE_CURVE ( 'NONE', #70455, #253683, #69081, .T. ) ;
#211551 = CARTESIAN_POINT ( 'NONE',  ( 18.41789779300685481, -9.499999999988844479, -40.53206966636064124 ) ) ;
#211552 = CARTESIAN_POINT ( 'NONE',  ( -21.05000000000000071, 18.26942912180536638, -237.6183358664095238 ) ) ;
#211553 = DIRECTION ( 'NONE',  ( 1.000000000000000000, 0.000000000000000000, 0.000000000000000000 ) ) ;
#211554 = VERTEX_POINT ( 'NONE', #86842 ) ;
#211555 = ORIENTED_EDGE ( 'NONE', *, *, #134450, .T. ) ;
#211556 = AXIS2_PLACEMENT_3D ( 'NONE', #190226, #51966, #154969 ) ;
#211557 = FACE_OUTER_BOUND ( 'NONE', #194217, .T. ) ;
#211558 = DIRECTION ( 'NONE',  ( 0.000000000000000000, 1.000000000000000000, 0.000000000000000000 ) ) ;
#211559 = EDGE_CURVE ( 'NONE', #10849, #217568, #227274, .T. ) ;
#211560 = CARTESIAN_POINT ( 'NONE',  ( -20.54999999999999716, 85.00000000001251976, -179.9170766071767389 ) ) ;
#211562 = ORIENTED_EDGE ( 'NONE', *, *, #14391, .F. ) ;
#211561 = CARTESIAN_POINT ( 'NONE',  ( -21.05000000000000071, -1.835341550213255957, -45.05515129256298223 ) ) ;
#211563 = DIRECTION ( 'NONE',  ( 0.000000000000000000, -1.000000000000000000, -6.982962677686265922E-15 ) ) ;
#211564 = DIRECTION ( 'NONE',  ( -0.000000000000000000, 1.000000000000000000, 6.982962677686266711E-15 ) ) ;
#211565 = EDGE_CURVE ( 'NONE', #185463, #247867, #40057, .T. ) ;
#211566 = CARTESIAN_POINT ( 'NONE',  ( -23.39999999999994529, 77.16254490893143725, -44.02310748452479316 ) ) ;
#211567 = DIRECTION ( 'NONE',  ( 1.000000000000000000, 0.000000000000000000, 0.000000000000000000 ) ) ;
#211568 = ORIENTED_EDGE ( 'NONE', *, *, #103401, .F. ) ;
#211569 = CARTESIAN_POINT ( 'NONE',  ( -12.25000000000000178, 47.91805600923872532, -233.7139610577891631 ) ) ;
#211570 = DIRECTION ( 'NONE',  ( 0.000000000000000000, 0.000000000000000000, 1.000000000000000000 ) ) ;
#211571 = DIRECTION ( 'NONE',  ( 1.296989514748957922E-15, 0.9887567792719351711, -0.1495327102803594987 ) ) ;
#211573 = DIRECTION ( 'NONE',  ( 1.000000000000000000, 0.000000000000000000, 0.000000000000000000 ) ) ;
#211572 = CARTESIAN_POINT ( 'NONE',  ( -16.83794237512073266, 66.07364077890456144, -123.7195653258253998 ) ) ;
#211574 = DIRECTION ( 'NONE',  ( 0.000000000000000000, 0.000000000000000000, -1.000000000000000000 ) ) ;
#211575 = CARTESIAN_POINT ( 'NONE',  ( -16.77180007708460607, 9.950000000011137047, -54.36438588104517322 ) ) ;
#211576 = CARTESIAN_POINT ( 'NONE',  ( -23.39999999999994529, 74.94272479589878344, -3.023107484524792277 ) ) ;
#211577 = TOROIDAL_SURFACE ( 'NONE', #244873, 12.97499999999999609, 0.1000000000000000056 ) ;
#211578 = AXIS2_PLACEMENT_3D ( 'NONE', #8590, #133664, #170276 ) ;
#211579 = DIRECTION ( 'NONE',  ( 0.000000000000000000, 0.000000000000000000, -1.000000000000000000 ) ) ;
#211580 = LINE ( 'NONE', #112486, #130899 ) ;
#211581 = CIRCLE ( 'NONE', #132269, 3.900000000000000799 ) ;
#211582 = ORIENTED_EDGE ( 'NONE', *, *, #80333, .F. ) ;
#211583 = ORIENTED_EDGE ( 'NONE', *, *, #174044, .F. ) ;
#211584 = ORIENTED_EDGE ( 'NONE', *, *, #201559, .T. ) ;
#211585 = CARTESIAN_POINT ( 'NONE',  ( -21.52071067811865746, 7.779289321892505882, -188.6499999999999488 ) ) ;
#211586 = FACE_OUTER_BOUND ( 'NONE', #2459, .T. ) ;
#211587 = ADVANCED_FACE ( 'NONE', ( #128564 ), #225069, .F. ) ;
#211588 = EDGE_LOOP ( 'NONE', ( #78826, #4941, #221825, #251750 ) ) ;
#211589 = EDGE_CURVE ( 'NONE', #119534, #25751, #30771, .T. ) ;
#211590 = PLANE ( 'NONE',  #217808 ) ;
#211591 = EDGE_LOOP ( 'NONE', ( #82240, #15169, #224972, #231675 ) ) ;
#211592 = CIRCLE ( 'NONE', #24348, 11.80000000000000426 ) ;
#211593 = EDGE_CURVE ( 'NONE', #151867, #223317, #144234, .T. ) ;
#211594 = VECTOR ( 'NONE', #77284, 1000.000000000000227 ) ;
#211595 = EDGE_LOOP ( 'NONE', ( #188255, #100518, #65712, #55024 ) ) ;
#211596 = CARTESIAN_POINT ( 'NONE',  ( 21.05000000000000071, 75.90156250001166427, -109.3223383946165939 ) ) ;
#211597 = EDGE_LOOP ( 'NONE', ( #41815, #243841, #58485, #13451 ) ) ;
#211598 = VECTOR ( 'NONE', #155105, 1000.000000000000000 ) ;
#211599 = DIRECTION ( 'NONE',  ( 1.000000000000000000, 0.000000000000000000, 0.000000000000000000 ) ) ;
#211600 = CARTESIAN_POINT ( 'NONE',  ( -16.79140778683512281, 30.18607848682776762, -234.8019360275262102 ) ) ;
#211601 = DIRECTION ( 'NONE',  ( 0.000000000000000000, 0.9908441862701782288, -0.1350103645450542456 ) ) ;
#211602 = LINE ( 'NONE', #49942, #112443 ) ;
#211603 = FACE_OUTER_BOUND ( 'NONE', #57523, .T. ) ;
#211605 = ORIENTED_EDGE ( 'NONE', *, *, #149528, .F. ) ;
#211604 = CARTESIAN_POINT ( 'NONE',  ( -16.85722902420145530, 30.10447401013609436, -234.7524843106976107 ) ) ;
#211607 = CARTESIAN_POINT ( 'NONE',  ( 20.85000000000000142, 78.48087866980282001, -232.8271061603568910 ) ) ;
#211606 = CARTESIAN_POINT ( 'NONE',  ( 21.05000000000000071, 6.093673009692417430, -199.5727803633481301 ) ) ;
#211608 = CARTESIAN_POINT ( 'NONE',  ( -16.95709691156346466, 9.949999999999770139, -20.83994243748941599 ) ) ;
#211609 =( BOUNDED_CURVE ( )  B_SPLINE_CURVE ( 3, ( #188192, #30410, #168675, #254543 ),
 .UNSPECIFIED., .F., .F. ) 
 B_SPLINE_CURVE_WITH_KNOTS ( ( 4, 4 ),
 ( 1.570796326794901665, 3.141592653589733608 ),
 .UNSPECIFIED. ) 
 CURVE ( )  GEOMETRIC_REPRESENTATION_ITEM ( )  RATIONAL_B_SPLINE_CURVE ( ( 1.000000000000000000, 0.8047378541243801475, 0.8047378541243801475, 1.000000000000000000 ) ) 
 REPRESENTATION_ITEM ( '' )  );
#211610 = CARTESIAN_POINT ( 'NONE',  ( -18.59999999999999787, 77.16412189325360771, -162.1082593989527254 ) ) ;
#211611 = CARTESIAN_POINT ( 'NONE',  ( -20.94999999999999929, 77.83534155023646406, -124.9679561919612922 ) ) ;
#211612 = DIRECTION ( 'NONE',  ( 0.000000000000000000, 0.1350103645451876666, -0.9908441862701600211 ) ) ;
#211613 = VERTEX_POINT ( 'NONE', #6029 ) ;
#211614 = EDGE_CURVE ( 'NONE', #77719, #163390, #169241, .T. ) ;
#211615 = PRESENTATION_STYLE_ASSIGNMENT (( #132071 ) ) ;
#211616 = LINE ( 'NONE', #252008, #96006 ) ;
#211617 = EDGE_CURVE ( 'NONE', #135298, #166393, #85541, .T. ) ;
#211618 = AXIS2_PLACEMENT_3D ( 'NONE', #253890, #56950, #154830 ) ;
#211619 = DIRECTION ( 'NONE',  ( 1.000000000000000000, 0.000000000000000000, 0.000000000000000000 ) ) ;
#211620 = VERTEX_POINT ( 'NONE', #125985 ) ;
#211621 = AXIS2_PLACEMENT_3D ( 'NONE', #51073, #31586, #250589 ) ;
#211622 = CIRCLE ( 'NONE', #45015, 0.09999999999999939493 ) ;
#211623 = DIRECTION ( 'NONE',  ( 0.000000000000000000, -1.000000000000000000, 0.000000000000000000 ) ) ;
#211624 =( BOUNDED_CURVE ( )  B_SPLINE_CURVE ( 3, ( #81709, #139118, #161307, #240830 ),
 .UNSPECIFIED., .F., .F. ) 
 B_SPLINE_CURVE_WITH_KNOTS ( ( 4, 4 ),
 ( 4.712388980384689674, 5.672655318024773408 ),
 .UNSPECIFIED. ) 
 CURVE ( )  GEOMETRIC_REPRESENTATION_ITEM ( )  RATIONAL_B_SPLINE_CURVE ( ( 1.000000000000000000, 0.9246222802177227473, 0.9246222802177227473, 1.000000000000000000 ) ) 
 REPRESENTATION_ITEM ( '' )  );
#211625 = DIRECTION ( 'NONE',  ( 0.000000000000000000, 0.000000000000000000, -1.000000000000000000 ) ) ;
#211626 = EDGE_CURVE ( 'NONE', #245971, #215605, #69263, .T. ) ;
#211627 = CARTESIAN_POINT ( 'NONE',  ( -21.05000000000000071, 64.35000000001234355, -163.2392418215462726 ) ) ;
#211628 = VERTEX_POINT ( 'NONE', #146822 ) ;
#211629 = CIRCLE ( 'NONE', #16012, 0.1000000000000046685 ) ;
#211630 = EDGE_LOOP ( 'NONE', ( #212708, #20213, #192256, #106581 ) ) ;
#211631 = ADVANCED_FACE ( 'NONE', ( #110270 ), #145544, .T. ) ;
#211632 = CARTESIAN_POINT ( 'NONE',  ( -18.59999999999999787, 77.16412189325258453, -28.30825939895270693 ) ) ;
#211633 = CARTESIAN_POINT ( 'NONE',  ( 20.94999999999999929, 7.128833340094563376, -233.7327013124401276 ) ) ;
#211634 = DIRECTION ( 'NONE',  ( 0.000000000000000000, 0.000000000000000000, 1.000000000000000000 ) ) ;
#211635 = DIRECTION ( 'NONE',  ( -0.000000000000000000, 0.000000000000000000, 1.000000000000000000 ) ) ;
#211636 = EDGE_CURVE ( 'NONE', #26637, #103956, #226350, .T. ) ;
#211638 = CARTESIAN_POINT ( 'NONE',  ( 21.05000000000000071, 69.35000000001207354, -126.5060803140843291 ) ) ;
#211637 = CARTESIAN_POINT ( 'NONE',  ( 21.05000000000000071, 1.115600667400684642E-11, -45.65000000000000568 ) ) ;
#211639 = CIRCLE ( 'NONE', #207549, 14.30833333333334600 ) ;
#211641 = DIRECTION ( 'NONE',  ( -0.000000000000000000, 0.1298341882520054891, 0.9915357197604850459 ) ) ;
#211640 = TOROIDAL_SURFACE ( 'NONE', #16022, 12.97499999999999609, 0.1000000000000000056 ) ;
#211642 = DIRECTION ( 'NONE',  ( 0.000000000000000000, 0.000000000000000000, -1.000000000000000000 ) ) ;
#211643 = DIRECTION ( 'NONE',  ( 1.000000000000000000, 0.000000000000000000, 0.000000000000000000 ) ) ;
#211644 = AXIS2_PLACEMENT_3D ( 'NONE', #187048, #189603, #104868 ) ;
#211645 = VERTEX_POINT ( 'NONE', #247214 ) ;
#211647 =( BOUNDED_CURVE ( )  B_SPLINE_CURVE ( 3, ( #111233, #150373, #190803, #211627 ),
 .UNSPECIFIED., .F., .F. ) 
 B_SPLINE_CURVE_WITH_KNOTS ( ( 4, 4 ),
 ( 3.141592653589793116, 4.712388980384689674 ),
 .UNSPECIFIED. ) 
 CURVE ( )  GEOMETRIC_REPRESENTATION_ITEM ( )  RATIONAL_B_SPLINE_CURVE ( ( 1.000000000000000000, 0.8047378541243649375, 0.8047378541243649375, 1.000000000000000000 ) ) 
 REPRESENTATION_ITEM ( '' )  );
#211646 = DIRECTION ( 'NONE',  ( 0.000000000000000000, 0.8814952561688444987, -0.4721928772777320149 ) ) ;
#211648 = ADVANCED_FACE ( 'NONE', ( #163843 ), #210893, .F. ) ;
#211650 = ORIENTED_EDGE ( 'NONE', *, *, #198917, .F. ) ;
#211649 = CARTESIAN_POINT ( 'NONE',  ( 16.87683809663749557, 9.950000000011131718, -54.35000000000000142 ) ) ;
#211651 = CARTESIAN_POINT ( 'NONE',  ( 23.14999999999999503, 11.65000000001116298, -155.3500000000000227 ) ) ;
#211654 = ADVANCED_FACE ( 'NONE', ( #223794 ), #228952, .T. ) ;
#211653 = EDGE_CURVE ( 'NONE', #205739, #3432, #144248, .T. ) ;
#211652 = CIRCLE ( 'NONE', #99178, 4.049999999999998046 ) ;
#211655 = CYLINDRICAL_SURFACE ( 'NONE', #7486, 0.09999999999998898659 ) ;
#211657 = CARTESIAN_POINT ( 'NONE',  ( -18.59999999999999787, -0.6576273345615599730, -242.5323337003318898 ) ) ;
#211656 = DIRECTION ( 'NONE',  ( 0.000000000000000000, 0.000000000000000000, -1.000000000000000000 ) ) ;
#211658 = CARTESIAN_POINT ( 'NONE',  ( -22.50875500270927887, 76.10085791378664055, -114.7726746119221986 ) ) ;
#211659 = DIRECTION ( 'NONE',  ( 0.000000000000000000, 1.000000000000000000, 2.891205793294679805E-16 ) ) ;
#211661 = ORIENTED_EDGE ( 'NONE', *, *, #180296, .F. ) ;
#211660 = DIRECTION ( 'NONE',  ( -1.000000000000000000, -0.000000000000000000, -0.000000000000000000 ) ) ;
#211662 = CARTESIAN_POINT ( 'NONE',  ( -22.50000000000000000, 76.00000000001237765, -170.0231074845243597 ) ) ;
#211663 = CYLINDRICAL_SURFACE ( 'NONE', #103822, 0.1000000000000028644 ) ;
#211664 = DIRECTION ( 'NONE',  ( 1.000000000000000000, -0.000000000000000000, -0.000000000000000000 ) ) ;
#211665 = DIRECTION ( 'NONE',  ( 0.000000000000000000, -0.8814952561688430555, 0.4721928772777346239 ) ) ;
#211666 = EDGE_LOOP ( 'NONE', ( #162930, #80608, #147941, #22467 ) ) ;
#211667 = CARTESIAN_POINT ( 'NONE',  ( -23.25000000000000000, 69.01799029515544248, -99.32695536626806643 ) ) ;
#211668 = ORIENTED_EDGE ( 'NONE', *, *, #95798, .F. ) ;
#211669 = DIRECTION ( 'NONE',  ( 1.000000000000000000, 0.000000000000000000, 0.000000000000000000 ) ) ;
#211670 = VECTOR ( 'NONE', #36921, 1000.000000000000227 ) ;
#211671 = ORIENTED_EDGE ( 'NONE', *, *, #244008, .F. ) ;
#211672 = DIRECTION ( 'NONE',  ( 1.000000000000000000, 0.000000000000000000, 0.000000000000000000 ) ) ;
#211673 = ADVANCED_FACE ( 'NONE', ( #232820 ), #34619, .T. ) ;
#211675 = EDGE_CURVE ( 'NONE', #131609, #74676, #248305, .T. ) ;
#211674 = VECTOR ( 'NONE', #38017, 1000.000000000000000 ) ;
#211676 = EDGE_LOOP ( 'NONE', ( #194196, #27151, #216887, #236565 ) ) ;
#211677 = CARTESIAN_POINT ( 'NONE',  ( -21.05000000000000071, 87.48912529308798014, -106.0231074845242176 ) ) ;
#211679 = DIRECTION ( 'NONE',  ( 0.000000000000000000, 0.9651348961776677893, -0.2617529984166795387 ) ) ;
#211678 = AXIS2_PLACEMENT_3D ( 'NONE', #212778, #130654, #31596 ) ;
#211680 = CIRCLE ( 'NONE', #199180, 0.09999999999998807065 ) ;
#211681 = AXIS2_PLACEMENT_3D ( 'NONE', #156700, #40611, #254450 ) ;
#211682 = ADVANCED_FACE ( 'NONE', ( #211965 ), #251060, .T. ) ;
#211683 = CARTESIAN_POINT ( 'NONE',  ( -18.69999999999999929, -10.84999999999999076, 32.89999999999999858 ) ) ;
#211684 = ORIENTED_EDGE ( 'NONE', *, *, #254464, .T. ) ;
#211685 = VECTOR ( 'NONE', #36901, 1000.000000000000000 ) ;
#211686 = DIRECTION ( 'NONE',  ( 1.186688945009010077E-16, 0.4088369013363280513, -0.9126074666063769270 ) ) ;
#211687 = EDGE_CURVE ( 'NONE', #187394, #110538, #160846, .T. ) ;
#211688 = CARTESIAN_POINT ( 'NONE',  ( -18.50000000000000000, 1.115600667400684642E-11, -33.50000000000000000 ) ) ;
#211689 = FACE_OUTER_BOUND ( 'NONE', #78161, .T. ) ;
#211690 = CARTESIAN_POINT ( 'NONE',  ( 12.25000000000000000, 9.349999999999983658, -16.74999999999999645 ) ) ;
#211691 = DIRECTION ( 'NONE',  ( 1.000000000000000000, 0.000000000000000000, 0.000000000000000000 ) ) ;
#211692 = EDGE_LOOP ( 'NONE', ( #198399, #53678, #215872 ) ) ;
#211694 = CIRCLE ( 'NONE', #20146, 0.1000000000000132172 ) ;
#211693 = CARTESIAN_POINT ( 'NONE',  ( -18.59999999999999787, 85.48068669529106955, -129.5819923157664562 ) ) ;
#211695 = AXIS2_PLACEMENT_3D ( 'NONE', #245612, #171258, #248178 ) ;
#211696 = ORIENTED_EDGE ( 'NONE', *, *, #180906, .T. ) ;
#211698 = VERTEX_POINT ( 'NONE', #253621 ) ;
#211697 = CARTESIAN_POINT ( 'NONE',  ( -17.04761207306817283, 65.97354912661445780, -149.1731074845244507 ) ) ;
#211699 = ORIENTED_EDGE ( 'NONE', *, *, #36486, .F. ) ;
#211700 = DIRECTION ( 'NONE',  ( 2.940209281316622495E-16, -1.000000000000000000, -2.352167425053297996E-15 ) ) ;
#211701 = CYLINDRICAL_SURFACE ( 'NONE', #167419, 0.1000000000000055844 ) ;
#211702 = CARTESIAN_POINT ( 'NONE',  ( 21.93340585898988948, 1.115541036281197940E-11, -26.17585297787523047 ) ) ;
#211703 = LINE ( 'NONE', #73488, #91672 ) ;
#211704 = ORIENTED_EDGE ( 'NONE', *, *, #221494, .F. ) ;
#211705 = ADVANCED_FACE ( 'NONE', ( #75042 ), #154578, .F. ) ;
#211706 = FACE_OUTER_BOUND ( 'NONE', #126511, .T. ) ;
#211707 = CARTESIAN_POINT ( 'NONE',  ( 18.59999999999999076, 69.55000000001223270, -148.7731074845244166 ) ) ;
#211708 = ORIENTED_EDGE ( 'NONE', *, *, #139476, .F. ) ;
#211709 = VECTOR ( 'NONE', #46381, 1000.000000000000000 ) ;
#211711 = ORIENTED_EDGE ( 'NONE', *, *, #32116, .T. ) ;
#211710 = CARTESIAN_POINT ( 'NONE',  ( -16.92778301347279424, 65.99905508317672798, -115.5945893765551915 ) ) ;
#211712 = LINE ( 'NONE', #34370, #165065 ) ;
#211713 = AXIS2_PLACEMENT_3D ( 'NONE', #245116, #122622, #104296 ) ;
#211714 = DIRECTION ( 'NONE',  ( 1.000000000000000000, -7.304098846218134667E-16, -5.100424963727256530E-30 ) ) ;
#211715 = ADVANCED_FACE ( 'NONE', ( #116695 ), #12488, .T. ) ;
#211716 = AXIS2_PLACEMENT_3D ( 'NONE', #236332, #100637, #255848 ) ;
#211717 = EDGE_LOOP ( 'NONE', ( #131752, #57273, #64160, #22723 ) ) ;
#211718 = ORIENTED_EDGE ( 'NONE', *, *, #100696, .F. ) ;
#211719 = TOROIDAL_SURFACE ( 'NONE', #157572, 7.791421356237335338, 0.1000000000000000056 ) ;
#211720 = DIRECTION ( 'NONE',  ( -1.000000000000000000, 0.000000000000000000, 0.000000000000000000 ) ) ;
#211721 = ORIENTED_EDGE ( 'NONE', *, *, #120212, .F. ) ;
#211722 = CARTESIAN_POINT ( 'NONE',  ( 21.00000000000000000, 9.750000000011153745, -188.7499999999999716 ) ) ;
#211723 = ADVANCED_FACE ( 'NONE', ( #230226 ), #150695, .T. ) ;
#211724 = CARTESIAN_POINT ( 'NONE',  ( -16.27683809663750480, 9.350000000011133849, -121.4500000000000313 ) ) ;
#211725 = AXIS2_PLACEMENT_3D ( 'NONE', #207978, #188388, #108848 ) ;
#211726 = LINE ( 'NONE', #93039, #109347 ) ;
#211727 = AXIS2_PLACEMENT_3D ( 'NONE', #239183, #81357, #181782 ) ;
#211728 = VECTOR ( 'NONE', #232150, 1000.000000000000000 ) ;
#211729 = AXIS2_PLACEMENT_3D ( 'NONE', #163665, #241899, #202781 ) ;
#211730 = CIRCLE ( 'NONE', #190897, 0.2000000000000027867 ) ;
#211731 = ORIENTED_EDGE ( 'NONE', *, *, #69892, .T. ) ;
#211732 = FACE_OUTER_BOUND ( 'NONE', #67277, .T. ) ;
#211733 = VERTEX_POINT ( 'NONE', #35902 ) ;
#211734 = DIRECTION ( 'NONE',  ( -0.000000000000000000, 1.000000000000000000, 0.000000000000000000 ) ) ;
#211735 = LINE ( 'NONE', #134726, #187739 ) ;
#211737 = EDGE_LOOP ( 'NONE', ( #66856, #251831, #129129, #99985 ) ) ;
#211736 = FACE_OUTER_BOUND ( 'NONE', #126537, .T. ) ;
#211738 = FACE_OUTER_BOUND ( 'NONE', #7818, .T. ) ;
#211739 = PLANE ( 'NONE',  #248953 ) ;
#211740 = DIRECTION ( 'NONE',  ( 0.000000000000000000, -6.982962677686266711E-15, 1.000000000000000000 ) ) ;
#211741 = CARTESIAN_POINT ( 'NONE',  ( 18.50000000000000000, -9.399999999988843058, -74.29725975966333351 ) ) ;
#211742 = CARTESIAN_POINT ( 'NONE',  ( -23.25000000000000000, 65.66751761918648356, -63.92826094061123143 ) ) ;
#211743 = AXIS2_PLACEMENT_3D ( 'NONE', #96222, #256527, #240886 ) ;
#211744 = CARTESIAN_POINT ( 'NONE',  ( -18.59999999999999787, 15.92646454033039305, -219.3818586450342707 ) ) ;
#211745 = DIRECTION ( 'NONE',  ( 0.000000000000000000, -1.000000000000000000, -2.891205793294679805E-16 ) ) ;
#211746 = VERTEX_POINT ( 'NONE', #213217 ) ;
#211747 = DIRECTION ( 'NONE',  ( -1.000000000000000000, 0.000000000000000000, 0.000000000000000000 ) ) ;
#211748 = DIRECTION ( 'NONE',  ( 0.000000000000000000, 0.2868887416116073785, -0.9579639084728132081 ) ) ;
#211749 = CARTESIAN_POINT ( 'NONE',  ( -18.40000000000000213, 16.38400329561159907, -222.2501914957450424 ) ) ;
#211750 = DIRECTION ( 'NONE',  ( 0.000000000000000000, -0.9126074666063768159, -0.4088369013363282178 ) ) ;
#211751 = VERTEX_POINT ( 'NONE', #15050 ) ;
#211752 = EDGE_CURVE ( 'NONE', #365, #245608, #31855, .T. ) ;
#211753 = DIRECTION ( 'NONE',  ( 0.000000000000000000, 0.000000000000000000, -1.000000000000000000 ) ) ;
#211754 = CARTESIAN_POINT ( 'NONE',  ( -21.05000000000000071, 5.900000000011162093, -123.7809002353436654 ) ) ;
#211755 = AXIS2_PLACEMENT_3D ( 'NONE', #65094, #144613, #175767 ) ;
#211756 = CIRCLE ( 'NONE', #170099, 0.09999999999998898659 ) ;
#211757 = VERTEX_POINT ( 'NONE', #214506 ) ;
#211758 = VECTOR ( 'NONE', #108967, 999.9999999999998863 ) ;
#211759 = CARTESIAN_POINT ( 'NONE',  ( -21.05000000000000071, 1.249999999999999334, -8.000000000000000000 ) ) ;
#211760 = EDGE_LOOP ( 'NONE', ( #194969, #177407, #124588, #139259 ) ) ;
#211761 = CIRCLE ( 'NONE', #41094, 12.77499999999999503 ) ;
#211762 = LINE ( 'NONE', #173964, #81880 ) ;
#211763 = ORIENTED_EDGE ( 'NONE', *, *, #137616, .F. ) ;
#211764 = EDGE_CURVE ( 'NONE', #228920, #8033, #65140, .T. ) ;
#211765 = DIRECTION ( 'NONE',  ( 0.000000000000000000, 0.2128009952263403282, -0.9770955615653358350 ) ) ;
#211767 = ORIENTED_EDGE ( 'NONE', *, *, #44965, .T. ) ;
#211766 = CARTESIAN_POINT ( 'NONE',  ( -20.85000000000000142, 14.80545736607782814, -235.9842437978701639 ) ) ;
#211769 = EDGE_CURVE ( 'NONE', #46074, #217380, #115408, .T. ) ;
#211768 = DIRECTION ( 'NONE',  ( 1.000000000000000000, 0.000000000000000000, 0.000000000000000000 ) ) ;
#211770 = ORIENTED_EDGE ( 'NONE', *, *, #171588, .F. ) ;
#211771 = LINE ( 'NONE', #112668, #105468 ) ;
#211772 = CIRCLE ( 'NONE', #141043, 0.1000000000000088318 ) ;
#211773 = AXIS2_PLACEMENT_3D ( 'NONE', #170881, #232100, #32640 ) ;
#211774 = ORIENTED_EDGE ( 'NONE', *, *, #156645, .T. ) ;
#211776 = ORIENTED_EDGE ( 'NONE', *, *, #30682, .F. ) ;
#211775 = ORIENTED_EDGE ( 'NONE', *, *, #239726, .F. ) ;
#211778 = CARTESIAN_POINT ( 'NONE',  ( 18.50000000000000000, 85.40000000001207070, -129.2258477248609552 ) ) ;
#211777 = AXIS2_PLACEMENT_3D ( 'NONE', #160409, #120001, #196927 ) ;
#211780 = VERTEX_POINT ( 'NONE', #192390 ) ;
#211779 = CARTESIAN_POINT ( 'NONE',  ( -22.39999999999999503, 10.71943444926882449, -226.8179467668883547 ) ) ;
#211781 = CYLINDRICAL_SURFACE ( 'NONE', #102234, 0.1000000000000055844 ) ;
#211782 = ORIENTED_EDGE ( 'NONE', *, *, #145478, .T. ) ;
#211783 = VECTOR ( 'NONE', #19088, 1000.000000000000000 ) ;
#211784 = ADVANCED_FACE ( 'NONE', ( #90707 ), #194977, .T. ) ;
#211785 = EDGE_CURVE ( 'NONE', #60290, #123266, #140140, .T. ) ;
#211786 = ORIENTED_EDGE ( 'NONE', *, *, #65669, .T. ) ;
#211787 = DIRECTION ( 'NONE',  ( 1.000000000000000000, 0.000000000000000000, 0.000000000000000000 ) ) ;
#211788 = CYLINDRICAL_SURFACE ( 'NONE', #238941, 0.09999999999999939493 ) ;
#211789 = CARTESIAN_POINT ( 'NONE',  ( -21.37071067811865532, 67.92928932189387581, -182.2731074845244166 ) ) ;
#211790 = ORIENTED_EDGE ( 'NONE', *, *, #76738, .T. ) ;
#211791 = EDGE_CURVE ( 'NONE', #162828, #39149, #235350, .T. ) ;
#211792 = CARTESIAN_POINT ( 'NONE',  ( -18.58222699835055280, 65.66799936921553638, -130.9299399888601272 ) ) ;
#211793 = DIRECTION ( 'NONE',  ( 0.000000000000000000, -0.000000000000000000, 1.000000000000000000 ) ) ;
#211794 = VERTEX_POINT ( 'NONE', #174153 ) ;
#211795 = CARTESIAN_POINT ( 'NONE',  ( -18.59999999999999787, -9.480686695267820596, -73.94111516875784673 ) ) ;
#211796 = CARTESIAN_POINT ( 'NONE',  ( -20.94999999999999929, 70.97296516614450468, -234.1788952109995137 ) ) ;
#211797 = FACE_OUTER_BOUND ( 'NONE', #198102, .T. ) ;
#211798 = ADVANCED_FACE ( 'NONE', ( #56687 ), #215779, .F. ) ;
#211799 = VERTEX_POINT ( 'NONE', #140093 ) ;
#211800 = CARTESIAN_POINT ( 'NONE',  ( 18.50211644919734866, 10.30207779525984613, -105.9895520716782897 ) ) ;
#211801 = ORIENTED_EDGE ( 'NONE', *, *, #120095, .F. ) ;
#211802 = CARTESIAN_POINT ( 'NONE',  ( -18.45037301276683195, -7.780528700220050276, -209.8715768735301594 ) ) ;
#211803 = CIRCLE ( 'NONE', #186686, 0.1000000000000032391 ) ;
#211804 = VERTEX_POINT ( 'NONE', #176693 ) ;
#211805 = AXIS2_PLACEMENT_3D ( 'NONE', #243395, #64759, #144271 ) ;
#211806 = EDGE_CURVE ( 'NONE', #202516, #247315, #44317, .T. ) ;
#211807 = DIRECTION ( 'NONE',  ( -1.000000000000000000, -0.000000000000000000, -0.000000000000000000 ) ) ;
#211808 = LINE ( 'NONE', #111417, #206255 ) ;
#211809 = ORIENTED_EDGE ( 'NONE', *, *, #187175, .T. ) ;
#211810 = ORIENTED_EDGE ( 'NONE', *, *, #2473, .F. ) ;
#211811 = DIRECTION ( 'NONE',  ( 2.952720810173289112E-16, -1.000000000000000000, 0.000000000000000000 ) ) ;
#211812 = DIRECTION ( 'NONE',  ( -1.000000000000000000, 0.000000000000000000, 0.000000000000000000 ) ) ;
#211813 = ORIENTED_EDGE ( 'NONE', *, *, #113980, .T. ) ;
#211814 = AXIS2_PLACEMENT_3D ( 'NONE', #107933, #88337, #29715 ) ;
#211815 = VERTEX_POINT ( 'NONE', #41041 ) ;
#211816 = DIRECTION ( 'NONE',  ( 0.000000000000000000, 0.000000000000000000, 1.000000000000000000 ) ) ;
#211817 = DIRECTION ( 'NONE',  ( 0.000000000000000000, 1.000000000000000000, 6.982962677686266711E-15 ) ) ;
#211818 = EDGE_CURVE ( 'NONE', #193318, #239043, #157134, .T. ) ;
#211819 = ORIENTED_EDGE ( 'NONE', *, *, #251487, .F. ) ;
#211820 = B_SPLINE_CURVE_WITH_KNOTS ( 'NONE', 3,
 ( #241071, #119846, #199377, #239775, #61127, #220217, #62423, #141944, #66272, #68851 ),
 .UNSPECIFIED., .F., .F.,
 ( 4, 3, 3, 4 ),
 ( 1.957469226477651626E-15, 8.145022132840017156E-06, 1.905645951092857371E-05, 2.061107371226198839E-05 ),
 .UNSPECIFIED. ) ;
#211821 = VECTOR ( 'NONE', #54279, 1000.000000000000227 ) ;
#211822 = CIRCLE ( 'NONE', #103630, 4.149999999999996803 ) ;
#211824 = ORIENTED_EDGE ( 'NONE', *, *, #96388, .F. ) ;
#211823 = AXIS2_PLACEMENT_3D ( 'NONE', #63881, #137305, #181283 ) ;
#211826 = LINE ( 'NONE', #256016, #39256 ) ;
#211825 = CIRCLE ( 'NONE', #199361, 0.1999999999999987899 ) ;
#211827 = DIRECTION ( 'NONE',  ( 0.000000000000000000, 0.3343365196859449662, -0.9424537609900497381 ) ) ;
#211828 = CARTESIAN_POINT ( 'NONE',  ( -16.87851181299898684, 9.950042924018893231, -46.14985648463308365 ) ) ;
#211829 = VERTEX_POINT ( 'NONE', #43589 ) ;
#211830 = TOROIDAL_SURFACE ( 'NONE', #120293, 0.2000000000000000111, 0.1000000000000000056 ) ;
#211832 = VECTOR ( 'NONE', #204881, 1000.000000000000000 ) ;
#211831 = CARTESIAN_POINT ( 'NONE',  ( -17.29158576265544056, 10.36474766602906605, -111.9172417552078684 ) ) ;
#211833 = DIRECTION ( 'NONE',  ( 0.000000000000000000, -7.056502275159890043E-15, 1.000000000000000000 ) ) ;
#211834 = DIRECTION ( 'NONE',  ( 2.952720810173289112E-16, 1.000000000000000000, 6.938893903907222067E-15 ) ) ;
#211836 = DIRECTION ( 'NONE',  ( 0.000000000000000000, 6.982962677686266711E-15, -1.000000000000000000 ) ) ;
#211835 = CARTESIAN_POINT ( 'NONE',  ( 21.05000000000000071, 76.00000000001213607, -136.5231074845242745 ) ) ;
#211837 = CARTESIAN_POINT ( 'NONE',  ( -18.40000000000000213, 5.650000000011139001, -188.3499999999999659 ) ) ;
#211838 = CARTESIAN_POINT ( 'NONE',  ( -23.15000000000000213, 87.48912529308798014, -106.1231074845242262 ) ) ;
#211839 = CIRCLE ( 'NONE', #178544, 0.09999999999999711897 ) ;
#211840 = CARTESIAN_POINT ( 'NONE',  ( 18.59999999999999076, 46.54514716347711101, -243.1111603596801842 ) ) ;
#211841 = CARTESIAN_POINT ( 'NONE',  ( -21.07954763557765432, 75.93412408139404590, -176.3523984745653195 ) ) ;
#211842 = ORIENTED_EDGE ( 'NONE', *, *, #52524, .F. ) ;
#211843 = ADVANCED_FACE ( 'NONE', ( #217059 ), #48387, .T. ) ;
#211844 = VECTOR ( 'NONE', #73048, 1000.000000000000114 ) ;
#211845 = VECTOR ( 'NONE', #81081, 1000.000000000000000 ) ;
#211846 = CIRCLE ( 'NONE', #249448, 11.70000000000000284 ) ;
#211847 = CIRCLE ( 'NONE', #132924, 12.87500000000000178 ) ;
#211848 = ORIENTED_EDGE ( 'NONE', *, *, #181686, .T. ) ;
#211849 = CIRCLE ( 'NONE', #170373, 0.09999999999998898659 ) ;
#211850 = ADVANCED_FACE ( 'NONE', ( #38446 ), #63129, .T. ) ;
#211851 = ADVANCED_FACE ( 'NONE', ( #218343 ), #180537, .T. ) ;
#211852 = CARTESIAN_POINT ( 'NONE',  ( -18.59999999999999787, 23.34004772283014972, -229.2004250369967338 ) ) ;
#211853 = CARTESIAN_POINT ( 'NONE',  ( 20.94999999999999929, 6.650000000011155876, -155.2500000000000284 ) ) ;
#211854 = ORIENTED_EDGE ( 'NONE', *, *, #140449, .T. ) ;
#211855 = ADVANCED_FACE ( 'NONE', ( #57986 ), #117984, .T. ) ;
#211856 =( NAMED_UNIT ( * ) SI_UNIT ( $, .STERADIAN. ) SOLID_ANGLE_UNIT ( ) );
#211857 = EDGE_CURVE ( 'NONE', #92855, #155056, #27767, .T. ) ;
#211858 = CARTESIAN_POINT ( 'NONE',  ( 18.54999999999999716, 64.24389422848744857, -213.4417251850286164 ) ) ;
#211859 = PRODUCT ( 'Snap Open Cable Crossbars 2', 'Snap Open Cable Crossbars 2', '', ( #11844 ) ) ;
#211860 = ADVANCED_FACE ( 'NONE', ( #17584 ), #184134, .T. ) ;
#211861 = CARTESIAN_POINT ( 'NONE',  ( 20.94999999999999929, 8.876614585098254295, -142.3850804788447135 ) ) ;
#211862 = EDGE_LOOP ( 'NONE', ( #168752, #202585, #174876, #226580, #76673 ) ) ;
#211864 = EDGE_CURVE ( 'NONE', #90236, #188280, #236634, .T. ) ;
#211863 = VECTOR ( 'NONE', #184501, 1000.000000000000000 ) ;
#211865 = AXIS2_PLACEMENT_3D ( 'NONE', #18247, #138167, #195623 ) ;
#211866 = VERTEX_POINT ( 'NONE', #59244 ) ;
#211867 = CARTESIAN_POINT ( 'NONE',  ( 20.85000000000000142, 76.32388570108174974, -36.06551789521033413 ) ) ;
#211869 = AXIS2_PLACEMENT_3D ( 'NONE', #27344, #211074, #32471 ) ;
#211868 = CARTESIAN_POINT ( 'NONE',  ( -23.15000000000000213, 11.65000000001115588, -112.6500000000000483 ) ) ;
#211870 = ORIENTED_EDGE ( 'NONE', *, *, #257197, .F. ) ;
#211871 = ADVANCED_FACE ( 'NONE', ( #39763 ), #107404, .T. ) ;
#211872 = LINE ( 'NONE', #13652, #166201 ) ;
#211874 = ORIENTED_EDGE ( 'NONE', *, *, #252813, .F. ) ;
#211873 = CARTESIAN_POINT ( 'NONE',  ( 20.94999999999999929, 45.73145985849338047, -239.4600911154851133 ) ) ;
#211875 = FACE_OUTER_BOUND ( 'NONE', #103351, .T. ) ;
#211877 = ORIENTED_EDGE ( 'NONE', *, *, #191542, .T. ) ;
#211876 = CARTESIAN_POINT ( 'NONE',  ( -20.64999999999999858, 54.82645269529697885, -239.3027372265576957 ) ) ;
#211878 = CIRCLE ( 'NONE', #245196, 0.09999999999998898659 ) ;
#211879 = CARTESIAN_POINT ( 'NONE',  ( 20.94999999999999929, 67.22371710471952611, -115.2731074845243597 ) ) ;
#211880 = CARTESIAN_POINT ( 'NONE',  ( -16.97683809663755028, 9.950000000011142376, -87.22847083211067343 ) ) ;
#211881 = DIRECTION ( 'NONE',  ( -1.000000000000000000, 0.000000000000000000, 0.000000000000000000 ) ) ;
#211882 = CIRCLE ( 'NONE', #141150, 0.09999999999999993616 ) ;
#211883 = CARTESIAN_POINT ( 'NONE',  ( -18.59999999999999787, 64.35000000001187459, -90.87310748452438247 ) ) ;
#211885 = CARTESIAN_POINT ( 'NONE',  ( 20.54374330479337374, 10.50501031423420351, -108.2256836348895632 ) ) ;
#211884 = DIRECTION ( 'NONE',  ( 0.000000000000000000, 0.4721928772777294059, 0.8814952561688458310 ) ) ;
#211886 = DIRECTION ( 'NONE',  ( 0.7071067811865475727, 0.7071067811865475727, 4.937700262164531476E-15 ) ) ;
#211887 = CIRCLE ( 'NONE', #41020, 0.1000000000000043493 ) ;
#211888 = FACE_OUTER_BOUND ( 'NONE', #53681, .T. ) ;
#211889 = CARTESIAN_POINT ( 'NONE',  ( -5.899999999999938183, 64.65000000001120384, -26.02310748452479316 ) ) ;
#211890 = FACE_OUTER_BOUND ( 'NONE', #27206, .T. ) ;
#211892 = EDGE_LOOP ( 'NONE', ( #88390, #194167, #19979, #165230, #160548, #122652 ) ) ;
#211891 = CIRCLE ( 'NONE', #124400, 7.720710678118692272 ) ;
#211893 = EDGE_CURVE ( 'NONE', #54334, #208398, #52657, .T. ) ;
#211894 = CYLINDRICAL_SURFACE ( 'NONE', #213943, 0.09999999999999939493 ) ;
#211895 = EDGE_LOOP ( 'NONE', ( #147552, #245939, #257380, #156100 ) ) ;
#211896 = CARTESIAN_POINT ( 'NONE',  ( -23.49999999999994316, 74.25000000001119815, -47.64205752314703801 ) ) ;
#211897 = EDGE_LOOP ( 'NONE', ( #136082, #9673, #146829, #55989 ) ) ;
#211898 = CARTESIAN_POINT ( 'NONE',  ( -20.85000000000000142, 77.85161776048053639, -57.91991776492063337 ) ) ;
#211899 = CARTESIAN_POINT ( 'NONE',  ( -18.50000000000000000, 74.93036000061670165, -233.6816308724374949 ) ) ;
#211900 = ADVANCED_FACE ( 'NONE', ( #146516 ), #145236, .T. ) ;
#211901 = ADVANCED_FACE ( 'NONE', ( #123131 ), #143957, .T. ) ;
#211902 = AXIS2_PLACEMENT_3D ( 'NONE', #234715, #75659, #194330 ) ;
#211903 = VECTOR ( 'NONE', #96449, 1000.000000000000000 ) ;
#211904 = VERTEX_POINT ( 'NONE', #166140 ) ;
#211905 = AXIS2_PLACEMENT_3D ( 'NONE', #205329, #8445, #86655 ) ;
#211906 = DIRECTION ( 'NONE',  ( -4.448008912761047751E-16, -0.4088369013363289950, 0.9126074666063765939 ) ) ;
#211907 = PRESENTATION_STYLE_ASSIGNMENT (( #35835 ) ) ;
#211908 = EDGE_LOOP ( 'NONE', ( #155364, #200526, #226938, #243581 ) ) ;
#211909 = ORIENTED_EDGE ( 'NONE', *, *, #165949, .F. ) ;
#211910 = CARTESIAN_POINT ( 'NONE',  ( 20.94999999999999929, -9.399999999988844834, -157.6060308773475640 ) ) ;
#211911 = CYLINDRICAL_SURFACE ( 'NONE', #124390, 11.75000000000001066 ) ;
#211912 = PLANE ( 'NONE',  #113676 ) ;
#211913 = CARTESIAN_POINT ( 'NONE',  ( 20.94999999999999574, 10.47338541492405994, -41.07865446424855094 ) ) ;
#211914 = CARTESIAN_POINT ( 'NONE',  ( -23.15000000000000213, 1.115600667400684642E-11, -134.0000000000000284 ) ) ;
#211916 = DIRECTION ( 'NONE',  ( 1.000000000000000000, 7.304098846218134667E-16, 0.000000000000000000 ) ) ;
#211915 = FACE_OUTER_BOUND ( 'NONE', #125300, .T. ) ;
#211917 = CARTESIAN_POINT ( 'NONE',  ( -13.77178122865953824, 9.456028260519072859, -82.01119803506577455 ) ) ;
#211919 = ORIENTED_EDGE ( 'NONE', *, *, #234035, .T. ) ;
#211918 = DIRECTION ( 'NONE',  ( 0.000000000000000000, 1.000000000000000000, 0.000000000000000000 ) ) ;
#211921 = CARTESIAN_POINT ( 'NONE',  ( -21.14999999999999858, 76.00000000001222134, -148.1726782920690937 ) ) ;
#211920 = CARTESIAN_POINT ( 'NONE',  ( 22.60000000000000142, 75.89914163091351895, -148.2726746080136877 ) ) ;
#211922 = DIRECTION ( 'NONE',  ( -1.000000000000000000, 0.000000000000000000, 0.000000000000000000 ) ) ;
#211923 = ORIENTED_EDGE ( 'NONE', *, *, #180459, .F. ) ;
#211924 = CARTESIAN_POINT ( 'NONE',  ( -18.40000000000000213, -9.519327731081286714, -174.4729763765592736 ) ) ;
#211925 = AXIS2_PLACEMENT_3D ( 'NONE', #222572, #63508, #47786 ) ;
#211926 = DIRECTION ( 'NONE',  ( -0.000000000000000000, -0.000000000000000000, -1.000000000000000000 ) ) ;
#211927 = ORIENTED_EDGE ( 'NONE', *, *, #17635, .F. ) ;
#211928 = DIRECTION ( 'NONE',  ( -1.000000000000000000, 2.849773892568378313E-16, -7.728835255496647986E-17 ) ) ;
#211929 = DIRECTION ( 'NONE',  ( -1.000000000000000000, -0.000000000000000000, -0.000000000000000000 ) ) ;
#211930 = CARTESIAN_POINT ( 'NONE',  ( 20.94999999999999929, 62.04503132991427350, -248.4786563706009588 ) ) ;
#211931 = EDGE_LOOP ( 'NONE', ( #81469, #22859, #96283, #162480 ) ) ;
#211932 = ORIENTED_EDGE ( 'NONE', *, *, #36589, .F. ) ;
#211933 = CARTESIAN_POINT ( 'NONE',  ( 20.94999999999999929, 4.999999999999997335, -21.09473398108690390 ) ) ;
#211934 = CARTESIAN_POINT ( 'NONE',  ( -18.55807992284871943, 10.32898536001801304, -173.0826683222764757 ) ) ;
#211935 = DIRECTION ( 'NONE',  ( -4.701977403289178058E-30, -2.433019743745433765E-14, 1.000000000000000000 ) ) ;
#211936 = CARTESIAN_POINT ( 'NONE',  ( 18.59999999999999787, -1.835341550224411922, -11.65515129256297833 ) ) ;
#211937 = EDGE_LOOP ( 'NONE', ( #147998, #186229, #225624, #154013, #126581, #255120 ) ) ;
#211938 = CARTESIAN_POINT ( 'NONE',  ( 13.22261339317536866, 46.65242889160096951, -234.7339858363277187 ) ) ;
#211939 = ADVANCED_FACE ( 'NONE', ( #202650 ), #246910, .T. ) ;
#211940 = FACE_OUTER_BOUND ( 'NONE', #142665, .T. ) ;
#211941 = DIRECTION ( 'NONE',  ( 1.000000000000000000, 0.000000000000000000, 0.000000000000000000 ) ) ;
#211942 = VECTOR ( 'NONE', #247585, 999.9999999999998863 ) ;
#211943 = DIRECTION ( 'NONE',  ( 0.000000000000000000, 0.000000000000000000, -1.000000000000000000 ) ) ;
#211944 = CIRCLE ( 'NONE', #86996, 0.1000000000000011990 ) ;
#211945 = ADVANCED_FACE ( 'NONE', ( #205208 ), #210795, .F. ) ;
#211946 = VECTOR ( 'NONE', #7994, 1000.000000000000000 ) ;
#211947 = ORIENTED_EDGE ( 'NONE', *, *, #176278, .T. ) ;
#211948 = CARTESIAN_POINT ( 'NONE',  ( 20.94999999999999574, 60.83337574417771521, -225.3422414619149095 ) ) ;
#211949 = EDGE_CURVE ( 'NONE', #58594, #194619, #119320, .T. ) ;
#211951 = ORIENTED_EDGE ( 'NONE', *, *, #200022, .F. ) ;
#211950 = CYLINDRICAL_SURFACE ( 'NONE', #91885, 1.749999999999999778 ) ;
#211952 = CIRCLE ( 'NONE', #37169, 0.09999999999999939493 ) ;
#211953 = DIRECTION ( 'NONE',  ( 0.000000000000000000, 2.891205793294679805E-16, -1.000000000000000000 ) ) ;
#211954 = EDGE_CURVE ( 'NONE', #78587, #71514, #40234, .T. ) ;
#211955 = CYLINDRICAL_SURFACE ( 'NONE', #120352, 2.599999999999998312 ) ;
#211956 = DIRECTION ( 'NONE',  ( 0.7071067811865460184, 0.6824534298470606997, -0.1850873201761399356 ) ) ;
#211957 = CARTESIAN_POINT ( 'NONE',  ( 20.94999999999999929, 76.00000000001155342, -56.54810748452432279 ) ) ;
#211958 = CARTESIAN_POINT ( 'NONE',  ( -21.05000000000000071, 87.48912529308779540, -72.62310748452422615 ) ) ;
#211959 = ORIENTED_EDGE ( 'NONE', *, *, #70550, .T. ) ;
#211960 = DIRECTION ( 'NONE',  ( 0.000000000000000000, 1.224646799147316229E-16, 1.000000000000000000 ) ) ;
#211961 = DIRECTION ( 'NONE',  ( -1.000000000000000000, -5.641646265808601873E-14, 4.044497296483820071E-14 ) ) ;
#211962 = LINE ( 'NONE', #192385, #98778 ) ;
#211963 = EDGE_LOOP ( 'NONE', ( #83310, #238810, #37977, #159252 ) ) ;
#211964 = DIRECTION ( 'NONE',  ( 1.000000000000000000, 0.000000000000000000, 0.000000000000000000 ) ) ;
#211965 = FACE_OUTER_BOUND ( 'NONE', #78763, .T. ) ;
#211966 = CARTESIAN_POINT ( 'NONE',  ( 20.04142135623731136, 11.75000000001116085, -58.26715728752539292 ) ) ;
#211967 = AXIS2_PLACEMENT_3D ( 'NONE', #156347, #38946, #57183 ) ;
#211968 = CIRCLE ( 'NONE', #107885, 0.09999999999999489853 ) ;
#211969 = DIRECTION ( 'NONE',  ( -1.000000000000000000, 0.000000000000000000, -0.000000000000000000 ) ) ;
#211970 = AXIS2_PLACEMENT_3D ( 'NONE', #226762, #187667, #212360 ) ;
#211971 = CYLINDRICAL_SURFACE ( 'NONE', #246354, 0.1000000000000055844 ) ;
#211972 = CARTESIAN_POINT ( 'NONE',  ( 13.88638282980484284, 9.457426452500056868, -186.0000418683999897 ) ) ;
#211974 = EDGE_CURVE ( 'NONE', #224742, #125106, #219265, .T. ) ;
#211973 = CIRCLE ( 'NONE', #74445, 12.77500000000000924 ) ;
#211975 = EDGE_CURVE ( 'NONE', #217568, #611, #116743, .T. ) ;
#211976 = ORIENTED_EDGE ( 'NONE', *, *, #191598, .T. ) ;
#211977 = VERTEX_POINT ( 'NONE', #41879 ) ;
#211978 = DIRECTION ( 'NONE',  ( 1.000000000000000000, 0.000000000000000000, 0.000000000000000000 ) ) ;
#211979 = DIRECTION ( 'NONE',  ( 1.000000000000000000, 0.000000000000000000, 0.000000000000000000 ) ) ;
#211980 = DIRECTION ( 'NONE',  ( 1.000000000000000000, 0.000000000000000000, 0.000000000000000000 ) ) ;
#211981 = CYLINDRICAL_SURFACE ( 'NONE', #18357, 0.1000000000000028644 ) ;
#211982 = CARTESIAN_POINT ( 'NONE',  ( 20.04999999999999716, 8.750000000011173285, -176.7499999999999716 ) ) ;
#211983 = FACE_OUTER_BOUND ( 'NONE', #227148, .T. ) ;
#211984 = ADVANCED_FACE ( 'NONE', ( #143513 ), #180096, .T. ) ;
#211985 = DIRECTION ( 'NONE',  ( -1.000000000000000000, -0.000000000000000000, -0.000000000000000000 ) ) ;
#211986 = EDGE_CURVE ( 'NONE', #79953, #184680, #40610, .T. ) ;
#211987 = AXIS2_PLACEMENT_3D ( 'NONE', #213729, #135463, #113352 ) ;
#211989 = DIRECTION ( 'NONE',  ( 0.000000000000000000, 0.000000000000000000, -1.000000000000000000 ) ) ;
#211988 = VECTOR ( 'NONE', #4159, 1000.000000000000000 ) ;
#211990 = ORIENTED_EDGE ( 'NONE', *, *, #139723, .F. ) ;
#211991 = FACE_OUTER_BOUND ( 'NONE', #212972, .T. ) ;
#211992 = ORIENTED_EDGE ( 'NONE', *, *, #257212, .T. ) ;
#211993 = CARTESIAN_POINT ( 'NONE',  ( 18.59999999999999076, 63.85700577439690306, -209.2959117565043243 ) ) ;
#211994 = CARTESIAN_POINT ( 'NONE',  ( 21.05000000000000071, 10.56271494672853528, -7.456802105644634082 ) ) ;
#211995 = AXIS2_PLACEMENT_3D ( 'NONE', #111793, #73975, #51788 ) ;
#211997 = ORIENTED_EDGE ( 'NONE', *, *, #190710, .T. ) ;
#211996 = CARTESIAN_POINT ( 'NONE',  ( 20.95512820512820440, 64.22684239030566289, -213.0226507412649255 ) ) ;
#211998 = EDGE_CURVE ( 'NONE', #91113, #5814, #131963, .T. ) ;
#211999 = CARTESIAN_POINT ( 'NONE',  ( 23.25000000000000000, 85.00000000001251976, -179.9170766071767389 ) ) ;
#212000 = DIRECTION ( 'NONE',  ( 1.000000000000000000, 0.000000000000000000, 0.000000000000000000 ) ) ;
#212001 = EDGE_CURVE ( 'NONE', #243580, #95790, #82225, .T. ) ;
#212002 = ORIENTED_EDGE ( 'NONE', *, *, #57283, .T. ) ;
#212003 = CARTESIAN_POINT ( 'NONE',  ( -16.93339986808596365, 22.93003596233614161, -230.8468223696792734 ) ) ;
#212004 = CARTESIAN_POINT ( 'NONE',  ( 20.94999999999999929, 28.40523720341322544, -239.6697522603257937 ) ) ;
#212005 = CARTESIAN_POINT ( 'NONE',  ( 20.94999999999999929, 85.50000000001232081, -160.1291383618718385 ) ) ;
#212006 = DIRECTION ( 'NONE',  ( 0.000000000000000000, 1.000000000000000000, 0.000000000000000000 ) ) ;
#212007 = ADVANCED_FACE ( 'NONE', ( #203501 ), #238776, .F. ) ;
#212008 = AXIS2_PLACEMENT_3D ( 'NONE', #123094, #104765, #184325 ) ;
#212009 = AXIS2_PLACEMENT_3D ( 'NONE', #148110, #211941, #189803 ) ;
#212010 = DIRECTION ( 'NONE',  ( -0.7071067811865457964, -0.2890913453342137673, 0.6453109281988465007 ) ) ;
#212011 = VECTOR ( 'NONE', #176418, 1000.000000000000000 ) ;
#212012 = ORIENTED_EDGE ( 'NONE', *, *, #212538, .T. ) ;
#212013 = DIRECTION ( 'NONE',  ( 1.000000000000000000, 0.000000000000000000, 0.000000000000000000 ) ) ;
#212014 = FACE_OUTER_BOUND ( 'NONE', #166255, .T. ) ;
#212015 = VERTEX_POINT ( 'NONE', #39310 ) ;
#212016 = ADVANCED_FACE ( 'NONE', ( #121428 ), #118843, .T. ) ;
#212017 = ORIENTED_EDGE ( 'NONE', *, *, #112263, .T. ) ;
#212018 = LINE ( 'NONE', #32104, #1573 ) ;
#212019 = DIRECTION ( 'NONE',  ( 0.000000000000000000, -0.000000000000000000, -1.000000000000000000 ) ) ;
#212020 = CIRCLE ( 'NONE', #253682, 2.000000000000000000 ) ;
#212021 = CIRCLE ( 'NONE', #257740, 0.1000000000000028644 ) ;
#212022 = EDGE_CURVE ( 'NONE', #77477, #106096, #69446, .T. ) ;
#212023 = VERTEX_POINT ( 'NONE', #200930 ) ;
#212024 = DIRECTION ( 'NONE',  ( -0.000000000000000000, 0.1022405907414166287, 0.9947597004326451664 ) ) ;
#212025 = LINE ( 'NONE', #35953, #197489 ) ;
#212026 = EDGE_LOOP ( 'NONE', ( #73160, #32309, #101931, #117228 ) ) ;
#212027 = AXIS2_PLACEMENT_3D ( 'NONE', #186236, #23335, #166699 ) ;
#212028 = AXIS2_PLACEMENT_3D ( 'NONE', #229304, #212316, #113197 ) ;
#212029 = VECTOR ( 'NONE', #12717, 1000.000000000000000 ) ;
#212030 = CARTESIAN_POINT ( 'NONE',  ( 20.12500000000000000, 9.750000000011153745, -188.6499999999999488 ) ) ;
#212031 = EDGE_LOOP ( 'NONE', ( #215633, #196508, #212951, #8764 ) ) ;
#212032 = CARTESIAN_POINT ( 'NONE',  ( -20.94999999999999929, 1.736257131608553550, -179.0686523290174819 ) ) ;
#212033 = CIRCLE ( 'NONE', #141289, 0.1000000000000002554 ) ;
#212034 = DIRECTION ( 'NONE',  ( 0.000000000000000000, -1.000000000000000000, 0.000000000000000000 ) ) ;
#212036 = EDGE_LOOP ( 'NONE', ( #209365, #25207, #190131, #185183 ) ) ;
#212035 = CARTESIAN_POINT ( 'NONE',  ( -16.87683809663752399, 9.849999999999988987, -13.40236401819630530 ) ) ;
#212037 = CYLINDRICAL_SURFACE ( 'NONE', #219807, 0.1000000000000028644 ) ;
#212039 = CARTESIAN_POINT ( 'NONE',  ( -22.39999999999999503, 7.790779598384560245, -133.9000000000000057 ) ) ;
#212038 = UNCERTAINTY_MEASURE_WITH_UNIT (LENGTH_MEASURE( 1.000000000000000082E-05 ), #230116, 'distance_accuracy_value', 'NONE');
#212040 = CARTESIAN_POINT ( 'NONE',  ( -18.59999999999999787, 64.25000000001264766, -196.5083017138704236 ) ) ;
#212041 = LINE ( 'NONE', #34690, #230933 ) ;
#212042 = CARTESIAN_POINT ( 'NONE',  ( -16.27683809663750480, 9.350000000011133849, -154.9500000000000455 ) ) ;
#212043 = DIRECTION ( 'NONE',  ( 1.000000000000000000, 0.000000000000000000, 0.000000000000000000 ) ) ;
#212044 = DIRECTION ( 'NONE',  ( 1.000000000000000000, 0.000000000000000000, 0.000000000000000000 ) ) ;
#212046 = ORIENTED_EDGE ( 'NONE', *, *, #139948, .T. ) ;
#212045 = CARTESIAN_POINT ( 'NONE',  ( 23.24999999999999289, 31.98723526783714277, -238.8784020251475511 ) ) ;
#212047 = VERTEX_POINT ( 'NONE', #221746 ) ;
#212049 = DIRECTION ( 'NONE',  ( -1.000000000000000000, 0.000000000000000000, 0.000000000000000000 ) ) ;
#212048 = DIRECTION ( 'NONE',  ( 0.000000000000000000, 0.000000000000000000, 1.000000000000000000 ) ) ;
#212051 = ORIENTED_EDGE ( 'NONE', *, *, #28306, .F. ) ;
#212050 = CARTESIAN_POINT ( 'NONE',  ( 20.95263205890712399, 8.895740107905197647, -75.48950840694165265 ) ) ;
#212052 = ORIENTED_EDGE ( 'NONE', *, *, #152556, .T. ) ;
#212053 = CARTESIAN_POINT ( 'NONE',  ( 21.05000000000000071, -10.60885044396467158, -206.2784744251879374 ) ) ;
#212054 = AXIS2_PLACEMENT_3D ( 'NONE', #83315, #140758, #220308 ) ;
#212055 = DIRECTION ( 'NONE',  ( -1.000000000000000000, -2.952720810173289112E-16, 0.000000000000000000 ) ) ;
#212056 = CARTESIAN_POINT ( 'NONE',  ( 23.14999999999999503, 45.02833974712562792, -238.5149546970766892 ) ) ;
#212057 = DIRECTION ( 'NONE',  ( 0.000000000000000000, 0.000000000000000000, 1.000000000000000000 ) ) ;
#212058 = DIRECTION ( 'NONE',  ( 0.000000000000000000, 0.000000000000000000, -1.000000000000000000 ) ) ;
#212059 = PLANE ( 'NONE',  #219618 ) ;
#212060 = CIRCLE ( 'NONE', #49557, 0.1999999999999987899 ) ;
#212061 = AXIS2_PLACEMENT_3D ( 'NONE', #128996, #170735, #252768 ) ;
#212062 = DIRECTION ( 'NONE',  ( 0.000000000000000000, 0.000000000000000000, -1.000000000000000000 ) ) ;
#212063 = ORIENTED_EDGE ( 'NONE', *, *, #107991, .F. ) ;
#212064 = EDGE_LOOP ( 'NONE', ( #103344, #61983 ) ) ;
#212065 = EDGE_CURVE ( 'NONE', #87244, #84905, #141, .T. ) ;
#212066 = CARTESIAN_POINT ( 'NONE',  ( -20.15000000000000568, 13.57934761686182057, -219.6883474154335261 ) ) ;
#212067 = AXIS2_PLACEMENT_3D ( 'NONE', #233182, #153678, #74114 ) ;
#212068 = ORIENTED_EDGE ( 'NONE', *, *, #205268, .T. ) ;
#212069 = CARTESIAN_POINT ( 'NONE',  ( -22.39999999999999858, 31.89597452117651244, -238.9192857152811769 ) ) ;
#212070 = ORIENTED_EDGE ( 'NONE', *, *, #127798, .F. ) ;
#212071 = DIRECTION ( 'NONE',  ( 1.000000000000000000, 0.000000000000000000, 0.000000000000000000 ) ) ;
#212072 = AXIS2_PLACEMENT_3D ( 'NONE', #163453, #25242, #185577 ) ;
#212073 = CARTESIAN_POINT ( 'NONE',  ( -33.72168855820452649, 54.09900352584866567, -229.1663746252470446 ) ) ;
#212074 = EDGE_CURVE ( 'NONE', #81149, #30084, #199666, .T. ) ;
#212075 = LINE ( 'NONE', #34733, #48414 ) ;
#212076 = ORIENTED_EDGE ( 'NONE', *, *, #116924, .T. ) ;
#212077 = DIRECTION ( 'NONE',  ( 1.000000000000000000, 0.000000000000000000, 0.000000000000000000 ) ) ;
#212078 = ORIENTED_EDGE ( 'NONE', *, *, #172631, .F. ) ;
#212079 = EDGE_CURVE ( 'NONE', #65499, #17436, #43148, .T. ) ;
#212081 = EDGE_CURVE ( 'NONE', #206540, #181805, #102712, .T. ) ;
#212080 = AXIS2_PLACEMENT_3D ( 'NONE', #187598, #149756, #53196 ) ;
#212082 = DIRECTION ( 'NONE',  ( -1.000000000000000000, -0.000000000000000000, 0.000000000000000000 ) ) ;
#212083 = CARTESIAN_POINT ( 'NONE',  ( -18.59999999999999787, 52.32046880629621199, -232.2896150449452364 ) ) ;
#212084 = AXIS2_PLACEMENT_3D ( 'NONE', #62677, #67799, #146043 ) ;
#212085 = ORIENTED_EDGE ( 'NONE', *, *, #99075, .T. ) ;
#212086 = CARTESIAN_POINT ( 'NONE',  ( -23.15000000000000213, 74.00000000001156764, -56.29848556176223440 ) ) ;
#212087 = ORIENTED_EDGE ( 'NONE', *, *, #61729, .T. ) ;
#212090 = EDGE_LOOP ( 'NONE', ( #161125, #57972, #173965, #32607, #172867, #33130, #100193, #143012, #90728, #5756, #118408, #30107, #117836, #241858, #203711, #233900, #154608, #114569 ) ) ;
#212089 = DIRECTION ( 'NONE',  ( 2.915501640297155269E-16, -1.000000000000000000, 0.000000000000000000 ) ) ;
#212088 = DIRECTION ( 'NONE',  ( 0.000000000000000000, 0.000000000000000000, -1.000000000000000000 ) ) ;
#212091 = VECTOR ( 'NONE', #143731, 1000.000000000000000 ) ;
#212092 = ORIENTED_EDGE ( 'NONE', *, *, #152698, .T. ) ;
#212093 = ORIENTED_EDGE ( 'NONE', *, *, #108779, .T. ) ;
#212094 = ADVANCED_FACE ( 'NONE', ( #122697 ), #103086, .F. ) ;
#212095 = LINE ( 'NONE', #251183, #244776 ) ;
#212096 = EDGE_CURVE ( 'NONE', #14406, #20329, #115211, .T. ) ;
#212097 = ORIENTED_EDGE ( 'NONE', *, *, #10899, .T. ) ;
#212098 = DIRECTION ( 'NONE',  ( 0.000000000000000000, 0.9126074666063771490, 0.4088369013363278293 ) ) ;
#212099 = CARTESIAN_POINT ( 'NONE',  ( 22.49436431346199683, 64.11729402989250559, -247.0813885053079275 ) ) ;
#212100 = CARTESIAN_POINT ( 'NONE',  ( 21.00000000000000000, 61.05385884576949707, -221.3836188041226762 ) ) ;
#212101 = DIRECTION ( 'NONE',  ( -4.336808689942053235E-15, -0.8660254037844482555, -0.4999999999999836797 ) ) ;
#212102 = ORIENTED_EDGE ( 'NONE', *, *, #244962, .T. ) ;
#212103 = CARTESIAN_POINT ( 'NONE',  ( -20.99142135623731065, 62.99095723518624368, -207.1734234082435364 ) ) ;
#212104 = DIRECTION ( 'NONE',  ( 0.000000000000000000, -1.000000000000000000, -6.352154140967427193E-15 ) ) ;
#212105 = AXIS2_PLACEMENT_3D ( 'NONE', #166510, #203029, #81772 ) ;
#212106 = FACE_OUTER_BOUND ( 'NONE', #83758, .T. ) ;
#212107 = ORIENTED_EDGE ( 'NONE', *, *, #38810, .T. ) ;
#212108 = CARTESIAN_POINT ( 'NONE',  ( -21.53551880898957904, 0.09896973457166240162, 6.784797761416331952 ) ) ;
#212109 = ORIENTED_EDGE ( 'NONE', *, *, #228544, .F. ) ;
#212110 = CARTESIAN_POINT ( 'NONE',  ( 21.00000000000000000, 12.13349391679638778, -210.8946109257198032 ) ) ;
#212111 = ORIENTED_EDGE ( 'NONE', *, *, #241004, .F. ) ;
#212112 = ADVANCED_FACE ( 'NONE', ( #130367 ), #65333, .T. ) ;
#212113 = FACE_OUTER_BOUND ( 'NONE', #86174, .T. ) ;
#212114 = DIRECTION ( 'NONE',  ( 3.816391647148962481E-13, 0.8825714802517645730, -0.4701782451860243017 ) ) ;
#212116 = ORIENTED_EDGE ( 'NONE', *, *, #185961, .T. ) ;
#212115 = FACE_BOUND ( 'NONE', #120182, .T. ) ;
#212117 = DIRECTION ( 'NONE',  ( -1.000000000000000000, -0.000000000000000000, -0.000000000000000000 ) ) ;
#212118 = ORIENTED_EDGE ( 'NONE', *, *, #135415, .F. ) ;
#212119 = FACE_OUTER_BOUND ( 'NONE', #67240, .T. ) ;
#212120 = CARTESIAN_POINT ( 'NONE',  ( -16.83233564386401682, 9.930221796595743555, -113.2754793365244126 ) ) ;
#212122 = ADVANCED_FACE ( 'NONE', ( #65263 ), #125247, .F. ) ;
#212121 = ORIENTED_EDGE ( 'NONE', *, *, #250503, .T. ) ;
#212123 = VECTOR ( 'NONE', #182172, 1000.000000000000227 ) ;
#212125 = AXIS2_PLACEMENT_3D ( 'NONE', #127839, #189089, #224353 ) ;
#212124 = DIRECTION ( 'NONE',  ( 0.000000000000000000, 0.000000000000000000, 1.000000000000000000 ) ) ;
#212126 = ORIENTED_EDGE ( 'NONE', *, *, #19230, .T. ) ;
#212127 = AXIS2_PLACEMENT_3D ( 'NONE', #13769, #93300, #209396 ) ;
#212129 = CARTESIAN_POINT ( 'NONE',  ( 18.52928932188133970, 65.72071067813085676, -145.2731074845244450 ) ) ;
#212128 = AXIS2_PLACEMENT_3D ( 'NONE', #108895, #168924, #228857 ) ;
#212130 = VERTEX_POINT ( 'NONE', #9152 ) ;
#212131 = CARTESIAN_POINT ( 'NONE',  ( -21.14999999999999858, 11.65000000001115588, -67.10000000000005116 ) ) ;
#212132 = AXIS2_PLACEMENT_3D ( 'NONE', #3800, #181168, #2494 ) ;
#212133 = CARTESIAN_POINT ( 'NONE',  ( 20.94999999999999929, 1.115600667400684642E-11, -200.9999999999999432 ) ) ;
#212136 = ORIENTED_EDGE ( 'NONE', *, *, #248185, .F. ) ;
#212135 = EDGE_LOOP ( 'NONE', ( #60557, #153012, #151554, #178842 ) ) ;
#212134 = DIRECTION ( 'NONE',  ( 1.000000000000000000, 0.000000000000000000, 0.000000000000000000 ) ) ;
#212137 = EDGE_CURVE ( 'NONE', #70064, #108484, #106947, .T. ) ;
#212138 = CARTESIAN_POINT ( 'NONE',  ( -23.25000000000000000, 1.115600667400684642E-11, -169.6000000000000227 ) ) ;
#212139 = AXIS2_PLACEMENT_3D ( 'NONE', #42906, #200695, #157766 ) ;
#212140 = CARTESIAN_POINT ( 'NONE',  ( 21.14999999999999858, 12.37888392014804495, -249.8746333190754569 ) ) ;
#212141 = LINE ( 'NONE', #113028, #6810 ) ;
#212142 = AXIS2_PLACEMENT_3D ( 'NONE', #249873, #174231, #252421 ) ;
#212144 = FACE_OUTER_BOUND ( 'NONE', #108133, .T. ) ;
#212143 = CYLINDRICAL_SURFACE ( 'NONE', #198236, 0.1000000000000028644 ) ;
#212145 = CARTESIAN_POINT ( 'NONE',  ( -18.40000000000000213, 11.48667500176882861, -158.2500000000000284 ) ) ;
#212146 = DIRECTION ( 'NONE',  ( 1.000000000000000000, 0.000000000000000000, 0.000000000000000000 ) ) ;
#212147 = CARTESIAN_POINT ( 'NONE',  ( -18.50000000000000000, 64.25000000001277556, -215.2731074845244450 ) ) ;
#212148 = VECTOR ( 'NONE', #9490, 1000.000000000000227 ) ;
#212149 = ORIENTED_EDGE ( 'NONE', *, *, #124575, .T. ) ;
#212150 = VERTEX_POINT ( 'NONE', #168268 ) ;
#212151 = ADVANCED_FACE ( 'NONE', ( #86080 ), #108254, .T. ) ;
#212152 = CARTESIAN_POINT ( 'NONE',  ( -22.59999999999999787, 11.74987124438766273, -33.43457040898632471 ) ) ;
#212153 = EDGE_CURVE ( 'NONE', #183226, #141859, #61238, .T. ) ;
#212154 = ORIENTED_EDGE ( 'NONE', *, *, #238293, .T. ) ;
#212155 = ORIENTED_EDGE ( 'NONE', *, *, #255338, .T. ) ;
#212156 = DIRECTION ( 'NONE',  ( -1.000000000000000000, 0.000000000000000000, 0.000000000000000000 ) ) ;
#212157 = ORIENTED_EDGE ( 'NONE', *, *, #122609, .T. ) ;
#212158 = CARTESIAN_POINT ( 'NONE',  ( 21.09793522318407355, 43.44397040381475961, -234.7599165424315402 ) ) ;
#212159 = EDGE_CURVE ( 'NONE', #244896, #71915, #190242, .T. ) ;
#212160 = EDGE_CURVE ( 'NONE', #84620, #5997, #243898, .T. ) ;
#212161 = ORIENTED_EDGE ( 'NONE', *, *, #106129, .T. ) ;
#212162 = EDGE_CURVE ( 'NONE', #125918, #114829, #186511, .T. ) ;
#212163 = CARTESIAN_POINT ( 'NONE',  ( 20.94999999999999929, 70.60000000001254250, -182.4283735034374843 ) ) ;
#212164 = AXIS2_PLACEMENT_3D ( 'NONE', #205903, #162956, #203348 ) ;
#212165 = EDGE_CURVE ( 'NONE', #239723, #111333, #77781, .T. ) ;
#212167 = ORIENTED_EDGE ( 'NONE', *, *, #25208, .F. ) ;
#212166 = ORIENTED_EDGE ( 'NONE', *, *, #243225, .T. ) ;
#212168 = ORIENTED_EDGE ( 'NONE', *, *, #67634, .T. ) ;
#212170 = EDGE_CURVE ( 'NONE', #79652, #167877, #126529, .T. ) ;
#212169 = EDGE_CURVE ( 'NONE', #119326, #207618, #19556, .T. ) ;
#212171 = VERTEX_POINT ( 'NONE', #185217 ) ;
#212172 = VERTEX_POINT ( 'NONE', #226904 ) ;
#212173 = LINE ( 'NONE', #173081, #55364 ) ;
#212174 = CARTESIAN_POINT ( 'NONE',  ( -20.64999999999999858, 2.000000000011154189, -120.7753780772379315 ) ) ;
#212175 = CARTESIAN_POINT ( 'NONE',  ( -15.75000000000001066, 9.350000000011142731, -184.3642676076160853 ) ) ;
#212177 = ORIENTED_EDGE ( 'NONE', *, *, #23240, .T. ) ;
#212176 = CARTESIAN_POINT ( 'NONE',  ( -21.55000000000000426, 7.708578643773852157, -146.3500000000000227 ) ) ;
#212178 = CIRCLE ( 'NONE', #199721, 0.1000000000000028644 ) ;
#212179 = CARTESIAN_POINT ( 'NONE',  ( 21.05000000000000071, 71.00000000001151079, -48.42837350343745584 ) ) ;
#212180 = CARTESIAN_POINT ( 'NONE',  ( 21.07016717456945187, 6.320940838111420490, -167.4999999999999432 ) ) ;
#212182 = ORIENTED_EDGE ( 'NONE', *, *, #137221, .T. ) ;
#212181 = DIRECTION ( 'NONE',  ( 1.000000000000000000, 0.000000000000000000, 0.000000000000000000 ) ) ;
#212183 = DIRECTION ( 'NONE',  ( 0.000000000000000000, 0.000000000000000000, -1.000000000000000000 ) ) ;
#212184 = ORIENTED_EDGE ( 'NONE', *, *, #164728, .T. ) ;
#212185 = CARTESIAN_POINT ( 'NONE',  ( 15.48841904831874849, 8.561580951692381092, -154.8500000000000227 ) ) ;
#212186 = EDGE_LOOP ( 'NONE', ( #217804, #145762, #208886, #198276 ) ) ;
#212187 = CARTESIAN_POINT ( 'NONE',  ( 18.59999999999999076, 64.25000000001176659, -78.17310748452439384 ) ) ;
#212189 = ADVANCED_FACE ( 'NONE', ( #66560 ), #223529, .T. ) ;
#212188 = CARTESIAN_POINT ( 'NONE',  ( -16.92778301347288661, 30.29959772668862783, -234.7992129936043284 ) ) ;
#212190 = EDGE_LOOP ( 'NONE', ( #56543, #238652, #96866, #226907 ) ) ;
#212192 = CARTESIAN_POINT ( 'NONE',  ( -22.59999999999999787, 1.115600667400684642E-11, -100.5000000000000284 ) ) ;
#212191 = FACE_OUTER_BOUND ( 'NONE', #125700, .T. ) ;
#212193 = ADVANCED_FACE ( 'NONE', ( #49559 ), #225595, .F. ) ;
#212194 = ADVANCED_FACE ( 'NONE', ( #129099 ), #111120, .T. ) ;
#212195 = CIRCLE ( 'NONE', #49854, 0.9750000000000036415 ) ;
#212196 = DIRECTION ( 'NONE',  ( 0.000000000000000000, 0.000000000000000000, 1.000000000000000000 ) ) ;
#212197 = FACE_OUTER_BOUND ( 'NONE', #180242, .T. ) ;
#212198 = FACE_OUTER_BOUND ( 'NONE', #36385, .T. ) ;
#212199 = CIRCLE ( 'NONE', #116507, 0.1999999999999945155 ) ;
#212200 = ORIENTED_EDGE ( 'NONE', *, *, #3119, .F. ) ;
#212201 = VERTEX_POINT ( 'NONE', #208650 ) ;
#212202 = EDGE_CURVE ( 'NONE', #142261, #148565, #256810, .T. ) ;
#212203 = CARTESIAN_POINT ( 'NONE',  ( -21.05000000000000071, 0.03175835306687004034, -127.7411528769171980 ) ) ;
#212204 = DIRECTION ( 'NONE',  ( -1.000000000000000000, -0.000000000000000000, 0.000000000000000000 ) ) ;
#212205 = ORIENTED_EDGE ( 'NONE', *, *, #34136, .F. ) ;
#212206 = DIRECTION ( 'NONE',  ( 1.000000000000000000, 0.000000000000000000, 0.000000000000000000 ) ) ;
#212207 = VERTEX_POINT ( 'NONE', #178388 ) ;
#212208 = CARTESIAN_POINT ( 'NONE',  ( -20.85000000000000142, 6.846123162363745074, -70.73772626684986164 ) ) ;
#212209 = CARTESIAN_POINT ( 'NONE',  ( -20.64999999999999858, 71.65000000001187175, -90.67310748452433700 ) ) ;
#212210 = EDGE_CURVE ( 'NONE', #41069, #87179, #107017, .T. ) ;
#212211 = AXIS2_PLACEMENT_3D ( 'NONE', #209991, #52175, #50876 ) ;
#212212 = AXIS2_PLACEMENT_3D ( 'NONE', #141730, #197854, #136587 ) ;
#212213 = FACE_OUTER_BOUND ( 'NONE', #25191, .T. ) ;
#212214 = VERTEX_POINT ( 'NONE', #136650 ) ;
#212215 = FACE_OUTER_BOUND ( 'NONE', #106698, .T. ) ;
#212217 = ORIENTED_EDGE ( 'NONE', *, *, #197516, .T. ) ;
#212216 = AXIS2_PLACEMENT_3D ( 'NONE', #59197, #537, #175370 ) ;
#212218 = ORIENTED_EDGE ( 'NONE', *, *, #94389, .F. ) ;
#212219 = AXIS2_PLACEMENT_3D ( 'NONE', #60909, #84275, #161323 ) ;
#212220 = AXIS2_PLACEMENT_3D ( 'NONE', #124039, #21104, #23675 ) ;
#212221 = EDGE_LOOP ( 'NONE', ( #4246, #233305, #241940, #241361 ) ) ;
#212222 = AXIS2_PLACEMENT_3D ( 'NONE', #19424, #216323, #199352 ) ;
#212223 = CARTESIAN_POINT ( 'NONE',  ( -21.05000000000000071, 16.52766025697963315, -240.8672687545768270 ) ) ;
#212224 = CARTESIAN_POINT ( 'NONE',  ( 13.43443725621852991, 66.55344247693902560, -54.43316553017851334 ) ) ;
#212225 = CARTESIAN_POINT ( 'NONE',  ( 22.39999999999999503, 64.35000000001213039, -136.6231074845243825 ) ) ;
#212226 = CARTESIAN_POINT ( 'NONE',  ( 20.94999999999999929, 82.20113918088273408, -215.0418453737790401 ) ) ;
#212227 = LINE ( 'NONE', #188787, #213345 ) ;
#212228 = AXIS2_PLACEMENT_3D ( 'NONE', #232732, #170229, #228867 ) ;
#212230 = CARTESIAN_POINT ( 'NONE',  ( 21.05995757104869526, 8.775389244721274906, -12.19490512299120866 ) ) ;
#212229 = CARTESIAN_POINT ( 'NONE',  ( -21.00023020733437562, 10.14655627732183873, -228.0991803899404431 ) ) ;
#212232 = ORIENTED_EDGE ( 'NONE', *, *, #136026, .T. ) ;
#212231 = DIRECTION ( 'NONE',  ( -0.000000000000000000, 0.000000000000000000, -1.000000000000000000 ) ) ;
#212233 = CARTESIAN_POINT ( 'NONE',  ( -21.12642695952773764, 10.05219176827227123, -228.0658859103580767 ) ) ;
#212234 = ORIENTED_EDGE ( 'NONE', *, *, #107408, .T. ) ;
#212235 = CARTESIAN_POINT ( 'NONE',  ( -13.43673303185029688, 9.446648990640015953, -149.0891632959232140 ) ) ;
#212236 = EDGE_LOOP ( 'NONE', ( #131586, #39006, #26100, #58366 ) ) ;
#212237 = ORIENTED_EDGE ( 'NONE', *, *, #19359, .T. ) ;
#212238 = CARTESIAN_POINT ( 'NONE',  ( -20.54999999999999716, 2.000000000011154189, -87.27537807723794572 ) ) ;
#212239 = CARTESIAN_POINT ( 'NONE',  ( -16.94062896051973865, 9.992719105111833144, -46.10251654211879924 ) ) ;
#212240 = CARTESIAN_POINT ( 'NONE',  ( -16.94275863006528482, 66.01050395134400617, -48.63141010244781626 ) ) ;
#212241 = CARTESIAN_POINT ( 'NONE',  ( 20.95083306685154056, 8.916842641901356004, -75.47732485325839491 ) ) ;
#212242 = AXIS2_PLACEMENT_3D ( 'NONE', #5727, #27921, #222205 ) ;
#212243 = DIRECTION ( 'NONE',  ( 1.000000000000000000, 0.000000000000000000, 0.000000000000000000 ) ) ;
#212244 = ORIENTED_EDGE ( 'NONE', *, *, #32282, .T. ) ;
#212245 = EDGE_LOOP ( 'NONE', ( #83393, #168106, #105933, #221724 ) ) ;
#212246 = CARTESIAN_POINT ( 'NONE',  ( 0.8999999999999993561, -11.75000000000000000, 23.30000000000000426 ) ) ;
#212247 = ORIENTED_EDGE ( 'NONE', *, *, #195541, .T. ) ;
#212248 = DIRECTION ( 'NONE',  ( 0.000000000000000000, 0.000000000000000000, -1.000000000000000000 ) ) ;
#212249 = CARTESIAN_POINT ( 'NONE',  ( -18.59999999999999787, 64.35000000001234355, -163.0083017138704236 ) ) ;
#212250 = VERTEX_POINT ( 'NONE', #154975 ) ;
#212251 = DIRECTION ( 'NONE',  ( -0.000000000000000000, -0.8660254037844411501, -0.4999999999999956701 ) ) ;
#212252 = FACE_OUTER_BOUND ( 'NONE', #235796, .T. ) ;
#212253 = CARTESIAN_POINT ( 'NONE',  ( -16.87372397896795562, 9.880599536652891146, -120.8507245100358176 ) ) ;
#212254 = LINE ( 'NONE', #33650, #175859 ) ;
#212255 = ORIENTED_EDGE ( 'NONE', *, *, #189177, .F. ) ;
#212256 = VECTOR ( 'NONE', #247324, 1000.000000000000000 ) ;
#212257 = DIRECTION ( 'NONE',  ( 0.000000000000000000, 0.9623856809447771665, 0.2716869542551821892 ) ) ;
#212258 = EDGE_CURVE ( 'NONE', #62371, #138714, #2778, .T. ) ;
#212259 = CARTESIAN_POINT ( 'NONE',  ( -20.54999999999999716, 85.00000000001159606, -59.62913836187181715 ) ) ;
#212260 = AXIS2_PLACEMENT_3D ( 'NONE', #166478, #7367, #186009 ) ;
#212261 = CARTESIAN_POINT ( 'NONE',  ( 22.39999999999999503, 11.65000000001116298, -100.6000000000000369 ) ) ;
#212262 = EDGE_CURVE ( 'NONE', #92669, #78944, #174570, .T. ) ;
#212263 = VECTOR ( 'NONE', #38087, 1000.000000000000000 ) ;
#212264 = VERTEX_POINT ( 'NONE', #235755 ) ;
#212265 = ADVANCED_FACE ( 'NONE', ( #55808 ), #114544, .T. ) ;
#212266 = ADVANCED_FACE ( 'NONE', ( #113253 ), #194097, .T. ) ;
#212267 = EDGE_LOOP ( 'NONE', ( #109861, #219224, #183365, #87491 ) ) ;
#212268 = CARTESIAN_POINT ( 'NONE',  ( -22.39999999999999858, 7.790779598384560245, -67.00000000000004263 ) ) ;
#212269 = CARTESIAN_POINT ( 'NONE',  ( -16.93826681692523195, 14.23933697485878902, -219.3352725080944481 ) ) ;
#212270 = DIRECTION ( 'NONE',  ( 0.000000000000000000, 0.9908441862701596881, -0.1350103645451904977 ) ) ;
#212271 = CARTESIAN_POINT ( 'NONE',  ( 21.14999999999999503, 76.00000000001237765, -170.0231074845243597 ) ) ;
#212272 = DIRECTION ( 'NONE',  ( 0.000000000000000000, -0.4721928772777334582, -0.8814952561688437216 ) ) ;
#212273 = DIRECTION ( 'NONE',  ( 0.000000000000000000, 0.2617529984165030688, 0.9651348961777157509 ) ) ;
#212274 = CIRCLE ( 'NONE', #95709, 0.9000000000000014655 ) ;
#212275 = ORIENTED_EDGE ( 'NONE', *, *, #70773, .T. ) ;
#212276 = CARTESIAN_POINT ( 'NONE',  ( -16.94180778212363236, 66.00755694427991216, -123.9189239139911223 ) ) ;
#212277 = AXIS2_PLACEMENT_3D ( 'NONE', #198006, #218847, #156360 ) ;
#212278 = LINE ( 'NONE', #136550, #210709 ) ;
#212279 = DIRECTION ( 'NONE',  ( 0.000000000000000000, -0.000000000000000000, -1.000000000000000000 ) ) ;
#212280 = PLANE ( 'NONE',  #75730 ) ;
#212281 = AXIS2_PLACEMENT_3D ( 'NONE', #78089, #21997, #20718 ) ;
#212282 = FACE_OUTER_BOUND ( 'NONE', #90323, .T. ) ;
#212283 = EDGE_CURVE ( 'NONE', #114552, #221948, #117111, .T. ) ;
#212284 = EDGE_CURVE ( 'NONE', #189559, #141625, #206800, .T. ) ;
#212285 = VERTEX_POINT ( 'NONE', #212374 ) ;
#212286 = ORIENTED_EDGE ( 'NONE', *, *, #124284, .F. ) ;
#212287 = CARTESIAN_POINT ( 'NONE',  ( -20.85000000000000142, 68.97833521811233481, -166.1895420826271277 ) ) ;
#212288 = DIRECTION ( 'NONE',  ( 1.000000000000000000, 3.190570557967288949E-16, 6.948722487160392945E-17 ) ) ;
#212289 = DIRECTION ( 'NONE',  ( 0.000000000000000000, 0.000000000000000000, 1.000000000000000000 ) ) ;
#212290 = FACE_OUTER_BOUND ( 'NONE', #178483, .T. ) ;
#212291 = CARTESIAN_POINT ( 'NONE',  ( -37.88850191057539973, -9.849999999999990763, 31.39999999999999858 ) ) ;
#212292 = VERTEX_POINT ( 'NONE', #195384 ) ;
#212293 = DIRECTION ( 'NONE',  ( 0.000000000000000000, 0.000000000000000000, -1.000000000000000000 ) ) ;
#212294 = DIRECTION ( 'NONE',  ( 0.000000000000000000, 0.3042567129660006531, 0.9525900758537875213 ) ) ;
#212295 = EDGE_LOOP ( 'NONE', ( #100200, #178814 ) ) ;
#212296 = PLANE ( 'NONE',  #129652 ) ;
#212297 = ADVANCED_FACE ( 'NONE', ( #192801 ), #211081, .T. ) ;
#212298 = AXIS2_PLACEMENT_3D ( 'NONE', #170386, #33430, #247286 ) ;
#212299 = VECTOR ( 'NONE', #129616, 1000.000000000000000 ) ;
#212300 = DIRECTION ( 'NONE',  ( 1.000000000000000000, -2.952720810173289112E-16, -2.061873921506763405E-30 ) ) ;
#212301 = EDGE_CURVE ( 'NONE', #203779, #190519, #98602, .T. ) ;
#212302 = ORIENTED_EDGE ( 'NONE', *, *, #176246, .T. ) ;
#212303 = DIRECTION ( 'NONE',  ( 1.000000000000000000, -0.000000000000000000, 0.000000000000000000 ) ) ;
#212304 = ORIENTED_EDGE ( 'NONE', *, *, #163064, .F. ) ;
#212305 = DIRECTION ( 'NONE',  ( 1.000000000000000000, 0.000000000000000000, 0.000000000000000000 ) ) ;
#212306 = DIRECTION ( 'NONE',  ( -1.000000000000000000, -2.885090398161910739E-16, -6.283419270304611573E-17 ) ) ;
#212307 = CARTESIAN_POINT ( 'NONE',  ( 21.09551895715267378, 10.62143732717967382, -112.7371246658993726 ) ) ;
#212308 = EDGE_CURVE ( 'NONE', #232010, #8374, #119510, .T. ) ;
#212309 = CARTESIAN_POINT ( 'NONE',  ( 20.94999999999999929, -4.557064143889601127, -233.1584191572127622 ) ) ;
#212310 = CYLINDRICAL_SURFACE ( 'NONE', #94634, 0.09999999999999939493 ) ;
#212311 = CARTESIAN_POINT ( 'NONE',  ( 21.05000000000000071, 4.999999999999997335, -21.09473398108690390 ) ) ;
#212312 = FACE_OUTER_BOUND ( 'NONE', #11066, .T. ) ;
#212313 = DIRECTION ( 'NONE',  ( 0.000000000000000000, 1.000000000000000000, 0.000000000000000000 ) ) ;
#212314 = ADVANCED_FACE ( 'NONE', ( #94966 ), #256554, .F. ) ;
#212316 = DIRECTION ( 'NONE',  ( 0.000000000000000000, -6.240597636138643358E-14, -1.000000000000000000 ) ) ;
#212315 = DIRECTION ( 'NONE',  ( -1.073024830501117725E-15, 6.982962677686266711E-15, -1.000000000000000000 ) ) ;
#212317 = AXIS2_PLACEMENT_3D ( 'NONE', #44909, #162298, #164858 ) ;
#212318 = DIRECTION ( 'NONE',  ( 0.000000000000000000, 2.664535259100316927E-15, 1.000000000000000000 ) ) ;
#212319 = VECTOR ( 'NONE', #68199, 1000.000000000000000 ) ;
#212320 = DIRECTION ( 'NONE',  ( 0.000000000000000000, 0.000000000000000000, 1.000000000000000000 ) ) ;
#212321 = AXIS2_PLACEMENT_3D ( 'NONE', #160993, #59266, #137549 ) ;
#212323 = CARTESIAN_POINT ( 'NONE',  ( 21.00000000000000000, 66.25000000001179501, -81.87310748452438247 ) ) ;
#212322 = VECTOR ( 'NONE', #28486, 1000.000000000000000 ) ;
#212325 = EDGE_CURVE ( 'NONE', #50336, #241487, #236197, .T. ) ;
#212324 = B_SPLINE_CURVE_WITH_KNOTS ( 'NONE', 3,
 ( #169663, #70546, #150076, #229595, #91372, #170952, #118652, #153956, #93924, #159064 ),
 .UNSPECIFIED., .F., .F.,
 ( 4, 3, 3, 4 ),
 ( 0.000000000000000000, 3.394313611811197040E-05, 6.779740500701634262E-05, 0.0001049857339142623287 ),
 .UNSPECIFIED. ) ;
#212326 = ORIENTED_EDGE ( 'NONE', *, *, #82200, .T. ) ;
#212327 = CARTESIAN_POINT ( 'NONE',  ( -18.44232395689901693, -9.552282557050347123, -40.34225198480720564 ) ) ;
#212328 = CARTESIAN_POINT ( 'NONE',  ( 21.04999999999999716, 10.62872031401550466, -79.15000000000004832 ) ) ;
#212329 = CARTESIAN_POINT ( 'NONE',  ( -20.54999999999999716, 2.400000000011155432, -191.1060308773475356 ) ) ;
#212330 = EDGE_CURVE ( 'NONE', #34617, #227159, #137932, .T. ) ;
#212331 = AXIS2_PLACEMENT_3D ( 'NONE', #22093, #202002, #123754 ) ;
#212332 = CARTESIAN_POINT ( 'NONE',  ( -20.64999999999999858, -8.999999999988844479, -57.60603087734755690 ) ) ;
#212333 = CARTESIAN_POINT ( 'NONE',  ( -20.64999999999999858, 21.30332930069722863, -233.2143729774842882 ) ) ;
#212334 = APPLICATION_CONTEXT ( 'automotive_design' ) ;
#212335 = EDGE_CURVE ( 'NONE', #31369, #87279, #93691, .T. ) ;
#212336 = ORIENTED_EDGE ( 'NONE', *, *, #176979, .T. ) ;
#212338 = CIRCLE ( 'NONE', #37360, 0.09999999999998898659 ) ;
#212337 = FACE_OUTER_BOUND ( 'NONE', #170751, .T. ) ;
#212339 = EDGE_CURVE ( 'NONE', #22805, #72701, #197913, .T. ) ;
#212340 = VERTEX_POINT ( 'NONE', #254034 ) ;
#212341 = CARTESIAN_POINT ( 'NONE',  ( -18.59999999999999787, 66.65000000001259650, -191.3731074845244393 ) ) ;
#212342 = CARTESIAN_POINT ( 'NONE',  ( -20.64999999999999858, 1.115600667400684642E-11, -169.4000000000000625 ) ) ;
#212343 = B_SPLINE_CURVE_WITH_KNOTS ( 'NONE', 3,
 ( #217352, #235642, #136533, #23053, #216077, #257723, #175705, #116995, #17878, #97390, #20478, #157441, #255156, #218640, #236936, #122133 ),
 .UNSPECIFIED., .F., .F.,
 ( 4, 3, 3, 3, 3, 4 ),
 ( 0.000000000000000000, 2.209075297427991918E-05, 5.594258369009683308E-05, 8.979524372340886272E-05, 0.0001236472815274528567, 0.0001574990747609496733 ),
 .UNSPECIFIED. ) ;
#212344 = CIRCLE ( 'NONE', #16520, 0.1000000000000028644 ) ;
#212345 = ORIENTED_EDGE ( 'NONE', *, *, #84935, .F. ) ;
#212346 = DIRECTION ( 'NONE',  ( -1.000000000000000000, 0.000000000000000000, 0.000000000000000000 ) ) ;
#212347 = EDGE_CURVE ( 'NONE', #244838, #45673, #15463, .T. ) ;
#212348 =( BOUNDED_SURFACE ( )  B_SPLINE_SURFACE ( 3, 2, ( 
 ( #16, #78265, #176123 ),
 ( #157865, #216502, #196934 ),
 ( #18305, #177413, #138230 ),
 ( #39181, #118712, #198221 ) ),
 .UNSPECIFIED., .F., .F., .F. ) 
 B_SPLINE_SURFACE_WITH_KNOTS ( ( 4, 4 ),
 ( 3, 3 ),
 ( 0.000000000000000000, 0.001979672783031562362 ),
 ( 0.000000000000000000, 1.000000000000000000 ),
 .UNSPECIFIED. ) 
 GEOMETRIC_REPRESENTATION_ITEM ( )  RATIONAL_B_SPLINE_SURFACE ( (
 ( 1.000000000000000000, 0.7103081912008196719, 1.000000000000000000),
 ( 1.000000000000000000, 0.7104998333558631973, 1.000000000000000000),
 ( 1.000000000000000000, 0.7107238315755253222, 1.000000000000000000),
 ( 1.000000000000000000, 0.7110073749539376209, 1.000000000000000000) ) ) 
 REPRESENTATION_ITEM ( '' )  SURFACE ( )  );
#212349 = ORIENTED_EDGE ( 'NONE', *, *, #49037, .F. ) ;
#212350 = DIRECTION ( 'NONE',  ( -1.000000000000000000, 0.000000000000000000, 0.000000000000000000 ) ) ;
#212351 = CARTESIAN_POINT ( 'NONE',  ( 21.09546886439513713, 67.12144688699748940, -124.2860136339693611 ) ) ;
#212353 = DIRECTION ( 'NONE',  ( -1.000000000000000000, 0.000000000000000000, 0.000000000000000000 ) ) ;
#212352 = PRODUCT_DEFINITION_CONTEXT ( 'detailed design', #2476, 'design' ) ;
#212354 = CARTESIAN_POINT ( 'NONE',  ( 22.39999999999999503, 7.790779598373379855, 0.000000000000000000 ) ) ;
#212355 = CARTESIAN_POINT ( 'NONE',  ( -16.80100426158790228, 9.943150520396139669, -12.68294575283405479 ) ) ;
#212356 = CARTESIAN_POINT ( 'NONE',  ( 20.85000000000000142, 42.96960653111219131, -254.4772109693542745 ) ) ;
#212357 = DIRECTION ( 'NONE',  ( -1.000000000000000000, -0.000000000000000000, -0.000000000000000000 ) ) ;
#212358 = CYLINDRICAL_SURFACE ( 'NONE', #187166, 0.1000000000000124678 ) ;
#212359 = ORIENTED_EDGE ( 'NONE', *, *, #137671, .T. ) ;
#212361 = DIRECTION ( 'NONE',  ( 2.952720810173289112E-16, -1.000000000000000000, 0.000000000000000000 ) ) ;
#212360 = DIRECTION ( 'NONE',  ( 0.000000000000000000, 0.2617529984165180013, 0.9651348961777117541 ) ) ;
#212362 = VERTEX_POINT ( 'NONE', #199217 ) ;
#212364 = EDGE_LOOP ( 'NONE', ( #198177, #169460, #569, #51833 ) ) ;
#212363 = CARTESIAN_POINT ( 'NONE',  ( -23.25000000000000000, 1.115600667400684642E-11, -134.0000000000000284 ) ) ;
#212365 = AXIS2_PLACEMENT_3D ( 'NONE', #57075, #234443, #140475 ) ;
#212366 = EDGE_LOOP ( 'NONE', ( #3004, #145363, #186257, #120523 ) ) ;
#212367 = CARTESIAN_POINT ( 'NONE',  ( -21.05000000000000071, 76.00000000001267608, -203.5231074845243597 ) ) ;
#212368 = SPHERICAL_SURFACE ( 'NONE', #176156, 0.1000000000000000056 ) ;
#212369 = DIRECTION ( 'NONE',  ( 1.000000000000000000, 0.000000000000000000, 0.000000000000000000 ) ) ;
#212370 = DIRECTION ( 'NONE',  ( -1.000000000000000000, -0.000000000000000000, -0.000000000000000000 ) ) ;
#212371 = VECTOR ( 'NONE', #108300, 1000.000000000000000 ) ;
#212372 = DIRECTION ( 'NONE',  ( 0.000000000000000000, 0.000000000000000000, 1.000000000000000000 ) ) ;
#212373 = DIRECTION ( 'NONE',  ( 0.000000000000000000, 0.000000000000000000, 1.000000000000000000 ) ) ;
#212374 = CARTESIAN_POINT ( 'NONE',  ( 18.59999999999996945, 10.33248238083634440, -139.5948465439131780 ) ) ;
#212375 = DIRECTION ( 'NONE',  ( 0.000000000000000000, 0.7397890806274345366, 0.6728388485992877754 ) ) ;
#212376 = ORIENTED_EDGE ( 'NONE', *, *, #212642, .F. ) ;
#212377 = ORIENTED_EDGE ( 'NONE', *, *, #60726, .F. ) ;
#212378 = CARTESIAN_POINT ( 'NONE',  ( 23.14999999999999858, 70.40000000001229807, -157.6178414656113205 ) ) ;
#212379 = AXIS2_PLACEMENT_3D ( 'NONE', #31151, #72832, #248878 ) ;
#212380 = EDGE_LOOP ( 'NONE', ( #36470, #169756, #226629, #212552 ) ) ;
#212381 = FACE_OUTER_BOUND ( 'NONE', #234767, .T. ) ;
#212383 = EDGE_LOOP ( 'NONE', ( #126385, #203828, #245233, #250599 ) ) ;
#212382 = CIRCLE ( 'NONE', #116675, 0.1000000000000076522 ) ;
#212384 = MECHANICAL_DESIGN_GEOMETRIC_PRESENTATION_REPRESENTATION (  '', ( #108331 ), #99905 ) ;
#212385 = DIRECTION ( 'NONE',  ( -0.000000000000000000, -6.982962677686266711E-15, 1.000000000000000000 ) ) ;
#212386 = FACE_OUTER_BOUND ( 'NONE', #206360, .T. ) ;
#212387 = EDGE_CURVE ( 'NONE', #156376, #256436, #86322, .T. ) ;
#212388 = DIRECTION ( 'NONE',  ( -0.000000000000000000, -1.000000000000000000, -1.734723475976757554E-14 ) ) ;
#212389 = DIRECTION ( 'NONE',  ( 0.000000000000000000, -0.8814952561688429444, 0.4721928772777349570 ) ) ;
#212390 = ORIENTED_EDGE ( 'NONE', *, *, #146302, .F. ) ;
#212391 = CIRCLE ( 'NONE', #24960, 0.1999999999999987899 ) ;
#212393 = AXIS2_PLACEMENT_3D ( 'NONE', #185377, #208799, #109676 ) ;
#212392 = CARTESIAN_POINT ( 'NONE',  ( -18.33682934331473291, -9.511185591082572444, -207.9056547686734575 ) ) ;
#212394 = ADVANCED_FACE ( 'NONE', ( #139204 ), #177951, .F. ) ;
#212395 = EDGE_CURVE ( 'NONE', #197595, #147011, #204324, .T. ) ;
#212396 = LINE ( 'NONE', #113278, #152188 ) ;
#212397 = DIRECTION ( 'NONE',  ( -1.000000000000000000, 0.000000000000000000, 0.000000000000000000 ) ) ;
#212398 = DIRECTION ( 'NONE',  ( 4.239556034732056743E-17, -0.1298341882520022694, -0.9915357197604852679 ) ) ;
#212399 = ORIENTED_EDGE ( 'NONE', *, *, #61779, .T. ) ;
#212401 = PLANE ( 'NONE',  #73455 ) ;
#212400 = DIRECTION ( 'NONE',  ( -1.000000000000000000, 0.000000000000000000, 0.000000000000000000 ) ) ;
#212402 = VERTEX_POINT ( 'NONE', #223884 ) ;
#212405 = ORIENTED_EDGE ( 'NONE', *, *, #159680, .T. ) ;
#212404 = CARTESIAN_POINT ( 'NONE',  ( 23.24999999999999289, 11.65000000001116298, -79.15000000000004832 ) ) ;
#212403 = DIRECTION ( 'NONE',  ( 0.000000000000000000, 0.4721928772777346239, 0.8814952561688430555 ) ) ;
#212406 = AXIS2_PLACEMENT_3D ( 'NONE', #22079, #232464, #212884 ) ;
#212407 = CARTESIAN_POINT ( 'NONE',  ( 23.14999999999999503, 66.34920340998563404, -213.7018660128499334 ) ) ;
#212408 = CIRCLE ( 'NONE', #99918, 0.1000000000000029060 ) ;
#212409 = CIRCLE ( 'NONE', #70765, 0.5000000000000004441 ) ;
#212410 = CIRCLE ( 'NONE', #199758, 0.4000000000000033529 ) ;
#212411 = DIRECTION ( 'NONE',  ( 0.000000000000000000, -0.1568667991644714932, 0.9876197685951274563 ) ) ;
#212412 = ORIENTED_EDGE ( 'NONE', *, *, #150224, .T. ) ;
#212413 = CARTESIAN_POINT ( 'NONE',  ( -20.64999999999999858, -8.663551401858004652, -110.0241011180673354 ) ) ;
#212414 = EDGE_CURVE ( 'NONE', #216736, #138911, #165487, .T. ) ;
#212415 = CIRCLE ( 'NONE', #186906, 0.1000000000000018374 ) ;
#212416 = FACE_OUTER_BOUND ( 'NONE', #137678, .T. ) ;
#212417 = CARTESIAN_POINT ( 'NONE',  ( 18.39999999999999503, 70.35000000001201670, -115.6731074845243370 ) ) ;
#212419 = EDGE_LOOP ( 'NONE', ( #86371, #27411, #254309, #138481 ) ) ;
#212418 = DIRECTION ( 'NONE',  ( -0.000000000000000000, 6.982962677686266711E-15, -1.000000000000000000 ) ) ;
#212420 = ORIENTED_EDGE ( 'NONE', *, *, #242240, .F. ) ;
#212421 = CARTESIAN_POINT ( 'NONE',  ( -17.78241384942104020, 10.85557575279232800, -110.7490376724656187 ) ) ;
#212422 = LINE ( 'NONE', #175866, #74343 ) ;
#212423 = DIRECTION ( 'NONE',  ( 0.000000000000000000, -0.1350103645451876666, -0.9908441862701600211 ) ) ;
#212424 = DIRECTION ( 'NONE',  ( -1.000000000000000000, 0.000000000000000000, 0.000000000000000000 ) ) ;
#212425 = ORIENTED_EDGE ( 'NONE', *, *, #209381, .F. ) ;
#212426 = DIRECTION ( 'NONE',  ( 7.589415207398576792E-15, -0.9770955615653316162, -0.2128009952263604232 ) ) ;
#212427 = EDGE_CURVE ( 'NONE', #238502, #137554, #28122, .T. ) ;
#212428 = CARTESIAN_POINT ( 'NONE',  ( -23.15000000000000213, -0.8618440306552707098, -197.0427629756619297 ) ) ;
#212429 = DIRECTION ( 'NONE',  ( 0.000000000000000000, 0.000000000000000000, 1.000000000000000000 ) ) ;
#212430 = EDGE_CURVE ( 'NONE', #252282, #52715, #120983, .T. ) ;
#212431 = VERTEX_POINT ( 'NONE', #161378 ) ;
#212432 = DIRECTION ( 'NONE',  ( -1.000000000000000000, 0.000000000000000000, -0.000000000000000000 ) ) ;
#212433 = AXIS2_PLACEMENT_3D ( 'NONE', #225829, #165917, #108485 ) ;
#212434 = DIRECTION ( 'NONE',  ( 1.000000000000000000, -7.304098846218163263E-16, 4.217023435051626718E-16 ) ) ;
#212436 = ADVANCED_FACE ( 'NONE', ( #200494 ), #102905, .F. ) ;
#212435 = ORIENTED_EDGE ( 'NONE', *, *, #126774, .F. ) ;
#212437 = CARTESIAN_POINT ( 'NONE',  ( -20.54999999999999716, 47.57365439703043108, -242.5355162900727919 ) ) ;
#212438 = DIRECTION ( 'NONE',  ( 0.000000000000000000, 0.9126074666063545004, 0.4088369013363783999 ) ) ;
#212439 = VECTOR ( 'NONE', #230852, 1000.000000000000000 ) ;
#212440 = ORIENTED_EDGE ( 'NONE', *, *, #232779, .F. ) ;
#212441 = EDGE_LOOP ( 'NONE', ( #57181, #229820, #204680, #197988 ) ) ;
#212442 =( BOUNDED_CURVE ( )  B_SPLINE_CURVE ( 3, ( #223736, #146751, #183357, #45118 ),
 .UNSPECIFIED., .F., .F. ) 
 B_SPLINE_CURVE_WITH_KNOTS ( ( 4, 4 ),
 ( 3.432212674861196522, 3.693332928900581624 ),
 .UNSPECIFIED. ) 
 CURVE ( )  GEOMETRIC_REPRESENTATION_ITEM ( )  RATIONAL_B_SPLINE_CURVE ( ( 1.000000000000000000, 0.9943260843901261525, 0.9943260843901261525, 1.000000000000000000 ) ) 
 REPRESENTATION_ITEM ( '' )  );
#212443 = CARTESIAN_POINT ( 'NONE',  ( 20.94999999999999574, 65.52661458509942349, -162.4444530202758870 ) ) ;
#212444 = ORIENTED_EDGE ( 'NONE', *, *, #71590, .F. ) ;
#212446 = ORIENTED_EDGE ( 'NONE', *, *, #44938, .T. ) ;
#212445 = DIRECTION ( 'NONE',  ( 0.000000000000000000, 0.9875102702516490583, 0.1575546449569643070 ) ) ;
#212447 = CIRCLE ( 'NONE', #29309, 12.97499999999999964 ) ;
#212451 = EDGE_CURVE ( 'NONE', #54600, #114424, #107195, .T. ) ;
#212450 = ORIENTED_EDGE ( 'NONE', *, *, #30707, .F. ) ;
#212449 = ORIENTED_EDGE ( 'NONE', *, *, #220128, .F. ) ;
#212448 = DIRECTION ( 'NONE',  ( 1.000000000000000000, 0.000000000000000000, -0.000000000000000000 ) ) ;
#212452 = AXIS2_PLACEMENT_3D ( 'NONE', #190012, #93461, #89608 ) ;
#212453 = DIRECTION ( 'NONE',  ( 0.000000000000000000, -8.881784197001252323E-16, 1.000000000000000000 ) ) ;
#212454 = ORIENTED_EDGE ( 'NONE', *, *, #35057, .F. ) ;
#212455 = DIRECTION ( 'NONE',  ( -1.000000000000000000, 0.000000000000000000, 0.000000000000000000 ) ) ;
#212456 = DIRECTION ( 'NONE',  ( 1.000000000000000000, -2.952720810173289112E-16, -2.061873921506763405E-30 ) ) ;
#212457 = AXIS2_PLACEMENT_3D ( 'NONE', #112460, #188129, #227244 ) ;
#212458 = CARTESIAN_POINT ( 'NONE',  ( -18.50000000000000000, 43.18640298906419162, -245.2812653309023574 ) ) ;
#212459 = LINE ( 'NONE', #114624, #76414 ) ;
#212460 = CARTESIAN_POINT ( 'NONE',  ( -22.39999999999999858, 25.93539162822980160, -254.3551732743586626 ) ) ;
#212461 = EDGE_LOOP ( 'NONE', ( #162203, #116449, #5929, #26127 ) ) ;
#212462 = ORIENTED_EDGE ( 'NONE', *, *, #29607, .F. ) ;
#212463 = ORIENTED_EDGE ( 'NONE', *, *, #74632, .T. ) ;
#212464 = EDGE_CURVE ( 'NONE', #14621, #198491, #237455, .T. ) ;
#212465 = CARTESIAN_POINT ( 'NONE',  ( -18.59999999999999787, 9.350000000000001421, -12.25000000000000000 ) ) ;
#212467 = ORIENTED_EDGE ( 'NONE', *, *, #246644, .T. ) ;
#212466 = CARTESIAN_POINT ( 'NONE',  ( -18.59999999999999787, -1.736257131586239844, -179.0686523290174819 ) ) ;
#212468 = CARTESIAN_POINT ( 'NONE',  ( 20.94999999999999929, 84.66355140188075268, -59.99900636645695329 ) ) ;
#212469 = EDGE_LOOP ( 'NONE', ( #54906, #14325, #143776 ) ) ;
#212470 = ORIENTED_EDGE ( 'NONE', *, *, #158388, .T. ) ;
#212471 = CARTESIAN_POINT ( 'NONE',  ( -18.45140287520618472, -0.7268611856809952254, -242.2397737697636444 ) ) ;
#212472 = EDGE_CURVE ( 'NONE', #194417, #176716, #6120, .T. ) ;
#212473 = EDGE_CURVE ( 'NONE', #225681, #125503, #143064, .T. ) ;
#212474 = VERTEX_POINT ( 'NONE', #218751 ) ;
#212475 = AXIS2_PLACEMENT_3D ( 'NONE', #55612, #218550, #201569 ) ;
#212476 = CARTESIAN_POINT ( 'NONE',  ( -33.72168855820451938, 9.950000000011156587, -54.35000000000005826 ) ) ;
#212477 = CARTESIAN_POINT ( 'NONE',  ( 20.94999999999999929, 82.22731448072437388, -214.9453318841612486 ) ) ;
#212478 = ADVANCED_FACE ( 'NONE', ( #42697 ), #40165, .F. ) ;
#212480 = ORIENTED_EDGE ( 'NONE', *, *, #119070, .F. ) ;
#212479 = ORIENTED_EDGE ( 'NONE', *, *, #57928, .T. ) ;
#212481 = ORIENTED_EDGE ( 'NONE', *, *, #184204, .T. ) ;
#212483 = ADVANCED_FACE ( 'NONE', ( #2270 ), #122244, .T. ) ;
#212482 = DIRECTION ( 'NONE',  ( -1.000000000000000000, 0.000000000000000000, -0.000000000000000000 ) ) ;
#212484 = ORIENTED_EDGE ( 'NONE', *, *, #171350, .F. ) ;
#212485 = EDGE_LOOP ( 'NONE', ( #206103, #191876, #250447, #121694, #184580 ) ) ;
#212486 = CARTESIAN_POINT ( 'NONE',  ( 19.58285714285715073, 65.61500148966121060, -195.8934228171345069 ) ) ;
#212488 = EDGE_LOOP ( 'NONE', ( #139981, #99207, #85728, #48129, #63097 ) ) ;
#212487 = CARTESIAN_POINT ( 'NONE',  ( 23.50000000000005684, 85.84984265665381997, -47.78991727088349251 ) ) ;
#212489 = DIRECTION ( 'NONE',  ( 1.000000000000000000, -2.952720810173289112E-16, -2.061873921506763405E-30 ) ) ;
#212490 = EDGE_CURVE ( 'NONE', #179904, #16905, #161198, .T. ) ;
#212492 = DIRECTION ( 'NONE',  ( 0.000000000000000000, -6.467318590049456648E-15, 1.000000000000000000 ) ) ;
#212491 = DIRECTION ( 'NONE',  ( -1.000000000000000000, -0.000000000000000000, -0.000000000000000000 ) ) ;
#212493 = DIRECTION ( 'NONE',  ( 0.000000000000000000, 0.4088369013363281623, -0.9126074666063771490 ) ) ;
#212494 = SPHERICAL_SURFACE ( 'NONE', #2868, 0.1000000000000000056 ) ;
#212495 = VERTEX_POINT ( 'NONE', #222591 ) ;
#212496 = ORIENTED_EDGE ( 'NONE', *, *, #217389, .T. ) ;
#212497 = CARTESIAN_POINT ( 'NONE',  ( 21.05000000000000071, 5.000000000011153745, -155.0947339810869323 ) ) ;
#212499 = CIRCLE ( 'NONE', #41637, 0.1000000000000042799 ) ;
#212498 = CARTESIAN_POINT ( 'NONE',  ( -21.04999999999999716, 76.08574093704558550, -142.9369337733372447 ) ) ;
#212501 = EDGE_CURVE ( 'NONE', #156710, #72605, #2953, .T. ) ;
#212500 = FACE_OUTER_BOUND ( 'NONE', #192910, .T. ) ;
#212502 = AXIS2_PLACEMENT_3D ( 'NONE', #217953, #161884, #238830 ) ;
#212503 = CIRCLE ( 'NONE', #237429, 0.8750000000000007772 ) ;
#212504 = AXIS2_PLACEMENT_3D ( 'NONE', #47994, #127543, #247485 ) ;
#212505 = ORIENTED_EDGE ( 'NONE', *, *, #231841, .F. ) ;
#212506 = CARTESIAN_POINT ( 'NONE',  ( 20.94999999999999574, 71.93512633425886804, -225.1442869522136334 ) ) ;
#212507 = ADVANCED_FACE ( 'NONE', ( #103925 ), #40613, .F. ) ;
#212508 = ADVANCED_FACE ( 'NONE', ( #84334 ), #226443, .F. ) ;
#212509 = DIRECTION ( 'NONE',  ( 0.000000000000000000, -1.000000000000000000, 0.000000000000000000 ) ) ;
#212510 = VECTOR ( 'NONE', #178614, 1000.000000000000000 ) ;
#212511 = CARTESIAN_POINT ( 'NONE',  ( -18.59999999999999787, 74.16465844978819177, -191.8679561919614116 ) ) ;
#212512 = ORIENTED_EDGE ( 'NONE', *, *, #183782, .T. ) ;
#212513 = ORIENTED_EDGE ( 'NONE', *, *, #199238, .F. ) ;
#212514 = EDGE_CURVE ( 'NONE', #183226, #10605, #227747, .T. ) ;
#212515 = CARTESIAN_POINT ( 'NONE',  ( 13.40000000000000036, -11.65000000000000036, 15.00000000000000355 ) ) ;
#212516 = DIRECTION ( 'NONE',  ( 1.000000000000000000, 0.000000000000000000, 0.000000000000000000 ) ) ;
#212517 = ORIENTED_EDGE ( 'NONE', *, *, #179597, .F. ) ;
#212518 = CARTESIAN_POINT ( 'NONE',  ( -21.05000000000000071, 74.75000000001159606, -61.52310748452433131 ) ) ;
#212519 = EDGE_LOOP ( 'NONE', ( #78609, #118186, #232771, #147712 ) ) ;
#212520 = DIRECTION ( 'NONE',  ( -2.557131231893036492E-16, 0.9525900758537791946, -0.3042567129660267988 ) ) ;
#212521 = DIRECTION ( 'NONE',  ( 0.000000000000000000, 0.9126074666063768159, 0.4088369013363282178 ) ) ;
#212523 = CYLINDRICAL_SURFACE ( 'NONE', #86721, 0.5000000000000004441 ) ;
#212522 = CARTESIAN_POINT ( 'NONE',  ( -20.94999999999999929, 70.15000000001192859, -92.89061026024637613 ) ) ;
#212524 = EDGE_CURVE ( 'NONE', #205142, #31458, #36310, .T. ) ;
#212525 = CARTESIAN_POINT ( 'NONE',  ( 18.59999999999998721, 69.15387683765929694, -99.28538121767448388 ) ) ;
#212527 = EDGE_CURVE ( 'NONE', #14594, #161400, #219269, .T. ) ;
#212526 = FACE_OUTER_BOUND ( 'NONE', #98017, .T. ) ;
#212528 = AXIS2_PLACEMENT_3D ( 'NONE', #76491, #77765, #56903 ) ;
#212529 = DIRECTION ( 'NONE',  ( 0.000000000000000000, 0.9651348961777160840, -0.2617529984165015700 ) ) ;
#212530 = EDGE_CURVE ( 'NONE', #132241, #100848, #149526, .T. ) ;
#212532 = EDGE_LOOP ( 'NONE', ( #198250, #46620, #42408, #39618, #241625, #49172, #93328, #109296 ) ) ;
#212531 = DIRECTION ( 'NONE',  ( 0.000000000000000000, 0.000000000000000000, -1.000000000000000000 ) ) ;
#212534 = EDGE_LOOP ( 'NONE', ( #190034, #96941, #5206, #86197, #84473 ) ) ;
#212533 = ORIENTED_EDGE ( 'NONE', *, *, #183914, .F. ) ;
#212535 = ORIENTED_EDGE ( 'NONE', *, *, #101421, .F. ) ;
#212536 = CARTESIAN_POINT ( 'NONE',  ( -16.80438519320023261, 60.93976421501079699, -221.0410730170675606 ) ) ;
#212537 = CARTESIAN_POINT ( 'NONE',  ( 18.59999999999999787, 77.85102823015273543, -91.36919421510179973 ) ) ;
#212538 = EDGE_CURVE ( 'NONE', #127173, #87867, #132157, .T. ) ;
#212540 = CARTESIAN_POINT ( 'NONE',  ( 21.05000000000000071, 76.00000000001213607, -136.5231074845242745 ) ) ;
#212539 = CARTESIAN_POINT ( 'NONE',  ( -16.79140778683511215, 66.05505840115797866, -182.6933702507536452 ) ) ;
#212541 = CARTESIAN_POINT ( 'NONE',  ( 20.94999999999999929, -11.64999999998883595, -200.9999999999999432 ) ) ;
#212542 = ORIENTED_EDGE ( 'NONE', *, *, #54382, .T. ) ;
#212543 = DIRECTION ( 'NONE',  ( 0.000000000000000000, 1.000000000000000000, 6.982962677686266711E-15 ) ) ;
#212544 = ORIENTED_EDGE ( 'NONE', *, *, #248052, .T. ) ;
#212545 = ORIENTED_EDGE ( 'NONE', *, *, #5645, .F. ) ;
#212546 = DIRECTION ( 'NONE',  ( 0.000000000000000000, -0.9887567792719351711, 0.1495327102803594987 ) ) ;
#212547 = CARTESIAN_POINT ( 'NONE',  ( -16.97683809663752186, 13.99889777621145903, -218.5199410132753144 ) ) ;
#212548 = CARTESIAN_POINT ( 'NONE',  ( 20.94999999999999574, 1.115600667400684642E-11, -100.5000000000000284 ) ) ;
#212549 = AXIS2_PLACEMENT_3D ( 'NONE', #52633, #209140, #91773 ) ;
#212550 = DIRECTION ( 'NONE',  ( -0.000000000000000000, 0.8490545835447252943, 0.5283051335749947564 ) ) ;
#212551 = CARTESIAN_POINT ( 'NONE',  ( 22.39999999999999503, 68.20922040163900135, -170.0231074845243882 ) ) ;
#212552 = ORIENTED_EDGE ( 'NONE', *, *, #5630, .T. ) ;
#212553 = EDGE_LOOP ( 'NONE', ( #206538, #226185, #127865, #205774 ) ) ;
#212554 = CARTESIAN_POINT ( 'NONE',  ( -16.92973740335360233, 9.992503814478528312, -54.40605903520227571 ) ) ;
#212555 = AXIS2_PLACEMENT_3D ( 'NONE', #5648, #82609, #205140 ) ;
#212556 = DIRECTION ( 'NONE',  ( -1.000000000000000000, 3.469446951953635015E-14, 0.000000000000000000 ) ) ;
#212557 = DIRECTION ( 'NONE',  ( -1.836970198721029934E-16, -1.000000000000000000, -6.982962677686266711E-15 ) ) ;
#212558 = CARTESIAN_POINT ( 'NONE',  ( 6.000000000000060396, 64.65000000001120384, -26.02310748452479316 ) ) ;
#212559 = CARTESIAN_POINT ( 'NONE',  ( -16.90138253750126651, 9.950000000011137047, -188.2115627079045339 ) ) ;
#212560 = CARTESIAN_POINT ( 'NONE',  ( 18.59999999999999076, 74.83412143252222393, -233.7087995678629966 ) ) ;
#212561 = CARTESIAN_POINT ( 'NONE',  ( -21.00023020733438273, 6.390869245278866018, -33.50000000000000711 ) ) ;
#212563 = CARTESIAN_POINT ( 'NONE',  ( 20.94999999999999929, -8.999999999988842703, -157.6060308773475640 ) ) ;
#212562 = CARTESIAN_POINT ( 'NONE',  ( -20.54999999999999716, 74.00000000001180922, -82.74772940728641402 ) ) ;
#212564 = CARTESIAN_POINT ( 'NONE',  ( 21.05000000000000071, -1.249999999988843369, -41.40000000000000568 ) ) ;
#212565 = CARTESIAN_POINT ( 'NONE',  ( 20.85000000000000142, 7.788796164756791818, -245.4641525896719543 ) ) ;
#212566 = EDGE_CURVE ( 'NONE', #183612, #134457, #190446, .T. ) ;
#212567 = DIRECTION ( 'NONE',  ( 0.000000000000000000, 0.000000000000000000, -1.000000000000000000 ) ) ;
#212568 = CARTESIAN_POINT ( 'NONE',  ( -21.05000000000000071, 87.48912529308798014, -106.1231074845242262 ) ) ;
#212569 = CIRCLE ( 'NONE', #141793, 0.09999999999999939493 ) ;
#212571 = ORIENTED_EDGE ( 'NONE', *, *, #142449, .T. ) ;
#212570 = DIRECTION ( 'NONE',  ( -0.000000000000000000, 6.982962677686266711E-15, -1.000000000000000000 ) ) ;
#212572 = EDGE_CURVE ( 'NONE', #203112, #190086, #47810, .T. ) ;
#212573 = AXIS2_PLACEMENT_3D ( 'NONE', #205586, #26996, #106473 ) ;
#212574 = TOROIDAL_SURFACE ( 'NONE', #233428, 0.2000000000000000111, 0.1000000000000000056 ) ;
#212575 = CARTESIAN_POINT ( 'NONE',  ( -21.05000000000000071, 87.48912529308852015, -173.1231074845242688 ) ) ;
#212576 = AXIS2_PLACEMENT_3D ( 'NONE', #99333, #74708, #253286 ) ;
#212577 = AXIS2_PLACEMENT_3D ( 'NONE', #238625, #258106, #221598 ) ;
#212578 = CARTESIAN_POINT ( 'NONE',  ( 22.49806830649814060, 11.64988965485023620, -100.4225356836745249 ) ) ;
#212579 = ADVANCED_FACE ( 'NONE', ( #244731 ), #223710, .F. ) ;
#212580 = CARTESIAN_POINT ( 'NONE',  ( -23.25000000000000000, 54.35515994658447880, -237.0760575614320089 ) ) ;
#212581 = FACE_OUTER_BOUND ( 'NONE', #202668, .T. ) ;
#212582 = CIRCLE ( 'NONE', #4450, 7.720710678118678061 ) ;
#212583 = FACE_OUTER_BOUND ( 'NONE', #155765, .T. ) ;
#212584 = CIRCLE ( 'NONE', #100110, 0.1999999999999996503 ) ;
#212585 = AXIS2_PLACEMENT_3D ( 'NONE', #121189, #3771, #22069 ) ;
#212586 = CARTESIAN_POINT ( 'NONE',  ( 18.53691006697099652, 10.30215155715038122, -24.70219871729854333 ) ) ;
#212587 = DIRECTION ( 'NONE',  ( -0.000000000000000000, -0.000000000000000000, -1.000000000000000000 ) ) ;
#212588 = VECTOR ( 'NONE', #78748, 1000.000000000000000 ) ;
#212589 = TOROIDAL_SURFACE ( 'NONE', #62552, 11.65000000000000036, 0.1000000000000000056 ) ;
#212590 = ORIENTED_EDGE ( 'NONE', *, *, #238665, .T. ) ;
#212591 = DIRECTION ( 'NONE',  ( 0.000000000000000000, -1.776356839400189131E-15, 1.000000000000000000 ) ) ;
#212593 = ORIENTED_EDGE ( 'NONE', *, *, #81811, .T. ) ;
#212592 = DIRECTION ( 'NONE',  ( -1.000000000000000000, 0.000000000000000000, 0.000000000000000000 ) ) ;
#212594 = LINE ( 'NONE', #135589, #50737 ) ;
#212595 = CARTESIAN_POINT ( 'NONE',  ( -22.50000000000000000, 31.80488924422932584, -238.9605610896540213 ) ) ;
#212596 = ORIENTED_EDGE ( 'NONE', *, *, #162483, .F. ) ;
#212597 = CARTESIAN_POINT ( 'NONE',  ( 20.94999999999999929, -8.663551401857999323, -90.97589888193273566 ) ) ;
#212598 = SHAPE_DEFINITION_REPRESENTATION ( #165904, #90142 ) ;
#212599 = AXIS2_PLACEMENT_3D ( 'NONE', #95690, #155711, #56542 ) ;
#212600 = CARTESIAN_POINT ( 'NONE',  ( -18.59999999999999787, 64.35000000001190301, -96.00830171387039513 ) ) ;
#212601 = CARTESIAN_POINT ( 'NONE',  ( -18.50000000000000355, 85.40000000001187175, -95.72584772486095517 ) ) ;
#212602 = ORIENTED_EDGE ( 'NONE', *, *, #75310, .F. ) ;
#212603 = DIRECTION ( 'NONE',  ( -1.000000000000000000, -0.000000000000000000, -0.000000000000000000 ) ) ;
#212604 = CYLINDRICAL_SURFACE ( 'NONE', #229913, 0.09999999999999939493 ) ;
#212605 = CARTESIAN_POINT ( 'NONE',  ( -21.05000000000000071, 86.30329675166747450, -209.4258251677035787 ) ) ;
#212606 = ORIENTED_EDGE ( 'NONE', *, *, #86285, .T. ) ;
#212607 = ORIENTED_EDGE ( 'NONE', *, *, #90289, .F. ) ;
#212608 = DIRECTION ( 'NONE',  ( 0.000000000000000000, 0.000000000000000000, -1.000000000000000000 ) ) ;
#212609 = EDGE_CURVE ( 'NONE', #971, #67224, #188621, .T. ) ;
#212610 = AXIS2_PLACEMENT_3D ( 'NONE', #84724, #88595, #103029 ) ;
#212611 = DIRECTION ( 'NONE',  ( 0.000000000000000000, 0.9875102702516471709, 0.1575546449569757979 ) ) ;
#212612 = DIRECTION ( 'NONE',  ( 0.000000000000000000, -0.9651348961777157509, 0.2617529984165031243 ) ) ;
#212613 = CARTESIAN_POINT ( 'NONE',  ( -17.01764560440508944, 30.11817903520203288, -234.7598257174429648 ) ) ;
#212614 = CIRCLE ( 'NONE', #170962, 0.8750000000000007772 ) ;
#212615 = EDGE_CURVE ( 'NONE', #192558, #257053, #90447, .T. ) ;
#212617 = DIRECTION ( 'NONE',  ( 1.000000000000000000, 0.000000000000000000, 0.000000000000000000 ) ) ;
#212616 = CARTESIAN_POINT ( 'NONE',  ( -18.40000000000000213, 31.05627573922685514, -233.2203535436961488 ) ) ;
#212618 = CARTESIAN_POINT ( 'NONE',  ( -21.08078803292166725, 75.92081401285471998, -176.3561204489614909 ) ) ;
#212619 = CARTESIAN_POINT ( 'NONE',  ( -16.87683809663752399, 54.76195096157953657, -190.8731074845245246 ) ) ;
#212620 = FACE_OUTER_BOUND ( 'NONE', #195895, .T. ) ;
#212621 = DIRECTION ( 'NONE',  ( 0.000000000000000000, 0.000000000000000000, 1.000000000000000000 ) ) ;
#212622 = VERTEX_POINT ( 'NONE', #206909 ) ;
#212623 = AXIS2_PLACEMENT_3D ( 'NONE', #248811, #28517, #71471 ) ;
#212625 = ORIENTED_EDGE ( 'NONE', *, *, #183040, .T. ) ;
#212624 = CARTESIAN_POINT ( 'NONE',  ( 12.30626653967341078, 62.70412490954448259, -216.8009802157223191 ) ) ;
#212626 = CYLINDRICAL_SURFACE ( 'NONE', #243586, 0.09999999999999961697 ) ;
#212627 = CARTESIAN_POINT ( 'NONE',  ( -20.64999999999999858, 61.88149656937975607, -248.1136133839584090 ) ) ;
#212629 = DIRECTION ( 'NONE',  ( -1.000000000000000000, -0.000000000000000000, -0.000000000000000000 ) ) ;
#212628 = DIRECTION ( 'NONE',  ( 0.000000000000000000, 0.9126074666063660468, 0.4088369013363524762 ) ) ;
#212630 = ADVANCED_FACE ( 'NONE', ( #225160 ), #69631, .F. ) ;
#212631 = CIRCLE ( 'NONE', #125145, 0.2000000000000057288 ) ;
#212632 = ORIENTED_EDGE ( 'NONE', *, *, #116633, .F. ) ;
#212633 = DIRECTION ( 'NONE',  ( 0.000000000000000000, 0.000000000000000000, 1.000000000000000000 ) ) ;
#212634 = CARTESIAN_POINT ( 'NONE',  ( -20.94999999999999929, 11.65000000001115232, -194.2161343370218560 ) ) ;
#212635 = CARTESIAN_POINT ( 'NONE',  ( -21.05000000000000071, 69.65527659592170551, -103.0378253410479203 ) ) ;
#212636 = DIRECTION ( 'NONE',  ( 0.000000000000000000, 0.9126074666063660468, 0.4088369013363524762 ) ) ;
#212637 = EDGE_CURVE ( 'NONE', #45717, #207052, #170404, .T. ) ;
#212638 = ORIENTED_EDGE ( 'NONE', *, *, #2199, .T. ) ;
#212639 = ORIENTED_EDGE ( 'NONE', *, *, #57423, .T. ) ;
#212640 = AXIS2_PLACEMENT_3D ( 'NONE', #161838, #150, #202226 ) ;
#212641 = LINE ( 'NONE', #113527, #251148 ) ;
#212642 = EDGE_CURVE ( 'NONE', #24511, #110094, #8712, .T. ) ;
#212643 = EDGE_LOOP ( 'NONE', ( #131315, #146310, #218581, #26168 ) ) ;
#212644 = CARTESIAN_POINT ( 'NONE',  ( -21.55000000000000426, 62.98412863812492901, -221.9071248009556712 ) ) ;
#212645 = AXIS2_PLACEMENT_3D ( 'NONE', #42878, #141966, #20766 ) ;
#212646 =( GEOMETRIC_REPRESENTATION_CONTEXT ( 3 ) GLOBAL_UNCERTAINTY_ASSIGNED_CONTEXT ( ( #44026 ) ) GLOBAL_UNIT_ASSIGNED_CONTEXT ( ( #28463, #224037, #243612 ) ) REPRESENTATION_CONTEXT ( 'NONE', 'WORKASPACE' ) );
#212647 = CARTESIAN_POINT ( 'NONE',  ( 20.85000000000000142, -4.871452838297987142, -233.3782557782877518 ) ) ;
#212648 = CARTESIAN_POINT ( 'NONE',  ( -21.07928932188134041, 65.47931918658504458, -241.9371126717015841 ) ) ;
#212649 = CIRCLE ( 'NONE', #17018, 2.600000000000000089 ) ;
#212650 = ORIENTED_EDGE ( 'NONE', *, *, #90687, .T. ) ;
#212651 = DIRECTION ( 'NONE',  ( 1.000000000000000000, 0.000000000000000000, 0.000000000000000000 ) ) ;
#212652 = EDGE_CURVE ( 'NONE', #170896, #59827, #247306, .T. ) ;
#212653 = DIRECTION ( 'NONE',  ( -0.7071067811865474617, -0.7071067811865474617, -2.044391222244499837E-16 ) ) ;
#212654 = CARTESIAN_POINT ( 'NONE',  ( -22.48660254037843487, 11.65000000001115588, -66.95000000000005969 ) ) ;
#212655 = DIRECTION ( 'NONE',  ( 0.000000000000000000, 0.000000000000000000, -1.000000000000000000 ) ) ;
#212656 = DIRECTION ( 'NONE',  ( 1.000000000000000000, 0.000000000000000000, 0.000000000000000000 ) ) ;
#212658 = CARTESIAN_POINT ( 'NONE',  ( -20.54999999999999716, -9.000000000000003553, -9.393969122652443104 ) ) ;
#212657 = DIRECTION ( 'NONE',  ( -0.000000000000000000, -0.000000000000000000, 1.000000000000000000 ) ) ;
#212659 = AXIS2_PLACEMENT_3D ( 'NONE', #102679, #119720, #45305 ) ;
#212660 = CYLINDRICAL_SURFACE ( 'NONE', #178139, 0.09999999999999939493 ) ;
#212661 = ORIENTED_EDGE ( 'NONE', *, *, #101457, .F. ) ;
#212663 = CARTESIAN_POINT ( 'NONE',  ( -18.59999999999999787, -1.835859311432481045, -179.0044391687985410 ) ) ;
#212662 = DIRECTION ( 'NONE',  ( -1.000000000000000000, -2.952720810173289112E-16, 0.000000000000000000 ) ) ;
#212664 = VERTEX_POINT ( 'NONE', #249886 ) ;
#212666 = EDGE_LOOP ( 'NONE', ( #41826, #24289, #180616, #215301 ) ) ;
#212665 = CARTESIAN_POINT ( 'NONE',  ( -18.40000000000000213, 11.33174054713631662, -180.1499999999999773 ) ) ;
#212667 = ORIENTED_EDGE ( 'NONE', *, *, #178132, .T. ) ;
#212668 = CARTESIAN_POINT ( 'NONE',  ( 22.60000000000000142, 12.58798907299599179, -223.3278890275437050 ) ) ;
#212669 = CARTESIAN_POINT ( 'NONE',  ( 15.57250062127603130, 66.62931007840965947, -152.4966423578634078 ) ) ;
#212670 = CARTESIAN_POINT ( 'NONE',  ( -23.15000000000000213, 76.00000000001267608, -203.5231074845243597 ) ) ;
#212671 = DIRECTION ( 'NONE',  ( 0.000000000000000000, 0.2617529984164915779, 0.9651348961777189706 ) ) ;
#212672 = VERTEX_POINT ( 'NONE', #9992 ) ;
#212673 = CARTESIAN_POINT ( 'NONE',  ( 18.49999999999999289, 10.20857864377385127, -125.1500000000000341 ) ) ;
#212674 = CARTESIAN_POINT ( 'NONE',  ( -20.94999999999999929, 64.25000000001263345, -196.5083017138704236 ) ) ;
#212675 = B_SPLINE_CURVE_WITH_KNOTS ( 'NONE', 3,
 ( #210874, #32264, #130034, #237820, #13970, #248724, #75240, #10111, #113060, #89627, #111783, #70110, #173082, #149640, #133897, #131332 ),
 .UNSPECIFIED., .F., .F.,
 ( 4, 3, 3, 3, 3, 4 ),
 ( 0.000000000000000000, 3.357088238233183250E-05, 6.714213034886279538E-05, 0.0001007408646120870187, 0.0001343627955914160831, 0.0001573956632895967837 ),
 .UNSPECIFIED. ) ;
#212676 = ORIENTED_EDGE ( 'NONE', *, *, #168214, .T. ) ;
#212677 = DIRECTION ( 'NONE',  ( 1.000000000000000000, 0.000000000000000000, -0.000000000000000000 ) ) ;
#212678 = AXIS2_PLACEMENT_3D ( 'NONE', #193108, #14487, #93982 ) ;
#212679 = VECTOR ( 'NONE', #2463, 1000.000000000000000 ) ;
#212681 = AXIS2_PLACEMENT_3D ( 'NONE', #64390, #143910, #223441 ) ;
#212680 = CARTESIAN_POINT ( 'NONE',  ( 21.14250536705908345, 6.518172176880724145, -1.950243336660753025E-16 ) ) ;
#212682 = VERTEX_POINT ( 'NONE', #71273 ) ;
#212683 = CARTESIAN_POINT ( 'NONE',  ( 22.50000000000000000, 1.115600667400684642E-11, -67.00000000000004263 ) ) ;
#212684 = EDGE_CURVE ( 'NONE', #219363, #51801, #32216, .T. ) ;
#212685 = ORIENTED_EDGE ( 'NONE', *, *, #162636, .T. ) ;
#212686 = CIRCLE ( 'NONE', #162611, 12.77499999999999503 ) ;
#212687 = CARTESIAN_POINT ( 'NONE',  ( 23.25000000000000000, -11.74999999998883560, -164.4000000000000057 ) ) ;
#212688 = ORIENTED_EDGE ( 'NONE', *, *, #56243, .T. ) ;
#212689 = CARTESIAN_POINT ( 'NONE',  ( -23.15000000000000213, 2.499999999999998668, -20.27537807723790309 ) ) ;
#212690 = CARTESIAN_POINT ( 'NONE',  ( -20.94999999999999929, 1.115600667400684642E-11, -67.00000000000000000 ) ) ;
#212691 = DIRECTION ( 'NONE',  ( 0.000000000000000000, 0.000000000000000000, -1.000000000000000000 ) ) ;
#212692 = ADVANCED_FACE ( 'NONE', ( #89511 ), #150786, .T. ) ;
#212693 = DIRECTION ( 'NONE',  ( 0.000000000000000000, 0.000000000000000000, 1.000000000000000000 ) ) ;
#212694 = AXIS2_PLACEMENT_3D ( 'NONE', #164487, #24988, #104471 ) ;
#212695 = ADVANCED_FACE ( 'NONE', ( #69990 ), #34714, .F. ) ;
#212696 = ADVANCED_FACE ( 'NONE', ( #55495 ), #118073, .F. ) ;
#212697 = CARTESIAN_POINT ( 'NONE',  ( 23.14999999999999503, 6.450000000011156587, -188.6499999999999488 ) ) ;
#212698 = CARTESIAN_POINT ( 'NONE',  ( 18.39999999999999858, -9.682403433465237796, -73.65684337741279819 ) ) ;
#212699 = CYLINDRICAL_SURFACE ( 'NONE', #184731, 0.09999999999999781286 ) ;
#212700 = VERTEX_POINT ( 'NONE', #73850 ) ;
#212702 = LINE ( 'NONE', #34093, #23182 ) ;
#212701 = CARTESIAN_POINT ( 'NONE',  ( 21.12400247839537926, 22.98976051637114182, -230.0661232092074329 ) ) ;
#212703 = VERTEX_POINT ( 'NONE', #133783 ) ;
#212706 = VERTEX_POINT ( 'NONE', #152097 ) ;
#212705 = DIRECTION ( 'NONE',  ( -3.469446951953529623E-14, -0.9126074666063660468, -0.4088369013363524762 ) ) ;
#212704 = CARTESIAN_POINT ( 'NONE',  ( 23.14999999999999858, 9.374458193048763377, -220.5475659691911119 ) ) ;
#212707 = B_SPLINE_CURVE_WITH_KNOTS ( 'NONE', 3,
 ( #128778, #85749, #187476, #165331, #8825, #148331, #88323, #44099, #242285, #244852, #243579, #46641, #87046, #144452, #167926, #123643 ),
 .UNSPECIFIED., .F., .F.,
 ( 4, 3, 3, 3, 3, 4 ),
 ( 0.000000000000000000, 3.357088238233693503E-05, 6.714213034886854165E-05, 0.0001007408646120936052, 0.0001343627955914235370, 0.0001573956632896016355 ),
 .UNSPECIFIED. ) ;
#212708 = ORIENTED_EDGE ( 'NONE', *, *, #191194, .F. ) ;
#212709 = DIRECTION ( 'NONE',  ( -2.602085213965226419E-14, -0.000000000000000000, 1.000000000000000000 ) ) ;
#212710 = DIRECTION ( 'NONE',  ( 0.000000000000000000, 0.000000000000000000, 1.000000000000000000 ) ) ;
#212711 = CARTESIAN_POINT ( 'NONE',  ( 20.94999999999999929, 76.00000000001213607, -136.5231074845243313 ) ) ;
#212712 = CARTESIAN_POINT ( 'NONE',  ( 20.95568717954149562, 58.98889948345964740, -225.7425766489790533 ) ) ;
#212713 = VERTEX_POINT ( 'NONE', #172961 ) ;
#212715 = VERTEX_POINT ( 'NONE', #114227 ) ;
#212714 = CARTESIAN_POINT ( 'NONE',  ( -16.89268316805465986, 66.04827818676982076, -115.6673550059788340 ) ) ;
#212716 = ADVANCED_FACE ( 'NONE', ( #97178 ), #13848, .F. ) ;
#212717 = AXIS2_PLACEMENT_3D ( 'NONE', #107711, #187273, #86845 ) ;
#212718 = ADVANCED_FACE ( 'NONE', ( #231622 ), #212059, .F. ) ;
#212720 = CARTESIAN_POINT ( 'NONE',  ( 18.49999999999999289, 15.22030141505243428, -222.9130098973476777 ) ) ;
#212719 = DIRECTION ( 'NONE',  ( -1.000000000000000000, 0.000000000000000000, 0.000000000000000000 ) ) ;
#212722 = EDGE_LOOP ( 'NONE', ( #44560, #110075, #223414, #30273 ) ) ;
#212721 = CARTESIAN_POINT ( 'NONE',  ( -18.59999999999999787, -1.164121893230052995, -175.4148480855716059 ) ) ;
#212723 = VECTOR ( 'NONE', #45157, 1000.000000000000000 ) ;
#212724 = EDGE_LOOP ( 'NONE', ( #241613, #183236, #141260, #25288 ) ) ;
#212725 = AXIS2_PLACEMENT_3D ( 'NONE', #174592, #92415, #251491 ) ;
#212726 = CARTESIAN_POINT ( 'NONE',  ( -20.65000000000000568, 70.35000000001153353, -48.67310748452436542 ) ) ;
#212727 = CARTESIAN_POINT ( 'NONE',  ( -21.14999999999999858, 65.51923798433686841, -242.1677427744926092 ) ) ;
#212728 = EDGE_LOOP ( 'NONE', ( #209235, #135032, #200603, #173195 ) ) ;
#212729 = DIRECTION ( 'NONE',  ( 0.000000000000000000, 1.000000000000000000, 0.000000000000000000 ) ) ;
#212730 = ORIENTED_EDGE ( 'NONE', *, *, #137902, .F. ) ;
#212731 = EDGE_CURVE ( 'NONE', #15058, #104983, #17678, .T. ) ;
#212732 = TOROIDAL_SURFACE ( 'NONE', #33698, 0.2000000000000000111, 0.1000000000000000056 ) ;
#212734 = ADVANCED_FACE ( 'NONE', ( #253719 ), #153399, .T. ) ;
#212733 = CARTESIAN_POINT ( 'NONE',  ( -18.35668295345803713, 11.47316190337362940, -158.2500000000000284 ) ) ;
#212735 = CARTESIAN_POINT ( 'NONE',  ( -23.15000000000000213, 76.00000000001267608, -203.5231074845243597 ) ) ;
#212736 = EDGE_CURVE ( 'NONE', #47066, #183282, #136322, .T. ) ;
#212737 = VERTEX_POINT ( 'NONE', #33449 ) ;
#212738 = CARTESIAN_POINT ( 'NONE',  ( 23.25000000000000000, 85.60000000001197407, -112.9170766071766820 ) ) ;
#212739 = AXIS2_PLACEMENT_3D ( 'NONE', #136280, #158473, #59302 ) ;
#212740 = DIRECTION ( 'NONE',  ( 3.265361837132813093E-16, -1.000000000000000000, -0.000000000000000000 ) ) ;
#212741 = VECTOR ( 'NONE', #250517, 1000.000000000000000 ) ;
#212742 = ORIENTED_EDGE ( 'NONE', *, *, #244529, .T. ) ;
#212743 = ORIENTED_EDGE ( 'NONE', *, *, #80848, .F. ) ;
#212744 = CARTESIAN_POINT ( 'NONE',  ( -18.40000000000000213, -9.682403433465244902, -73.65684337741278398 ) ) ;
#212745 = AXIS2_PLACEMENT_3D ( 'NONE', #123760, #62503, #23401 ) ;
#212746 = ORIENTED_EDGE ( 'NONE', *, *, #219530, .F. ) ;
#212747 = LINE ( 'NONE', #131914, #46401 ) ;
#212748 = VERTEX_POINT ( 'NONE', #234163 ) ;
#212750 = ORIENTED_EDGE ( 'NONE', *, *, #180165, .F. ) ;
#212749 = DIRECTION ( 'NONE',  ( 1.000000000000000000, 0.000000000000000000, 0.000000000000000000 ) ) ;
#212751 = AXIS2_PLACEMENT_3D ( 'NONE', #26257, #164482, #182764 ) ;
#212752 = AXIS2_PLACEMENT_3D ( 'NONE', #943, #137909, #256528 ) ;
#212753 = ORIENTED_EDGE ( 'NONE', *, *, #173626, .F. ) ;
#212754 = DIRECTION ( 'NONE',  ( -1.000000000000000000, 0.000000000000000000, -0.000000000000000000 ) ) ;
#212755 = ORIENTED_EDGE ( 'NONE', *, *, #135821, .F. ) ;
#212759 = ADVANCED_FACE ( 'NONE', ( #35991 ), #115575, .F. ) ;
#212758 = ORIENTED_EDGE ( 'NONE', *, *, #181331, .F. ) ;
#212757 = ORIENTED_EDGE ( 'NONE', *, *, #49151, .T. ) ;
#212756 = DIRECTION ( 'NONE',  ( 0.000000000000000000, 0.000000000000000000, -1.000000000000000000 ) ) ;
#212760 = VERTEX_POINT ( 'NONE', #254953 ) ;
#212761 = VECTOR ( 'NONE', #245944, 1000.000000000000000 ) ;
#212762 = AXIS2_PLACEMENT_3D ( 'NONE', #167185, #246672, #32813 ) ;
#212763 = AXIS2_PLACEMENT_3D ( 'NONE', #193974, #216074, #15345 ) ;
#212764 = CIRCLE ( 'NONE', #54332, 11.74999999999999645 ) ;
#212765 = AXIS2_PLACEMENT_3D ( 'NONE', #128863, #208410, #170600 ) ;
#212766 = CARTESIAN_POINT ( 'NONE',  ( 21.13920837816993270, 8.783247050131068434, -45.75000000000000711 ) ) ;
#212767 = EDGE_LOOP ( 'NONE', ( #239705, #234854, #97040, #170113 ) ) ;
#212768 = EDGE_CURVE ( 'NONE', #203718, #166805, #115500, .T. ) ;
#212769 = DIRECTION ( 'NONE',  ( -1.000000000000000000, 0.000000000000000000, 0.000000000000000000 ) ) ;
#212771 = ORIENTED_EDGE ( 'NONE', *, *, #119733, .T. ) ;
#212770 = FACE_OUTER_BOUND ( 'NONE', #179798, .T. ) ;
#212772 = FACE_OUTER_BOUND ( 'NONE', #21512, .T. ) ;
#212773 = ORIENTED_EDGE ( 'NONE', *, *, #152304, .F. ) ;
#212775 = ORIENTED_EDGE ( 'NONE', *, *, #216250, .F. ) ;
#212774 = EDGE_CURVE ( 'NONE', #35062, #182351, #119900, .T. ) ;
#212776 = DIRECTION ( 'NONE',  ( -1.000000000000000000, -0.000000000000000000, 0.000000000000000000 ) ) ;
#212777 = AXIS2_PLACEMENT_3D ( 'NONE', #93780, #254133, #155084 ) ;
#212778 = CARTESIAN_POINT ( 'NONE',  ( -20.94999999999999929, -11.74999999998884448, -36.39999999999999858 ) ) ;
#212779 = ADVANCED_FACE ( 'NONE', ( #196320 ), #176788, .F. ) ;
#212780 = EDGE_LOOP ( 'NONE', ( #217219, #119006, #75991, #135237 ) ) ;
#212781 = EDGE_LOOP ( 'NONE', ( #224028, #86032, #35955, #105544 ) ) ;
#212782 = CARTESIAN_POINT ( 'NONE',  ( 20.94999999999999574, 67.07338541492499928, -128.0514244653012383 ) ) ;
#212783 = ADVANCED_FACE ( 'NONE', ( #236724 ), #217153, .F. ) ;
#212785 = ORIENTED_EDGE ( 'NONE', *, *, #221092, .F. ) ;
#212784 = ORIENTED_EDGE ( 'NONE', *, *, #147138, .T. ) ;
#212786 = ORIENTED_EDGE ( 'NONE', *, *, #165993, .T. ) ;
#212788 = ADVANCED_FACE ( 'NONE', ( #251145 ), #219734, .T. ) ;
#212787 = DIRECTION ( 'NONE',  ( 0.000000000000000000, 0.2280421351061330537, -0.9736512643735621975 ) ) ;
#212789 = EDGE_LOOP ( 'NONE', ( #176935, #193125, #90, #2113 ) ) ;
#212790 = EDGE_LOOP ( 'NONE', ( #71672, #226198, #19257, #225304 ) ) ;
#212791 = CARTESIAN_POINT ( 'NONE',  ( -20.90000000000000213, -1.212568896937008089, -7.900000000000000355 ) ) ;
#212792 = ORIENTED_EDGE ( 'NONE', *, *, #24001, .F. ) ;
#212793 = CARTESIAN_POINT ( 'NONE',  ( 18.59999999999999076, 10.20857864377385127, -91.75000000000005684 ) ) ;
#212794 = B_SPLINE_CURVE_WITH_KNOTS ( 'NONE', 3,
 ( #16425, #157227, #236716, #174237, #41128, #135041, #115494, #38539, #154661, #118067, #238005, #214591, #75124, #200183, #197597, #235433, #138873, #253714, #35982 ),
 .UNSPECIFIED., .F., .F.,
 ( 4, 3, 3, 3, 3, 3, 4 ),
 ( 0.000000000000000000, 2.646747978908405840E-05, 5.271166642128090210E-05, 9.008788829884082239E-05, 0.0001426648776560918196, 0.0001897378458659811703, 0.0001917382627806267395 ),
 .UNSPECIFIED. ) ;
#212795 = CARTESIAN_POINT ( 'NONE',  ( 18.49999999999999289, 11.75000000001115907, -41.60000000000000142 ) ) ;
#212796 = CIRCLE ( 'NONE', #83743, 0.09999999999999939493 ) ;
#212797 = VERTEX_POINT ( 'NONE', #124506 ) ;
#212798 = EDGE_LOOP ( 'NONE', ( #192904, #257658, #17768, #108285 ) ) ;
#212799 = DIRECTION ( 'NONE',  ( -0.000000000000000000, 0.2617529984165031243, 0.9651348961777157509 ) ) ;
#212800 = ORIENTED_EDGE ( 'NONE', *, *, #116414, .T. ) ;
#212801 = EDGE_CURVE ( 'NONE', #120394, #209230, #78918, .T. ) ;
#212802 = EDGE_CURVE ( 'NONE', #178394, #257053, #82759, .T. ) ;
#212803 = TOROIDAL_SURFACE ( 'NONE', #100343, 0.4000000000000005773, 0.1000000000000000056 ) ;
#212804 = DIRECTION ( 'NONE',  ( 0.000000000000000000, -6.982962677686266711E-15, 1.000000000000000000 ) ) ;
#212805 = VERTEX_POINT ( 'NONE', #102326 ) ;
#212806 = ORIENTED_EDGE ( 'NONE', *, *, #139801, .T. ) ;
#212807 = EDGE_CURVE ( 'NONE', #124432, #44347, #28315, .T. ) ;
#212808 = CARTESIAN_POINT ( 'NONE',  ( -18.40000000000000213, 11.74999999999998224, -12.65000000000000213 ) ) ;
#212810 = ORIENTED_EDGE ( 'NONE', *, *, #210822, .T. ) ;
#212809 = CARTESIAN_POINT ( 'NONE',  ( 18.43579564894457690, 85.51932753530486764, -163.0501308406639964 ) ) ;
#212811 = DIRECTION ( 'NONE',  ( 1.000000000000000000, -0.000000000000000000, -0.000000000000000000 ) ) ;
#212812 = DIRECTION ( 'NONE',  ( -1.000000000000000000, 0.000000000000000000, -0.000000000000000000 ) ) ;
#212813 = CARTESIAN_POINT ( 'NONE',  ( 20.95556889135987788, 65.37805641227699027, -128.8807132626668306 ) ) ;
#212814 = CARTESIAN_POINT ( 'NONE',  ( -23.15000000000000213, 84.66355140188093742, -79.04720860259155302 ) ) ;
#212815 = LINE ( 'NONE', #164395, #215395 ) ;
#212816 = DIRECTION ( 'NONE',  ( -0.000000000000000000, 7.109473446599835262E-15, -1.000000000000000000 ) ) ;
#212817 = CYLINDRICAL_SURFACE ( 'NONE', #58051, 0.5000000000000022204 ) ;
#212818 = FACE_OUTER_BOUND ( 'NONE', #149513, .T. ) ;
#212820 = EDGE_CURVE ( 'NONE', #213068, #34846, #207367, .T. ) ;
#212819 = CARTESIAN_POINT ( 'NONE',  ( -21.59780538579341069, 69.15290947006839417, -69.62208615412235702 ) ) ;
#212821 = CARTESIAN_POINT ( 'NONE',  ( 18.52130828395272033, -9.481395502614633486, -74.02450672388368957 ) ) ;
#212822 = CARTESIAN_POINT ( 'NONE',  ( 23.25000000000000000, -11.74999999998883560, -197.8999999999999773 ) ) ;
#212823 = EDGE_CURVE ( 'NONE', #5597, #182327, #218438, .T. ) ;
#212824 = AXIS2_PLACEMENT_3D ( 'NONE', #85813, #31053, #107986 ) ;
#212825 = VERTEX_POINT ( 'NONE', #142755 ) ;
#212826 = AXIS2_PLACEMENT_3D ( 'NONE', #167608, #188425, #25521 ) ;
#212827 = CIRCLE ( 'NONE', #133702, 0.1000000000000001860 ) ;
#212828 = EDGE_CURVE ( 'NONE', #16273, #162055, #174072, .T. ) ;
#212830 = ORIENTED_EDGE ( 'NONE', *, *, #26990, .F. ) ;
#212829 = VERTEX_POINT ( 'NONE', #42392 ) ;
#212831 = VERTEX_POINT ( 'NONE', #240592 ) ;
#212832 = CARTESIAN_POINT ( 'NONE',  ( -21.11101077989000174, 0.01528526892543874242, -94.07631526527390520 ) ) ;
#212833 = CARTESIAN_POINT ( 'NONE',  ( -18.50000000000000000, 64.35000000001174669, -81.27310748452440237 ) ) ;
#212835 = DIRECTION ( 'NONE',  ( 0.000000000000000000, 0.000000000000000000, 1.000000000000000000 ) ) ;
#212834 = CARTESIAN_POINT ( 'NONE',  ( -21.05000000000000071, 77.26178616857710324, -128.4366085209788366 ) ) ;
#212836 = EDGE_CURVE ( 'NONE', #603, #89644, #240661, .T. ) ;
#212837 = ORIENTED_EDGE ( 'NONE', *, *, #236451, .T. ) ;
#212838 = VERTEX_POINT ( 'NONE', #120671 ) ;
#212839 = CARTESIAN_POINT ( 'NONE',  ( -21.14999999999999858, 87.75000000001213607, -136.5231074845242176 ) ) ;
#212841 = AXIS2_PLACEMENT_3D ( 'NONE', #226482, #90830, #110402 ) ;
#212840 = FACE_OUTER_BOUND ( 'NONE', #157415, .T. ) ;
#212842 = DIRECTION ( 'NONE',  ( 1.000000000000000000, -0.000000000000000000, -0.000000000000000000 ) ) ;
#212843 = VERTEX_POINT ( 'NONE', #84031 ) ;
#212844 = VERTEX_POINT ( 'NONE', #101026 ) ;
#212845 = CARTESIAN_POINT ( 'NONE',  ( 22.88900146558018989, 8.703904791123973084, -143.2500000000000284 ) ) ;
#212846 = DIRECTION ( 'NONE',  ( 0.000000000000000000, 0.000000000000000000, -1.000000000000000000 ) ) ;
#212847 = VERTEX_POINT ( 'NONE', #144041 ) ;
#212849 = ORIENTED_EDGE ( 'NONE', *, *, #198556, .T. ) ;
#212848 = CARTESIAN_POINT ( 'NONE',  ( -23.15000000000000213, 54.89227652059045681, -239.1913228807104588 ) ) ;
#212850 = CARTESIAN_POINT ( 'NONE',  ( 18.39999999999999503, 67.17743825834509153, -45.27310748452438816 ) ) ;
#212851 = DIRECTION ( 'NONE',  ( 1.000000000000000000, 2.952720810173289112E-16, -0.000000000000000000 ) ) ;
#212852 = ORIENTED_EDGE ( 'NONE', *, *, #49968, .T. ) ;
#212853 = CARTESIAN_POINT ( 'NONE',  ( 14.88075390448864788, 66.56831044948773979, -84.74381745228832585 ) ) ;
#212854 = DIRECTION ( 'NONE',  ( 0.000000000000000000, -8.881784197001252323E-16, 1.000000000000000000 ) ) ;
#212855 = DIRECTION ( 'NONE',  ( 1.000000000000000000, 0.000000000000000000, 0.000000000000000000 ) ) ;
#212856 = AXIS2_PLACEMENT_3D ( 'NONE', #88183, #47783, #43953 ) ;
#212859 = LINE ( 'NONE', #18510, #37236 ) ;
#212858 = CIRCLE ( 'NONE', #100393, 0.5000000000000004441 ) ;
#212857 = DIRECTION ( 'NONE',  ( 1.000000000000000000, 0.000000000000000000, 0.000000000000000000 ) ) ;
#212861 = DIRECTION ( 'NONE',  ( 0.000000000000000000, -1.000000000000000000, -6.982962677686265922E-15 ) ) ;
#212860 = AXIS2_PLACEMENT_3D ( 'NONE', #184725, #145600, #30827 ) ;
#212862 = CIRCLE ( 'NONE', #100396, 0.1000000000000124678 ) ;
#212863 = CARTESIAN_POINT ( 'NONE',  ( -20.64999999999999858, 74.00000000001223555, -149.7477294072864709 ) ) ;
#212864 = DIRECTION ( 'NONE',  ( 1.000000000000000000, 2.952720810173289112E-16, -0.000000000000000000 ) ) ;
#212865 = DIRECTION ( 'NONE',  ( 0.000000000000000000, -0.4791956752371546169, -0.8777080977375152360 ) ) ;
#212866 = ORIENTED_EDGE ( 'NONE', *, *, #62432, .F. ) ;
#212867 = CIRCLE ( 'NONE', #87755, 0.09999999999999939493 ) ;
#212868 = ORIENTED_EDGE ( 'NONE', *, *, #22766, .F. ) ;
#212869 = EDGE_CURVE ( 'NONE', #27613, #143316, #59347, .T. ) ;
#212870 = CARTESIAN_POINT ( 'NONE',  ( -21.05000000000000071, -1.249999999988843369, -175.4999999999999716 ) ) ;
#212871 = CARTESIAN_POINT ( 'NONE',  ( 21.05000000000000071, 77.25000000001159606, -61.62310748452431142 ) ) ;
#212872 = ORIENTED_EDGE ( 'NONE', *, *, #251868, .F. ) ;
#212873 = DIRECTION ( 'NONE',  ( 0.000000000000000000, 0.000000000000000000, -1.000000000000000000 ) ) ;
#212874 = CIRCLE ( 'NONE', #58715, 2.000000000000001776 ) ;
#212875 = ORIENTED_EDGE ( 'NONE', *, *, #175002, .F. ) ;
#212876 = FILL_AREA_STYLE ('',( #171224 ) ) ;
#212877 = EDGE_CURVE ( 'NONE', #201773, #230992, #138879, .T. ) ;
#212878 = ORIENTED_EDGE ( 'NONE', *, *, #222530, .F. ) ;
#212879 = DIRECTION ( 'NONE',  ( 0.000000000000000000, 0.9126074666063660468, 0.4088369013363524762 ) ) ;
#212880 = ORIENTED_EDGE ( 'NONE', *, *, #179867, .T. ) ;
#212881 = CARTESIAN_POINT ( 'NONE',  ( 21.07946286933444924, 0.07668384326757191061, -161.1709626809922895 ) ) ;
#212882 = FACE_OUTER_BOUND ( 'NONE', #143203, .T. ) ;
#212883 = DIRECTION ( 'NONE',  ( 0.000000000000000000, -1.000000000000000000, 0.000000000000000000 ) ) ;
#212884 = DIRECTION ( 'NONE',  ( 0.000000000000000000, 0.9126074666063769270, 0.4088369013363280513 ) ) ;
#212886 = VERTEX_POINT ( 'NONE', #20275 ) ;
#212885 = CARTESIAN_POINT ( 'NONE',  ( -16.89935556175704079, 29.77468116918558394, -234.5758233140741140 ) ) ;
#212888 = PLANE ( 'NONE',  #216928 ) ;
#212887 = CARTESIAN_POINT ( 'NONE',  ( 21.05000000000000071, 6.108733535351102972, -199.6370801574273628 ) ) ;
#212890 = DIRECTION ( 'NONE',  ( -0.5932847527679309119, 0.3801118060259214282, 0.7095972217059529630 ) ) ;
#212889 = AXIS2_PLACEMENT_3D ( 'NONE', #125072, #122507, #203321 ) ;
#212891 = CARTESIAN_POINT ( 'NONE',  ( 14.77516762759921498, 66.56332574816920555, -121.3462455535251792 ) ) ;
#212892 = CARTESIAN_POINT ( 'NONE',  ( -13.54795643572457919, 9.450668889178686527, -115.5555464902073766 ) ) ;
#212893 = DIRECTION ( 'NONE',  ( 0.000000000000000000, 0.2617529984165031243, 0.9651348961777157509 ) ) ;
#212894 = ORIENTED_EDGE ( 'NONE', *, *, #68943, .T. ) ;
#212895 = AXIS2_PLACEMENT_3D ( 'NONE', #29191, #184350, #166126 ) ;
#212896 = DIRECTION ( 'NONE',  ( -1.000000000000000000, -0.000000000000000000, -0.000000000000000000 ) ) ;
#212897 = ORIENTED_EDGE ( 'NONE', *, *, #202594, .F. ) ;
#212898 = AXIS2_PLACEMENT_3D ( 'NONE', #47828, #64836, #144351 ) ;
#212899 = CARTESIAN_POINT ( 'NONE',  ( 18.59999999999999076, 18.18127959618848166, -237.5711165786817389 ) ) ;
#212900 = ORIENTED_EDGE ( 'NONE', *, *, #51416, .F. ) ;
#212901 = FACE_OUTER_BOUND ( 'NONE', #170813, .T. ) ;
#212902 = AXIS2_PLACEMENT_3D ( 'NONE', #143909, #4395, #39713 ) ;
#212903 = VECTOR ( 'NONE', #239846, 1000.000000000000000 ) ;
#212904 = CYLINDRICAL_SURFACE ( 'NONE', #82458, 0.09999999999999939493 ) ;
#212905 = ORIENTED_EDGE ( 'NONE', *, *, #114913, .F. ) ;
#212906 = ORIENTED_EDGE ( 'NONE', *, *, #71599, .T. ) ;
#212907 = AXIS2_PLACEMENT_3D ( 'NONE', #199012, #174366, #234275 ) ;
#212908 = DIRECTION ( 'NONE',  ( 1.000000000000000000, -0.000000000000000000, -0.000000000000000000 ) ) ;
#212909 = DIRECTION ( 'NONE',  ( 0.000000000000000000, 0.000000000000000000, 1.000000000000000000 ) ) ;
#212910 = CARTESIAN_POINT ( 'NONE',  ( 20.94403535211772294, 65.69367753730709580, -164.5189238066348594 ) ) ;
#212911 = CARTESIAN_POINT ( 'NONE',  ( -16.92570016628985385, 66.04121104227199623, -90.40245681448537596 ) ) ;
#212912 = EDGE_CURVE ( 'NONE', #203031, #156064, #223890, .T. ) ;
#212914 = CARTESIAN_POINT ( 'NONE',  ( 18.49999999999999289, 10.20857864377384239, -158.7671572875253787 ) ) ;
#212913 = DIRECTION ( 'NONE',  ( -0.000000000000000000, -0.8814952561688430555, 0.4721928772777346239 ) ) ;
#212915 = CARTESIAN_POINT ( 'NONE',  ( -20.54999999999999716, 30.27561093622783517, -235.5248193094124645 ) ) ;
#212917 = CARTESIAN_POINT ( 'NONE',  ( 23.14999999999999858, 79.86053958472213310, -204.5701194781909180 ) ) ;
#212916 = CIRCLE ( 'NONE', #125607, 0.09999999999999939493 ) ;
#212918 = ORIENTED_EDGE ( 'NONE', *, *, #120850, .T. ) ;
#212919 = DIRECTION ( 'NONE',  ( 0.000000000000000000, 0.9126074666063769270, 0.4088369013363282733 ) ) ;
#212921 = ORIENTED_EDGE ( 'NONE', *, *, #229825, .F. ) ;
#212920 = DIRECTION ( 'NONE',  ( 0.000000000000000000, 0.000000000000000000, -1.000000000000000000 ) ) ;
#212922 = CARTESIAN_POINT ( 'NONE',  ( 20.95132126680579887, 65.51005012986584575, -195.9527829460899113 ) ) ;
#212923 = CARTESIAN_POINT ( 'NONE',  ( 18.57071067811864040, 65.82071067813119214, -182.1731074845244223 ) ) ;
#212925 = DIRECTION ( 'NONE',  ( 0.000000000000000000, 0.000000000000000000, -1.000000000000000000 ) ) ;
#212924 = FACE_OUTER_BOUND ( 'NONE', #253724, .T. ) ;
#212926 = AXIS2_PLACEMENT_3D ( 'NONE', #112852, #192391, #172874 ) ;
#212927 = EDGE_CURVE ( 'NONE', #235108, #162078, #248867, .T. ) ;
#212929 = ORIENTED_EDGE ( 'NONE', *, *, #118732, .F. ) ;
#212928 = CARTESIAN_POINT ( 'NONE',  ( -14.87779219673427811, 62.11640146696787923, -218.6859212199907745 ) ) ;
#212930 = LINE ( 'NONE', #94252, #55152 ) ;
#212931 = DIRECTION ( 'NONE',  ( 0.000000000000000000, -1.000000000000000000, 0.000000000000000000 ) ) ;
#212932 = DIRECTION ( 'NONE',  ( -0.000000000000000000, -0.000000000000000000, -1.000000000000000000 ) ) ;
#212933 = CARTESIAN_POINT ( 'NONE',  ( -16.94107738177415712, 65.98576071487524075, -90.47310748452437679 ) ) ;
#212935 = CARTESIAN_POINT ( 'NONE',  ( -18.52643265882458579, 10.31973158071402530, -139.5505334713354841 ) ) ;
#212934 = AXIS2_PLACEMENT_3D ( 'NONE', #37257, #17656, #97157 ) ;
#212936 = ADVANCED_FACE ( 'NONE', ( #198894 ), #5909, .T. ) ;
#212937 = ORIENTED_EDGE ( 'NONE', *, *, #188632, .F. ) ;
#212938 = DIRECTION ( 'NONE',  ( 0.000000000000000000, 0.000000000000000000, -1.000000000000000000 ) ) ;
#212939 = VERTEX_POINT ( 'NONE', #70975 ) ;
#212940 = CARTESIAN_POINT ( 'NONE',  ( -17.11825945287482753, 65.95000000001188312, -90.37310748452436826 ) ) ;
#212941 = EDGE_CURVE ( 'NONE', #143163, #142060, #15842, .T. ) ;
#212942 = ORIENTED_EDGE ( 'NONE', *, *, #95603, .F. ) ;
#212943 = AXIS2_PLACEMENT_3D ( 'NONE', #58037, #217110, #77596 ) ;
#212944 = CIRCLE ( 'NONE', #217006, 0.1999999999999987899 ) ;
#212945 = AXIS2_PLACEMENT_3D ( 'NONE', #12461, #91972, #231503 ) ;
#212946 = ORIENTED_EDGE ( 'NONE', *, *, #59171, .F. ) ;
#212947 = VECTOR ( 'NONE', #53226, 1000.000000000000000 ) ;
#212948 = DIRECTION ( 'NONE',  ( 0.000000000000000000, 1.000000000000000000, 7.272083257015735086E-15 ) ) ;
#212949 = CYLINDRICAL_SURFACE ( 'NONE', #245754, 2.000000000000001776 ) ;
#212950 = CARTESIAN_POINT ( 'NONE',  ( 18.59999999999999432, 77.16270174994961906, -61.52310748452431710 ) ) ;
#212951 = ORIENTED_EDGE ( 'NONE', *, *, #125358, .T. ) ;
#212952 = EDGE_CURVE ( 'NONE', #243017, #11996, #107377, .T. ) ;
#212953 = CYLINDRICAL_SURFACE ( 'NONE', #79552, 1.749999999999998002 ) ;
#212954 = CARTESIAN_POINT ( 'NONE',  ( 23.14999999999999858, 70.10000000001177511, -79.74220724918072278 ) ) ;
#212955 = CARTESIAN_POINT ( 'NONE',  ( -22.01447462590972748, 7.076351764553705515, -199.3574874748654224 ) ) ;
#212956 = DIRECTION ( 'NONE',  ( -0.000000000000000000, 0.7280513885559045661, -0.6855225566105168644 ) ) ;
#212957 = CARTESIAN_POINT ( 'NONE',  ( -21.14999999999999858, 11.75000000001115552, -67.00000000000004263 ) ) ;
#212958 = ORIENTED_EDGE ( 'NONE', *, *, #216856, .F. ) ;
#212959 = CARTESIAN_POINT ( 'NONE',  ( -18.41817142474038960, 85.49870306661419761, -129.9191419968872765 ) ) ;
#212960 = ORIENTED_EDGE ( 'NONE', *, *, #4507, .T. ) ;
#212962 = ORIENTED_EDGE ( 'NONE', *, *, #242280, .T. ) ;
#212961 = CARTESIAN_POINT ( 'NONE',  ( 21.07964655665547582, 67.22511038503330383, -90.80119090156031803 ) ) ;
#212963 = VERTEX_POINT ( 'NONE', #205298 ) ;
#212964 = DIRECTION ( 'NONE',  ( 0.000000000000000000, 0.2617529984165031243, 0.9651348961777157509 ) ) ;
#212965 = DIRECTION ( 'NONE',  ( -1.000000000000000000, -8.673617379884087537E-15, 0.000000000000000000 ) ) ;
#212966 = CARTESIAN_POINT ( 'NONE',  ( -23.15000000000000213, 34.80778438379478246, -248.5595576589601592 ) ) ;
#212967 = CARTESIAN_POINT ( 'NONE',  ( -23.15000000000000213, 76.00000000001244871, -170.0231074845243597 ) ) ;
#212968 = ORIENTED_EDGE ( 'NONE', *, *, #132156, .T. ) ;
#212969 = DIRECTION ( 'NONE',  ( -1.000000000000000000, 2.952720810173289112E-16, 2.061873921506763405E-30 ) ) ;
#212970 = DIRECTION ( 'NONE',  ( 2.342056488767301376E-15, -0.1350103645451904977, -0.9908441862701596881 ) ) ;
#212972 = EDGE_LOOP ( 'NONE', ( #90726, #126588, #62352, #205176, #256424, #219780, #226923, #5602, #134722, #84293, #77371, #244262, #74608, #252420, #197022, #111068, #61252, #115826 ) ) ;
#212971 = CIRCLE ( 'NONE', #154727, 0.09999999999999363565 ) ;
#212973 = EDGE_CURVE ( 'NONE', #14418, #242494, #90620, .T. ) ;
#212975 = ORIENTED_EDGE ( 'NONE', *, *, #69470, .T. ) ;
#212974 = DIRECTION ( 'NONE',  ( -0.000000000000000000, -0.2617529984165030132, -0.9651348961777158619 ) ) ;
#212976 = CARTESIAN_POINT ( 'NONE',  ( -18.50000000000000000, 69.15387683765909799, -65.78538121767449809 ) ) ;
#212977 = DIRECTION ( 'NONE',  ( -1.000000000000000000, 0.000000000000000000, -0.000000000000000000 ) ) ;
#212978 = CARTESIAN_POINT ( 'NONE',  ( 21.05000000000000071, 64.35000000001237197, -170.0231074845244166 ) ) ;
#212979 = EDGE_LOOP ( 'NONE', ( #108663, #229462, #34860, #176506, #57153 ) ) ;
#212980 = DIRECTION ( 'NONE',  ( -1.000000000000000000, 0.000000000000000000, 0.000000000000000000 ) ) ;
#212981 = EDGE_CURVE ( 'NONE', #139309, #46709, #148914, .T. ) ;
#212982 = CARTESIAN_POINT ( 'NONE',  ( 21.14999999999999858, 69.45000000001229523, -157.8731074845244109 ) ) ;
#212983 = EDGE_LOOP ( 'NONE', ( #41866, #234193, #35545, #37029 ) ) ;
#212984 = CARTESIAN_POINT ( 'NONE',  ( 23.24999999999999289, 59.07123845373075000, -221.0531397865252075 ) ) ;
#212985 = DIRECTION ( 'NONE',  ( 0.000000000000000000, -0.5283051335750404975, 0.8490545835446967615 ) ) ;
#212986 = EDGE_CURVE ( 'NONE', #79677, #34477, #103089, .T. ) ;
#212987 = DIRECTION ( 'NONE',  ( -1.000000000000000000, 0.000000000000000000, -0.000000000000000000 ) ) ;
#212988 = ADVANCED_FACE ( 'NONE', ( #227438 ), #7103, .T. ) ;
#212989 = AXIS2_PLACEMENT_3D ( 'NONE', #187233, #129798, #86805 ) ;
#212990 = AXIS2_PLACEMENT_3D ( 'NONE', #199998, #40947, #99572 ) ;
#212992 = ORIENTED_EDGE ( 'NONE', *, *, #64401, .F. ) ;
#212991 = AXIS2_PLACEMENT_3D ( 'NONE', #100340, #166798, #114154 ) ;
#212993 = CARTESIAN_POINT ( 'NONE',  ( 21.05000000000000071, 8.876614585098254295, -75.38508047884472774 ) ) ;
#212994 = VERTEX_POINT ( 'NONE', #206600 ) ;
#212995 = CARTESIAN_POINT ( 'NONE',  ( -20.94999999999994600, 65.19115966511134275, -29.92310748452479174 ) ) ;
#212996 = CARTESIAN_POINT ( 'NONE',  ( 18.59999999999996945, 10.33248238083634440, -173.0948465439131496 ) ) ;
#212999 = EDGE_CURVE ( 'NONE', #25605, #148456, #128059, .T. ) ;
#212998 = ORIENTED_EDGE ( 'NONE', *, *, #207075, .T. ) ;
#212997 = CARTESIAN_POINT ( 'NONE',  ( 21.09551895715245706, 10.62143732718000244, -146.2371246658989890 ) ) ;
#213000 = CARTESIAN_POINT ( 'NONE',  ( 21.05000000000000071, -11.38316329222461754, -203.4791315943886048 ) ) ;
#213001 = DIRECTION ( 'NONE',  ( 1.836970198721029934E-16, -1.000000000000000000, -0.000000000000000000 ) ) ;
#213002 = DIRECTION ( 'NONE',  ( 0.000000000000000000, -6.661338147750933721E-15, 1.000000000000000000 ) ) ;
#213003 = CARTESIAN_POINT ( 'NONE',  ( -16.89021194854740315, 9.949999999999981526, -20.74256813160433666 ) ) ;
#213004 = DIRECTION ( 'NONE',  ( -0.8049926720990042694, 0.5932847527679310229, 4.142885285818786163E-15 ) ) ;
#213005 = EDGE_CURVE ( 'NONE', #202492, #211140, #228750, .T. ) ;
#213006 = DIRECTION ( 'NONE',  ( -1.000000000000000000, 0.000000000000000000, 0.000000000000000000 ) ) ;
#213007 = ADVANCED_FACE ( 'NONE', ( #107494 ), #187064, .F. ) ;
#213008 = DIRECTION ( 'NONE',  ( 0.000000000000000000, 0.000000000000000000, -1.000000000000000000 ) ) ;
#213010 = ORIENTED_EDGE ( 'NONE', *, *, #204717, .T. ) ;
#213009 = DIRECTION ( 'NONE',  ( 0.000000000000000000, 0.000000000000000000, -1.000000000000000000 ) ) ;
#213011 = CIRCLE ( 'NONE', #100549, 0.09999999999999939493 ) ;
#213013 = ADVANCED_FACE ( 'NONE', ( #29292 ), #198961, .F. ) ;
#213012 = CARTESIAN_POINT ( 'NONE',  ( 22.39999999999999503, 68.20922040163929978, -203.6231074845244109 ) ) ;
#213015 = ADVANCED_FACE ( 'NONE', ( #188320 ), #161386, .F. ) ;
#213014 = CARTESIAN_POINT ( 'NONE',  ( -18.59999999999999787, 85.48068669529106955, -129.5819923157664562 ) ) ;
#213016 = CARTESIAN_POINT ( 'NONE',  ( 18.59999999999999432, 77.29973367124280514, -112.9949779616549108 ) ) ;
#213017 = EDGE_CURVE ( 'NONE', #51613, #84837, #194727, .T. ) ;
#213018 = ORIENTED_EDGE ( 'NONE', *, *, #235606, .F. ) ;
#213019 = FACE_OUTER_BOUND ( 'NONE', #150262, .T. ) ;
#213020 = TOROIDAL_SURFACE ( 'NONE', #34004, 0.4000000000000012990, 0.1000000000000000056 ) ;
#213021 = AXIS2_PLACEMENT_3D ( 'NONE', #82979, #162577, #223800 ) ;
#213022 = CYLINDRICAL_SURFACE ( 'NONE', #122861, 0.1000000000000101918 ) ;
#213023 = CARTESIAN_POINT ( 'NONE',  ( 22.47071067811865319, 1.115600667400684642E-11, -67.00000000000004263 ) ) ;
#213024 = CIRCLE ( 'NONE', #92216, 0.1000000000000028644 ) ;
#213025 = VERTEX_POINT ( 'NONE', #16131 ) ;
#213026 = DIRECTION ( 'NONE',  ( 0.000000000000000000, 0.2128009952263606730, -0.9770955615653313941 ) ) ;
#213027 = CARTESIAN_POINT ( 'NONE',  ( -16.94445028196808778, 9.992063609708889516, -79.60733017841850767 ) ) ;
#213028 = ORIENTED_EDGE ( 'NONE', *, *, #70820, .F. ) ;
#213029 = DIRECTION ( 'NONE',  ( 1.000000000000000000, 0.000000000000000000, 0.000000000000000000 ) ) ;
#213030 = EDGE_CURVE ( 'NONE', #156620, #9837, #203054, .T. ) ;
#213031 = VERTEX_POINT ( 'NONE', #213014 ) ;
#213032 = EDGE_CURVE ( 'NONE', #43685, #997, #236389, .T. ) ;
#213034 = EDGE_LOOP ( 'NONE', ( #15941, #74302, #170134, #170341 ) ) ;
#213033 = CARTESIAN_POINT ( 'NONE',  ( 23.14999999999999858, 67.23127455305835554, -235.8551265064784559 ) ) ;
#213035 = AXIS2_PLACEMENT_3D ( 'NONE', #57022, #75366, #32395 ) ;
#213036 = CARTESIAN_POINT ( 'NONE',  ( 23.24999999999999289, 52.81534179157632991, -244.1198638051726277 ) ) ;
#213037 = ORIENTED_EDGE ( 'NONE', *, *, #125107, .F. ) ;
#213038 = FACE_OUTER_BOUND ( 'NONE', #70477, .T. ) ;
#213039 = ORIENTED_EDGE ( 'NONE', *, *, #15550, .F. ) ;
#213042 = EDGE_CURVE ( 'NONE', #219381, #45344, #140711, .T. ) ;
#213041 = ORIENTED_EDGE ( 'NONE', *, *, #159690, .F. ) ;
#213040 = ORIENTED_EDGE ( 'NONE', *, *, #29094, .F. ) ;
#213043 = DIRECTION ( 'NONE',  ( 2.465190328815661345E-32, -0.8814952561688430555, 0.4721928772777344574 ) ) ;
#213045 = ORIENTED_EDGE ( 'NONE', *, *, #147066, .F. ) ;
#213044 = LINE ( 'NONE', #52676, #9835 ) ;
#213046 = DIRECTION ( 'NONE',  ( 1.000000000000000000, 0.000000000000000000, -0.000000000000000000 ) ) ;
#213047 = ORIENTED_EDGE ( 'NONE', *, *, #201474, .T. ) ;
#213048 = ORIENTED_EDGE ( 'NONE', *, *, #26392, .F. ) ;
#213049 = DIRECTION ( 'NONE',  ( 0.000000000000000000, 0.000000000000000000, -1.000000000000000000 ) ) ;
#213051 = DIRECTION ( 'NONE',  ( 1.000000000000000000, 0.000000000000000000, 0.000000000000000000 ) ) ;
#213050 = CIRCLE ( 'NONE', #142320, 0.09999999999999852063 ) ;
#213052 = CARTESIAN_POINT ( 'NONE',  ( -20.94999999999999929, 77.83534155023701828, -191.9679561919613491 ) ) ;
#213053 = EDGE_LOOP ( 'NONE', ( #179380, #33949, #14537, #55755 ) ) ;
#213054 = DIRECTION ( 'NONE',  ( 1.000000000000000000, 0.000000000000000000, 0.000000000000000000 ) ) ;
#213055 = CARTESIAN_POINT ( 'NONE',  ( -18.48550754432021748, -9.463399778548760466, -74.04878975241544481 ) ) ;
#213056 = DIRECTION ( 'NONE',  ( 0.000000000000000000, 0.000000000000000000, -1.000000000000000000 ) ) ;
#213057 = CIRCLE ( 'NONE', #221413, 0.1000000000000000472 ) ;
#213059 = ORIENTED_EDGE ( 'NONE', *, *, #180946, .F. ) ;
#213058 = EDGE_CURVE ( 'NONE', #22150, #89706, #211442, .T. ) ;
#213060 = DIRECTION ( 'NONE',  ( 0.000000000000000000, 0.000000000000000000, -1.000000000000000000 ) ) ;
#213061 = FACE_OUTER_BOUND ( 'NONE', #223887, .T. ) ;
#213062 = CIRCLE ( 'NONE', #71628, 0.1000000000000054040 ) ;
#213063 = EDGE_CURVE ( 'NONE', #165183, #209328, #115202, .T. ) ;
#213064 = ORIENTED_EDGE ( 'NONE', *, *, #11494, .F. ) ;
#213065 = DIRECTION ( 'NONE',  ( -0.000000000000000000, 1.000000000000000000, -0.000000000000000000 ) ) ;
#213066 = ORIENTED_EDGE ( 'NONE', *, *, #220128, .T. ) ;
#213067 = DIRECTION ( 'NONE',  ( 1.000000000000000000, 0.000000000000000000, 0.000000000000000000 ) ) ;
#213068 = VERTEX_POINT ( 'NONE', #233868 ) ;
#213069 = CIRCLE ( 'NONE', #58922, 0.1000000000000001860 ) ;
#213070 = PLANE ( 'NONE',  #26363 ) ;
#213071 = ORIENTED_EDGE ( 'NONE', *, *, #134287, .T. ) ;
#213072 = VERTEX_POINT ( 'NONE', #111356 ) ;
#213074 = EDGE_CURVE ( 'NONE', #181336, #9664, #52647, .T. ) ;
#213073 = DIRECTION ( 'NONE',  ( -1.000000000000000000, 3.265361837132813093E-16, 2.280189983783949500E-30 ) ) ;
#213075 = LINE ( 'NONE', #113971, #62748 ) ;
#213076 = ORIENTED_EDGE ( 'NONE', *, *, #69402, .T. ) ;
#213077 = ORIENTED_EDGE ( 'NONE', *, *, #7653, .F. ) ;
#213078 = CYLINDRICAL_SURFACE ( 'NONE', #235314, 11.80000000000000426 ) ;
#213079 = EDGE_CURVE ( 'NONE', #69658, #200509, #153215, .T. ) ;
#213080 = CIRCLE ( 'NONE', #142170, 0.09999999999999971412 ) ;
#213081 = CARTESIAN_POINT ( 'NONE',  ( -16.94107738177414291, 10.01423928514777373, -54.44999999999999574 ) ) ;
#213083 = ORIENTED_EDGE ( 'NONE', *, *, #206134, .T. ) ;
#213082 = AXIS2_PLACEMENT_3D ( 'NONE', #136176, #116649, #176646 ) ;
#213084 = EDGE_CURVE ( 'NONE', #101456, #109830, #88542, .T. ) ;
#213085 = B_SPLINE_CURVE_WITH_KNOTS ( 'NONE', 3,
 ( #22994, #245863, #65942, #84158, #5939, #82898 ),
 .UNSPECIFIED., .F., .F.,
 ( 4, 2, 4 ),
 ( 0.000000000000000000, 0.0001497467027049226784, 0.0002994934054098453567 ),
 .UNSPECIFIED. ) ;
#213086 = AXIS2_PLACEMENT_3D ( 'NONE', #197908, #237047, #80499 ) ;
#213087 = AXIS2_PLACEMENT_3D ( 'NONE', #29610, #229073, #209492 ) ;
#213088 = EDGE_LOOP ( 'NONE', ( #89175, #109853, #248452, #135488, #108627 ) ) ;
#213089 = ADVANCED_FACE ( 'NONE', ( #196036 ), #214310, .F. ) ;
#213092 = EDGE_CURVE ( 'NONE', #214929, #201200, #95105, .T. ) ;
#213091 = ADVANCED_FACE ( 'NONE', ( #253419 ), #155651, .T. ) ;
#213090 = DIRECTION ( 'NONE',  ( 1.000000000000000000, 0.000000000000000000, 0.000000000000000000 ) ) ;
#213093 = CARTESIAN_POINT ( 'NONE',  ( -23.25000000000000000, 76.00000000001213607, -136.5231074845243313 ) ) ;
#213094 = CIRCLE ( 'NONE', #175529, 0.09999999999999939493 ) ;
#213095 = CARTESIAN_POINT ( 'NONE',  ( 23.14999999999999858, 76.00000000001142553, -36.02310748452432421 ) ) ;
#213097 = ORIENTED_EDGE ( 'NONE', *, *, #10472, .F. ) ;
#213096 = FACE_OUTER_BOUND ( 'NONE', #128965, .T. ) ;
#213098 = DIRECTION ( 'NONE',  ( -0.7071067811865463515, -0.7071067811865487940, -4.937700262164540154E-15 ) ) ;
#213099 = CARTESIAN_POINT ( 'NONE',  ( 20.94999999999999574, 76.00000000001267608, -203.5231074845243597 ) ) ;
#213100 = CARTESIAN_POINT ( 'NONE',  ( 21.05000000000000071, 43.04635563724865932, -239.7315875678428370 ) ) ;
#213102 = CARTESIAN_POINT ( 'NONE',  ( 22.47071067811865319, 0.000000000000000000, 0.000000000000000000 ) ) ;
#213101 = CARTESIAN_POINT ( 'NONE',  ( 20.94999999999999574, 87.65000000001163016, -66.52310748452423184 ) ) ;
#213103 = CARTESIAN_POINT ( 'NONE',  ( 23.24999999999999645, 10.58889512527366428, -208.1606840254082158 ) ) ;
#213104 = LINE ( 'NONE', #231403, #61297 ) ;
#213105 = CYLINDRICAL_SURFACE ( 'NONE', #192979, 0.8750000000000007772 ) ;
#213106 = VECTOR ( 'NONE', #244397, 1000.000000000000000 ) ;
#213107 = DIRECTION ( 'NONE',  ( -1.000000000000000000, -0.000000000000000000, -0.000000000000000000 ) ) ;
#213108 = EDGE_CURVE ( 'NONE', #171727, #94242, #144974, .T. ) ;
#213109 = ADVANCED_FACE ( 'NONE', ( #255944 ), #32639, .T. ) ;
#213110 = CIRCLE ( 'NONE', #17323, 0.1999999999999945155 ) ;
#213112 = VERTEX_POINT ( 'NONE', #119067 ) ;
#213111 = AXIS2_PLACEMENT_3D ( 'NONE', #50321, #129868, #150733 ) ;
#213113 = AXIS2_PLACEMENT_3D ( 'NONE', #84840, #49605, #147425 ) ;
#213114 = EDGE_CURVE ( 'NONE', #74489, #116965, #74294, .T. ) ;
#213116 = ORIENTED_EDGE ( 'NONE', *, *, #146156, .F. ) ;
#213115 = DIRECTION ( 'NONE',  ( 0.000000000000000000, -1.000000000000000000, 0.000000000000000000 ) ) ;
#213117 =( BOUNDED_SURFACE ( )  B_SPLINE_SURFACE ( 3, 2, ( 
 ( #92337, #208464, #187612 ),
 ( #250138, #54491, #49369 ),
 ( #168076, #33702, #191477 ),
 ( #173216, #212307, #247564 ),
 ( #71521, #188878, #229297 ),
 ( #169355, #131469, #211013 ) ),
 .UNSPECIFIED., .F., .F., .F. ) 
 B_SPLINE_SURFACE_WITH_KNOTS ( ( 4, 2, 4 ),
 ( 3, 3 ),
 ( 0.0001342700090130013644, 0.0002909192928057326741, 0.0004475685765984639838 ),
 ( 0.000000000000000000, 1.000000000000000000 ),
 .UNSPECIFIED. ) 
 GEOMETRIC_REPRESENTATION_ITEM ( )  RATIONAL_B_SPLINE_SURFACE ( (
 ( 1.000000000000000000, 0.7250110520819876836, 1.000000000000000000),
 ( 1.000000000000000000, 0.7257599279127774361, 1.000000000000000000),
 ( 1.000000000000000000, 0.7137594617292282173, 1.000000000000000000),
 ( 1.000000000000000000, 0.6959270178801697515, 1.000000000000000000),
 ( 1.000000000000000000, 0.6919879549344937208, 1.000000000000000000),
 ( 1.000000000000000000, 0.7071067811865966446, 1.000000000000000000) ) ) 
 REPRESENTATION_ITEM ( '' )  SURFACE ( )  );
#213118 = ADVANCED_FACE ( 'NONE', ( #219418 ), #78627, .F. ) ;
#213119 = DIRECTION ( 'NONE',  ( 0.000000000000000000, -0.9770955615653315052, -0.2128009952263603954 ) ) ;
#213120 = CARTESIAN_POINT ( 'NONE',  ( -23.15000000000000213, 85.00000000001149658, -45.91707660717669626 ) ) ;
#213121 = EDGE_CURVE ( 'NONE', #230427, #85875, #179065, .T. ) ;
#213122 = ORIENTED_EDGE ( 'NONE', *, *, #20603, .T. ) ;
#213123 = CARTESIAN_POINT ( 'NONE',  ( 18.59999999999999076, 14.51805813080544638, -219.6885945441820809 ) ) ;
#213124 = DIRECTION ( 'NONE',  ( 1.000000000000000000, 0.000000000000000000, 0.000000000000000000 ) ) ;
#213125 = AXIS2_PLACEMENT_3D ( 'NONE', #5927, #85449, #165028 ) ;
#213126 = ORIENTED_EDGE ( 'NONE', *, *, #197164, .F. ) ;
#213127 = PLANE ( 'NONE',  #29678 ) ;
#213128 = CARTESIAN_POINT ( 'NONE',  ( -23.25000000000000000, 46.46967969402478360, -243.0849751855955674 ) ) ;
#213129 =( BOUNDED_SURFACE ( )  B_SPLINE_SURFACE ( 3, 2, ( 
 ( #21922, #25761, #102699 ),
 ( #3617, #66171, #122298 ),
 ( #199273, #200544, #63597 ),
 ( #83122, #105253, #204383 ),
 ( #165268, #201828, #243520 ),
 ( #163997, #183558, #184824 ) ),
 .UNSPECIFIED., .F., .F., .F. ) 
 B_SPLINE_SURFACE_WITH_KNOTS ( ( 4, 2, 4 ),
 ( 3, 3 ),
 ( -1.776356839400250465E-15, 0.7853981633974468357, 1.570796326794895448 ),
 ( 0.000000000000000000, 1.000000000000000000 ),
 .UNSPECIFIED. ) 
 GEOMETRIC_REPRESENTATION_ITEM ( )  RATIONAL_B_SPLINE_SURFACE ( (
 ( 1.000000000000000000, 0.4999999999999739098, 1.000000000000000000),
 ( 1.000000000000000000, 0.4993418825349509316, 1.000000000000000000),
 ( 1.000000000000000000, 0.5278258667037128982, 1.000000000000000000),
 ( 1.000000000000000000, 0.6092287576717151376, 1.000000000000000000),
 ( 1.000000000000000000, 0.6611148371763631015, 1.000000000000000000),
 ( 1.000000000000000000, 0.7071067811864732988, 1.000000000000000000) ) ) 
 REPRESENTATION_ITEM ( '' )  SURFACE ( )  );
#213130 = ADVANCED_FACE ( 'NONE', ( #378 ), #141191, .T. ) ;
#213131 = CARTESIAN_POINT ( 'NONE',  ( -11.60000000000000320, -8.250000000000005329, 15.00000000000000355 ) ) ;
#213133 = ORIENTED_EDGE ( 'NONE', *, *, #163862, .F. ) ;
#213132 = CARTESIAN_POINT ( 'NONE',  ( -21.64999999999999858, 66.65000000001188596, -90.37310748452436826 ) ) ;
#213134 = CARTESIAN_POINT ( 'NONE',  ( 21.14999999999999858, 0.09779029131994770863, -94.24218538952391100 ) ) ;
#213135 = EDGE_CURVE ( 'NONE', #239657, #177002, #213863, .T. ) ;
#213137 = EDGE_LOOP ( 'NONE', ( #76545, #126823, #147, #118060, #84770 ) ) ;
#213136 = LINE ( 'NONE', #50199, #68856 ) ;
#213138 = CARTESIAN_POINT ( 'NONE',  ( -18.59999999999999787, 14.81796439977981272, -236.5325475414793743 ) ) ;
#213139 = LINE ( 'NONE', #97005, #137443 ) ;
#213140 = DIRECTION ( 'NONE',  ( 0.000000000000000000, 0.8814952561688438326, -0.4721928772777334582 ) ) ;
#213141 = DIRECTION ( 'NONE',  ( 0.000000000000000000, 0.4930308989875324399, 0.8700118002898268310 ) ) ;
#213142 = ADVANCED_FACE ( 'NONE', ( #216862 ), #137318, .T. ) ;
#213144 = DIRECTION ( 'NONE',  ( 1.000000000000000000, 0.000000000000000000, -0.000000000000000000 ) ) ;
#213143 = DIRECTION ( 'NONE',  ( -3.469446951953515108E-14, 0.000000000000000000, 1.000000000000000000 ) ) ;
#213145 = DIRECTION ( 'NONE',  ( 0.7071067811865474617, -0.7071067811865474617, -4.937700262164531476E-15 ) ) ;
#213146 = FACE_OUTER_BOUND ( 'NONE', #240343, .T. ) ;
#213147 = DIRECTION ( 'NONE',  ( 1.000000000000000000, 0.000000000000000000, 0.000000000000000000 ) ) ;
#213148 = DIRECTION ( 'NONE',  ( -1.000000000000000000, -0.000000000000000000, 0.000000000000000000 ) ) ;
#213149 = DIRECTION ( 'NONE',  ( 0.000000000000000000, 1.000000000000000000, 2.891205793294679805E-16 ) ) ;
#213150 =( BOUNDED_CURVE ( )  B_SPLINE_CURVE ( 3, ( #211913, #232759, #129785, #253574 ),
 .UNSPECIFIED., .F., .F. ) 
 B_SPLINE_CURVE_WITH_KNOTS ( ( 4, 4 ),
 ( 0.06456096931748307732, 3.077031684272310219 ),
 .UNSPECIFIED. ) 
 CURVE ( )  GEOMETRIC_REPRESENTATION_ITEM ( )  RATIONAL_B_SPLINE_CURVE ( ( 1.000000000000000000, 0.3763440860215093164, 0.3763440860215093164, 1.000000000000000000 ) ) 
 REPRESENTATION_ITEM ( '' )  );
#213151 = ORIENTED_EDGE ( 'NONE', *, *, #224816, .T. ) ;
#213153 = AXIS2_PLACEMENT_3D ( 'NONE', #207757, #104744, #242999 ) ;
#213152 = CARTESIAN_POINT ( 'NONE',  ( 21.72449340488910252, 65.71604372252150483, -194.2731074845244166 ) ) ;
#213154 = ORIENTED_EDGE ( 'NONE', *, *, #6121, .F. ) ;
#213155 = ORIENTED_EDGE ( 'NONE', *, *, #89203, .T. ) ;
#213156 = EDGE_CURVE ( 'NONE', #223333, #213112, #203253, .T. ) ;
#213157 = LINE ( 'NONE', #218273, #227753 ) ;
#213158 = DIRECTION ( 'NONE',  ( 0.000000000000000000, 0.000000000000000000, -1.000000000000000000 ) ) ;
#213159 = ORIENTED_EDGE ( 'NONE', *, *, #55422, .F. ) ;
#213160 = EDGE_LOOP ( 'NONE', ( #38196, #247203, #61049, #207228 ) ) ;
#213161 = DIRECTION ( 'NONE',  ( 0.000000000000000000, -0.4791956752371546169, -0.8777080977375152360 ) ) ;
#213162 = AXIS2_PLACEMENT_3D ( 'NONE', #147452, #28845, #48348 ) ;
#213163 = EDGE_CURVE ( 'NONE', #70620, #220627, #32608, .T. ) ;
#213165 = ORIENTED_EDGE ( 'NONE', *, *, #168203, .T. ) ;
#213164 = VECTOR ( 'NONE', #63699, 1000.000000000000000 ) ;
#213166 = EDGE_LOOP ( 'NONE', ( #183148, #105299, #16666, #227857 ) ) ;
#213167 = CIRCLE ( 'NONE', #100710, 11.70000000000000817 ) ;
#213168 = CARTESIAN_POINT ( 'NONE',  ( -16.87036670365548474, 65.91505003675726471, -182.5731074845244279 ) ) ;
#213169 = CARTESIAN_POINT ( 'NONE',  ( 21.05000000000000071, 10.48459288120565702, -40.95671357058389361 ) ) ;
#213170 = DIRECTION ( 'NONE',  ( 1.000000000000000000, 0.000000000000000000, 0.000000000000000000 ) ) ;
#213171 = DIRECTION ( 'NONE',  ( 0.000000000000000000, -7.086529944415893080E-15, 1.000000000000000000 ) ) ;
#213172 = CARTESIAN_POINT ( 'NONE',  ( -18.50000000000000000, -9.499999999988849808, -155.7499999999999716 ) ) ;
#213173 = CARTESIAN_POINT ( 'NONE',  ( 18.53691006697098942, 10.30215155716143016, -58.20219871729846517 ) ) ;
#213175 = ORIENTED_EDGE ( 'NONE', *, *, #130555, .T. ) ;
#213174 = DIRECTION ( 'NONE',  ( 0.000000000000000000, -6.982962677686267499E-15, 1.000000000000000000 ) ) ;
#213177 = DIRECTION ( 'NONE',  ( 0.000000000000000000, 0.000000000000000000, -1.000000000000000000 ) ) ;
#213176 = PLANE ( 'NONE',  #96345 ) ;
#213178 = CARTESIAN_POINT ( 'NONE',  ( 20.04999999999999716, 8.750000000011173285, -154.8500000000000227 ) ) ;
#213179 = EDGE_LOOP ( 'NONE', ( #184167, #49925, #234148, #1117 ) ) ;
#213180 = CARTESIAN_POINT ( 'NONE',  ( 23.14999999999999858, 9.125777775466493935, -211.6520035670780544 ) ) ;
#213181 = ORIENTED_EDGE ( 'NONE', *, *, #208252, .F. ) ;
#213182 = AXIS2_PLACEMENT_3D ( 'NONE', #166624, #66211, #6217 ) ;
#213183 = DIRECTION ( 'NONE',  ( 0.7071067811865456854, 0.7071067811865493491, 4.937700262164544098E-15 ) ) ;
#213184 = DIRECTION ( 'NONE',  ( 9.044546369203339308E-15, -0.7397360091702694929, -0.6728971962616898672 ) ) ;
#213185 = CARTESIAN_POINT ( 'NONE',  ( 12.29592348164039528, 66.64419340838171024, -86.73200495297822954 ) ) ;
#213186 = VERTEX_POINT ( 'NONE', #2943 ) ;
#213187 = ORIENTED_EDGE ( 'NONE', *, *, #77516, .F. ) ;
#213188 = DIRECTION ( 'NONE',  ( -0.000000000000000000, 0.1350103645451835865, 0.9908441862701605762 ) ) ;
#213189 = CARTESIAN_POINT ( 'NONE',  ( -17.29838795460002032, 65.62845014204981453, -158.6278487671399375 ) ) ;
#213190 = CYLINDRICAL_SURFACE ( 'NONE', #144838, 0.09999999999999939493 ) ;
#213191 = ORIENTED_EDGE ( 'NONE', *, *, #47205, .T. ) ;
#213192 = DIRECTION ( 'NONE',  ( 0.000000000000000000, 0.000000000000000000, 1.000000000000000000 ) ) ;
#213195 = EDGE_CURVE ( 'NONE', #222258, #129130, #39558, .T. ) ;
#213194 = FACE_OUTER_BOUND ( 'NONE', #65558, .T. ) ;
#213193 = TOROIDAL_SURFACE ( 'NONE', #59222, 11.89999999999999858, 0.1000000000000000056 ) ;
#213196 = AXIS2_PLACEMENT_3D ( 'NONE', #241770, #164817, #163526 ) ;
#213197 = FACE_OUTER_BOUND ( 'NONE', #144369, .T. ) ;
#213198 = CARTESIAN_POINT ( 'NONE',  ( 20.94999999999999929, -8.999999999988842703, -158.0060308773475697 ) ) ;
#213199 = CARTESIAN_POINT ( 'NONE',  ( -18.47690164073607022, -9.464844538001077723, -207.7013809398360422 ) ) ;
#213201 = EDGE_LOOP ( 'NONE', ( #117653, #223034, #20309, #92671, #178825, #251848, #24966, #246338 ) ) ;
#213200 = CARTESIAN_POINT ( 'NONE',  ( 18.69999999999999929, 1.885425182446133663, -11.49641995933507843 ) ) ;
#213202 = CARTESIAN_POINT ( 'NONE',  ( 20.94999999999999574, 87.65000000001192859, -100.1231074845242262 ) ) ;
#213203 = DIRECTION ( 'NONE',  ( 0.000000000000000000, 0.000000000000000000, -1.000000000000000000 ) ) ;
#213204 = DIRECTION ( 'NONE',  ( 1.000000000000000000, -0.000000000000000000, -0.000000000000000000 ) ) ;
#213205 = DIRECTION ( 'NONE',  ( -0.000000000000000000, 1.000000000000000000, -0.000000000000000000 ) ) ;
#213206 = EDGE_CURVE ( 'NONE', #8048, #40297, #252953, .T. ) ;
#213207 = DIRECTION ( 'NONE',  ( 1.000000000000000000, 0.000000000000000000, 0.000000000000000000 ) ) ;
#213209 = ORIENTED_EDGE ( 'NONE', *, *, #164502, .F. ) ;
#213208 = DIRECTION ( 'NONE',  ( 0.000000000000000000, 0.1575844902526452040, 0.9875055080513798211 ) ) ;
#213210 = DIRECTION ( 'NONE',  ( 1.000000000000000000, -0.000000000000000000, -0.000000000000000000 ) ) ;
#213211 = DIRECTION ( 'NONE',  ( 1.000000000000000000, 0.000000000000000000, 0.000000000000000000 ) ) ;
#213212 = CARTESIAN_POINT ( 'NONE',  ( -18.59999999999999787, 64.35000000001187459, -90.87310748452438247 ) ) ;
#213213 = CIRCLE ( 'NONE', #21703, 0.1000000000000043771 ) ;
#213214 = EDGE_CURVE ( 'NONE', #43175, #6368, #86315, .T. ) ;
#213215 = EDGE_LOOP ( 'NONE', ( #108205, #232752, #243257, #189928 ) ) ;
#213216 = LINE ( 'NONE', #132418, #67788 ) ;
#213217 = CARTESIAN_POINT ( 'NONE',  ( -20.54999999999999716, 68.85000000001200249, -115.3731074845243540 ) ) ;
#213218 = LINE ( 'NONE', #18877, #79803 ) ;
#213219 = LINE ( 'NONE', #34621, #137653 ) ;
#213220 = DIRECTION ( 'NONE',  ( 0.000000000000000000, -0.2128009952263485993, 0.9770955615653341697 ) ) ;
#213221 = EDGE_CURVE ( 'NONE', #19150, #178237, #240856, .T. ) ;
#213222 = VECTOR ( 'NONE', #19746, 1000.000000000000000 ) ;
#213223 = CARTESIAN_POINT ( 'NONE',  ( -22.50000000000000000, -3.140208063160686791, -228.2318569537739847 ) ) ;
#213224 = ORIENTED_EDGE ( 'NONE', *, *, #100915, .F. ) ;
#213225 = ORIENTED_EDGE ( 'NONE', *, *, #235489, .F. ) ;
#213226 = EDGE_CURVE ( 'NONE', #211698, #2625, #207601, .T. ) ;
#213227 = CARTESIAN_POINT ( 'NONE',  ( -17.11825945287482753, 66.05000000001207638, -123.7731074845243739 ) ) ;
#213228 = CARTESIAN_POINT ( 'NONE',  ( -16.93388492042257809, 66.01145817749609535, -115.6225623613381970 ) ) ;
#213229 = ADVANCED_FACE ( 'NONE', ( #143745 ), #161588, .F. ) ;
#213230 = VECTOR ( 'NONE', #5232, 1000.000000000000000 ) ;
#213231 = CARTESIAN_POINT ( 'NONE',  ( -21.00448002041583706, 38.10493783585286565, -236.0281705111790131 ) ) ;
#213232 = CARTESIAN_POINT ( 'NONE',  ( -18.59999999999999787, -1.835341550213255957, -112.0551512925630107 ) ) ;
#213233 = EDGE_CURVE ( 'NONE', #225625, #8311, #194894, .T. ) ;
#213234 = DIRECTION ( 'NONE',  ( 0.000000000000000000, -0.8660254037844459241, -0.4999999999999873990 ) ) ;
#213235 = AXIS2_PLACEMENT_3D ( 'NONE', #76871, #156462, #37780 ) ;
#213236 = CARTESIAN_POINT ( 'NONE',  ( -20.64999999999999858, 74.00000000001259082, -190.2984855617622770 ) ) ;
#213238 = ADVANCED_FACE ( 'NONE', ( #223277 ), #68071, .T. ) ;
#213237 = AXIS2_PLACEMENT_3D ( 'NONE', #80196, #239312, #251829 ) ;
#213239 = CARTESIAN_POINT ( 'NONE',  ( -16.93255653858138388, 9.998451453988312920, -113.0816433679897131 ) ) ;
#213240 = AXIS2_PLACEMENT_3D ( 'NONE', #39279, #82192, #161790 ) ;
#213241 = AXIS2_PLACEMENT_3D ( 'NONE', #113673, #114961, #97933 ) ;
#213242 = CARTESIAN_POINT ( 'NONE',  ( -20.94999999999999929, 7.791794839520818527, -245.4663415047620845 ) ) ;
#213243 = CIRCLE ( 'NONE', #230009, 0.1000000000000028644 ) ;
#213244 = ORIENTED_EDGE ( 'NONE', *, *, #239965, .F. ) ;
#213245 = DIRECTION ( 'NONE',  ( -1.000000000000000000, 0.000000000000000000, 0.000000000000000000 ) ) ;
#213246 = VERTEX_POINT ( 'NONE', #10674 ) ;
#213247 = CARTESIAN_POINT ( 'NONE',  ( -15.75000000000000355, 9.850000000011133849, -83.75000000000004263 ) ) ;
#213248 = CARTESIAN_POINT ( 'NONE',  ( -21.05000000000000071, 6.540656951712400691, -100.6000000000000369 ) ) ;
#213249 = CARTESIAN_POINT ( 'NONE',  ( 21.05000000000000071, 10.54375127549566926, -7.556387808664851491 ) ) ;
#213251 = EDGE_LOOP ( 'NONE', ( #41612, #211919, #49600, #74176, #195388, #70142, #157943, #232421, #48268, #58202, #120156, #238409, #203148, #102062, #108354, #82257 ) ) ;
#213250 = DIRECTION ( 'NONE',  ( 1.000000000000000000, 0.000000000000000000, 0.000000000000000000 ) ) ;
#213252 = CARTESIAN_POINT ( 'NONE',  ( -22.57848426163147693, -3.230800903051896267, -228.1881664583613656 ) ) ;
#213253 = CARTESIAN_POINT ( 'NONE',  ( 21.04999999999908411, 21.99007072299442100, -231.7373276070881616 ) ) ;
#213255 = CARTESIAN_POINT ( 'NONE',  ( 18.46163235739473407, 85.48015080692994161, -62.86549694464678595 ) ) ;
#213254 = VECTOR ( 'NONE', #194586, 1000.000000000000000 ) ;
#213256 = VERTEX_POINT ( 'NONE', #128051 ) ;
#213257 = EDGE_CURVE ( 'NONE', #64653, #171719, #28520, .T. ) ;
#213258 = CARTESIAN_POINT ( 'NONE',  ( -23.15000000000000213, 2.600000000000000089, 11.75000000000000000 ) ) ;
#213259 = CARTESIAN_POINT ( 'NONE',  ( 18.58143601961852909, 65.56427058491723869, -145.2731074845244166 ) ) ;
#213260 = DIRECTION ( 'NONE',  ( 0.000000000000000000, -0.9876197685951263461, 0.1568667991644794590 ) ) ;
#213261 = CARTESIAN_POINT ( 'NONE',  ( -18.50000000000000355, 85.40000000001229807, -162.7258477248610404 ) ) ;
#213262 = AXIS2_PLACEMENT_3D ( 'NONE', #208205, #131212, #227743 ) ;
#213263 = AXIS2_PLACEMENT_3D ( 'NONE', #65975, #235939, #183366 ) ;
#213264 = CYLINDRICAL_SURFACE ( 'NONE', #178957, 0.5000000000000007772 ) ;
#213265 = ORIENTED_EDGE ( 'NONE', *, *, #251922, .F. ) ;
#213266 = CIRCLE ( 'NONE', #109219, 0.1000000000000028644 ) ;
#213267 = DIRECTION ( 'NONE',  ( 0.000000000000000000, -0.8814952561688430555, 0.4721928772777346239 ) ) ;
#213269 = EDGE_CURVE ( 'NONE', #8900, #231640, #178335, .T. ) ;
#213268 = CARTESIAN_POINT ( 'NONE',  ( -16.80468759584937288, 66.05784632487771546, -90.33308861832274772 ) ) ;
#213270 = ORIENTED_EDGE ( 'NONE', *, *, #16199, .T. ) ;
#213271 = CARTESIAN_POINT ( 'NONE',  ( -16.87683809663752399, 66.15000000001231228, -157.3731074845244393 ) ) ;
#213272 = AXIS2_PLACEMENT_3D ( 'NONE', #144354, #204348, #225184 ) ;
#213273 = CARTESIAN_POINT ( 'NONE',  ( 20.99999999999999645, 66.25000000001159606, -56.87310748452438958 ) ) ;
#213274 = DIRECTION ( 'NONE',  ( 0.000000000000000000, 0.8660254037844424824, 0.4999999999999934497 ) ) ;
#213275 = VERTEX_POINT ( 'NONE', #109752 ) ;
#213276 = CARTESIAN_POINT ( 'NONE',  ( 18.60000000000000142, -9.480686695267808162, -174.4411151687578752 ) ) ;
#213277 = CARTESIAN_POINT ( 'NONE',  ( 21.05000000000000071, 8.876614585098257848, -41.88508047884467800 ) ) ;
#213278 = ORIENTED_EDGE ( 'NONE', *, *, #19503, .F. ) ;
#213279 = CIRCLE ( 'NONE', #188179, 0.4000000000000114575 ) ;
#213280 = VECTOR ( 'NONE', #10934, 1000.000000000000000 ) ;
#213281 = EDGE_CURVE ( 'NONE', #86438, #253135, #30248, .T. ) ;
#213282 = CIRCLE ( 'NONE', #204916, 0.1000000000000013933 ) ;
#213283 = ORIENTED_EDGE ( 'NONE', *, *, #92735, .F. ) ;
#213284 = CARTESIAN_POINT ( 'NONE',  ( -23.15000000000000213, 85.00000000001207923, -127.1291383618717816 ) ) ;
#213285 = CARTESIAN_POINT ( 'NONE',  ( 18.49999999999999289, 64.25000000001188027, -94.92310748452439384 ) ) ;
#213288 = EDGE_CURVE ( 'NONE', #102678, #18466, #182428, .T. ) ;
#213287 = ORIENTED_EDGE ( 'NONE', *, *, #4532, .F. ) ;
#213286 = CARTESIAN_POINT ( 'NONE',  ( -20.85000000000000142, 74.93036000061670165, -233.6816308724374949 ) ) ;
#213289 = DIRECTION ( 'NONE',  ( 0.000000000000000000, -1.000000000000000000, 0.000000000000000000 ) ) ;
#213290 = CARTESIAN_POINT ( 'NONE',  ( -22.50000000000000000, 31.89597452117652665, -238.9192857152812053 ) ) ;
#213291 = DIRECTION ( 'NONE',  ( -1.000000000000000000, 1.207181226542539700E-16, -2.694675058168174199E-16 ) ) ;
#213292 = DIRECTION ( 'NONE',  ( 0.000000000000000000, -1.000000000000000000, -6.982962677686265922E-15 ) ) ;
#213293 = LINE ( 'NONE', #38528, #158412 ) ;
#213294 = ADVANCED_FACE ( 'NONE', ( #208868 ), #26391, .T. ) ;
#213295 = CARTESIAN_POINT ( 'NONE',  ( 23.14999999999999503, 6.650000000011155876, -121.6500000000000341 ) ) ;
#213296 = CARTESIAN_POINT ( 'NONE',  ( -16.77683809663752257, 66.05416425680813575, -157.3591584654202222 ) ) ;
#213297 = EDGE_CURVE ( 'NONE', #232094, #139384, #61783, .T. ) ;
#213299 = ORIENTED_EDGE ( 'NONE', *, *, #101345, .F. ) ;
#213298 = DIRECTION ( 'NONE',  ( 0.000000000000000000, 0.2128009952263601734, -0.9770955615653315052 ) ) ;
#213300 = ORIENTED_EDGE ( 'NONE', *, *, #92523, .T. ) ;
#213301 = LINE ( 'NONE', #251134, #228725 ) ;
#213303 = VERTEX_POINT ( 'NONE', #105883 ) ;
#213302 = DIRECTION ( 'NONE',  ( 1.000000000000000000, 0.000000000000000000, 0.000000000000000000 ) ) ;
#213304 = ORIENTED_EDGE ( 'NONE', *, *, #76428, .F. ) ;
#213305 = LINE ( 'NONE', #12577, #72514 ) ;
#213306 = AXIS2_PLACEMENT_3D ( 'NONE', #28488, #145809, #89682 ) ;
#213307 = EDGE_CURVE ( 'NONE', #110957, #124745, #168505, .T. ) ;
#213308 = DIRECTION ( 'NONE',  ( 0.000000000000000000, 0.000000000000000000, -1.000000000000000000 ) ) ;
#213310 = EDGE_CURVE ( 'NONE', #69302, #106574, #6811, .T. ) ;
#213309 = CARTESIAN_POINT ( 'NONE',  ( -22.49436431346200038, 64.35004905235850003, -103.0900110142466417 ) ) ;
#213311 = CARTESIAN_POINT ( 'NONE',  ( -16.97683809663752186, 9.850000000011140955, -180.1499999999999773 ) ) ;
#213312 = CARTESIAN_POINT ( 'NONE',  ( -21.05000000000000071, 76.25610579210437834, -136.5580039261965908 ) ) ;
#213313 = DIRECTION ( 'NONE',  ( 1.000000000000000000, 0.000000000000000000, 0.000000000000000000 ) ) ;
#213314 = DIRECTION ( 'NONE',  ( 1.000000000000000000, 0.000000000000000000, 0.000000000000000000 ) ) ;
#213315 = VERTEX_POINT ( 'NONE', #148907 ) ;
#213316 = VERTEX_POINT ( 'NONE', #107185 ) ;
#213317 = DIRECTION ( 'NONE',  ( 1.000000000000000000, 0.000000000000000000, 0.000000000000000000 ) ) ;
#213318 = ORIENTED_EDGE ( 'NONE', *, *, #120095, .T. ) ;
#213319 = CARTESIAN_POINT ( 'NONE',  ( -18.50000000000000000, 42.98415524044398950, -233.9519173640448173 ) ) ;
#213320 = VERTEX_POINT ( 'NONE', #49787 ) ;
#213321 = CARTESIAN_POINT ( 'NONE',  ( -18.59999999999999787, 74.16465844978745281, -91.46795619196133487 ) ) ;
#213322 = ADVANCED_FACE ( 'NONE', ( #186753 ), #140902, .T. ) ;
#213323 = AXIS2_PLACEMENT_3D ( 'NONE', #158434, #194985, #237931 ) ;
#213324 = CARTESIAN_POINT ( 'NONE',  ( -16.90257928357874562, 9.954106821116520010, -79.63628543011373040 ) ) ;
#213325 = CARTESIAN_POINT ( 'NONE',  ( -14.22969084473441725, 66.54399267394272499, -118.0344739903776343 ) ) ;
#213326 = EDGE_CURVE ( 'NONE', #120740, #115352, #87614, .T. ) ;
#213327 = ORIENTED_EDGE ( 'NONE', *, *, #202739, .T. ) ;
#213328 = EDGE_CURVE ( 'NONE', #146247, #74153, #211639, .T. ) ;
#213329 = CARTESIAN_POINT ( 'NONE',  ( -20.64999999999999858, 4.768403829798271154, -213.4961173936592331 ) ) ;
#213330 = ORIENTED_EDGE ( 'NONE', *, *, #117733, .F. ) ;
#213331 = DIRECTION ( 'NONE',  ( 0.000000000000000000, -6.982962677686266711E-15, 1.000000000000000000 ) ) ;
#213332 = CARTESIAN_POINT ( 'NONE',  ( 16.87683809663750267, 66.05000000001187743, -90.37310748452438247 ) ) ;
#213333 = ORIENTED_EDGE ( 'NONE', *, *, #228070, .T. ) ;
#213334 = ADVANCED_FACE ( 'NONE', ( #234858 ), #193174, .F. ) ;
#213336 = CARTESIAN_POINT ( 'NONE',  ( -21.14999999999999858, -0.09999999998884338825, -88.85042919245522341 ) ) ;
#213335 = AXIS2_PLACEMENT_3D ( 'NONE', #5038, #160323, #84556 ) ;
#213337 = ORIENTED_EDGE ( 'NONE', *, *, #28139, .F. ) ;
#213340 = EDGE_LOOP ( 'NONE', ( #110672, #152752, #68621, #104776 ) ) ;
#213339 = CARTESIAN_POINT ( 'NONE',  ( 23.24999999999999289, 11.65000000001116298, -126.9851942293460922 ) ) ;
#213338 = DIRECTION ( 'NONE',  ( 0.000000000000000000, -0.9126074666063770380, -0.4088369013363281068 ) ) ;
#213341 = DIRECTION ( 'NONE',  ( 0.000000000000000000, -0.9651348961777157509, 0.2617529984165031243 ) ) ;
#213342 = ORIENTED_EDGE ( 'NONE', *, *, #77677, .F. ) ;
#213343 = CIRCLE ( 'NONE', #121794, 12.87499999999999822 ) ;
#213344 = VERTEX_POINT ( 'NONE', #150194 ) ;
#213345 = VECTOR ( 'NONE', #92246, 1000.000000000000114 ) ;
#213346 = CARTESIAN_POINT ( 'NONE',  ( 21.00023020733503643, -5.827586677109586333E-16, 6.390869245268367749 ) ) ;
#213347 = ORIENTED_EDGE ( 'NONE', *, *, #39483, .T. ) ;
#213348 = CYLINDRICAL_SURFACE ( 'NONE', #151787, 0.09999999999999939493 ) ;
#213349 = CARTESIAN_POINT ( 'NONE',  ( 22.42196299218230493, 64.17959721473168599, -247.0979341721383378 ) ) ;
#213350 = DIRECTION ( 'NONE',  ( 0.000000000000000000, 0.000000000000000000, -1.000000000000000000 ) ) ;
#213351 = LINE ( 'NONE', #192528, #168576 ) ;
#213352 = CARTESIAN_POINT ( 'NONE',  ( -18.39999999999999858, -0.7490476236415750666, -242.2033265267442061 ) ) ;
#213353 = EDGE_CURVE ( 'NONE', #65641, #88893, #49315, .T. ) ;
#213354 = AXIS2_PLACEMENT_3D ( 'NONE', #142836, #9771, #123314 ) ;
#213355 = ORIENTED_EDGE ( 'NONE', *, *, #207102, .F. ) ;
#213356 = AXIS2_PLACEMENT_3D ( 'NONE', #41491, #141842, #83117 ) ;
#213357 = DIRECTION ( 'NONE',  ( 0.000000000000000000, 0.000000000000000000, 1.000000000000000000 ) ) ;
#213358 = CARTESIAN_POINT ( 'NONE',  ( -21.04999999999999716, 64.25000000001195133, -109.8647081744214375 ) ) ;
#213359 = CARTESIAN_POINT ( 'NONE',  ( -21.05000000000000071, 11.60000000001115339, -160.5717967697245285 ) ) ;
#213360 = EDGE_CURVE ( 'NONE', #75395, #8169, #113017, .T. ) ;
#213361 = VERTEX_POINT ( 'NONE', #231025 ) ;
#213362 = SPHERICAL_SURFACE ( 'NONE', #176176, 0.1000000000000000056 ) ;
#213363 = ORIENTED_EDGE ( 'NONE', *, *, #196337, .F. ) ;
#213364 = CARTESIAN_POINT ( 'NONE',  ( 21.05000000000000071, 34.89593390941166007, -248.6067769466879156 ) ) ;
#213365 = ORIENTED_EDGE ( 'NONE', *, *, #79299, .T. ) ;
#213366 = DIRECTION ( 'NONE',  ( 0.000000000000000000, -0.4088369013363205573, 0.9126074666063803686 ) ) ;
#213367 = DIRECTION ( 'NONE',  ( 0.000000000000000000, 0.000000000000000000, 1.000000000000000000 ) ) ;
#213368 = CIRCLE ( 'NONE', #221733, 0.1000000000000072220 ) ;
#213371 = ORIENTED_EDGE ( 'NONE', *, *, #210391, .T. ) ;
#213370 = ADVANCED_FACE ( 'NONE', ( #14545 ), #49115, .T. ) ;
#213369 = LINE ( 'NONE', #59402, #202710 ) ;
#213372 = DIRECTION ( 'NONE',  ( 0.000000000000000000, -0.1575844902526579161, -0.9875055080513779338 ) ) ;
#213373 = ORIENTED_EDGE ( 'NONE', *, *, #251258, .T. ) ;
#213374 = CARTESIAN_POINT ( 'NONE',  ( 33.80000000000000426, 3.175288713399626594, -347.0000000000001137 ) ) ;
#213375 = EDGE_CURVE ( 'NONE', #241009, #170452, #249064, .T. ) ;
#213376 = VECTOR ( 'NONE', #117119, 1000.000000000000000 ) ;
#213377 = AXIS2_PLACEMENT_3D ( 'NONE', #28907, #168420, #250464 ) ;
#213378 = CARTESIAN_POINT ( 'NONE',  ( -16.97683809663752186, 9.950000000011137047, -113.9023640181965220 ) ) ;
#213379 = EDGE_LOOP ( 'NONE', ( #94638, #110773, #56712, #115814 ) ) ;
#213380 = AXIS2_PLACEMENT_3D ( 'NONE', #201064, #4140, #241481 ) ;
#213381 = CARTESIAN_POINT ( 'NONE',  ( -21.93340585898186390, 1.115541036281197940E-11, -126.6758529778672369 ) ) ;
#213383 = ADVANCED_FACE ( 'NONE', ( #114906 ), #90802, .T. ) ;
#213382 = LINE ( 'NONE', #34791, #15172 ) ;
#213384 = ORIENTED_EDGE ( 'NONE', *, *, #137976, .F. ) ;
#213385 = CARTESIAN_POINT ( 'NONE',  ( 18.59999999999999432, 80.78317333349157536, -192.9003134612048882 ) ) ;
#213386 = VERTEX_POINT ( 'NONE', #130610 ) ;
#213387 = ADVANCED_FACE ( 'NONE', ( #91492 ), #124162, .F. ) ;
#213388 = CARTESIAN_POINT ( 'NONE',  ( -18.59999999999999787, 64.35000000001234355, -163.1083017138704179 ) ) ;
#213390 = EDGE_CURVE ( 'NONE', #165864, #211107, #20101, .T. ) ;
#213389 = DIRECTION ( 'NONE',  ( -0.000000000000000000, 1.000000000000000000, 6.982962677686266711E-15 ) ) ;
#213392 = EDGE_LOOP ( 'NONE', ( #120914, #5555, #140211, #64959 ) ) ;
#213391 = DIRECTION ( 'NONE',  ( 0.000000000000000000, -0.000000000000000000, 1.000000000000000000 ) ) ;
#213393 = CARTESIAN_POINT ( 'NONE',  ( -2.995603634470891112E-16, 69.35000000001200249, -115.2731074845243455 ) ) ;
#213394 = DIRECTION ( 'NONE',  ( -0.000000000000000000, 0.4721928772777346239, 0.8814952561688430555 ) ) ;
#213395 = DIRECTION ( 'NONE',  ( -1.000000000000000000, -0.000000000000000000, 0.000000000000000000 ) ) ;
#213397 = CARTESIAN_POINT ( 'NONE',  ( 20.94999999999999929, 45.93315328338058379, -256.6017782078560003 ) ) ;
#213396 = DIRECTION ( 'NONE',  ( 0.000000000000000000, -1.000000000000000000, 0.000000000000000000 ) ) ;
#213398 = CARTESIAN_POINT ( 'NONE',  ( -18.50000000000000000, 77.83585931145546510, -91.51866831572576189 ) ) ;
#213399 = CARTESIAN_POINT ( 'NONE',  ( 22.39999999999999503, 11.75000000001116263, -100.6000000000000369 ) ) ;
#213400 = CIRCLE ( 'NONE', #155197, 0.09999999999999939493 ) ;
#213401 = CARTESIAN_POINT ( 'NONE',  ( -18.59999999999999787, -10.74999999999999289, -15.00000000000000000 ) ) ;
#213402 = AXIS2_PLACEMENT_3D ( 'NONE', #228211, #63991, #30029 ) ;
#213403 = LINE ( 'NONE', #72647, #154957 ) ;
#213404 = EDGE_CURVE ( 'NONE', #256073, #134179, #218758, .T. ) ;
#213405 = ADVANCED_FACE ( 'NONE', ( #95342 ), #215285, .T. ) ;
#213406 = ORIENTED_EDGE ( 'NONE', *, *, #9175, .T. ) ;
#213407 = VERTEX_POINT ( 'NONE', #36686 ) ;
#213408 = CARTESIAN_POINT ( 'NONE',  ( -21.05000000000000071, 1.115600667400684642E-11, -167.4999999999999716 ) ) ;
#213410 = ORIENTED_EDGE ( 'NONE', *, *, #232062, .T. ) ;
#213409 = DIRECTION ( 'NONE',  ( 0.000000000000000000, 0.000000000000000000, -1.000000000000000000 ) ) ;
#213411 = ORIENTED_EDGE ( 'NONE', *, *, #75351, .F. ) ;
#213412 = LINE ( 'NONE', #197701, #218451 ) ;
#213413 = ORIENTED_EDGE ( 'NONE', *, *, #70226, .F. ) ;
#213414 = CARTESIAN_POINT ( 'NONE',  ( 22.00356870140716126, 33.69312245271871120, -242.9308869566589237 ) ) ;
#213415 = CIRCLE ( 'NONE', #246739, 0.1000000000000043771 ) ;
#213416 = EDGE_CURVE ( 'NONE', #111271, #151453, #78338, .T. ) ;
#213417 = ORIENTED_EDGE ( 'NONE', *, *, #135082, .F. ) ;
#213419 = CIRCLE ( 'NONE', #55186, 0.09999999999999943656 ) ;
#213418 =( NAMED_UNIT ( * ) SI_UNIT ( $, .STERADIAN. ) SOLID_ANGLE_UNIT ( ) );
#213420 = CARTESIAN_POINT ( 'NONE',  ( 21.05000000000000071, 76.00000000001186606, -90.87310748452429721 ) ) ;
#213421 = AXIS2_PLACEMENT_3D ( 'NONE', #16853, #211186, #256676 ) ;
#213422 = ADVANCED_FACE ( 'NONE', ( #60053 ), #77053, .F. ) ;
#213424 = ORIENTED_EDGE ( 'NONE', *, *, #87523, .F. ) ;
#213423 = ORIENTED_EDGE ( 'NONE', *, *, #181646, .F. ) ;
#213425 = ORIENTED_EDGE ( 'NONE', *, *, #88220, .F. ) ;
#213426 = CIRCLE ( 'NONE', #230192, 0.09999999999998898659 ) ;
#213427 = ORIENTED_EDGE ( 'NONE', *, *, #173115, .T. ) ;
#213429 = ORIENTED_EDGE ( 'NONE', *, *, #33531, .F. ) ;
#213428 = AXIS2_PLACEMENT_3D ( 'NONE', #67726, #126408, #105528 ) ;
#213430 = CARTESIAN_POINT ( 'NONE',  ( 20.93284271247462414, 11.75000000000000355, -26.48519422934606382 ) ) ;
#213431 = CARTESIAN_POINT ( 'NONE',  ( 22.50000000000000000, 76.00000000001267608, -203.5231074845243597 ) ) ;
#213432 = CARTESIAN_POINT ( 'NONE',  ( 23.24999999999999289, 55.39363411790989034, -234.6384634766556303 ) ) ;
#213434 = ORIENTED_EDGE ( 'NONE', *, *, #89183, .F. ) ;
#213433 = CARTESIAN_POINT ( 'NONE',  ( -22.50000000000000000, 1.115600667400684642E-11, -100.5000000000000284 ) ) ;
#213435 = FACE_OUTER_BOUND ( 'NONE', #75433, .T. ) ;
#213436 = EDGE_CURVE ( 'NONE', #242494, #246420, #97873, .T. ) ;
#213437 = DIRECTION ( 'NONE',  ( 1.000000000000000000, 3.469446951953704435E-14, -2.003086131649669752E-14 ) ) ;
#213439 = EDGE_LOOP ( 'NONE', ( #101053, #26332, #237447, #205369 ) ) ;
#213438 = CARTESIAN_POINT ( 'NONE',  ( 20.95325940946048249, 10.52339007070744614, -141.5644621292400984 ) ) ;
#213440 = DIRECTION ( 'NONE',  ( 1.000000000000000000, 0.000000000000000000, -0.000000000000000000 ) ) ;
#213441 = ORIENTED_EDGE ( 'NONE', *, *, #30938, .T. ) ;
#213442 = DIRECTION ( 'NONE',  ( -0.000000000000000000, 0.9770955615653313941, 0.2128009952263603954 ) ) ;
#213443 = VECTOR ( 'NONE', #192652, 1000.000000000000000 ) ;
#213445 = ORIENTED_EDGE ( 'NONE', *, *, #128615, .T. ) ;
#213444 = CARTESIAN_POINT ( 'NONE',  ( 21.09706851349342216, 8.775842513484549912, -112.7355662163996755 ) ) ;
#213446 = AXIS2_PLACEMENT_3D ( 'NONE', #41663, #218984, #76906 ) ;
#213447 = CARTESIAN_POINT ( 'NONE',  ( -20.64999999999999858, 4.349999999999999645, -21.25000000000000000 ) ) ;
#213448 = CARTESIAN_POINT ( 'NONE',  ( 18.39999999999999503, 8.822561741677553471, -191.7499999999999716 ) ) ;
#213451 = EDGE_CURVE ( 'NONE', #236931, #18989, #257529, .T. ) ;
#213450 = EDGE_LOOP ( 'NONE', ( #133335, #90137, #205776, #49590, #175247, #12128, #60803, #98613 ) ) ;
#213449 = AXIS2_PLACEMENT_3D ( 'NONE', #154664, #235436, #58074 ) ;
#213452 = CIRCLE ( 'NONE', #130054, 0.1000000000000028644 ) ;
#213454 = FACE_OUTER_BOUND ( 'NONE', #168549, .T. ) ;
#213453 = CARTESIAN_POINT ( 'NONE',  ( -16.87998658237754768, 9.950000000011137047, -46.36363956773774930 ) ) ;
#213455 = CARTESIAN_POINT ( 'NONE',  ( -20.54999999999999716, -9.000000000000001776, -23.60603087734756045 ) ) ;
#213456 = LINE ( 'NONE', #132651, #242950 ) ;
#213457 = B_SPLINE_CURVE_WITH_KNOTS ( 'NONE', 3,
 ( #86754, #163757, #102451, #162481, #52449, #3368, #25533, #151601, #31656, #243267, #244557, #111163, #43806, #65934, #106315, #190728, #12086, #184587, #185872 ),
 .UNSPECIFIED., .F., .F.,
 ( 4, 3, 3, 3, 3, 3, 4 ),
 ( -2.000416914663624153E-06, 4.235164736271501695E-22, 4.714008503747322393E-05, 9.979203887779870851E-05, 0.0001372215519229730426, 0.0001635031576221134507, 0.0001900083748504316744 ),
 .UNSPECIFIED. ) ;
#213458 = DIRECTION ( 'NONE',  ( 0.000000000000000000, 0.000000000000000000, -1.000000000000000000 ) ) ;
#213459 = ORIENTED_EDGE ( 'NONE', *, *, #230621, .F. ) ;
#213460 = ORIENTED_EDGE ( 'NONE', *, *, #38576, .T. ) ;
#213461 = AXIS2_PLACEMENT_3D ( 'NONE', #181807, #100929, #121845 ) ;
#213462 = CARTESIAN_POINT ( 'NONE',  ( 20.95512820512820440, 8.876151316288117599, -8.558628995140949769 ) ) ;
#213463 = CARTESIAN_POINT ( 'NONE',  ( -20.94999999999999929, -1.835341550213255957, -179.0551512925629538 ) ) ;
#213464 = ORIENTED_EDGE ( 'NONE', *, *, #209862, .T. ) ;
#213465 = DIRECTION ( 'NONE',  ( 0.000000000000000000, 0.8700118002898321601, -0.4930308989875230030 ) ) ;
#213466 = ORIENTED_EDGE ( 'NONE', *, *, #222787, .T. ) ;
#213467 = EDGE_CURVE ( 'NONE', #93167, #194728, #236730, .T. ) ;
#213468 = CARTESIAN_POINT ( 'NONE',  ( 23.24999999999999645, 70.40000000001253966, -182.4283735034374843 ) ) ;
#213469 = VECTOR ( 'NONE', #50188, 1000.000000000000000 ) ;
#213470 = DIRECTION ( 'NONE',  ( 0.000000000000000000, 0.4930308989875230585, 0.8700118002898322711 ) ) ;
#213471 = ORIENTED_EDGE ( 'NONE', *, *, #32895, .F. ) ;
#213472 = CARTESIAN_POINT ( 'NONE',  ( 21.05000000000000071, 67.22371710471961137, -128.0351067629399893 ) ) ;
#213473 = VECTOR ( 'NONE', #51569, 1000.000000000000000 ) ;
#213474 = CIRCLE ( 'NONE', #238423, 0.1000000000000028644 ) ;
#213475 = ORIENTED_EDGE ( 'NONE', *, *, #85587, .T. ) ;
#213477 = ORIENTED_EDGE ( 'NONE', *, *, #6850, .T. ) ;
#213476 = VECTOR ( 'NONE', #46407, 1000.000000000000000 ) ;
#213478 = EDGE_LOOP ( 'NONE', ( #92467, #8882, #178530 ) ) ;
#213479 = DIRECTION ( 'NONE',  ( -0.000000000000000000, -6.982962677686266711E-15, 1.000000000000000000 ) ) ;
#213480 = FACE_OUTER_BOUND ( 'NONE', #101722, .T. ) ;
#213481 = DIRECTION ( 'NONE',  ( 7.304098846218134667E-16, 1.000000000000000000, 6.982962677686267499E-15 ) ) ;
#213482 = CYLINDRICAL_SURFACE ( 'NONE', #169505, 0.09999999999999939493 ) ;
#213483 = CARTESIAN_POINT ( 'NONE',  ( 12.42718393586866021, 66.62934494888854431, -118.9972842285435064 ) ) ;
#213485 = CARTESIAN_POINT ( 'NONE',  ( 20.94999999999999929, 23.45160524131172153, -253.2535058871250726 ) ) ;
#213484 = CARTESIAN_POINT ( 'NONE',  ( 22.45301702632625762, -3.133220771888840073, -228.2183440840713047 ) ) ;
#213487 = ORIENTED_EDGE ( 'NONE', *, *, #35193, .F. ) ;
#213486 = DIRECTION ( 'NONE',  ( -0.7071067811865389130, 4.937700262164590641E-15, -0.7071067811865561215 ) ) ;
#213488 = CARTESIAN_POINT ( 'NONE',  ( -16.87368910959167678, 9.961273816702552963, -79.61249309664063389 ) ) ;
#213489 = ORIENTED_EDGE ( 'NONE', *, *, #229534, .T. ) ;
#213490 = CARTESIAN_POINT ( 'NONE',  ( -12.29659703204451837, 9.355888454513703323, -150.2886428967780148 ) ) ;
#213491 = VERTEX_POINT ( 'NONE', #160480 ) ;
#213492 = ORIENTED_EDGE ( 'NONE', *, *, #70285, .F. ) ;
#213493 = DIRECTION ( 'NONE',  ( 0.000000000000000000, 0.5000000000000209832, 0.8660254037844264952 ) ) ;
#213494 = CARTESIAN_POINT ( 'NONE',  ( -21.45000000000000284, 7.708578643773852157, -88.25000000000005684 ) ) ;
#213495 = FACE_OUTER_BOUND ( 'NONE', #94747, .T. ) ;
#213496 = VECTOR ( 'NONE', #185884, 1000.000000000000000 ) ;
#213497 = B_SPLINE_CURVE_WITH_KNOTS ( 'NONE', 3,
 ( #1247, #118673, #121263, #42971, #23436, #256817, #200756, #198183, #101612, #178661, #182496, #80781, #20862, #2538, #82055, #99057 ),
 .UNSPECIFIED., .F., .F.,
 ( 4, 3, 3, 3, 3, 4 ),
 ( 0.000000000000000000, 2.372700795694925591E-05, 5.739057815867077772E-05, 9.073899019181627494E-05, 0.0001243544287365772689, 0.0001585386695601308422 ),
 .UNSPECIFIED. ) ;
#213498 = CARTESIAN_POINT ( 'NONE',  ( 20.94999999999999929, 53.86595165227826243, -236.3638196928718855 ) ) ;
#213499 = VERTEX_POINT ( 'NONE', #156640 ) ;
#213500 = ORIENTED_EDGE ( 'NONE', *, *, #255289, .F. ) ;
#213501 = AXIS2_PLACEMENT_3D ( 'NONE', #126657, #104496, #180229 ) ;
#213502 = CARTESIAN_POINT ( 'NONE',  ( -21.05000000000000071, 38.17611739746671873, -236.1379531878919806 ) ) ;
#213503 = ORIENTED_EDGE ( 'NONE', *, *, #251721, .F. ) ;
#213504 = DIRECTION ( 'NONE',  ( 0.000000000000000000, 0.000000000000000000, -1.000000000000000000 ) ) ;
#213505 = DIRECTION ( 'NONE',  ( -1.000000000000000000, 0.000000000000000000, 0.000000000000000000 ) ) ;
#213506 = ORIENTED_EDGE ( 'NONE', *, *, #687, .F. ) ;
#213507 = FACE_OUTER_BOUND ( 'NONE', #154700, .T. ) ;
#213508 = CARTESIAN_POINT ( 'NONE',  ( -20.94999999999999929, 11.65000000001115232, -60.21613433702190576 ) ) ;
#213509 = CARTESIAN_POINT ( 'NONE',  ( 18.39999999999999503, 34.05335961020092839, -234.8258093264404636 ) ) ;
#213510 = CARTESIAN_POINT ( 'NONE',  ( -21.59142135623730852, 7.850000000000003197, -21.25000000000000000 ) ) ;
#213511 = ORIENTED_EDGE ( 'NONE', *, *, #143561, .F. ) ;
#213512 = DIRECTION ( 'NONE',  ( -2.940209281316622002E-16, -0.9651348961777163060, 0.2617529984165007928 ) ) ;
#213514 = EDGE_CURVE ( 'NONE', #219341, #91448, #128608, .T. ) ;
#213513 = LINE ( 'NONE', #191432, #220523 ) ;
#213515 = CARTESIAN_POINT ( 'NONE',  ( -23.15000000000000213, 71.85000000001222986, -148.2731074845243313 ) ) ;
#213516 = ORIENTED_EDGE ( 'NONE', *, *, #75155, .F. ) ;
#213517 = CARTESIAN_POINT ( 'NONE',  ( 21.13461538461538680, 10.61458296202553875, -12.35000000000000142 ) ) ;
#213518 = ORIENTED_EDGE ( 'NONE', *, *, #236230, .T. ) ;
#213519 = CARTESIAN_POINT ( 'NONE',  ( 18.59999999999999432, 71.93512633425886804, -225.1442869522136334 ) ) ;
#213520 = SHAPE_REPRESENTATION ( 'Injection Molded Chain Links 11', ( #2425 ), #239393 ) ;
#213521 = DIRECTION ( 'NONE',  ( -0.000000000000000000, -0.000000000000000000, -1.000000000000000000 ) ) ;
#213522 = DIRECTION ( 'NONE',  ( 0.000000000000000000, 0.9908441862701420355, 0.1350103645453197554 ) ) ;
#213523 = DIRECTION ( 'NONE',  ( -1.000000000000000000, -0.000000000000000000, -0.000000000000000000 ) ) ;
#213524 = CYLINDRICAL_SURFACE ( 'NONE', #238214, 0.1000000000000028644 ) ;
#213525 = DIRECTION ( 'NONE',  ( 1.000000000000000000, 0.000000000000000000, 0.000000000000000000 ) ) ;
#213526 = EDGE_CURVE ( 'NONE', #15852, #114879, #10516, .T. ) ;
#213527 = ORIENTED_EDGE ( 'NONE', *, *, #11670, .T. ) ;
#213528 = CARTESIAN_POINT ( 'NONE',  ( -16.93226657140833069, 66.00045617728764569, -123.9443943735507503 ) ) ;
#213529 = DIRECTION ( 'NONE',  ( 1.000000000000000000, 0.000000000000000000, 0.000000000000000000 ) ) ;
#213530 = CARTESIAN_POINT ( 'NONE',  ( 21.53699400380535423, 10.33394250185612684, -227.7493655665005576 ) ) ;
#213531 = CARTESIAN_POINT ( 'NONE',  ( 20.85000000000000142, -0.3238857010591806307, -100.4575895893140256 ) ) ;
#213532 = AXIS2_PLACEMENT_3D ( 'NONE', #73747, #95828, #32057 ) ;
#213534 = DIRECTION ( 'NONE',  ( 0.000000000000000000, 0.000000000000000000, -1.000000000000000000 ) ) ;
#213533 = CIRCLE ( 'NONE', #92727, 0.3999999999999965250 ) ;
#213535 = ORIENTED_EDGE ( 'NONE', *, *, #143947, .F. ) ;
#213536 = EDGE_LOOP ( 'NONE', ( #4330, #31506, #207059, #152193 ) ) ;
#213537 = DIRECTION ( 'NONE',  ( 0.000000000000000000, 0.9126074666063773710, 0.4088369013363272741 ) ) ;
#213539 = CARTESIAN_POINT ( 'NONE',  ( -21.05000000000000071, 69.74218538953583391, -103.1208977758331571 ) ) ;
#213538 = AXIS2_PLACEMENT_3D ( 'NONE', #182073, #3409, #5975 ) ;
#213541 = ADVANCED_FACE ( 'NONE', ( #216569 ), #62303, .T. ) ;
#213540 = CARTESIAN_POINT ( 'NONE',  ( 18.58719872626880942, -9.566644397598638605, -40.32247819639701447 ) ) ;
#213542 = FACE_OUTER_BOUND ( 'NONE', #101977, .T. ) ;
#213543 = LINE ( 'NONE', #238244, #112144 ) ;
#213544 = EDGE_CURVE ( 'NONE', #257030, #225564, #196991, .T. ) ;
#213545 = VERTEX_POINT ( 'NONE', #43077 ) ;
#213546 = DIRECTION ( 'NONE',  ( -0.000000000000000000, 1.000000000000000000, -0.000000000000000000 ) ) ;
#213547 = ADVANCED_FACE ( 'NONE', ( #161760 ), #79608, .F. ) ;
#213548 = DIRECTION ( 'NONE',  ( 0.000000000000000000, 0.000000000000000000, -1.000000000000000000 ) ) ;
#213549 = AXIS2_PLACEMENT_3D ( 'NONE', #28088, #29383, #24224 ) ;
#213550 = EDGE_LOOP ( 'NONE', ( #199768, #112271, #122551 ) ) ;
#213551 = CIRCLE ( 'NONE', #30418, 0.6000000000000005329 ) ;
#213552 = DIRECTION ( 'NONE',  ( 1.000000000000000000, 0.000000000000000000, 0.000000000000000000 ) ) ;
#213553 = EDGE_CURVE ( 'NONE', #184335, #221704, #157932, .T. ) ;
#213554 = LINE ( 'NONE', #34968, #16320 ) ;
#213555 = ADVANCED_FACE ( 'NONE', ( #237423 ), #118771, .T. ) ;
#213556 = ORIENTED_EDGE ( 'NONE', *, *, #99441, .F. ) ;
#213557 = DIRECTION ( 'NONE',  ( 2.715809747126120452E-16, -0.4721928772777324035, -0.8814952561688441657 ) ) ;
#213558 = AXIS2_PLACEMENT_3D ( 'NONE', #64961, #164079, #25860 ) ;
#213559 = ORIENTED_EDGE ( 'NONE', *, *, #116741, .T. ) ;
#213560 = DIRECTION ( 'NONE',  ( 0.000000000000000000, -6.454785026890510900E-15, 1.000000000000000000 ) ) ;
#213561 = DIRECTION ( 'NONE',  ( 1.000000000000000000, 0.000000000000000000, 0.000000000000000000 ) ) ;
#213562 = CARTESIAN_POINT ( 'NONE',  ( 20.94999999999999929, 86.27712145182582049, -209.5223386573213702 ) ) ;
#213563 = CYLINDRICAL_SURFACE ( 'NONE', #65718, 0.09999999999999939493 ) ;
#213565 = CIRCLE ( 'NONE', #205363, 11.80000000000000426 ) ;
#213564 = LINE ( 'NONE', #15392, #240235 ) ;
#213566 = CARTESIAN_POINT ( 'NONE',  ( -18.59999999999999787, 9.350000000011156942, -79.35000000000005116 ) ) ;
#213568 = CARTESIAN_POINT ( 'NONE',  ( -23.25000000000000000, 73.40000000001157332, -56.29848556176223440 ) ) ;
#213567 = CIRCLE ( 'NONE', #59603, 0.09999999999999939493 ) ;
#213569 = CIRCLE ( 'NONE', #246704, 0.1000000000000028644 ) ;
#213570 = DIRECTION ( 'NONE',  ( 0.000000000000000000, 0.01562500000001045344, 0.9998779222360096863 ) ) ;
#213571 = EDGE_CURVE ( 'NONE', #175353, #223991, #215874, .T. ) ;
#213574 = DIRECTION ( 'NONE',  ( 1.000000000000000000, 0.000000000000000000, 0.000000000000000000 ) ) ;
#213573 = VECTOR ( 'NONE', #227880, 1000.000000000000000 ) ;
#213572 = CARTESIAN_POINT ( 'NONE',  ( 20.95325940946048249, 10.52339007070744437, -108.0644621292401126 ) ) ;
#213575 = DIRECTION ( 'NONE',  ( 0.000000000000000000, 0.000000000000000000, -1.000000000000000000 ) ) ;
#213576 = LINE ( 'NONE', #151054, #77204 ) ;
#213577 = CARTESIAN_POINT ( 'NONE',  ( 18.59999999999999787, 87.75000000001146816, -44.67310748452424463 ) ) ;
#213578 = EDGE_LOOP ( 'NONE', ( #40645, #198350, #120549, #247172 ) ) ;
#213579 = CARTESIAN_POINT ( 'NONE',  ( -18.50000000000000000, -9.480686695278974341, -40.44111516875785384 ) ) ;
#213580 = CARTESIAN_POINT ( 'NONE',  ( -18.59999999999999787, -1.164121893230052995, -208.9148480855715775 ) ) ;
#213581 = CARTESIAN_POINT ( 'NONE',  ( -22.94999999999999929, 7.900000000000000355, 1.300000000000000044 ) ) ;
#213582 = ORIENTED_EDGE ( 'NONE', *, *, #101820, .T. ) ;
#213583 = FACE_OUTER_BOUND ( 'NONE', #112844, .T. ) ;
#213584 = DIRECTION ( 'NONE',  ( -0.000000000000000000, 1.000000000000000000, 6.982962677686266711E-15 ) ) ;
#213585 = DIRECTION ( 'NONE',  ( 2.915501640297155269E-16, -0.4721928772777346239, -0.8814952561688430555 ) ) ;
#213586 = ORIENTED_EDGE ( 'NONE', *, *, #181233, .F. ) ;
#213587 = DIRECTION ( 'NONE',  ( 1.000000000000000000, 0.000000000000000000, 0.000000000000000000 ) ) ;
#213588 = ORIENTED_EDGE ( 'NONE', *, *, #218961, .F. ) ;
#213589 = CARTESIAN_POINT ( 'NONE',  ( 21.14999999999999858, 65.28660755661196902, -90.77310748452438816 ) ) ;
#213590 = CARTESIAN_POINT ( 'NONE',  ( 21.05000000000000071, 7.128833340094563376, -233.7327013124401276 ) ) ;
#213591 = AXIS2_PLACEMENT_3D ( 'NONE', #44774, #147730, #48615 ) ;
#213592 = EDGE_CURVE ( 'NONE', #209835, #163148, #186890, .T. ) ;
#213593 = EDGE_CURVE ( 'NONE', #195224, #8263, #220436, .T. ) ;
#213594 = ORIENTED_EDGE ( 'NONE', *, *, #111144, .F. ) ;
#213596 = DIRECTION ( 'NONE',  ( -1.000000000000000000, 0.000000000000000000, 0.000000000000000000 ) ) ;
#213595 = CIRCLE ( 'NONE', #1772, 0.2000000000000057288 ) ;
#213597 = CIRCLE ( 'NONE', #22099, 0.5999999999999987566 ) ;
#213598 = VERTEX_POINT ( 'NONE', #63920 ) ;
#213599 = EDGE_CURVE ( 'NONE', #232238, #235554, #153605, .T. ) ;
#213600 = ADVANCED_FACE ( 'NONE', ( #7806 ), #231665, .F. ) ;
#213601 = LINE ( 'NONE', #252722, #7831 ) ;
#213603 = VECTOR ( 'NONE', #215150, 1000.000000000000000 ) ;
#213602 = DIRECTION ( 'NONE',  ( 1.000000000000000000, -0.000000000000000000, -0.000000000000000000 ) ) ;
#213604 = DIRECTION ( 'NONE',  ( 1.000000000000000000, 0.000000000000000000, 0.000000000000000000 ) ) ;
#213605 = CARTESIAN_POINT ( 'NONE',  ( -16.85312841634287651, 9.913606177320202661, -12.89717313329253479 ) ) ;
#213606 = CARTESIAN_POINT ( 'NONE',  ( -15.75000000000000355, 48.12247445990688988, -234.1702647910923361 ) ) ;
#213607 = VECTOR ( 'NONE', #5847, 1000.000000000000000 ) ;
#213608 = ADVANCED_FACE ( 'NONE', ( #32189 ), #182600, .T. ) ;
#213609 = DIRECTION ( 'NONE',  ( 0.5932847527679310229, 0.3291107096594076964, -0.7346423231209702198 ) ) ;
#213611 = DIRECTION ( 'NONE',  ( 1.000000000000000000, 0.000000000000000000, 0.000000000000000000 ) ) ;
#213610 = AXIS2_PLACEMENT_3D ( 'NONE', #34490, #56556, #76143 ) ;
#213612 = CIRCLE ( 'NONE', #251196, 0.1000000000000002554 ) ;
#213614 = EDGE_LOOP ( 'NONE', ( #85098, #203586, #70106, #94050 ) ) ;
#213613 = CARTESIAN_POINT ( 'NONE',  ( 21.05000000000000071, 69.74218538953581970, -103.1208977758331429 ) ) ;
#213615 = ORIENTED_EDGE ( 'NONE', *, *, #236349, .F. ) ;
#213617 = CARTESIAN_POINT ( 'NONE',  ( -21.03922262424652345, 64.37609936600685501, -62.66389944163073977 ) ) ;
#213616 = CARTESIAN_POINT ( 'NONE',  ( 20.94999999999999929, 1.115600667400684642E-11, -134.0000000000000284 ) ) ;
#213618 = ORIENTED_EDGE ( 'NONE', *, *, #13213, .F. ) ;
#213620 = ORIENTED_EDGE ( 'NONE', *, *, #11627, .T. ) ;
#213619 = CARTESIAN_POINT ( 'NONE',  ( 18.59999999999999432, 74.83729825007408465, -128.4231074845243086 ) ) ;
#213621 = ADVANCED_FACE ( 'NONE', ( #86012 ), #195272, .F. ) ;
#213622 = ORIENTED_EDGE ( 'NONE', *, *, #335, .F. ) ;
#213623 = DIRECTION ( 'NONE',  ( 0.000000000000000000, 0.000000000000000000, 1.000000000000000000 ) ) ;
#213625 = EDGE_CURVE ( 'NONE', #62371, #89738, #16200, .T. ) ;
#213624 = EDGE_CURVE ( 'NONE', #77390, #239872, #243830, .T. ) ;
#213626 = DIRECTION ( 'NONE',  ( 0.000000000000000000, 0.000000000000000000, -1.000000000000000000 ) ) ;
#213627 = CIRCLE ( 'NONE', #101135, 0.09999999999999892308 ) ;
#213629 = EDGE_CURVE ( 'NONE', #133198, #127404, #65196, .T. ) ;
#213628 = CARTESIAN_POINT ( 'NONE',  ( -18.59999999999999787, 1.750000000011155743, -78.66951155790169992 ) ) ;
#213630 = FACE_OUTER_BOUND ( 'NONE', #113137, .T. ) ;
#213631 = DIRECTION ( 'NONE',  ( -0.000000000000000000, -0.000000000000000000, -1.000000000000000000 ) ) ;
#213632 = CARTESIAN_POINT ( 'NONE',  ( 20.09999999999999787, 9.750000000011137757, -146.6500000000000341 ) ) ;
#213633 = CIRCLE ( 'NONE', #51107, 0.1000000000000008799 ) ;
#213634 = DIRECTION ( 'NONE',  ( 0.000000000000000000, 0.9126074666063771490, 0.4088369013363281623 ) ) ;
#213635 = CIRCLE ( 'NONE', #80322, 0.09999999999998898659 ) ;
#213636 = EDGE_CURVE ( 'NONE', #111193, #4968, #28697, .T. ) ;
#213637 = DIRECTION ( 'NONE',  ( 0.000000000000000000, 0.000000000000000000, -1.000000000000000000 ) ) ;
#213638 = AXIS2_PLACEMENT_3D ( 'NONE', #93415, #118126, #115549 ) ;
#213639 = ORIENTED_EDGE ( 'NONE', *, *, #124270, .F. ) ;
#213640 = ORIENTED_EDGE ( 'NONE', *, *, #239462, .F. ) ;
#213641 = DIRECTION ( 'NONE',  ( 1.000000000000000000, 0.000000000000000000, 0.000000000000000000 ) ) ;
#213642 = EDGE_CURVE ( 'NONE', #228375, #55828, #203441, .T. ) ;
#213643 = EDGE_CURVE ( 'NONE', #25903, #167521, #147300, .T. ) ;
#213644 = ORIENTED_EDGE ( 'NONE', *, *, #56858, .F. ) ;
#213645 = CARTESIAN_POINT ( 'NONE',  ( -18.79999999999999716, -11.75000000000000000, -15.00000000000000000 ) ) ;
#213646 = ORIENTED_EDGE ( 'NONE', *, *, #196152, .F. ) ;
#213648 = AXIS2_PLACEMENT_3D ( 'NONE', #148299, #106576, #188701 ) ;
#213647 = FACE_OUTER_BOUND ( 'NONE', #55501, .T. ) ;
#213649 = CIRCLE ( 'NONE', #67724, 0.1000000000000028644 ) ;
#213650 = VECTOR ( 'NONE', #49775, 1000.000000000000000 ) ;
#213651 = EDGE_CURVE ( 'NONE', #234718, #120848, #161944, .T. ) ;
#213652 = AXIS2_PLACEMENT_3D ( 'NONE', #87788, #249469, #70849 ) ;
#213653 = DIRECTION ( 'NONE',  ( 0.000000000000000000, 0.2617529984165031243, 0.9651348961777157509 ) ) ;
#213654 = DIRECTION ( 'NONE',  ( 0.000000000000000000, -0.8814952561688476074, 0.4721928772777262417 ) ) ;
#213655 = DIRECTION ( 'NONE',  ( -0.7070776581709311559, 0.000000000000000000, 0.7071359030027479786 ) ) ;
#213656 = EDGE_CURVE ( 'NONE', #187685, #35927, #190618, .T. ) ;
#213657 = CARTESIAN_POINT ( 'NONE',  ( -23.25000000000000000, 74.08971962618075224, -182.6544753397233194 ) ) ;
#213658 = VERTEX_POINT ( 'NONE', #165604 ) ;
#213659 = ADVANCED_FACE ( 'NONE', ( #186443 ), #92133, .T. ) ;
#213660 = CARTESIAN_POINT ( 'NONE',  ( 23.14999999999999503, 11.75000000001116263, -112.6500000000000341 ) ) ;
#213661 = DIRECTION ( 'NONE',  ( 0.000000000000000000, -0.2128009952263601456, 0.9770955615653316162 ) ) ;
#213662 = CARTESIAN_POINT ( 'NONE',  ( -23.15000000000000213, 72.91131461869652242, -214.9116992594219369 ) ) ;
#213663 = DIRECTION ( 'NONE',  ( 0.000000000000000000, -0.2617529984165031243, -0.9651348961777157509 ) ) ;
#213664 = CARTESIAN_POINT ( 'NONE',  ( -21.05000000000000071, 6.258316057343182415, -133.9342983896779344 ) ) ;
#213665 = EDGE_LOOP ( 'NONE', ( #30760, #164891, #165503, #190167 ) ) ;
#213667 = CARTESIAN_POINT ( 'NONE',  ( -18.33682934331482883, 85.51118559110493322, -29.11745271585079919 ) ) ;
#213666 = DIRECTION ( 'NONE',  ( 0.000000000000000000, 0.000000000000000000, 1.000000000000000000 ) ) ;
#213668 = AXIS2_PLACEMENT_3D ( 'NONE', #160464, #99149, #79586 ) ;
#213669 = VERTEX_POINT ( 'NONE', #23550 ) ;
#213672 = ORIENTED_EDGE ( 'NONE', *, *, #207751, .T. ) ;
#213671 = LINE ( 'NONE', #97535, #26427 ) ;
#213670 = DIRECTION ( 'NONE',  ( 1.000000000000000000, 0.000000000000000000, 0.000000000000000000 ) ) ;
#213673 = CIRCLE ( 'NONE', #126162, 0.09999999999998898659 ) ;
#213674 = CYLINDRICAL_SURFACE ( 'NONE', #226986, 7.899999999999990585 ) ;
#213675 = AXIS2_PLACEMENT_3D ( 'NONE', #63622, #28391, #45343 ) ;
#213676 = DIRECTION ( 'NONE',  ( 1.000000000000000000, 0.000000000000000000, 0.000000000000000000 ) ) ;
#213677 = ORIENTED_EDGE ( 'NONE', *, *, #151648, .T. ) ;
#213678 = FACE_OUTER_BOUND ( 'NONE', #133773, .T. ) ;
#213679 = CARTESIAN_POINT ( 'NONE',  ( -17.05016517656095942, 9.949999999999985079, -12.67269799599932156 ) ) ;
#213681 = VERTEX_POINT ( 'NONE', #44371 ) ;
#213680 = CARTESIAN_POINT ( 'NONE',  ( -23.15000000000000213, -11.64999999998884483, -63.89999999999999858 ) ) ;
#213682 = EDGE_LOOP ( 'NONE', ( #38388, #46360, #66325, #102 ) ) ;
#213683 = DIRECTION ( 'NONE',  ( 0.000000000000000000, 0.2617529984165152257, 0.9651348961777124202 ) ) ;
#213684 = CARTESIAN_POINT ( 'NONE',  ( 18.58703555225022797, -9.406336740777600625, -74.12494464124685578 ) ) ;
#213685 = CARTESIAN_POINT ( 'NONE',  ( -20.94999999999999929, 63.48958393997221350, -237.5313578019574265 ) ) ;
#213686 = DIRECTION ( 'NONE',  ( 1.000000000000000000, 1.836970198721029934E-16, 0.000000000000000000 ) ) ;
#213687 = VERTEX_POINT ( 'NONE', #205995 ) ;
#213688 = DIRECTION ( 'NONE',  ( 1.000000000000000000, 1.875376730785737719E-16, 0.000000000000000000 ) ) ;
#213689 = AXIS2_PLACEMENT_3D ( 'NONE', #145272, #183147, #245677 ) ;
#213690 = CARTESIAN_POINT ( 'NONE',  ( -6.100000000000005862, -11.65000000000000036, 13.90000000000000213 ) ) ;
#213691 = CARTESIAN_POINT ( 'NONE',  ( -16.92209698673575957, 9.950000000011138823, -46.21063556705156827 ) ) ;
#213692 = ORIENTED_EDGE ( 'NONE', *, *, #104637, .T. ) ;
#213693 = CARTESIAN_POINT ( 'NONE',  ( 23.25000000000000000, 84.59626168225506149, -127.0729799673739677 ) ) ;
#213694 = CARTESIAN_POINT ( 'NONE',  ( 18.59999999999999787, 1.866714910068465239, -145.7526752462820241 ) ) ;
#213695 = EDGE_CURVE ( 'NONE', #153546, #112516, #228393, .T. ) ;
#213696 = VERTEX_POINT ( 'NONE', #144722 ) ;
#213697 = CYLINDRICAL_SURFACE ( 'NONE', #147280, 11.74999999999999822 ) ;
#213699 = ADVANCED_FACE ( 'NONE', ( #6500 ), #245126, .T. ) ;
#213698 = CARTESIAN_POINT ( 'NONE',  ( -21.05000000000000071, 76.00000000001216449, -140.5231074845243597 ) ) ;
#213701 = CARTESIAN_POINT ( 'NONE',  ( 18.39999999999999858, -9.399999999988843058, -21.75000000000000355 ) ) ;
#213700 = AXIS2_PLACEMENT_3D ( 'NONE', #96255, #173299, #72893 ) ;
#213703 = ORIENTED_EDGE ( 'NONE', *, *, #242992, .F. ) ;
#213702 = CONICAL_SURFACE ( 'NONE', #47091, 4.299999999999956302, 0.7853981633974466137 ) ;
#213704 = ORIENTED_EDGE ( 'NONE', *, *, #179070, .T. ) ;
#213705 = ADVANCED_FACE ( 'NONE', ( #214638 ), #252476, .F. ) ;
#213706 = CYLINDRICAL_SURFACE ( 'NONE', #254094, 0.09999999999999939493 ) ;
#213707 = ORIENTED_EDGE ( 'NONE', *, *, #127080, .T. ) ;
#213710 = EDGE_CURVE ( 'NONE', #236521, #151746, #61969, .T. ) ;
#213709 = ORIENTED_EDGE ( 'NONE', *, *, #116810, .T. ) ;
#213708 = CARTESIAN_POINT ( 'NONE',  ( 22.45380639572341153, 25.93539157114272342, -254.3551731436069474 ) ) ;
#213713 = ORIENTED_EDGE ( 'NONE', *, *, #31383, .T. ) ;
#213712 = ORIENTED_EDGE ( 'NONE', *, *, #257844, .F. ) ;
#213711 = SPHERICAL_SURFACE ( 'NONE', #209386, 0.1000000000000000056 ) ;
#213714 = DIRECTION ( 'NONE',  ( -1.073024830501117725E-15, -6.982962677686266711E-15, 1.000000000000000000 ) ) ;
#213715 = AXIS2_PLACEMENT_3D ( 'NONE', #203939, #184366, #5712 ) ;
#213716 = CARTESIAN_POINT ( 'NONE',  ( 20.89192007715127986, 46.45729338110133710, -243.0823073233429170 ) ) ;
#213717 = FACE_OUTER_BOUND ( 'NONE', #82961, .T. ) ;
#213718 = DIRECTION ( 'NONE',  ( 0.000000000000000000, 0.000000000000000000, 1.000000000000000000 ) ) ;
#213719 = VECTOR ( 'NONE', #206905, 999.9999999999998863 ) ;
#213720 = ADVANCED_FACE ( 'NONE', ( #97220 ), #207737, .F. ) ;
#213721 = CARTESIAN_POINT ( 'NONE',  ( 23.14999999999998792, 64.35000000001195986, -103.0231074845244024 ) ) ;
#213722 = DIRECTION ( 'NONE',  ( 0.000000000000000000, -0.4999999999999689138, 0.8660254037844565822 ) ) ;
#213724 = EDGE_CURVE ( 'NONE', #97226, #253940, #118116, .T. ) ;
#213723 = ORIENTED_EDGE ( 'NONE', *, *, #34338, .T. ) ;
#213725 = VERTEX_POINT ( 'NONE', #59385 ) ;
#213726 = EDGE_LOOP ( 'NONE', ( #139191, #78625, #181274, #32226, #170424 ) ) ;
#213727 = CIRCLE ( 'NONE', #109667, 0.09999999999998898659 ) ;
#213728 = DIRECTION ( 'NONE',  ( 0.000000000000000000, 6.982962677686266711E-15, -1.000000000000000000 ) ) ;
#213730 = ORIENTED_EDGE ( 'NONE', *, *, #55266, .T. ) ;
#213729 = CARTESIAN_POINT ( 'NONE',  ( -20.64999999999999858, 71.65000000001180069, -81.87310748452433984 ) ) ;
#213731 = CARTESIAN_POINT ( 'NONE',  ( -23.25000000000000000, 1.115600667400684642E-11, -180.2749999999999773 ) ) ;
#213732 = ORIENTED_EDGE ( 'NONE', *, *, #148267, .F. ) ;
#213733 = CARTESIAN_POINT ( 'NONE',  ( 21.53752568617672836, 6.786807874515049299, -100.4010255387293427 ) ) ;
#213734 = ORIENTED_EDGE ( 'NONE', *, *, #122314, .T. ) ;
#213735 = CARTESIAN_POINT ( 'NONE',  ( -18.39999999999999858, -0.7490476236415750666, -242.2033265267442061 ) ) ;
#213736 = AXIS2_PLACEMENT_3D ( 'NONE', #98218, #113964, #74883 ) ;
#213737 = EDGE_CURVE ( 'NONE', #253488, #179315, #192526, .T. ) ;
#213738 = ORIENTED_EDGE ( 'NONE', *, *, #205814, .F. ) ;
#213739 = CIRCLE ( 'NONE', #101259, 0.1000000000000028644 ) ;
#213740 = CARTESIAN_POINT ( 'NONE',  ( -18.59999999999999787, -1.736257131586239844, -78.56865232901753870 ) ) ;
#213741 = CARTESIAN_POINT ( 'NONE',  ( -21.05000000000000426, 76.10000000001241460, -176.5001745056490847 ) ) ;
#213742 = ADVANCED_FACE ( 'NONE', ( #133825 ), #193811, .T. ) ;
#213744 = ORIENTED_EDGE ( 'NONE', *, *, #118481, .T. ) ;
#213743 = VERTEX_POINT ( 'NONE', #34759 ) ;
#213745 = ORIENTED_EDGE ( 'NONE', *, *, #179060, .T. ) ;
#213746 = CARTESIAN_POINT ( 'NONE',  ( -23.15000000000000213, 27.86742726211138788, -240.0204451158735708 ) ) ;
#213747 = ORIENTED_EDGE ( 'NONE', *, *, #220025, .F. ) ;
#213748 = ORIENTED_EDGE ( 'NONE', *, *, #46197, .F. ) ;
#213750 = PLANE ( 'NONE',  #26202 ) ;
#213749 = AXIS2_PLACEMENT_3D ( 'NONE', #220204, #200638, #42843 ) ;
#213752 = VERTEX_POINT ( 'NONE', #195116 ) ;
#213751 = CARTESIAN_POINT ( 'NONE',  ( 18.41815437325349691, -9.498709853130263170, -107.1039458388021615 ) ) ;
#213753 = CARTESIAN_POINT ( 'NONE',  ( -23.15000000000000213, 87.65000000001192859, -106.0231074845242176 ) ) ;
#213755 = CARTESIAN_POINT ( 'NONE',  ( -23.25000000000000000, 76.00000000001246292, -172.1231074845243540 ) ) ;
#213754 = DIRECTION ( 'NONE',  ( 0.000000000000000000, 0.000000000000000000, 1.000000000000000000 ) ) ;
#213756 = EDGE_CURVE ( 'NONE', #111921, #108159, #36879, .T. ) ;
#213757 = DIRECTION ( 'NONE',  ( 0.000000000000000000, 0.9126074666063660468, 0.4088369013363524762 ) ) ;
#213758 = CARTESIAN_POINT ( 'NONE',  ( 18.46858270002952906, -9.474202674699409243, -74.10202193470389886 ) ) ;
#213759 = CARTESIAN_POINT ( 'NONE',  ( -21.14999999999999858, 75.90220970870321082, -109.2809220950004203 ) ) ;
#213760 = VERTEX_POINT ( 'NONE', #158552 ) ;
#213761 = AXIS2_PLACEMENT_3D ( 'NONE', #31745, #91682, #214204 ) ;
#213762 = AXIS2_PLACEMENT_3D ( 'NONE', #153409, #54249, #176796 ) ;
#213763 = AXIS2_PLACEMENT_3D ( 'NONE', #36269, #33730, #153690 ) ;
#213764 = EDGE_CURVE ( 'NONE', #236044, #52, #70195, .T. ) ;
#213765 = ORIENTED_EDGE ( 'NONE', *, *, #38643, .F. ) ;
#213767 = CIRCLE ( 'NONE', #105401, 0.1000000000000067224 ) ;
#213766 = FACE_OUTER_BOUND ( 'NONE', #61451, .T. ) ;
#213768 = CARTESIAN_POINT ( 'NONE',  ( 20.94999999999999574, 74.83729825007462466, -195.6231074845243540 ) ) ;
#213769 = DIRECTION ( 'NONE',  ( 0.000000000000000000, -1.000000000000000000, 0.000000000000000000 ) ) ;
#213771 = EDGE_CURVE ( 'NONE', #210045, #111477, #99356, .T. ) ;
#213770 = VERTEX_POINT ( 'NONE', #13888 ) ;
#213772 = DIRECTION ( 'NONE',  ( 0.000000000000000000, -0.000000000000000000, 1.000000000000000000 ) ) ;
#213773 = CARTESIAN_POINT ( 'NONE',  ( -23.25000000000000000, 78.48087866980282001, -232.8271061603568910 ) ) ;
#213774 = DIRECTION ( 'NONE',  ( -0.000000000000000000, -0.4721928772777351790, -0.8814952561688427224 ) ) ;
#213775 = VERTEX_POINT ( 'NONE', #33491 ) ;
#213776 = EDGE_LOOP ( 'NONE', ( #165546, #29713, #134766, #225583 ) ) ;
#213777 = DIRECTION ( 'NONE',  ( 0.000000000000000000, -6.982962677686266711E-15, 1.000000000000000000 ) ) ;
#213778 = DIRECTION ( 'NONE',  ( 1.000000000000000000, -0.000000000000000000, -0.000000000000000000 ) ) ;
#213779 = ORIENTED_EDGE ( 'NONE', *, *, #116491, .F. ) ;
#213780 = DIRECTION ( 'NONE',  ( 0.000000000000000000, 0.9893560106964510714, -0.1455152366551481502 ) ) ;
#213781 = VERTEX_POINT ( 'NONE', #173003 ) ;
#213782 = ADVANCED_FACE ( 'NONE', ( #75168 ), #256267, .F. ) ;
#213783 = CARTESIAN_POINT ( 'NONE',  ( -20.54999999999999716, -8.663551401869161950, -9.524101118067305194 ) ) ;
#213785 = CARTESIAN_POINT ( 'NONE',  ( -21.04999999999979821, -1.396821799461749780, -194.6552352087717850 ) ) ;
#213784 = CARTESIAN_POINT ( 'NONE',  ( -23.25000000000000000, 71.65000000001207070, -124.1731074845243228 ) ) ;
#213786 = CARTESIAN_POINT ( 'NONE',  ( 18.49999999999999289, 65.70729864261056719, -164.5657455973725121 ) ) ;
#213788 = ADVANCED_FACE ( 'NONE', ( #95968 ), #132718, .F. ) ;
#213787 = LINE ( 'NONE', #24599, #132749 ) ;
#213789 = CIRCLE ( 'NONE', #134653, 0.09999999999999860389 ) ;
#213790 = AXIS2_PLACEMENT_3D ( 'NONE', #257047, #78447, #240112 ) ;
#213791 = DIRECTION ( 'NONE',  ( -1.000000000000000000, -0.000000000000000000, -0.000000000000000000 ) ) ;
#213792 = AXIS2_PLACEMENT_3D ( 'NONE', #50971, #87541, #251767 ) ;
#213794 = ORIENTED_EDGE ( 'NONE', *, *, #249193, .F. ) ;
#213793 = EDGE_LOOP ( 'NONE', ( #32246, #184484, #244303, #91744 ) ) ;
#213795 = VERTEX_POINT ( 'NONE', #155986 ) ;
#213796 = AXIS2_PLACEMENT_3D ( 'NONE', #89265, #206660, #167559 ) ;
#213797 = DIRECTION ( 'NONE',  ( 1.000000000000000000, 0.000000000000000000, -6.938893903907270030E-14 ) ) ;
#213798 = LINE ( 'NONE', #152578, #19980 ) ;
#213799 = CIRCLE ( 'NONE', #251392, 0.09999999999999939493 ) ;
#213800 = FACE_OUTER_BOUND ( 'NONE', #91467, .T. ) ;
#213802 = CARTESIAN_POINT ( 'NONE',  ( -13.54795643572457919, 66.54933111084433506, -87.96756099431704001 ) ) ;
#213801 = CARTESIAN_POINT ( 'NONE',  ( -16.85312964099708566, 66.08639531794483446, -182.9202917780939970 ) ) ;
#213803 = FACE_OUTER_BOUND ( 'NONE', #250121, .T. ) ;
#213804 = ORIENTED_EDGE ( 'NONE', *, *, #46310, .F. ) ;
#213805 = CIRCLE ( 'NONE', #105623, 12.87500000000000000 ) ;
#213806 = DIRECTION ( 'NONE',  ( 0.000000000000000000, 0.000000000000000000, 1.000000000000000000 ) ) ;
#213807 = VERTEX_POINT ( 'NONE', #77683 ) ;
#213808 = VERTEX_POINT ( 'NONE', #236766 ) ;
#213809 = CARTESIAN_POINT ( 'NONE',  ( 22.39999999999999503, 0.000000000000000000, 7.750000000000007105 ) ) ;
#213810 = AXIS2_PLACEMENT_3D ( 'NONE', #158266, #100767, #98203 ) ;
#213811 = DIRECTION ( 'NONE',  ( 0.000000000000000000, 0.000000000000000000, -1.000000000000000000 ) ) ;
#213812 = CIRCLE ( 'NONE', #176416, 0.1000000000000002831 ) ;
#213813 = AXIS2_PLACEMENT_3D ( 'NONE', #199308, #140596, #101427 ) ;
#213814 = FACE_OUTER_BOUND ( 'NONE', #100147, .T. ) ;
#213815 = AXIS2_PLACEMENT_3D ( 'NONE', #167293, #169883, #250637 ) ;
#213816 = DIRECTION ( 'NONE',  ( 1.000000000000000000, 0.000000000000000000, 0.000000000000000000 ) ) ;
#213817 = CIRCLE ( 'NONE', #1408, 0.09999999999999939493 ) ;
#213818 = CARTESIAN_POINT ( 'NONE',  ( 21.14999999999999503, 55.98745301258800566, -232.8057040749260977 ) ) ;
#213819 = ORIENTED_EDGE ( 'NONE', *, *, #30786, .T. ) ;
#213820 = VERTEX_POINT ( 'NONE', #257564 ) ;
#213821 = CARTESIAN_POINT ( 'NONE',  ( 22.45305468355010703, -0.1008583690885486023, -88.75043287651031676 ) ) ;
#213822 = DIRECTION ( 'NONE',  ( 1.000000000000000000, -3.265361837132813093E-16, -2.280189983783949500E-30 ) ) ;
#213823 = DIRECTION ( 'NONE',  ( 1.000000000000000000, 0.000000000000000000, 0.000000000000000000 ) ) ;
#213824 = DIRECTION ( 'NONE',  ( 1.000000000000000000, 0.000000000000000000, 0.000000000000000000 ) ) ;
#213826 = VECTOR ( 'NONE', #151647, 1000.000000000000000 ) ;
#213825 = LINE ( 'NONE', #36502, #125368 ) ;
#213827 = DIRECTION ( 'NONE',  ( -1.000000000000000000, 0.000000000000000000, -0.000000000000000000 ) ) ;
#213828 = LINE ( 'NONE', #168333, #199934 ) ;
#213830 = FACE_OUTER_BOUND ( 'NONE', #181935, .T. ) ;
#213829 = DIRECTION ( 'NONE',  ( 1.000000000000000000, 0.000000000000000000, 0.000000000000000000 ) ) ;
#213831 = CARTESIAN_POINT ( 'NONE',  ( -22.50000000000000000, 76.00000000001246292, -181.6726782920691505 ) ) ;
#213832 = LINE ( 'NONE', #117305, #166627 ) ;
#213833 = CIRCLE ( 'NONE', #188688, 0.2000000000000057288 ) ;
#213834 = DIRECTION ( 'NONE',  ( 0.000000000000000000, 0.000000000000000000, 1.000000000000000000 ) ) ;
#213835 = LINE ( 'NONE', #229560, #52433 ) ;
#213837 = ORIENTED_EDGE ( 'NONE', *, *, #222801, .T. ) ;
#213836 = CARTESIAN_POINT ( 'NONE',  ( -18.50000000000000000, 52.21971469324220294, -232.5539039185337913 ) ) ;
#213838 = CIRCLE ( 'NONE', #18006, 0.09999999999999939493 ) ;
#213839 = AXIS2_PLACEMENT_3D ( 'NONE', #6484, #245108, #166891 ) ;
#213840 = VECTOR ( 'NONE', #217384, 1000.000000000000114 ) ;
#213841 = DIRECTION ( 'NONE',  ( 1.000000000000000000, -0.000000000000000000, 0.000000000000000000 ) ) ;
#213842 = EDGE_CURVE ( 'NONE', #197295, #102120, #56823, .T. ) ;
#213843 = VERTEX_POINT ( 'NONE', #137655 ) ;
#213844 = LINE ( 'NONE', #194312, #161666 ) ;
#213845 = ADVANCED_FACE ( 'NONE', ( #217196 ), #98502, .F. ) ;
#213846 = EDGE_CURVE ( 'NONE', #144364, #62401, #86880, .T. ) ;
#213847 = DIRECTION ( 'NONE',  ( 0.000000000000000000, -1.000000000000000000, -6.982962677686265922E-15 ) ) ;
#213848 = CARTESIAN_POINT ( 'NONE',  ( 21.13461538461538325, 8.885417037985616773, -45.85000000000000142 ) ) ;
#213849 = CARTESIAN_POINT ( 'NONE',  ( 22.46250603428203618, 0.02114417614996233138, -21.85013690265992281 ) ) ;
#213850 = CIRCLE ( 'NONE', #255302, 0.5000000000000004441 ) ;
#213851 = VECTOR ( 'NONE', #120655, 1000.000000000000000 ) ;
#213852 = MECHANICAL_DESIGN_GEOMETRIC_PRESENTATION_REPRESENTATION (  '', ( #113894 ), #14146 ) ;
#213854 = CARTESIAN_POINT ( 'NONE',  ( -0.8999999999999438449, 67.65000000001120384, -14.06452884076210275 ) ) ;
#213853 = CIRCLE ( 'NONE', #55590, 0.6000000000000033085 ) ;
#213855 = CARTESIAN_POINT ( 'NONE',  ( 18.59999999999999432, 85.48068669529062902, -62.58199231576638510 ) ) ;
#213856 = FACE_OUTER_BOUND ( 'NONE', #51149, .T. ) ;
#213857 = ORIENTED_EDGE ( 'NONE', *, *, #137878, .T. ) ;
#213858 = DIRECTION ( 'NONE',  ( 0.000000000000000000, 0.000000000000000000, -1.000000000000000000 ) ) ;
#213860 = ORIENTED_EDGE ( 'NONE', *, *, #186473, .T. ) ;
#213859 = LINE ( 'NONE', #193024, #26222 ) ;
#213861 = CARTESIAN_POINT ( 'NONE',  ( -18.40000000000000213, 70.35000000001207354, -123.8731074845243398 ) ) ;
#213862 = EDGE_CURVE ( 'NONE', #44729, #17866, #223876, .T. ) ;
#213863 =( BOUNDED_CURVE ( )  B_SPLINE_CURVE ( 3, ( #42110, #43376, #180319, #83737 ),
 .UNSPECIFIED., .F., .F. ) 
 B_SPLINE_CURVE_WITH_KNOTS ( ( 4, 4 ),
 ( 1.570796326794955622, 3.141592653589791784 ),
 .UNSPECIFIED. ) 
 CURVE ( )  GEOMETRIC_REPRESENTATION_ITEM ( )  RATIONAL_B_SPLINE_CURVE ( ( 1.000000000000000000, 0.8047378541243791483, 0.8047378541243791483, 1.000000000000000000 ) ) 
 REPRESENTATION_ITEM ( '' )  );
#213864 = DIRECTION ( 'NONE',  ( -1.000000000000000000, -0.000000000000000000, -0.000000000000000000 ) ) ;
#213865 = DIRECTION ( 'NONE',  ( -1.000000000000000000, -0.000000000000000000, -0.000000000000000000 ) ) ;
#213866 = ORIENTED_EDGE ( 'NONE', *, *, #35868, .T. ) ;
#213867 = APPLICATION_PROTOCOL_DEFINITION ( 'draft international standard', 'automotive_design', 1998, #177321 ) ;
#213868 = LINE ( 'NONE', #114772, #156642 ) ;
#213869 = CARTESIAN_POINT ( 'NONE',  ( 22.49999999999999645, -2.381330705637466405, -189.5959759702857923 ) ) ;
#213870 = EDGE_LOOP ( 'NONE', ( #112899, #200629, #23797, #100266 ) ) ;
#213871 = DIRECTION ( 'NONE',  ( 0.000000000000000000, 0.000000000000000000, -1.000000000000000000 ) ) ;
#213872 = CARTESIAN_POINT ( 'NONE',  ( 18.49999999999999645, 77.16412189325330928, -128.6082593989527254 ) ) ;
#213873 = AXIS2_PLACEMENT_3D ( 'NONE', #171021, #13190, #250494 ) ;
#213874 = LINE ( 'NONE', #19540, #7678 ) ;
#213875 = EDGE_CURVE ( 'NONE', #196680, #228703, #203615, .T. ) ;
#213876 = EDGE_LOOP ( 'NONE', ( #227049, #213713, #231137 ) ) ;
#213877 = EDGE_CURVE ( 'NONE', #39149, #54998, #243187, .T. ) ;
#213878 = EDGE_LOOP ( 'NONE', ( #17442, #219898, #172882, #183254 ) ) ;
#213879 = DIRECTION ( 'NONE',  ( 0.000000000000000000, 0.2617529984165044565, 0.9651348961777151958 ) ) ;
#213880 = CARTESIAN_POINT ( 'NONE',  ( 23.25000000000000000, -8.999999999988844479, -177.3939691226524076 ) ) ;
#213881 = CYLINDRICAL_SURFACE ( 'NONE', #227725, 0.09999999999999939493 ) ;
#213882 = CARTESIAN_POINT ( 'NONE',  ( -21.93642651522410247, 68.67283376068614587, -103.0231074845243739 ) ) ;
#213883 = EDGE_CURVE ( 'NONE', #225653, #78723, #244726, .T. ) ;
#213885 = CARTESIAN_POINT ( 'NONE',  ( -21.45000000000000284, 68.29142135624910281, -81.87310748452436826 ) ) ;
#213884 = CARTESIAN_POINT ( 'NONE',  ( -16.97683809663752186, 66.15000000001231228, -157.3731074845244393 ) ) ;
#213886 = CARTESIAN_POINT ( 'NONE',  ( -20.54999999999999716, 4.768403829798271154, -213.4961173936592331 ) ) ;
#213887 = DIRECTION ( 'NONE',  ( 0.000000000000000000, 8.673617379884087537E-15, 1.000000000000000000 ) ) ;
#213888 = DIRECTION ( 'NONE',  ( 1.000000000000000000, -0.000000000000000000, -0.000000000000000000 ) ) ;
#213890 = LINE ( 'NONE', #92652, #80644 ) ;
#213889 = AXIS2_PLACEMENT_3D ( 'NONE', #70976, #53942, #153092 ) ;
#213891 = ORIENTED_EDGE ( 'NONE', *, *, #130147, .F. ) ;
#213892 = CIRCLE ( 'NONE', #222238, 4.000000000000003553 ) ;
#213893 = ORIENTED_EDGE ( 'NONE', *, *, #218005, .F. ) ;
#213894 = SPHERICAL_SURFACE ( 'NONE', #193710, 0.1000000000000000056 ) ;
#213895 = CARTESIAN_POINT ( 'NONE',  ( 23.14999999999999858, 70.10000000001220144, -146.7422072491807796 ) ) ;
#213898 = CARTESIAN_POINT ( 'NONE',  ( -20.54999999999999716, 76.00000000001172396, -71.52310748452431710 ) ) ;
#213897 = LINE ( 'NONE', #236024, #171352 ) ;
#213896 = AXIS2_PLACEMENT_3D ( 'NONE', #64028, #164423, #159297 ) ;
#213899 = DIRECTION ( 'NONE',  ( -0.000000000000000000, 0.4856429311786307768, 0.8741572761215384846 ) ) ;
#213900 = CARTESIAN_POINT ( 'NONE',  ( -18.59999999999999787, 65.66751761918648356, -63.92826094061123143 ) ) ;
#213901 = FACE_OUTER_BOUND ( 'NONE', #136420, .T. ) ;
#213902 = ORIENTED_EDGE ( 'NONE', *, *, #88581, .T. ) ;
#213903 = EDGE_LOOP ( 'NONE', ( #230896, #32390 ) ) ;
#213904 = EDGE_CURVE ( 'NONE', #9718, #181648, #201491, .T. ) ;
#213906 = CIRCLE ( 'NONE', #30776, 0.1000000000000028644 ) ;
#213905 = CARTESIAN_POINT ( 'NONE',  ( -18.34374000495060386, 64.52683809665015247, -194.2731074845244450 ) ) ;
#213907 = ORIENTED_EDGE ( 'NONE', *, *, #173029, .T. ) ;
#213908 = CARTESIAN_POINT ( 'NONE',  ( -20.94999999999999929, 77.83585931145526615, -58.01866831572577610 ) ) ;
#213909 = AXIS2_PLACEMENT_3D ( 'NONE', #136542, #139089, #201664 ) ;
#213910 = DIRECTION ( 'NONE',  ( 1.000000000000000000, 0.000000000000000000, 0.000000000000000000 ) ) ;
#213912 = CARTESIAN_POINT ( 'NONE',  ( 20.95429402530550433, 8.876194151113340425, -142.5230866979379698 ) ) ;
#213911 = AXIS2_PLACEMENT_3D ( 'NONE', #142297, #1498, #177614 ) ;
#213913 = CIRCLE ( 'NONE', #159748, 0.5999999999999968692 ) ;
#213914 = ADVANCED_FACE ( 'NONE', ( #164943 ), #70374, .F. ) ;
#213915 = EDGE_CURVE ( 'NONE', #24375, #178700, #102364, .T. ) ;
#213916 = ORIENTED_EDGE ( 'NONE', *, *, #219331, .F. ) ;
#213917 = DIRECTION ( 'NONE',  ( -1.000000000000000000, -0.000000000000000000, 0.000000000000000000 ) ) ;
#213918 = EDGE_CURVE ( 'NONE', #149981, #246634, #22892, .T. ) ;
#213920 = ADVANCED_FACE ( 'NONE', ( #183232 ), #2001, .F. ) ;
#213919 = DIRECTION ( 'NONE',  ( 0.000000000000000000, -0.4999999999999949485, 0.8660254037844415942 ) ) ;
#213921 = DIRECTION ( 'NONE',  ( -1.000000000000000000, -0.000000000000000000, -0.000000000000000000 ) ) ;
#213922 = PLANE ( 'NONE',  #57586 ) ;
#213923 = AXIS2_PLACEMENT_3D ( 'NONE', #193914, #171807, #253855 ) ;
#213925 = CARTESIAN_POINT ( 'NONE',  ( 21.78635804494511419, 75.90099493450451007, -143.5587689696774873 ) ) ;
#213924 = CIRCLE ( 'NONE', #76551, 0.1000000000000028644 ) ;
#213926 = CARTESIAN_POINT ( 'NONE',  ( 20.94999999999999929, 1.115600667400684642E-11, -67.00000000000000000 ) ) ;
#213929 = DIRECTION ( 'NONE',  ( 0.000000000000000000, -1.000000000000000000, -6.982962677686265922E-15 ) ) ;
#213928 = CIRCLE ( 'NONE', #72291, 0.2000000000000057288 ) ;
#213927 = DIRECTION ( 'NONE',  ( 0.000000000000000000, 6.982962677686266711E-15, -1.000000000000000000 ) ) ;
#213930 = CARTESIAN_POINT ( 'NONE',  ( -16.88705144915421030, 66.05000000001224691, -149.4540860792365322 ) ) ;
#213931 = EDGE_LOOP ( 'NONE', ( #256721, #52844, #48941, #112645 ) ) ;
#213933 = DIRECTION ( 'NONE',  ( -5.603264701231743991E-32, -7.172728831056617961E-15, 1.000000000000000000 ) ) ;
#213932 = DIRECTION ( 'NONE',  ( 0.000000000000000000, 0.9908441862701605762, 0.1350103645451835310 ) ) ;
#213934 = VERTEX_POINT ( 'NONE', #80230 ) ;
#213936 = ORIENTED_EDGE ( 'NONE', *, *, #95023, .F. ) ;
#213935 = DIRECTION ( 'NONE',  ( 0.000000000000000000, 7.056502275159890043E-15, -1.000000000000000000 ) ) ;
#213937 = EDGE_CURVE ( 'NONE', #7257, #66229, #43714, .T. ) ;
#213938 = VERTEX_POINT ( 'NONE', #81520 ) ;
#213939 = CARTESIAN_POINT ( 'NONE',  ( -16.92778301347272674, 10.00094491684634690, -146.5714818920313860 ) ) ;
#213940 = ADVANCED_FACE ( 'NONE', ( #241902 ), #25447, .F. ) ;
#213941 = DIRECTION ( 'NONE',  ( 6.938893903907222067E-15, -1.000000000000000000, -0.000000000000000000 ) ) ;
#213942 = CARTESIAN_POINT ( 'NONE',  ( -23.25000000000000000, 11.75000000000000000, -21.34999999999999787 ) ) ;
#213943 = AXIS2_PLACEMENT_3D ( 'NONE', #133615, #33278, #112779 ) ;
#213944 = CARTESIAN_POINT ( 'NONE',  ( -16.87036670365549540, 22.88247411645691543, -230.8391385443351567 ) ) ;
#213945 = ORIENTED_EDGE ( 'NONE', *, *, #65551, .F. ) ;
#213946 = DIRECTION ( 'NONE',  ( -0.000000000000000000, -0.000000000000000000, 1.000000000000000000 ) ) ;
#213948 = EDGE_CURVE ( 'NONE', #119315, #18766, #144762, .T. ) ;
#213947 = DIRECTION ( 'NONE',  ( 1.000000000000000000, 0.000000000000000000, 0.000000000000000000 ) ) ;
#213949 = CIRCLE ( 'NONE', #9742, 0.1000000000000028644 ) ;
#213950 = VERTEX_POINT ( 'NONE', #218475 ) ;
#213951 = CIRCLE ( 'NONE', #134809, 11.64999999999999325 ) ;
#213952 = FACE_OUTER_BOUND ( 'NONE', #88792, .T. ) ;
#213953 = AXIS2_PLACEMENT_3D ( 'NONE', #71519, #11534, #51902 ) ;
#213954 = EDGE_CURVE ( 'NONE', #220244, #196380, #4568, .T. ) ;
#213955 = DIRECTION ( 'NONE',  ( -0.000000000000000000, 0.9770955615653313941, 0.2128009952263603677 ) ) ;
#213956 = EDGE_LOOP ( 'NONE', ( #162887, #198841, #149976, #224593 ) ) ;
#213957 = ORIENTED_EDGE ( 'NONE', *, *, #184137, .F. ) ;
#213958 = CARTESIAN_POINT ( 'NONE',  ( -16.92778301347360426, 10.00094491684723685, -188.4285181079673350 ) ) ;
#213959 = EDGE_CURVE ( 'NONE', #199601, #64710, #84068, .T. ) ;
#213960 = EDGE_CURVE ( 'NONE', #215121, #785, #3280, .T. ) ;
#213961 = VERTEX_POINT ( 'NONE', #239351 ) ;
#213962 = CARTESIAN_POINT ( 'NONE',  ( -21.05000000000000071, 76.00000000001267608, -203.5231074845243597 ) ) ;
#213963 = ORIENTED_EDGE ( 'NONE', *, *, #91497, .F. ) ;
#213964 = CARTESIAN_POINT ( 'NONE',  ( 23.14999999999999503, 17.01923898301590654, -224.3994341343041867 ) ) ;
#213965 =( BOUNDED_SURFACE ( )  B_SPLINE_SURFACE ( 3, 2, ( 
 ( #230851, #88723, #247823 ),
 ( #228271, #49619, #208717 ),
 ( #186582, #165741, #189134 ),
 ( #90019, #169619, #249126 ),
 ( #131726, #70506, #26224 ),
 ( #150028, #245264, #36506 ) ),
 .UNSPECIFIED., .F., .F., .T. ) 
 B_SPLINE_SURFACE_WITH_KNOTS ( ( 4, 2, 4 ),
 ( 3, 3 ),
 ( 1.570796326794895448, 2.356194490192343505, 3.141592653589791784 ),
 ( 0.000000000000000000, 1.000000000000000000 ),
 .UNSPECIFIED. ) 
 GEOMETRIC_REPRESENTATION_ITEM ( )  RATIONAL_B_SPLINE_SURFACE ( (
 ( 1.000000000000000000, 0.7071067811865352493, 1.000000000000000000),
 ( 1.000000000000000000, 0.6611148371775361632, 1.000000000000000000),
 ( 1.000000000000000000, 0.6092287576700777807, 1.000000000000000000),
 ( 1.000000000000000000, 0.5278258667052361242, 1.000000000000000000),
 ( 1.000000000000000000, 0.4993418825340519285, 1.000000000000000000),
 ( 1.000000000000000000, 0.4999999999998459010, 1.000000000000000000) ) ) 
 REPRESENTATION_ITEM ( '' )  SURFACE ( )  );
#213966 = EDGE_CURVE ( 'NONE', #156656, #116760, #86492, .T. ) ;
#213967 = CARTESIAN_POINT ( 'NONE',  ( -20.85000000000000142, 43.62273694548321856, -253.2814864317374770 ) ) ;
#213968 = CARTESIAN_POINT ( 'NONE',  ( 0.000000000000000000, -11.65000000000000036, 33.00000000000000000 ) ) ;
#213969 = CARTESIAN_POINT ( 'NONE',  ( -21.05000000000000071, 87.65000000001238334, -170.0231074845242745 ) ) ;
#213970 = ADVANCED_FACE ( 'NONE', ( #163667 ), #224454, .F. ) ;
#213971 = EDGE_CURVE ( 'NONE', #50215, #56908, #248848, .T. ) ;
#213972 = AXIS2_PLACEMENT_3D ( 'NONE', #71228, #154629, #152052 ) ;
#213973 = EDGE_CURVE ( 'NONE', #140135, #178016, #17377, .T. ) ;
#213974 = AXIS2_PLACEMENT_3D ( 'NONE', #116182, #155325, #13230 ) ;
#213975 = CARTESIAN_POINT ( 'NONE',  ( -20.94999999999999929, 1.749999999999999778, -11.66951155790164307 ) ) ;
#213976 = CARTESIAN_POINT ( 'NONE',  ( 18.60000000000000142, -9.480686695267818820, -73.94111516875786094 ) ) ;
#213977 = CARTESIAN_POINT ( 'NONE',  ( 20.94999999999999929, 28.08470566095357057, -239.2860081655328770 ) ) ;
#213978 = ORIENTED_EDGE ( 'NONE', *, *, #3264, .T. ) ;
#213980 = CARTESIAN_POINT ( 'NONE',  ( -20.64999999999999858, 11.41170713998152841, -246.6906184681487559 ) ) ;
#213979 = CARTESIAN_POINT ( 'NONE',  ( 21.08804281139617487, 23.03085422597683163, -230.2011867825314653 ) ) ;
#213981 = ORIENTED_EDGE ( 'NONE', *, *, #179161, .T. ) ;
#213984 = EDGE_LOOP ( 'NONE', ( #106498, #229162, #68148, #75957 ) ) ;
#213983 = DIRECTION ( 'NONE',  ( -0.000000000000000000, -6.982962677686266711E-15, 1.000000000000000000 ) ) ;
#213982 = CARTESIAN_POINT ( 'NONE',  ( 21.05000000000000071, 85.00000000001197975, -112.9170766071766820 ) ) ;
#213985 = ORIENTED_EDGE ( 'NONE', *, *, #239888, .T. ) ;
#213986 = DIRECTION ( 'NONE',  ( 0.000000000000000000, 0.8814952561688434995, -0.4721928772777335137 ) ) ;
#213987 = DIRECTION ( 'NONE',  ( 1.000000000000000000, 0.000000000000000000, 0.000000000000000000 ) ) ;
#213988 = CIRCLE ( 'NONE', #130580, 0.09999999999999491240 ) ;
#213989 = DIRECTION ( 'NONE',  ( 1.000000000000000000, 0.000000000000000000, 0.000000000000000000 ) ) ;
#213990 = CARTESIAN_POINT ( 'NONE',  ( -16.81930730667006202, 9.936998068885202429, -113.2267677305382136 ) ) ;
#213991 = CIRCLE ( 'NONE', #255626, 0.09999999999999939493 ) ;
#213992 = ORIENTED_EDGE ( 'NONE', *, *, #160385, .F. ) ;
#213994 = ORIENTED_EDGE ( 'NONE', *, *, #91271, .F. ) ;
#213993 = DIRECTION ( 'NONE',  ( -0.000000000000000000, -1.000000000000000000, -7.272083257015735086E-15 ) ) ;
#213995 = ADVANCED_FACE ( 'NONE', ( #206639 ), #124512, .T. ) ;
#213996 = AXIS2_PLACEMENT_3D ( 'NONE', #200108, #196243, #239229 ) ;
#213998 = CARTESIAN_POINT ( 'NONE',  ( 21.05000000000000071, -8.999999999988844479, -177.3939691226524076 ) ) ;
#213997 = FACE_OUTER_BOUND ( 'NONE', #35357, .T. ) ;
#214000 = VERTEX_POINT ( 'NONE', #147954 ) ;
#213999 = CARTESIAN_POINT ( 'NONE',  ( 22.48660254037844197, 64.35000000001267040, -203.5731074845244564 ) ) ;
#214001 = VECTOR ( 'NONE', #147040, 1000.000000000000114 ) ;
#214002 = VECTOR ( 'NONE', #211017, 1000.000000000000114 ) ;
#214003 = AXIS2_PLACEMENT_3D ( 'NONE', #143536, #21060, #240086 ) ;
#214004 = ORIENTED_EDGE ( 'NONE', *, *, #246309, .T. ) ;
#214005 = AXIS2_PLACEMENT_3D ( 'NONE', #157614, #237111, #123581 ) ;
#214006 = CARTESIAN_POINT ( 'NONE',  ( 23.24999999999999289, 6.650000000011155876, -146.3500000000000227 ) ) ;
#214007 = CARTESIAN_POINT ( 'NONE',  ( 21.05000000000000071, 67.22371710471941242, -94.46447848938342418 ) ) ;
#214008 = ORIENTED_EDGE ( 'NONE', *, *, #180584, .T. ) ;
#214009 = FACE_OUTER_BOUND ( 'NONE', #91683, .T. ) ;
#214010 = ORIENTED_EDGE ( 'NONE', *, *, #153677, .T. ) ;
#214011 = DIRECTION ( 'NONE',  ( 0.7070776581709139474, 0.7071359030027652981, 2.946958787807621248E-14 ) ) ;
#214012 = FACE_OUTER_BOUND ( 'NONE', #197866, .T. ) ;
#214013 = CIRCLE ( 'NONE', #47389, 0.1000000000000028644 ) ;
#214014 = ORIENTED_EDGE ( 'NONE', *, *, #164497, .T. ) ;
#214015 = CARTESIAN_POINT ( 'NONE',  ( -18.59999999999999787, -1.261786168553869603, -41.58649896354548048 ) ) ;
#214016 = AXIS2_PLACEMENT_3D ( 'NONE', #166622, #42791, #63632 ) ;
#214017 = EDGE_CURVE ( 'NONE', #175552, #54821, #182214, .T. ) ;
#214019 = EDGE_CURVE ( 'NONE', #9515, #139907, #226160, .T. ) ;
#214018 = DIRECTION ( 'NONE',  ( -0.000000000000000000, 6.982962677686266711E-15, -1.000000000000000000 ) ) ;
#214020 = AXIS2_PLACEMENT_3D ( 'NONE', #125841, #202821, #28070 ) ;
#214021 = AXIS2_PLACEMENT_3D ( 'NONE', #194792, #18694, #136045 ) ;
#214022 = ORIENTED_EDGE ( 'NONE', *, *, #133559, .F. ) ;
#214023 = ORIENTED_EDGE ( 'NONE', *, *, #242095, .T. ) ;
#214024 = CARTESIAN_POINT ( 'NONE',  ( 20.86036036209913647, 18.90186385150083836, -227.9902976072726233 ) ) ;
#214025 = EDGE_LOOP ( 'NONE', ( #142974, #40890, #135384, #158517 ) ) ;
#214026 = ADVANCED_FACE ( 'NONE', ( #29328 ), #224899, .F. ) ;
#214027 = ORIENTED_EDGE ( 'NONE', *, *, #175313, .F. ) ;
#214030 = ADVANCED_FACE ( 'NONE', ( #106230 ), #136976, .T. ) ;
#214029 = ORIENTED_EDGE ( 'NONE', *, *, #80659, .T. ) ;
#214028 = DIRECTION ( 'NONE',  ( -1.000000000000000000, -0.000000000000000000, -0.000000000000000000 ) ) ;
#214031 = EDGE_LOOP ( 'NONE', ( #159162, #189533, #116764, #8423 ) ) ;
#214032 = CARTESIAN_POINT ( 'NONE',  ( -20.54999999999999716, 76.00000000001170974, -69.52310748452431710 ) ) ;
#214033 = VERTEX_POINT ( 'NONE', #150528 ) ;
#214036 = EDGE_LOOP ( 'NONE', ( #55892, #86314, #126618, #180849 ) ) ;
#214035 = EDGE_LOOP ( 'NONE', ( #125230, #198060, #86917, #231961 ) ) ;
#214034 = DIRECTION ( 'NONE',  ( 1.000000000000000000, -0.000000000000000000, -0.000000000000000000 ) ) ;
#214037 = ORIENTED_EDGE ( 'NONE', *, *, #98439, .F. ) ;
#214038 = CIRCLE ( 'NONE', #168295, 11.70000000000001528 ) ;
#214039 = AXIS2_PLACEMENT_3D ( 'NONE', #256218, #51642, #136313 ) ;
#214040 = AXIS2_PLACEMENT_3D ( 'NONE', #102405, #21634, #5892 ) ;
#214041 = CARTESIAN_POINT ( 'NONE',  ( 18.49999999999998934, 65.75000000001222134, -145.2731074845244450 ) ) ;
#214042 = ORIENTED_EDGE ( 'NONE', *, *, #35705, .F. ) ;
#214043 = CARTESIAN_POINT ( 'NONE',  ( -16.93211319090181988, 9.999986781168624717, -154.9225054992730861 ) ) ;
#214045 = ORIENTED_EDGE ( 'NONE', *, *, #96917, .F. ) ;
#214044 = DIRECTION ( 'NONE',  ( 0.000000000000000000, -0.000000000000000000, 1.000000000000000000 ) ) ;
#214046 = EDGE_LOOP ( 'NONE', ( #67806, #227899, #62068, #15478 ) ) ;
#214047 = ORIENTED_EDGE ( 'NONE', *, *, #186956, .T. ) ;
#214048 = CARTESIAN_POINT ( 'NONE',  ( 20.73486653747088937, 68.25000000001259082, -194.2731074845244166 ) ) ;
#214049 = CARTESIAN_POINT ( 'NONE',  ( 20.12500000000000000, 66.25000000001161027, -61.41133620241011215 ) ) ;
#214050 = ORIENTED_EDGE ( 'NONE', *, *, #135729, .F. ) ;
#214051 = ORIENTED_EDGE ( 'NONE', *, *, #254475, .T. ) ;
#214052 = CARTESIAN_POINT ( 'NONE',  ( -21.05000000000000071, 36.65892442174935439, -249.5511627012433848 ) ) ;
#214053 = CARTESIAN_POINT ( 'NONE',  ( 23.15000000000000213, -4.892732937820623462, -233.2805462221312496 ) ) ;
#214054 = EDGE_CURVE ( 'NONE', #139621, #38939, #215518, .T. ) ;
#214056 = VERTEX_POINT ( 'NONE', #87946 ) ;
#214055 = EDGE_LOOP ( 'NONE', ( #72227, #99628, #41794, #187353 ) ) ;
#214057 = VECTOR ( 'NONE', #29892, 1000.000000000000000 ) ;
#214058 = ORIENTED_EDGE ( 'NONE', *, *, #115647, .F. ) ;
#214059 = CARTESIAN_POINT ( 'NONE',  ( -20.64999999999999858, 1.115600667400684642E-11, -146.8750000000000000 ) ) ;
#214060 = VERTEX_POINT ( 'NONE', #189650 ) ;
#214061 = VERTEX_POINT ( 'NONE', #149256 ) ;
#214062 = DIRECTION ( 'NONE',  ( 2.952720810173288126E-16, -0.9770955615653313941, -0.2128009952263603677 ) ) ;
#214063 = ORIENTED_EDGE ( 'NONE', *, *, #164578, .T. ) ;
#214064 = FACE_OUTER_BOUND ( 'NONE', #84323, .T. ) ;
#214065 = DIRECTION ( 'NONE',  ( -1.000000000000000000, 0.000000000000000000, 0.000000000000000000 ) ) ;
#214066 = EDGE_CURVE ( 'NONE', #152778, #134706, #190601, .T. ) ;
#214067 = ORIENTED_EDGE ( 'NONE', *, *, #122082, .T. ) ;
#214068 = EDGE_CURVE ( 'NONE', #19594, #167556, #103067, .T. ) ;
#214069 = ORIENTED_EDGE ( 'NONE', *, *, #21887, .F. ) ;
#214070 = DIRECTION ( 'NONE',  ( 0.000000000000000000, -0.9908441862701420355, -0.1350103645453197554 ) ) ;
#214071 = AXIS2_PLACEMENT_3D ( 'NONE', #212735, #232308, #168506 ) ;
#214072 = ORIENTED_EDGE ( 'NONE', *, *, #191902, .F. ) ;
#214073 = CIRCLE ( 'NONE', #168343, 4.000000000000003553 ) ;
#214074 = VECTOR ( 'NONE', #167020, 1000.000000000000000 ) ;
#214075 = CIRCLE ( 'NONE', #118412, 0.09999999999999999167 ) ;
#214076 = EDGE_CURVE ( 'NONE', #94319, #257480, #233991, .T. ) ;
#214077 = FACE_OUTER_BOUND ( 'NONE', #112132, .T. ) ;
#214078 = ORIENTED_EDGE ( 'NONE', *, *, #42809, .F. ) ;
#214079 = VERTEX_POINT ( 'NONE', #188362 ) ;
#214080 = DIRECTION ( 'NONE',  ( 0.000000000000000000, 0.000000000000000000, -1.000000000000000000 ) ) ;
#214083 = ADVANCED_FACE ( 'NONE', ( #207949 ), #187101, .F. ) ;
#214082 = ORIENTED_EDGE ( 'NONE', *, *, #221700, .T. ) ;
#214081 = CARTESIAN_POINT ( 'NONE',  ( -16.97683809663754317, 9.950000000011140600, -120.7284708321106166 ) ) ;
#214084 = DIRECTION ( 'NONE',  ( 1.000000000000000000, -0.000000000000000000, -0.000000000000000000 ) ) ;
#214085 = DIRECTION ( 'NONE',  ( 0.000000000000000000, 0.000000000000000000, 1.000000000000000000 ) ) ;
#214086 = ADVANCED_FACE ( 'NONE', ( #31884 ), #214347, .T. ) ;
#214087 = DIRECTION ( 'NONE',  ( 0.000000000000000000, -0.9126074666063771490, -0.4088369013363276627 ) ) ;
#214088 = DIRECTION ( 'NONE',  ( 1.000000000000000000, 0.000000000000000000, 0.000000000000000000 ) ) ;
#214089 = CARTESIAN_POINT ( 'NONE',  ( 20.94999999999999929, 85.50000000001149658, -45.91707660717669626 ) ) ;
#214090 = DIRECTION ( 'NONE',  ( 0.000000000000000000, -1.265107689135680095E-16, 1.000000000000000000 ) ) ;
#214091 = FACE_OUTER_BOUND ( 'NONE', #23521, .T. ) ;
#214092 = CARTESIAN_POINT ( 'NONE',  ( -21.05000000000000071, 14.05000000001115623, -72.51369507076104526 ) ) ;
#214093 = FACE_OUTER_BOUND ( 'NONE', #13925, .T. ) ;
#214094 = AXIS2_PLACEMENT_3D ( 'NONE', #233544, #95298, #193130 ) ;
#214096 = ADVANCED_FACE ( 'NONE', ( #56524 ), #112683, .T. ) ;
#214095 = CARTESIAN_POINT ( 'NONE',  ( 22.44352723754029810, 75.99072290496894766, -148.1728288298729979 ) ) ;
#214097 = LINE ( 'NONE', #216660, #68250 ) ;
#214098 = AXIS2_PLACEMENT_3D ( 'NONE', #59797, #158956, #117238 ) ;
#214099 = EDGE_LOOP ( 'NONE', ( #101960, #180961, #90977, #179543 ) ) ;
#214100 = AXIS2_PLACEMENT_3D ( 'NONE', #171680, #72561, #230325 ) ;
#214101 = CIRCLE ( 'NONE', #81167, 0.09999999999999939493 ) ;
#214103 = ORIENTED_EDGE ( 'NONE', *, *, #50472, .F. ) ;
#214102 = VERTEX_POINT ( 'NONE', #73582 ) ;
#214105 = ORIENTED_EDGE ( 'NONE', *, *, #240695, .T. ) ;
#214104 = AXIS2_PLACEMENT_3D ( 'NONE', #126661, #164521, #107090 ) ;
#214107 = EDGE_CURVE ( 'NONE', #226140, #199368, #12111, .T. ) ;
#214106 = DIRECTION ( 'NONE',  ( 1.020425574104004196E-15, 1.210927747993693964E-31, -1.000000000000000000 ) ) ;
#214108 = LINE ( 'NONE', #111153, #144442 ) ;
#214110 = CARTESIAN_POINT ( 'NONE',  ( 23.14999999999999147, 76.00000000001213607, -136.5231074845242745 ) ) ;
#214109 = CARTESIAN_POINT ( 'NONE',  ( 21.14999999999999503, -0.09999999998884338825, -155.8504291924551808 ) ) ;
#214111 = ORIENTED_EDGE ( 'NONE', *, *, #177271, .F. ) ;
#214112 = EDGE_LOOP ( 'NONE', ( #168102, #131882, #64688, #57289, #5780, #817, #67419, #62414, #145395, #177718 ) ) ;
#214113 = AXIS2_PLACEMENT_3D ( 'NONE', #29419, #106322, #184596 ) ;
#214114 = CARTESIAN_POINT ( 'NONE',  ( 18.59999999999999076, 10.20857864377385127, -155.3500000000000227 ) ) ;
#214116 = TOROIDAL_SURFACE ( 'NONE', #168371, 12.77499999999999858, 0.1000000000000000056 ) ;
#214115 = SURFACE_SIDE_STYLE ('',( #70779 ) ) ;
#214118 = VECTOR ( 'NONE', #254328, 1000.000000000000000 ) ;
#214117 = CARTESIAN_POINT ( 'NONE',  ( -22.59999999999999787, -3.092988775432913506, -228.1437074281570858 ) ) ;
#214119 = DIRECTION ( 'NONE',  ( -0.000000000000000000, 0.1350103645451859180, 0.9908441862701603542 ) ) ;
#214120 = CARTESIAN_POINT ( 'NONE',  ( -21.05000000000000071, 57.76315019072730905, -226.2583585926041110 ) ) ;
#214122 = ORIENTED_EDGE ( 'NONE', *, *, #186846, .F. ) ;
#214121 = AXIS2_PLACEMENT_3D ( 'NONE', #23834, #102027, #65487 ) ;
#214123 = VERTEX_POINT ( 'NONE', #172702 ) ;
#214124 = SPHERICAL_SURFACE ( 'NONE', #4949, 0.1000000000000000056 ) ;
#214125 = CARTESIAN_POINT ( 'NONE',  ( 18.60000000000001563, 9.036467987174443550, -245.3776959182873156 ) ) ;
#214126 = AXIS2_PLACEMENT_3D ( 'NONE', #45643, #251185, #210798 ) ;
#214127 = EDGE_LOOP ( 'NONE', ( #174004, #180848, #127216, #197013 ) ) ;
#214128 = DIRECTION ( 'NONE',  ( 0.000000000000000000, 0.9651348961777157509, -0.2617529984165028467 ) ) ;
#214129 = FACE_OUTER_BOUND ( 'NONE', #26864, .T. ) ;
#214130 = FACE_OUTER_BOUND ( 'NONE', #29949, .T. ) ;
#214131 = LINE ( 'NONE', #253239, #77376 ) ;
#214132 = CARTESIAN_POINT ( 'NONE',  ( 13.99999999999999822, 62.10905854918434699, -217.1108499610991203 ) ) ;
#214134 = ORIENTED_EDGE ( 'NONE', *, *, #246180, .F. ) ;
#214133 = AXIS2_PLACEMENT_3D ( 'NONE', #31497, #11924, #32786 ) ;
#214135 = LINE ( 'NONE', #18505, #94567 ) ;
#214136 = CARTESIAN_POINT ( 'NONE',  ( -20.85000000000000142, 77.83585931145498193, -24.51866831572578675 ) ) ;
#214137 = CIRCLE ( 'NONE', #201655, 14.20833333333333748 ) ;
#214139 = DIRECTION ( 'NONE',  ( -1.000000000000000000, 0.000000000000000000, 0.000000000000000000 ) ) ;
#214138 = CARTESIAN_POINT ( 'NONE',  ( 20.95512820512820440, 10.62384868372303615, -188.7499999999999716 ) ) ;
#214140 = LINE ( 'NONE', #231156, #224698 ) ;
#214141 = CARTESIAN_POINT ( 'NONE',  ( 21.12230431290519306, 0.005209851700162270761, -27.04243334670699284 ) ) ;
#214142 = DIRECTION ( 'NONE',  ( -0.7071067811865127117, -0.7071067811865821007, 0.000000000000000000 ) ) ;
#214143 = DIRECTION ( 'NONE',  ( 1.000000000000000000, 0.000000000000000000, 0.000000000000000000 ) ) ;
#214144 = ORIENTED_EDGE ( 'NONE', *, *, #61934, .F. ) ;
#214145 = EDGE_CURVE ( 'NONE', #64951, #10686, #98204, .T. ) ;
#214146 = ORIENTED_EDGE ( 'NONE', *, *, #99946, .T. ) ;
#214147 = CARTESIAN_POINT ( 'NONE',  ( -21.05000000000000071, 69.70000000001236629, -169.9231074845244223 ) ) ;
#214148 = ORIENTED_EDGE ( 'NONE', *, *, #124436, .T. ) ;
#214149 = EDGE_CURVE ( 'NONE', #104276, #99797, #203040, .T. ) ;
#214150 = DIRECTION ( 'NONE',  ( 4.377807931758638789E-15, -0.5041370733442360752, -0.8636236514129915776 ) ) ;
#214151 = EDGE_LOOP ( 'NONE', ( #126890, #37902, #143082, #122400, #160535, #252626, #186844, #67431, #67030, #134181, #63606 ) ) ;
#214152 = AXIS2_PLACEMENT_3D ( 'NONE', #178694, #10, #135661 ) ;
#214153 = EDGE_CURVE ( 'NONE', #134395, #117471, #119878, .T. ) ;
#214154 = EDGE_CURVE ( 'NONE', #232695, #66196, #76112, .T. ) ;
#214155 = AXIS2_PLACEMENT_3D ( 'NONE', #31527, #73217, #173628 ) ;
#214156 = EDGE_LOOP ( 'NONE', ( #156541, #213738, #171977, #230750, #36438 ) ) ;
#214157 = VECTOR ( 'NONE', #239606, 1000.000000000000000 ) ;
#214158 = CARTESIAN_POINT ( 'NONE',  ( 21.53752568622107333, 65.35928353583771866, -242.3794047578606410 ) ) ;
#214159 = ORIENTED_EDGE ( 'NONE', *, *, #102892, .T. ) ;
#214160 = DIRECTION ( 'NONE',  ( -0.000000000000000000, -6.982962677686266711E-15, 1.000000000000000000 ) ) ;
#214161 = FACE_OUTER_BOUND ( 'NONE', #18320, .T. ) ;
#214162 = LINE ( 'NONE', #135881, #173658 ) ;
#214163 = AXIS2_PLACEMENT_3D ( 'NONE', #254962, #109413, #226802 ) ;
#214164 = AXIS2_PLACEMENT_3D ( 'NONE', #139024, #120816, #176942 ) ;
#214165 = FACE_OUTER_BOUND ( 'NONE', #138738, .T. ) ;
#214167 = VERTEX_POINT ( 'NONE', #18711 ) ;
#214166 = LINE ( 'NONE', #57637, #109204 ) ;
#214168 = CARTESIAN_POINT ( 'NONE',  ( 19.99999999999998934, 64.35000000001222986, -148.7731074845244450 ) ) ;
#214169 = EDGE_CURVE ( 'NONE', #219313, #70737, #16172, .T. ) ;
#214170 = DIRECTION ( 'NONE',  ( 0.000000000000000000, -0.9654727137038715545, -0.2605042016806676242 ) ) ;
#214171 = DIRECTION ( 'NONE',  ( -0.7071067811865388020, 0.7071067811865561215, 0.000000000000000000 ) ) ;
#214172 = TOROIDAL_SURFACE ( 'NONE', #101708, 11.65000000000000036, 0.1000000000000000056 ) ;
#214173 = CARTESIAN_POINT ( 'NONE',  ( -12.84409460144753545, 9.410682294279107296, -115.9311434419482936 ) ) ;
#214175 = EDGE_CURVE ( 'NONE', #19089, #153900, #123953, .T. ) ;
#214174 = DIRECTION ( 'NONE',  ( 1.000000000000000000, 0.000000000000000000, 0.000000000000000000 ) ) ;
#214176 = VERTEX_POINT ( 'NONE', #151829 ) ;
#214177 = FACE_OUTER_BOUND ( 'NONE', #232942, .T. ) ;
#214178 = AXIS2_PLACEMENT_3D ( 'NONE', #33386, #153340, #232853 ) ;
#214179 = PRODUCT_RELATED_PRODUCT_CATEGORY ( 'part', '', ( #5496 ) ) ;
#214180 = VECTOR ( 'NONE', #92220, 1000.000000000000000 ) ;
#214181 = ORIENTED_EDGE ( 'NONE', *, *, #229620, .F. ) ;
#214182 = CARTESIAN_POINT ( 'NONE',  ( -18.59999999999999787, 64.25000000001152500, -48.17310748452440805 ) ) ;
#214183 = VERTEX_POINT ( 'NONE', #94384 ) ;
#214184 = AXIS2_PLACEMENT_3D ( 'NONE', #17725, #240645, #140238 ) ;
#214185 = DIRECTION ( 'NONE',  ( 0.000000000000000000, 0.000000000000000000, 1.000000000000000000 ) ) ;
#214186 = EDGE_CURVE ( 'NONE', #109477, #212495, #45397, .T. ) ;
#214187 = CARTESIAN_POINT ( 'NONE',  ( -16.94165728009536664, 9.987869755923775017, -20.89105500851019670 ) ) ;
#214188 = DIRECTION ( 'NONE',  ( 1.000000000000000000, -0.000000000000000000, 0.000000000000000000 ) ) ;
#214189 = EDGE_CURVE ( 'NONE', #251285, #213112, #254705, .T. ) ;
#214190 = VERTEX_POINT ( 'NONE', #231358 ) ;
#214191 = ADVANCED_FACE ( 'NONE', ( #136062 ), #233907, .F. ) ;
#214192 = CIRCLE ( 'NONE', #226649, 0.09999999999998898659 ) ;
#214193 = ORIENTED_EDGE ( 'NONE', *, *, #207913, .T. ) ;
#214194 = CARTESIAN_POINT ( 'NONE',  ( 21.14999999999999858, 67.21339244341194785, -124.1731074845243512 ) ) ;
#214196 = CIRCLE ( 'NONE', #14311, 0.1999999999999987899 ) ;
#214195 = CARTESIAN_POINT ( 'NONE',  ( -18.59999999999999787, 30.22839164850006455, -235.6129688350293350 ) ) ;
#214197 = CARTESIAN_POINT ( 'NONE',  ( -16.85697194749134553, 63.05114253962987192, -213.4135404582943067 ) ) ;
#214198 = CARTESIAN_POINT ( 'NONE',  ( -20.94999999999999929, 1.162701749949165642, -75.10000000000003695 ) ) ;
#214199 = EDGE_CURVE ( 'NONE', #91289, #10718, #34459, .T. ) ;
#214201 = DIRECTION ( 'NONE',  ( 1.000000000000000000, 0.000000000000000000, 0.000000000000000000 ) ) ;
#214200 = CARTESIAN_POINT ( 'NONE',  ( -22.39999999999999858, 7.790779598373403836, 0.09999999999999939493 ) ) ;
#214202 = CARTESIAN_POINT ( 'NONE',  ( 23.24999999999999645, 71.00000000001260503, -191.1178414656112921 ) ) ;
#214203 = CARTESIAN_POINT ( 'NONE',  ( 12.30626653967341255, 9.356790025057037496, -50.70482650861389828 ) ) ;
#214204 = DIRECTION ( 'NONE',  ( 0.000000000000000000, 0.000000000000000000, 1.000000000000000000 ) ) ;
#214205 = AXIS2_PLACEMENT_3D ( 'NONE', #117838, #5252, #200917 ) ;
#214206 = EDGE_LOOP ( 'NONE', ( #190105, #52319, #146772, #192824 ) ) ;
#214207 = DIRECTION ( 'NONE',  ( -1.000000000000000000, 0.000000000000000000, 0.000000000000000000 ) ) ;
#214208 = CIRCLE ( 'NONE', #47581, 0.1000000000000005607 ) ;
#214210 = ORIENTED_EDGE ( 'NONE', *, *, #189016, .F. ) ;
#214209 = CARTESIAN_POINT ( 'NONE',  ( -21.05000000000000071, 1.148907358139439339E-11, -201.0000000000015064 ) ) ;
#214211 = VECTOR ( 'NONE', #147846, 1000.000000000000114 ) ;
#214212 = DIRECTION ( 'NONE',  ( 0.000000000000000000, 0.2617529984164955192, 0.9651348961777178603 ) ) ;
#214213 = CARTESIAN_POINT ( 'NONE',  ( 22.49436431346199683, 11.36887822570846041, -198.4555077020579290 ) ) ;
#214215 = DIRECTION ( 'NONE',  ( -0.000000000000000000, 1.000000000000000000, -0.000000000000000000 ) ) ;
#214214 = DIRECTION ( 'NONE',  ( 0.000000000000000000, -0.2617529984165031243, -0.9651348961777157509 ) ) ;
#214217 = EDGE_LOOP ( 'NONE', ( #225151, #247959, #239865, #194706 ) ) ;
#214216 = CARTESIAN_POINT ( 'NONE',  ( 21.07016717456945187, 69.67905916191187998, -136.5231074845243597 ) ) ;
#214219 = CARTESIAN_POINT ( 'NONE',  ( -18.50000000000000000, 43.35377423437995503, -245.1717807829448930 ) ) ;
#214218 = DIRECTION ( 'NONE',  ( 1.836970198721029934E-16, 1.000000000000000000, 6.982962677686266711E-15 ) ) ;
#214220 = DIRECTION ( 'NONE',  ( 0.000000000000000000, 0.000000000000000000, -1.000000000000000000 ) ) ;
#214221 = CARTESIAN_POINT ( 'NONE',  ( -21.05000000000000071, -11.64999999998884306, -64.10000000000000853 ) ) ;
#214222 = DIRECTION ( 'NONE',  ( 0.000000000000000000, 0.000000000000000000, -1.000000000000000000 ) ) ;
#214223 = DIRECTION ( 'NONE',  ( -1.000000000000000000, 0.000000000000000000, 0.000000000000000000 ) ) ;
#214224 = ORIENTED_EDGE ( 'NONE', *, *, #149449, .F. ) ;
#214225 = DIRECTION ( 'NONE',  ( 1.000000000000000000, 0.000000000000000000, 0.000000000000000000 ) ) ;
#214226 = ORIENTED_EDGE ( 'NONE', *, *, #116918, .F. ) ;
#214227 = EDGE_CURVE ( 'NONE', #76729, #130685, #40774, .T. ) ;
#214228 = DIRECTION ( 'NONE',  ( -1.000000000000000000, -0.000000000000000000, -0.000000000000000000 ) ) ;
#214229 = ORIENTED_EDGE ( 'NONE', *, *, #232407, .T. ) ;
#214230 = CARTESIAN_POINT ( 'NONE',  ( 21.15000000000005542, 85.52235250936195143, -34.45408804175119144 ) ) ;
#214231 = CIRCLE ( 'NONE', #101751, 11.80000000000000426 ) ;
#214232 = ORIENTED_EDGE ( 'NONE', *, *, #249232, .F. ) ;
#214233 = DIRECTION ( 'NONE',  ( 1.000000000000000000, 0.000000000000000000, 0.000000000000000000 ) ) ;
#214234 = SPHERICAL_SURFACE ( 'NONE', #166680, 0.1000000000000000056 ) ;
#214235 = EDGE_CURVE ( 'NONE', #223036, #139879, #193514, .T. ) ;
#214236 = AXIS2_PLACEMENT_3D ( 'NONE', #188214, #227332, #9567 ) ;
#214237 = FACE_OUTER_BOUND ( 'NONE', #116853, .T. ) ;
#214238 = ORIENTED_EDGE ( 'NONE', *, *, #169537, .F. ) ;
#214239 = EDGE_CURVE ( 'NONE', #165694, #183114, #175261, .T. ) ;
#214240 = DIRECTION ( 'NONE',  ( 0.000000000000000000, 0.000000000000000000, -1.000000000000000000 ) ) ;
#214241 = CARTESIAN_POINT ( 'NONE',  ( 20.94999999999999929, 16.44800918141279666, -240.8068063186265135 ) ) ;
#214242 = CARTESIAN_POINT ( 'NONE',  ( -21.78635804494510708, 6.853445233358327116, -199.4060668238051051 ) ) ;
#214243 = CARTESIAN_POINT ( 'NONE',  ( 12.30626653967341078, 9.356790025045880199, -17.20482650861389118 ) ) ;
#214244 = DIRECTION ( 'NONE',  ( -1.000000000000000000, -2.952720810173289112E-16, 0.000000000000000000 ) ) ;
#214245 = ORIENTED_EDGE ( 'NONE', *, *, #43549, .F. ) ;
#214246 = LINE ( 'NONE', #215517, #211594 ) ;
#214247 = ORIENTED_EDGE ( 'NONE', *, *, #3728, .T. ) ;
#214249 = ORIENTED_EDGE ( 'NONE', *, *, #49919, .F. ) ;
#214248 = CARTESIAN_POINT ( 'NONE',  ( -17.11825945287481332, 65.95000000001225260, -149.1731074845244223 ) ) ;
#214250 = EDGE_CURVE ( 'NONE', #195640, #92142, #155689, .T. ) ;
#214251 = ORIENTED_EDGE ( 'NONE', *, *, #49665, .T. ) ;
#214252 = TOROIDAL_SURFACE ( 'NONE', #80943, 0.2000000000000000111, 0.1000000000000000056 ) ;
#214253 = CARTESIAN_POINT ( 'NONE',  ( 18.49505832270841310, 85.43802806279552442, -196.3246343096304827 ) ) ;
#214254 = EDGE_CURVE ( 'NONE', #41396, #254122, #176521, .T. ) ;
#214255 = CARTESIAN_POINT ( 'NONE',  ( -16.89060415895971090, 66.04877923721039679, -190.8771872602539474 ) ) ;
#214256 = DIRECTION ( 'NONE',  ( -1.000000000000000000, 0.000000000000000000, 0.000000000000000000 ) ) ;
#214257 = DIRECTION ( 'NONE',  ( 0.000000000000000000, 0.000000000000000000, 1.000000000000000000 ) ) ;
#214258 = ORIENTED_EDGE ( 'NONE', *, *, #27098, .F. ) ;
#214259 = CARTESIAN_POINT ( 'NONE',  ( -18.50000000000000000, 11.65000000001115232, -112.7500000000000284 ) ) ;
#214260 = CARTESIAN_POINT ( 'NONE',  ( -20.94999999999999929, 18.18127959618848521, -237.5711165786817389 ) ) ;
#214261 = ORIENTED_EDGE ( 'NONE', *, *, #14831, .T. ) ;
#214263 = VERTEX_POINT ( 'NONE', #1701 ) ;
#214262 = CARTESIAN_POINT ( 'NONE',  ( 21.05000000000000071, 87.48912529308798014, -106.0231074845242176 ) ) ;
#214264 = DIRECTION ( 'NONE',  ( 0.000000000000000000, -0.1332476588733448597, -0.9910827722268067408 ) ) ;
#214265 = CARTESIAN_POINT ( 'NONE',  ( 18.50000000000000000, -9.399999999988843058, -107.4992856778388841 ) ) ;
#214267 = CIRCLE ( 'NONE', #251676, 4.150000000000000355 ) ;
#214266 = CARTESIAN_POINT ( 'NONE',  ( -16.87683809663752754, 9.865889849343227880, -80.26742680707030786 ) ) ;
#214268 = ORIENTED_EDGE ( 'NONE', *, *, #178252, .F. ) ;
#214269 = CIRCLE ( 'NONE', #76883, 0.09999999999999939493 ) ;
#214270 = EDGE_CURVE ( 'NONE', #157570, #34375, #218168, .T. ) ;
#214271 = VERTEX_POINT ( 'NONE', #223314 ) ;
#214272 = AXIS2_PLACEMENT_3D ( 'NONE', #149179, #228713, #12237 ) ;
#214273 = CARTESIAN_POINT ( 'NONE',  ( -20.94983749550516450, 18.35558276679135048, -236.8903279188150464 ) ) ;
#214274 = ORIENTED_EDGE ( 'NONE', *, *, #214019, .F. ) ;
#214275 = CARTESIAN_POINT ( 'NONE',  ( -23.25000000000000000, 76.00000000001195133, -103.0231074845243171 ) ) ;
#214276 = COLOUR_RGB ( '', 0.40784314, 0.44705882, 0.49803922) ;
#214277 = ADVANCED_FACE ( 'NONE', ( #22579 ), #21312, .T. ) ;
#214278 = CARTESIAN_POINT ( 'NONE',  ( 12.30626653967340900, 66.64320997496565724, -52.31828097591050408 ) ) ;
#214279 = DIRECTION ( 'NONE',  ( 0.000000000000000000, -0.4999999999999949485, 0.8660254037844415942 ) ) ;
#214280 = ADVANCED_FACE ( 'NONE', ( #220768 ), #219785, .F. ) ;
#214281 = AXIS2_PLACEMENT_3D ( 'NONE', #76695, #35059, #156280 ) ;
#214282 = ADVANCED_FACE ( 'NONE', ( #44708 ), #111650, .F. ) ;
#214283 = TOROIDAL_SURFACE ( 'NONE', #210195, 4.149999999999999467, 0.1000000000000000056 ) ;
#214284 = AXIS2_PLACEMENT_3D ( 'NONE', #137033, #54907, #52335 ) ;
#214285 = ORIENTED_EDGE ( 'NONE', *, *, #60303, .F. ) ;
#214286 = CARTESIAN_POINT ( 'NONE',  ( -18.39999999999999858, 64.52683809664961245, -127.2232782360583911 ) ) ;
#214287 = AXIS2_PLACEMENT_3D ( 'NONE', #161657, #102916, #182498 ) ;
#214288 = EDGE_LOOP ( 'NONE', ( #170614, #212535, #98220, #123672 ) ) ;
#214289 = CARTESIAN_POINT ( 'NONE',  ( -23.15000000000000213, 76.00000000001247713, -174.0231074845243882 ) ) ;
#214290 = DIRECTION ( 'NONE',  ( 0.000000000000000000, -1.000000000000000000, 6.308085367188393199E-16 ) ) ;
#214292 = ORIENTED_EDGE ( 'NONE', *, *, #72718, .T. ) ;
#214291 = CARTESIAN_POINT ( 'NONE',  ( 20.27550659511088682, 9.216043722520002035, -180.1499999999999773 ) ) ;
#214294 = EDGE_CURVE ( 'NONE', #103333, #167448, #138623, .T. ) ;
#214293 = LINE ( 'NONE', #154364, #45032 ) ;
#214295 = DIRECTION ( 'NONE',  ( -1.000000000000000000, -0.000000000000000000, 0.000000000000000000 ) ) ;
#214296 = CARTESIAN_POINT ( 'NONE',  ( -20.65000000000000568, 65.08943781962308606, -222.1672656287770451 ) ) ;
#214297 = CARTESIAN_POINT ( 'NONE',  ( 17.74533788810829904, 65.18150020854071158, -46.33673015947196916 ) ) ;
#214298 = EDGE_CURVE ( 'NONE', #229766, #116664, #239046, .T. ) ;
#214299 = CIRCLE ( 'NONE', #139443, 0.1999999999999966804 ) ;
#214300 = AXIS2_PLACEMENT_3D ( 'NONE', #234997, #121494, #135865 ) ;
#214301 = DIRECTION ( 'NONE',  ( 1.000000000000000000, -1.145314911736513664E-16, 3.106193895438251016E-17 ) ) ;
#214302 = AXIS2_PLACEMENT_3D ( 'NONE', #109351, #53256, #11578 ) ;
#214303 = DIRECTION ( 'NONE',  ( 1.000000000000000000, 7.304098846218134667E-16, -4.607487905232622991E-31 ) ) ;
#214305 = ORIENTED_EDGE ( 'NONE', *, *, #124244, .F. ) ;
#214304 = DIRECTION ( 'NONE',  ( 1.000000000000000000, -0.000000000000000000, -0.000000000000000000 ) ) ;
#214306 = CIRCLE ( 'NONE', #201815, 0.1000000000000002692 ) ;
#214307 = AXIS2_PLACEMENT_3D ( 'NONE', #246692, #189306, #70666 ) ;
#214308 = CARTESIAN_POINT ( 'NONE',  ( -22.48660254037843487, 12.58580559757028183, -223.4396719342083770 ) ) ;
#214309 = AXIS2_PLACEMENT_3D ( 'NONE', #56820, #196360, #17709 ) ;
#214310 = CYLINDRICAL_SURFACE ( 'NONE', #128421, 0.09999999999999867328 ) ;
#214311 = CARTESIAN_POINT ( 'NONE',  ( 21.05000000000000071, 5.499999999999998224, -21.09473398108690390 ) ) ;
#214312 = AXIS2_PLACEMENT_3D ( 'NONE', #223927, #47853, #209512 ) ;
#214314 = VERTEX_POINT ( 'NONE', #219463 ) ;
#214313 = CIRCLE ( 'NONE', #201835, 0.09999999999999939493 ) ;
#214315 = DIRECTION ( 'NONE',  ( 1.000000000000000000, 0.000000000000000000, 0.000000000000000000 ) ) ;
#214316 = LINE ( 'NONE', #252140, #222782 ) ;
#214317 = CYLINDRICAL_SURFACE ( 'NONE', #140927, 0.5000000000000004441 ) ;
#214318 = VERTEX_POINT ( 'NONE', #62973 ) ;
#214320 = ADVANCED_FACE ( 'NONE', ( #100768 ), #40876, .F. ) ;
#214319 = DIRECTION ( 'NONE',  ( 1.000000000000000000, 0.000000000000000000, 0.000000000000000000 ) ) ;
#214321 = CARTESIAN_POINT ( 'NONE',  ( 23.24999999999999289, 11.04098673250373785, -220.4458636211660689 ) ) ;
#214322 = ORIENTED_EDGE ( 'NONE', *, *, #235285, .T. ) ;
#214323 = CARTESIAN_POINT ( 'NONE',  ( -17.22767730083325333, 65.65075578754444052, -47.38067879395489967 ) ) ;
#214324 = ORIENTED_EDGE ( 'NONE', *, *, #225399, .T. ) ;
#214325 = DIRECTION ( 'NONE',  ( 0.000000000000000000, -1.000000000000000000, 0.000000000000000000 ) ) ;
#214327 = ORIENTED_EDGE ( 'NONE', *, *, #183739, .T. ) ;
#214326 = CARTESIAN_POINT ( 'NONE',  ( 21.05000000000000071, 6.477552182504828338, -134.0999999652991050 ) ) ;
#214328 = DIRECTION ( 'NONE',  ( -0.000000000000000000, 1.000000000000000000, 6.352154140967427193E-15 ) ) ;
#214329 = ORIENTED_EDGE ( 'NONE', *, *, #58559, .F. ) ;
#214330 = AXIS2_PLACEMENT_3D ( 'NONE', #10310, #166835, #92383 ) ;
#214331 = FACE_OUTER_BOUND ( 'NONE', #43719, .T. ) ;
#214332 = ORIENTED_EDGE ( 'NONE', *, *, #140664, .T. ) ;
#214333 = VECTOR ( 'NONE', #107838, 1000.000000000000000 ) ;
#214335 = ORIENTED_EDGE ( 'NONE', *, *, #81196, .T. ) ;
#214334 = ORIENTED_EDGE ( 'NONE', *, *, #238731, .T. ) ;
#214336 = LINE ( 'NONE', #155680, #115280 ) ;
#214337 = EDGE_LOOP ( 'NONE', ( #73057, #216297, #121417, #243540 ) ) ;
#214338 = EDGE_CURVE ( 'NONE', #122837, #192375, #257329, .T. ) ;
#214339 = CIRCLE ( 'NONE', #10348, 0.1000000000000124678 ) ;
#214340 = DIRECTION ( 'NONE',  ( 0.000000000000000000, 0.000000000000000000, 1.000000000000000000 ) ) ;
#214341 = EDGE_LOOP ( 'NONE', ( #92195, #176742, #122136, #75999 ) ) ;
#214342 = AXIS2_PLACEMENT_3D ( 'NONE', #166874, #215879, #7773 ) ;
#214343 = CIRCLE ( 'NONE', #101885, 0.1000000000000028644 ) ;
#214344 = ORIENTED_EDGE ( 'NONE', *, *, #242295, .F. ) ;
#214345 = DIRECTION ( 'NONE',  ( 8.673617379884085959E-15, -0.8814952561688430555, 0.4721928772777346239 ) ) ;
#214346 = DIRECTION ( 'NONE',  ( 0.000000000000000000, 0.9126074666063660468, 0.4088369013363524762 ) ) ;
#214347 = CYLINDRICAL_SURFACE ( 'NONE', #170347, 0.09999999999999939493 ) ;
#214348 = ORIENTED_EDGE ( 'NONE', *, *, #87131, .T. ) ;
#214349 = CARTESIAN_POINT ( 'NONE',  ( 20.04999999999999716, 19.41435213583508457, -230.3874019357809289 ) ) ;
#214350 = CARTESIAN_POINT ( 'NONE',  ( 21.03675099975490070, 67.12481996722748079, -157.6975653477463766 ) ) ;
#214351 = CARTESIAN_POINT ( 'NONE',  ( -18.40000000000000213, 11.47316190337364183, -191.7499999999999716 ) ) ;
#214352 = AXIS2_PLACEMENT_3D ( 'NONE', #150309, #210282, #233700 ) ;
#214353 = ORIENTED_EDGE ( 'NONE', *, *, #143159, .F. ) ;
#214354 = FACE_OUTER_BOUND ( 'NONE', #153783, .T. ) ;
#214355 = CARTESIAN_POINT ( 'NONE',  ( 20.12500000000000000, 30.46448808713892831, -235.1722212069449256 ) ) ;
#214356 = CARTESIAN_POINT ( 'NONE',  ( 18.39999999999999503, 15.64727632337704222, -218.9309421872099790 ) ) ;
#214357 = VECTOR ( 'NONE', #204147, 1000.000000000000000 ) ;
#214358 = ORIENTED_EDGE ( 'NONE', *, *, #15857, .F. ) ;
#214359 = DIRECTION ( 'NONE',  ( 0.000000000000000000, -0.9651348961777157509, 0.2617529984165031243 ) ) ;
#214360 = EDGE_LOOP ( 'NONE', ( #242562, #251720, #133359, #62078, #147582 ) ) ;
#214361 = ORIENTED_EDGE ( 'NONE', *, *, #73646, .F. ) ;
#214362 = DIRECTION ( 'NONE',  ( 1.000000000000000000, 0.000000000000000000, 0.000000000000000000 ) ) ;
#214363 = ORIENTED_EDGE ( 'NONE', *, *, #198802, .T. ) ;
#214364 = ORIENTED_EDGE ( 'NONE', *, *, #243585, .T. ) ;
#214365 = LINE ( 'NONE', #192253, #244769 ) ;
#214366 = CARTESIAN_POINT ( 'NONE',  ( -16.93234230245721861, 9.998107370558241058, -188.4176902816662107 ) ) ;
#214367 = ORIENTED_EDGE ( 'NONE', *, *, #78306, .T. ) ;
#214368 = AXIS2_PLACEMENT_3D ( 'NONE', #4133, #105778, #86214 ) ;
#214369 = ORIENTED_EDGE ( 'NONE', *, *, #200290, .F. ) ;
#214370 = DIRECTION ( 'NONE',  ( 0.000000000000000000, 0.4999999999999478195, 0.8660254037844686836 ) ) ;
#214371 = DIRECTION ( 'NONE',  ( 0.000000000000000000, -0.2128009952263479332, 0.9770955615653342807 ) ) ;
#214372 = ORIENTED_EDGE ( 'NONE', *, *, #21357, .F. ) ;
#214373 = AXIS2_PLACEMENT_3D ( 'NONE', #197389, #56568, #133573 ) ;
#214374 = ADVANCED_FACE ( 'NONE', ( #82505 ), #203769, .T. ) ;
#214376 = ORIENTED_EDGE ( 'NONE', *, *, #252058, .T. ) ;
#214375 = AXIS2_PLACEMENT_3D ( 'NONE', #168257, #247744, #69131 ) ;
#214377 = TOROIDAL_SURFACE ( 'NONE', #206011, 0.2000000000000000111, 0.1000000000000000056 ) ;
#214378 = DIRECTION ( 'NONE',  ( 0.000000000000000000, 0.5907332058517377193, -0.8068669527896954463 ) ) ;
#214379 = ADVANCED_FACE ( 'NONE', ( #222020 ), #199939, .T. ) ;
#214380 = CARTESIAN_POINT ( 'NONE',  ( -18.79999999999999716, 0.000000000000000000, 33.00000000000000000 ) ) ;
#214381 = ADVANCED_FACE ( 'NONE', ( #43414 ), #64262, .T. ) ;
#214382 = CARTESIAN_POINT ( 'NONE',  ( -20.64999999999999858, 0.000000000000000000, 0.000000000000000000 ) ) ;
#214383 = CARTESIAN_POINT ( 'NONE',  ( -23.15000000000000213, 76.00000000001142553, -36.02310748452432421 ) ) ;
#214384 = CARTESIAN_POINT ( 'NONE',  ( -20.64999999999999858, 1.115625160336667635E-11, -102.5000000000000426 ) ) ;
#214385 = DIRECTION ( 'NONE',  ( -3.265361837132813093E-16, -1.000000000000000000, -6.982962677686266711E-15 ) ) ;
#214386 = DIRECTION ( 'NONE',  ( -0.000000000000000000, 1.000000000000000000, 6.982962677686266711E-15 ) ) ;
#214388 = DIRECTION ( 'NONE',  ( 0.000000000000000000, 0.1350103645451876666, -0.9908441862701600211 ) ) ;
#214387 = CARTESIAN_POINT ( 'NONE',  ( 21.05000000000000071, 76.08559286337361982, -75.93677021939394933 ) ) ;
#214389 = DIRECTION ( 'NONE',  ( -0.000000000000000000, -0.2128009952263604232, 0.9770955615653316162 ) ) ;
#214390 = LINE ( 'NONE', #157013, #177842 ) ;
#214391 = EDGE_CURVE ( 'NONE', #7751, #31598, #124145, .T. ) ;
#214392 = CARTESIAN_POINT ( 'NONE',  ( -20.94999999999999929, 1.162701749949165642, -75.10000000000003695 ) ) ;
#214393 = CARTESIAN_POINT ( 'NONE',  ( 21.05000000000000071, -1.162701749938009677, -8.099999999999999645 ) ) ;
#214394 = EDGE_LOOP ( 'NONE', ( #50103, #122473, #178563, #204573 ) ) ;
#214395 = AXIS2_PLACEMENT_3D ( 'NONE', #150089, #10567, #126650 ) ;
#214397 = EDGE_LOOP ( 'NONE', ( #15523, #94584, #41459, #66688 ) ) ;
#214396 = DIRECTION ( 'NONE',  ( 0.000000000000000000, -1.000000000000000000, 0.000000000000000000 ) ) ;
#214398 = EDGE_CURVE ( 'NONE', #63710, #691, #36678, .T. ) ;
#214399 = DIRECTION ( 'NONE',  ( 0.000000000000000000, -7.026728003956695223E-15, 1.000000000000000000 ) ) ;
#214400 = DIRECTION ( 'NONE',  ( 1.000000000000000000, 0.000000000000000000, 0.000000000000000000 ) ) ;
#214401 = VERTEX_POINT ( 'NONE', #182941 ) ;
#214402 = DIRECTION ( 'NONE',  ( 0.5932847527679310229, 0.8049926720990042694, 6.257843056355992909E-15 ) ) ;
#214403 = CARTESIAN_POINT ( 'NONE',  ( -16.87242674293849731, 9.950000000011138823, -54.35109024637235819 ) ) ;
#214404 = EDGE_LOOP ( 'NONE', ( #56800, #162110, #181288, #80903 ) ) ;
#214406 = CARTESIAN_POINT ( 'NONE',  ( 21.10642757222115407, 60.08602150078414894, -221.2343838615410618 ) ) ;
#214405 = VECTOR ( 'NONE', #187423, 1000.000000000000000 ) ;
#214407 = AXIS2_PLACEMENT_3D ( 'NONE', #45923, #122908, #4216 ) ;
#214408 = PLANE ( 'NONE',  #183871 ) ;
#214409 = CARTESIAN_POINT ( 'NONE',  ( 23.14999999999999858, 5.950000000011160139, -157.1942976949652007 ) ) ;
#214411 = ORIENTED_EDGE ( 'NONE', *, *, #56660, .F. ) ;
#214410 = DIRECTION ( 'NONE',  ( 1.000000000000000000, 0.000000000000000000, 0.000000000000000000 ) ) ;
#214412 = DIRECTION ( 'NONE',  ( 0.000000000000000000, 0.1350103645451904977, -0.9908441862701596881 ) ) ;
#214414 = ORIENTED_EDGE ( 'NONE', *, *, #248374, .T. ) ;
#214413 = DIRECTION ( 'NONE',  ( 1.000000000000000000, 0.000000000000000000, 0.000000000000000000 ) ) ;
#214415 = CARTESIAN_POINT ( 'NONE',  ( 21.00000000000000000, 63.35728523183471594, -212.8904317177587870 ) ) ;
#214416 = CARTESIAN_POINT ( 'NONE',  ( 21.10642757222115407, 10.72315628915859520, -12.24069752378520093 ) ) ;
#214417 = DIRECTION ( 'NONE',  ( 0.000000000000000000, 0.9770955615653316162, 0.2128009952263597848 ) ) ;
#214418 = DIRECTION ( 'NONE',  ( -1.000000000000000000, 0.000000000000000000, -0.000000000000000000 ) ) ;
#214420 = CARTESIAN_POINT ( 'NONE',  ( -18.59999999999999787, 64.35000000001264198, -196.6083017138704179 ) ) ;
#214419 = CARTESIAN_POINT ( 'NONE',  ( -16.83558968593874638, 9.950000000011137047, -154.8376948123833188 ) ) ;
#214421 = CARTESIAN_POINT ( 'NONE',  ( 18.49999999999998934, 53.28269063671665151, -234.9266833317103647 ) ) ;
#214422 = CIRCLE ( 'NONE', #52108, 0.5000000000000004441 ) ;
#214423 = CARTESIAN_POINT ( 'NONE',  ( -21.03922262424653056, 64.37609936600757976, -163.1638994416307469 ) ) ;
#214424 = DIRECTION ( 'NONE',  ( 0.000000000000000000, 0.4721928772777343464, 0.8814952561688431665 ) ) ;
#214425 = AXIS2_PLACEMENT_3D ( 'NONE', #221633, #122575, #202099 ) ;
#214426 = FACE_OUTER_BOUND ( 'NONE', #214775, .T. ) ;
#214427 = CIRCLE ( 'NONE', #231215, 0.09999999999999817368 ) ;
#214428 = ORIENTED_EDGE ( 'NONE', *, *, #72207, .T. ) ;
#214429 = CIRCLE ( 'NONE', #127137, 0.09999999999999939493 ) ;
#214430 = EDGE_CURVE ( 'NONE', #219647, #163114, #215676, .T. ) ;
#214431 = DIRECTION ( 'NONE',  ( -4.391705002472927119E-16, -1.000000000000000000, -7.026728003956683390E-15 ) ) ;
#214432 = ORIENTED_EDGE ( 'NONE', *, *, #187950, .F. ) ;
#214434 = VERTEX_POINT ( 'NONE', #25158 ) ;
#214433 = PRESENTATION_LAYER_ASSIGNMENT (  '', '', ( #143711 ) ) ;
#214435 = CYLINDRICAL_SURFACE ( 'NONE', #173489, 0.09999999999998898659 ) ;
#214436 = FACE_OUTER_BOUND ( 'NONE', #20279, .T. ) ;
#214437 = ORIENTED_EDGE ( 'NONE', *, *, #61458, .T. ) ;
#214438 = EDGE_CURVE ( 'NONE', #199921, #194460, #206346, .T. ) ;
#214439 = EDGE_LOOP ( 'NONE', ( #183259, #2258 ) ) ;
#214440 = CARTESIAN_POINT ( 'NONE',  ( 18.49999999999998934, 69.45000000001149942, -48.37310748452436826 ) ) ;
#214441 = ADVANCED_FACE ( 'NONE', ( #70709, #107233 ), #68114, .T. ) ;
#214442 = VERTEX_POINT ( 'NONE', #6852 ) ;
#214443 = VECTOR ( 'NONE', #204689, 1000.000000000000227 ) ;
#214444 = ORIENTED_EDGE ( 'NONE', *, *, #85405, .F. ) ;
#214445 = DIRECTION ( 'NONE',  ( 0.000000000000000000, 0.9553114395363127009, 0.2956011730204364252 ) ) ;
#214446 = CARTESIAN_POINT ( 'NONE',  ( -23.15000000000000213, 87.39257802171783851, -139.5970570643562212 ) ) ;
#214447 = LINE ( 'NONE', #76217, #26217 ) ;
#214448 = DIRECTION ( 'NONE',  ( 1.000000000000000000, -1.836970198721029934E-16, -1.601412966608202925E-30 ) ) ;
#214449 = EDGE_CURVE ( 'NONE', #61696, #102268, #74090, .T. ) ;
#214451 = LINE ( 'NONE', #151952, #250041 ) ;
#214450 = CARTESIAN_POINT ( 'NONE',  ( -18.52328366898031931, 77.30140549317121668, -241.9095147967482546 ) ) ;
#214452 = CARTESIAN_POINT ( 'NONE',  ( 21.05000000000000071, 75.90220970870296924, -142.7809220950058204 ) ) ;
#214454 = ORIENTED_EDGE ( 'NONE', *, *, #26423, .T. ) ;
#214453 = CARTESIAN_POINT ( 'NONE',  ( -21.05000000000000071, 77.83534155023670564, -158.3679561919613548 ) ) ;
#214456 = CARTESIAN_POINT ( 'NONE',  ( -20.94999999999999929, 36.65892442174935439, -249.5511627012433848 ) ) ;
#214455 = DIRECTION ( 'NONE',  ( -6.938893903907224433E-15, -1.000000000000000000, -6.982962677686266711E-15 ) ) ;
#214457 = DIRECTION ( 'NONE',  ( -1.000000000000000000, 0.000000000000000000, 0.000000000000000000 ) ) ;
#214458 = EDGE_LOOP ( 'NONE', ( #166992, #115879, #21210, #55236 ) ) ;
#214459 = CIRCLE ( 'NONE', #197889, 0.1000000000000026007 ) ;
#214460 = CARTESIAN_POINT ( 'NONE',  ( -16.94445028196807002, 63.05630424923659660, -213.0754291771441729 ) ) ;
#214462 = EDGE_CURVE ( 'NONE', #195525, #167819, #190799, .T. ) ;
#214461 = CARTESIAN_POINT ( 'NONE',  ( -23.25000000000000000, -1.149570369564537842, -141.8159124845019790 ) ) ;
#214463 = AXIS2_PLACEMENT_3D ( 'NONE', #242145, #186032, #42665 ) ;
#214466 = EDGE_CURVE ( 'NONE', #81812, #241878, #107364, .T. ) ;
#214465 = ORIENTED_EDGE ( 'NONE', *, *, #124135, .F. ) ;
#214464 = VECTOR ( 'NONE', #30621, 1000.000000000000000 ) ;
#214467 = AXIS2_PLACEMENT_3D ( 'NONE', #42092, #121630, #62913 ) ;
#214468 = CYLINDRICAL_SURFACE ( 'NONE', #257724, 0.09999999999999939493 ) ;
#214469 = LINE ( 'NONE', #17547, #85917 ) ;
#214470 = CARTESIAN_POINT ( 'NONE',  ( 15.15590539855245744, 66.58931770574392317, -87.59196404257609458 ) ) ;
#214471 = EDGE_LOOP ( 'NONE', ( #69760, #88376, #99348, #165760 ) ) ;
#214472 = VERTEX_POINT ( 'NONE', #86354 ) ;
#214473 = EDGE_CURVE ( 'NONE', #140937, #56169, #140692, .T. ) ;
#214474 = AXIS2_PLACEMENT_3D ( 'NONE', #71317, #231669, #33493 ) ;
#214475 = CARTESIAN_POINT ( 'NONE',  ( -20.94999999999999929, 36.65892442174935439, -249.5511627012433848 ) ) ;
#214476 = AXIS2_PLACEMENT_3D ( 'NONE', #232851, #54181, #11221 ) ;
#214477 = FACE_OUTER_BOUND ( 'NONE', #52044, .T. ) ;
#214478 = DIRECTION ( 'NONE',  ( 0.000000000000000000, -1.000000000000000000, -6.982962677686265922E-15 ) ) ;
#214480 = EDGE_CURVE ( 'NONE', #102037, #146336, #167245, .T. ) ;
#214479 = CARTESIAN_POINT ( 'NONE',  ( -21.14999999999999858, 76.10000000001203091, -114.6726782920691079 ) ) ;
#214481 = ORIENTED_EDGE ( 'NONE', *, *, #11621, .F. ) ;
#214482 = EDGE_CURVE ( 'NONE', #222464, #137276, #26432, .T. ) ;
#214483 = CIRCLE ( 'NONE', #176918, 0.09999999999998898659 ) ;
#214484 = AXIS2_PLACEMENT_3D ( 'NONE', #103928, #220059, #43984 ) ;
#214485 = CARTESIAN_POINT ( 'NONE',  ( -18.50000000000000000, 77.16412189325258453, -28.30825939895270693 ) ) ;
#214486 = CARTESIAN_POINT ( 'NONE',  ( -21.05000000000000071, 87.29603075034701476, -72.57100664418810254 ) ) ;
#214487 = LINE ( 'NONE', #95807, #235842 ) ;
#214488 = CARTESIAN_POINT ( 'NONE',  ( -21.05000000000000071, 0.6713328740235187109, -212.7808875799876205 ) ) ;
#214489 = DIRECTION ( 'NONE',  ( -0.000000000000000000, -0.1686199900910312910, 0.9856811345164826488 ) ) ;
#214491 = ORIENTED_EDGE ( 'NONE', *, *, #215887, .T. ) ;
#214490 = DIRECTION ( 'NONE',  ( 1.000000000000000000, 0.000000000000000000, 0.000000000000000000 ) ) ;
#214492 = CARTESIAN_POINT ( 'NONE',  ( -23.15000000000000213, 1.115600667400684642E-11, -100.5000000000000284 ) ) ;
#214494 = ADVANCED_FACE ( 'NONE', ( #246733 ), #108519, .F. ) ;
#214493 = FACE_OUTER_BOUND ( 'NONE', #37450, .T. ) ;
#214495 = FACE_OUTER_BOUND ( 'NONE', #28144, .T. ) ;
#214496 = CARTESIAN_POINT ( 'NONE',  ( -22.45305610364634674, -0.1008583690875579225, -122.2504328765106294 ) ) ;
#214497 = EDGE_CURVE ( 'NONE', #58688, #59743, #7605, .T. ) ;
#214498 = DIRECTION ( 'NONE',  ( 0.000000000000000000, 8.673617379883787770E-15, -1.000000000000000000 ) ) ;
#214500 = VERTEX_POINT ( 'NONE', #165954 ) ;
#214499 = CARTESIAN_POINT ( 'NONE',  ( -20.85000000000000142, 0.000000000000000000, -33.50000000000000000 ) ) ;
#214501 = LINE ( 'NONE', #176689, #238140 ) ;
#214502 = LINE ( 'NONE', #97088, #238405 ) ;
#214503 = CARTESIAN_POINT ( 'NONE',  ( -20.85000000000000142, 87.75000000001192291, -105.9231074845242091 ) ) ;
#214504 = ORIENTED_EDGE ( 'NONE', *, *, #218127, .F. ) ;
#214505 = AXIS2_PLACEMENT_3D ( 'NONE', #105178, #81777, #21849 ) ;
#214506 = CARTESIAN_POINT ( 'NONE',  ( 23.24999999999999645, 64.17386235947780904, -213.4227319315771183 ) ) ;
#214507 = DIRECTION ( 'NONE',  ( 0.7071067811865475727, 0.7071067811865475727, 4.937700262164531476E-15 ) ) ;
#214509 = AXIS2_PLACEMENT_3D ( 'NONE', #124846, #186100, #86963 ) ;
#214508 = LINE ( 'NONE', #192392, #117025 ) ;
#214510 = EDGE_CURVE ( 'NONE', #25443, #2987, #157479, .T. ) ;
#214511 = CIRCLE ( 'NONE', #185485, 0.1000000000000081657 ) ;
#214512 = DIRECTION ( 'NONE',  ( 0.000000000000000000, -7.056502275159890832E-15, 1.000000000000000000 ) ) ;
#214513 = ORIENTED_EDGE ( 'NONE', *, *, #87388, .T. ) ;
#214514 = ORIENTED_EDGE ( 'NONE', *, *, #177179, .F. ) ;
#214515 = AXIS2_PLACEMENT_3D ( 'NONE', #6821, #4234, #47210 ) ;
#214516 = CYLINDRICAL_SURFACE ( 'NONE', #43342, 0.1000000000000124678 ) ;
#214517 = CARTESIAN_POINT ( 'NONE',  ( -16.97092634996641891, 65.99911103366385134, -115.6532502508221540 ) ) ;
#214518 = CARTESIAN_POINT ( 'NONE',  ( -22.39999999999999858, 64.25000000001215028, -136.5231074845243597 ) ) ;
#214519 = CARTESIAN_POINT ( 'NONE',  ( -20.85000000000000142, 76.00000000001190870, -103.0231074845243029 ) ) ;
#214521 = AXIS2_PLACEMENT_3D ( 'NONE', #53132, #153573, #132683 ) ;
#214520 = DIRECTION ( 'NONE',  ( 0.000000000000000000, 0.000000000000000000, -1.000000000000000000 ) ) ;
#214522 = EDGE_CURVE ( 'NONE', #250290, #74558, #109791, .T. ) ;
#214523 = LINE ( 'NONE', #230242, #129830 ) ;
#214524 = CIRCLE ( 'NONE', #160404, 11.74999999999998757 ) ;
#214525 = CARTESIAN_POINT ( 'NONE',  ( -16.94445028196808778, 9.992063609708889516, -113.1073301784184792 ) ) ;
#214526 = EDGE_CURVE ( 'NONE', #26951, #55509, #169964, .T. ) ;
#214528 = TOROIDAL_SURFACE ( 'NONE', #2144, 2.100000000000002309, 0.1000000000000000056 ) ;
#214527 = PLANE ( 'NONE',  #123589 ) ;
#214529 = VERTEX_POINT ( 'NONE', #185493 ) ;
#214530 = CARTESIAN_POINT ( 'NONE',  ( 22.39999999999999858, 7.790779598384538929, -167.3999999999999773 ) ) ;
#214531 = ADVANCED_FACE ( 'NONE', ( #88940 ), #65852, .T. ) ;
#214532 = ORIENTED_EDGE ( 'NONE', *, *, #163051, .F. ) ;
#214533 = ADVANCED_FACE ( 'NONE', ( #66831 ), #168548, .F. ) ;
#214534 = ORIENTED_EDGE ( 'NONE', *, *, #157397, .F. ) ;
#214535 = FACE_OUTER_BOUND ( 'NONE', #45566, .T. ) ;
#214536 = DIRECTION ( 'NONE',  ( -4.408576920032448588E-17, 0.1350103645451876666, 0.9908441862701600211 ) ) ;
#214537 = FACE_BOUND ( 'NONE', #142851, .T. ) ;
#214540 = EDGE_LOOP ( 'NONE', ( #226896, #12429 ) ) ;
#214539 = CIRCLE ( 'NONE', #10556, 0.1999999999999981515 ) ;
#214538 = CARTESIAN_POINT ( 'NONE',  ( 18.59999999999997655, 1.115600667400684642E-11, -67.00000000000000000 ) ) ;
#214541 = DIRECTION ( 'NONE',  ( 1.000000000000000000, 0.000000000000000000, 0.000000000000000000 ) ) ;
#214543 = ADVANCED_FACE ( 'NONE', ( #30281 ), #90218, .T. ) ;
#214542 = DIRECTION ( 'NONE',  ( 1.000000000000000000, 0.000000000000000000, 0.000000000000000000 ) ) ;
#214544 = CARTESIAN_POINT ( 'NONE',  ( 18.31572054635706692, 85.54847543579069225, -62.67253731977577758 ) ) ;
#214545 = ORIENTED_EDGE ( 'NONE', *, *, #9279, .T. ) ;
#214546 = CARTESIAN_POINT ( 'NONE',  ( 23.24999999999999645, 67.92720994251783395, -214.1870976236629929 ) ) ;
#214547 = FACE_OUTER_BOUND ( 'NONE', #18490, .T. ) ;
#214548 = CARTESIAN_POINT ( 'NONE',  ( 20.73486653747090003, 68.75000000001178080, -82.17310748452436542 ) ) ;
#214549 = CARTESIAN_POINT ( 'NONE',  ( 20.94999999999999929, 64.35000000001176090, -76.36470817442145176 ) ) ;
#214550 = CIRCLE ( 'NONE', #35541, 11.70000000000000284 ) ;
#214551 = EDGE_CURVE ( 'NONE', #44660, #235293, #45013, .T. ) ;
#214552 = EDGE_CURVE ( 'NONE', #117379, #66806, #155386, .T. ) ;
#214553 = VERTEX_POINT ( 'NONE', #236167 ) ;
#214554 = CARTESIAN_POINT ( 'NONE',  ( -16.78569801330232636, 9.947933733124651567, -79.65691290534755353 ) ) ;
#214555 = CARTESIAN_POINT ( 'NONE',  ( -23.25000000000000000, 7.128833340094563376, -233.7327013124401276 ) ) ;
#214556 = ORIENTED_EDGE ( 'NONE', *, *, #233109, .F. ) ;
#214557 = CARTESIAN_POINT ( 'NONE',  ( 21.08198257630413508, 6.336596734026219480, -133.9273566762154246 ) ) ;
#214558 = ADVANCED_FACE ( 'NONE', ( #212770 ), #32879, .T. ) ;
#214559 = DIRECTION ( 'NONE',  ( 1.000000000000000000, 0.000000000000000000, 0.000000000000000000 ) ) ;
#214560 = CARTESIAN_POINT ( 'NONE',  ( -21.14999999999999858, 11.65000000000000036, -0.1000000000000028644 ) ) ;
#214561 = EDGE_LOOP ( 'NONE', ( #135946, #254487, #202777, #91110 ) ) ;
#214562 = CARTESIAN_POINT ( 'NONE',  ( 18.48197441911520400, -9.517954794694846399, -174.3902116422105735 ) ) ;
#214563 = CARTESIAN_POINT ( 'NONE',  ( 21.05000000000000426, 61.06350993105852609, -234.0935366736971162 ) ) ;
#214564 = VERTEX_POINT ( 'NONE', #34158 ) ;
#214565 = ADVANCED_FACE ( 'NONE', ( #57513 ), #7404, .F. ) ;
#214566 = CIRCLE ( 'NONE', #52249, 0.1000000000000028644 ) ;
#214567 = ADVANCED_FACE ( 'NONE', ( #176218 ), #92794, .F. ) ;
#214568 = TOROIDAL_SURFACE ( 'NONE', #243625, 12.97499999999999609, 0.1000000000000000056 ) ;
#214569 = ORIENTED_EDGE ( 'NONE', *, *, #86968, .T. ) ;
#214570 = CARTESIAN_POINT ( 'NONE',  ( -23.25000000000000000, 35.97645343225766368, -235.9694016464868298 ) ) ;
#214571 = DIRECTION ( 'NONE',  ( 0.000000000000000000, 0.2128009952263605897, -0.9770955615653315052 ) ) ;
#214572 = ORIENTED_EDGE ( 'NONE', *, *, #200446, .F. ) ;
#214573 = EDGE_CURVE ( 'NONE', #192382, #116639, #203429, .T. ) ;
#214574 = DIRECTION ( 'NONE',  ( 1.000000000000000000, 0.000000000000000000, 0.000000000000000000 ) ) ;
#214575 = DIRECTION ( 'NONE',  ( 0.000000000000000000, -0.8068669527896844551, -0.5907332058517525963 ) ) ;
#214576 = CARTESIAN_POINT ( 'NONE',  ( -20.90851465518106167, 65.67467670974440352, -130.9531731826884879 ) ) ;
#214577 = DIRECTION ( 'NONE',  ( 1.000000000000000000, 0.000000000000000000, 0.000000000000000000 ) ) ;
#214578 = ADVANCED_FACE ( 'NONE', ( #52379 ), #71973, .F. ) ;
#214579 = DIRECTION ( 'NONE',  ( 0.000000000000000000, 0.8814952561688476074, -0.4721928772777262417 ) ) ;
#214580 = CARTESIAN_POINT ( 'NONE',  ( 13.99999999999999822, 26.54497872210689735, -232.9592037335782209 ) ) ;
#214581 = CYLINDRICAL_SURFACE ( 'NONE', #190574, 0.09999999999999939493 ) ;
#214583 = ORIENTED_EDGE ( 'NONE', *, *, #239759, .T. ) ;
#214582 = DIRECTION ( 'NONE',  ( 0.000000000000000000, 0.000000000000000000, -1.000000000000000000 ) ) ;
#214585 = ORIENTED_EDGE ( 'NONE', *, *, #82310, .T. ) ;
#214584 = CARTESIAN_POINT ( 'NONE',  ( 18.49999999999999645, 77.83585931145498193, -24.51866831572578320 ) ) ;
#214587 = CARTESIAN_POINT ( 'NONE',  ( 22.50000000000000000, 10.70017861337865916, -226.8538937894029743 ) ) ;
#214586 = CARTESIAN_POINT ( 'NONE',  ( -23.15000000000000213, -13.88357498613435936, -191.9982587459959689 ) ) ;
#214589 = ORIENTED_EDGE ( 'NONE', *, *, #180622, .T. ) ;
#214588 = DIRECTION ( 'NONE',  ( 0.000000000000000000, -1.000000000000000000, 8.673617379884043361E-16 ) ) ;
#214590 = ORIENTED_EDGE ( 'NONE', *, *, #55721, .T. ) ;
#214591 = CARTESIAN_POINT ( 'NONE',  ( -18.51024323315077424, 10.31104185824062647, -106.0204516983106373 ) ) ;
#214592 = CARTESIAN_POINT ( 'NONE',  ( 20.94999999999999929, 67.22371710472015138, -194.9644784893834810 ) ) ;
#214593 = AXIS2_PLACEMENT_3D ( 'NONE', #48871, #125834, #127128 ) ;
#214594 = CIRCLE ( 'NONE', #227072, 0.9750000000000036415 ) ;
#214595 = DIRECTION ( 'NONE',  ( 1.000000000000000000, 0.000000000000000000, 0.000000000000000000 ) ) ;
#214596 = DIRECTION ( 'NONE',  ( -0.000000000000000000, 0.9910827722268048534, 0.1332476588733589040 ) ) ;
#214597 = EDGE_CURVE ( 'NONE', #139104, #208826, #107543, .T. ) ;
#214598 = CARTESIAN_POINT ( 'NONE',  ( 20.94999999999999929, 71.00000000001151079, -47.92837350343745584 ) ) ;
#214599 = DIRECTION ( 'NONE',  ( 0.000000000000000000, -0.000000000000000000, -1.000000000000000000 ) ) ;
#214600 = CARTESIAN_POINT ( 'NONE',  ( -20.00857864376270001, 52.21971469324220294, -232.5539039185337913 ) ) ;
#214601 = ADVANCED_FACE ( 'NONE', ( #135772 ), #173689, .T. ) ;
#214602 = ORIENTED_EDGE ( 'NONE', *, *, #244581, .T. ) ;
#214603 = ORIENTED_EDGE ( 'NONE', *, *, #31641, .T. ) ;
#214604 = CARTESIAN_POINT ( 'NONE',  ( -23.15000000000000213, -11.48912529307605546, -30.39999999999999503 ) ) ;
#214605 = AXIS2_PLACEMENT_3D ( 'NONE', #28052, #128409, #150546 ) ;
#214606 = VECTOR ( 'NONE', #126076, 1000.000000000000000 ) ;
#214607 = ORIENTED_EDGE ( 'NONE', *, *, #174259, .F. ) ;
#214608 = CARTESIAN_POINT ( 'NONE',  ( -18.79999999999999716, -1.212568896937008089, -7.800000000000000711 ) ) ;
#214609 = DIRECTION ( 'NONE',  ( -1.000000000000000000, 0.000000000000000000, 0.000000000000000000 ) ) ;
#214610 = VECTOR ( 'NONE', #216729, 1000.000000000000000 ) ;
#214611 = AXIS2_PLACEMENT_3D ( 'NONE', #60079, #155378, #177514 ) ;
#214612 = DIRECTION ( 'NONE',  ( 0.000000000000000000, 0.000000000000000000, -1.000000000000000000 ) ) ;
#214613 = VERTEX_POINT ( 'NONE', #95378 ) ;
#214614 = EDGE_CURVE ( 'NONE', #42982, #34543, #171113, .T. ) ;
#214615 = CARTESIAN_POINT ( 'NONE',  ( -12.25000000000000178, 66.65000000001204228, -119.7731074845243739 ) ) ;
#214616 = ORIENTED_EDGE ( 'NONE', *, *, #132465, .T. ) ;
#214617 = CARTESIAN_POINT ( 'NONE',  ( -23.49999999999994316, 76.00000000001119815, -36.02310748452479316 ) ) ;
#214618 = VERTEX_POINT ( 'NONE', #233617 ) ;
#214619 = DIRECTION ( 'NONE',  ( -3.265361837132813093E-16, -0.9651348961777146407, 0.2617529984165072321 ) ) ;
#214620 = DIRECTION ( 'NONE',  ( -0.000000000000000000, -1.000000000000000000, -0.000000000000000000 ) ) ;
#214621 = ORIENTED_EDGE ( 'NONE', *, *, #128913, .F. ) ;
#214622 = DIRECTION ( 'NONE',  ( 1.000000000000000000, 0.000000000000000000, 0.000000000000000000 ) ) ;
#214624 = ORIENTED_EDGE ( 'NONE', *, *, #249196, .F. ) ;
#214623 = DIRECTION ( 'NONE',  ( 0.000000000000000000, 1.000000000000000000, 0.000000000000000000 ) ) ;
#214625 = EDGE_CURVE ( 'NONE', #247963, #178157, #57652, .T. ) ;
#214626 = FACE_OUTER_BOUND ( 'NONE', #44936, .T. ) ;
#214628 = ORIENTED_EDGE ( 'NONE', *, *, #212981, .T. ) ;
#214627 = AXIS2_PLACEMENT_3D ( 'NONE', #257896, #240959, #42754 ) ;
#214629 = COLOUR_RGB ( '', 0.09019608, 0.27058824, 0.51372549) ;
#214630 = ORIENTED_EDGE ( 'NONE', *, *, #195079, .F. ) ;
#214631 = AXIS2_PLACEMENT_3D ( 'NONE', #6138, #184785, #160122 ) ;
#214632 = CARTESIAN_POINT ( 'NONE',  ( 21.53752568622133978, 0.09897446126636881558, 6.786807874548579811 ) ) ;
#214633 = ORIENTED_EDGE ( 'NONE', *, *, #247672, .F. ) ;
#214634 = AXIS2_PLACEMENT_3D ( 'NONE', #140119, #102257, #85269 ) ;
#214635 = DIRECTION ( 'NONE',  ( 0.000000000000000000, 0.4999999999999348299, -0.8660254037844762331 ) ) ;
#214636 = CARTESIAN_POINT ( 'NONE',  ( 21.05000000000000071, 69.52244781751853964, -69.42310751922482837 ) ) ;
#214637 =( BOUNDED_SURFACE ( )  B_SPLINE_SURFACE ( 3, 2, ( 
 ( #186202, #183638, #4956 ),
 ( #165353, #166665, #200630 ),
 ( #22001, #143204, #144475 ),
 ( #224024, #63671, #45399 ),
 ( #222736, #42836, #44122 ),
 ( #124946, #101474, #27158 ) ),
 .UNSPECIFIED., .F., .F., .F. ) 
 B_SPLINE_SURFACE_WITH_KNOTS ( ( 4, 2, 4 ),
 ( 3, 3 ),
 ( 0.0001342700090130081948, 0.0002909192928057395587, 0.0004475685765984709769 ),
 ( 0.000000000000000000, 1.000000000000000000 ),
 .UNSPECIFIED. ) 
 GEOMETRIC_REPRESENTATION_ITEM ( )  RATIONAL_B_SPLINE_SURFACE ( (
 ( 1.000000000000000000, 0.7250110520819876836, 1.000000000000000000),
 ( 1.000000000000000000, 0.7257599279138178261, 1.000000000000000000),
 ( 1.000000000000000000, 0.7137594617278574249, 1.000000000000000000),
 ( 1.000000000000000000, 0.6959270178815749608, 1.000000000000000000),
 ( 1.000000000000000000, 0.6919879549334437829, 1.000000000000000000),
 ( 1.000000000000000000, 0.7071067811865494601, 1.000000000000000000) ) ) 
 REPRESENTATION_ITEM ( '' )  SURFACE ( )  );
#214638 = FACE_OUTER_BOUND ( 'NONE', #49684, .T. ) ;
#214639 = CARTESIAN_POINT ( 'NONE',  ( -20.94999999999999929, 1.162701749949165642, -41.60000000000000142 ) ) ;
#214640 = VECTOR ( 'NONE', #144969, 1000.000000000000000 ) ;
#214641 = AXIS2_PLACEMENT_3D ( 'NONE', #82427, #19941, #162022 ) ;
#214642 = AXIS2_PLACEMENT_3D ( 'NONE', #12037, #251900, #52405 ) ;
#214643 = CARTESIAN_POINT ( 'NONE',  ( -23.25000000000000000, -11.74999999998884448, -164.4000000000000057 ) ) ;
#214644 = ORIENTED_EDGE ( 'NONE', *, *, #162341, .T. ) ;
#214645 = DIRECTION ( 'NONE',  ( -2.561896900575096011E-15, 0.5907332058517336115, -0.8068669527896984439 ) ) ;
#214646 = CARTESIAN_POINT ( 'NONE',  ( -23.15000000000000213, 11.60000000001115517, -93.57179676972454274 ) ) ;
#214647 = CARTESIAN_POINT ( 'NONE',  ( 18.55807992284871588, 10.32898536001801659, -139.5826683222764757 ) ) ;
#214648 = VERTEX_POINT ( 'NONE', #56227 ) ;
#214649 = CARTESIAN_POINT ( 'NONE',  ( 20.85882249326303040, 68.11287320386161070, -224.1382462126928488 ) ) ;
#214650 = VERTEX_POINT ( 'NONE', #116243 ) ;
#214651 = CARTESIAN_POINT ( 'NONE',  ( 21.05000000000000071, 76.00000000001244871, -170.0231074845243597 ) ) ;
#214652 = ORIENTED_EDGE ( 'NONE', *, *, #106827, .F. ) ;
#214653 = AXIS2_PLACEMENT_3D ( 'NONE', #79934, #143789, #44714 ) ;
#214654 = AXIS2_PLACEMENT_3D ( 'NONE', #38285, #117809, #43416 ) ;
#214655 = DIRECTION ( 'NONE',  ( -1.000000000000000000, 3.265361837132813093E-16, 2.280189983783949500E-30 ) ) ;
#214656 = DIRECTION ( 'NONE',  ( 0.000000000000000000, 0.000000000000000000, -1.000000000000000000 ) ) ;
#214658 = ORIENTED_EDGE ( 'NONE', *, *, #151824, .T. ) ;
#214657 = CARTESIAN_POINT ( 'NONE',  ( -20.00857864376270001, 9.150000000011157653, -155.1500000000000057 ) ) ;
#214659 = FACE_OUTER_BOUND ( 'NONE', #252498, .T. ) ;
#214660 = ORIENTED_EDGE ( 'NONE', *, *, #114701, .T. ) ;
#214661 = AXIS2_PLACEMENT_3D ( 'NONE', #43097, #160501, #20994 ) ;
#214662 = AXIS2_PLACEMENT_3D ( 'NONE', #231623, #133786, #253721 ) ;
#214663 = DIRECTION ( 'NONE',  ( 0.000000000000000000, -0.4721928772777346239, -0.8814952561688430555 ) ) ;
#214664 = EDGE_CURVE ( 'NONE', #154965, #193883, #16006, .T. ) ;
#214665 = CARTESIAN_POINT ( 'NONE',  ( -16.93710578446423654, 9.950000000011137047, -113.4188039837994353 ) ) ;
#214666 = VERTEX_POINT ( 'NONE', #35441 ) ;
#214667 = DIRECTION ( 'NONE',  ( 0.000000000000000000, 0.000000000000000000, -1.000000000000000000 ) ) ;
#214668 = CARTESIAN_POINT ( 'NONE',  ( -22.50000000000088463, -3.119615478075010717, -228.1914279391694720 ) ) ;
#214669 = VERTEX_POINT ( 'NONE', #54939 ) ;
#214670 = CARTESIAN_POINT ( 'NONE',  ( 21.04999999999958149, 10.11149931895240606, -228.1331641884628141 ) ) ;
#214671 = B_SPLINE_CURVE_WITH_KNOTS ( 'NONE', 3,
 ( #129756, #45086, #124628, #167625, #108903, #25536, #204142, #48928, #128478, #208031 ),
 .UNSPECIFIED., .F., .F.,
 ( 4, 2, 2, 2, 4 ),
 ( 0.000000000000000000, 0.0003916577441627133380, 0.0005874866162440714164, 0.0006854010522847114786, 0.0007833154883253517576 ),
 .UNSPECIFIED. ) ;
#214672 = ORIENTED_EDGE ( 'NONE', *, *, #102341, .T. ) ;
#214673 =( BOUNDED_SURFACE ( )  B_SPLINE_SURFACE ( 3, 2, ( 
 ( #84788, #164373, #63982 ),
 ( #161825, #65259, #140964 ),
 ( #144777, #66554, #163100 ),
 ( #26151, #143508, #224333 ),
 ( #43143, #24881, #220496 ),
 ( #104364, #105644, #240056 ),
 ( #241347, #121423, #83507 ),
 ( #62702, #5256, #182660 ) ),
 .UNSPECIFIED., .F., .F., .F. ) 
 B_SPLINE_SURFACE_WITH_KNOTS ( ( 4, 2, 2, 4 ),
 ( 3, 3 ),
 ( 0.0001704874539069910233, 0.0003809798300636633517, 0.0004862260181419994888, 0.0005914722062203356260 ),
 ( 0.000000000000000000, 1.000000000000000000 ),
 .UNSPECIFIED. ) 
 GEOMETRIC_REPRESENTATION_ITEM ( )  RATIONAL_B_SPLINE_SURFACE ( (
 ( 1.000000000000000000, 0.7071067811864942820, 1.000000000000000000),
 ( 1.000000000000000000, 0.7670648383574680818, 1.000000000000000000),
 ( 1.000000000000000000, 0.8204820770254317441, 1.000000000000000000),
 ( 1.000000000000000000, 0.8877218296112791007, 1.000000000000000000),
 ( 1.000000000000000000, 0.9080815932666936874, 1.000000000000000000),
 ( 1.000000000000000000, 0.9395541505860436349, 1.000000000000000000),
 ( 1.000000000000000000, 0.9506520335379957665, 1.000000000000000000),
 ( 1.000000000000000000, 0.9504532311154669788, 1.000000000000000000) ) ) 
 REPRESENTATION_ITEM ( '' )  SURFACE ( )  );
#214674 = CARTESIAN_POINT ( 'NONE',  ( 14.45963434102924161, 9.451541661396667848, -118.9538754988305840 ) ) ;
#214675 = DIRECTION ( 'NONE',  ( 0.000000000000000000, -0.8814952561688430555, 0.4721928772777346239 ) ) ;
#214676 = EDGE_CURVE ( 'NONE', #153832, #134771, #82569, .T. ) ;
#214677 = ADVANCED_FACE ( 'NONE', ( #53680 ), #99339, .T. ) ;
#214679 = ORIENTED_EDGE ( 'NONE', *, *, #245428, .F. ) ;
#214678 = DIRECTION ( 'NONE',  ( 0.000000000000000000, 1.000000000000000000, 0.000000000000000000 ) ) ;
#214680 = AXIS2_PLACEMENT_3D ( 'NONE', #253086, #190581, #150167 ) ;
#214681 = DIRECTION ( 'NONE',  ( 1.000000000000000000, 0.000000000000000000, 0.000000000000000000 ) ) ;
#214682 = DIRECTION ( 'NONE',  ( -1.927189404645529861E-14, 0.9875102702516478370, -0.1575546449569727725 ) ) ;
#214683 = AXIS2_PLACEMENT_3D ( 'NONE', #240620, #238044, #77673 ) ;
#214684 = CARTESIAN_POINT ( 'NONE',  ( -16.93234230245721861, 9.998107370547087314, -20.91769028166625688 ) ) ;
#214686 = CARTESIAN_POINT ( 'NONE',  ( -22.39999999999999858, 76.00000000001246292, -181.6726782920691505 ) ) ;
#214685 = CARTESIAN_POINT ( 'NONE',  ( 20.95346350065193519, 8.887177249185649330, -42.01173194703538627 ) ) ;
#214687 = DIRECTION ( 'NONE',  ( 0.000000000000000000, 0.4859085964047519801, 0.8740096314915323239 ) ) ;
#214688 = CIRCLE ( 'NONE', #210603, 0.09999999999998898659 ) ;
#214689 = CARTESIAN_POINT ( 'NONE',  ( -21.05000000000000071, 55.49311008795314848, -234.6486875357297492 ) ) ;
#214690 = ADVANCED_FACE ( 'NONE', ( #13281 ), #66035, .T. ) ;
#214691 = CARTESIAN_POINT ( 'NONE',  ( 23.15000000000000213, 86.27712145182582049, -209.5223386573213702 ) ) ;
#214692 = DIRECTION ( 'NONE',  ( 0.000000000000000000, -0.1568667991644355497, 0.9876197685951332295 ) ) ;
#214693 = ORIENTED_EDGE ( 'NONE', *, *, #35488, .T. ) ;
#214695 = ORIENTED_EDGE ( 'NONE', *, *, #197351, .T. ) ;
#214694 = AXIS2_PLACEMENT_3D ( 'NONE', #65202, #62652, #86019 ) ;
#214696 = EDGE_CURVE ( 'NONE', #238407, #223496, #149971, .T. ) ;
#214697 = DIRECTION ( 'NONE',  ( 0.000000000000000000, 0.000000000000000000, -1.000000000000000000 ) ) ;
#214700 = VERTEX_POINT ( 'NONE', #221714 ) ;
#214699 = EDGE_CURVE ( 'NONE', #214669, #116070, #163078, .T. ) ;
#214698 = DIRECTION ( 'NONE',  ( 0.000000000000000000, 0.000000000000000000, 1.000000000000000000 ) ) ;
#214701 = VERTEX_POINT ( 'NONE', #78368 ) ;
#214702 = DIRECTION ( 'NONE',  ( 0.000000000000000000, -0.1350103645451945777, 0.9908441862701590219 ) ) ;
#214703 = ORIENTED_EDGE ( 'NONE', *, *, #124780, .T. ) ;
#214704 = ADVANCED_FACE ( 'NONE', ( #43112 ), #121401, .F. ) ;
#214705 = AXIS2_PLACEMENT_3D ( 'NONE', #65584, #126845, #23923 ) ;
#214706 = AXIS2_PLACEMENT_3D ( 'NONE', #42550, #162529, #221180 ) ;
#214707 = EDGE_LOOP ( 'NONE', ( #245142, #248666, #65184, #142658 ) ) ;
#214708 = EDGE_CURVE ( 'NONE', #74571, #123919, #159223, .T. ) ;
#214709 = AXIS2_PLACEMENT_3D ( 'NONE', #9070, #226832, #29946 ) ;
#214710 = DIRECTION ( 'NONE',  ( 0.000000000000000000, -0.2617529984163859957, -0.9651348961777475033 ) ) ;
#214712 = VERTEX_POINT ( 'NONE', #238739 ) ;
#214711 = ORIENTED_EDGE ( 'NONE', *, *, #150607, .F. ) ;
#214713 = ORIENTED_EDGE ( 'NONE', *, *, #184122, .T. ) ;
#214714 = ORIENTED_EDGE ( 'NONE', *, *, #171361, .T. ) ;
#214715 = ORIENTED_EDGE ( 'NONE', *, *, #245377, .T. ) ;
#214716 = DIRECTION ( 'NONE',  ( -1.000000000000000000, 0.000000000000000000, 0.000000000000000000 ) ) ;
#214717 = DIRECTION ( 'NONE',  ( -1.000000000000000000, 0.000000000000000000, -0.000000000000000000 ) ) ;
#214719 = ORIENTED_EDGE ( 'NONE', *, *, #256188, .T. ) ;
#214718 = DIRECTION ( 'NONE',  ( 0.000000000000000000, 1.000000000000000000, 6.352154140967427193E-15 ) ) ;
#214720 = AXIS2_PLACEMENT_3D ( 'NONE', #153803, #76770, #191628 ) ;
#214721 = CARTESIAN_POINT ( 'NONE',  ( 20.52683494730153413, 40.74930916959595351, -237.8782020542120392 ) ) ;
#214722 = CARTESIAN_POINT ( 'NONE',  ( 15.15590539855245211, 12.47889858296947807, -214.0750992090277975 ) ) ;
#214724 = ORIENTED_EDGE ( 'NONE', *, *, #6503, .F. ) ;
#214723 = CARTESIAN_POINT ( 'NONE',  ( 21.05000000000000071, 85.40000000001158753, -59.62913836187181715 ) ) ;
#214725 = DIRECTION ( 'NONE',  ( 7.589415207398576792E-15, 1.000000000000000000, 6.982962677686266711E-15 ) ) ;
#214726 = ORIENTED_EDGE ( 'NONE', *, *, #236653, .F. ) ;
#214727 = CARTESIAN_POINT ( 'NONE',  ( -23.39999999999994529, 77.25000000001119815, -43.92310748452479885 ) ) ;
#214730 = EDGE_CURVE ( 'NONE', #142564, #158004, #186863, .T. ) ;
#214729 = EDGE_LOOP ( 'NONE', ( #196175, #93798, #96749, #123668 ) ) ;
#214728 = CARTESIAN_POINT ( 'NONE',  ( -18.40000000000000213, 64.25000000001202238, -115.6731074845243938 ) ) ;
#214731 = DIRECTION ( 'NONE',  ( -1.000000000000000000, -0.000000000000000000, -0.000000000000000000 ) ) ;
#214732 = CARTESIAN_POINT ( 'NONE',  ( -20.94999999999999929, 1.835341550235567887, -112.1551512925630192 ) ) ;
#214733 = CARTESIAN_POINT ( 'NONE',  ( 23.14999999999999503, 23.34004772283015683, -229.2004250369967338 ) ) ;
#214734 = ORIENTED_EDGE ( 'NONE', *, *, #45737, .T. ) ;
#214736 = CARTESIAN_POINT ( 'NONE',  ( -21.05000000000000071, -1.835341550213255957, -145.5551512925629822 ) ) ;
#214735 = LINE ( 'NONE', #217286, #7232 ) ;
#214737 = CARTESIAN_POINT ( 'NONE',  ( 20.94999999999999929, 76.00000000001213607, -136.5231074845243313 ) ) ;
#214738 = AXIS2_PLACEMENT_3D ( 'NONE', #70462, #129115, #209949 ) ;
#214739 = DIRECTION ( 'NONE',  ( 0.000000000000000000, 1.000000000000000000, 0.000000000000000000 ) ) ;
#214740 = AXIS2_PLACEMENT_3D ( 'NONE', #171337, #117725, #36947 ) ;
#214742 = CARTESIAN_POINT ( 'NONE',  ( -23.25000000000000000, 71.65000000001222702, -148.6731074845243938 ) ) ;
#214741 = VECTOR ( 'NONE', #99954, 1000.000000000000000 ) ;
#214743 = VERTEX_POINT ( 'NONE', #219158 ) ;
#214744 = VERTEX_POINT ( 'NONE', #140933 ) ;
#214745 = ADVANCED_FACE ( 'NONE', ( #58790 ), #202180, .F. ) ;
#214746 = CARTESIAN_POINT ( 'NONE',  ( 23.15000000000000213, 28.56975825374500388, -258.1421690862028413 ) ) ;
#214747 = DIRECTION ( 'NONE',  ( 0.000000000000000000, 0.9887567792719341719, -0.1495327102803664099 ) ) ;
#214748 = VERTEX_POINT ( 'NONE', #157966 ) ;
#214749 = CARTESIAN_POINT ( 'NONE',  ( 21.05000000000000071, -9.000000000000000000, -23.60603087734755690 ) ) ;
#214750 = ORIENTED_EDGE ( 'NONE', *, *, #11716, .T. ) ;
#214751 = CYLINDRICAL_SURFACE ( 'NONE', #69220, 0.1000000000000028644 ) ;
#214752 = DIRECTION ( 'NONE',  ( 1.000000000000000000, 0.000000000000000000, 0.000000000000000000 ) ) ;
#214753 = ORIENTED_EDGE ( 'NONE', *, *, #138034, .F. ) ;
#214754 = DIRECTION ( 'NONE',  ( 0.000000000000000000, 0.2128009952263582305, -0.9770955615653319493 ) ) ;
#214755 = EDGE_CURVE ( 'NONE', #26051, #114106, #211803, .T. ) ;
#214756 = AXIS2_PLACEMENT_3D ( 'NONE', #58875, #216690, #116327 ) ;
#214757 = EDGE_CURVE ( 'NONE', #252099, #60383, #103429, .T. ) ;
#214758 = VERTEX_POINT ( 'NONE', #2679 ) ;
#214759 = ORIENTED_EDGE ( 'NONE', *, *, #233839, .F. ) ;
#214760 = EDGE_LOOP ( 'NONE', ( #213489, #108366, #239396, #227777, #177638 ) ) ;
#214761 = CARTESIAN_POINT ( 'NONE',  ( -20.94999999999999929, 1.148907358139439339E-11, -201.0000000000015064 ) ) ;
#214762 = CARTESIAN_POINT ( 'NONE',  ( 12.25000000000000000, 66.65000000001155911, -52.77310748452440237 ) ) ;
#214763 = AXIS2_PLACEMENT_3D ( 'NONE', #119631, #59610, #199154 ) ;
#214764 = FACE_OUTER_BOUND ( 'NONE', #25781, .T. ) ;
#214765 = DIRECTION ( 'NONE',  ( -2.827886303505248766E-16, 0.8660254037844411501, 0.4999999999999956146 ) ) ;
#214766 = DIRECTION ( 'NONE',  ( 0.000000000000000000, -0.4009882990724537022, 0.9160831752668424643 ) ) ;
#214767 = EDGE_CURVE ( 'NONE', #182610, #244309, #101757, .T. ) ;
#214769 = CARTESIAN_POINT ( 'NONE',  ( 18.59999999999999432, 77.16270174995064224, -195.4231074845243370 ) ) ;
#214768 = DIRECTION ( 'NONE',  ( -0.7071067811865463515, 0.7071067811865487940, 4.178957128135655137E-15 ) ) ;
#214771 = ORIENTED_EDGE ( 'NONE', *, *, #116277, .T. ) ;
#214770 = DIRECTION ( 'NONE',  ( 1.000000000000000000, -0.000000000000000000, -0.000000000000000000 ) ) ;
#214772 = DIRECTION ( 'NONE',  ( 1.000000000000000000, 0.000000000000000000, 0.000000000000000000 ) ) ;
#214773 = ORIENTED_EDGE ( 'NONE', *, *, #41835, .F. ) ;
#214774 = CARTESIAN_POINT ( 'NONE',  ( 21.05000000000000071, 71.00000000001199396, -115.0283735034374359 ) ) ;
#214775 = EDGE_LOOP ( 'NONE', ( #232872, #38379, #119619, #92506 ) ) ;
#214776 = ORIENTED_EDGE ( 'NONE', *, *, #2809, .F. ) ;
#214777 = DIRECTION ( 'NONE',  ( 1.000000000000000000, 3.265361837132813093E-16, -0.000000000000000000 ) ) ;
#214778 = CARTESIAN_POINT ( 'NONE',  ( -16.93909480342659890, 9.993078364812696179, -46.10034701667233037 ) ) ;
#214780 = ADVANCED_FACE ( 'NONE', ( #181354 ), #60086, .T. ) ;
#214779 = FACE_OUTER_BOUND ( 'NONE', #74662, .T. ) ;
#214781 = EDGE_CURVE ( 'NONE', #56204, #26640, #40945, .T. ) ;
#214782 = CARTESIAN_POINT ( 'NONE',  ( 20.95512820512820440, 8.876151316299271343, -75.55862899514100661 ) ) ;
#214783 = CIRCLE ( 'NONE', #31660, 0.1000000000000028644 ) ;
#214784 = AXIS2_PLACEMENT_3D ( 'NONE', #96780, #138479, #115098 ) ;
#214785 = DIRECTION ( 'NONE',  ( -1.000000000000000000, -3.265361837132813093E-16, 0.000000000000000000 ) ) ;
#214786 = ORIENTED_EDGE ( 'NONE', *, *, #91404, .T. ) ;
#214787 = ORIENTED_EDGE ( 'NONE', *, *, #198539, .F. ) ;
#214788 = ADVANCED_FACE ( 'NONE', ( #99203 ), #90986, .F. ) ;
#214789 = DIRECTION ( 'NONE',  ( 0.000000000000000000, -0.8700118002898321601, 0.4930308989875230030 ) ) ;
#214790 = VERTEX_POINT ( 'NONE', #198321 ) ;
#214791 = CARTESIAN_POINT ( 'NONE',  ( -18.50000000000000000, 77.16412189325330928, -128.6082593989527254 ) ) ;
#214792 = CARTESIAN_POINT ( 'NONE',  ( 21.05000000000000071, 5.000000000011153745, -155.0947339810869323 ) ) ;
#214793 = VERTEX_POINT ( 'NONE', #160514 ) ;
#214794 = DIRECTION ( 'NONE',  ( -0.000000000000000000, 0.8660254037844377084, 0.5000000000000016653 ) ) ;
#214795 = DIRECTION ( 'NONE',  ( 1.000000000000000000, 0.000000000000000000, 0.000000000000000000 ) ) ;
#214796 = CARTESIAN_POINT ( 'NONE',  ( 21.06280952165552023, 65.37286769941131581, -157.8190535977451248 ) ) ;
#214797 = ORIENTED_EDGE ( 'NONE', *, *, #223124, .T. ) ;
#214798 = DIRECTION ( 'NONE',  ( 0.000000000000000000, 0.000000000000000000, -1.000000000000000000 ) ) ;
#214799 = LINE ( 'NONE', #32356, #108092 ) ;
#214800 = AXIS2_PLACEMENT_3D ( 'NONE', #127792, #9124, #249031 ) ;
#214801 = CARTESIAN_POINT ( 'NONE',  ( -20.65000000000000568, 5.650000000011139001, -109.7500000000000426 ) ) ;
#214802 = AXIS2_PLACEMENT_3D ( 'NONE', #108984, #8621, #25618 ) ;
#214803 = CIRCLE ( 'NONE', #160678, 0.09999999999999134581 ) ;
#214804 = ORIENTED_EDGE ( 'NONE', *, *, #110469, .T. ) ;
#214805 = CARTESIAN_POINT ( 'NONE',  ( 20.85000000000000142, 79.19526988099229925, -196.1889237952725296 ) ) ;
#214806 = ORIENTED_EDGE ( 'NONE', *, *, #226020, .T. ) ;
#214807 = EDGE_CURVE ( 'NONE', #133804, #243786, #257516, .T. ) ;
#214808 = CARTESIAN_POINT ( 'NONE',  ( -21.65000000000000213, 65.95000000001201101, -115.6731074845243796 ) ) ;
#214809 = ADVANCED_FACE ( 'NONE', ( #166942 ), #45189, .T. ) ;
#214810 = LINE ( 'NONE', #101233, #162688 ) ;
#214811 = CYLINDRICAL_SURFACE ( 'NONE', #42175, 0.09999999999999939493 ) ;
#214812 = CARTESIAN_POINT ( 'NONE',  ( -15.55912972643740488, 64.52016466995087285, -213.4130396782846901 ) ) ;
#214813 = DIRECTION ( 'NONE',  ( 0.000000000000000000, -1.000000000000000000, -6.352154140967427193E-15 ) ) ;
#214814 = FACE_OUTER_BOUND ( 'NONE', #13642, .T. ) ;
#214815 = ORIENTED_EDGE ( 'NONE', *, *, #143200, .T. ) ;
#214816 = CARTESIAN_POINT ( 'NONE',  ( -17.01764560440413376, 66.05000000001224691, -149.2731074837355436 ) ) ;
#214817 = CARTESIAN_POINT ( 'NONE',  ( 21.05995757104869526, 67.22461075529079721, -124.3282023615331440 ) ) ;
#214818 = LINE ( 'NONE', #253938, #254726 ) ;
#214819 = EDGE_CURVE ( 'NONE', #171180, #96601, #195064, .T. ) ;
#214820 = VECTOR ( 'NONE', #111712, 1000.000000000000000 ) ;
#214821 =( GEOMETRIC_REPRESENTATION_CONTEXT ( 3 ) GLOBAL_UNCERTAINTY_ASSIGNED_CONTEXT ( ( #128645 ) ) GLOBAL_UNIT_ASSIGNED_CONTEXT ( ( #93169, #176587, #210562 ) ) REPRESENTATION_CONTEXT ( 'NONE', 'WORKASPACE' ) );
#214822 = ORIENTED_EDGE ( 'NONE', *, *, #61522, .F. ) ;
#214823 = EDGE_LOOP ( 'NONE', ( #122402, #124605, #143226, #139287 ) ) ;
#214824 = FACE_OUTER_BOUND ( 'NONE', #25520, .T. ) ;
#214826 = B_SPLINE_CURVE_WITH_KNOTS ( 'NONE', 3,
 ( #173879, #215513, #151729, #135966, #14785, #176420, #13482, #31786, #94281, #253357, #93004, #130844, #74770 ),
 .UNSPECIFIED., .F., .F.,
 ( 4, 3, 3, 3, 4 ),
 ( -3.224855718275878119E-06, 0.000000000000000000, 6.199515528664636366E-06, 4.034952380127537373E-05, 7.452715123699773787E-05 ),
 .UNSPECIFIED. ) ;
#214825 = CARTESIAN_POINT ( 'NONE',  ( -18.39999999999999858, 85.50000000001209344, -129.4910380878245633 ) ) ;
#214827 = CARTESIAN_POINT ( 'NONE',  ( -16.92507428761700439, 66.05000000001261640, -190.8097100249028699 ) ) ;
#214828 = DIRECTION ( 'NONE',  ( 0.000000000000000000, 1.000000000000000000, 6.982962677686267499E-15 ) ) ;
#214829 = DIRECTION ( 'NONE',  ( -1.000000000000000000, 0.000000000000000000, 0.000000000000000000 ) ) ;
#214830 = AXIS2_PLACEMENT_3D ( 'NONE', #101964, #220668, #202384 ) ;
#214831 = ORIENTED_EDGE ( 'NONE', *, *, #92233, .T. ) ;
#214832 = CARTESIAN_POINT ( 'NONE',  ( 20.94999999999999574, 10.42338541492406279, -74.49205192387015018 ) ) ;
#214833 = TOROIDAL_SURFACE ( 'NONE', #69113, 0.2000000000000000111, 0.1000000000000000056 ) ;
#214834 = ITEM_DEFINED_TRANSFORMATION ( 'NONE', 'NONE', #123598,  #2425 ) ;
#214835 = AXIS2_PLACEMENT_3D ( 'NONE', #49551, #11727, #251599 ) ;
#214836 = B_SPLINE_CURVE_WITH_KNOTS ( 'NONE', 3,
 ( #240947, #163983, #40205, #238364, #62304, #144374, #199259, #80549, #160147, #141831, #42737, #222636, #179699, #178431, #143105, #122283 ),
 .UNSPECIFIED., .F., .F.,
 ( 4, 3, 3, 3, 3, 4 ),
 ( 0.000000000000000000, 1.810570668010275846E-05, 2.740575833571578222E-05, 4.256816319435761416E-05, 5.213463471025089587E-05, 6.641585710717965742E-05 ),
 .UNSPECIFIED. ) ;
#214837 = LINE ( 'NONE', #34962, #221465 ) ;
#214838 = ORIENTED_EDGE ( 'NONE', *, *, #147764, .F. ) ;
#214839 = CARTESIAN_POINT ( 'NONE',  ( 20.94999999999999929, 67.44464249442897597, -214.0562211244547655 ) ) ;
#214840 = CARTESIAN_POINT ( 'NONE',  ( 23.25000000000000000, -11.74999999999999112, 11.75000000000000000 ) ) ;
#214841 = EDGE_CURVE ( 'NONE', #240562, #181952, #84758, .T. ) ;
#214842 = VERTEX_POINT ( 'NONE', #164350 ) ;
#214844 = TOROIDAL_SURFACE ( 'NONE', #60704, 7.800000000000000711, 0.1000000000000000056 ) ;
#214843 = CARTESIAN_POINT ( 'NONE',  ( -21.12844524849339223, 12.95013890645382837, -205.2458600636644519 ) ) ;
#214845 = EDGE_CURVE ( 'NONE', #65949, #146046, #20267, .T. ) ;
#214846 = ORIENTED_EDGE ( 'NONE', *, *, #95635, .F. ) ;
#214847 = CARTESIAN_POINT ( 'NONE',  ( -21.07954763557422595, 75.93412408139332115, -75.85239847456186624 ) ) ;
#214848 = VECTOR ( 'NONE', #118676, 1000.000000000000000 ) ;
#214849 = CARTESIAN_POINT ( 'NONE',  ( 23.14999999999999503, 6.650000000011155876, -112.6500000000000341 ) ) ;
#214850 = CARTESIAN_POINT ( 'NONE',  ( 20.99999999999999645, 9.750000000011137757, -146.6500000000000341 ) ) ;
#214851 = CIRCLE ( 'NONE', #169106, 0.1000000000000046685 ) ;
#214852 = CARTESIAN_POINT ( 'NONE',  ( -18.50000000000000000, 9.350000000011156942, -146.3500000000000227 ) ) ;
#214853 = CARTESIAN_POINT ( 'NONE',  ( -23.25000000000000000, 67.23127455305841238, -235.8551265064783991 ) ) ;
#214855 = ADVANCED_FACE ( 'NONE', ( #143482 ), #88939, .T. ) ;
#214854 = FACE_OUTER_BOUND ( 'NONE', #113722, .T. ) ;
#214856 = CARTESIAN_POINT ( 'NONE',  ( -21.05000000000000071, 74.83729825007360148, -61.42310748452432989 ) ) ;
#214857 = CARTESIAN_POINT ( 'NONE',  ( 23.15000000000000213, 28.42524210734032408, -258.3567845160494585 ) ) ;
#214858 = CARTESIAN_POINT ( 'NONE',  ( 21.05000000000000071, 77.83534155023671985, -158.4679561919613491 ) ) ;
#214859 = CARTESIAN_POINT ( 'NONE',  ( 18.47654891039378811, -7.732063376463896631, -209.9769793578955728 ) ) ;
#214860 = EDGE_CURVE ( 'NONE', #213808, #30344, #187768, .T. ) ;
#214861 = CARTESIAN_POINT ( 'NONE',  ( 18.39999999999999858, -9.499999999988842703, -207.9146583429696307 ) ) ;
#214862 = DIRECTION ( 'NONE',  ( 0.000000000000000000, 0.9999631594459053030, 0.008583690987162899758 ) ) ;
#214863 = CARTESIAN_POINT ( 'NONE',  ( 18.55807992284871588, 10.32898536001801659, -206.5826683222763904 ) ) ;
#214864 = ORIENTED_EDGE ( 'NONE', *, *, #24580, .T. ) ;
#214865 = CARTESIAN_POINT ( 'NONE',  ( 21.12400247839502754, 10.72148804404156586, -79.25000000000005684 ) ) ;
#214866 = DIRECTION ( 'NONE',  ( -1.000000000000000000, 0.000000000000000000, 0.000000000000000000 ) ) ;
#214867 = EDGE_CURVE ( 'NONE', #124485, #145626, #249219, .T. ) ;
#214869 = EDGE_CURVE ( 'NONE', #122630, #128703, #24858, .T. ) ;
#214868 = EDGE_CURVE ( 'NONE', #1028, #56540, #126492, .T. ) ;
#214870 = ORIENTED_EDGE ( 'NONE', *, *, #51727, .T. ) ;
#214871 = CARTESIAN_POINT ( 'NONE',  ( -23.25000000000000000, 76.00000000001237765, -170.0231074845243597 ) ) ;
#214872 = DIRECTION ( 'NONE',  ( 1.000000000000000000, 0.000000000000000000, 0.000000000000000000 ) ) ;
#214873 = CARTESIAN_POINT ( 'NONE',  ( -18.59999999999999787, 66.75000000001179501, -81.87310748452438247 ) ) ;
#214874 = ORIENTED_EDGE ( 'NONE', *, *, #251384, .F. ) ;
#214875 = AXIS2_PLACEMENT_3D ( 'NONE', #110716, #190267, #93717 ) ;
#214876 = AXIS2_PLACEMENT_3D ( 'NONE', #107221, #248016, #87647 ) ;
#214877 = DIRECTION ( 'NONE',  ( -0.7071067811865456854, 0.7071067811865493491, 0.000000000000000000 ) ) ;
#214878 = ORIENTED_EDGE ( 'NONE', *, *, #116698, .F. ) ;
#214880 = CIRCLE ( 'NONE', #252458, 0.1000000000000028644 ) ;
#214879 = DIRECTION ( 'NONE',  ( 0.000000000000000000, 0.9126074666063772600, 0.4088369013363277182 ) ) ;
#214881 = FACE_OUTER_BOUND ( 'NONE', #113217, .T. ) ;
#214882 = AXIS2_PLACEMENT_3D ( 'NONE', #68399, #65820, #166246 ) ;
#214883 = EDGE_CURVE ( 'NONE', #183016, #159861, #69105, .T. ) ;
#214884 = EDGE_CURVE ( 'NONE', #183886, #82821, #136762, .T. ) ;
#214885 = AXIS2_PLACEMENT_3D ( 'NONE', #45333, #122307, #123591 ) ;
#214886 = EDGE_LOOP ( 'NONE', ( #134006, #38317, #164362, #137936 ) ) ;
#214887 = CARTESIAN_POINT ( 'NONE',  ( 18.55857864376268296, 65.63284271248657831, -111.7731074845243597 ) ) ;
#214888 = EDGE_CURVE ( 'NONE', #242879, #227113, #28499, .T. ) ;
#214889 = ORIENTED_EDGE ( 'NONE', *, *, #115989, .T. ) ;
#214890 = CARTESIAN_POINT ( 'NONE',  ( -23.15000000000000213, 85.60000000001173248, -81.27310748452424605 ) ) ;
#214891 = DIRECTION ( 'NONE',  ( 0.000000000000000000, 0.2617529984165152257, 0.9651348961777124202 ) ) ;
#214893 = DIRECTION ( 'NONE',  ( 0.000000000000000000, 5.551115123126393596E-13, -1.000000000000000000 ) ) ;
#214892 = PRODUCT_DEFINITION_CONTEXT ( 'detailed design', #237440, 'design' ) ;
#214894 = FACE_OUTER_BOUND ( 'NONE', #184038, .T. ) ;
#214895 = CARTESIAN_POINT ( 'NONE',  ( -16.87683809663753465, 9.864913778538415556, -13.27571563563853907 ) ) ;
#214896 = EDGE_CURVE ( 'NONE', #180338, #113296, #177670, .T. ) ;
#214897 = DIRECTION ( 'NONE',  ( -1.000000000000000000, -0.000000000000000000, -0.000000000000000000 ) ) ;
#214898 = AXIS2_PLACEMENT_3D ( 'NONE', #36873, #17287, #96773 ) ;
#214899 = DIRECTION ( 'NONE',  ( 0.000000000000000000, -0.2617529984165031243, -0.9651348961777157509 ) ) ;
#214902 = ORIENTED_EDGE ( 'NONE', *, *, #9229, .F. ) ;
#214901 = EDGE_CURVE ( 'NONE', #151679, #121144, #3486, .T. ) ;
#214900 = CARTESIAN_POINT ( 'NONE',  ( 21.14999999999999858, 69.45934304831071415, -103.0231074845243597 ) ) ;
#214903 = ORIENTED_EDGE ( 'NONE', *, *, #113890, .F. ) ;
#214905 = DIRECTION ( 'NONE',  ( -0.000000000000000000, -0.9770955615653313941, -0.2128009952263609228 ) ) ;
#214904 = LINE ( 'NONE', #75428, #245282 ) ;
#214907 = EDGE_LOOP ( 'NONE', ( #205250, #253896, #120005, #204934, #180040 ) ) ;
#214906 = DIRECTION ( 'NONE',  ( -0.000000000000000000, 0.9770955615653316162, 0.2128009952263604232 ) ) ;
#214908 = ORIENTED_EDGE ( 'NONE', *, *, #136770, .T. ) ;
#214909 = CARTESIAN_POINT ( 'NONE',  ( -16.94275863006528482, 66.01050395134471671, -149.1314101024478589 ) ) ;
#214910 = CARTESIAN_POINT ( 'NONE',  ( 20.12518398540832365, 9.975088720679844201, -175.4966682524667192 ) ) ;
#214911 = CARTESIAN_POINT ( 'NONE',  ( 20.94999999999999574, 62.98323157773585734, -207.0610388790105958 ) ) ;
#214912 = DIRECTION ( 'NONE',  ( 0.000000000000000000, 0.2617529984165152257, 0.9651348961777124202 ) ) ;
#214914 = CARTESIAN_POINT ( 'NONE',  ( 18.49999999999999645, 0.000000000000000000, 0.000000000000000000 ) ) ;
#214913 = AXIS2_PLACEMENT_3D ( 'NONE', #79321, #122324, #140589 ) ;
#214915 = ADVANCED_FACE ( 'NONE', ( #33861 ), #36862, .T. ) ;
#214916 = CARTESIAN_POINT ( 'NONE',  ( -21.05000000000000071, 87.65000000001172964, -72.62310748452422615 ) ) ;
#214917 = CARTESIAN_POINT ( 'NONE',  ( -20.94999999999999929, 4.184122562697133674, -245.3714803909117279 ) ) ;
#214918 = CARTESIAN_POINT ( 'NONE',  ( -20.94999999999999929, 1.261786168576181755, -142.0864989635454947 ) ) ;
#214919 = EDGE_CURVE ( 'NONE', #256904, #11722, #170144, .T. ) ;
#214920 = ORIENTED_EDGE ( 'NONE', *, *, #197667, .T. ) ;
#214921 = EDGE_LOOP ( 'NONE', ( #211992, #151340, #17378, #134146, #94827, #199513, #158720, #14675, #84085 ) ) ;
#214922 = CARTESIAN_POINT ( 'NONE',  ( 21.14999999999999858, 6.390846877240206503, -199.6081416912452653 ) ) ;
#214923 = VECTOR ( 'NONE', #145494, 1000.000000000000114 ) ;
#214924 = AXIS2_PLACEMENT_3D ( 'NONE', #111817, #208363, #190064 ) ;
#214925 = EDGE_LOOP ( 'NONE', ( #117223, #193960, #159918, #10587 ) ) ;
#214926 = AXIS2_PLACEMENT_3D ( 'NONE', #109388, #50683, #149834 ) ;
#214928 = DIRECTION ( 'NONE',  ( 1.000000000000000000, 7.304098846218134667E-16, 5.100424963727256530E-30 ) ) ;
#214927 = AXIS2_PLACEMENT_3D ( 'NONE', #55974, #112150, #14336 ) ;
#214929 = VERTEX_POINT ( 'NONE', #54646 ) ;
#214930 = CARTESIAN_POINT ( 'NONE',  ( 18.47135592147654748, -9.471088613265669309, -40.18359493984359432 ) ) ;
#214931 = CARTESIAN_POINT ( 'NONE',  ( -18.59999999999999787, 13.71992543034163958, -238.5823796952984992 ) ) ;
#214932 = CARTESIAN_POINT ( 'NONE',  ( 21.05000000000000071, -4.259020970815407203, -226.0869574510824123 ) ) ;
#214933 = EDGE_CURVE ( 'NONE', #130315, #216335, #75528, .T. ) ;
#214935 = ORIENTED_EDGE ( 'NONE', *, *, #41565, .F. ) ;
#214934 = CARTESIAN_POINT ( 'NONE',  ( 18.43709777086140988, -9.682403433465237796, -207.6568433774128266 ) ) ;
#214936 = CARTESIAN_POINT ( 'NONE',  ( -18.79999999999999716, -11.65000000000000036, 32.89999999999999858 ) ) ;
#214937 = EDGE_LOOP ( 'NONE', ( #245867, #95475, #70241, #228317 ) ) ;
#214938 = CARTESIAN_POINT ( 'NONE',  ( -22.50000000000000000, 55.96169194136206215, -232.9023299069559130 ) ) ;
#214939 = B_SPLINE_CURVE_WITH_KNOTS ( 'NONE', 3,
 ( #237041, #60956, #177092, #199200, #256539, #79222, #40153, #100061 ),
 .UNSPECIFIED., .F., .F.,
 ( 4, 2, 2, 4 ),
 ( 0.000000000000000000, 0.0002181133598168967676, 0.0003271700397253451379, 0.0004362267196337935352 ),
 .UNSPECIFIED. ) ;
#214940 = CARTESIAN_POINT ( 'NONE',  ( -18.59999999999999787, 85.48068669529035901, -29.08199231576641353 ) ) ;
#214941 = CARTESIAN_POINT ( 'NONE',  ( -18.59999999999999787, 1.162701749949165642, -75.10000000000003695 ) ) ;
#214942 = CARTESIAN_POINT ( 'NONE',  ( -21.14999999999994174, 64.35000000001120668, -51.02310748452479316 ) ) ;
#214943 = VECTOR ( 'NONE', #147442, 1000.000000000000000 ) ;
#214944 = CARTESIAN_POINT ( 'NONE',  ( -18.50000000000000000, 64.25000000001206502, -124.3731074845243825 ) ) ;
#214945 = EDGE_LOOP ( 'NONE', ( #100738, #6320, #221419, #181388 ) ) ;
#214946 = AXIS2_PLACEMENT_3D ( 'NONE', #21093, #1487, #45758 ) ;
#214948 = CARTESIAN_POINT ( 'NONE',  ( -18.33981767444299393, 85.56957578981555912, -29.20394564079942867 ) ) ;
#214947 = CARTESIAN_POINT ( 'NONE',  ( -21.00023020733438273, 6.390869245278866018, -134.0000000000000000 ) ) ;
#214949 = ORIENTED_EDGE ( 'NONE', *, *, #210955, .T. ) ;
#214952 = ORIENTED_EDGE ( 'NONE', *, *, #75201, .T. ) ;
#214951 = CARTESIAN_POINT ( 'NONE',  ( -18.50000000000000000, -1.835859311432484375, -112.0044391687985694 ) ) ;
#214950 = CARTESIAN_POINT ( 'NONE',  ( -18.40000000000000213, 11.47316190337364183, -191.6740539331919990 ) ) ;
#214953 = DIRECTION ( 'NONE',  ( 1.000000000000000000, 0.000000000000000000, 0.000000000000000000 ) ) ;
#214954 = CARTESIAN_POINT ( 'NONE',  ( 20.94999999999999929, 8.776282895292471409, -8.558628995140949769 ) ) ;
#214955 = VECTOR ( 'NONE', #210703, 1000.000000000000000 ) ;
#214956 = VERTEX_POINT ( 'NONE', #11700 ) ;
#214957 = DIRECTION ( 'NONE',  ( 0.000000000000000000, 0.9126074666063660468, 0.4088369013363524762 ) ) ;
#214958 = CARTESIAN_POINT ( 'NONE',  ( -21.05000000000000071, 68.13014604066189861, -227.7202878558733516 ) ) ;
#214959 = CARTESIAN_POINT ( 'NONE',  ( 20.94999999999999574, 74.15091558138456662, -57.86709696307720918 ) ) ;
#214961 = ORIENTED_EDGE ( 'NONE', *, *, #201660, .T. ) ;
#214960 = CARTESIAN_POINT ( 'NONE',  ( -21.65000000000000213, 68.29142135624960019, -157.7731074845244166 ) ) ;
#214962 = CYLINDRICAL_SURFACE ( 'NONE', #26894, 0.1000000000000033362 ) ;
#214963 = ORIENTED_EDGE ( 'NONE', *, *, #227153, .F. ) ;
#214964 = DIRECTION ( 'NONE',  ( 0.000000000000000000, 0.000000000000000000, 1.000000000000000000 ) ) ;
#214965 = FACE_OUTER_BOUND ( 'NONE', #201968, .T. ) ;
#214966 = CARTESIAN_POINT ( 'NONE',  ( 18.49999999999999289, 65.79142135624907439, -78.37310748452438247 ) ) ;
#214967 = CIRCLE ( 'NONE', #102505, 0.09999999999999939493 ) ;
#214968 = EDGE_LOOP ( 'NONE', ( #57811, #18003, #227595, #26821, #25346 ) ) ;
#214969 = DIRECTION ( 'NONE',  ( -0.000000000000000000, -1.000000000000000000, -0.000000000000000000 ) ) ;
#214970 = EDGE_LOOP ( 'NONE', ( #237671, #167637, #159406, #257146 ) ) ;
#214971 = DIRECTION ( 'NONE',  ( 1.000000000000000000, 0.000000000000000000, 0.000000000000000000 ) ) ;
#214972 = DIRECTION ( 'NONE',  ( 0.000000000000000000, 0.6728971962616792091, -0.7397360091702790408 ) ) ;
#214973 = CARTESIAN_POINT ( 'NONE',  ( 23.14999999999999503, 31.44980407958351876, -233.5445995079518582 ) ) ;
#214974 = ORIENTED_EDGE ( 'NONE', *, *, #188763, .T. ) ;
#214975 = FACE_OUTER_BOUND ( 'NONE', #166482, .T. ) ;
#214976 = FACE_OUTER_BOUND ( 'NONE', #389, .T. ) ;
#214977 = EDGE_CURVE ( 'NONE', #10839, #74222, #116131, .T. ) ;
#214978 = EDGE_LOOP ( 'NONE', ( #245948, #212244, #179198 ) ) ;
#214979 = FACE_OUTER_BOUND ( 'NONE', #39572, .T. ) ;
#214980 = DIRECTION ( 'NONE',  ( 0.000000000000000000, 0.000000000000000000, -1.000000000000000000 ) ) ;
#214981 = DIRECTION ( 'NONE',  ( -0.000000000000000000, 1.000000000000000000, -0.000000000000000000 ) ) ;
#214982 = CIRCLE ( 'NONE', #35943, 0.1000000000000008937 ) ;
#214983 = VERTEX_POINT ( 'NONE', #72975 ) ;
#214984 = VERTEX_POINT ( 'NONE', #74261 ) ;
#214985 = PRESENTATION_LAYER_ASSIGNMENT (  '', '', ( #169247 ) ) ;
#214986 = CARTESIAN_POINT ( 'NONE',  ( -18.40000000000000213, 64.25000000001230660, -157.3731074845244393 ) ) ;
#214987 = ORIENTED_EDGE ( 'NONE', *, *, #100831, .T. ) ;
#214989 = ORIENTED_EDGE ( 'NONE', *, *, #153555, .T. ) ;
#214988 = CARTESIAN_POINT ( 'NONE',  ( -20.85000000000000142, 77.25000000001185185, -95.22262673010919798 ) ) ;
#214990 = EDGE_CURVE ( 'NONE', #139006, #28076, #253473, .T. ) ;
#214991 = EDGE_CURVE ( 'NONE', #193988, #165270, #31288, .T. ) ;
#214994 = VERTEX_POINT ( 'NONE', #50781 ) ;
#214993 = ORIENTED_EDGE ( 'NONE', *, *, #248794, .T. ) ;
#214992 = CARTESIAN_POINT ( 'NONE',  ( 21.05000000000000071, 65.27628289530517236, -203.5231074845244166 ) ) ;
#214995 = CARTESIAN_POINT ( 'NONE',  ( 21.14999999999999858, 69.74218538953624602, -170.1208977758331855 ) ) ;
#214996 = CARTESIAN_POINT ( 'NONE',  ( -16.77431908686105899, 12.41294867713261496, -211.2576179284957334 ) ) ;
#214997 = CARTESIAN_POINT ( 'NONE',  ( 21.12769345151713196, 10.71928767695172624, -112.7474803461975199 ) ) ;
#214998 = AXIS2_PLACEMENT_3D ( 'NONE', #83917, #185642, #222165 ) ;
#214999 = CARTESIAN_POINT ( 'NONE',  ( -21.05000000000000071, 6.257814610487270279, -33.40220970869120265 ) ) ;
#215000 =( BOUNDED_CURVE ( )  B_SPLINE_CURVE ( 3, ( #32095, #167756, #228996, #146856 ),
 .UNSPECIFIED., .F., .T. ) 
 B_SPLINE_CURVE_WITH_KNOTS ( ( 4, 4 ),
 ( 0.5235987755982449698, 1.570796326794896558 ),
 .UNSPECIFIED. ) 
 CURVE ( )  GEOMETRIC_REPRESENTATION_ITEM ( )  RATIONAL_B_SPLINE_CURVE ( ( 1.000000000000000000, 0.9106836025229499976, 0.9106836025229499976, 1.000000000000000000 ) ) 
 REPRESENTATION_ITEM ( '' )  );
#215001 = CARTESIAN_POINT ( 'NONE',  ( -20.54999999999999716, -8.999999999988846255, -76.39396912265249284 ) ) ;
#215002 = DIRECTION ( 'NONE',  ( -1.000000000000000000, 0.000000000000000000, -0.000000000000000000 ) ) ;
#215004 = ORIENTED_EDGE ( 'NONE', *, *, #237296, .F. ) ;
#215003 = AXIS2_PLACEMENT_3D ( 'NONE', #170419, #109092, #249906 ) ;
#215005 = ORIENTED_EDGE ( 'NONE', *, *, #72077, .T. ) ;
#215006 = ORIENTED_EDGE ( 'NONE', *, *, #188023, .F. ) ;
#215007 = EDGE_CURVE ( 'NONE', #51843, #90327, #141069, .T. ) ;
#215008 = DIRECTION ( 'NONE',  ( 0.000000000000000000, 0.8814952561688444987, -0.4721928772777320149 ) ) ;
#215011 = VERTEX_POINT ( 'NONE', #212466 ) ;
#215010 = EDGE_CURVE ( 'NONE', #147515, #77132, #232034, .T. ) ;
#215009 = CARTESIAN_POINT ( 'NONE',  ( 23.24999999999999289, 69.35000000001228670, -157.6731074845243938 ) ) ;
#215013 = CARTESIAN_POINT ( 'NONE',  ( -23.25000000000000000, 4.350000000011156054, -45.75000000000000711 ) ) ;
#215012 = CIRCLE ( 'NONE', #106663, 0.09999999999999939493 ) ;
#215014 = EDGE_LOOP ( 'NONE', ( #136704, #118682, #116018, #26733 ) ) ;
#215015 = DIRECTION ( 'NONE',  ( 0.000000000000000000, 0.9126074666063545004, 0.4088369013363783999 ) ) ;
#215016 = EDGE_LOOP ( 'NONE', ( #191979, #220363, #219577 ) ) ;
#215017 = DIRECTION ( 'NONE',  ( -1.000000000000000000, 0.000000000000000000, 0.000000000000000000 ) ) ;
#215018 = AXIS2_PLACEMENT_3D ( 'NONE', #238323, #200491, #180930 ) ;
#215019 = EDGE_CURVE ( 'NONE', #61669, #153040, #103616, .T. ) ;
#215020 = AXIS2_PLACEMENT_3D ( 'NONE', #96979, #157022, #99564 ) ;
#215021 = EDGE_LOOP ( 'NONE', ( #189920, #165465, #21208, #239181 ) ) ;
#215022 = EDGE_CURVE ( 'NONE', #220769, #129083, #191641, .T. ) ;
#215023 = LINE ( 'NONE', #76794, #114691 ) ;
#215024 = DIRECTION ( 'NONE',  ( -0.000000000000000000, -1.000000000000000000, -6.982962677686266711E-15 ) ) ;
#215027 = ORIENTED_EDGE ( 'NONE', *, *, #162810, .T. ) ;
#215026 = VERTEX_POINT ( 'NONE', #173374 ) ;
#215025 = CIRCLE ( 'NONE', #102563, 0.09999999999999657774 ) ;
#215028 = B_SPLINE_CURVE_WITH_KNOTS ( 'NONE', 3,
 ( #40733, #44556, #242731, #122816, #103211, #201050, #238902, #4127, #202333, #65390, #22440, #60244, #221867, #100629 ),
 .UNSPECIFIED., .F., .F.,
 ( 4, 2, 2, 2, 2, 2, 4 ),
 ( 0.000000000000000000, 2.389617747642148448E-05, 4.779235495284296897E-05, 9.558470990570041204E-05, 0.0001911694198114009054, 0.0003823388396228294579, 0.0007646776792456864546 ),
 .UNSPECIFIED. ) ;
#215029 = VERTEX_POINT ( 'NONE', #95064 ) ;
#215030 = CIRCLE ( 'NONE', #23545, 0.09999999999998898659 ) ;
#215032 = VERTEX_POINT ( 'NONE', #92494 ) ;
#215031 = EDGE_CURVE ( 'NONE', #228950, #232210, #52072, .T. ) ;
#215033 = VECTOR ( 'NONE', #51578, 1000.000000000000000 ) ;
#215034 = EDGE_LOOP ( 'NONE', ( #211767, #199250 ) ) ;
#215035 = DIRECTION ( 'NONE',  ( 1.000000000000000000, 0.000000000000000000, 0.000000000000000000 ) ) ;
#215037 = ORIENTED_EDGE ( 'NONE', *, *, #26508, .T. ) ;
#215036 = CARTESIAN_POINT ( 'NONE',  ( 23.40000000000005542, 83.97335046823651794, -37.38386894789040582 ) ) ;
#215038 = DIRECTION ( 'NONE',  ( 0.000000000000000000, 1.000000000000000000, 0.000000000000000000 ) ) ;
#215039 = AXIS2_PLACEMENT_3D ( 'NONE', #126131, #204387, #166591 ) ;
#215041 = CARTESIAN_POINT ( 'NONE',  ( -21.05000000000000071, 14.00000000001115374, -195.5729074696174905 ) ) ;
#215040 = DIRECTION ( 'NONE',  ( 0.000000000000000000, 6.982962677686266711E-15, -1.000000000000000000 ) ) ;
#215042 = DIRECTION ( 'NONE',  ( 3.616040088954490704E-32, 7.105427357601001859E-15, -1.000000000000000000 ) ) ;
#215043 = CARTESIAN_POINT ( 'NONE',  ( -22.50485643085238863, 76.07878633908995880, -215.2729024236967916 ) ) ;
#215044 = CARTESIAN_POINT ( 'NONE',  ( -20.54999999999999716, 68.75000000001205080, -124.2731074845243455 ) ) ;
#215045 = VERTEX_POINT ( 'NONE', #254126 ) ;
#215047 = EDGE_CURVE ( 'NONE', #158005, #128159, #7983, .T. ) ;
#215046 = ORIENTED_EDGE ( 'NONE', *, *, #241288, .T. ) ;
#215048 = CARTESIAN_POINT ( 'NONE',  ( 18.60000000000000142, 85.48068669529082797, -96.08199231576635668 ) ) ;
#215049 = CARTESIAN_POINT ( 'NONE',  ( -21.05000000000000426, 76.10000000001218723, -143.0001745056490847 ) ) ;
#215050 = DIRECTION ( 'NONE',  ( 0.000000000000000000, -0.4999999999999088507, -0.8660254037844913322 ) ) ;
#215051 = AXIS2_PLACEMENT_3D ( 'NONE', #43764, #125852, #82848 ) ;
#215052 = ORIENTED_EDGE ( 'NONE', *, *, #212774, .T. ) ;
#215053 = DIRECTION ( 'NONE',  ( 0.000000000000000000, -1.000000000000000000, 0.000000000000000000 ) ) ;
#215054 = CARTESIAN_POINT ( 'NONE',  ( -20.64999999999999858, 84.66355140188123585, -126.9990063664569391 ) ) ;
#215055 = DIRECTION ( 'NONE',  ( -1.000000000000000000, 0.000000000000000000, 0.000000000000000000 ) ) ;
#215056 = ORIENTED_EDGE ( 'NONE', *, *, #120297, .F. ) ;
#215057 = ORIENTED_EDGE ( 'NONE', *, *, #223629, .T. ) ;
#215058 = DIRECTION ( 'NONE',  ( -1.000000000000000000, -0.000000000000000000, -0.000000000000000000 ) ) ;
#215059 = DIRECTION ( 'NONE',  ( 1.000000000000000000, 0.000000000000000000, 0.000000000000000000 ) ) ;
#215060 = ORIENTED_EDGE ( 'NONE', *, *, #16936, .F. ) ;
#215061 = DIRECTION ( 'NONE',  ( 1.000000000000000000, 0.000000000000000000, 0.000000000000000000 ) ) ;
#215062 = ORIENTED_EDGE ( 'NONE', *, *, #55888, .F. ) ;
#215064 = FACE_OUTER_BOUND ( 'NONE', #160880, .T. ) ;
#215063 = SHAPE_REPRESENTATION ( 'Injection Molded Chain Links 3', ( #2425 ), #94000 ) ;
#215066 = CARTESIAN_POINT ( 'NONE',  ( -21.04999999999896687, -1.290533477727345169, -194.8331962964030595 ) ) ;
#215065 = DIRECTION ( 'NONE',  ( -1.000000000000000000, 0.000000000000000000, 0.000000000000000000 ) ) ;
#215067 = AXIS2_PLACEMENT_3D ( 'NONE', #49135, #33475, #170430 ) ;
#215068 = CARTESIAN_POINT ( 'NONE',  ( -20.94999999999999929, 56.55376719376374695, -240.6385182521135278 ) ) ;
#215069 = CIRCLE ( 'NONE', #73459, 4.049999999999998934 ) ;
#215070 = DIRECTION ( 'NONE',  ( 0.000000000000000000, 0.000000000000000000, 1.000000000000000000 ) ) ;
#215071 = CIRCLE ( 'NONE', #102603, 0.09999999999999939493 ) ;
#215072 = CARTESIAN_POINT ( 'NONE',  ( -20.05000000000000426, 44.14788529697245423, -236.0604079036328073 ) ) ;
#215073 = AXIS2_PLACEMENT_3D ( 'NONE', #215330, #178817, #159236 ) ;
#215074 = ADVANCED_FACE ( 'NONE', ( #234575 ), #120434, .T. ) ;
#215076 = ORIENTED_EDGE ( 'NONE', *, *, #209944, .F. ) ;
#215075 = EDGE_LOOP ( 'NONE', ( #208740, #229596, #81697, #1525 ) ) ;
#215077 = ORIENTED_EDGE ( 'NONE', *, *, #136189, .T. ) ;
#215078 = DIRECTION ( 'NONE',  ( -1.000000000000000000, -4.336808689942044242E-14, 0.000000000000000000 ) ) ;
#215079 = FACE_OUTER_BOUND ( 'NONE', #125641, .T. ) ;
#215080 = DIRECTION ( 'NONE',  ( 0.000000000000000000, 0.000000000000000000, 1.000000000000000000 ) ) ;
#215081 = CARTESIAN_POINT ( 'NONE',  ( 20.73486653747088226, 21.70314669089255943, -233.3151006027784717 ) ) ;
#215082 = EDGE_CURVE ( 'NONE', #122058, #75479, #82754, .T. ) ;
#215084 = ADVANCED_FACE ( 'NONE', ( #61067 ), #160207, .T. ) ;
#215083 = AXIS2_PLACEMENT_3D ( 'NONE', #236860, #161190, #120800 ) ;
#215086 = FACE_OUTER_BOUND ( 'NONE', #214099, .T. ) ;
#215085 = DIRECTION ( 'NONE',  ( 0.000000000000000000, -0.4088369013363783999, 0.9126074666063545004 ) ) ;
#215087 = CARTESIAN_POINT ( 'NONE',  ( -16.81453563122429529, 66.06089979457456707, -48.73484882387909067 ) ) ;
#215088 = ORIENTED_EDGE ( 'NONE', *, *, #86729, .T. ) ;
#215089 = AXIS2_PLACEMENT_3D ( 'NONE', #121842, #179261, #3143 ) ;
#215090 = ORIENTED_EDGE ( 'NONE', *, *, #3115, .T. ) ;
#215091 = VERTEX_POINT ( 'NONE', #157655 ) ;
#215092 = CARTESIAN_POINT ( 'NONE',  ( -21.05000000000000071, 69.69982018209479691, -69.57459036640655370 ) ) ;
#215093 = CIRCLE ( 'NONE', #106743, 0.1000000000000028644 ) ;
#215094 = CARTESIAN_POINT ( 'NONE',  ( -22.49510344025093644, 0.06712767820541533370, -88.85002989488579317 ) ) ;
#215095 = ADVANCED_FACE ( 'NONE', ( #141890 ), #100170, .F. ) ;
#215096 = DIRECTION ( 'NONE',  ( 1.000000000000000000, 0.000000000000000000, 0.000000000000000000 ) ) ;
#215097 = EDGE_CURVE ( 'NONE', #170728, #64541, #241007, .T. ) ;
#215098 = EDGE_CURVE ( 'NONE', #244466, #90118, #57198, .T. ) ;
#215099 = DIRECTION ( 'NONE',  ( 0.7071067811865475727, -0.7071067811865475727, -5.142139384388981164E-15 ) ) ;
#215100 = LINE ( 'NONE', #11795, #92309 ) ;
#215101 = ORIENTED_EDGE ( 'NONE', *, *, #112491, .T. ) ;
#215102 = ORIENTED_EDGE ( 'NONE', *, *, #180196, .F. ) ;
#215103 = FACE_OUTER_BOUND ( 'NONE', #215016, .T. ) ;
#215104 = EDGE_CURVE ( 'NONE', #56430, #68386, #98884, .T. ) ;
#215105 = AXIS2_PLACEMENT_3D ( 'NONE', #101105, #238094, #198978 ) ;
#215106 = DIRECTION ( 'NONE',  ( -2.915501640297152804E-16, -1.000000000000000000, -6.997203936713167125E-15 ) ) ;
#215107 = DIRECTION ( 'NONE',  ( 0.000000000000000000, 0.2128009952263604232, -0.9770955615653316162 ) ) ;
#215108 = DIRECTION ( 'NONE',  ( -4.336808689942017736E-16, 0.000000000000000000, -1.000000000000000000 ) ) ;
#215109 = CARTESIAN_POINT ( 'NONE',  ( -22.39999999999999858, 75.90000000001170122, -77.31388708289772183 ) ) ;
#215110 = DIRECTION ( 'NONE',  ( 0.000000000000000000, 0.000000000000000000, -1.000000000000000000 ) ) ;
#215111 = CYLINDRICAL_SURFACE ( 'NONE', #216836, 0.09999999999999216460 ) ;
#215113 = DIRECTION ( 'NONE',  ( -0.000000000000000000, -0.000000000000000000, 1.000000000000000000 ) ) ;
#215112 = LINE ( 'NONE', #35228, #128609 ) ;
#215114 = CARTESIAN_POINT ( 'NONE',  ( -21.14999999999999858, -1.489567864901279792, -194.6304332222954372 ) ) ;
#215115 = DIRECTION ( 'NONE',  ( 0.000000000000000000, 0.000000000000000000, 1.000000000000000000 ) ) ;
#215116 = CARTESIAN_POINT ( 'NONE',  ( -20.64999999999999858, -7.176961358819843539, -212.6889627706600834 ) ) ;
#215117 = CARTESIAN_POINT ( 'NONE',  ( 21.08621493067296271, 69.65070570884101642, -203.5793023240005084 ) ) ;
#215118 = AXIS2_PLACEMENT_3D ( 'NONE', #231476, #193621, #77488 ) ;
#215121 = VERTEX_POINT ( 'NONE', #37690 ) ;
#215120 = VECTOR ( 'NONE', #180773, 1000.000000000000000 ) ;
#215119 = CARTESIAN_POINT ( 'NONE',  ( 21.05000000000000071, 1.115600667400684642E-11, -67.00000000000004263 ) ) ;
#215122 = AXIS2_PLACEMENT_3D ( 'NONE', #192185, #29287, #89204 ) ;
#215123 = VECTOR ( 'NONE', #156106, 1000.000000000000000 ) ;
#215124 = ADVANCED_FACE ( 'NONE', ( #220159 ), #18094, .T. ) ;
#215125 = CARTESIAN_POINT ( 'NONE',  ( 21.05000000000000071, 69.34766280046808617, -247.6726305063181144 ) ) ;
#215126 = ORIENTED_EDGE ( 'NONE', *, *, #252395, .F. ) ;
#215127 = EDGE_CURVE ( 'NONE', #40198, #59439, #78679, .T. ) ;
#215128 = EDGE_CURVE ( 'NONE', #163089, #225164, #220170, .T. ) ;
#215129 = CARTESIAN_POINT ( 'NONE',  ( -22.47071067811865319, 0.09909245471376171288, -92.77992525550196490 ) ) ;
#215130 = CARTESIAN_POINT ( 'NONE',  ( 21.13736287352038445, 67.95335762362759624, -60.27310748452438105 ) ) ;
#215131 = ORIENTED_EDGE ( 'NONE', *, *, #234164, .F. ) ;
#215132 = CARTESIAN_POINT ( 'NONE',  ( -20.64999999999999858, 68.85000000001222986, -148.8731074845244109 ) ) ;
#215133 = AXIS2_PLACEMENT_3D ( 'NONE', #42565, #122115, #116037 ) ;
#215134 = CARTESIAN_POINT ( 'NONE',  ( 15.69410316191958898, 9.356746017089403011, -84.20335972136422242 ) ) ;
#215135 = DIRECTION ( 'NONE',  ( 0.000000000000000000, 0.2617529984165152257, 0.9651348961777124202 ) ) ;
#215136 = VECTOR ( 'NONE', #96422, 1000.000000000000000 ) ;
#215137 = VECTOR ( 'NONE', #150175, 1000.000000000000000 ) ;
#215138 = CARTESIAN_POINT ( 'NONE',  ( -21.14999999999994174, 82.84256550613280012, -26.34830530078816935 ) ) ;
#215139 = DIRECTION ( 'NONE',  ( 1.000000000000000000, 0.000000000000000000, 0.000000000000000000 ) ) ;
#215140 = DIRECTION ( 'NONE',  ( 1.000000000000000000, 7.304098846218133681E-16, 5.311601492717083645E-30 ) ) ;
#215141 = AXIS2_PLACEMENT_3D ( 'NONE', #46825, #229349, #91106 ) ;
#215142 = VERTEX_POINT ( 'NONE', #21965 ) ;
#215143 = CYLINDRICAL_SURFACE ( 'NONE', #95598, 0.09999999999999939493 ) ;
#215145 = EDGE_LOOP ( 'NONE', ( #135103, #33156, #12454 ) ) ;
#215144 = DIRECTION ( 'NONE',  ( 0.000000000000000000, -1.000000000000000000, -6.352154140967427193E-15 ) ) ;
#215146 = CARTESIAN_POINT ( 'NONE',  ( 11.60000000000000142, -11.65000000000000036, 15.00000000000000355 ) ) ;
#215147 = CARTESIAN_POINT ( 'NONE',  ( -20.94999999999999929, -10.74476030654554215, -206.4104182790846096 ) ) ;
#215148 = DIRECTION ( 'NONE',  ( 0.000000000000000000, 0.000000000000000000, -1.000000000000000000 ) ) ;
#215149 = ORIENTED_EDGE ( 'NONE', *, *, #40751, .F. ) ;
#215150 = DIRECTION ( 'NONE',  ( -0.000000000000000000, 0.8096735173027155286, -0.5868805631290315850 ) ) ;
#215151 = PRODUCT_CONTEXT ( 'NONE', #83934, 'mechanical' ) ;
#215152 = CARTESIAN_POINT ( 'NONE',  ( 22.50014994444028105, 11.46291945964638082, -198.4184706950397299 ) ) ;
#215153 = CARTESIAN_POINT ( 'NONE',  ( 21.05000000000000071, 1.115600667400684642E-11, -167.5000000000000284 ) ) ;
#215154 = ORIENTED_EDGE ( 'NONE', *, *, #71512, .F. ) ;
#215155 = CARTESIAN_POINT ( 'NONE',  ( -18.59999999999999787, 15.92646454033039305, -219.3818586450342707 ) ) ;
#215156 = DIRECTION ( 'NONE',  ( 1.000000000000000000, -0.000000000000000000, -0.000000000000000000 ) ) ;
#215157 = TOROIDAL_SURFACE ( 'NONE', #156924, 3.899999999999999467, 0.1000000000000000056 ) ;
#215158 = LINE ( 'NONE', #219000, #112099 ) ;
#215159 = ORIENTED_EDGE ( 'NONE', *, *, #22895, .F. ) ;
#215160 = VERTEX_POINT ( 'NONE', #138025 ) ;
#215161 = AXIS2_PLACEMENT_3D ( 'NONE', #79761, #141058, #60214 ) ;
#215162 = CARTESIAN_POINT ( 'NONE',  ( 22.50000000000000000, 67.23127455305841238, -235.8551265064783991 ) ) ;
#215163 = DIRECTION ( 'NONE',  ( 0.000000000000000000, -1.000000000000000000, 0.000000000000000000 ) ) ;
#215164 = CARTESIAN_POINT ( 'NONE',  ( 18.50000000000000000, 85.50000000001161027, -62.49103808782458458 ) ) ;
#215165 = EDGE_CURVE ( 'NONE', #128159, #158005, #153771, .T. ) ;
#215166 = CARTESIAN_POINT ( 'NONE',  ( -16.95709691155922982, 30.19746286648991074, -234.8022958954214801 ) ) ;
#215169 = PLANE ( 'NONE',  #249447 ) ;
#215168 = AXIS2_PLACEMENT_3D ( 'NONE', #72479, #155878, #56708 ) ;
#215167 = CARTESIAN_POINT ( 'NONE',  ( 21.04999999999999716, -1.396784380639764622, -194.6548880948980127 ) ) ;
#215170 = CARTESIAN_POINT ( 'NONE',  ( 20.94999999999999929, 65.70711192142317714, -30.56510546851222188 ) ) ;
#215171 = EDGE_CURVE ( 'NONE', #50106, #257602, #112037, .T. ) ;
#215172 = DIRECTION ( 'NONE',  ( 0.000000000000000000, 6.982962677686266711E-15, -1.000000000000000000 ) ) ;
#215173 = CARTESIAN_POINT ( 'NONE',  ( 18.50000324121758055, 65.70692517833163038, -30.56446533783042696 ) ) ;
#215174 = CARTESIAN_POINT ( 'NONE',  ( -18.40000000000000213, 11.75000000001113953, -87.85000000000003695 ) ) ;
#215175 = AXIS2_PLACEMENT_3D ( 'NONE', #70446, #247755, #146077 ) ;
#215176 = ORIENTED_EDGE ( 'NONE', *, *, #40950, .F. ) ;
#215177 = AXIS2_PLACEMENT_3D ( 'NONE', #243230, #64596, #204107 ) ;
#215178 = ORIENTED_EDGE ( 'NONE', *, *, #248453, .T. ) ;
#215179 = FACE_OUTER_BOUND ( 'NONE', #19506, .T. ) ;
#215180 = CARTESIAN_POINT ( 'NONE',  ( -23.25000000000000355, 40.29670989715187090, -235.0462836312595130 ) ) ;
#215182 = CARTESIAN_POINT ( 'NONE',  ( -20.94999999999999929, -1.362429037182149694, -74.88888124792120493 ) ) ;
#215181 = CARTESIAN_POINT ( 'NONE',  ( -23.25000000000000000, -9.599999999988847676, -143.8939691226524644 ) ) ;
#215183 = AXIS2_PLACEMENT_3D ( 'NONE', #45804, #28862, #66660 ) ;
#215184 = ADVANCED_FACE ( 'NONE', ( #179753 ), #23266, .T. ) ;
#215185 = EDGE_CURVE ( 'NONE', #7750, #213950, #149453, .T. ) ;
#215186 = DIRECTION ( 'NONE',  ( -0.000000000000000000, -6.982962677686266711E-15, 1.000000000000000000 ) ) ;
#215187 = DIRECTION ( 'NONE',  ( 1.000000000000000000, 0.000000000000000000, 0.000000000000000000 ) ) ;
#215188 = CARTESIAN_POINT ( 'NONE',  ( 12.30626653967340900, 12.80368220771249810, -215.8196253896158794 ) ) ;
#215189 = ORIENTED_EDGE ( 'NONE', *, *, #151172, .F. ) ;
#215190 = ORIENTED_EDGE ( 'NONE', *, *, #86016, .T. ) ;
#215191 = DIRECTION ( 'NONE',  ( -3.035766082959430717E-14, -6.982962677686266711E-15, 1.000000000000000000 ) ) ;
#215192 = VERTEX_POINT ( 'NONE', #1073 ) ;
#215193 = CARTESIAN_POINT ( 'NONE',  ( -18.39999999999999858, -9.682403433465239573, -73.65684337741279819 ) ) ;
#215194 = CIRCLE ( 'NONE', #169450, 0.1000000000000011990 ) ;
#215196 = EDGE_CURVE ( 'NONE', #23656, #241512, #66227, .T. ) ;
#215195 = DIRECTION ( 'NONE',  ( 1.000000000000000000, 0.000000000000000000, 0.000000000000000000 ) ) ;
#215198 = EDGE_CURVE ( 'NONE', #225332, #221934, #156362, .T. ) ;
#215197 = AXIS2_PLACEMENT_3D ( 'NONE', #99479, #199911, #257243 ) ;
#215199 = DIRECTION ( 'NONE',  ( 0.000000000000000000, -0.4999999999999943379, -0.8660254037844420383 ) ) ;
#215200 = AXIS2_PLACEMENT_3D ( 'NONE', #82291, #4065, #124030 ) ;
#215202 = ORIENTED_EDGE ( 'NONE', *, *, #208138, .T. ) ;
#215201 = AXIS2_PLACEMENT_3D ( 'NONE', #227415, #209134, #27975 ) ;
#215203 = DIRECTION ( 'NONE',  ( -0.000000000000000000, -0.8660254037844420383, 0.4999999999999943379 ) ) ;
#215204 = ORIENTED_EDGE ( 'NONE', *, *, #91905, .F. ) ;
#215205 = AXIS2_PLACEMENT_3D ( 'NONE', #25412, #183196, #104889 ) ;
#215206 = DIRECTION ( 'NONE',  ( 0.000000000000000000, -0.9667078373770112698, -0.2558827019434132821 ) ) ;
#215207 = AXIS2_PLACEMENT_3D ( 'NONE', #11071, #240396, #22650 ) ;
#215208 = CARTESIAN_POINT ( 'NONE',  ( -16.94445028196808778, 66.00793639031432747, -123.9157773061059231 ) ) ;
#215209 = DIRECTION ( 'NONE',  ( -1.000000000000000000, 0.000000000000000000, 0.000000000000000000 ) ) ;
#215210 = DIRECTION ( 'NONE',  ( 0.000000000000000000, 0.000000000000000000, 1.000000000000000000 ) ) ;
#215211 = ADVANCED_FACE ( 'NONE', ( #117204 ), #196729, .T. ) ;
#215213 = CARTESIAN_POINT ( 'NONE',  ( 23.15000000000000213, -11.48912529306489994, -197.8999999999999773 ) ) ;
#215212 = DIRECTION ( 'NONE',  ( 1.000000000000000000, 0.000000000000000000, 0.000000000000000000 ) ) ;
#215214 = DIRECTION ( 'NONE',  ( 0.000000000000000000, 1.000000000000000000, 6.982962677686266711E-15 ) ) ;
#215216 = VERTEX_POINT ( 'NONE', #24542 ) ;
#215215 = ADVANCED_FACE ( 'NONE', ( #247403 ), #27121, .F. ) ;
#215217 = DIRECTION ( 'NONE',  ( 1.000000000000000000, -0.000000000000000000, 0.000000000000000000 ) ) ;
#215218 = ORIENTED_EDGE ( 'NONE', *, *, #81387, .T. ) ;
#215220 = EDGE_LOOP ( 'NONE', ( #161364, #80306, #219089, #3516 ) ) ;
#215219 = DIRECTION ( 'NONE',  ( 0.000000000000000000, 0.9654727137038715545, -0.2605042016806676242 ) ) ;
#215221 = CIRCLE ( 'NONE', #161062, 11.64999999999999325 ) ;
#215222 = ORIENTED_EDGE ( 'NONE', *, *, #176310, .F. ) ;
#215223 = CARTESIAN_POINT ( 'NONE',  ( -18.35668295345803713, 11.47316190337363118, -91.25000000000005684 ) ) ;
#215224 = CIRCLE ( 'NONE', #194403, 0.09999999999999530098 ) ;
#215225 = LINE ( 'NONE', #174867, #100880 ) ;
#215226 = AXIS2_PLACEMENT_3D ( 'NONE', #33377, #197536, #158451 ) ;
#215227 = CARTESIAN_POINT ( 'NONE',  ( -21.05000000000000426, 30.78878838668999052, -252.2904874585705102 ) ) ;
#215228 = CARTESIAN_POINT ( 'NONE',  ( -23.39999999999994529, 83.90000000001120384, -37.18565239344504647 ) ) ;
#215229 = EDGE_LOOP ( 'NONE', ( #256931, #180279, #222031, #230153 ) ) ;
#215230 = DIRECTION ( 'NONE',  ( 0.000000000000000000, 0.8814952561688437216, -0.4721928772777334582 ) ) ;
#215231 = DIRECTION ( 'NONE',  ( 0.000000000000000000, 0.000000000000000000, 1.000000000000000000 ) ) ;
#215232 = CARTESIAN_POINT ( 'NONE',  ( 22.49999999999999645, 64.25043287652330548, -203.6239658536231900 ) ) ;
#215233 = ADVANCED_FACE ( 'NONE', ( #144434 ), #227847, .F. ) ;
#215234 = EDGE_LOOP ( 'NONE', ( #224286, #227311, #143092, #48071 ) ) ;
#215235 = EDGE_CURVE ( 'NONE', #65124, #31563, #67486, .T. ) ;
#215236 = CYLINDRICAL_SURFACE ( 'NONE', #239890, 0.09999999999999939493 ) ;
#215237 = CIRCLE ( 'NONE', #186393, 0.1000000000000028644 ) ;
#215238 = DIRECTION ( 'NONE',  ( 0.000000000000000000, 0.8814952561688437216, -0.4721928772777334582 ) ) ;
#215239 = EDGE_CURVE ( 'NONE', #160823, #51816, #226540, .T. ) ;
#215240 = EDGE_LOOP ( 'NONE', ( #228220, #144344, #227283, #216517 ) ) ;
#215241 = ORIENTED_EDGE ( 'NONE', *, *, #208484, .F. ) ;
#215242 = DIRECTION ( 'NONE',  ( -4.408576920032447355E-17, 0.3427706569149636118, -0.9394191166662961834 ) ) ;
#215243 = B_SPLINE_CURVE_WITH_KNOTS ( 'NONE', 3,
 ( #130549, #31491, #110997, #190555, #11919, #112293 ),
 .UNSPECIFIED., .F., .F.,
 ( 4, 2, 4 ),
 ( 0.000000000000000000, 0.0001895189928937423326, 0.0003790379857874846652 ),
 .UNSPECIFIED. ) ;
#215244 = ORIENTED_EDGE ( 'NONE', *, *, #202355, .T. ) ;
#215245 = DIRECTION ( 'NONE',  ( 0.000000000000000000, 0.1350103645451974088, -0.9908441862701587999 ) ) ;
#215246 = ORIENTED_EDGE ( 'NONE', *, *, #108977, .T. ) ;
#215247 = CARTESIAN_POINT ( 'NONE',  ( 23.25000000000000000, -11.74999999998883560, -130.9000000000000341 ) ) ;
#215248 = CARTESIAN_POINT ( 'NONE',  ( -12.25000000000000178, 9.850000000011133849, -117.2500000000000284 ) ) ;
#215249 = ADVANCED_FACE ( 'NONE', ( #63639 ), #104026, .T. ) ;
#215250 = DIRECTION ( 'NONE',  ( 0.000000000000000000, 0.000000000000000000, -1.000000000000000000 ) ) ;
#215251 = AXIS2_PLACEMENT_3D ( 'NONE', #145359, #149246, #150517 ) ;
#215252 = VECTOR ( 'NONE', #151840, 1000.000000000000000 ) ;
#215253 = EDGE_CURVE ( 'NONE', #173389, #214956, #47917, .T. ) ;
#215254 = AXIS2_PLACEMENT_3D ( 'NONE', #246202, #49275, #247479 ) ;
#215255 = CARTESIAN_POINT ( 'NONE',  ( 18.50000000000000355, -9.399999999988846611, -73.88204184817267617 ) ) ;
#215256 = CARTESIAN_POINT ( 'NONE',  ( 18.54999999999999716, 8.750000000000014211, -12.65000000000000213 ) ) ;
#215257 = ORIENTED_EDGE ( 'NONE', *, *, #34728, .T. ) ;
#215259 = CARTESIAN_POINT ( 'NONE',  ( -21.14999999999999858, -0.09999999998884338825, -127.7500000000000284 ) ) ;
#215258 = CARTESIAN_POINT ( 'NONE',  ( 18.59999999999999076, 33.89981536720673461, -236.1713368690715527 ) ) ;
#215260 = EDGE_LOOP ( 'NONE', ( #19612, #216706, #57366, #220223 ) ) ;
#215263 = ORIENTED_EDGE ( 'NONE', *, *, #10618, .F. ) ;
#215262 = DIRECTION ( 'NONE',  ( 0.000000000000000000, 0.000000000000000000, -1.000000000000000000 ) ) ;
#215261 = FACE_OUTER_BOUND ( 'NONE', #89965, .T. ) ;
#215264 = AXIS2_PLACEMENT_3D ( 'NONE', #189050, #169530, #91241 ) ;
#215265 = ORIENTED_EDGE ( 'NONE', *, *, #254472, .F. ) ;
#215266 = CARTESIAN_POINT ( 'NONE',  ( -22.39999999999999858, 75.90000000001199965, -110.8138870828977218 ) ) ;
#215267 = CARTESIAN_POINT ( 'NONE',  ( 12.93225390519044637, 66.58234804117128647, -154.6643200920840400 ) ) ;
#215268 = DIRECTION ( 'NONE',  ( 0.000000000000000000, 0.000000000000000000, -1.000000000000000000 ) ) ;
#215269 = CARTESIAN_POINT ( 'NONE',  ( -22.39999999999999858, 75.90000000001242597, -177.8138870828977360 ) ) ;
#215270 = ORIENTED_EDGE ( 'NONE', *, *, #152044, .T. ) ;
#215272 = VERTEX_POINT ( 'NONE', #68786 ) ;
#215271 = CARTESIAN_POINT ( 'NONE',  ( 23.14999999999998437, 4.050000000011155343, -167.4999999999999716 ) ) ;
#215273 = AXIS2_PLACEMENT_3D ( 'NONE', #250676, #211571, #171199 ) ;
#215275 = CARTESIAN_POINT ( 'NONE',  ( 20.95561247346651967, 10.59500736520355346, -7.593782766981634680 ) ) ;
#215274 = CARTESIAN_POINT ( 'NONE',  ( 21.05000000000000071, 28.43730376342110944, -239.4748853164439879 ) ) ;
#215276 = TOROIDAL_SURFACE ( 'NONE', #15568, 4.099999999999999645, 0.1000000000000000056 ) ;
#215277 = VERTEX_POINT ( 'NONE', #246139 ) ;
#215278 = EDGE_LOOP ( 'NONE', ( #136046, #138849, #58821, #249091 ) ) ;
#215279 = CIRCLE ( 'NONE', #128365, 0.1000000000000028644 ) ;
#215280 = CARTESIAN_POINT ( 'NONE',  ( -20.64999999999999858, 44.87429835298446790, -237.9265065269792103 ) ) ;
#215281 = LINE ( 'NONE', #75781, #38411 ) ;
#215282 = ORIENTED_EDGE ( 'NONE', *, *, #247778, .T. ) ;
#215283 = CYLINDRICAL_SURFACE ( 'NONE', #80986, 0.09999999999999939493 ) ;
#215284 = ORIENTED_EDGE ( 'NONE', *, *, #167427, .F. ) ;
#215285 = CYLINDRICAL_SURFACE ( 'NONE', #120080, 1.500000000000001332 ) ;
#215286 = LINE ( 'NONE', #78331, #164201 ) ;
#215287 = EDGE_LOOP ( 'NONE', ( #137745, #3463, #231629, #182806 ) ) ;
#215288 = CARTESIAN_POINT ( 'NONE',  ( 23.24999999999999645, 2.100000000011158274, -167.5000000000000284 ) ) ;
#215289 = EDGE_CURVE ( 'NONE', #208402, #14866, #186163, .T. ) ;
#215290 = CIRCLE ( 'NONE', #227752, 0.4000000000000114575 ) ;
#215291 = CARTESIAN_POINT ( 'NONE',  ( -23.15000000000000213, -4.831324760611774849, -83.96969694219879443 ) ) ;
#215292 = AXIS2_PLACEMENT_3D ( 'NONE', #373, #79885, #232607 ) ;
#215293 = AXIS2_PLACEMENT_3D ( 'NONE', #201609, #182062, #8554 ) ;
#215294 = ORIENTED_EDGE ( 'NONE', *, *, #217489, .F. ) ;
#215295 = ORIENTED_EDGE ( 'NONE', *, *, #51195, .T. ) ;
#215296 = CARTESIAN_POINT ( 'NONE',  ( 20.59588692710267921, 18.75868443233201077, -228.1998404859263303 ) ) ;
#215297 = EDGE_LOOP ( 'NONE', ( #256433, #160780, #8470, #114594, #202794, #57009, #126762, #256962, #168919, #9254, #71985, #249058, #233191, #41562, #246549, #68177, #218828, #190659 ) ) ;
#215299 = ADVANCED_FACE ( 'NONE', ( #4918 ), #87030, .F. ) ;
#215298 = EDGE_LOOP ( 'NONE', ( #25165, #128890, #205921, #123185 ) ) ;
#215301 = ORIENTED_EDGE ( 'NONE', *, *, #35354, .F. ) ;
#215300 = DIRECTION ( 'NONE',  ( 0.000000000000000000, 0.2617529984165031243, 0.9651348961777157509 ) ) ;
#215302 = ORIENTED_EDGE ( 'NONE', *, *, #201955, .T. ) ;
#215303 = EDGE_CURVE ( 'NONE', #228033, #189967, #87041, .T. ) ;
#215304 = DIRECTION ( 'NONE',  ( -1.000000000000000000, 0.000000000000000000, -0.000000000000000000 ) ) ;
#215305 = EDGE_CURVE ( 'NONE', #105344, #148418, #91174, .T. ) ;
#215308 = ORIENTED_EDGE ( 'NONE', *, *, #59685, .F. ) ;
#215307 = ORIENTED_EDGE ( 'NONE', *, *, #105230, .T. ) ;
#215306 = CARTESIAN_POINT ( 'NONE',  ( 20.94999999999999929, 18.18127959618848877, -237.5711165786817389 ) ) ;
#215309 = AXIS2_PLACEMENT_3D ( 'NONE', #26572, #184328, #108655 ) ;
#215310 = CIRCLE ( 'NONE', #102864, 0.09999999999999982514 ) ;
#215311 = AXIS2_PLACEMENT_3D ( 'NONE', #214198, #74724, #52535 ) ;
#215312 = ORIENTED_EDGE ( 'NONE', *, *, #11166, .T. ) ;
#215313 = DIRECTION ( 'NONE',  ( -0.000000000000000000, -0.9651348961777157509, 0.2617529984165031243 ) ) ;
#215314 = CARTESIAN_POINT ( 'NONE',  ( 20.94999999999999574, 64.37928932189309705, -76.39152413686537102 ) ) ;
#215315 = AXIS2_PLACEMENT_3D ( 'NONE', #64806, #145617, #144319 ) ;
#215316 = FACE_OUTER_BOUND ( 'NONE', #229441, .T. ) ;
#215317 = VERTEX_POINT ( 'NONE', #28410 ) ;
#215318 = EDGE_CURVE ( 'NONE', #77283, #79198, #143161, .T. ) ;
#215319 = CARTESIAN_POINT ( 'NONE',  ( -20.64999999999999858, 2.400000000011155432, -120.7753780772379315 ) ) ;
#215321 = ORIENTED_EDGE ( 'NONE', *, *, #106959, .F. ) ;
#215320 = DIRECTION ( 'NONE',  ( 0.000000000000000000, 0.000000000000000000, -1.000000000000000000 ) ) ;
#215322 = DIRECTION ( 'NONE',  ( 0.000000000000000000, -1.000000000000000000, -6.982962677686266711E-15 ) ) ;
#215323 = ORIENTED_EDGE ( 'NONE', *, *, #158474, .F. ) ;
#215324 = ORIENTED_EDGE ( 'NONE', *, *, #58339, .F. ) ;
#215325 = CARTESIAN_POINT ( 'NONE',  ( 20.94999999999999929, 84.73084112150795022, -193.9250327655399531 ) ) ;
#215326 = CARTESIAN_POINT ( 'NONE',  ( -21.14999999999994174, 76.00000000001119815, -3.023107484524792277 ) ) ;
#215327 = EDGE_LOOP ( 'NONE', ( #17260, #215709, #58851, #22537 ) ) ;
#215328 = ORIENTED_EDGE ( 'NONE', *, *, #137085, .F. ) ;
#215329 = CARTESIAN_POINT ( 'NONE',  ( 21.14999999999999858, 11.65000000000000391, -0.1000000000000028644 ) ) ;
#215330 = CARTESIAN_POINT ( 'NONE',  ( -20.64999999999999858, 2.761092913073515120, -213.6778149113116854 ) ) ;
#215331 = CIRCLE ( 'NONE', #69608, 0.9750000000000036415 ) ;
#215333 = ORIENTED_EDGE ( 'NONE', *, *, #55893, .T. ) ;
#215332 = ORIENTED_EDGE ( 'NONE', *, *, #158357, .T. ) ;
#215334 = ORIENTED_EDGE ( 'NONE', *, *, #119828, .T. ) ;
#215336 = EDGE_LOOP ( 'NONE', ( #64468, #164259, #186932, #114400 ) ) ;
#215335 = EDGE_CURVE ( 'NONE', #26083, #1255, #161930, .T. ) ;
#215337 = ORIENTED_EDGE ( 'NONE', *, *, #206223, .F. ) ;
#215338 = FACE_OUTER_BOUND ( 'NONE', #62101, .T. ) ;
#215339 = VERTEX_POINT ( 'NONE', #44084 ) ;
#215340 = CARTESIAN_POINT ( 'NONE',  ( 18.59999999999997655, 76.00000000001190870, -103.0231074845243029 ) ) ;
#215342 = DIRECTION ( 'NONE',  ( -1.000000000000000000, -0.000000000000000000, -0.000000000000000000 ) ) ;
#215341 = FACE_OUTER_BOUND ( 'NONE', #243896, .T. ) ;
#215343 = ORIENTED_EDGE ( 'NONE', *, *, #208449, .F. ) ;
#215345 = EDGE_CURVE ( 'NONE', #23181, #173183, #12090, .T. ) ;
#215344 = ORIENTED_EDGE ( 'NONE', *, *, #161091, .T. ) ;
#215346 = AXIS2_PLACEMENT_3D ( 'NONE', #68315, #108719, #248232 ) ;
#215347 = DIRECTION ( 'NONE',  ( 0.000000000000000000, -6.982962677686266711E-15, 1.000000000000000000 ) ) ;
#215348 = ORIENTED_EDGE ( 'NONE', *, *, #17558, .T. ) ;
#215349 = AXIS2_PLACEMENT_3D ( 'NONE', #208208, #29588, #109081 ) ;
#215350 = VECTOR ( 'NONE', #185539, 1000.000000000000000 ) ;
#215351 = EDGE_CURVE ( 'NONE', #241281, #240431, #143899, .T. ) ;
#215352 = LINE ( 'NONE', #233651, #84173 ) ;
#215353 = ORIENTED_EDGE ( 'NONE', *, *, #150017, .F. ) ;
#215354 = ORIENTED_EDGE ( 'NONE', *, *, #88142, .F. ) ;
#215355 = AXIS2_PLACEMENT_3D ( 'NONE', #34914, #114416, #15337 ) ;
#215357 = ORIENTED_EDGE ( 'NONE', *, *, #80194, .T. ) ;
#215356 = CARTESIAN_POINT ( 'NONE',  ( -16.81744102076748959, 9.950000000011138823, -121.3500000000000369 ) ) ;
#215358 = DIRECTION ( 'NONE',  ( 1.000000000000000000, 0.000000000000000000, 0.000000000000000000 ) ) ;
#215359 = DIRECTION ( 'NONE',  ( 0.000000000000000000, 1.156482317317873105E-15, -1.000000000000000000 ) ) ;
#215360 = ORIENTED_EDGE ( 'NONE', *, *, #118099, .F. ) ;
#215361 = CARTESIAN_POINT ( 'NONE',  ( -23.49999999999994316, 87.51781941433023349, -34.28670414799875488 ) ) ;
#215362 = CARTESIAN_POINT ( 'NONE',  ( 18.49999999999999289, 33.78452921692649369, -236.3958672130747800 ) ) ;
#215363 = DIRECTION ( 'NONE',  ( 0.000000000000000000, -1.000000000000000000, 0.000000000000000000 ) ) ;
#215364 = CARTESIAN_POINT ( 'NONE',  ( -23.25000000000000000, -11.74999999998884448, -137.1000000000000227 ) ) ;
#215365 = LINE ( 'NONE', #36778, #16403 ) ;
#215366 = DIRECTION ( 'NONE',  ( 0.000000000000000000, 0.000000000000000000, 1.000000000000000000 ) ) ;
#215367 = CARTESIAN_POINT ( 'NONE',  ( -22.47071067811865319, 68.27992525551360359, -69.62219993922698791 ) ) ;
#215368 = CARTESIAN_POINT ( 'NONE',  ( -18.40000000000000213, 33.87871438666832091, -235.0463117791480556 ) ) ;
#215369 = FACE_OUTER_BOUND ( 'NONE', #138207, .T. ) ;
#215370 = VERTEX_POINT ( 'NONE', #207008 ) ;
#215371 = AXIS2_PLACEMENT_3D ( 'NONE', #45950, #29003, #164626 ) ;
#215372 = ADVANCED_FACE ( 'NONE', ( #165314 ), #204423, .T. ) ;
#215374 = EDGE_LOOP ( 'NONE', ( #60204, #206756, #92712, #190771 ) ) ;
#215373 = EDGE_LOOP ( 'NONE', ( #189718, #129293, #16535, #186376 ) ) ;
#215376 = ORIENTED_EDGE ( 'NONE', *, *, #190965, .F. ) ;
#215375 = ADVANCED_FACE ( 'NONE', ( #88306 ), #167913, .F. ) ;
#215377 = COLOUR_RGB ( '', 0.72549020, 0.75294118, 0.79215686) ;
#215378 = CARTESIAN_POINT ( 'NONE',  ( -21.14250536705909411, 1.115600667400684642E-11, -93.98182782311928918 ) ) ;
#215379 =( BOUNDED_SURFACE ( )  B_SPLINE_SURFACE ( 3, 2, ( 
 ( #23193, #220088, #41472 ),
 ( #121015, #200519, #21889 ),
 ( #81817, #63563, #161413 ),
 ( #240938, #141818, #187389 ),
 ( #84363, #27050, #67423 ),
 ( #7444, #25736, #203079 ),
 ( #66143, #144365, #10020 ),
 ( #106527, #206941, #188653 ) ),
 .UNSPECIFIED., .F., .F., .F. ) 
 B_SPLINE_SURFACE_WITH_KNOTS ( ( 4, 2, 2, 4 ),
 ( 3, 3 ),
 ( 0.0001704874539069812654, 0.0003809798300636641107, 0.0004862260181420055062, 0.0005914722062203469017 ),
 ( 0.000000000000000000, 1.000000000000000000 ),
 .UNSPECIFIED. ) 
 GEOMETRIC_REPRESENTATION_ITEM ( )  RATIONAL_B_SPLINE_SURFACE ( (
 ( 1.000000000000000000, 0.7071067811865259234, 1.000000000000000000),
 ( 1.000000000000000000, 0.7670648383569823592, 1.000000000000000000),
 ( 1.000000000000000000, 0.8204820770261218588, 1.000000000000000000),
 ( 1.000000000000000000, 0.8877218296109600226, 1.000000000000000000),
 ( 1.000000000000000000, 0.9080815932658325984, 1.000000000000000000),
 ( 1.000000000000000000, 0.9395541505869027255, 1.000000000000000000),
 ( 1.000000000000000000, 0.9506520335373465080, 1.000000000000000000),
 ( 1.000000000000000000, 0.9504532311154414437, 1.000000000000000000) ) ) 
 REPRESENTATION_ITEM ( '' )  SURFACE ( )  );
#215380 = DIRECTION ( 'NONE',  ( 0.000000000000000000, 0.000000000000000000, -1.000000000000000000 ) ) ;
#215381 = AXIS2_PLACEMENT_3D ( 'NONE', #78313, #211748, #178756 ) ;
#215382 = ADVANCED_FACE ( 'NONE', ( #135149 ), #75287, .F. ) ;
#215383 = ADVANCED_FACE ( 'NONE', ( #33554 ), #83595, .F. ) ;
#215384 = AXIS2_PLACEMENT_3D ( 'NONE', #109850, #229808, #173750 ) ;
#215386 = DIRECTION ( 'NONE',  ( 0.000000000000000000, -7.086529944415886769E-15, 1.000000000000000000 ) ) ;
#215385 = CARTESIAN_POINT ( 'NONE',  ( -21.64999999999999858, 14.25671114421267127, -219.2337924566137701 ) ) ;
#215387 = VERTEX_POINT ( 'NONE', #192580 ) ;
#215388 = DIRECTION ( 'NONE',  ( -1.000000000000000000, 0.000000000000000000, 0.000000000000000000 ) ) ;
#215389 = DIRECTION ( 'NONE',  ( -4.336808689942017736E-16, 0.000000000000000000, -1.000000000000000000 ) ) ;
#215390 = DIRECTION ( 'NONE',  ( 0.000000000000000000, 0.2128009952263601179, -0.9770955615653315052 ) ) ;
#215391 = EDGE_CURVE ( 'NONE', #72316, #160017, #204245, .T. ) ;
#215392 = ORIENTED_EDGE ( 'NONE', *, *, #216985, .F. ) ;
#215393 = VERTEX_POINT ( 'NONE', #251250 ) ;
#215394 = EDGE_CURVE ( 'NONE', #140899, #38982, #13953, .T. ) ;
#215395 = VECTOR ( 'NONE', #243912, 1000.000000000000000 ) ;
#215398 = EDGE_CURVE ( 'NONE', #211446, #297, #50297, .T. ) ;
#215397 = EDGE_CURVE ( 'NONE', #236846, #114775, #229400, .T. ) ;
#215396 = AXIS2_PLACEMENT_3D ( 'NONE', #138484, #38149, #19870 ) ;
#215399 = AXIS2_PLACEMENT_3D ( 'NONE', #218951, #181136, #143270 ) ;
#215400 = ORIENTED_EDGE ( 'NONE', *, *, #93816, .T. ) ;
#215401 = FACE_OUTER_BOUND ( 'NONE', #163621, .T. ) ;
#215402 = FACE_OUTER_BOUND ( 'NONE', #78804, .T. ) ;
#215403 = CARTESIAN_POINT ( 'NONE',  ( -18.59999999999999787, 64.35000000001264198, -196.5083017138704236 ) ) ;
#215404 = CYLINDRICAL_SURFACE ( 'NONE', #90037, 0.09999999999999939493 ) ;
#215405 = DIRECTION ( 'NONE',  ( 0.000000000000000000, -0.8454177738465953329, -0.5341055959866617409 ) ) ;
#215406 = ORIENTED_EDGE ( 'NONE', *, *, #104171, .T. ) ;
#215407 = LINE ( 'NONE', #57605, #40454 ) ;
#215408 = CARTESIAN_POINT ( 'NONE',  ( 21.05000000000000071, 34.10258817885969052, -248.1818033571379658 ) ) ;
#215409 = DIRECTION ( 'NONE',  ( 1.000000000000000000, 0.000000000000000000, 0.000000000000000000 ) ) ;
#215410 = VECTOR ( 'NONE', #78436, 1000.000000000000227 ) ;
#215411 = ADVANCED_FACE ( 'NONE', ( #11378 ), #4504, .T. ) ;
#215413 = FACE_OUTER_BOUND ( 'NONE', #116102, .T. ) ;
#215412 = DIRECTION ( 'NONE',  ( 1.000000000000000000, -0.000000000000000000, -0.000000000000000000 ) ) ;
#215414 = DIRECTION ( 'NONE',  ( 1.000000000000000000, 0.000000000000000000, 0.000000000000000000 ) ) ;
#215415 = TOROIDAL_SURFACE ( 'NONE', #32281, 0.2000000000000000111, 0.1000000000000000056 ) ;
#215416 = LINE ( 'NONE', #195881, #41536 ) ;
#215417 = DIRECTION ( 'NONE',  ( -1.836970198721029934E-16, -1.000000000000000000, -6.982962677686266711E-15 ) ) ;
#215418 = DIRECTION ( 'NONE',  ( -1.000000000000000000, -2.952720810173289112E-16, 0.000000000000000000 ) ) ;
#215419 = EDGE_CURVE ( 'NONE', #89549, #145938, #188721, .T. ) ;
#215420 = EDGE_CURVE ( 'NONE', #213316, #21796, #133881, .T. ) ;
#215421 = ORIENTED_EDGE ( 'NONE', *, *, #244362, .F. ) ;
#215422 = VECTOR ( 'NONE', #183587, 1000.000000000000000 ) ;
#215423 = EDGE_LOOP ( 'NONE', ( #166692, #157423, #99600, #128330 ) ) ;
#215424 = EDGE_CURVE ( 'NONE', #193842, #156378, #91826, .T. ) ;
#215425 = DIRECTION ( 'NONE',  ( 0.000000000000000000, -0.8660254037844445918, -0.4999999999999897304 ) ) ;
#215426 = ORIENTED_EDGE ( 'NONE', *, *, #141105, .F. ) ;
#215427 = PLANE ( 'NONE',  #18092 ) ;
#215428 = EDGE_CURVE ( 'NONE', #247963, #17731, #137587, .T. ) ;
#215429 = AXIS2_PLACEMENT_3D ( 'NONE', #213701, #129356, #146337 ) ;
#215430 = CIRCLE ( 'NONE', #61314, 0.09999999999999691080 ) ;
#215431 = VECTOR ( 'NONE', #258033, 1000.000000000000000 ) ;
#215432 = CIRCLE ( 'NONE', #244648, 0.5000000000000004441 ) ;
#215433 = ADVANCED_FACE ( 'NONE', ( #152196 ), #174349, .T. ) ;
#215434 = FACE_OUTER_BOUND ( 'NONE', #252997, .T. ) ;
#215435 = ORIENTED_EDGE ( 'NONE', *, *, #195026, .T. ) ;
#215436 = AXIS2_PLACEMENT_3D ( 'NONE', #36420, #96341, #21977 ) ;
#215437 = B_SPLINE_CURVE_WITH_KNOTS ( 'NONE', 3,
 ( #72817, #166786, #67647, #147182, #253972, #200116, #198820, #213572, #192747, #54498, #100955, #179293, #240524, #42324, #119297, #180556, #233169, #21495, #94902, #1886, #234413, #20202 ),
 .UNSPECIFIED., .F., .F.,
 ( 4, 3, 3, 3, 3, 3, 3, 4 ),
 ( 0.000000000000000000, 7.307836821080901168E-06, 4.161455748548376624E-05, 7.576591810647682044E-05, 0.0001098090429817505560, 0.0001438003617351163335, 0.0001777914035423660871, 0.0002117966137403033873 ),
 .UNSPECIFIED. ) ;
#215438 = FACE_OUTER_BOUND ( 'NONE', #251388, .T. ) ;
#215439 = DIRECTION ( 'NONE',  ( 0.000000000000000000, 0.000000000000000000, -1.000000000000000000 ) ) ;
#215440 = FACE_OUTER_BOUND ( 'NONE', #49817, .T. ) ;
#215442 = ORIENTED_EDGE ( 'NONE', *, *, #247571, .T. ) ;
#215441 = DIRECTION ( 'NONE',  ( -3.265361837132813093E-16, -0.9651348961777157509, 0.2617529984165031243 ) ) ;
#215444 = DIRECTION ( 'NONE',  ( 0.000000000000000000, 0.000000000000000000, -1.000000000000000000 ) ) ;
#215443 = CARTESIAN_POINT ( 'NONE',  ( 21.05000000000000071, 6.350467579472245383, -199.7192799711882287 ) ) ;
#215445 = EDGE_CURVE ( 'NONE', #250193, #233212, #93577, .T. ) ;
#215446 = CARTESIAN_POINT ( 'NONE',  ( 23.14999999999999858, 7.554435330547283556, -235.6868924355707691 ) ) ;
#215447 = CARTESIAN_POINT ( 'NONE',  ( -22.10000000000000142, -11.75000000000000000, 12.09999999999999609 ) ) ;
#215448 = DIRECTION ( 'NONE',  ( -3.469446951953635015E-14, 1.000000000000000000, 0.000000000000000000 ) ) ;
#215449 = ORIENTED_EDGE ( 'NONE', *, *, #159742, .T. ) ;
#215450 = VECTOR ( 'NONE', #189850, 1000.000000000000000 ) ;
#215451 = DIRECTION ( 'NONE',  ( 1.000000000000000000, 0.000000000000000000, 0.000000000000000000 ) ) ;
#215452 = FACE_OUTER_BOUND ( 'NONE', #234314, .T. ) ;
#215453 = ORIENTED_EDGE ( 'NONE', *, *, #50725, .T. ) ;
#215454 = DIRECTION ( 'NONE',  ( -1.000000000000000000, 0.000000000000000000, -0.000000000000000000 ) ) ;
#215455 = ORIENTED_EDGE ( 'NONE', *, *, #156511, .F. ) ;
#215456 = VECTOR ( 'NONE', #132142, 1000.000000000000000 ) ;
#215457 = CARTESIAN_POINT ( 'NONE',  ( 18.52928932188133970, 54.95214567929434679, -230.0923768967488456 ) ) ;
#215458 = CARTESIAN_POINT ( 'NONE',  ( -16.89268316805465986, 9.951721813242182080, -20.85575247854553993 ) ) ;
#215459 = CARTESIAN_POINT ( 'NONE',  ( -18.59999999999999787, 74.16465844978715438, -57.96795619196135618 ) ) ;
#215460 = VERTEX_POINT ( 'NONE', #131314 ) ;
#215461 = VERTEX_POINT ( 'NONE', #130011 ) ;
#215462 = CARTESIAN_POINT ( 'NONE',  ( -23.15000000000000213, 4.250000000011156409, -179.8499999999999943 ) ) ;
#215463 = CARTESIAN_POINT ( 'NONE',  ( 20.94999999999999574, 10.52493806863738079, -207.3780514093641330 ) ) ;
#215464 = EDGE_CURVE ( 'NONE', #183644, #102952, #29509, .T. ) ;
#215465 = CARTESIAN_POINT ( 'NONE',  ( -22.50000000000000000, 11.65000000000000036, -3.469446951953614189E-15 ) ) ;
#215467 = DIRECTION ( 'NONE',  ( -1.000000000000000000, -0.000000000000000000, -0.000000000000000000 ) ) ;
#215466 = CARTESIAN_POINT ( 'NONE',  ( -23.25000000000000355, 20.94763808724815846, -234.7254930126486556 ) ) ;
#215468 = CIRCLE ( 'NONE', #136328, 0.1000000000000028644 ) ;
#215469 = VECTOR ( 'NONE', #56980, 1000.000000000000000 ) ;
#215470 = DIRECTION ( 'NONE',  ( 1.000000000000000000, 0.000000000000000000, 0.000000000000000000 ) ) ;
#215471 = ADVANCED_FACE ( 'NONE', ( #53058 ), #179329, .T. ) ;
#215473 = VECTOR ( 'NONE', #210152, 1000.000000000000000 ) ;
#215472 = DIRECTION ( 'NONE',  ( -1.000000000000000000, 0.000000000000000000, 0.000000000000000000 ) ) ;
#215474 = AXIS2_PLACEMENT_3D ( 'NONE', #157769, #58593, #80721 ) ;
#215475 = CARTESIAN_POINT ( 'NONE',  ( 23.24999999999999289, 6.450000000011156587, -45.85000000000000142 ) ) ;
#215476 = ORIENTED_EDGE ( 'NONE', *, *, #222787, .F. ) ;
#215477 = DIRECTION ( 'NONE',  ( -0.000000000000000000, 0.000000000000000000, -1.000000000000000000 ) ) ;
#215479 = ORIENTED_EDGE ( 'NONE', *, *, #121385, .T. ) ;
#215478 = CARTESIAN_POINT ( 'NONE',  ( 20.84999999999999432, 68.97833521811203639, -132.6895420826271277 ) ) ;
#215480 = CARTESIAN_POINT ( 'NONE',  ( 0.8999999999999992450, -8.250000000000005329, 30.04142135623731136 ) ) ;
#215481 = CARTESIAN_POINT ( 'NONE',  ( -18.59999999999999787, 1.162701749949165642, -41.60000000000000142 ) ) ;
#215483 = CARTESIAN_POINT ( 'NONE',  ( -23.15000000000000213, -8.999999999988846255, -143.3939691226524644 ) ) ;
#215482 = CARTESIAN_POINT ( 'NONE',  ( 18.39999999999999503, 64.52683809665003878, -179.2731074845244450 ) ) ;
#215484 =( BOUNDED_SURFACE ( )  B_SPLINE_SURFACE ( 3, 2, ( 
 ( #227028, #69262, #4128 ),
 ( #67958, #208771, #144912 ),
 ( #146202, #147500, #148794 ),
 ( #228331, #129225, #109642 ),
 ( #83631, #163223, #143638 ),
 ( #223170, #124101, #104489 ),
 ( #184052, #5386, #84919 ),
 ( #34013, #152667, #75685 ) ),
 .UNSPECIFIED., .F., .F., .T. ) 
 B_SPLINE_SURFACE_WITH_KNOTS ( ( 4, 2, 2, 4 ),
 ( 3, 3 ),
 ( 0.0001723339234021436671, 0.0002782939632050007717, 0.0003842540030078578491, 0.0005961740826135720041 ),
 ( 0.000000000000000000, 1.000000000000000000 ),
 .UNSPECIFIED. ) 
 GEOMETRIC_REPRESENTATION_ITEM ( )  RATIONAL_B_SPLINE_SURFACE ( (
 ( 1.000000000000000000, 0.9504532311154467727, 1.000000000000000000),
 ( 1.000000000000000000, 0.9506023220712702670, 1.000000000000000000),
 ( 1.000000000000000000, 0.9395774818177810017, 1.000000000000000000),
 ( 1.000000000000000000, 0.9079328464651014174, 1.000000000000000000),
 ( 1.000000000000000000, 0.8875702416200158540, 1.000000000000000000),
 ( 1.000000000000000000, 0.8205919608051213121, 1.000000000000000000),
 ( 1.000000000000000000, 0.7666842783589820076, 1.000000000000000000),
 ( 1.000000000000000000, 0.7071067811865475727, 1.000000000000000000) ) ) 
 REPRESENTATION_ITEM ( '' )  SURFACE ( )  );
#215485 = EDGE_CURVE ( 'NONE', #231239, #87552, #34486, .T. ) ;
#215486 = ADVANCED_FACE ( 'NONE', ( #39948 ), #196418, .T. ) ;
#215487 = VERTEX_POINT ( 'NONE', #244197 ) ;
#215489 = CARTESIAN_POINT ( 'NONE',  ( -21.05000000000000071, 1.316055977212913009, -230.7323992127457473 ) ) ;
#215488 = DIRECTION ( 'NONE',  ( -1.000000000000000000, 0.000000000000000000, 0.000000000000000000 ) ) ;
#215490 = CARTESIAN_POINT ( 'NONE',  ( 18.59999999999999787, -10.35479209691423996, -60.75654098307376216 ) ) ;
#215491 = DIRECTION ( 'NONE',  ( -1.000000000000000000, -0.000000000000000000, -0.000000000000000000 ) ) ;
#215492 = DIRECTION ( 'NONE',  ( -0.000000000000000000, 6.982962677686266711E-15, -1.000000000000000000 ) ) ;
#215493 = CARTESIAN_POINT ( 'NONE',  ( -19.89999999999999858, 1.249999999999999334, 16.50000000000000000 ) ) ;
#215494 = ORIENTED_EDGE ( 'NONE', *, *, #188015, .F. ) ;
#215495 = ADVANCED_FACE ( 'NONE', ( #163408 ), #236824, .F. ) ;
#215496 = ORIENTED_EDGE ( 'NONE', *, *, #12349, .T. ) ;
#215497 = AXIS2_PLACEMENT_3D ( 'NONE', #71907, #15802, #193134 ) ;
#215499 = AXIS2_PLACEMENT_3D ( 'NONE', #111939, #209740, #33712 ) ;
#215498 = CARTESIAN_POINT ( 'NONE',  ( -18.50000000000000000, -9.400000000000005684, -40.38204184817266906 ) ) ;
#215500 = VERTEX_POINT ( 'NONE', #98562 ) ;
#215501 = CARTESIAN_POINT ( 'NONE',  ( -22.50000000000000000, 64.35042919246788529, -203.6231074845244393 ) ) ;
#215502 = ORIENTED_EDGE ( 'NONE', *, *, #177493, .F. ) ;
#215503 = EDGE_CURVE ( 'NONE', #47203, #68795, #198992, .T. ) ;
#215505 = DIRECTION ( 'NONE',  ( 0.000000000000000000, -1.000000000000000000, -6.982962677686265922E-15 ) ) ;
#215504 = AXIS2_PLACEMENT_3D ( 'NONE', #139874, #240290, #180307 ) ;
#215506 = CARTESIAN_POINT ( 'NONE',  ( 21.05000000000000071, 1.115600667400684642E-11, -146.1500000000000341 ) ) ;
#215507 = DIRECTION ( 'NONE',  ( 1.000000000000000000, 0.000000000000000000, 0.000000000000000000 ) ) ;
#215508 = ORIENTED_EDGE ( 'NONE', *, *, #82715, .T. ) ;
#215509 = CARTESIAN_POINT ( 'NONE',  ( -22.32929514600008503, -1.515937339026276032, -193.5738536982988478 ) ) ;
#215510 = DIRECTION ( 'NONE',  ( 0.000000000000000000, 0.000000000000000000, 1.000000000000000000 ) ) ;
#215511 = DIRECTION ( 'NONE',  ( 0.000000000000000000, 0.000000000000000000, -1.000000000000000000 ) ) ;
#215512 = CARTESIAN_POINT ( 'NONE',  ( 18.59999999999999787, -11.74999999998883737, -54.85000000000000142 ) ) ;
#215513 = CARTESIAN_POINT ( 'NONE',  ( -16.94389599337535657, 66.00880201025528038, -115.6307522863227604 ) ) ;
#215514 = AXIS2_PLACEMENT_3D ( 'NONE', #116005, #134247, #57271 ) ;
#215516 = ORIENTED_EDGE ( 'NONE', *, *, #118085, .F. ) ;
#215515 = EDGE_CURVE ( 'NONE', #89756, #144975, #212649, .T. ) ;
#215517 = CARTESIAN_POINT ( 'NONE',  ( -20.94999999999999929, -4.892732937820632344, -233.2805462221312496 ) ) ;
#215519 = ORIENTED_EDGE ( 'NONE', *, *, #193954, .F. ) ;
#215518 = CIRCLE ( 'NONE', #98967, 0.09999999999999939493 ) ;
#215521 = ORIENTED_EDGE ( 'NONE', *, *, #118034, .F. ) ;
#215520 = FACE_OUTER_BOUND ( 'NONE', #20734, .T. ) ;
#215522 = VERTEX_POINT ( 'NONE', #136419 ) ;
#215523 = CYLINDRICAL_SURFACE ( 'NONE', #202798, 0.09999999999999939493 ) ;
#215524 = CARTESIAN_POINT ( 'NONE',  ( -1.820710678118658388, 85.92928932189282420, -44.87310748452424747 ) ) ;
#215525 = DIRECTION ( 'NONE',  ( 0.000000000000000000, 0.000000000000000000, -1.000000000000000000 ) ) ;
#215526 = DIRECTION ( 'NONE',  ( -0.000000000000000000, 0.8660254037844411501, 0.4999999999999956146 ) ) ;
#215527 = ORIENTED_EDGE ( 'NONE', *, *, #97299, .T. ) ;
#215528 = CARTESIAN_POINT ( 'NONE',  ( -20.64999999999999858, 85.40000000001252545, -179.9170766071767389 ) ) ;
#215529 = CIRCLE ( 'NONE', #248854, 3.999999999999999112 ) ;
#215530 = DIRECTION ( 'NONE',  ( -0.000000000000000000, 0.2128009952263604232, -0.9770955615653316162 ) ) ;
#215531 = EDGE_CURVE ( 'NONE', #155848, #217558, #38640, .T. ) ;
#215532 = ORIENTED_EDGE ( 'NONE', *, *, #153362, .F. ) ;
#215534 = ORIENTED_EDGE ( 'NONE', *, *, #253950, .T. ) ;
#215533 = CARTESIAN_POINT ( 'NONE',  ( -21.05000000000000071, 76.00000000001244871, -170.0231074845243597 ) ) ;
#215535 = EDGE_CURVE ( 'NONE', #144794, #19688, #245961, .T. ) ;
#215536 = CARTESIAN_POINT ( 'NONE',  ( 18.59999999999999076, 66.37537870982728805, -213.6053525232321704 ) ) ;
#215537 = AXIS2_PLACEMENT_3D ( 'NONE', #140815, #198211, #62565 ) ;
#215538 = CARTESIAN_POINT ( 'NONE',  ( -16.87401514999241314, 9.950000000011137047, -79.71998200746823215 ) ) ;
#215539 = ORIENTED_EDGE ( 'NONE', *, *, #115460, .F. ) ;
#215540 = AXIS2_PLACEMENT_3D ( 'NONE', #184910, #181080, #6255 ) ;
#215541 = EDGE_CURVE ( 'NONE', #12728, #223175, #150288, .T. ) ;
#215542 = CARTESIAN_POINT ( 'NONE',  ( 20.99780126800921209, 64.39461131213536760, -109.9357549128188936 ) ) ;
#215544 = ORIENTED_EDGE ( 'NONE', *, *, #1268, .T. ) ;
#215543 = AXIS2_PLACEMENT_3D ( 'NONE', #104682, #219522, #145118 ) ;
#215545 = DIRECTION ( 'NONE',  ( 0.000000000000000000, -6.853228547068871147E-15, 1.000000000000000000 ) ) ;
#215546 = CIRCLE ( 'NONE', #157125, 3.900000000000020783 ) ;
#215547 = EDGE_CURVE ( 'NONE', #161999, #145174, #175257, .T. ) ;
#215548 = CARTESIAN_POINT ( 'NONE',  ( 15.51872946208854565, 66.62341902196757815, -51.89616123751244459 ) ) ;
#215549 = EDGE_CURVE ( 'NONE', #133691, #178504, #112679, .T. ) ;
#215550 = DIRECTION ( 'NONE',  ( 0.000000000000000000, 0.000000000000000000, -1.000000000000000000 ) ) ;
#215551 = EDGE_CURVE ( 'NONE', #227951, #41664, #200158, .T. ) ;
#215552 = AXIS2_PLACEMENT_3D ( 'NONE', #168866, #230079, #51406 ) ;
#215553 = VERTEX_POINT ( 'NONE', #156045 ) ;
#215554 = FACE_OUTER_BOUND ( 'NONE', #96916, .T. ) ;
#215555 = TOROIDAL_SURFACE ( 'NONE', #119719, 4.099999999999999645, 0.1000000000000000056 ) ;
#215556 = VECTOR ( 'NONE', #85077, 1000.000000000000000 ) ;
#215557 = EDGE_LOOP ( 'NONE', ( #82812, #229427, #29734, #165315 ) ) ;
#215558 = CARTESIAN_POINT ( 'NONE',  ( -21.55000000000000071, 68.75000000001158185, -57.17310748452437252 ) ) ;
#215560 = EDGE_CURVE ( 'NONE', #57578, #104336, #20379, .T. ) ;
#215559 = DIRECTION ( 'NONE',  ( -1.000000000000000000, 0.000000000000000000, 0.000000000000000000 ) ) ;
#215562 = ORIENTED_EDGE ( 'NONE', *, *, #48003, .T. ) ;
#215561 = CARTESIAN_POINT ( 'NONE',  ( 23.14999999999999858, 6.650000000011155876, -146.3500000000000227 ) ) ;
#215563 = CARTESIAN_POINT ( 'NONE',  ( -18.40000000000000213, 5.650000000011139001, -46.15000000000000568 ) ) ;
#215565 = CIRCLE ( 'NONE', #124008, 0.1000000000000028644 ) ;
#215564 = DIRECTION ( 'NONE',  ( 1.073024830501117725E-15, -0.2128009952263604232, 0.9770955615653316162 ) ) ;
#215566 = CARTESIAN_POINT ( 'NONE',  ( -18.59999999999999787, 4.252251777740764460, -211.8999245327126744 ) ) ;
#215567 = LINE ( 'NONE', #368, #254596 ) ;
#215568 = CARTESIAN_POINT ( 'NONE',  ( -18.39999999999999858, -9.599999999988849453, -174.1001893912220737 ) ) ;
#215569 = DIRECTION ( 'NONE',  ( -0.000000000000000000, 0.9770955615653313941, 0.2128009952263603954 ) ) ;
#215570 = CARTESIAN_POINT ( 'NONE',  ( -18.48550754432078236, 85.46339977857184067, -129.4743177321095970 ) ) ;
#215572 = ORIENTED_EDGE ( 'NONE', *, *, #176143, .T. ) ;
#215571 = CARTESIAN_POINT ( 'NONE',  ( -20.85000000000000142, 77.13501884592155022, -28.30613060109199353 ) ) ;
#215573 = AXIS2_PLACEMENT_3D ( 'NONE', #20737, #221457, #123677 ) ;
#215574 = CIRCLE ( 'NONE', #44897, 0.1000000000000028644 ) ;
#215575 = DIRECTION ( 'NONE',  ( 0.000000000000000000, 0.000000000000000000, -1.000000000000000000 ) ) ;
#215576 = DIRECTION ( 'NONE',  ( 1.000000000000000000, 0.000000000000000000, 0.000000000000000000 ) ) ;
#215577 = CARTESIAN_POINT ( 'NONE',  ( 18.59999999999999432, 70.44746257310249860, -228.4383880063670347 ) ) ;
#215578 = ORIENTED_EDGE ( 'NONE', *, *, #193040, .F. ) ;
#215579 = CYLINDRICAL_SURFACE ( 'NONE', #174877, 4.049999999999998046 ) ;
#215580 = AXIS2_PLACEMENT_3D ( 'NONE', #109239, #128828, #126237 ) ;
#215581 = AXIS2_PLACEMENT_3D ( 'NONE', #25869, #31024, #165371 ) ;
#215582 = CARTESIAN_POINT ( 'NONE',  ( 23.14999999999999858, 1.115600667400684642E-11, -67.00000000000000000 ) ) ;
#215584 = VERTEX_POINT ( 'NONE', #79012 ) ;
#215583 = AXIS2_PLACEMENT_3D ( 'NONE', #222178, #183097, #8319 ) ;
#215585 = CARTESIAN_POINT ( 'NONE',  ( 18.59999999999999432, 13.63177590472475487, -238.5351604075707144 ) ) ;
#215587 = CARTESIAN_POINT ( 'NONE',  ( 21.14999999999999503, 11.48087284840413425, -198.4995883060917947 ) ) ;
#215586 = AXIS2_PLACEMENT_3D ( 'NONE', #201238, #180408, #196122 ) ;
#215588 = ORIENTED_EDGE ( 'NONE', *, *, #198015, .F. ) ;
#215589 = CARTESIAN_POINT ( 'NONE',  ( -18.39418127959864790, 11.48390560170929220, -124.7500000000000284 ) ) ;
#215590 = ORIENTED_EDGE ( 'NONE', *, *, #6621, .F. ) ;
#215591 = CARTESIAN_POINT ( 'NONE',  ( 21.05000000000000071, 88.41227409416185878, -139.5231074845242745 ) ) ;
#215592 = EDGE_CURVE ( 'NONE', #248319, #171697, #71006, .T. ) ;
#215594 = VERTEX_POINT ( 'NONE', #17766 ) ;
#215593 = FACE_OUTER_BOUND ( 'NONE', #86938, .T. ) ;
#215595 = CIRCLE ( 'NONE', #49013, 0.9000000000000014655 ) ;
#215596 = FACE_OUTER_BOUND ( 'NONE', #10201, .T. ) ;
#215597 = EDGE_LOOP ( 'NONE', ( #203125, #26457, #137680 ) ) ;
#215598 = EDGE_CURVE ( 'NONE', #149301, #35579, #241841, .T. ) ;
#215599 = LINE ( 'NONE', #57800, #47402 ) ;
#215601 = EDGE_CURVE ( 'NONE', #88487, #255725, #235541, .T. ) ;
#215600 = AXIS2_PLACEMENT_3D ( 'NONE', #229238, #70179, #31062 ) ;
#215602 = AXIS2_PLACEMENT_3D ( 'NONE', #217013, #159629, #134893 ) ;
#215603 = VERTEX_POINT ( 'NONE', #119470 ) ;
#215605 = VERTEX_POINT ( 'NONE', #124285 ) ;
#215604 = VERTEX_POINT ( 'NONE', #56880 ) ;
#215606 = CARTESIAN_POINT ( 'NONE',  ( -21.05000000000000071, 76.00000000001168132, -73.82310748452428584 ) ) ;
#215607 = VECTOR ( 'NONE', #103602, 1000.000000000000000 ) ;
#215608 = VERTEX_POINT ( 'NONE', #203802 ) ;
#215609 = DIRECTION ( 'NONE',  ( 1.000000000000000000, 0.000000000000000000, 0.000000000000000000 ) ) ;
#215610 = ORIENTED_EDGE ( 'NONE', *, *, #84653, .T. ) ;
#215611 = CIRCLE ( 'NONE', #211535, 0.1000000000000002554 ) ;
#215612 = ORIENTED_EDGE ( 'NONE', *, *, #188632, .T. ) ;
#215613 = ADVANCED_FACE ( 'NONE', ( #188101 ), #87709, .T. ) ;
#215614 = CARTESIAN_POINT ( 'NONE',  ( -20.85000000000000142, 77.16412189325258453, -28.10825939895270764 ) ) ;
#215615 = CARTESIAN_POINT ( 'NONE',  ( -23.25000000000000000, -11.74999999998884448, -70.10000000000005116 ) ) ;
#215616 = DIRECTION ( 'NONE',  ( -1.000000000000000000, 0.000000000000000000, 0.000000000000000000 ) ) ;
#215617 = EDGE_LOOP ( 'NONE', ( #170807, #10956, #157901, #149790 ) ) ;
#215618 = CARTESIAN_POINT ( 'NONE',  ( -20.64999999999999858, 66.23941198528750363, -222.8935984851895853 ) ) ;
#215619 = CARTESIAN_POINT ( 'NONE',  ( 21.05000000000000071, 28.52545328903799415, -239.5221046041717443 ) ) ;
#215620 = CARTESIAN_POINT ( 'NONE',  ( 19.99999999999998934, 11.65000000001115943, -54.75000000000000000 ) ) ;
#215621 = VECTOR ( 'NONE', #80133, 1000.000000000000000 ) ;
#215622 = VERTEX_POINT ( 'NONE', #185531 ) ;
#215623 = CARTESIAN_POINT ( 'NONE',  ( -18.40000000000000213, 11.47316190337362762, -146.6500000000000341 ) ) ;
#215624 = CARTESIAN_POINT ( 'NONE',  ( -18.33981767444368671, 38.15129771152390248, -261.2066580151159769 ) ) ;
#215625 = CARTESIAN_POINT ( 'NONE',  ( 21.04999999999999716, 65.31569084252699042, -128.9964106941975501 ) ) ;
#215626 = ORIENTED_EDGE ( 'NONE', *, *, #119588, .T. ) ;
#215627 = CARTESIAN_POINT ( 'NONE',  ( -17.04295772865507175, 14.23218548404114436, -219.2391338838992567 ) ) ;
#215628 = EDGE_LOOP ( 'NONE', ( #85446, #98539, #14030, #241623 ) ) ;
#215630 = EDGE_LOOP ( 'NONE', ( #168416, #12418, #165590, #65928 ) ) ;
#215629 = AXIS2_PLACEMENT_3D ( 'NONE', #124151, #143689, #109688 ) ;
#215631 = CARTESIAN_POINT ( 'NONE',  ( -21.64999999999999858, 7.350000000011155166, -155.2500000000000284 ) ) ;
#215632 = ORIENTED_EDGE ( 'NONE', *, *, #135729, .T. ) ;
#215633 = ORIENTED_EDGE ( 'NONE', *, *, #134121, .T. ) ;
#215634 = DIRECTION ( 'NONE',  ( -0.000000000000000000, -6.982962677686266711E-15, 1.000000000000000000 ) ) ;
#215635 = ADVANCED_FACE ( 'NONE', ( #206382 ), #148992, .F. ) ;
#215636 = CARTESIAN_POINT ( 'NONE',  ( 19.75857864376268935, 11.65000000001115943, -158.8500000000000227 ) ) ;
#215637 = ORIENTED_EDGE ( 'NONE', *, *, #151029, .T. ) ;
#215638 = ADVANCED_FACE ( 'NONE', ( #229787 ), #49862, .T. ) ;
#215639 = EDGE_LOOP ( 'NONE', ( #11317, #67324, #144033, #112390 ) ) ;
#215640 = CARTESIAN_POINT ( 'NONE',  ( 18.39999999999999858, 85.50000000001136868, -29.10844914155459051 ) ) ;
#215641 = DIRECTION ( 'NONE',  ( 0.000000000000000000, -0.2617529984172316526, -0.9651348961775180202 ) ) ;
#215642 = ORIENTED_EDGE ( 'NONE', *, *, #111327, .T. ) ;
#215643 = EDGE_CURVE ( 'NONE', #96910, #116285, #162760, .T. ) ;
#215644 = CIRCLE ( 'NONE', #61543, 0.4000000000000114575 ) ;
#215645 = CIRCLE ( 'NONE', #65628, 0.2000000000000057288 ) ;
#215646 = AXIS2_PLACEMENT_3D ( 'NONE', #180827, #2158, #161269 ) ;
#215647 = ORIENTED_EDGE ( 'NONE', *, *, #176048, .T. ) ;
#215648 = DIRECTION ( 'NONE',  ( 0.000000000000000000, 0.000000000000000000, -1.000000000000000000 ) ) ;
#215649 = FACE_OUTER_BOUND ( 'NONE', #80688, .T. ) ;
#215650 = CARTESIAN_POINT ( 'NONE',  ( -16.88815647973234135, 9.950832619326892114, -46.14721706332599638 ) ) ;
#215651 = CYLINDRICAL_SURFACE ( 'NONE', #140179, 0.09999999999999939493 ) ;
#215653 = EDGE_CURVE ( 'NONE', #65247, #168942, #139717, .T. ) ;
#215652 = CARTESIAN_POINT ( 'NONE',  ( -21.14999999999999503, 11.74999999999999467, -6.919147245958762404 ) ) ;
#215656 = DIRECTION ( 'NONE',  ( 0.000000000000000000, 0.000000000000000000, -1.000000000000000000 ) ) ;
#215655 = CIRCLE ( 'NONE', #232271, 0.4000000000000085154 ) ;
#215654 = CARTESIAN_POINT ( 'NONE',  ( 21.05000000000000071, 76.01454569058276434, -76.02012527095639882 ) ) ;
#215657 = DIRECTION ( 'NONE',  ( -3.469446951953515108E-14, -1.000000000000000000, 0.000000000000000000 ) ) ;
#215658 = CARTESIAN_POINT ( 'NONE',  ( -16.84793658983427278, 23.05180160922629895, -230.9745607765919999 ) ) ;
#215659 = CIRCLE ( 'NONE', #28273, 0.1000000000000045852 ) ;
#215660 = DIRECTION ( 'NONE',  ( 0.000000000000000000, -0.8814952561688430555, 0.4721928772777346239 ) ) ;
#215661 = DIRECTION ( 'NONE',  ( 0.000000000000000000, -1.000000000000000000, -6.982962677686265922E-15 ) ) ;
#215662 = VERTEX_POINT ( 'NONE', #91566 ) ;
#215663 = AXIS2_PLACEMENT_3D ( 'NONE', #151234, #211192, #153840 ) ;
#215664 = EDGE_CURVE ( 'NONE', #94854, #9091, #68150, .T. ) ;
#215666 = ORIENTED_EDGE ( 'NONE', *, *, #72815, .T. ) ;
#215665 = DIRECTION ( 'NONE',  ( 1.000000000000000000, 0.000000000000000000, 0.000000000000000000 ) ) ;
#215667 = CARTESIAN_POINT ( 'NONE',  ( 22.39999999999999858, 7.128833340093095217, -233.7327013124392749 ) ) ;
#215668 = EDGE_CURVE ( 'NONE', #116663, #132890, #165998, .T. ) ;
#215669 = ADVANCED_FACE ( 'NONE', ( #146377 ), #26469, .F. ) ;
#215670 = DIRECTION ( 'NONE',  ( 1.875376730785737719E-16, -1.000000000000000000, 0.000000000000000000 ) ) ;
#215671 = ORIENTED_EDGE ( 'NONE', *, *, #97986, .T. ) ;
#215672 = FACE_OUTER_BOUND ( 'NONE', #176179, .T. ) ;
#215673 = VECTOR ( 'NONE', #115680, 1000.000000000000000 ) ;
#215674 = DIRECTION ( 'NONE',  ( -1.000000000000000000, 0.000000000000000000, 0.000000000000000000 ) ) ;
#215675 = ORIENTED_EDGE ( 'NONE', *, *, #157343, .T. ) ;
#215676 = CIRCLE ( 'NONE', #253106, 0.1999999999999987899 ) ;
#215677 = AXIS2_PLACEMENT_3D ( 'NONE', #25960, #105447, #106756 ) ;
#215678 = EDGE_CURVE ( 'NONE', #75238, #79726, #125552, .T. ) ;
#215679 = DIRECTION ( 'NONE',  ( 1.000000000000000000, 0.000000000000000000, -0.000000000000000000 ) ) ;
#215680 = CARTESIAN_POINT ( 'NONE',  ( 21.30000000000002558, 0.8618440306782489957, -204.9572370243411115 ) ) ;
#215681 = ADVANCED_FACE ( 'NONE', ( #107268 ), #30324, .T. ) ;
#215682 = CYLINDRICAL_SURFACE ( 'NONE', #24537, 0.1000000000000013933 ) ;
#215684 = ORIENTED_EDGE ( 'NONE', *, *, #66326, .F. ) ;
#215683 = LINE ( 'NONE', #39668, #93734 ) ;
#215685 = AXIS2_PLACEMENT_3D ( 'NONE', #167112, #44567, #245337 ) ;
#215686 = EDGE_CURVE ( 'NONE', #217030, #195501, #200343, .T. ) ;
#215688 = ORIENTED_EDGE ( 'NONE', *, *, #207150, .F. ) ;
#215687 = CARTESIAN_POINT ( 'NONE',  ( -23.15000000000000213, 73.42097182497056451, -249.7082903213649558 ) ) ;
#215689 = DIRECTION ( 'NONE',  ( 0.000000000000000000, -0.2617529984165031243, -0.9651348961777157509 ) ) ;
#215690 = DIRECTION ( 'NONE',  ( 0.000000000000000000, -7.109473446599835262E-15, 1.000000000000000000 ) ) ;
#215691 = LINE ( 'NONE', #177887, #165722 ) ;
#215692 = DIRECTION ( 'NONE',  ( -1.000000000000000000, 0.000000000000000000, -0.000000000000000000 ) ) ;
#215693 = ADVANCED_FACE ( 'NONE', ( #87693 ), #47276, .F. ) ;
#215695 = DIRECTION ( 'NONE',  ( 0.000000000000000000, 0.000000000000000000, 1.000000000000000000 ) ) ;
#215694 = DIRECTION ( 'NONE',  ( -1.000000000000000000, -0.000000000000000000, -0.000000000000000000 ) ) ;
#215696 = CARTESIAN_POINT ( 'NONE',  ( -18.50000000000000000, 77.63717271298244782, -124.9409541190522788 ) ) ;
#215697 = DIRECTION ( 'NONE',  ( -1.000000000000000000, -1.836970198721029934E-16, -3.186635328391151676E-31 ) ) ;
#215698 = FACE_OUTER_BOUND ( 'NONE', #122041, .T. ) ;
#215699 = AXIS2_PLACEMENT_3D ( 'NONE', #53648, #194469, #229717 ) ;
#215700 = AXIS2_PLACEMENT_3D ( 'NONE', #67216, #227570, #9809 ) ;
#215701 = CARTESIAN_POINT ( 'NONE',  ( -18.50000000000000000, -1.637172712959223952, -179.0821533654719815 ) ) ;
#215702 = EDGE_CURVE ( 'NONE', #204053, #241599, #117145, .T. ) ;
#215703 = EDGE_CURVE ( 'NONE', #102805, #219709, #158678, .T. ) ;
#215704 = VECTOR ( 'NONE', #231592, 1000.000000000000000 ) ;
#215705 = VERTEX_POINT ( 'NONE', #249370 ) ;
#215706 = CARTESIAN_POINT ( 'NONE',  ( 21.05000000000000071, 87.65000000001192859, -105.9231074845242091 ) ) ;
#215707 = AXIS2_PLACEMENT_3D ( 'NONE', #177667, #218018, #180216 ) ;
#215708 = ORIENTED_EDGE ( 'NONE', *, *, #237792, .F. ) ;
#215709 = ORIENTED_EDGE ( 'NONE', *, *, #23556, .T. ) ;
#215710 = ADVANCED_FACE ( 'NONE', ( #70747 ), #150271, .T. ) ;
#215711 = LINE ( 'NONE', #236562, #40376 ) ;
#215712 = PLANE ( 'NONE',  #56970 ) ;
#215713 = ORIENTED_EDGE ( 'NONE', *, *, #231921, .F. ) ;
#215714 =( REPRESENTATION_RELATIONSHIP ('NONE','NONE', #36900, #53611 ) REPRESENTATION_RELATIONSHIP_WITH_TRANSFORMATION ( #31114 )SHAPE_REPRESENTATION_RELATIONSHIP( ) );
#215715 = ADVANCED_FACE ( 'NONE', ( #253197 ), #95416, .T. ) ;
#215716 = EDGE_CURVE ( 'NONE', #38637, #70992, #25389, .T. ) ;
#215717 = ORIENTED_EDGE ( 'NONE', *, *, #171046, .T. ) ;
#215718 = DIRECTION ( 'NONE',  ( -1.000000000000000000, -0.000000000000000000, -0.000000000000000000 ) ) ;
#215719 = EDGE_CURVE ( 'NONE', #132498, #29869, #4682, .T. ) ;
#215720 = AXIS2_PLACEMENT_3D ( 'NONE', #58320, #2206, #20528 ) ;
#215721 = ORIENTED_EDGE ( 'NONE', *, *, #247949, .T. ) ;
#215722 = AXIS2_PLACEMENT_3D ( 'NONE', #165977, #108542, #167264 ) ;
#215723 = VERTEX_POINT ( 'NONE', #14620 ) ;
#215724 = DIRECTION ( 'NONE',  ( -1.000000000000000000, 0.000000000000000000, -0.000000000000000000 ) ) ;
#215725 = DIRECTION ( 'NONE',  ( -0.000000000000000000, -6.982962677686266711E-15, 1.000000000000000000 ) ) ;
#215726 = TOROIDAL_SURFACE ( 'NONE', #78364, 4.099999999999999645, 0.1000000000000000056 ) ;
#215727 = DIRECTION ( 'NONE',  ( 0.000000000000000000, 0.7049548389605067023, -0.7092521942342977503 ) ) ;
#215728 = CARTESIAN_POINT ( 'NONE',  ( 13.22261339317536333, 9.436552840004416964, -15.17795547276030632 ) ) ;
#215729 = CIRCLE ( 'NONE', #115791, 0.2000000000000027867 ) ;
#215730 = DIRECTION ( 'NONE',  ( 1.000000000000000000, 0.000000000000000000, 0.000000000000000000 ) ) ;
#215731 = CARTESIAN_POINT ( 'NONE',  ( -22.39999999999999858, -0.09999999998884338825, -88.85042919245522341 ) ) ;
#215733 = EDGE_LOOP ( 'NONE', ( #143400, #37762, #201902, #185490, #30582, #238050, #35707 ) ) ;
#215732 = CARTESIAN_POINT ( 'NONE',  ( 21.05000000000000071, 5.900000000011162093, -190.7809002353436085 ) ) ;
#215734 = CARTESIAN_POINT ( 'NONE',  ( 23.25000000000000000, -11.74999999998883560, -179.6499999999999773 ) ) ;
#215736 = EDGE_CURVE ( 'NONE', #78857, #230044, #6257, .T. ) ;
#215735 = B_SPLINE_CURVE_WITH_KNOTS ( 'NONE', 3,
 ( #153048, #93027, #68651, #109037, #94301, #172619 ),
 .UNSPECIFIED., .F., .F.,
 ( 4, 2, 4 ),
 ( 0.000000000000000000, 0.0001496588209255842611, 0.0002993176418511685221 ),
 .UNSPECIFIED. ) ;
#215737 = CIRCLE ( 'NONE', #78189, 0.09999999999999749367 ) ;
#215738 = DIRECTION ( 'NONE',  ( 0.000000000000000000, -6.661338147750933721E-15, 1.000000000000000000 ) ) ;
#215739 = ADVANCED_FACE ( 'NONE', ( #74612 ), #168966, .T. ) ;
#215740 = VERTEX_POINT ( 'NONE', #251917 ) ;
#215741 = DIRECTION ( 'NONE',  ( 0.000000000000000000, 7.109473446599835262E-15, -1.000000000000000000 ) ) ;
#215742 = DIRECTION ( 'NONE',  ( 0.000000000000000000, 0.000000000000000000, 1.000000000000000000 ) ) ;
#215743 = ORIENTED_EDGE ( 'NONE', *, *, #211653, .T. ) ;
#215745 = LINE ( 'NONE', #197472, #116689 ) ;
#215744 = CARTESIAN_POINT ( 'NONE',  ( -23.15000000000000213, 0.000000000000000000, -21.69999999999999929 ) ) ;
#215746 = CARTESIAN_POINT ( 'NONE',  ( -21.14999999999999858, -0.09999999998884338825, -122.3504291924552234 ) ) ;
#215747 = CARTESIAN_POINT ( 'NONE',  ( 22.59999999999999432, 64.25043287652226809, -69.62396585362311896 ) ) ;
#215748 = AXIS2_PLACEMENT_3D ( 'NONE', #53077, #33569, #192599 ) ;
#215750 = EDGE_LOOP ( 'NONE', ( #209348, #221586, #23595, #137435, #25725, #150750, #104353, #110956, #70148, #204000, #96378, #91607, #221403, #112284, #98163, #244901, #36099, #111660, #196235, #229225, #153477, #18342, #20398, #250010, #257278 ) ) ;
#215749 = CIRCLE ( 'NONE', #103320, 0.1000000000000028644 ) ;
#215751 = EDGE_LOOP ( 'NONE', ( #158691, #213175, #179375 ) ) ;
#215752 = DIRECTION ( 'NONE',  ( 1.000000000000000000, 0.000000000000000000, -0.000000000000000000 ) ) ;
#215753 = CARTESIAN_POINT ( 'NONE',  ( -18.48179518609380523, -0.7053438610020049682, -242.4901111488185848 ) ) ;
#215754 = CARTESIAN_POINT ( 'NONE',  ( -18.59999999999999787, 80.78317333349157536, -192.9003134612049166 ) ) ;
#215755 = CARTESIAN_POINT ( 'NONE',  ( 23.14999999999999503, 11.65000000001116298, -79.25000000000004263 ) ) ;
#215756 = ORIENTED_EDGE ( 'NONE', *, *, #106508, .T. ) ;
#215757 = CARTESIAN_POINT ( 'NONE',  ( 15.74999999999999645, 48.12247445990688988, -234.1702647910923361 ) ) ;
#215758 = AXIS2_PLACEMENT_3D ( 'NONE', #158681, #40019, #161224 ) ;
#215759 = AXIS2_PLACEMENT_3D ( 'NONE', #114590, #132879, #211123 ) ;
#215760 = FACE_OUTER_BOUND ( 'NONE', #15559, .T. ) ;
#215761 = ADVANCED_FACE ( 'NONE', ( #15911 ), #96661, .T. ) ;
#215762 = CARTESIAN_POINT ( 'NONE',  ( -18.50000000000000000, 85.40000000001241176, -163.1084491415546438 ) ) ;
#215763 = AXIS2_PLACEMENT_3D ( 'NONE', #118969, #156831, #177679 ) ;
#215764 = EDGE_CURVE ( 'NONE', #229965, #60057, #38055, .T. ) ;
#215765 = FACE_OUTER_BOUND ( 'NONE', #96715, .T. ) ;
#215766 = CIRCLE ( 'NONE', #257414, 0.09999999999999939493 ) ;
#215767 = ORIENTED_EDGE ( 'NONE', *, *, #106778, .T. ) ;
#215768 = CARTESIAN_POINT ( 'NONE',  ( 20.94999999999999574, -11.74999999998883560, -69.90000000000004832 ) ) ;
#215769 = CARTESIAN_POINT ( 'NONE',  ( -16.87998658237743399, 66.05000000001187743, -90.15946791678636885 ) ) ;
#215770 = CARTESIAN_POINT ( 'NONE',  ( 19.99999999999998934, 64.35000000001254250, -182.2731074845244450 ) ) ;
#215771 = CARTESIAN_POINT ( 'NONE',  ( 21.05000000000000071, 10.62872031401550288, -175.1649135690876165 ) ) ;
#215773 = ORIENTED_EDGE ( 'NONE', *, *, #196185, .F. ) ;
#215772 = CARTESIAN_POINT ( 'NONE',  ( 23.24999999999999645, 76.00000000001213607, -136.5231074845242745 ) ) ;
#215774 = CARTESIAN_POINT ( 'NONE',  ( 22.48660254037844197, 64.35000000001237197, -170.0731074845244279 ) ) ;
#215775 = LINE ( 'NONE', #95824, #209175 ) ;
#215776 = DIRECTION ( 'NONE',  ( 0.000000000000000000, 1.000000000000000000, 0.000000000000000000 ) ) ;
#215777 = ORIENTED_EDGE ( 'NONE', *, *, #22766, .T. ) ;
#215778 = CARTESIAN_POINT ( 'NONE',  ( 20.94999999999999929, 5.000000000011153745, -155.0947339810869323 ) ) ;
#215779 = CYLINDRICAL_SURFACE ( 'NONE', #156764, 0.5000000000000004441 ) ;
#215780 = DIRECTION ( 'NONE',  ( 0.000000000000000000, -6.982962677686266711E-15, 1.000000000000000000 ) ) ;
#215781 = VECTOR ( 'NONE', #20466, 1000.000000000000114 ) ;
#215782 = CIRCLE ( 'NONE', #86778, 0.1000000000000028644 ) ;
#215783 = CARTESIAN_POINT ( 'NONE',  ( 23.14999999999999503, 64.35000000001195986, -110.0379132551783243 ) ) ;
#215784 = AXIS2_PLACEMENT_3D ( 'NONE', #197288, #154365, #138566 ) ;
#215785 = EDGE_CURVE ( 'NONE', #31357, #60192, #128978, .T. ) ;
#215786 = CARTESIAN_POINT ( 'NONE',  ( 18.79999999999999716, 7.900000000000000355, 1.300000000000000044 ) ) ;
#215787 = AXIS2_PLACEMENT_3D ( 'NONE', #165630, #225556, #195471 ) ;
#215788 = CARTESIAN_POINT ( 'NONE',  ( 23.15000000000000213, 28.37802281961254991, -258.4449340416662722 ) ) ;
#215789 = ORIENTED_EDGE ( 'NONE', *, *, #169125, .F. ) ;
#215790 = EDGE_LOOP ( 'NONE', ( #89077, #7248, #63002, #76709 ) ) ;
#215791 = DIRECTION ( 'NONE',  ( 0.000000000000000000, 6.982962677686266711E-15, -1.000000000000000000 ) ) ;
#215792 = CARTESIAN_POINT ( 'NONE',  ( -23.15000000000000213, 76.00000000001213607, -136.5231074845243313 ) ) ;
#215793 = CARTESIAN_POINT ( 'NONE',  ( -21.05000000000000071, 68.20313450767837082, -227.8297066677462794 ) ) ;
#215794 = CARTESIAN_POINT ( 'NONE',  ( -21.14999999999999858, 18.60615189616458309, -226.5511630304420976 ) ) ;
#215795 = ORIENTED_EDGE ( 'NONE', *, *, #230374, .F. ) ;
#215796 = CARTESIAN_POINT ( 'NONE',  ( -18.39999999999999858, -9.682403433465239573, -207.6568433774127413 ) ) ;
#215797 = AXIS2_PLACEMENT_3D ( 'NONE', #97794, #1275, #41727 ) ;
#215798 = CARTESIAN_POINT ( 'NONE',  ( 20.84451136049160880, 11.97160813258156331, -206.0623036569039357 ) ) ;
#215799 = CARTESIAN_POINT ( 'NONE',  ( -16.77828822508139694, 9.946229374920743993, -12.66262825137395254 ) ) ;
#215800 = CARTESIAN_POINT ( 'NONE',  ( -23.25000000000000000, 4.250000000011156409, -54.64999999999999858 ) ) ;
#215801 = ORIENTED_EDGE ( 'NONE', *, *, #97431, .T. ) ;
#215802 = CARTESIAN_POINT ( 'NONE',  ( -18.59999999999999787, 36.65892442174935439, -249.5511627012433848 ) ) ;
#215803 = ORIENTED_EDGE ( 'NONE', *, *, #46203, .T. ) ;
#215804 = VERTEX_POINT ( 'NONE', #70310 ) ;
#215805 = CARTESIAN_POINT ( 'NONE',  ( -21.05000000000000071, -0.09999996528894644632, -27.02244781750650304 ) ) ;
#215806 = DIRECTION ( 'NONE',  ( -1.000000000000000000, -0.000000000000000000, -0.000000000000000000 ) ) ;
#215807 = FACE_OUTER_BOUND ( 'NONE', #130571, .T. ) ;
#215808 = EDGE_LOOP ( 'NONE', ( #166371, #190766, #200511, #168208 ) ) ;
#215809 = CARTESIAN_POINT ( 'NONE',  ( -21.52071067811865746, 12.12313021711449323, -220.1078401734146723 ) ) ;
#215810 = DIRECTION ( 'NONE',  ( -1.000000000000000000, -0.000000000000000000, 0.000000000000000000 ) ) ;
#215811 = CARTESIAN_POINT ( 'NONE',  ( 15.48841904831874849, 11.05741533749496242, -211.5383459065741647 ) ) ;
#215812 = EDGE_CURVE ( 'NONE', #23430, #241950, #410, .T. ) ;
#215813 = ORIENTED_EDGE ( 'NONE', *, *, #134256, .T. ) ;
#215814 = DIRECTION ( 'NONE',  ( 0.000000000000000000, 0.9770955615653313941, 0.2128009952263606730 ) ) ;
#215816 = ORIENTED_EDGE ( 'NONE', *, *, #196254, .T. ) ;
#215815 = CARTESIAN_POINT ( 'NONE',  ( 18.49999999999999289, 65.50857864377491069, -145.1731074845244223 ) ) ;
#215818 = EDGE_CURVE ( 'NONE', #40557, #28383, #89823, .T. ) ;
#215817 = CARTESIAN_POINT ( 'NONE',  ( 23.15000000000000213, -9.599999999999999645, -23.60603087734755690 ) ) ;
#215819 = VECTOR ( 'NONE', #207501, 1000.000000000000000 ) ;
#215820 = AXIS2_PLACEMENT_3D ( 'NONE', #60231, #5372, #62808 ) ;
#215821 = AXIS2_PLACEMENT_3D ( 'NONE', #158596, #58157, #157315 ) ;
#215822 = AXIS2_PLACEMENT_3D ( 'NONE', #50268, #129817, #209356 ) ;
#215823 = ORIENTED_EDGE ( 'NONE', *, *, #160376, .F. ) ;
#215824 = CARTESIAN_POINT ( 'NONE',  ( 18.49999999999999289, 63.61019970229975229, -209.1253633388161006 ) ) ;
#215826 = EDGE_CURVE ( 'NONE', #14270, #217574, #33798, .T. ) ;
#215825 = CARTESIAN_POINT ( 'NONE',  ( -20.85000000000000142, 77.13501884592227498, -128.8061306010920362 ) ) ;
#215827 = DIRECTION ( 'NONE',  ( -1.000000000000000000, -0.000000000000000000, -0.000000000000000000 ) ) ;
#215828 = ORIENTED_EDGE ( 'NONE', *, *, #46253, .T. ) ;
#215829 = CARTESIAN_POINT ( 'NONE',  ( 21.11927991906888025, 6.448493118502571342, -133.9909163205261109 ) ) ;
#215831 = EDGE_CURVE ( 'NONE', #138584, #166820, #250198, .T. ) ;
#215830 = CARTESIAN_POINT ( 'NONE',  ( -20.64999999999999858, 4.350000000011156054, -112.8500000000000369 ) ) ;
#215832 = CARTESIAN_POINT ( 'NONE',  ( -21.14999999999999858, -11.64999999998884483, -33.50000000000000000 ) ) ;
#215833 = ORIENTED_EDGE ( 'NONE', *, *, #151337, .T. ) ;
#215834 = CIRCLE ( 'NONE', #103404, 12.97499999999998721 ) ;
#215835 = DIRECTION ( 'NONE',  ( -1.000000000000000000, 3.265361837132813093E-16, 2.280189983783949500E-30 ) ) ;
#215836 = CIRCLE ( 'NONE', #103408, 0.1000000000000028644 ) ;
#215837 = EDGE_CURVE ( 'NONE', #56828, #212994, #250235, .T. ) ;
#215838 = VERTEX_POINT ( 'NONE', #50682 ) ;
#215839 = AXIS2_PLACEMENT_3D ( 'NONE', #149646, #229170, #231740 ) ;
#215840 = ORIENTED_EDGE ( 'NONE', *, *, #57206, .T. ) ;
#215841 = DIRECTION ( 'NONE',  ( 0.000000000000000000, 6.467318590049456648E-15, -1.000000000000000000 ) ) ;
#215843 = EDGE_CURVE ( 'NONE', #161543, #185034, #137779, .T. ) ;
#215842 = CYLINDRICAL_SURFACE ( 'NONE', #167090, 0.09999999999998898659 ) ;
#215845 = ORIENTED_EDGE ( 'NONE', *, *, #3424, .F. ) ;
#215844 = CARTESIAN_POINT ( 'NONE',  ( 18.49999999999998934, 6.450000000011156587, -144.0170271704400307 ) ) ;
#215846 = DIRECTION ( 'NONE',  ( 0.000000000000000000, 0.000000000000000000, -1.000000000000000000 ) ) ;
#215847 = CARTESIAN_POINT ( 'NONE',  ( 20.94999999999999929, 61.88149656937974896, -248.1136133839584090 ) ) ;
#215848 = DIRECTION ( 'NONE',  ( -1.000000000000000000, -0.000000000000000000, -0.000000000000000000 ) ) ;
#215849 = CARTESIAN_POINT ( 'NONE',  ( -18.42637059832564361, 85.49694546190137601, -62.91403017472440951 ) ) ;
#215850 = FACE_OUTER_BOUND ( 'NONE', #1632, .T. ) ;
#215851 = CARTESIAN_POINT ( 'NONE',  ( -18.40000000000000213, 16.35463830854640932, -222.1788605317357224 ) ) ;
#215852 = CARTESIAN_POINT ( 'NONE',  ( 20.94999999999999929, -8.663551401858002876, -110.0241011180673354 ) ) ;
#215854 = ORIENTED_EDGE ( 'NONE', *, *, #82875, .T. ) ;
#215853 = CYLINDRICAL_SURFACE ( 'NONE', #177918, 0.5000000000000004441 ) ;
#215856 = ORIENTED_EDGE ( 'NONE', *, *, #36726, .T. ) ;
#215855 = DIRECTION ( 'NONE',  ( -0.000000000000000000, 0.2128009952263603677, -0.9770955615653313941 ) ) ;
#215858 = DIRECTION ( 'NONE',  ( 0.000000000000000000, -6.982962677686266711E-15, 1.000000000000000000 ) ) ;
#215857 = CARTESIAN_POINT ( 'NONE',  ( 21.05000000000000071, 5.850000000011156942, -90.36750277572213008 ) ) ;
#215860 = ORIENTED_EDGE ( 'NONE', *, *, #19328, .F. ) ;
#215859 = CARTESIAN_POINT ( 'NONE',  ( 21.05000000000000071, 85.00000000001261924, -193.6291383618718385 ) ) ;
#215861 = EDGE_LOOP ( 'NONE', ( #38270, #249914, #119916, #93468 ) ) ;
#215862 = CARTESIAN_POINT ( 'NONE',  ( -20.85000000000000142, 87.65000000001215597, -139.4231074845242802 ) ) ;
#215864 = CARTESIAN_POINT ( 'NONE',  ( 23.24999999999999645, 2.100000000011158274, -134.0000000000000284 ) ) ;
#215863 = VECTOR ( 'NONE', #131934, 1000.000000000000000 ) ;
#215865 = VECTOR ( 'NONE', #49715, 1000.000000000000000 ) ;
#215866 = LINE ( 'NONE', #175504, #209170 ) ;
#215867 = LINE ( 'NONE', #170402, #56759 ) ;
#215869 = CARTESIAN_POINT ( 'NONE',  ( -18.52643265882458579, 67.49293571122092317, -195.4648732548341741 ) ) ;
#215868 = VECTOR ( 'NONE', #215492, 1000.000000000000000 ) ;
#215870 = DIRECTION ( 'NONE',  ( 0.000000000000000000, -0.3488585713686311318, -0.9371753822965249725 ) ) ;
#215871 = ORIENTED_EDGE ( 'NONE', *, *, #237385, .T. ) ;
#215872 = ORIENTED_EDGE ( 'NONE', *, *, #84414, .T. ) ;
#215873 = DIRECTION ( 'NONE',  ( -0.000000000000000000, -6.982962677686266711E-15, 1.000000000000000000 ) ) ;
#215874 = CIRCLE ( 'NONE', #20282, 0.1999999999999987899 ) ;
#215875 = CIRCLE ( 'NONE', #24389, 12.97499999999999787 ) ;
#215876 = ORIENTED_EDGE ( 'NONE', *, *, #206828, .F. ) ;
#215877 = DIRECTION ( 'NONE',  ( 0.000000000000000000, -1.000000000000000000, 0.000000000000000000 ) ) ;
#215878 = CIRCLE ( 'NONE', #157502, 0.2000000000000005107 ) ;
#215880 = EDGE_CURVE ( 'NONE', #149532, #182718, #96273, .T. ) ;
#215879 = DIRECTION ( 'NONE',  ( -0.000000000000000000, -0.9887567792719339499, -0.1495327102803676589 ) ) ;
#215881 = AXIS2_PLACEMENT_3D ( 'NONE', #232188, #53527, #133073 ) ;
#215882 = DIRECTION ( 'NONE',  ( -0.000000000000000000, -0.000000000000000000, -1.000000000000000000 ) ) ;
#215883 = ORIENTED_EDGE ( 'NONE', *, *, #185720, .T. ) ;
#215884 = CARTESIAN_POINT ( 'NONE',  ( -20.00857864376270001, 9.150000000000002132, -21.25000000000000000 ) ) ;
#215885 = VERTEX_POINT ( 'NONE', #248929 ) ;
#215887 = EDGE_CURVE ( 'NONE', #111234, #89290, #191994, .T. ) ;
#215886 = CARTESIAN_POINT ( 'NONE',  ( -17.73285935861373019, 10.85798180380192335, -90.25856180978082932 ) ) ;
#215888 = ORIENTED_EDGE ( 'NONE', *, *, #19887, .F. ) ;
#215889 = CARTESIAN_POINT ( 'NONE',  ( -16.89146115310546037, 9.951443245667611848, -87.85482241895425659 ) ) ;
#215890 = CARTESIAN_POINT ( 'NONE',  ( -22.39999999999999858, 76.10085836911093793, -148.2726746080136877 ) ) ;
#215891 = EDGE_CURVE ( 'NONE', #41254, #201767, #146166, .T. ) ;
#215892 = CARTESIAN_POINT ( 'NONE',  ( -21.59142135623730852, 7.850000000011158718, -155.1500000000000057 ) ) ;
#215893 = EDGE_CURVE ( 'NONE', #194433, #82553, #130236, .T. ) ;
#215894 = VERTEX_POINT ( 'NONE', #149833 ) ;
#215895 = DIRECTION ( 'NONE',  ( 1.186688945009010077E-16, -1.000000000000000000, -0.000000000000000000 ) ) ;
#215896 = CIRCLE ( 'NONE', #136810, 0.1000000000000043493 ) ;
#215898 = ORIENTED_EDGE ( 'NONE', *, *, #170471, .T. ) ;
#215897 = DIRECTION ( 'NONE',  ( 0.000000000000000000, -0.9964539953858966292, -0.08413937888696132461 ) ) ;
#215899 = CARTESIAN_POINT ( 'NONE',  ( 20.94999999999999574, 47.95459712139159336, -246.5019368548292675 ) ) ;
#215900 = ORIENTED_EDGE ( 'NONE', *, *, #146996, .T. ) ;
#215901 = AXIS2_PLACEMENT_3D ( 'NONE', #251944, #73344, #155461 ) ;
#215902 = AXIS2_PLACEMENT_3D ( 'NONE', #138477, #218019, #220618 ) ;
#215903 = AXIS2_PLACEMENT_3D ( 'NONE', #131678, #192946, #115984 ) ;
#215904 = CIRCLE ( 'NONE', #24416, 0.1000000000000106914 ) ;
#215905 = DIRECTION ( 'NONE',  ( 0.000000000000000000, -1.000000000000000000, 0.000000000000000000 ) ) ;
#215906 = ORIENTED_EDGE ( 'NONE', *, *, #45110, .F. ) ;
#215907 = ADVANCED_FACE ( 'NONE', ( #147241 ), #195609, .T. ) ;
#215909 = AXIS2_PLACEMENT_3D ( 'NONE', #35613, #98081, #96799 ) ;
#215908 = CARTESIAN_POINT ( 'NONE',  ( 21.05000000000000071, 76.00000000001205080, -123.6481074845242887 ) ) ;
#215910 = DIRECTION ( 'NONE',  ( 1.000000000000000000, 0.000000000000000000, 0.000000000000000000 ) ) ;
#215911 = DIRECTION ( 'NONE',  ( 1.000000000000000000, 0.000000000000000000, 0.000000000000000000 ) ) ;
#215912 = LINE ( 'NONE', #196364, #201834 ) ;
#215913 = ADVANCED_FACE ( 'NONE', ( #231939 ), #205934, .F. ) ;
#215914 = CARTESIAN_POINT ( 'NONE',  ( -21.08198257630413508, 0.07264332379574613141, -60.66340326598497512 ) ) ;
#215915 = ORIENTED_EDGE ( 'NONE', *, *, #59247, .T. ) ;
#215916 = CYLINDRICAL_SURFACE ( 'NONE', #111014, 0.1000000000000106914 ) ;
#215917 = CARTESIAN_POINT ( 'NONE',  ( -20.94999999999999929, 64.25000000001195133, -109.8069731475024753 ) ) ;
#215918 = CARTESIAN_POINT ( 'NONE',  ( -21.05315837450580574, 11.75000000001115197, -160.6583560043927434 ) ) ;
#215919 = ORIENTED_EDGE ( 'NONE', *, *, #127757, .F. ) ;
#215920 = DIRECTION ( 'NONE',  ( 0.000000000000000000, 0.9651348961777163060, -0.2617529984165013479 ) ) ;
#215922 = ORIENTED_EDGE ( 'NONE', *, *, #252970, .T. ) ;
#215921 = AXIS2_PLACEMENT_3D ( 'NONE', #27707, #164620, #242857 ) ;
#215924 = AXIS2_PLACEMENT_3D ( 'NONE', #148782, #228313, #129210 ) ;
#215923 = DIRECTION ( 'NONE',  ( 0.000000000000000000, 0.9698110461157734008, 0.2438576117980102709 ) ) ;
#215925 = ORIENTED_EDGE ( 'NONE', *, *, #28217, .T. ) ;
#215926 = CLOSED_SHELL ( 'NONE', ( #35312, #69781, #209793, #203358, #109764, #124688, #210295, #89330, #120512, #162414, #201107, #189880, #88015, #54001, #191291, #99001, #57594, #15632, #19766, #256795, #140444, #254769, #59257, #27966, #80295, #22831, #247993, #115298, #40258, #85104, #61741, #106204, #205301, #102634, #97281, #116684, #67855, #202817, #85934, #63790, #92653, #32337, #1635, #121911, #180623, #255393, #177893, #28093, #170384, #64711, #171797, #148954, #214494, #220227, #34616, #119935, #238055, #108536, #197742, #178949, #46080, #32548, #74990, #175388, #33635, #197272, #84817, #98795, #179249, #162701, #45236, #78155, #180373, #8956, #1683, #32355, #109911, #116081, #239150, #217786, #173460, #41651, #152640, #123290, #98170, #231294, #233981, #164579, #11978, #15837, #163192, #185588, #227430, #103114, #149377, #167371, #168369, #203632, #220375, #243463, #210010, #225750, #172556, #137364, #43096, #50236, #197972, #197006, #208369, #44311, #35292, #59054, #204401, #220997, #2612, #89071, #247406, #157166, #9916, #96515, #173136, #47683, #85017, #97456, #139029, #2938, #144174, #14343, #6636, #74712, #210760, #242750, #191057, #158693, #82028, #132743, #115157, #236345, #171987, #216216, #158070, #82334, #73239, #145559, #7537, #50634, #34263, #60672, #165258, #79006, #65446, #81414, #194145, #40898, #83194, #120390, #96493, #83404, #42267, #201416, #37149, #1663, #12735, #234195, #143939, #176753, #49954, #70642, #35089, #207565, #241251, #181088, #184875, #35297, #198310, #72775, #55256, #118031, #109302, #103096, #238691, #20091, #254452, #178261, #135369, #175059, #229964, #247746, #241125, #98130, #237728, #194238, #71425, #252592, #17311, #153570, #195490, #46383, #104133, #233830, #113790, #223189, #189151, #85896, #166232, #54376, #125390, #130924, #64747, #154146, #180949, #137116, #138073, #39450, #14687, #146998, #48527, #34712, #113690, #213914, #70638, #62501, #36027, #169544, #158288, #229016, #60635, #144742, #147101, #7241, #25513, #130045, #10147, #170088, #17621, #24011, #154869, #107590, #250087, #256153, #130533, #196001, #169862, #9424, #13294, #229363, #96974, #110764, #211851, #204589, #173263, #178224, #202862, #246627, #172924, #223942, #250130, #10239, #209024, #185368, #49291, #221579, #48802, #218638, #152253, #142146, #10761, #42481, #90854, #44615, #197445, #17002, #44416, #32800, #41093, #117419, #20823, #154302, #204042, #144099, #187120, #126033, #112742, #93858, #89901, #14043, #94083, #235991, #152389, #161644, #181328, #101179, #62302, #29277, #78724, #8163, #204800, #100373, #386, #149563, #31847, #243735, #75815, #253951, #46856, #204408, #229971, #819, #20320, #226331, #86043, #237678, #72308, #88238, #46029, #12003, #232092, #207789, #123286, #221870, #107456, #9445, #135934, #50560, #221543, #164681, #37830, #174380, #109076, #221379, #40092, #80107, #11939, #236751, #164163, #120592, #190829, #236590, #86208, #44805, #232542, #163977, #242249, #7339, #73529, #27649, #115108, #114173, #212094, #181459, #85666, #42032, #124870, #117536, #197875, #63686, #192527, #233078, #103730, #241379, #215739, #5402, #64786, #134668, #156623, #124967, #196519, #64963, #52371, #79256, #91195, #66402, #70855, #60285, #80531, #168841, #129729, #32091, #168952, #191920, #155668, #192758, #28073, #250957, #221849, #32960, #47868, #82913, #192939, #36197, #85534, #175772, #221511, #242070, #147792, #162716, #125521, #250543, #178321, #226667, #254091, #121841, #67718, #132631, #155113, #85696, #128528, #70627, #176244, #49766, #233389, #118641, #205596, #44443, #213995, #229192, #183520, #231830, #37747, #30174, #139126, #143374, #62399, #223257, #205649, #221641, #71517, #29072, #140644, #96014, #61371, #61296, #192407, #190427, #189933, #58522, #9081, #229065, #237607, #94004, #192325, #210433, #85263, #55773, #103628, #235793, #231967, #224408, #145912, #107894, #85922, #162703, #183847, #55269, #124137, #251212, #246799, #193544, #177782, #95682, #61831, #111819, #241929, #172308, #213845, #140515, #211860, #68014, #177156, #13813, #73089, #112393, #16598, #118835, #223401, #174035, #244630, #29867 ) ) ;
#215927 = FACE_OUTER_BOUND ( 'NONE', #206369, .T. ) ;
#215928 = DIRECTION ( 'NONE',  ( -0.000000000000000000, -6.982962677686266711E-15, 1.000000000000000000 ) ) ;
#215929 = EDGE_CURVE ( 'NONE', #251815, #251232, #233674, .T. ) ;
#215931 = ORIENTED_EDGE ( 'NONE', *, *, #99391, .F. ) ;
#215930 = PLANE ( 'NONE',  #173916 ) ;
#215932 = EDGE_CURVE ( 'NONE', #95676, #35026, #118454, .T. ) ;
#215933 = CARTESIAN_POINT ( 'NONE',  ( -18.54159361262961525, 8.874177542791873208, -245.4029526999691200 ) ) ;
#215934 = ORIENTED_EDGE ( 'NONE', *, *, #196253, .T. ) ;
#215935 = EDGE_CURVE ( 'NONE', #163777, #66482, #58667, .T. ) ;
#215936 = CARTESIAN_POINT ( 'NONE',  ( 20.94999999999999574, 74.14897176987119565, -124.8691942151018139 ) ) ;
#215937 = VECTOR ( 'NONE', #194310, 1000.000000000000000 ) ;
#215938 = CARTESIAN_POINT ( 'NONE',  ( 20.85000000000000142, 36.22724532936083364, -235.9903003947922286 ) ) ;
#215939 = AXIS2_PLACEMENT_3D ( 'NONE', #188997, #252798, #53329 ) ;
#215940 = ORIENTED_EDGE ( 'NONE', *, *, #148070, .F. ) ;
#215941 = EDGE_LOOP ( 'NONE', ( #204135, #132015, #20364, #147109 ) ) ;
#215942 = CARTESIAN_POINT ( 'NONE',  ( -22.00356870067200177, 1.197144702919310711E-11, -126.7457576382269480 ) ) ;
#215943 = DIRECTION ( 'NONE',  ( 2.557131231893037478E-16, -0.8660254037844385966, 0.5000000000000003331 ) ) ;
#215944 = AXIS2_PLACEMENT_3D ( 'NONE', #18266, #199492, #57369 ) ;
#215945 = VERTEX_POINT ( 'NONE', #214966 ) ;
#215946 = DIRECTION ( 'NONE',  ( 1.000000000000000000, 0.000000000000000000, 0.000000000000000000 ) ) ;
#215947 = ORIENTED_EDGE ( 'NONE', *, *, #73638, .T. ) ;
#215948 = AXIS2_PLACEMENT_3D ( 'NONE', #205430, #188448, #9811 ) ;
#215949 = DIRECTION ( 'NONE',  ( 0.000000000000000000, 6.982962677686266711E-15, -1.000000000000000000 ) ) ;
#215950 = DIRECTION ( 'NONE',  ( -1.000000000000000000, 0.000000000000000000, 0.000000000000000000 ) ) ;
#215951 = ADVANCED_FACE ( 'NONE', ( #100126 ), #178442, .F. ) ;
#215952 = AXIS2_PLACEMENT_3D ( 'NONE', #186545, #209966, #7915 ) ;
#215953 = ORIENTED_EDGE ( 'NONE', *, *, #206013, .T. ) ;
#215954 = DIRECTION ( 'NONE',  ( 0.7071067811865474617, -0.7071067811865474617, -4.937700262164531476E-15 ) ) ;
#215955 = CARTESIAN_POINT ( 'NONE',  ( -20.64999999999999858, 68.85000000001200249, -115.2731074845243455 ) ) ;
#215956 = CIRCLE ( 'NONE', #186980, 0.2000000000000057288 ) ;
#215958 = ADVANCED_FACE ( 'NONE', ( #179709, #37639 ), #235808, .F. ) ;
#215957 = CARTESIAN_POINT ( 'NONE',  ( 18.49999999999999289, 28.81810206650552075, -238.0339362645743222 ) ) ;
#215959 = AXIS2_PLACEMENT_3D ( 'NONE', #61189, #100290, #117315 ) ;
#215961 = DIRECTION ( 'NONE',  ( -1.000000000000000000, -0.000000000000000000, -0.000000000000000000 ) ) ;
#215960 = DIRECTION ( 'NONE',  ( 0.000000000000000000, 0.000000000000000000, -1.000000000000000000 ) ) ;
#215962 = FACE_OUTER_BOUND ( 'NONE', #220969, .T. ) ;
#215963 = CARTESIAN_POINT ( 'NONE',  ( -20.94999999999999929, 68.17695920783671681, -227.9262201573640141 ) ) ;
#215964 = CARTESIAN_POINT ( 'NONE',  ( 18.50000000000000000, 85.40000000001137437, -29.14106563635157698 ) ) ;
#215965 = CARTESIAN_POINT ( 'NONE',  ( -18.59999999999999787, 7.070967871809997973, -137.7465642218683399 ) ) ;
#215966 = ORIENTED_EDGE ( 'NONE', *, *, #248543, .T. ) ;
#215967 = ORIENTED_EDGE ( 'NONE', *, *, #211335, .T. ) ;
#215968 = DIRECTION ( 'NONE',  ( 0.000000000000000000, 0.9126074666063772600, 0.4088369013363274407 ) ) ;
#215970 = VERTEX_POINT ( 'NONE', #216237 ) ;
#215969 = DIRECTION ( 'NONE',  ( 0.000000000000000000, 0.8814952561688444987, -0.4721928772777320149 ) ) ;
#215971 = ORIENTED_EDGE ( 'NONE', *, *, #216681, .F. ) ;
#215972 = EDGE_CURVE ( 'NONE', #46505, #80843, #212827, .T. ) ;
#215973 = CARTESIAN_POINT ( 'NONE',  ( 18.59999999999999076, 6.550000000011156231, -188.6499999999999488 ) ) ;
#215974 = EDGE_LOOP ( 'NONE', ( #164679, #147820, #97119, #5483 ) ) ;
#215975 = LINE ( 'NONE', #96034, #63560 ) ;
#215976 = AXIS2_PLACEMENT_3D ( 'NONE', #113225, #50663, #212353 ) ;
#215977 = EDGE_CURVE ( 'NONE', #80879, #26247, #121280, .T. ) ;
#215978 = EDGE_LOOP ( 'NONE', ( #238134, #179006, #48066, #106871 ) ) ;
#215980 = ADVANCED_FACE ( 'NONE', ( #233281 ), #174621, .F. ) ;
#215979 = CARTESIAN_POINT ( 'NONE',  ( 23.15000000000000213, -9.499999999988848032, -177.3939691226524076 ) ) ;
#215982 = EDGE_LOOP ( 'NONE', ( #63042, #1503, #46671 ) ) ;
#215981 = ORIENTED_EDGE ( 'NONE', *, *, #60834, .F. ) ;
#215983 = VERTEX_POINT ( 'NONE', #134137 ) ;
#215984 = VERTEX_POINT ( 'NONE', #213685 ) ;
#215985 = EDGE_LOOP ( 'NONE', ( #5571, #52746, #183561, #23824 ) ) ;
#215986 = EDGE_CURVE ( 'NONE', #217030, #251464, #46205, .T. ) ;
#215987 = DIRECTION ( 'NONE',  ( -1.000000000000000000, -0.000000000000000000, 0.000000000000000000 ) ) ;
#215988 = CARTESIAN_POINT ( 'NONE',  ( 18.49999999999999645, -1.362429037182155023, -74.88888124792120493 ) ) ;
#215991 = EDGE_CURVE ( 'NONE', #19542, #158987, #21307, .T. ) ;
#215990 = ORIENTED_EDGE ( 'NONE', *, *, #18776, .F. ) ;
#215989 = DIRECTION ( 'NONE',  ( 0.000000000000000000, 0.000000000000000000, 1.000000000000000000 ) ) ;
#215992 = DIRECTION ( 'NONE',  ( -1.000000000000000000, 0.000000000000000000, 0.000000000000000000 ) ) ;
#215993 = CARTESIAN_POINT ( 'NONE',  ( 12.84233041328156055, 12.47908687115373283, -214.0766389635194855 ) ) ;
#215995 = ORIENTED_EDGE ( 'NONE', *, *, #199277, .F. ) ;
#215994 = CARTESIAN_POINT ( 'NONE',  ( -16.91247567987036859, 60.92502281432796707, -221.0598840834026930 ) ) ;
#215996 = CARTESIAN_POINT ( 'NONE',  ( -18.59999999999999787, -1.866714910046153308, -179.2526752462819672 ) ) ;
#215997 = ORIENTED_EDGE ( 'NONE', *, *, #110446, .F. ) ;
#215998 = DIRECTION ( 'NONE',  ( -1.000000000000000000, 0.000000000000000000, -0.000000000000000000 ) ) ;
#216000 = VERTEX_POINT ( 'NONE', #57151 ) ;
#215999 = DIRECTION ( 'NONE',  ( 1.000000000000000000, 0.000000000000000000, 0.000000000000000000 ) ) ;
#216001 = DIRECTION ( 'NONE',  ( 0.000000000000000000, -0.2128009952263485993, 0.9770955615653341697 ) ) ;
#216002 = CARTESIAN_POINT ( 'NONE',  ( 20.94999999999999929, 4.850467289730776344, -188.9657325909983001 ) ) ;
#216003 = CARTESIAN_POINT ( 'NONE',  ( 19.94784844284971115, 11.71308993304012525, -91.70219871729848649 ) ) ;
#216004 = VERTEX_POINT ( 'NONE', #35095 ) ;
#216005 = VECTOR ( 'NONE', #106777, 1000.000000000000000 ) ;
#216008 = DIRECTION ( 'NONE',  ( 0.000000000000000000, 0.9126074666063791474, 0.4088369013363231108 ) ) ;
#216007 = AXIS2_PLACEMENT_3D ( 'NONE', #51426, #110146, #190998 ) ;
#216006 = CARTESIAN_POINT ( 'NONE',  ( -18.59999999999999787, 7.633102355717365839, -241.5185714324494484 ) ) ;
#216009 = CIRCLE ( 'NONE', #249362, 0.1000000000000028644 ) ;
#216010 = CARTESIAN_POINT ( 'NONE',  ( -22.84999999999999787, 0.000000000000000000, 3.900000000000000355 ) ) ;
#216011 = EDGE_CURVE ( 'NONE', #163693, #56126, #192871, .T. ) ;
#216012 = CARTESIAN_POINT ( 'NONE',  ( 21.00000000000000000, -0.04453801223857078301, 0.3305886640091971196 ) ) ;
#216013 = LINE ( 'NONE', #20416, #243283 ) ;
#216014 = ADVANCED_FACE ( 'NONE', ( #254083 ), #78016, .T. ) ;
#216015 = EDGE_LOOP ( 'NONE', ( #21685, #28676, #85273, #173903, #86364, #156707, #21562, #43400, #91385, #78432, #32551, #58656 ) ) ;
#216016 = ORIENTED_EDGE ( 'NONE', *, *, #187529, .F. ) ;
#216017 = DIRECTION ( 'NONE',  ( 0.000000000000000000, -0.9908441862701411473, 0.1350103645453267498 ) ) ;
#216018 = CIRCLE ( 'NONE', #24517, 0.1000000000000028644 ) ;
#216019 = CARTESIAN_POINT ( 'NONE',  ( 18.59999999999999432, 74.27191306321758191, -116.1386724793565577 ) ) ;
#216020 = ORIENTED_EDGE ( 'NONE', *, *, #254850, .F. ) ;
#216021 = CARTESIAN_POINT ( 'NONE',  ( 23.24999999999999289, 6.450000000011156587, -188.6499999999999488 ) ) ;
#216022 = VERTEX_POINT ( 'NONE', #237105 ) ;
#216023 = EDGE_CURVE ( 'NONE', #187977, #238808, #162951, .T. ) ;
#216024 = CARTESIAN_POINT ( 'NONE',  ( -5.999999999999938716, 64.65000000001120384, -26.02310748452479316 ) ) ;
#216025 = CARTESIAN_POINT ( 'NONE',  ( -21.93340585898181061, 76.00000000001243450, -177.3472545066570945 ) ) ;
#216026 = VECTOR ( 'NONE', #173989, 1000.000000000000000 ) ;
#216027 = AXIS2_PLACEMENT_3D ( 'NONE', #71740, #173451, #152579 ) ;
#216028 = EDGE_CURVE ( 'NONE', #130397, #132961, #59720, .T. ) ;
#216029 = ORIENTED_EDGE ( 'NONE', *, *, #192125, .F. ) ;
#216030 = VECTOR ( 'NONE', #101320, 1000.000000000000000 ) ;
#216031 = DIRECTION ( 'NONE',  ( 0.000000000000000000, 0.8814952561688476074, -0.4721928772777262417 ) ) ;
#216032 =( LENGTH_UNIT ( ) NAMED_UNIT ( * ) SI_UNIT ( .MILLI., .METRE. ) );
#216033 = ADVANCED_FACE ( 'NONE', ( #222649 ), #222204, .T. ) ;
#216034 = EDGE_LOOP ( 'NONE', ( #122818, #60076, #130030 ) ) ;
#216035 = AXIS2_PLACEMENT_3D ( 'NONE', #90602, #170214, #249698 ) ;
#216036 = VERTEX_POINT ( 'NONE', #204377 ) ;
#216037 = VERTEX_POINT ( 'NONE', #201820 ) ;
#216038 = EDGE_CURVE ( 'NONE', #139587, #257124, #2319, .T. ) ;
#216039 = DIRECTION ( 'NONE',  ( -1.000000000000000000, 0.000000000000000000, 0.000000000000000000 ) ) ;
#216040 = CARTESIAN_POINT ( 'NONE',  ( 22.50000000000000000, 75.90000000001276703, -215.1726782920691505 ) ) ;
#216041 = CARTESIAN_POINT ( 'NONE',  ( -21.14999999999999858, 1.115600667400684642E-11, -127.4593430482987912 ) ) ;
#216042 = DIRECTION ( 'NONE',  ( 1.000000000000000000, 7.304098846218134667E-16, 4.639676173203993355E-30 ) ) ;
#216043 = CARTESIAN_POINT ( 'NONE',  ( 15.07585980824113392, 66.58236703690573677, -118.3741590187920991 ) ) ;
#216044 = DIRECTION ( 'NONE',  ( 0.000000000000000000, 1.000000000000000000, 0.000000000000000000 ) ) ;
#216045 = CARTESIAN_POINT ( 'NONE',  ( -21.05000000000000071, 74.16465844978819177, -191.9679561919613775 ) ) ;
#216047 = ORIENTED_EDGE ( 'NONE', *, *, #24841, .F. ) ;
#216046 = FACE_OUTER_BOUND ( 'NONE', #236564, .T. ) ;
#216048 = DIRECTION ( 'NONE',  ( -0.000000000000000000, 0.2128009952263604232, -0.9770955615653316162 ) ) ;
#216049 = ORIENTED_EDGE ( 'NONE', *, *, #5094, .F. ) ;
#216050 = CARTESIAN_POINT ( 'NONE',  ( -18.43473496883411045, -9.494952410988167557, -141.0458715722282648 ) ) ;
#216051 = ADVANCED_FACE ( 'NONE', ( #42749 ), #184817, .T. ) ;
#216052 = ORIENTED_EDGE ( 'NONE', *, *, #32141, .T. ) ;
#216053 = ORIENTED_EDGE ( 'NONE', *, *, #59501, .T. ) ;
#216054 = DIRECTION ( 'NONE',  ( 0.000000000000000000, -0.09425075112712516523, -0.9955484899852807823 ) ) ;
#216055 = CARTESIAN_POINT ( 'NONE',  ( 22.39999999999999503, 0.1000000000111554016, -159.7092204016265669 ) ) ;
#216056 = FACE_OUTER_BOUND ( 'NONE', #122746, .T. ) ;
#216057 = VERTEX_POINT ( 'NONE', #162711 ) ;
#216058 = CARTESIAN_POINT ( 'NONE',  ( -21.05000000000000071, 56.55376719376374695, -240.6385182521135278 ) ) ;
#216059 = AXIS2_PLACEMENT_3D ( 'NONE', #257940, #2367, #122339 ) ;
#216060 = VECTOR ( 'NONE', #61579, 1000.000000000000000 ) ;
#216061 = FACE_OUTER_BOUND ( 'NONE', #127956, .T. ) ;
#216062 = EDGE_LOOP ( 'NONE', ( #129839, #47813, #14268, #3691 ) ) ;
#216063 = VERTEX_POINT ( 'NONE', #4872 ) ;
#216064 = CARTESIAN_POINT ( 'NONE',  ( 20.94999999999999929, 34.10258817885969052, -248.1818033571379658 ) ) ;
#216065 = VERTEX_POINT ( 'NONE', #61018 ) ;
#216066 = CARTESIAN_POINT ( 'NONE',  ( -21.05000000000000071, 76.00000000001267608, -203.5231074845243597 ) ) ;
#216067 = DIRECTION ( 'NONE',  ( 0.000000000000000000, 1.000000000000000000, 0.000000000000000000 ) ) ;
#216068 = EDGE_LOOP ( 'NONE', ( #228083, #249352, #182968, #229043 ) ) ;
#216070 = CARTESIAN_POINT ( 'NONE',  ( -20.54999999999999716, 7.250000000011155521, -146.2500000000000284 ) ) ;
#216069 = AXIS2_PLACEMENT_3D ( 'NONE', #250011, #94780, #16550 ) ;
#216071 = DIRECTION ( 'NONE',  ( 1.000000000000000000, 0.000000000000000000, 0.000000000000000000 ) ) ;
#216072 = DIRECTION ( 'NONE',  ( -1.000000000000000000, -0.000000000000000000, -0.000000000000000000 ) ) ;
#216073 = ORIENTED_EDGE ( 'NONE', *, *, #34551, .F. ) ;
#216074 = DIRECTION ( 'NONE',  ( -0.000000000000000000, 0.9770955615653313941, 0.2128009952263603954 ) ) ;
#216075 = CARTESIAN_POINT ( 'NONE',  ( 20.27550659511088682, 9.216043722520002035, -42.75000000000000000 ) ) ;
#216076 = VECTOR ( 'NONE', #39891, 1000.000000000000000 ) ;
#216077 = CARTESIAN_POINT ( 'NONE',  ( -22.49510344025093644, 25.99963044612954022, -254.2528391593452000 ) ) ;
#216078 = VECTOR ( 'NONE', #6633, 1000.000000000000000 ) ;
#216079 = AXIS2_PLACEMENT_3D ( 'NONE', #248948, #246373, #131554 ) ;
#216080 = ORIENTED_EDGE ( 'NONE', *, *, #193921, .F. ) ;
#216081 = AXIS2_PLACEMENT_3D ( 'NONE', #7040, #147856, #86550 ) ;
#216083 = EDGE_CURVE ( 'NONE', #194690, #56718, #67902, .T. ) ;
#216082 = CARTESIAN_POINT ( 'NONE',  ( 21.09551895715246772, 10.62143732716875100, -12.23712466589941883 ) ) ;
#216084 = ORIENTED_EDGE ( 'NONE', *, *, #203559, .F. ) ;
#216085 = DIRECTION ( 'NONE',  ( -1.000000000000000000, 0.000000000000000000, 0.000000000000000000 ) ) ;
#216086 = DIRECTION ( 'NONE',  ( 2.952720810173289112E-16, -1.000000000000000000, -0.000000000000000000 ) ) ;
#216087 = DIRECTION ( 'NONE',  ( 1.000000000000000000, 0.000000000000000000, 0.000000000000000000 ) ) ;
#216089 = AXIS2_PLACEMENT_3D ( 'NONE', #58883, #154211, #214139 ) ;
#216088 = LINE ( 'NONE', #17889, #135779 ) ;
#216090 = CARTESIAN_POINT ( 'NONE',  ( -20.94999999999999929, 74.83729825007431202, -161.9231074845243654 ) ) ;
#216091 = CARTESIAN_POINT ( 'NONE',  ( -21.05000000000000071, 69.16514130714681130, -247.7543978865853660 ) ) ;
#216092 = AXIS2_PLACEMENT_3D ( 'NONE', #48079, #49373, #204580 ) ;
#216093 = ORIENTED_EDGE ( 'NONE', *, *, #221140, .T. ) ;
#216094 = CARTESIAN_POINT ( 'NONE',  ( -20.64999999999999858, 66.26558728512915764, -222.7970849955717938 ) ) ;
#216095 = CARTESIAN_POINT ( 'NONE',  ( 21.11747605621531321, 67.22129199451916293, -124.2785443147345745 ) ) ;
#216096 = CARTESIAN_POINT ( 'NONE',  ( -22.39999999999999858, -0.1008583690987135961, 11.74956712348939192 ) ) ;
#216097 = DIRECTION ( 'NONE',  ( 1.000000000000000000, -0.000000000000000000, -0.000000000000000000 ) ) ;
#216098 = EDGE_CURVE ( 'NONE', #196307, #232013, #227026, .T. ) ;
#216099 = CARTESIAN_POINT ( 'NONE',  ( 20.77766267348356166, 65.55095760939242666, -61.93039856864697157 ) ) ;
#216100 = AXIS2_PLACEMENT_3D ( 'NONE', #83551, #243932, #105683 ) ;
#216101 = CONICAL_SURFACE ( 'NONE', #166257, 4.049999999999996270, 0.7853981633974604915 ) ;
#216103 = VERTEX_POINT ( 'NONE', #47862 ) ;
#216102 = VECTOR ( 'NONE', #250350, 1000.000000000000000 ) ;
#216104 = ORIENTED_EDGE ( 'NONE', *, *, #105928, .F. ) ;
#216105 = DIRECTION ( 'NONE',  ( 0.000000000000000000, 0.000000000000000000, -1.000000000000000000 ) ) ;
#216106 = CIRCLE ( 'NONE', #37080, 0.2000000000000005107 ) ;
#216107 = SPHERICAL_SURFACE ( 'NONE', #242659, 0.1000000000000000056 ) ;
#216108 = DIRECTION ( 'NONE',  ( 1.000000000000000000, -0.000000000000000000, -0.000000000000000000 ) ) ;
#216109 = CARTESIAN_POINT ( 'NONE',  ( 18.49999999999998934, 6.550000000011156231, -121.7500000000000426 ) ) ;
#216110 =( BOUNDED_SURFACE ( )  B_SPLINE_SURFACE ( 3, 2, ( 
 ( #167984, #247481, #10165 ),
 ( #248779, #38715, #16599 ),
 ( #75295, #120844, #41304 ),
 ( #58251, #137785, #253889 ),
 ( #136496, #217318, #234328 ),
 ( #255127, #157409, #76538 ) ),
 .UNSPECIFIED., .F., .F., .F. ) 
 B_SPLINE_SURFACE_WITH_KNOTS ( ( 4, 2, 4 ),
 ( 3, 3 ),
 ( 0.0001300404313046571046, 0.0003183318589266621477, 0.0005066232865486671637 ),
 ( 0.000000000000000000, 1.000000000000000000 ),
 .UNSPECIFIED. ) 
 GEOMETRIC_REPRESENTATION_ITEM ( )  RATIONAL_B_SPLINE_SURFACE ( (
 ( 1.000000000000000000, 0.7071067811865475727, 1.000000000000000000),
 ( 1.000000000000000000, 0.7625113560541822988, 1.000000000000000000),
 ( 1.000000000000000000, 0.8126073484686407999, 1.000000000000000000),
 ( 1.000000000000000000, 0.8923049332734508399, 1.000000000000000000),
 ( 1.000000000000000000, 0.9231914937768306295, 1.000000000000000000),
 ( 1.000000000000000000, 0.9238795325112714174, 1.000000000000000000) ) ) 
 REPRESENTATION_ITEM ( '' )  SURFACE ( )  );
#216111 = FACE_OUTER_BOUND ( 'NONE', #71974, .T. ) ;
#216112 = AXIS2_PLACEMENT_3D ( 'NONE', #231109, #207686, #169876 ) ;
#216113 = VERTEX_POINT ( 'NONE', #166576 ) ;
#216114 = DIRECTION ( 'NONE',  ( -1.000000000000000000, 0.000000000000000000, 0.000000000000000000 ) ) ;
#216115 = DIRECTION ( 'NONE',  ( 1.000000000000000000, -0.000000000000000000, -0.000000000000000000 ) ) ;
#216116 = EDGE_LOOP ( 'NONE', ( #168449, #249014, #171737, #163459 ) ) ;
#216117 = CARTESIAN_POINT ( 'NONE',  ( -23.15000000000000213, -9.599999999988847676, -76.89396912265249284 ) ) ;
#216118 = PRODUCT_DEFINITION_SHAPE ( 'NONE', 'NONE',  #258123 ) ;
#216119 = DIRECTION ( 'NONE',  ( 0.000000000000000000, -0.2617529984165701262, -0.9651348961776977653 ) ) ;
#216120 = AXIS2_PLACEMENT_3D ( 'NONE', #2512, #182473, #85883 ) ;
#216121 = VERTEX_POINT ( 'NONE', #231674 ) ;
#216122 = CARTESIAN_POINT ( 'NONE',  ( -21.00448002041627049, 12.93820659955309615, -205.1910717667425104 ) ) ;
#216123 = EDGE_LOOP ( 'NONE', ( #65830, #138624, #186159, #216608 ) ) ;
#216124 = DIRECTION ( 'NONE',  ( 1.000000000000000000, 0.000000000000000000, 0.000000000000000000 ) ) ;
#216125 = CARTESIAN_POINT ( 'NONE',  ( 21.05000000000000071, 69.74115287693328469, -170.0548658375798823 ) ) ;
#216126 = DIRECTION ( 'NONE',  ( 1.000000000000000000, 0.000000000000000000, 0.000000000000000000 ) ) ;
#216127 = CARTESIAN_POINT ( 'NONE',  ( 22.47071067811865319, 75.90090754530983475, -177.7431822290224090 ) ) ;
#216129 = CIRCLE ( 'NONE', #103682, 0.1000000000000028644 ) ;
#216128 = DIRECTION ( 'NONE',  ( 1.000000000000000000, -0.000000000000000000, -0.000000000000000000 ) ) ;
#216130 = CARTESIAN_POINT ( 'NONE',  ( -20.64999999999999858, 76.00000000001165290, -69.52310748452431710 ) ) ;
#216131 = DIRECTION ( 'NONE',  ( 0.000000000000000000, 1.000000000000000000, 6.982962677686266711E-15 ) ) ;
#216132 = EDGE_CURVE ( 'NONE', #179043, #208600, #189625, .T. ) ;
#216133 = DIRECTION ( 'NONE',  ( 0.000000000000000000, -6.982962677686267499E-15, 1.000000000000000000 ) ) ;
#216134 = AXIS2_PLACEMENT_3D ( 'NONE', #150162, #194425, #95300 ) ;
#216135 = CARTESIAN_POINT ( 'NONE',  ( -20.85000000000000142, -1.263275465206102233, -208.9018646667463770 ) ) ;
#216136 = CARTESIAN_POINT ( 'NONE',  ( 21.05000000000000071, -11.38316329222461576, -203.4791315943886048 ) ) ;
#216137 = AXIS2_PLACEMENT_3D ( 'NONE', #250153, #88479, #53234 ) ;
#216138 = DIRECTION ( 'NONE',  ( -0.000000000000000000, -2.891205793294679805E-16, 1.000000000000000000 ) ) ;
#216139 = DIRECTION ( 'NONE',  ( -0.000000000000000000, -0.1618390714546093789, 0.9868171638914220445 ) ) ;
#216140 = CARTESIAN_POINT ( 'NONE',  ( 18.50596464788227280, 10.30632246271648889, -206.5041836778895572 ) ) ;
#216141 = DIRECTION ( 'NONE',  ( 0.000000000000000000, 0.000000000000000000, -1.000000000000000000 ) ) ;
#216142 = CARTESIAN_POINT ( 'NONE',  ( 20.85000000000000142, 56.23643450586806836, -227.9054833905874204 ) ) ;
#216143 = AXIS2_PLACEMENT_3D ( 'NONE', #133604, #110187, #34538 ) ;
#216144 = EDGE_LOOP ( 'NONE', ( #197885, #119121, #65556, #167120, #115840, #62704 ) ) ;
#216145 = LINE ( 'NONE', #179616, #81332 ) ;
#216147 = EDGE_CURVE ( 'NONE', #116664, #29779, #89562, .T. ) ;
#216146 = CARTESIAN_POINT ( 'NONE',  ( -20.64999999999999858, 0.000000000000000000, -12.87499999999999822 ) ) ;
#216148 = ORIENTED_EDGE ( 'NONE', *, *, #31968, .T. ) ;
#216150 = EDGE_CURVE ( 'NONE', #147651, #237661, #90848, .T. ) ;
#216149 = DIRECTION ( 'NONE',  ( 0.000000000000000000, -1.776356839400308840E-15, 1.000000000000000000 ) ) ;
#216151 = CIRCLE ( 'NONE', #124418, 0.1000000000000024342 ) ;
#216152 = DIRECTION ( 'NONE',  ( 0.000000000000000000, 0.000000000000000000, 1.000000000000000000 ) ) ;
#216153 = AXIS2_PLACEMENT_3D ( 'NONE', #218166, #138621, #60392 ) ;
#216154 = VERTEX_POINT ( 'NONE', #246097 ) ;
#216155 = CARTESIAN_POINT ( 'NONE',  ( 21.05000000000000071, 6.093673009692411213, -199.5727803633481301 ) ) ;
#216156 = ADVANCED_FACE ( 'NONE', ( #212106 ), #251199, .F. ) ;
#216157 = ORIENTED_EDGE ( 'NONE', *, *, #114540, .F. ) ;
#216158 = TOROIDAL_SURFACE ( 'NONE', #16284, 0.2000000000000000111, 0.1000000000000000056 ) ;
#216159 = ORIENTED_EDGE ( 'NONE', *, *, #123051, .F. ) ;
#216160 = CARTESIAN_POINT ( 'NONE',  ( 13.99999999999999822, 9.850000000011137402, -117.2500000000000284 ) ) ;
#216161 = VERTEX_POINT ( 'NONE', #208256 ) ;
#216162 = ADVANCED_FACE ( 'NONE', ( #206960 ), #71321, .T. ) ;
#216164 =( BOUNDED_SURFACE ( )  B_SPLINE_SURFACE ( 3, 2, ( 
 ( #245745, #149229, #227448 ),
 ( #4544, #123227, #5819 ),
 ( #164918, #147931, #28006 ),
 ( #226135, #67102, #228759 ),
 ( #9687, #125780, #205305 ),
 ( #85345, #86630, #187070 ) ),
 .UNSPECIFIED., .F., .F., .F. ) 
 B_SPLINE_SURFACE_WITH_KNOTS ( ( 4, 2, 4 ),
 ( 3, 3 ),
 ( 0.0001300404313046550988, 0.0003183318589266566725, 0.0005066232865486582733 ),
 ( 0.000000000000000000, 1.000000000000000000 ),
 .UNSPECIFIED. ) 
 GEOMETRIC_REPRESENTATION_ITEM ( )  RATIONAL_B_SPLINE_SURFACE ( (
 ( 1.000000000000000000, 0.7071067811865352493, 1.000000000000000000),
 ( 1.000000000000000000, 0.7625113560536035395, 1.000000000000000000),
 ( 1.000000000000000000, 0.8126073484694493754, 1.000000000000000000),
 ( 1.000000000000000000, 0.8923049332726276095, 1.000000000000000000),
 ( 1.000000000000000000, 0.9231914937774379215, 1.000000000000000000),
 ( 1.000000000000000000, 0.9238795325112713064, 1.000000000000000000) ) ) 
 REPRESENTATION_ITEM ( '' )  SURFACE ( )  );
#216163 = CARTESIAN_POINT ( 'NONE',  ( 21.05000000000000071, -1.124859753953710850E-15, 6.540656951701244282 ) ) ;
#216165 = LINE ( 'NONE', #37558, #166068 ) ;
#216166 = CARTESIAN_POINT ( 'NONE',  ( -21.05000000000000071, 70.15000000001198543, -113.1556047088022581 ) ) ;
#216167 = DIRECTION ( 'NONE',  ( -1.000000000000000000, 0.000000000000000000, 0.000000000000000000 ) ) ;
#216168 = DIRECTION ( 'NONE',  ( -1.000000000000000000, -7.304098846218163263E-16, 4.217023435051627211E-16 ) ) ;
#216169 = CARTESIAN_POINT ( 'NONE',  ( -13.12432614554022514, 46.70278183066206878, -234.7177704364561350 ) ) ;
#216170 = EDGE_CURVE ( 'NONE', #189375, #212285, #152234, .T. ) ;
#216171 = CARTESIAN_POINT ( 'NONE',  ( 18.59999999999999787, 77.83534155023670564, -158.3679561919613548 ) ) ;
#216173 = ORIENTED_EDGE ( 'NONE', *, *, #238707, .F. ) ;
#216172 = CARTESIAN_POINT ( 'NONE',  ( -23.25000000000000000, 87.75000000001202238, -114.7731074845242318 ) ) ;
#216174 = ORIENTED_EDGE ( 'NONE', *, *, #112123, .F. ) ;
#216176 = CARTESIAN_POINT ( 'NONE',  ( -17.11825945287481332, 62.96304356361481780, -213.1979597767049484 ) ) ;
#216175 = DIRECTION ( 'NONE',  ( 1.000000000000000000, 0.000000000000000000, 0.000000000000000000 ) ) ;
#216178 = VERTEX_POINT ( 'NONE', #158560 ) ;
#216177 = DIRECTION ( 'NONE',  ( -1.000000000000000000, 0.000000000000000000, 0.000000000000000000 ) ) ;
#216179 = ORIENTED_EDGE ( 'NONE', *, *, #109401, .F. ) ;
#216180 = CARTESIAN_POINT ( 'NONE',  ( -16.90128866880176872, 66.04620422280927983, -149.1604313011357874 ) ) ;
#216181 = CARTESIAN_POINT ( 'NONE',  ( -21.05000000000000071, -1.249999999988843369, -41.50000000000000000 ) ) ;
#216182 = CARTESIAN_POINT ( 'NONE',  ( 18.50000000000000000, -9.399999999999979039, -7.297259759663266898 ) ) ;
#216183 = FACE_OUTER_BOUND ( 'NONE', #119867, .T. ) ;
#216184 = CARTESIAN_POINT ( 'NONE',  ( -20.54999999999999716, 68.85000000001156195, -57.27310748452436684 ) ) ;
#216185 = DIRECTION ( 'NONE',  ( -1.000000000000000000, -0.000000000000000000, -0.000000000000000000 ) ) ;
#216186 = EDGE_CURVE ( 'NONE', #211780, #68319, #36037, .T. ) ;
#216187 = DIRECTION ( 'NONE',  ( -1.000000000000000000, 0.000000000000000000, 0.000000000000000000 ) ) ;
#216188 = AXIS2_PLACEMENT_3D ( 'NONE', #2220, #218700, #120935 ) ;
#216189 = VERTEX_POINT ( 'NONE', #15189 ) ;
#216190 = ORIENTED_EDGE ( 'NONE', *, *, #57421, .F. ) ;
#216191 = CARTESIAN_POINT ( 'NONE',  ( -23.25000000000000000, 28.37802281961254636, -258.4449340416662722 ) ) ;
#216192 = CIRCLE ( 'NONE', #107870, 4.000000000000000000 ) ;
#216193 = AXIS2_PLACEMENT_3D ( 'NONE', #249701, #224973, #71081 ) ;
#216194 = VERTEX_POINT ( 'NONE', #256276 ) ;
#216195 = LINE ( 'NONE', #213645, #167621 ) ;
#216196 = VERTEX_POINT ( 'NONE', #13900 ) ;
#216197 = DIRECTION ( 'NONE',  ( 0.000000000000000000, 0.000000000000000000, 1.000000000000000000 ) ) ;
#216198 =( BOUNDED_CURVE ( )  B_SPLINE_CURVE ( 3, ( #202302, #103178, #182754, #4094 ),
 .UNSPECIFIED., .F., .F. ) 
 B_SPLINE_CURVE_WITH_KNOTS ( ( 4, 4 ),
 ( 3.141592653589793116, 4.712388980384689674 ),
 .UNSPECIFIED. ) 
 CURVE ( )  GEOMETRIC_REPRESENTATION_ITEM ( )  RATIONAL_B_SPLINE_CURVE ( ( 1.000000000000000000, 0.8047378541243649375, 0.8047378541243649375, 1.000000000000000000 ) ) 
 REPRESENTATION_ITEM ( '' )  );
#216199 = EDGE_CURVE ( 'NONE', #110926, #23890, #9446, .T. ) ;
#216200 = AXIS2_PLACEMENT_3D ( 'NONE', #158090, #18533, #74695 ) ;
#216201 = LINE ( 'NONE', #81801, #192596 ) ;
#216202 = DIRECTION ( 'NONE',  ( 0.000000000000000000, 0.000000000000000000, 1.000000000000000000 ) ) ;
#216204 = VERTEX_POINT ( 'NONE', #154714 ) ;
#216203 = DIRECTION ( 'NONE',  ( 0.000000000000000000, 0.9770955615653313941, 0.2128009952263603677 ) ) ;
#216205 = DIRECTION ( 'NONE',  ( 0.000000000000000000, -0.8700118002898322711, 0.4930308989875231140 ) ) ;
#216206 = VERTEX_POINT ( 'NONE', #153451 ) ;
#216208 = EDGE_CURVE ( 'NONE', #155114, #150648, #201163, .T. ) ;
#216207 = CARTESIAN_POINT ( 'NONE',  ( -20.94999999999999929, 75.74389420792016381, -170.0580039261966476 ) ) ;
#216210 = CARTESIAN_POINT ( 'NONE',  ( 20.85000000000000142, 64.25000000001142553, -36.02310748452440237 ) ) ;
#216209 = AXIS2_PLACEMENT_3D ( 'NONE', #150240, #96316, #195468 ) ;
#216211 = CIRCLE ( 'NONE', #224592, 0.09999999999999063804 ) ;
#216212 = CARTESIAN_POINT ( 'NONE',  ( -22.47071067811865319, 7.720074744509219933, -133.9009075452974002 ) ) ;
#216214 = AXIS2_PLACEMENT_3D ( 'NONE', #12571, #152082, #133769 ) ;
#216213 = DIRECTION ( 'NONE',  ( 0.000000000000000000, 0.2128009952264288962, -0.9770955615653166282 ) ) ;
#216215 = DIRECTION ( 'NONE',  ( -1.000000000000000000, 0.000000000000000000, -0.000000000000000000 ) ) ;
#216216 = ADVANCED_FACE ( 'NONE', ( #235493 ), #138931, .F. ) ;
#216217 = ORIENTED_EDGE ( 'NONE', *, *, #159249, .F. ) ;
#216218 = CARTESIAN_POINT ( 'NONE',  ( -18.43459694179561836, 85.49421012500940265, -29.40610228186318409 ) ) ;
#216219 = ORIENTED_EDGE ( 'NONE', *, *, #217790, .T. ) ;
#216222 = VERTEX_POINT ( 'NONE', #73898 ) ;
#216221 = DIRECTION ( 'NONE',  ( 0.000000000000000000, -0.8814952561688476074, 0.4721928772777262417 ) ) ;
#216220 = CARTESIAN_POINT ( 'NONE',  ( -22.57320508075686405, 64.25000000001267608, -203.5231074845243882 ) ) ;
#216223 = CARTESIAN_POINT ( 'NONE',  ( -21.59142135623730852, 7.850000000000003197, -21.15000000000000213 ) ) ;
#216224 = DIRECTION ( 'NONE',  ( 0.000000000000000000, -0.9910827722268055195, -0.1332476588733540468 ) ) ;
#216225 = EDGE_LOOP ( 'NONE', ( #205711, #74569, #250761, #31849 ) ) ;
#216226 = FACE_OUTER_BOUND ( 'NONE', #238550, .T. ) ;
#216228 = EDGE_CURVE ( 'NONE', #17643, #12394, #1237, .T. ) ;
#216227 = CARTESIAN_POINT ( 'NONE',  ( -18.59999999999999787, 64.35000000001254250, -182.2731074845244450 ) ) ;
#216229 = DIRECTION ( 'NONE',  ( -1.000000000000000000, 2.952720810173289112E-16, 2.061873921506763405E-30 ) ) ;
#216231 = ORIENTED_EDGE ( 'NONE', *, *, #100993, .T. ) ;
#216230 = LINE ( 'NONE', #36354, #172483 ) ;
#216232 = EDGE_CURVE ( 'NONE', #68295, #3192, #193820, .T. ) ;
#216233 = EDGE_CURVE ( 'NONE', #256658, #166855, #238585, .T. ) ;
#216234 = CARTESIAN_POINT ( 'NONE',  ( 23.14999999999999858, 36.65892442174935439, -249.5511627012433848 ) ) ;
#216235 = ORIENTED_EDGE ( 'NONE', *, *, #146764, .T. ) ;
#216236 = PLANE ( 'NONE',  #99424 ) ;
#216237 = CARTESIAN_POINT ( 'NONE',  ( 18.59999999999997655, 74.44087353924872730, -232.6253149859214773 ) ) ;
#216238 = CIRCLE ( 'NONE', #157862, 11.74999999999999645 ) ;
#216239 = ORIENTED_EDGE ( 'NONE', *, *, #128672, .T. ) ;
#216240 = CARTESIAN_POINT ( 'NONE',  ( -16.87036670365549895, 66.01058118071065905, -157.5026676018264880 ) ) ;
#216241 = ORIENTED_EDGE ( 'NONE', *, *, #13208, .T. ) ;
#216242 = CARTESIAN_POINT ( 'NONE',  ( -21.05000000000000071, -11.64999999998884306, -164.4000000000000057 ) ) ;
#216243 = EDGE_CURVE ( 'NONE', #50465, #133529, #113683, .T. ) ;
#216244 = CARTESIAN_POINT ( 'NONE',  ( 23.14999999999999503, 35.97645343225767789, -235.9694016464868298 ) ) ;
#216245 = DIRECTION ( 'NONE',  ( 1.000000000000000000, 0.000000000000000000, 0.000000000000000000 ) ) ;
#216246 = AXIS2_PLACEMENT_3D ( 'NONE', #249692, #151898, #74934 ) ;
#216247 = EDGE_LOOP ( 'NONE', ( #51986, #104405, #256010, #73992 ) ) ;
#216248 = ADVANCED_FACE ( 'NONE', ( #175555 ), #248899, .T. ) ;
#216249 = CARTESIAN_POINT ( 'NONE',  ( -20.94999999999999929, 76.00000000001190870, -103.0231074845243029 ) ) ;
#216250 = EDGE_CURVE ( 'NONE', #182491, #248548, #22130, .T. ) ;
#216251 = DIRECTION ( 'NONE',  ( -1.000000000000000000, -8.034189347746081825E-16, 2.566115377699053685E-16 ) ) ;
#216252 = DIRECTION ( 'NONE',  ( 0.000000000000000000, 0.2128009952263630322, -0.9770955615653309501 ) ) ;
#216253 = ORIENTED_EDGE ( 'NONE', *, *, #24055, .T. ) ;
#216255 = TOROIDAL_SURFACE ( 'NONE', #128799, 0.2000000000000000111, 0.1000000000000000056 ) ;
#216254 = CARTESIAN_POINT ( 'NONE',  ( -2.995603634470891112E-16, -11.74999999998884448, -121.7500000000000426 ) ) ;
#216256 = CARTESIAN_POINT ( 'NONE',  ( 21.05000000000000071, -9.499999999988844479, -90.60603087734760663 ) ) ;
#216257 = DIRECTION ( 'NONE',  ( 0.7070776581708965169, 4.937903618720407826E-15, -0.7071359030027827286 ) ) ;
#216258 = AXIS2_PLACEMENT_3D ( 'NONE', #13453, #112557, #233788 ) ;
#216259 = ORIENTED_EDGE ( 'NONE', *, *, #204659, .T. ) ;
#216260 = AXIS2_PLACEMENT_3D ( 'NONE', #25352, #65735, #8345 ) ;
#216261 = DIRECTION ( 'NONE',  ( 1.000000000000000000, 0.000000000000000000, 0.000000000000000000 ) ) ;
#216262 = ORIENTED_EDGE ( 'NONE', *, *, #91200, .F. ) ;
#216264 = EDGE_LOOP ( 'NONE', ( #50013, #226748, #161340, #193259, #79342, #185887, #66278, #256454, #21884, #146372, #228688, #19694 ) ) ;
#216263 = CARTESIAN_POINT ( 'NONE',  ( 20.94999999999999929, -11.39257802169451317, -97.42605042016811012 ) ) ;
#216265 = ADVANCED_FACE ( 'NONE', ( #85376 ), #164953, .F. ) ;
#216266 = EDGE_CURVE ( 'NONE', #196163, #219149, #63608, .T. ) ;
#216267 = AXIS2_PLACEMENT_3D ( 'NONE', #249418, #27825, #229843 ) ;
#216268 = VECTOR ( 'NONE', #64152, 1000.000000000000000 ) ;
#216271 = ORIENTED_EDGE ( 'NONE', *, *, #235354, .F. ) ;
#216270 = ORIENTED_EDGE ( 'NONE', *, *, #19477, .F. ) ;
#216269 = DIRECTION ( 'NONE',  ( -0.000000000000000000, -0.000000000000000000, 1.000000000000000000 ) ) ;
#216272 = DIRECTION ( 'NONE',  ( -1.000000000000000000, -4.624352451196580357E-15, 3.439547145395922042E-14 ) ) ;
#216273 = FACE_OUTER_BOUND ( 'NONE', #25991, .T. ) ;
#216275 = EDGE_CURVE ( 'NONE', #101319, #137094, #76079, .T. ) ;
#216274 = DIRECTION ( 'NONE',  ( 1.836970198721029934E-16, 1.000000000000000000, 6.982962677686266711E-15 ) ) ;
#216276 = CARTESIAN_POINT ( 'NONE',  ( 18.49999999999999289, 68.87972903831409610, -65.86354444268503983 ) ) ;
#216277 = PLANE ( 'NONE',  #24288 ) ;
#216278 = DIRECTION ( 'NONE',  ( -1.000000000000000000, -0.000000000000000000, -0.000000000000000000 ) ) ;
#216279 = LINE ( 'NONE', #215001, #192977 ) ;
#216281 = DIRECTION ( 'NONE',  ( 0.000000000000000000, 0.9908441862701596881, -0.1350103645451904977 ) ) ;
#216280 = DIRECTION ( 'NONE',  ( 1.000000000000000000, -0.000000000000000000, -0.000000000000000000 ) ) ;
#216283 = ORIENTED_EDGE ( 'NONE', *, *, #224505, .F. ) ;
#216282 = AXIS2_PLACEMENT_3D ( 'NONE', #235700, #137870, #174517 ) ;
#216284 = ORIENTED_EDGE ( 'NONE', *, *, #196761, .F. ) ;
#216285 = VECTOR ( 'NONE', #85765, 1000.000000000000000 ) ;
#216286 = VERTEX_POINT ( 'NONE', #65846 ) ;
#216287 = DIRECTION ( 'NONE',  ( 2.715809747126117987E-16, 1.000000000000000000, 1.303588678620536555E-14 ) ) ;
#216289 = ORIENTED_EDGE ( 'NONE', *, *, #1581, .T. ) ;
#216288 = DIRECTION ( 'NONE',  ( 1.000000000000000000, -0.000000000000000000, -0.000000000000000000 ) ) ;
#216290 = DIRECTION ( 'NONE',  ( 0.000000000000000000, -0.000000000000000000, 1.000000000000000000 ) ) ;
#216291 = ORIENTED_EDGE ( 'NONE', *, *, #108189, .F. ) ;
#216292 = CIRCLE ( 'NONE', #112273, 11.80000000000000071 ) ;
#216293 = DIRECTION ( 'NONE',  ( 0.000000000000000000, -0.4930308989875170078, -0.8700118002898356018 ) ) ;
#216294 = EDGE_LOOP ( 'NONE', ( #141024, #193528, #117069, #237063 ) ) ;
#216295 = CYLINDRICAL_SURFACE ( 'NONE', #225206, 0.1000000000000050432 ) ;
#216296 = ADVANCED_FACE ( 'NONE', ( #140231 ), #198934, .F. ) ;
#216297 = ORIENTED_EDGE ( 'NONE', *, *, #233944, .F. ) ;
#216298 = CARTESIAN_POINT ( 'NONE',  ( 18.59999999999999432, -1.162701749926853712, -175.5999999999999659 ) ) ;
#216300 = ADVANCED_FACE ( 'NONE', ( #219777 ), #121980, .F. ) ;
#216299 = DIRECTION ( 'NONE',  ( 0.000000000000000000, 1.144917494144691673E-13, -1.000000000000000000 ) ) ;
#216301 = AXIS2_PLACEMENT_3D ( 'NONE', #247774, #24904, #104385 ) ;
#216303 = VERTEX_POINT ( 'NONE', #180674 ) ;
#216302 = EDGE_LOOP ( 'NONE', ( #63829, #4816, #172903, #210379, #257288, #99494 ) ) ;
#216304 = EDGE_LOOP ( 'NONE', ( #40513, #234642, #237028, #76864, #144560, #254495, #224033, #70656, #10874 ) ) ;
#216305 = DIRECTION ( 'NONE',  ( -1.000000000000000000, -0.000000000000000000, 0.000000000000000000 ) ) ;
#216306 = ORIENTED_EDGE ( 'NONE', *, *, #29838, .T. ) ;
#216307 = EDGE_LOOP ( 'NONE', ( #55576, #595, #25640 ) ) ;
#216308 = CARTESIAN_POINT ( 'NONE',  ( -23.25000000000000000, 1.115600667400684642E-11, -200.9999999999999432 ) ) ;
#216311 = ADVANCED_FACE ( 'NONE', ( #239358 ), #20327, .T. ) ;
#216310 = EDGE_LOOP ( 'NONE', ( #134195, #247068, #36626, #120261, #186034, #65917 ) ) ;
#216309 = CYLINDRICAL_SURFACE ( 'NONE', #243408, 0.09999999999999976963 ) ;
#216313 = DIRECTION ( 'NONE',  ( 1.000000000000000000, 0.000000000000000000, 0.000000000000000000 ) ) ;
#216312 = DIRECTION ( 'NONE',  ( 0.000000000000000000, 6.982962677686266711E-15, -1.000000000000000000 ) ) ;
#216314 = DIRECTION ( 'NONE',  ( 0.000000000000000000, 0.000000000000000000, -1.000000000000000000 ) ) ;
#216315 = CARTESIAN_POINT ( 'NONE',  ( -18.59999999999999787, -1.164121893230052995, -108.4148480855716485 ) ) ;
#216316 = CARTESIAN_POINT ( 'NONE',  ( 21.12642695952774119, 30.80001426052127300, -252.0675078730340601 ) ) ;
#216317 = ORIENTED_EDGE ( 'NONE', *, *, #114006, .T. ) ;
#216318 = ADVANCED_FACE ( 'NONE', ( #104939 ), #192805, .T. ) ;
#216319 = AXIS2_PLACEMENT_3D ( 'NONE', #12919, #247647, #33782 ) ;
#216320 = VERTEX_POINT ( 'NONE', #163679 ) ;
#216321 = FACE_OUTER_BOUND ( 'NONE', #222735, .T. ) ;
#216322 = CARTESIAN_POINT ( 'NONE',  ( 18.49999999999999289, 65.79142135624951493, -145.3731074845244109 ) ) ;
#216323 = DIRECTION ( 'NONE',  ( 0.000000000000000000, 1.000000000000000000, -0.000000000000000000 ) ) ;
#216324 = EDGE_CURVE ( 'NONE', #218203, #59200, #176672, .T. ) ;
#216325 = VECTOR ( 'NONE', #1606, 1000.000000000000000 ) ;
#216326 = ORIENTED_EDGE ( 'NONE', *, *, #90242, .F. ) ;
#216327 = CARTESIAN_POINT ( 'NONE',  ( 5.900000000000061640, 64.65000000001120384, -22.12310748452479103 ) ) ;
#216328 = CIRCLE ( 'NONE', #3949, 0.09999999999999939493 ) ;
#216329 = ADVANCED_FACE ( 'NONE', ( #120719 ), #63276, .T. ) ;
#216330 = CARTESIAN_POINT ( 'NONE',  ( -16.87683809663752399, 9.850000000011144508, -180.9023640181962662 ) ) ;
#216331 = CARTESIAN_POINT ( 'NONE',  ( -14.23072895065542909, 12.43387192838033428, -213.6554569813165756 ) ) ;
#216333 = EDGE_CURVE ( 'NONE', #74301, #124743, #123261, .T. ) ;
#216332 = ADVANCED_FACE ( 'NONE', ( #43724 ), #2007, .F. ) ;
#216334 = VERTEX_POINT ( 'NONE', #223621 ) ;
#216335 = VERTEX_POINT ( 'NONE', #124556 ) ;
#216336 = CARTESIAN_POINT ( 'NONE',  ( 18.54999999999999716, 67.25000000001155342, -56.87310748452438247 ) ) ;
#216337 = DIRECTION ( 'NONE',  ( -1.000000000000000000, 3.265361837132813093E-16, 2.280189983783949500E-30 ) ) ;
#216338 = ORIENTED_EDGE ( 'NONE', *, *, #37698, .F. ) ;
#216339 = CARTESIAN_POINT ( 'NONE',  ( -20.00857864376270001, 66.75000000001151079, -48.27310748452438816 ) ) ;
#216340 = EDGE_LOOP ( 'NONE', ( #41319, #38855, #29294 ) ) ;
#216341 = B_SPLINE_CURVE_WITH_KNOTS ( 'NONE', 3,
 ( #40083, #164818, #243056, #64434, #107398, #185661, #149121, #25324, #65708, #186973, #44868, #119608, #103531, #145232, #184361, #7016 ),
 .UNSPECIFIED., .F., .F.,
 ( 4, 3, 3, 3, 3, 4 ),
 ( 0.000000000000000000, 3.357088238232317244E-05, 6.714213034886757942E-05, 0.0001007408646120921551, 0.0001343627955914185768, 0.0001573956632895995484 ),
 .UNSPECIFIED. ) ;
#216342 = DIRECTION ( 'NONE',  ( 0.000000000000000000, -0.000000000000000000, 1.000000000000000000 ) ) ;
#216343 = CARTESIAN_POINT ( 'NONE',  ( -18.59999999999999787, 68.97833521811233481, -166.3895420826271163 ) ) ;
#216344 = CARTESIAN_POINT ( 'NONE',  ( -21.05000000000000071, 68.03098227380377239, -227.7073825336181869 ) ) ;
#216345 = AXIS2_PLACEMENT_3D ( 'NONE', #226690, #31109, #166765 ) ;
#216346 = FACE_OUTER_BOUND ( 'NONE', #100067, .T. ) ;
#216347 = DIRECTION ( 'NONE',  ( 0.000000000000000000, 0.000000000000000000, -1.000000000000000000 ) ) ;
#216348 = CIRCLE ( 'NONE', #195539, 11.75000000000000178 ) ;
#216349 = CARTESIAN_POINT ( 'NONE',  ( -19.99999999999999645, 4.547418889303922462, 21.90000000000000213 ) ) ;
#216350 = ADVANCED_FACE ( 'NONE', ( #204069 ), #9636, .T. ) ;
#216352 = EDGE_CURVE ( 'NONE', #103069, #73708, #21605, .T. ) ;
#216351 = VECTOR ( 'NONE', #17487, 1000.000000000000000 ) ;
#216354 = ORIENTED_EDGE ( 'NONE', *, *, #183323, .F. ) ;
#216353 = EDGE_LOOP ( 'NONE', ( #11522, #205471, #27716, #249167 ) ) ;
#216355 = ORIENTED_EDGE ( 'NONE', *, *, #22822, .T. ) ;
#216356 = ADVANCED_FACE ( 'NONE', ( #12328 ), #255093, .F. ) ;
#216357 = SPHERICAL_SURFACE ( 'NONE', #238102, 0.1000000000000000056 ) ;
#216358 = CARTESIAN_POINT ( 'NONE',  ( -16.81095280782811230, 60.93935776605868426, -221.0417277355869317 ) ) ;
#216359 = CARTESIAN_POINT ( 'NONE',  ( 18.49999999999999645, 74.13328508995498112, -158.2704322382423641 ) ) ;
#216360 = DIRECTION ( 'NONE',  ( 0.000000000000000000, 0.000000000000000000, -1.000000000000000000 ) ) ;
#216362 = CARTESIAN_POINT ( 'NONE',  ( 21.05000000000000071, 1.115600667400684642E-11, -134.0000000000000284 ) ) ;
#216361 = CARTESIAN_POINT ( 'NONE',  ( 20.11144452914042091, 9.933610851122994134, -7.890293453954491554 ) ) ;
#216363 = EDGE_CURVE ( 'NONE', #61134, #231898, #126136, .T. ) ;
#216364 = CARTESIAN_POINT ( 'NONE',  ( -20.94999999999999929, 1.115600667400684642E-11, -200.9999999999999432 ) ) ;
#216365 = ORIENTED_EDGE ( 'NONE', *, *, #49510, .F. ) ;
#216366 = DIRECTION ( 'NONE',  ( -1.000000000000000000, 0.000000000000000000, 0.000000000000000000 ) ) ;
#216367 = EDGE_CURVE ( 'NONE', #168233, #5474, #142711, .T. ) ;
#216368 = ORIENTED_EDGE ( 'NONE', *, *, #72904, .T. ) ;
#216369 = VERTEX_POINT ( 'NONE', #167551 ) ;
#216370 = CARTESIAN_POINT ( 'NONE',  ( -21.05000000000000071, 69.52192177891662084, -69.42310754921729199 ) ) ;
#216371 = CARTESIAN_POINT ( 'NONE',  ( -22.46246831459151494, 0.02191216695058596786, -88.85013543879007614 ) ) ;
#216372 = DIRECTION ( 'NONE',  ( -1.000000000000000000, 0.000000000000000000, 0.000000000000000000 ) ) ;
#216373 = CARTESIAN_POINT ( 'NONE',  ( -17.71734398241073194, 10.84235722847571459, -90.22513825300563894 ) ) ;
#216374 = AXIS2_PLACEMENT_3D ( 'NONE', #28291, #45249, #161362 ) ;
#216375 = CARTESIAN_POINT ( 'NONE',  ( 22.50927854361889047, -0.1008580735143998902, -155.7504328739730397 ) ) ;
#216376 = ORIENTED_EDGE ( 'NONE', *, *, #162458, .T. ) ;
#216377 = ORIENTED_EDGE ( 'NONE', *, *, #253740, .T. ) ;
#216378 = CARTESIAN_POINT ( 'NONE',  ( -21.05000000000000071, 11.63687328911526642, -40.32175921332488855 ) ) ;
#216379 = CYLINDRICAL_SURFACE ( 'NONE', #244647, 0.09999999999999939493 ) ;
#216381 = EDGE_CURVE ( 'NONE', #185866, #55604, #50132, .T. ) ;
#216380 = ORIENTED_EDGE ( 'NONE', *, *, #119574, .T. ) ;
#216382 = FACE_OUTER_BOUND ( 'NONE', #217220, .T. ) ;
#216383 = LINE ( 'NONE', #18193, #2733 ) ;
#216384 = CARTESIAN_POINT ( 'NONE',  ( 18.59999999999999787, -11.74999999999999289, -21.35000000000000142 ) ) ;
#216385 = B_SPLINE_CURVE_WITH_KNOTS ( 'NONE', 3,
 ( #23374, #1188, #222812, #258055, #101558, #182434, #81994, #239833, #84547, #3781 ),
 .UNSPECIFIED., .F., .F.,
 ( 4, 3, 3, 4 ),
 ( 0.000000000000000000, 1.004626015991573225E-05, 1.831183478183568230E-05, 2.062343583996359216E-05 ),
 .UNSPECIFIED. ) ;
#216386 = CARTESIAN_POINT ( 'NONE',  ( 23.25000000000000000, 84.59626168225520360, -145.9732350016745954 ) ) ;
#216387 = CARTESIAN_POINT ( 'NONE',  ( -20.64999999999999858, 4.350000000011156054, -146.3500000000000227 ) ) ;
#216389 = DIRECTION ( 'NONE',  ( -0.000000000000000000, -0.8814952561688430555, 0.4721928772777346239 ) ) ;
#216388 = CARTESIAN_POINT ( 'NONE',  ( 18.49999999999999289, 2.272311100394801109, -217.9150152700588592 ) ) ;
#216390 = CARTESIAN_POINT ( 'NONE',  ( -18.59999999999999787, 9.150000000011157653, -179.8499999999999943 ) ) ;
#216392 = EDGE_CURVE ( 'NONE', #43634, #141625, #190968, .T. ) ;
#216391 = CARTESIAN_POINT ( 'NONE',  ( 21.05000000000000071, 65.57661458509869590, -62.03105556065429482 ) ) ;
#216393 = AXIS2_PLACEMENT_3D ( 'NONE', #134981, #109010, #188560 ) ;
#216394 = VECTOR ( 'NONE', #98937, 1000.000000000000114 ) ;
#216395 = CARTESIAN_POINT ( 'NONE',  ( -22.49999999999999645, 11.74956712350054744, -133.8991416309012834 ) ) ;
#216396 = CARTESIAN_POINT ( 'NONE',  ( 21.13498764882293557, 69.50438185653881362, -203.5247638792557154 ) ) ;
#216397 = VECTOR ( 'NONE', #229945, 1000.000000000000000 ) ;
#216398 = VECTOR ( 'NONE', #64992, 1000.000000000000000 ) ;
#216400 = ORIENTED_EDGE ( 'NONE', *, *, #6134, .T. ) ;
#216399 = DIRECTION ( 'NONE',  ( 0.000000000000000000, 0.000000000000000000, 1.000000000000000000 ) ) ;
#216401 = CIRCLE ( 'NONE', #137283, 0.1000000000000124678 ) ;
#216403 = EDGE_CURVE ( 'NONE', #92189, #34456, #163585, .T. ) ;
#216402 = CARTESIAN_POINT ( 'NONE',  ( 23.24999999999999289, -4.149999999999999467, 0.000000000000000000 ) ) ;
#216404 = ORIENTED_EDGE ( 'NONE', *, *, #20406, .F. ) ;
#216405 = DIRECTION ( 'NONE',  ( 1.000000000000000000, -7.304098846218134667E-16, -5.100424963727255829E-30 ) ) ;
#216406 = DIRECTION ( 'NONE',  ( 0.000000000000000000, -6.938893903907222067E-15, 1.000000000000000000 ) ) ;
#216407 = AXIS2_PLACEMENT_3D ( 'NONE', #258047, #7627, #66321 ) ;
#216408 = ORIENTED_EDGE ( 'NONE', *, *, #122009, .F. ) ;
#216410 = CONICAL_SURFACE ( 'NONE', #158201, 7.750000000000020428, 0.7853981633974531640 ) ;
#216409 = LINE ( 'NONE', #37804, #96615 ) ;
#216411 = CARTESIAN_POINT ( 'NONE',  ( 21.05000000000000071, 85.40000000001188596, -93.12913836187179584 ) ) ;
#216412 = CARTESIAN_POINT ( 'NONE',  ( -18.59999999999999787, 76.00000000001213607, -136.5231074845243313 ) ) ;
#216413 = EDGE_CURVE ( 'NONE', #231071, #73311, #180327, .T. ) ;
#216414 = CIRCLE ( 'NONE', #29025, 0.5000000000000004441 ) ;
#216415 = CARTESIAN_POINT ( 'NONE',  ( -21.05000000000000071, 1.835341550235567887, -145.5551512925629822 ) ) ;
#216416 = CARTESIAN_POINT ( 'NONE',  ( -16.87331047859649757, 66.05000000001201954, -115.6731074845243796 ) ) ;
#216417 = DIRECTION ( 'NONE',  ( -1.000000000000000000, 1.335000415235278971E-16, -2.979993593738921214E-16 ) ) ;
#216418 = EDGE_LOOP ( 'NONE', ( #238978, #233112, #21299, #245580 ) ) ;
#216419 = CARTESIAN_POINT ( 'NONE',  ( -21.05000000000000071, 77.83534155023700407, -191.9679561919613491 ) ) ;
#216421 = ORIENTED_EDGE ( 'NONE', *, *, #114152, .F. ) ;
#216420 = CARTESIAN_POINT ( 'NONE',  ( -23.15000000000000213, 74.00000000001151079, -48.64772940728643391 ) ) ;
#216422 = CARTESIAN_POINT ( 'NONE',  ( -23.15000000000000213, 36.65892442174472876, -249.5511627012454596 ) ) ;
#216423 = CARTESIAN_POINT ( 'NONE',  ( -18.59999999999999787, 65.82247307196232100, -213.3517872345644832 ) ) ;
#216424 = DIRECTION ( 'NONE',  ( 0.000000000000000000, -1.000000000000000000, 0.000000000000000000 ) ) ;
#216425 = ORIENTED_EDGE ( 'NONE', *, *, #23138, .F. ) ;
#216426 = FACE_OUTER_BOUND ( 'NONE', #135689, .T. ) ;
#216427 = SHAPE_DEFINITION_REPRESENTATION ( #184567, #178537 ) ;
#216428 = CARTESIAN_POINT ( 'NONE',  ( 21.05000000000000071, 69.45934304831114048, -169.9231074845244223 ) ) ;
#216429 = CARTESIAN_POINT ( 'NONE',  ( 22.49999999999999645, -2.434660534977811430, -189.6066352242696382 ) ) ;
#216430 = ORIENTED_EDGE ( 'NONE', *, *, #72163, .T. ) ;
#216431 = CARTESIAN_POINT ( 'NONE',  ( 21.14999999999999858, 6.649999999999999467, -12.15000000000000036 ) ) ;
#216432 = CARTESIAN_POINT ( 'NONE',  ( 23.14999999999998437, 1.115600667400684642E-11, -67.00000000000004263 ) ) ;
#216433 = TOROIDAL_SURFACE ( 'NONE', #45572, 0.2000000000000000111, 0.1000000000000000056 ) ;
#216434 = CARTESIAN_POINT ( 'NONE',  ( -23.15000000000000213, 11.65000000001115588, -54.75000000000000000 ) ) ;
#216435 = ORIENTED_EDGE ( 'NONE', *, *, #200758, .T. ) ;
#216436 = VECTOR ( 'NONE', #155469, 1000.000000000000000 ) ;
#216437 = ORIENTED_EDGE ( 'NONE', *, *, #125053, .F. ) ;
#216438 = DIRECTION ( 'NONE',  ( 0.000000000000000000, 1.000000000000000000, 6.352154140967427193E-15 ) ) ;
#216439 = DIRECTION ( 'NONE',  ( 2.952720810173289112E-16, -1.000000000000000000, 0.000000000000000000 ) ) ;
#216440 = CARTESIAN_POINT ( 'NONE',  ( -23.25000000000000000, 4.250000000011156409, -79.15000000000004832 ) ) ;
#216441 = CARTESIAN_POINT ( 'NONE',  ( 22.48970261584622321, 64.35000000001268461, -203.5784769727418393 ) ) ;
#216442 = CARTESIAN_POINT ( 'NONE',  ( -21.44999999999999929, 7.150000000011155876, -155.1500000000000057 ) ) ;
#216443 = EDGE_CURVE ( 'NONE', #97383, #255010, #117777, .T. ) ;
#216445 = DIRECTION ( 'NONE',  ( 0.000000000000000000, 2.891205793294679805E-16, -1.000000000000000000 ) ) ;
#216444 = CARTESIAN_POINT ( 'NONE',  ( -18.59999999999999787, 1.249999999999999334, -8.000000000000000000 ) ) ;
#216446 = DIRECTION ( 'NONE',  ( 0.000000000000000000, -6.454785026890510900E-15, 1.000000000000000000 ) ) ;
#216447 = DIRECTION ( 'NONE',  ( 1.000000000000000000, -1.186688945009010077E-16, -8.286604613020808509E-31 ) ) ;
#216448 = LINE ( 'NONE', #198174, #154640 ) ;
#216449 = DIRECTION ( 'NONE',  ( 0.000000000000000000, -0.2617529984165031243, -0.9651348961777157509 ) ) ;
#216450 = AXIS2_PLACEMENT_3D ( 'NONE', #190516, #34024, #168411 ) ;
#216451 = ORIENTED_EDGE ( 'NONE', *, *, #71944, .T. ) ;
#216452 = ORIENTED_EDGE ( 'NONE', *, *, #184376, .T. ) ;
#216453 = LINE ( 'NONE', #74426, #27144 ) ;
#216454 = AXIS2_PLACEMENT_3D ( 'NONE', #148836, #212657, #210096 ) ;
#216455 = DIRECTION ( 'NONE',  ( 0.000000000000000000, 0.8814952561688433885, -0.4721928772777338468 ) ) ;
#216457 = LINE ( 'NONE', #250453, #203564 ) ;
#216456 = CARTESIAN_POINT ( 'NONE',  ( -23.15000000000000213, 76.00000000001240608, -174.0731074845243711 ) ) ;
#216458 = CIRCLE ( 'NONE', #29622, 12.77499999999999503 ) ;
#216459 = DIRECTION ( 'NONE',  ( 1.000000000000000000, 0.000000000000000000, 0.000000000000000000 ) ) ;
#216461 = EDGE_CURVE ( 'NONE', #248473, #253739, #151112, .T. ) ;
#216460 = DIRECTION ( 'NONE',  ( 0.000000000000000000, 6.769652589177772835E-15, -1.000000000000000000 ) ) ;
#216462 = CARTESIAN_POINT ( 'NONE',  ( -23.25000000000000000, 11.65000000001115588, -126.9851942293460922 ) ) ;
#216463 = ORIENTED_EDGE ( 'NONE', *, *, #257938, .F. ) ;
#216464 = CIRCLE ( 'NONE', #104003, 3.899999999999987033 ) ;
#216465 = CIRCLE ( 'NONE', #104004, 0.1999999999999987899 ) ;
#216466 = ORIENTED_EDGE ( 'NONE', *, *, #136809, .T. ) ;
#216467 = EDGE_CURVE ( 'NONE', #87934, #158368, #134510, .T. ) ;
#216468 = DIRECTION ( 'NONE',  ( 0.000000000000000000, 0.000000000000000000, 1.000000000000000000 ) ) ;
#216469 = ORIENTED_EDGE ( 'NONE', *, *, #115449, .F. ) ;
#216470 = CARTESIAN_POINT ( 'NONE',  ( 20.85000000000000142, -11.64999999998883595, -198.0999999999999659 ) ) ;
#216471 = EDGE_CURVE ( 'NONE', #190222, #242599, #111408, .T. ) ;
#216472 = TOROIDAL_SURFACE ( 'NONE', #158258, 1.900000000000002576, 0.1000000000000000056 ) ;
#216473 = AXIS2_PLACEMENT_3D ( 'NONE', #16376, #256178, #193716 ) ;
#216475 = PRESENTATION_LAYER_ASSIGNMENT (  '', '', ( #87290 ) ) ;
#216474 = CARTESIAN_POINT ( 'NONE',  ( -23.25000000000000000, 79.15532900748003442, -196.2806010913881778 ) ) ;
#216476 = CIRCLE ( 'NONE', #58243, 0.9000000000000014655 ) ;
#216477 = AXIS2_PLACEMENT_3D ( 'NONE', #186057, #242170, #165207 ) ;
#216478 = EDGE_CURVE ( 'NONE', #9149, #88287, #171994, .T. ) ;
#216479 = ADVANCED_FACE ( 'NONE', ( #248345 ), #166274, .F. ) ;
#216480 = EDGE_LOOP ( 'NONE', ( #138638, #231457 ) ) ;
#216481 = DIRECTION ( 'NONE',  ( 1.000000000000000000, -0.000000000000000000, -0.000000000000000000 ) ) ;
#216482 = AXIS2_PLACEMENT_3D ( 'NONE', #58211, #159925, #76502 ) ;
#216483 = ORIENTED_EDGE ( 'NONE', *, *, #66552, .T. ) ;
#216484 = ADVANCED_FACE ( 'NONE', ( #72292 ), #146649, .T. ) ;
#216485 = CARTESIAN_POINT ( 'NONE',  ( -18.43569575749026157, 85.51932773110478081, -163.0501311079650009 ) ) ;
#216486 = DIRECTION ( 'NONE',  ( 1.000000000000000000, 0.000000000000000000, 0.000000000000000000 ) ) ;
#216487 = CARTESIAN_POINT ( 'NONE',  ( -20.85000000000000142, 77.16412189325305349, -95.20825939895267709 ) ) ;
#216488 = CARTESIAN_POINT ( 'NONE',  ( -21.05000000000000071, 1.115600667400684642E-11, -100.5000000000000284 ) ) ;
#216489 = CARTESIAN_POINT ( 'NONE',  ( -16.90137573187934095, 9.949999999999986855, -12.78841742409689886 ) ) ;
#216491 = CARTESIAN_POINT ( 'NONE',  ( 18.50000972452444969, 65.70673848566984532, -131.0638252334829872 ) ) ;
#216490 = DIRECTION ( 'NONE',  ( -1.000000000000000000, -0.000000000000000000, -0.000000000000000000 ) ) ;
#216492 = EDGE_CURVE ( 'NONE', #248304, #172545, #155611, .T. ) ;
#216493 = DIRECTION ( 'NONE',  ( 0.000000000000000000, 1.000000000000000000, 0.000000000000000000 ) ) ;
#216494 = VERTEX_POINT ( 'NONE', #129679 ) ;
#216496 = DIRECTION ( 'NONE',  ( 0.000000000000000000, 0.000000000000000000, -1.000000000000000000 ) ) ;
#216495 = DIRECTION ( 'NONE',  ( 0.000000000000000000, 0.000000000000000000, -1.000000000000000000 ) ) ;
#216497 = ORIENTED_EDGE ( 'NONE', *, *, #154248, .F. ) ;
#216499 = ORIENTED_EDGE ( 'NONE', *, *, #257293, .F. ) ;
#216498 = DIRECTION ( 'NONE',  ( -1.000000000000000000, 0.000000000000000000, -0.000000000000000000 ) ) ;
#216500 = ORIENTED_EDGE ( 'NONE', *, *, #159496, .F. ) ;
#216501 = DIRECTION ( 'NONE',  ( 2.715809747126116508E-16, -1.000000000000000000, 0.000000000000000000 ) ) ;
#216502 = CARTESIAN_POINT ( 'NONE',  ( -22.00356870068577919, 8.752767083654352118E-12, -26.24575763824059749 ) ) ;
#216503 = CARTESIAN_POINT ( 'NONE',  ( -20.85000000000000142, 76.00000000001165290, -61.62310748452430431 ) ) ;
#216504 = CARTESIAN_POINT ( 'NONE',  ( -23.15000000000000213, 1.115600667400684642E-11, -134.0000000000000284 ) ) ;
#216505 = ORIENTED_EDGE ( 'NONE', *, *, #201061, .T. ) ;
#216506 = CARTESIAN_POINT ( 'NONE',  ( -20.65000000000000568, 70.35000000001261355, -190.8731074845244109 ) ) ;
#216507 = ADVANCED_FACE ( 'NONE', ( #47555 ), #29339, .T. ) ;
#216508 = SURFACE_STYLE_USAGE ( .BOTH. , #155292 ) ;
#216509 = PLANE ( 'NONE',  #127349 ) ;
#216510 = EDGE_LOOP ( 'NONE', ( #242590, #121452, #115147, #172721 ) ) ;
#216511 = AXIS2_PLACEMENT_3D ( 'NONE', #101349, #163956, #221329 ) ;
#216513 = ADVANCED_FACE ( 'NONE', ( #249643 ), #210507, .T. ) ;
#216512 = DIRECTION ( 'NONE',  ( 0.000000000000000000, -0.000000000000000000, 1.000000000000000000 ) ) ;
#216514 = AXIS2_PLACEMENT_3D ( 'NONE', #101739, #181335, #1368 ) ;
#216515 = CYLINDRICAL_SURFACE ( 'NONE', #118466, 0.09999999999999939493 ) ;
#216516 = ORIENTED_EDGE ( 'NONE', *, *, #33500, .F. ) ;
#216517 = ORIENTED_EDGE ( 'NONE', *, *, #228999, .F. ) ;
#216518 = CARTESIAN_POINT ( 'NONE',  ( -22.50000000000000000, 75.90000000001219860, -144.3138870828977076 ) ) ;
#216519 = AXIS2_PLACEMENT_3D ( 'NONE', #136855, #15664, #57300 ) ;
#216520 = VERTEX_POINT ( 'NONE', #97900 ) ;
#216521 = CARTESIAN_POINT ( 'NONE',  ( -21.05000000000000071, 1.835341550235567887, -179.0551512925629538 ) ) ;
#216522 = ORIENTED_EDGE ( 'NONE', *, *, #25606, .F. ) ;
#216523 = CARTESIAN_POINT ( 'NONE',  ( 20.94788355080264353, 10.30207779525982659, -172.9895520716782755 ) ) ;
#216524 = EDGE_CURVE ( 'NONE', #153515, #14757, #34789, .T. ) ;
#216525 = CARTESIAN_POINT ( 'NONE',  ( 23.14999999999999858, 9.863005973831429074, -220.4411654715779321 ) ) ;
#216526 = DIRECTION ( 'NONE',  ( 1.000000000000000000, 0.000000000000000000, 0.000000000000000000 ) ) ;
#216527 = CARTESIAN_POINT ( 'NONE',  ( -22.47071067811865319, 1.148907358139439339E-11, -201.0000000000015064 ) ) ;
#216528 = TOROIDAL_SURFACE ( 'NONE', #199811, 0.9750000000000019762, 0.1000000000000000056 ) ;
#216529 = AXIS2_PLACEMENT_3D ( 'NONE', #175917, #78061, #221405 ) ;
#216530 = FACE_OUTER_BOUND ( 'NONE', #11225, .T. ) ;
#216531 = CARTESIAN_POINT ( 'NONE',  ( -18.50000000000000000, 64.25000000001277556, -215.2731074845244450 ) ) ;
#216532 = FACE_OUTER_BOUND ( 'NONE', #137233, .T. ) ;
#216533 = ORIENTED_EDGE ( 'NONE', *, *, #188983, .T. ) ;
#216536 = DIRECTION ( 'NONE',  ( 0.000000000000000000, 0.2617529984165152257, 0.9651348961777124202 ) ) ;
#216535 = CARTESIAN_POINT ( 'NONE',  ( 21.04116576186301302, 23.01330991368982382, -230.1885797082096303 ) ) ;
#216534 = VECTOR ( 'NONE', #241678, 1000.000000000000000 ) ;
#216537 = ORIENTED_EDGE ( 'NONE', *, *, #239703, .F. ) ;
#216541 = EDGE_LOOP ( 'NONE', ( #169211, #166344, #204467 ) ) ;
#216540 =( BOUNDED_SURFACE ( )  B_SPLINE_SURFACE ( 3, 2, ( 
 ( #235323, #56655, #17551 ),
 ( #12455, #132385, #77510 ),
 ( #236601, #33323, #192359 ),
 ( #210633, #54117, #172844 ) ),
 .UNSPECIFIED., .F., .F., .T. ) 
 B_SPLINE_SURFACE_WITH_KNOTS ( ( 4, 4 ),
 ( 3, 3 ),
 ( -1.330858166725956693E-17, 0.0003124336600439406547 ),
 ( 0.000000000000000000, 1.000000000000000000 ),
 .UNSPECIFIED. ) 
 GEOMETRIC_REPRESENTATION_ITEM ( )  RATIONAL_B_SPLINE_SURFACE ( (
 ( 1.000000000000000000, 0.7071067811865475727, 1.000000000000000000),
 ( 1.000000000000000000, 0.7089187706049858706, 1.000000000000000000),
 ( 1.000000000000000000, 0.7039288185051936209, 1.000000000000000000),
 ( 1.000000000000000000, 0.7040654476016059427, 1.000000000000000000) ) ) 
 REPRESENTATION_ITEM ( '' )  SURFACE ( )  );
#216539 = CYLINDRICAL_SURFACE ( 'NONE', #237697, 0.8750000000000007772 ) ;
#216538 = DIRECTION ( 'NONE',  ( 0.000000000000000000, 0.000000000000000000, 1.000000000000000000 ) ) ;
#216542 = EDGE_CURVE ( 'NONE', #94181, #103069, #195784, .T. ) ;
#216543 = VERTEX_POINT ( 'NONE', #135767 ) ;
#216544 = DIRECTION ( 'NONE',  ( -1.000000000000000000, 0.000000000000000000, 0.000000000000000000 ) ) ;
#216545 = CARTESIAN_POINT ( 'NONE',  ( 14.22821877134046886, 66.54397173950437150, -155.0119094494586989 ) ) ;
#216546 = LINE ( 'NONE', #233561, #144362 ) ;
#216547 = CARTESIAN_POINT ( 'NONE',  ( -18.40000000000000213, 64.51332499825454647, -145.7731074845244450 ) ) ;
#216548 = ORIENTED_EDGE ( 'NONE', *, *, #204716, .T. ) ;
#216549 = CARTESIAN_POINT ( 'NONE',  ( 20.95346350065193519, 67.11282275083814852, -195.0113755374890445 ) ) ;
#216551 = EDGE_CURVE ( 'NONE', #248274, #17720, #80922, .T. ) ;
#216550 = LINE ( 'NONE', #195737, #198630 ) ;
#216553 = CARTESIAN_POINT ( 'NONE',  ( -18.40000000000000213, 11.47316190336248809, -24.17405393319204876 ) ) ;
#216552 = CARTESIAN_POINT ( 'NONE',  ( 21.98333005346336577, -1.569210568885920809, -193.7948237253318382 ) ) ;
#216555 = ORIENTED_EDGE ( 'NONE', *, *, #256277, .T. ) ;
#216554 = CARTESIAN_POINT ( 'NONE',  ( 21.05000000000000071, 55.98745301258800566, -232.8057040749261262 ) ) ;
#216556 = EDGE_CURVE ( 'NONE', #135741, #43638, #181348, .T. ) ;
#216557 = ADVANCED_FACE ( 'NONE', ( #255679 ), #118798, .F. ) ;
#216558 = CIRCLE ( 'NONE', #145621, 0.09999999999999939493 ) ;
#216559 = AXIS2_PLACEMENT_3D ( 'NONE', #77325, #137302, #60334 ) ;
#216560 = ORIENTED_EDGE ( 'NONE', *, *, #115109, .F. ) ;
#216561 = EDGE_CURVE ( 'NONE', #30313, #238821, #26400, .T. ) ;
#216562 = CARTESIAN_POINT ( 'NONE',  ( -20.85000000000000142, 43.30036367478129478, -245.0872390055602352 ) ) ;
#216563 = CARTESIAN_POINT ( 'NONE',  ( 22.50000000000000000, 75.90000000001245439, -181.7731074845243597 ) ) ;
#216564 = ORIENTED_EDGE ( 'NONE', *, *, #54153, .F. ) ;
#216565 = CARTESIAN_POINT ( 'NONE',  ( 21.05000000000000071, -11.48912529306489994, -130.9000000000000341 ) ) ;
#216566 = ORIENTED_EDGE ( 'NONE', *, *, #215289, .T. ) ;
#216567 = EDGE_CURVE ( 'NONE', #53558, #51895, #235917, .T. ) ;
#216568 = CARTESIAN_POINT ( 'NONE',  ( -21.05000000000000071, 11.75000000000000000, -26.48519422934605316 ) ) ;
#216569 = FACE_OUTER_BOUND ( 'NONE', #125495, .T. ) ;
#216570 = CARTESIAN_POINT ( 'NONE',  ( -22.19999999999999929, -11.65000000000000036, 17.70000000000000639 ) ) ;
#216571 = ORIENTED_EDGE ( 'NONE', *, *, #160867, .F. ) ;
#216572 = DIRECTION ( 'NONE',  ( 0.000000000000000000, 0.000000000000000000, -1.000000000000000000 ) ) ;
#216573 = VECTOR ( 'NONE', #110005, 1000.000000000000114 ) ;
#216574 = AXIS2_PLACEMENT_3D ( 'NONE', #227566, #8529, #143215 ) ;
#216575 = AXIS2_PLACEMENT_3D ( 'NONE', #77768, #199023, #58203 ) ;
#216576 = AXIS2_PLACEMENT_3D ( 'NONE', #56954, #216048, #37446 ) ;
#216577 = DIRECTION ( 'NONE',  ( 0.000000000000000000, 0.9126074666063783702, 0.4088369013363252757 ) ) ;
#216578 = ADVANCED_FACE ( 'NONE', ( #156665 ), #22270, .F. ) ;
#216579 = ORIENTED_EDGE ( 'NONE', *, *, #104260, .T. ) ;
#216580 = TOROIDAL_SURFACE ( 'NONE', #8317, 2.100000000000002309, 0.1000000000000000056 ) ;
#216581 = ORIENTED_EDGE ( 'NONE', *, *, #256129, .T. ) ;
#216582 = FACE_OUTER_BOUND ( 'NONE', #206722, .T. ) ;
#216583 = ORIENTED_EDGE ( 'NONE', *, *, #233382, .T. ) ;
#216584 = EDGE_LOOP ( 'NONE', ( #187047, #229312, #11999, #115029 ) ) ;
#216586 = ORIENTED_EDGE ( 'NONE', *, *, #221318, .T. ) ;
#216585 = CARTESIAN_POINT ( 'NONE',  ( -18.59999999999999787, 9.250000000011157297, -112.7500000000000284 ) ) ;
#216587 = ADVANCED_FACE ( 'NONE', ( #36713 ), #57506, .T. ) ;
#216588 = EDGE_CURVE ( 'NONE', #5569, #19748, #255275, .T. ) ;
#216589 =( BOUNDED_CURVE ( )  B_SPLINE_CURVE ( 3, ( #156554, #78249, #159109, #157846 ),
 .UNSPECIFIED., .F., .F. ) 
 B_SPLINE_CURVE_WITH_KNOTS ( ( 4, 4 ),
 ( 4.712388980384689674, 6.283185307179586232 ),
 .UNSPECIFIED. ) 
 CURVE ( )  GEOMETRIC_REPRESENTATION_ITEM ( )  RATIONAL_B_SPLINE_CURVE ( ( 1.000000000000000000, 0.8047378541243649375, 0.8047378541243649375, 1.000000000000000000 ) ) 
 REPRESENTATION_ITEM ( '' )  );
#216590 = EDGE_LOOP ( 'NONE', ( #237776, #70625, #11500 ) ) ;
#216591 = TOROIDAL_SURFACE ( 'NONE', #25090, 7.800000000000000711, 0.1000000000000000056 ) ;
#216594 = ORIENTED_EDGE ( 'NONE', *, *, #1956, .F. ) ;
#216593 = ORIENTED_EDGE ( 'NONE', *, *, #142843, .T. ) ;
#216592 = DIRECTION ( 'NONE',  ( -0.000000000000000000, 6.982962677686266711E-15, -1.000000000000000000 ) ) ;
#216595 = AXIS2_PLACEMENT_3D ( 'NONE', #75250, #192607, #212183 ) ;
#216596 = EDGE_CURVE ( 'NONE', #68804, #155635, #209542, .T. ) ;
#216597 = ORIENTED_EDGE ( 'NONE', *, *, #7343, .F. ) ;
#216598 = DIRECTION ( 'NONE',  ( 1.000000000000000000, -3.265361837132813093E-16, -2.280189983783949500E-30 ) ) ;
#216599 = CARTESIAN_POINT ( 'NONE',  ( 23.14999999999999503, 64.35000000001221565, -148.2731074845243882 ) ) ;
#216600 = CARTESIAN_POINT ( 'NONE',  ( -16.77431908686106254, 14.15188998083434235, -219.2421286581669335 ) ) ;
#216601 = ORIENTED_EDGE ( 'NONE', *, *, #112348, .T. ) ;
#216602 = CARTESIAN_POINT ( 'NONE',  ( -18.50000000000000000, 1.115600667400684642E-11, -167.4999999999999716 ) ) ;
#216604 = EDGE_LOOP ( 'NONE', ( #37687, #207061, #128767, #242486 ) ) ;
#216603 = CARTESIAN_POINT ( 'NONE',  ( -23.15000000000000213, 86.27712145182582049, -209.5223386573213702 ) ) ;
#216605 = CARTESIAN_POINT ( 'NONE',  ( 21.15000000000005187, 76.00000000001119815, -36.02310748452479316 ) ) ;
#216607 = ORIENTED_EDGE ( 'NONE', *, *, #9143, .T. ) ;
#216606 = CARTESIAN_POINT ( 'NONE',  ( 23.14999999999999503, 64.35000000001186038, -90.87310748452438247 ) ) ;
#216608 = ORIENTED_EDGE ( 'NONE', *, *, #146273, .T. ) ;
#216609 = CARTESIAN_POINT ( 'NONE',  ( -20.94999999999999929, 14.90151243843701856, -203.3975529985363551 ) ) ;
#216611 = EDGE_CURVE ( 'NONE', #164130, #59550, #234683, .T. ) ;
#216610 = DIRECTION ( 'NONE',  ( 1.000000000000000000, 0.000000000000000000, 0.000000000000000000 ) ) ;
#216612 = EDGE_LOOP ( 'NONE', ( #179475, #32323, #135132 ) ) ;
#216613 = ORIENTED_EDGE ( 'NONE', *, *, #199779, .F. ) ;
#216615 = VECTOR ( 'NONE', #247277, 1000.000000000000000 ) ;
#216614 = CARTESIAN_POINT ( 'NONE',  ( -16.93255653858138388, 9.998451453988312920, -180.0816433679896420 ) ) ;
#216616 = LINE ( 'NONE', #36734, #144501 ) ;
#216618 = ORIENTED_EDGE ( 'NONE', *, *, #121257, .F. ) ;
#216617 = VERTEX_POINT ( 'NONE', #39278 ) ;
#216619 = ORIENTED_EDGE ( 'NONE', *, *, #150069, .T. ) ;
#216620 = FACE_OUTER_BOUND ( 'NONE', #68447, .T. ) ;
#216621 = ORIENTED_EDGE ( 'NONE', *, *, #183604, .T. ) ;
#216622 = EDGE_LOOP ( 'NONE', ( #218864, #189561, #102804, #245049 ) ) ;
#216623 = FACE_OUTER_BOUND ( 'NONE', #132619, .T. ) ;
#216624 = AXIS2_PLACEMENT_3D ( 'NONE', #212548, #215096, #134255 ) ;
#216625 = VERTEX_POINT ( 'NONE', #198315 ) ;
#216626 = CARTESIAN_POINT ( 'NONE',  ( -21.05000000000000071, -11.64999999998884483, -170.3999999999999773 ) ) ;
#216628 = CARTESIAN_POINT ( 'NONE',  ( 22.39999999999999503, 76.00000000001170974, -77.31388708289769340 ) ) ;
#216627 = DIRECTION ( 'NONE',  ( 1.000000000000000000, 2.952720810173289112E-16, -0.000000000000000000 ) ) ;
#216629 = ORIENTED_EDGE ( 'NONE', *, *, #41182, .F. ) ;
#216630 = EDGE_CURVE ( 'NONE', #96528, #237868, #9808, .T. ) ;
#216631 = ORIENTED_EDGE ( 'NONE', *, *, #154094, .F. ) ;
#216632 = CARTESIAN_POINT ( 'NONE',  ( -21.65000000000000213, 7.750000000011155521, -179.8499999999999943 ) ) ;
#216633 = EDGE_CURVE ( 'NONE', #125708, #57514, #251216, .T. ) ;
#216635 = VERTEX_POINT ( 'NONE', #238733 ) ;
#216634 = CIRCLE ( 'NONE', #191740, 0.1000000000000028644 ) ;
#216636 = AXIS2_PLACEMENT_3D ( 'NONE', #2565, #7729, #182526 ) ;
#216637 = ADVANCED_FACE ( 'NONE', ( #60082 ), #180511, .T. ) ;
#216638 = DIRECTION ( 'NONE',  ( 1.000000000000000000, 0.000000000000000000, 0.000000000000000000 ) ) ;
#216639 = EDGE_CURVE ( 'NONE', #239382, #30570, #1384, .T. ) ;
#216640 = ORIENTED_EDGE ( 'NONE', *, *, #39785, .F. ) ;
#216641 = ORIENTED_EDGE ( 'NONE', *, *, #191687, .T. ) ;
#216642 = VECTOR ( 'NONE', #201329, 1000.000000000000000 ) ;
#216643 = DIRECTION ( 'NONE',  ( -0.000000000000000000, 0.9651348961777157509, -0.2617529984165031243 ) ) ;
#216644 = ORIENTED_EDGE ( 'NONE', *, *, #220465, .F. ) ;
#216645 = CARTESIAN_POINT ( 'NONE',  ( 23.14999999999998437, -4.049999999988842525, -167.4999999999999716 ) ) ;
#216646 = CARTESIAN_POINT ( 'NONE',  ( 23.15000000000000213, 87.48912529308822172, -139.6231074845242688 ) ) ;
#216647 = ORIENTED_EDGE ( 'NONE', *, *, #153109, .T. ) ;
#216648 = AXIS2_PLACEMENT_3D ( 'NONE', #116659, #157091, #41007 ) ;
#216649 = DIRECTION ( 'NONE',  ( 1.000000000000000000, 3.265361837132813093E-16, -0.000000000000000000 ) ) ;
#216651 = AXIS2_PLACEMENT_3D ( 'NONE', #123820, #202070, #162959 ) ;
#216650 = DIRECTION ( 'NONE',  ( 0.000000000000000000, 0.000000000000000000, -1.000000000000000000 ) ) ;
#216653 = FACE_OUTER_BOUND ( 'NONE', #134335, .T. ) ;
#216652 = CARTESIAN_POINT ( 'NONE',  ( -20.94999999999999929, 64.75617845954087670, -200.4736850529726269 ) ) ;
#216654 = CYLINDRICAL_SURFACE ( 'NONE', #139869, 0.09999999999999939493 ) ;
#216655 = LINE ( 'NONE', #34203, #257945 ) ;
#216656 = CARTESIAN_POINT ( 'NONE',  ( 23.15000000000000213, 85.60000000001197407, -112.9170766071766820 ) ) ;
#216657 = CARTESIAN_POINT ( 'NONE',  ( 23.24999999999999645, 0.000000000000000000, -33.50000000000000000 ) ) ;
#216658 = B_SPLINE_CURVE_WITH_KNOTS ( 'NONE', 3,
 ( #105101, #221218, #201668, #3461, #184668, #47718, #43887 ),
 .UNSPECIFIED., .F., .F.,
 ( 4, 3, 4 ),
 ( 0.000000000000000000, 0.0007844235214594253575, 0.001767853679404338563 ),
 .UNSPECIFIED. ) ;
#216659 = CARTESIAN_POINT ( 'NONE',  ( 22.49066049874202022, 75.94365674847999514, -148.1731197220414060 ) ) ;
#216660 = CARTESIAN_POINT ( 'NONE',  ( 21.05000000000000071, 3.017719325445665568, -208.5164861827997242 ) ) ;
#216661 = ORIENTED_EDGE ( 'NONE', *, *, #171045, .F. ) ;
#216662 = AXIS2_PLACEMENT_3D ( 'NONE', #220281, #34275, #23376 ) ;
#216663 = EDGE_CURVE ( 'NONE', #256334, #258105, #183894, .T. ) ;
#216665 = ADVANCED_FACE ( 'NONE', ( #7835 ), #146039, .T. ) ;
#216664 = CIRCLE ( 'NONE', #141823, 11.74999999999999822 ) ;
#216666 = CIRCLE ( 'NONE', #87471, 0.09999999999998898659 ) ;
#216667 = AXIS2_PLACEMENT_3D ( 'NONE', #79729, #98006, #58880 ) ;
#216669 = ORIENTED_EDGE ( 'NONE', *, *, #178627, .T. ) ;
#216668 = ORIENTED_EDGE ( 'NONE', *, *, #204103, .T. ) ;
#216670 = ORIENTED_EDGE ( 'NONE', *, *, #40950, .T. ) ;
#216671 = ORIENTED_EDGE ( 'NONE', *, *, #45494, .F. ) ;
#216672 = CARTESIAN_POINT ( 'NONE',  ( -21.07971444708686093, 0.08782343632898161057, -94.17020791837347815 ) ) ;
#216674 = DIRECTION ( 'NONE',  ( 0.000000000000000000, 0.000000000000000000, 1.000000000000000000 ) ) ;
#216673 = CARTESIAN_POINT ( 'NONE',  ( -23.24999999999999645, 85.60000000001186038, -96.42291809330220076 ) ) ;
#216675 = ORIENTED_EDGE ( 'NONE', *, *, #136555, .T. ) ;
#216676 = CARTESIAN_POINT ( 'NONE',  ( -20.85000000000000142, 76.00000000001142553, -36.02310748452432421 ) ) ;
#216677 = EDGE_CURVE ( 'NONE', #190519, #75640, #109585, .T. ) ;
#216678 = AXIS2_PLACEMENT_3D ( 'NONE', #230752, #170818, #55919 ) ;
#216679 = LINE ( 'NONE', #156741, #116585 ) ;
#216680 = LINE ( 'NONE', #253227, #230659 ) ;
#216681 = EDGE_CURVE ( 'NONE', #120136, #43801, #126338, .T. ) ;
#216682 = DIRECTION ( 'NONE',  ( 0.000000000000000000, 0.000000000000000000, 1.000000000000000000 ) ) ;
#216683 = ORIENTED_EDGE ( 'NONE', *, *, #228591, .T. ) ;
#216684 = DIRECTION ( 'NONE',  ( 1.000000000000000000, 3.265361837132813093E-16, -0.000000000000000000 ) ) ;
#216685 = VERTEX_POINT ( 'NONE', #122657 ) ;
#216686 = DIRECTION ( 'NONE',  ( 0.000000000000000000, 0.9893560106964510714, -0.1455152366551481502 ) ) ;
#216687 = LINE ( 'NONE', #39371, #11058 ) ;
#216688 = ADVANCED_FACE ( 'NONE', ( #147330 ), #84299, .F. ) ;
#216689 = CARTESIAN_POINT ( 'NONE',  ( 18.49999999999998934, 8.531609279343539853, -209.3937462695851366 ) ) ;
#216690 = DIRECTION ( 'NONE',  ( -0.000000000000000000, 0.000000000000000000, 1.000000000000000000 ) ) ;
#216691 = DIRECTION ( 'NONE',  ( 1.000000000000000000, 0.000000000000000000, 0.000000000000000000 ) ) ;
#216692 = EDGE_LOOP ( 'NONE', ( #154218, #196052, #8762, #174060 ) ) ;
#216693 = DIRECTION ( 'NONE',  ( 0.000000000000000000, -0.9188841341108708871, -0.3945274997757635127 ) ) ;
#216694 = DIRECTION ( 'NONE',  ( 0.000000000000000000, -0.4721928772777346239, -0.8814952561688430555 ) ) ;
#216695 = VECTOR ( 'NONE', #82465, 1000.000000000000000 ) ;
#216696 = CARTESIAN_POINT ( 'NONE',  ( -20.64999999999999858, 84.66355140188105111, -93.49900636645693908 ) ) ;
#216698 = DIRECTION ( 'NONE',  ( 1.000000000000000000, 0.000000000000000000, 0.000000000000000000 ) ) ;
#216697 = CARTESIAN_POINT ( 'NONE',  ( -16.87372386987899020, 66.11939976637529526, -123.3738376126579936 ) ) ;
#216699 = CARTESIAN_POINT ( 'NONE',  ( -20.64999999999999858, 74.00000000001254818, -183.2477294072864709 ) ) ;
#216700 = VECTOR ( 'NONE', #184842, 1000.000000000000000 ) ;
#216702 = EDGE_CURVE ( 'NONE', #83655, #23197, #213833, .T. ) ;
#216701 = CARTESIAN_POINT ( 'NONE',  ( -22.39999999999999858, 76.10000000001222986, -148.1726782920690937 ) ) ;
#216703 = CARTESIAN_POINT ( 'NONE',  ( -20.54999999999999716, 0.000000000000000000, -33.50000000000000000 ) ) ;
#216704 = CYLINDRICAL_SURFACE ( 'NONE', #194123, 0.09999999999999939493 ) ;
#216706 = ORIENTED_EDGE ( 'NONE', *, *, #32998, .T. ) ;
#216705 = AXIS2_PLACEMENT_3D ( 'NONE', #62468, #68898, #251358 ) ;
#216707 = ORIENTED_EDGE ( 'NONE', *, *, #165402, .T. ) ;
#216708 = DIRECTION ( 'NONE',  ( 0.000000000000000000, 0.000000000000000000, -1.000000000000000000 ) ) ;
#216709 = VERTEX_POINT ( 'NONE', #221708 ) ;
#216710 = EDGE_CURVE ( 'NONE', #12008, #416, #148984, .T. ) ;
#216711 = DIRECTION ( 'NONE',  ( 0.000000000000000000, 0.5859227990963362664, 0.8103668758649469339 ) ) ;
#216712 = AXIS2_PLACEMENT_3D ( 'NONE', #12052, #107266, #249369 ) ;
#216713 = CARTESIAN_POINT ( 'NONE',  ( -18.51555513499475580, -9.352657054492611977, -174.6951698956958978 ) ) ;
#216714 = CARTESIAN_POINT ( 'NONE',  ( -18.50000000000000000, -9.499999999988849808, -175.5999999999999659 ) ) ;
#216715 = AXIS2_PLACEMENT_3D ( 'NONE', #36487, #212546, #191714 ) ;
#216716 = EDGE_LOOP ( 'NONE', ( #56913, #257386, #203417, #174602 ) ) ;
#216717 = AXIS2_PLACEMENT_3D ( 'NONE', #35848, #114069, #120225 ) ;
#216718 = CARTESIAN_POINT ( 'NONE',  ( 18.39999999999999858, -7.817436562502981801, -209.8389866834999395 ) ) ;
#216719 = CARTESIAN_POINT ( 'NONE',  ( -14.77538296656414829, 9.436662931810239741, -51.82303673229489505 ) ) ;
#216721 = CARTESIAN_POINT ( 'NONE',  ( -18.55121869061588669, 65.67252876774529113, -97.44570419949944551 ) ) ;
#216720 = VECTOR ( 'NONE', #138981, 1000.000000000000000 ) ;
#216722 = CARTESIAN_POINT ( 'NONE',  ( 21.05000000000000071, 78.47509609352879068, -238.9045489380306435 ) ) ;
#216724 = ORIENTED_EDGE ( 'NONE', *, *, #35396, .T. ) ;
#216723 = CARTESIAN_POINT ( 'NONE',  ( -21.14999999999999858, 6.257814610487270279, -66.90220970869124528 ) ) ;
#216726 = CARTESIAN_POINT ( 'NONE',  ( -23.25000000000000000, 77.25000000001185185, -95.22262673010921219 ) ) ;
#216725 = DIRECTION ( 'NONE',  ( 0.000000000000000000, 0.000000000000000000, -1.000000000000000000 ) ) ;
#216727 = DIRECTION ( 'NONE',  ( -1.000000000000000000, 0.000000000000000000, -0.000000000000000000 ) ) ;
#216728 = CARTESIAN_POINT ( 'NONE',  ( -18.59999999999999787, 9.250000000011157297, -179.7499999999999716 ) ) ;
#216729 = DIRECTION ( 'NONE',  ( -0.000000000000000000, -6.982962677686266711E-15, 1.000000000000000000 ) ) ;
#216730 = DIRECTION ( 'NONE',  ( 4.377807931758638789E-15, 0.04908394489122119841, 0.9987946567507836049 ) ) ;
#216731 = ORIENTED_EDGE ( 'NONE', *, *, #123019, .F. ) ;
#216732 = DIRECTION ( 'NONE',  ( 1.000000000000000000, 0.000000000000000000, 0.000000000000000000 ) ) ;
#216733 = FACE_OUTER_BOUND ( 'NONE', #43135, .T. ) ;
#216734 = VECTOR ( 'NONE', #140300, 1000.000000000000000 ) ;
#216735 = VECTOR ( 'NONE', #83426, 1000.000000000000114 ) ;
#216736 = VERTEX_POINT ( 'NONE', #46926 ) ;
#216737 = LINE ( 'NONE', #38125, #69589 ) ;
#216738 = EDGE_LOOP ( 'NONE', ( #30600, #53822 ) ) ;
#216739 = DIRECTION ( 'NONE',  ( 1.000000000000000000, 0.000000000000000000, 0.000000000000000000 ) ) ;
#216740 = DIRECTION ( 'NONE',  ( 0.000000000000000000, 0.000000000000000000, -1.000000000000000000 ) ) ;
#216741 = CARTESIAN_POINT ( 'NONE',  ( -23.15000000000000213, 74.00000000001223555, -149.7477294072864709 ) ) ;
#216742 = ORIENTED_EDGE ( 'NONE', *, *, #20638, .F. ) ;
#216743 = ORIENTED_EDGE ( 'NONE', *, *, #85816, .F. ) ;
#216744 = LINE ( 'NONE', #159366, #194378 ) ;
#216745 = CARTESIAN_POINT ( 'NONE',  ( 20.94999999999999574, 74.83729825007408465, -128.6231074845242972 ) ) ;
#216746 = VECTOR ( 'NONE', #181565, 1000.000000000000000 ) ;
#216747 = DIRECTION ( 'NONE',  ( 0.000000000000000000, 1.000000000000000000, 0.000000000000000000 ) ) ;
#216749 = CARTESIAN_POINT ( 'NONE',  ( -16.89318236219977010, 66.04846474213672991, -90.37823711663024540 ) ) ;
#216748 = CIRCLE ( 'NONE', #104308, 7.791421356237317575 ) ;
#216750 = ADVANCED_FACE ( 'NONE', ( #243858 ), #97068, .T. ) ;
#216753 = CARTESIAN_POINT ( 'NONE',  ( 18.59999999999999076, 65.79142135624880439, -48.27310748452439526 ) ) ;
#216752 = VECTOR ( 'NONE', #80052, 1000.000000000000000 ) ;
#216751 = CARTESIAN_POINT ( 'NONE',  ( -21.46681500597191672, 76.00000000001219291, -143.3806186439590533 ) ) ;
#216754 = DIRECTION ( 'NONE',  ( 0.000000000000000000, -0.8490545835447252943, -0.5283051335749948674 ) ) ;
#216755 = DIRECTION ( 'NONE',  ( 1.000000000000000000, 0.000000000000000000, 0.000000000000000000 ) ) ;
#216756 = FACE_OUTER_BOUND ( 'NONE', #256464, .T. ) ;
#216757 = EDGE_LOOP ( 'NONE', ( #233722, #229597, #150896 ) ) ;
#216758 = DIRECTION ( 'NONE',  ( 0.000000000000000000, -0.1335171055202878931, -0.9910465087640865089 ) ) ;
#216760 = ORIENTED_EDGE ( 'NONE', *, *, #173563, .T. ) ;
#216759 = DIRECTION ( 'NONE',  ( 0.000000000000000000, -1.000000000000000000, -6.982962677686265922E-15 ) ) ;
#216761 = AXIS2_PLACEMENT_3D ( 'NONE', #134935, #91984, #170293 ) ;
#216762 = SPHERICAL_SURFACE ( 'NONE', #168633, 0.1000000000000000056 ) ;
#216763 = CARTESIAN_POINT ( 'NONE',  ( 21.00000000000000000, 9.750000000011153745, -121.6500000000000341 ) ) ;
#216765 = CARTESIAN_POINT ( 'NONE',  ( -18.43707690579160996, -0.9152171842607026431, -242.2974985173727021 ) ) ;
#216764 = LINE ( 'NONE', #40741, #163439 ) ;
#216766 = EDGE_CURVE ( 'NONE', #219189, #71001, #205427, .T. ) ;
#216767 = ORIENTED_EDGE ( 'NONE', *, *, #116594, .T. ) ;
#216769 = CARTESIAN_POINT ( 'NONE',  ( -22.50000000000000000, -1.560176095955062348, -193.3663837337744837 ) ) ;
#216768 = FACE_OUTER_BOUND ( 'NONE', #144304, .T. ) ;
#216770 = CYLINDRICAL_SURFACE ( 'NONE', #141438, 0.09999999999998898659 ) ;
#216771 = DIRECTION ( 'NONE',  ( 0.000000000000000000, -6.982962677686266711E-15, 1.000000000000000000 ) ) ;
#216772 = DIRECTION ( 'NONE',  ( 1.000000000000000000, 0.000000000000000000, 0.000000000000000000 ) ) ;
#216773 = DIRECTION ( 'NONE',  ( 0.000000000000000000, 6.938893903907511105E-14, -1.000000000000000000 ) ) ;
#216774 = ORIENTED_EDGE ( 'NONE', *, *, #186908, .T. ) ;
#216775 = DIRECTION ( 'NONE',  ( 0.000000000000000000, 6.982962677686266711E-15, -1.000000000000000000 ) ) ;
#216778 = EDGE_CURVE ( 'NONE', #206570, #215370, #5510, .T. ) ;
#216777 = VERTEX_POINT ( 'NONE', #26115 ) ;
#216776 = CIRCLE ( 'NONE', #16888, 0.09999999999998898659 ) ;
#216779 = LINE ( 'NONE', #38167, #84337 ) ;
#216780 = ORIENTED_EDGE ( 'NONE', *, *, #216266, .T. ) ;
#216781 = CARTESIAN_POINT ( 'NONE',  ( -18.50000000000000000, -9.400000000000005684, -7.297259759663287326 ) ) ;
#216782 = VERTEX_POINT ( 'NONE', #65221 ) ;
#216783 = DIRECTION ( 'NONE',  ( 1.186688945009010077E-16, 0.4088369013363280513, -0.9126074666063769270 ) ) ;
#216784 = ADVANCED_FACE ( 'NONE', ( #224297 ), #105608, .F. ) ;
#216786 = EDGE_CURVE ( 'NONE', #162975, #140018, #66521, .T. ) ;
#216785 = CYLINDRICAL_SURFACE ( 'NONE', #180466, 0.09999999999999810429 ) ;
#216787 = ORIENTED_EDGE ( 'NONE', *, *, #84650, .F. ) ;
#216788 = VECTOR ( 'NONE', #137530, 1000.000000000000000 ) ;
#216789 = ADVANCED_FACE ( 'NONE', ( #12985 ), #51302, .T. ) ;
#216790 = FACE_OUTER_BOUND ( 'NONE', #202754, .T. ) ;
#216791 = AXIS2_PLACEMENT_3D ( 'NONE', #106393, #185956, #167704 ) ;
#216792 = CARTESIAN_POINT ( 'NONE',  ( -17.11825945287481332, 65.95000000001255103, -182.7731074845244450 ) ) ;
#216793 = DIRECTION ( 'NONE',  ( 1.000000000000000000, 0.000000000000000000, 0.000000000000000000 ) ) ;
#216794 = PLANE ( 'NONE',  #41337 ) ;
#216796 = CARTESIAN_POINT ( 'NONE',  ( 12.47034474403012716, 62.33660315667518148, -218.0844802857457978 ) ) ;
#216795 = AXIS2_PLACEMENT_3D ( 'NONE', #59321, #20249, #17652 ) ;
#216797 = EDGE_LOOP ( 'NONE', ( #188055, #142724, #23831, #123064 ) ) ;
#216798 = DIRECTION ( 'NONE',  ( -1.462545276649575732E-15, -0.1686199900910455851, 0.9856811345164804283 ) ) ;
#216799 = ORIENTED_EDGE ( 'NONE', *, *, #36860, .T. ) ;
#216801 = ORIENTED_EDGE ( 'NONE', *, *, #224204, .F. ) ;
#216800 = CARTESIAN_POINT ( 'NONE',  ( 23.14999999999999858, 2.000000000011158630, -134.0000000000000284 ) ) ;
#216802 = ORIENTED_EDGE ( 'NONE', *, *, #237472, .F. ) ;
#216803 = CARTESIAN_POINT ( 'NONE',  ( 21.05000000000000071, 70.60000000001254250, -182.4283735034374843 ) ) ;
#216804 = EDGE_CURVE ( 'NONE', #196419, #143950, #192998, .T. ) ;
#216805 = DIRECTION ( 'NONE',  ( -0.000000000000000000, -6.982962677686266711E-15, 1.000000000000000000 ) ) ;
#216806 = CARTESIAN_POINT ( 'NONE',  ( -20.65000000000000568, 52.72272256579932304, -234.4105091754867942 ) ) ;
#216807 = CARTESIAN_POINT ( 'NONE',  ( -20.94999999999999929, 5.850000000011108092, -43.63249722427796939 ) ) ;
#216808 = TOROIDAL_SURFACE ( 'NONE', #208459, 0.9750000000000019762, 0.1000000000000000056 ) ;
#216809 = EDGE_LOOP ( 'NONE', ( #18243, #196390, #2698 ) ) ;
#216810 = DIRECTION ( 'NONE',  ( -1.000000000000000000, -2.885090398161910739E-16, -6.283419270304611573E-17 ) ) ;
#216811 = DIRECTION ( 'NONE',  ( -0.7071067811865127117, -0.7071067811865821007, 2.081668171172114492E-13 ) ) ;
#216812 = VERTEX_POINT ( 'NONE', #212458 ) ;
#216814 = ORIENTED_EDGE ( 'NONE', *, *, #78524, .F. ) ;
#216813 = CARTESIAN_POINT ( 'NONE',  ( 21.97500000000000497, 9.750000000011153745, -179.8499999999999943 ) ) ;
#216816 = ADVANCED_FACE ( 'NONE', ( #134175 ), #22315, .F. ) ;
#216815 = DIRECTION ( 'NONE',  ( -1.000000000000000000, -2.952720810173289112E-16, 0.000000000000000000 ) ) ;
#216817 = CARTESIAN_POINT ( 'NONE',  ( -16.77180007708460963, 9.950000000011137047, -79.63561411895486231 ) ) ;
#216818 = CIRCLE ( 'NONE', #208475, 0.1000000000000028644 ) ;
#216819 = EDGE_LOOP ( 'NONE', ( #22010, #12319, #10656, #199413, #207259 ) ) ;
#216820 = CIRCLE ( 'NONE', #175189, 0.09999999999999095723 ) ;
#216821 = TOROIDAL_SURFACE ( 'NONE', #113339, 4.149999999999999467, 0.1000000000000000056 ) ;
#216822 = DIRECTION ( 'NONE',  ( 0.000000000000000000, 0.1298341882519953583, 0.9915357197604862671 ) ) ;
#216823 = ORIENTED_EDGE ( 'NONE', *, *, #39771, .T. ) ;
#216824 = DIRECTION ( 'NONE',  ( 1.186688945009009831E-16, -0.4721928772777346239, -0.8814952561688430555 ) ) ;
#216825 = AXIS2_PLACEMENT_3D ( 'NONE', #74705, #175095, #75949 ) ;
#216826 = DIRECTION ( 'NONE',  ( 1.000000000000000000, 0.000000000000000000, 0.000000000000000000 ) ) ;
#216827 = DIRECTION ( 'NONE',  ( 1.000000000000000000, -2.952720810173289112E-16, -2.061873921506763405E-30 ) ) ;
#216828 = AXIS2_PLACEMENT_3D ( 'NONE', #98040, #18548, #19845 ) ;
#216829 = CIRCLE ( 'NONE', #254233, 0.09999999999999439892 ) ;
#216830 = CARTESIAN_POINT ( 'NONE',  ( -21.64999999999999858, 62.96304356361481780, -213.1979597767049484 ) ) ;
#216831 = AXIS2_PLACEMENT_3D ( 'NONE', #109281, #110580, #193990 ) ;
#216832 = AXIS2_PLACEMENT_3D ( 'NONE', #233556, #17082, #99141 ) ;
#216833 = AXIS2_PLACEMENT_3D ( 'NONE', #150991, #110568, #190121 ) ;
#216834 = ORIENTED_EDGE ( 'NONE', *, *, #109751, .T. ) ;
#216835 = AXIS2_PLACEMENT_3D ( 'NONE', #63717, #48000, #143251 ) ;
#216836 = AXIS2_PLACEMENT_3D ( 'NONE', #254218, #79431, #59861 ) ;
#216837 = EDGE_CURVE ( 'NONE', #191177, #223255, #72966, .T. ) ;
#216838 = EDGE_CURVE ( 'NONE', #180293, #193873, #13919, .T. ) ;
#216839 = ORIENTED_EDGE ( 'NONE', *, *, #29765, .T. ) ;
#216840 = CARTESIAN_POINT ( 'NONE',  ( -20.64999999999999858, 7.150000000011155876, -88.15000000000004832 ) ) ;
#216841 = CARTESIAN_POINT ( 'NONE',  ( 20.94999999999999574, -1.835341550213255957, -145.5551512925629822 ) ) ;
#216843 = EDGE_LOOP ( 'NONE', ( #62376, #160663, #111364, #222968 ) ) ;
#216842 = CARTESIAN_POINT ( 'NONE',  ( 21.06280952165543141, 10.62713230061201841, -146.2040538867793771 ) ) ;
#216844 = CARTESIAN_POINT ( 'NONE',  ( -20.00857864376270001, 66.75000000001199396, -115.2731074845243597 ) ) ;
#216845 = DIRECTION ( 'NONE',  ( 0.000000000000000000, 7.086529944415886769E-15, -1.000000000000000000 ) ) ;
#216847 = EDGE_CURVE ( 'NONE', #18097, #225728, #250285, .T. ) ;
#216846 = CARTESIAN_POINT ( 'NONE',  ( -20.94999999999994600, 64.35000000001120668, -6.123107484524794586 ) ) ;
#216849 = EDGE_CURVE ( 'NONE', #119804, #66395, #130323, .T. ) ;
#216848 = FACE_OUTER_BOUND ( 'NONE', #180272, .T. ) ;
#216850 = DIRECTION ( 'NONE',  ( 1.000000000000000000, -0.000000000000000000, 0.000000000000000000 ) ) ;
#216851 = DIRECTION ( 'NONE',  ( 0.000000000000000000, -1.000000000000000000, 0.000000000000000000 ) ) ;
#216852 = CARTESIAN_POINT ( 'NONE',  ( -18.51555513499414474, 85.35265705451615759, -129.3279375888285188 ) ) ;
#216853 = CIRCLE ( 'NONE', #212777, 12.87499999999999822 ) ;
#216855 = ORIENTED_EDGE ( 'NONE', *, *, #60325, .F. ) ;
#216854 = DIRECTION ( 'NONE',  ( -1.000000000000000000, 0.000000000000000000, 0.000000000000000000 ) ) ;
#216856 = EDGE_CURVE ( 'NONE', #200601, #229766, #55562, .T. ) ;
#216857 = EDGE_CURVE ( 'NONE', #247233, #96530, #169510, .T. ) ;
#216859 = ADVANCED_FACE ( 'NONE', ( #233314 ), #191633, .T. ) ;
#216858 = EDGE_CURVE ( 'NONE', #228818, #84841, #114031, .T. ) ;
#216860 = DIRECTION ( 'NONE',  ( 0.000000000000000000, 0.8814952561688429444, -0.4721928772777345684 ) ) ;
#216861 = ORIENTED_EDGE ( 'NONE', *, *, #3763, .T. ) ;
#216862 = FACE_OUTER_BOUND ( 'NONE', #138900, .T. ) ;
#216863 = CARTESIAN_POINT ( 'NONE',  ( -23.15000000000000213, 1.910280373831780176, -12.63136785519894012 ) ) ;
#216864 = ORIENTED_EDGE ( 'NONE', *, *, #102974, .T. ) ;
#216865 = CARTESIAN_POINT ( 'NONE',  ( 18.49999999999999645, 7.476371755685454090, -241.7308184205399471 ) ) ;
#216866 = CIRCLE ( 'NONE', #50264, 0.09999999999999939493 ) ;
#216867 = EDGE_CURVE ( 'NONE', #95210, #43942, #18201, .T. ) ;
#216868 = ORIENTED_EDGE ( 'NONE', *, *, #80247, .T. ) ;
#216869 = EDGE_CURVE ( 'NONE', #41808, #198388, #193181, .T. ) ;
#216870 = EDGE_CURVE ( 'NONE', #138993, #105545, #33854, .T. ) ;
#216871 = CIRCLE ( 'NONE', #125321, 0.09999999999999939493 ) ;
#216872 = CARTESIAN_POINT ( 'NONE',  ( 20.94999999999999574, 4.348235979057646361, -245.2768893876484810 ) ) ;
#216873 = EDGE_CURVE ( 'NONE', #186223, #253241, #9113, .T. ) ;
#216875 = ORIENTED_EDGE ( 'NONE', *, *, #154561, .F. ) ;
#216874 = VECTOR ( 'NONE', #14017, 1000.000000000000000 ) ;
#216876 = DIRECTION ( 'NONE',  ( 1.000000000000000000, -0.000000000000000000, -0.000000000000000000 ) ) ;
#216877 = ORIENTED_EDGE ( 'NONE', *, *, #30889, .T. ) ;
#216878 = DIRECTION ( 'NONE',  ( 1.000000000000000000, -0.000000000000000000, -0.000000000000000000 ) ) ;
#216880 = VERTEX_POINT ( 'NONE', #113341 ) ;
#216879 = CYLINDRICAL_SURFACE ( 'NONE', #147210, 12.87500000000000178 ) ;
#216881 = EDGE_CURVE ( 'NONE', #121414, #181313, #93192, .T. ) ;
#216882 = DIRECTION ( 'NONE',  ( 0.000000000000000000, 6.982962677686266711E-15, -1.000000000000000000 ) ) ;
#216883 = ORIENTED_EDGE ( 'NONE', *, *, #256768, .F. ) ;
#216884 = VECTOR ( 'NONE', #94123, 1000.000000000000000 ) ;
#216885 = DIRECTION ( 'NONE',  ( 0.000000000000000000, -6.982962677686266711E-15, 1.000000000000000000 ) ) ;
#216886 = ORIENTED_EDGE ( 'NONE', *, *, #1790, .T. ) ;
#216888 = ORIENTED_EDGE ( 'NONE', *, *, #167658, .T. ) ;
#216887 = ORIENTED_EDGE ( 'NONE', *, *, #253791, .F. ) ;
#216889 = ORIENTED_EDGE ( 'NONE', *, *, #147786, .F. ) ;
#216890 = CARTESIAN_POINT ( 'NONE',  ( -22.50000000000000000, 7.790779598384560245, -133.9000000000000057 ) ) ;
#216891 = AXIS2_PLACEMENT_3D ( 'NONE', #247493, #126251, #10176 ) ;
#216892 = VERTEX_POINT ( 'NONE', #172069 ) ;
#216893 = CIRCLE ( 'NONE', #46024, 0.9000000000000014655 ) ;
#216894 = AXIS2_PLACEMENT_3D ( 'NONE', #232384, #156709, #131973 ) ;
#216895 = ORIENTED_EDGE ( 'NONE', *, *, #159451, .T. ) ;
#216896 = FACE_OUTER_BOUND ( 'NONE', #145618, .T. ) ;
#216897 = CARTESIAN_POINT ( 'NONE',  ( -0.8999999999999993561, -11.75000000000000000, 23.30000000000000426 ) ) ;
#216898 =( BOUNDED_CURVE ( )  B_SPLINE_CURVE ( 3, ( #79881, #35686, #159457, #238998 ),
 .UNSPECIFIED., .F., .F. ) 
 B_SPLINE_CURVE_WITH_KNOTS ( ( 4, 4 ),
 ( 0.06456096931748382672, 3.077031684272309775 ),
 .UNSPECIFIED. ) 
 CURVE ( )  GEOMETRIC_REPRESENTATION_ITEM ( )  RATIONAL_B_SPLINE_CURVE ( ( 1.000000000000000000, 0.3763440860215097605, 0.3763440860215097605, 1.000000000000000000 ) ) 
 REPRESENTATION_ITEM ( '' )  );
#216900 = EDGE_LOOP ( 'NONE', ( #143095, #63689, #211164, #180693 ) ) ;
#216899 = DIRECTION ( 'NONE',  ( -1.020425574104004196E-15, 6.982962677686266711E-15, -1.000000000000000000 ) ) ;
#216901 = DIRECTION ( 'NONE',  ( 1.000000000000000000, 0.000000000000000000, 0.000000000000000000 ) ) ;
#216902 = ORIENTED_EDGE ( 'NONE', *, *, #17527, .F. ) ;
#216903 = DIRECTION ( 'NONE',  ( -1.000000000000000000, -0.000000000000000000, -0.000000000000000000 ) ) ;
#216904 = CARTESIAN_POINT ( 'NONE',  ( -23.15000000000000213, 73.50000000001180922, -82.74772940728642823 ) ) ;
#216905 = DIRECTION ( 'NONE',  ( -1.000000000000000000, 0.000000000000000000, 0.000000000000000000 ) ) ;
#216906 = EDGE_LOOP ( 'NONE', ( #234001, #17704, #78766 ) ) ;
#216907 = DIRECTION ( 'NONE',  ( 0.000000000000000000, 0.000000000000000000, -1.000000000000000000 ) ) ;
#216908 = CARTESIAN_POINT ( 'NONE',  ( -18.50000000000000000, 38.30077178631847801, -261.1858881914067751 ) ) ;
#216909 = DIRECTION ( 'NONE',  ( 0.000000000000000000, 0.9126074666063769270, 0.4088369013363280513 ) ) ;
#216910 = AXIS2_PLACEMENT_3D ( 'NONE', #153760, #139240, #237091 ) ;
#216911 = ORIENTED_EDGE ( 'NONE', *, *, #195020, .T. ) ;
#216912 = SPHERICAL_SURFACE ( 'NONE', #251333, 0.1000000000000000056 ) ;
#216913 = ORIENTED_EDGE ( 'NONE', *, *, #198935, .T. ) ;
#216914 = ORIENTED_EDGE ( 'NONE', *, *, #216639, .F. ) ;
#216915 = DIRECTION ( 'NONE',  ( 0.000000000000000000, 0.000000000000000000, 1.000000000000000000 ) ) ;
#216916 = VERTEX_POINT ( 'NONE', #252840 ) ;
#216917 = ORIENTED_EDGE ( 'NONE', *, *, #165292, .F. ) ;
#216918 = DIRECTION ( 'NONE',  ( 1.000000000000000000, 0.000000000000000000, 0.000000000000000000 ) ) ;
#216919 = DIRECTION ( 'NONE',  ( 1.000000000000000000, 0.000000000000000000, 0.000000000000000000 ) ) ;
#216920 = VERTEX_POINT ( 'NONE', #149925 ) ;
#216921 = EDGE_LOOP ( 'NONE', ( #98956, #67801, #81843, #193705 ) ) ;
#216922 = DIRECTION ( 'NONE',  ( -1.000000000000000000, 0.000000000000000000, 0.000000000000000000 ) ) ;
#216923 = CARTESIAN_POINT ( 'NONE',  ( 20.73486653747088582, 7.250000000011182166, -180.1499999999999773 ) ) ;
#216924 = ORIENTED_EDGE ( 'NONE', *, *, #90551, .T. ) ;
#216925 = VECTOR ( 'NONE', #161041, 1000.000000000000000 ) ;
#216926 = EDGE_CURVE ( 'NONE', #165708, #61363, #234864, .T. ) ;
#216927 = ORIENTED_EDGE ( 'NONE', *, *, #72913, .F. ) ;
#216928 = AXIS2_PLACEMENT_3D ( 'NONE', #216726, #137191, #38112 ) ;
#216929 = ADVANCED_FACE ( 'NONE', ( #50772 ), #5687, .T. ) ;
#216930 = ORIENTED_EDGE ( 'NONE', *, *, #66534, .F. ) ;
#216931 = VECTOR ( 'NONE', #48699, 1000.000000000000000 ) ;
#216932 = CARTESIAN_POINT ( 'NONE',  ( -20.64999999999999858, 65.89281126173843006, -213.4744760240239145 ) ) ;
#216933 = EDGE_CURVE ( 'NONE', #178157, #176425, #59866, .T. ) ;
#216934 = CARTESIAN_POINT ( 'NONE',  ( 23.14999999999999858, 1.115600667400684642E-11, -134.0000000000000284 ) ) ;
#216935 = EDGE_CURVE ( 'NONE', #7935, #37506, #239714, .T. ) ;
#216936 = CARTESIAN_POINT ( 'NONE',  ( -21.55000000000000071, 44.83341466285084209, -237.8352457803185871 ) ) ;
#216937 = CARTESIAN_POINT ( 'NONE',  ( 21.05000000000000071, 1.115600667400684642E-11, -33.50000000000000000 ) ) ;
#216938 = LINE ( 'NONE', #157004, #32728 ) ;
#216939 = VECTOR ( 'NONE', #105438, 1000.000000000000000 ) ;
#216940 = CARTESIAN_POINT ( 'NONE',  ( -23.49999999999994316, 82.84256550613280012, -26.34830530078816935 ) ) ;
#216942 = DIRECTION ( 'NONE',  ( -1.000000000000000000, -0.000000000000000000, -0.000000000000000000 ) ) ;
#216941 = CARTESIAN_POINT ( 'NONE',  ( -16.86422026484316916, 9.970447360860653419, -12.58221322567300859 ) ) ;
#216943 = DIRECTION ( 'NONE',  ( 1.000000000000000000, -3.469446951953718318E-14, 2.003086131649645455E-14 ) ) ;
#216944 = CARTESIAN_POINT ( 'NONE',  ( -16.79270642812283043, 22.98604926797965220, -230.9435997431117187 ) ) ;
#216945 = DIRECTION ( 'NONE',  ( 1.000000000000000000, 0.000000000000000000, 0.000000000000000000 ) ) ;
#216946 = LINE ( 'NONE', #99551, #38585 ) ;
#216947 = EDGE_LOOP ( 'NONE', ( #232665, #114383, #98325, #210166 ) ) ;
#216948 = EDGE_CURVE ( 'NONE', #216206, #201516, #39070, .T. ) ;
#216949 = EDGE_CURVE ( 'NONE', #90248, #183734, #14120, .T. ) ;
#216951 = ORIENTED_EDGE ( 'NONE', *, *, #180656, .T. ) ;
#216950 = DIRECTION ( 'NONE',  ( -3.265361837132813093E-16, -0.9651348961777158619, 0.2617529984165024026 ) ) ;
#216952 = AXIS2_PLACEMENT_3D ( 'NONE', #195636, #19554, #239884 ) ;
#216953 = DIRECTION ( 'NONE',  ( 0.000000000000000000, 0.9126074666063772600, 0.4088369013363276627 ) ) ;
#216954 = CARTESIAN_POINT ( 'NONE',  ( 20.85000000000000142, 76.00000000001190870, -103.0231074845243029 ) ) ;
#216955 = VERTEX_POINT ( 'NONE', #196720 ) ;
#216956 = CIRCLE ( 'NONE', #104521, 0.1000000000000028644 ) ;
#216957 = EDGE_CURVE ( 'NONE', #167911, #199951, #178478, .T. ) ;
#216958 = CARTESIAN_POINT ( 'NONE',  ( -21.65000000000000213, 66.05000000001187743, -90.37310748452438247 ) ) ;
#216959 = CIRCLE ( 'NONE', #254378, 0.09999999999999939493 ) ;
#216960 = EDGE_CURVE ( 'NONE', #16805, #6281, #57190, .T. ) ;
#216961 = CARTESIAN_POINT ( 'NONE',  ( -16.88328101497759448, 9.950352834218858078, -20.85117951492928157 ) ) ;
#216962 = VERTEX_POINT ( 'NONE', #1064 ) ;
#216963 = CARTESIAN_POINT ( 'NONE',  ( -20.94684162548871242, 11.75000000001115197, -140.8416439955713031 ) ) ;
#216964 = FACE_OUTER_BOUND ( 'NONE', #3037, .T. ) ;
#216965 = AXIS2_PLACEMENT_3D ( 'NONE', #248156, #69538, #55063 ) ;
#216966 = FACE_OUTER_BOUND ( 'NONE', #1675, .T. ) ;
#216967 = AXIS2_PLACEMENT_3D ( 'NONE', #64062, #22393, #185300 ) ;
#216968 = DIRECTION ( 'NONE',  ( 0.000000000000000000, 6.982962677686266711E-15, -1.000000000000000000 ) ) ;
#216970 = ORIENTED_EDGE ( 'NONE', *, *, #165431, .F. ) ;
#216969 = DIRECTION ( 'NONE',  ( 2.715809747126116508E-16, -1.000000000000000000, 0.000000000000000000 ) ) ;
#216971 = ADVANCED_FACE ( 'NONE', ( #195473 ), #38953, .T. ) ;
#216973 = ORIENTED_EDGE ( 'NONE', *, *, #13120, .F. ) ;
#216972 = CARTESIAN_POINT ( 'NONE',  ( -23.15000000000000213, 46.05992536685982230, -240.5730681801377102 ) ) ;
#216974 = DIRECTION ( 'NONE',  ( 1.000000000000000000, 0.000000000000000000, 0.000000000000000000 ) ) ;
#216975 = CARTESIAN_POINT ( 'NONE',  ( 21.07189867249812210, 10.72498027009314825, -12.21245144227673940 ) ) ;
#216976 = CARTESIAN_POINT ( 'NONE',  ( -20.64999999999999858, 71.65000000001151648, -48.37310748452434694 ) ) ;
#216977 = EDGE_CURVE ( 'NONE', #105004, #50700, #255358, .T. ) ;
#216978 = CYLINDRICAL_SURFACE ( 'NONE', #111035, 0.1000000000000028644 ) ;
#216980 = CARTESIAN_POINT ( 'NONE',  ( -23.25000000000000000, 1.115600667400684642E-11, -33.50000000000000000 ) ) ;
#216979 = DIRECTION ( 'NONE',  ( -3.469446951953618606E-14, -0.8814952561688437216, 0.4721928772777334582 ) ) ;
#216981 = DIRECTION ( 'NONE',  ( 4.408576920032446123E-17, -0.3427706569149635007, 0.9394191166662961834 ) ) ;
#216982 = CARTESIAN_POINT ( 'NONE',  ( 20.94999999999999929, 67.92720994251783395, -214.1870976236629929 ) ) ;
#216985 = EDGE_CURVE ( 'NONE', #114076, #37949, #89099, .T. ) ;
#216984 = DIRECTION ( 'NONE',  ( -1.000000000000000000, -1.394253735153569469E-16, -2.602809386958778209E-16 ) ) ;
#216983 = CIRCLE ( 'NONE', #162873, 0.1000000000000033223 ) ;
#216986 = CARTESIAN_POINT ( 'NONE',  ( -18.40000000000000213, 85.68240343348880117, -163.3662641071115331 ) ) ;
#216987 = LINE ( 'NONE', #157050, #105932 ) ;
#216988 = TOROIDAL_SURFACE ( 'NONE', #62889, 0.2000000000000000111, 0.1000000000000000056 ) ;
#216989 = ORIENTED_EDGE ( 'NONE', *, *, #114602, .T. ) ;
#216991 = DIRECTION ( 'NONE',  ( 1.000000000000000000, 0.000000000000000000, -0.000000000000000000 ) ) ;
#216990 = AXIS2_PLACEMENT_3D ( 'NONE', #187988, #88854, #168473 ) ;
#216992 = ORIENTED_EDGE ( 'NONE', *, *, #145300, .F. ) ;
#216994 =( BOUNDED_CURVE ( )  B_SPLINE_CURVE ( 3, ( #211649, #190823, #73437, #10873 ),
 .UNSPECIFIED., .F., .T. ) 
 B_SPLINE_CURVE_WITH_KNOTS ( ( 4, 4 ),
 ( 3.432212674861196966, 3.693332928900581624 ),
 .UNSPECIFIED. ) 
 CURVE ( )  GEOMETRIC_REPRESENTATION_ITEM ( )  RATIONAL_B_SPLINE_CURVE ( ( 1.000000000000000000, 0.9943260843901261525, 0.9943260843901261525, 1.000000000000000000 ) ) 
 REPRESENTATION_ITEM ( '' )  );
#216993 = CIRCLE ( 'NONE', #29600, 0.1000000000000053069 ) ;
#216995 = ORIENTED_EDGE ( 'NONE', *, *, #189391, .F. ) ;
#216996 = CARTESIAN_POINT ( 'NONE',  ( 20.94999999999999929, -12.41227409413852811, -64.00000000000000000 ) ) ;
#216997 = CARTESIAN_POINT ( 'NONE',  ( -20.64999999999999858, 7.150000000011155876, -179.7499999999999716 ) ) ;
#216998 = ORIENTED_EDGE ( 'NONE', *, *, #194413, .F. ) ;
#216999 = AXIS2_PLACEMENT_3D ( 'NONE', #130002, #71355, #68773 ) ;
#217000 = ADVANCED_FACE ( 'NONE', ( #254118 ), #191014, .F. ) ;
#217001 = AXIS2_PLACEMENT_3D ( 'NONE', #115194, #194757, #70965 ) ;
#217002 = EDGE_LOOP ( 'NONE', ( #241597, #51220, #71715, #59623 ) ) ;
#217003 = EDGE_CURVE ( 'NONE', #59396, #144177, #76437, .T. ) ;
#217005 = ORIENTED_EDGE ( 'NONE', *, *, #120936, .T. ) ;
#217004 = VECTOR ( 'NONE', #210657, 1000.000000000000000 ) ;
#217006 = AXIS2_PLACEMENT_3D ( 'NONE', #37618, #234506, #155007 ) ;
#217007 = AXIS2_PLACEMENT_3D ( 'NONE', #20156, #204864, #140065 ) ;
#217008 = EDGE_LOOP ( 'NONE', ( #119517, #50088, #111979, #118143 ) ) ;
#217009 = AXIS2_PLACEMENT_3D ( 'NONE', #170659, #127631, #132785 ) ;
#217010 = DIRECTION ( 'NONE',  ( -1.000000000000000000, 0.000000000000000000, 0.000000000000000000 ) ) ;
#217011 = DIRECTION ( 'NONE',  ( 0.000000000000000000, 0.000000000000000000, -1.000000000000000000 ) ) ;
#217012 = CARTESIAN_POINT ( 'NONE',  ( 22.39999999999999503, 0.09999999999999939493, 7.790779598373383408 ) ) ;
#217013 = CARTESIAN_POINT ( 'NONE',  ( -23.15000000000000213, 2.000000000011154189, -180.7246219227620543 ) ) ;
#217014 = CARTESIAN_POINT ( 'NONE',  ( 15.39793903038207290, 9.389686005655649481, -15.67284350635130430 ) ) ;
#217015 = CARTESIAN_POINT ( 'NONE',  ( -18.47140463609786565, 77.27494131181350667, -241.9533158081853230 ) ) ;
#217016 = FACE_OUTER_BOUND ( 'NONE', #16481, .T. ) ;
#217018 = ORIENTED_EDGE ( 'NONE', *, *, #219388, .F. ) ;
#217017 = CARTESIAN_POINT ( 'NONE',  ( -20.94999999999999929, 77.83585931145546510, -91.51866831572576189 ) ) ;
#217020 = FACE_OUTER_BOUND ( 'NONE', #115185, .T. ) ;
#217019 = CARTESIAN_POINT ( 'NONE',  ( 18.49999999999999645, 77.16412189325286874, -61.60825939895269698 ) ) ;
#217021 = FACE_OUTER_BOUND ( 'NONE', #190158, .T. ) ;
#217022 = ORIENTED_EDGE ( 'NONE', *, *, #215837, .F. ) ;
#217023 = CARTESIAN_POINT ( 'NONE',  ( -22.39999999999999858, 12.58895012248959766, -223.3279127647276141 ) ) ;
#217024 = DIRECTION ( 'NONE',  ( -1.000000000000000000, 0.000000000000000000, 0.000000000000000000 ) ) ;
#217025 = VERTEX_POINT ( 'NONE', #214999 ) ;
#217027 = DIRECTION ( 'NONE',  ( 0.000000000000000000, 0.000000000000000000, 1.000000000000000000 ) ) ;
#217026 = DIRECTION ( 'NONE',  ( -1.000000000000000000, -0.000000000000000000, -0.000000000000000000 ) ) ;
#217028 = CARTESIAN_POINT ( 'NONE',  ( -16.89268316805465986, 9.951721813242182080, -20.85575247854553993 ) ) ;
#217029 = DIRECTION ( 'NONE',  ( 0.000000000000000000, -1.000000000000000000, -8.717686153663073805E-15 ) ) ;
#217030 = VERTEX_POINT ( 'NONE', #217552 ) ;
#217031 = VERTEX_POINT ( 'NONE', #118495 ) ;
#217032 = CARTESIAN_POINT ( 'NONE',  ( 21.14999999999999858, 6.550000000011156231, -79.15000000000004832 ) ) ;
#217033 = CARTESIAN_POINT ( 'NONE',  ( -18.47130263965438601, -0.7031555602515183745, -242.2784977795686530 ) ) ;
#217034 = CARTESIAN_POINT ( 'NONE',  ( -20.00857864376270001, 66.85000000001254250, -182.3731074845244393 ) ) ;
#217035 = CYLINDRICAL_SURFACE ( 'NONE', #138570, 0.09999999999999939493 ) ;
#217036 = VERTEX_POINT ( 'NONE', #98875 ) ;
#217037 = AXIS2_PLACEMENT_3D ( 'NONE', #141849, #204386, #146974 ) ;
#217038 = DIRECTION ( 'NONE',  ( -1.000000000000000000, 0.000000000000000000, 0.000000000000000000 ) ) ;
#217039 = CARTESIAN_POINT ( 'NONE',  ( -17.78241384940961112, 10.85557575278324904, -123.7509623275517470 ) ) ;
#217040 = DIRECTION ( 'NONE',  ( 2.342056488767301376E-15, 0.1350103645451835865, 0.9908441862701605762 ) ) ;
#217041 = DIRECTION ( 'NONE',  ( 0.000000000000000000, -0.9770955615653316162, -0.2128009952263604232 ) ) ;
#217042 = CARTESIAN_POINT ( 'NONE',  ( 18.79999999999999716, 3.461118860469513336, 28.84309995045515507 ) ) ;
#217043 = AXIS2_PLACEMENT_3D ( 'NONE', #219578, #121795, #80042 ) ;
#217045 = ORIENTED_EDGE ( 'NONE', *, *, #5983, .T. ) ;
#217044 = CARTESIAN_POINT ( 'NONE',  ( -23.25000000000000000, 36.65892442174935439, -249.5511627012433848 ) ) ;
#217046 = DIRECTION ( 'NONE',  ( 0.000000000000000000, 0.8814952561688437216, -0.4721928772777334582 ) ) ;
#217047 = CARTESIAN_POINT ( 'NONE',  ( 20.94999999999999929, 85.00000000001222134, -146.4170766071767389 ) ) ;
#217048 = DIRECTION ( 'NONE',  ( 1.000000000000000000, -7.304098846218133681E-16, 4.217023435051677994E-16 ) ) ;
#217049 = DIRECTION ( 'NONE',  ( 0.000000000000000000, -1.000000000000000000, 0.000000000000000000 ) ) ;
#217050 = EDGE_CURVE ( 'NONE', #40901, #23353, #100161, .T. ) ;
#217051 = LINE ( 'NONE', #18867, #121207 ) ;
#217053 = ORIENTED_EDGE ( 'NONE', *, *, #198015, .T. ) ;
#217052 = DIRECTION ( 'NONE',  ( 1.000000000000000000, 0.000000000000000000, 0.000000000000000000 ) ) ;
#217054 = CARTESIAN_POINT ( 'NONE',  ( 18.59999999999999432, -1.736257131586239844, -78.56865232901753870 ) ) ;
#217055 = FACE_OUTER_BOUND ( 'NONE', #76685, .T. ) ;
#217056 = DIRECTION ( 'NONE',  ( 0.000000000000000000, 0.000000000000000000, -1.000000000000000000 ) ) ;
#217057 = ORIENTED_EDGE ( 'NONE', *, *, #46189, .T. ) ;
#217058 = DIRECTION ( 'NONE',  ( 0.000000000000000000, 1.000000000000000000, 6.982962677686266711E-15 ) ) ;
#217059 = FACE_OUTER_BOUND ( 'NONE', #171187, .T. ) ;
#217061 = EDGE_CURVE ( 'NONE', #10477, #199333, #186154, .T. ) ;
#217060 = DIRECTION ( 'NONE',  ( 0.000000000000000000, -0.9126074666063770380, -0.4088369013363281068 ) ) ;
#217062 = EDGE_CURVE ( 'NONE', #229414, #24913, #189071, .T. ) ;
#217063 = CARTESIAN_POINT ( 'NONE',  ( 20.94999999999999574, 77.16270174995010223, -128.5231074845242745 ) ) ;
#217065 = VECTOR ( 'NONE', #66636, 1000.000000000000000 ) ;
#217064 = DIRECTION ( 'NONE',  ( 0.000000000000000000, 0.000000000000000000, -1.000000000000000000 ) ) ;
#217067 = CIRCLE ( 'NONE', #204606, 11.64999999999999325 ) ;
#217066 = CARTESIAN_POINT ( 'NONE',  ( 18.59999999999998721, 69.15387683765909799, -65.78538121767449809 ) ) ;
#217068 = ORIENTED_EDGE ( 'NONE', *, *, #101678, .T. ) ;
#217069 = ORIENTED_EDGE ( 'NONE', *, *, #10148, .T. ) ;
#217070 = AXIS2_PLACEMENT_3D ( 'NONE', #78862, #137555, #220951 ) ;
#217071 = DIRECTION ( 'NONE',  ( 1.000000000000000000, 0.000000000000000000, 0.000000000000000000 ) ) ;
#217072 = DIRECTION ( 'NONE',  ( 1.000000000000000000, -0.000000000000000000, -0.000000000000000000 ) ) ;
#217073 = EDGE_CURVE ( 'NONE', #106155, #200983, #179421, .T. ) ;
#217074 = LINE ( 'NONE', #1876, #253526 ) ;
#217075 = CARTESIAN_POINT ( 'NONE',  ( -23.15000000000000213, 1.115600667400684642E-11, -67.00000000000004263 ) ) ;
#217076 = ORIENTED_EDGE ( 'NONE', *, *, #112198, .T. ) ;
#217077 = CARTESIAN_POINT ( 'NONE',  ( 20.95378194480896639, 10.53491199155394220, -175.0650541481478228 ) ) ;
#217078 = CARTESIAN_POINT ( 'NONE',  ( 20.97217846901851956, 10.48122442794478637, -207.4178090057411339 ) ) ;
#217079 = AXIS2_PLACEMENT_3D ( 'NONE', #227154, #64237, #5522 ) ;
#217080 = CARTESIAN_POINT ( 'NONE',  ( -21.45000000000000284, 68.29142135624935861, -124.1731074845243512 ) ) ;
#217081 = CARTESIAN_POINT ( 'NONE',  ( -23.25000000000000000, 77.85161776048096272, -124.9199177649206689 ) ) ;
#217082 = ORIENTED_EDGE ( 'NONE', *, *, #8096, .T. ) ;
#217083 = CARTESIAN_POINT ( 'NONE',  ( -18.50000000000000000, -1.135018845899022466, -141.7169768834323520 ) ) ;
#217084 = ORIENTED_EDGE ( 'NONE', *, *, #221105, .T. ) ;
#217085 = ORIENTED_EDGE ( 'NONE', *, *, #87834, .T. ) ;
#217086 = EDGE_CURVE ( 'NONE', #238714, #167295, #98532, .T. ) ;
#217087 = CARTESIAN_POINT ( 'NONE',  ( 21.09610168723073542, 75.96641049312093230, -176.4020631997491932 ) ) ;
#217088 = CARTESIAN_POINT ( 'NONE',  ( -21.09107601085560901, 6.363877975371195816, -100.4606928352827850 ) ) ;
#217089 = ADVANCED_FACE ( 'NONE', ( #106590 ), #24535, .T. ) ;
#217090 = FACE_OUTER_BOUND ( 'NONE', #237186, .T. ) ;
#217091 = ORIENTED_EDGE ( 'NONE', *, *, #136570, .T. ) ;
#217092 = CARTESIAN_POINT ( 'NONE',  ( 20.05000000000002913, 7.250000000011171508, -113.1500000000000483 ) ) ;
#217093 = DIRECTION ( 'NONE',  ( -6.938893903907224433E-15, 1.000000000000000000, 0.000000000000000000 ) ) ;
#217094 = CARTESIAN_POINT ( 'NONE',  ( 18.50000000000000000, 78.24072131640578220, -231.5548844243369047 ) ) ;
#217095 = ORIENTED_EDGE ( 'NONE', *, *, #39111, .F. ) ;
#217096 = CARTESIAN_POINT ( 'NONE',  ( -20.94999999999999929, 76.00000000001179501, -81.32310748452431426 ) ) ;
#217098 = ORIENTED_EDGE ( 'NONE', *, *, #194289, .T. ) ;
#217097 = CARTESIAN_POINT ( 'NONE',  ( -20.85000000000000142, -1.835859311432481045, -112.0044391687985694 ) ) ;
#217099 = AXIS2_PLACEMENT_3D ( 'NONE', #171865, #231814, #173161 ) ;
#217100 = VECTOR ( 'NONE', #242136, 1000.000000000000000 ) ;
#217101 = CARTESIAN_POINT ( 'NONE',  ( -21.05000000000000071, 74.16465844978745281, -91.46795619196133487 ) ) ;
#217103 = ADVANCED_FACE ( 'NONE', ( #62359 ), #47394, .F. ) ;
#217102 = DIRECTION ( 'NONE',  ( 0.000000000000000000, -0.4930308989874718772, -0.8700118002898612479 ) ) ;
#217104 = AXIS2_PLACEMENT_3D ( 'NONE', #43886, #66013, #120884 ) ;
#217105 = EDGE_LOOP ( 'NONE', ( #35174, #2927, #96202, #203155 ) ) ;
#217106 = DIRECTION ( 'NONE',  ( -1.000000000000000000, -0.000000000000000000, -0.000000000000000000 ) ) ;
#217107 = DIRECTION ( 'NONE',  ( 0.000000000000000000, 0.2128009952263605065, -0.9770955615653315052 ) ) ;
#217108 = DIRECTION ( 'NONE',  ( 0.000000000000000000, 1.810617628050740656E-13, 1.000000000000000000 ) ) ;
#217109 = ORIENTED_EDGE ( 'NONE', *, *, #52470, .T. ) ;
#217110 = DIRECTION ( 'NONE',  ( 0.000000000000000000, -0.000000000000000000, 1.000000000000000000 ) ) ;
#217111 = CARTESIAN_POINT ( 'NONE',  ( 15.69410316191959609, 48.53345590596379111, -233.9787581418636364 ) ) ;
#217112 = DIRECTION ( 'NONE',  ( 1.000000000000000000, 0.000000000000000000, 0.000000000000000000 ) ) ;
#217113 = CIRCLE ( 'NONE', #158901, 0.09999999999999939493 ) ;
#217114 = EDGE_CURVE ( 'NONE', #220552, #60670, #147006, .T. ) ;
#217115 = EDGE_LOOP ( 'NONE', ( #249644, #187495, #150172, #35743 ) ) ;
#217116 = EDGE_LOOP ( 'NONE', ( #118631, #149094, #169535, #176200 ) ) ;
#217117 = EDGE_CURVE ( 'NONE', #127795, #6867, #222346, .T. ) ;
#217118 = ORIENTED_EDGE ( 'NONE', *, *, #141397, .T. ) ;
#217119 = CARTESIAN_POINT ( 'NONE',  ( -1.820710678118657944, -9.929289321870186313, -91.75000000000005684 ) ) ;
#217120 = FACE_OUTER_BOUND ( 'NONE', #142570, .T. ) ;
#217121 = VECTOR ( 'NONE', #220475, 1000.000000000000000 ) ;
#217123 = ORIENTED_EDGE ( 'NONE', *, *, #33521, .F. ) ;
#217122 = CARTESIAN_POINT ( 'NONE',  ( -20.85000000000000142, 11.75000000001115197, -60.21613433702190576 ) ) ;
#217124 = CARTESIAN_POINT ( 'NONE',  ( -20.00857864376270001, 44.14788529697245423, -236.0604079036328073 ) ) ;
#217125 = LINE ( 'NONE', #5786, #65591 ) ;
#217126 = EDGE_CURVE ( 'NONE', #31922, #28696, #168267, .T. ) ;
#217128 = ADVANCED_FACE ( 'NONE', ( #222689 ), #21955, .T. ) ;
#217127 = DIRECTION ( 'NONE',  ( 1.000000000000000000, 0.000000000000000000, -0.000000000000000000 ) ) ;
#217129 = CARTESIAN_POINT ( 'NONE',  ( 20.94999999999999929, 70.60000000001178933, -79.41707660717679573 ) ) ;
#217130 = CARTESIAN_POINT ( 'NONE',  ( -18.59999999999999787, 70.47363787294415260, -228.3418745167492432 ) ) ;
#217131 = CIRCLE ( 'NONE', #150713, 0.1000000000000028644 ) ;
#217132 = CARTESIAN_POINT ( 'NONE',  ( 18.59999999999999432, -1.835859311432481045, -179.0044391687985410 ) ) ;
#217134 = ORIENTED_EDGE ( 'NONE', *, *, #204368, .T. ) ;
#217133 = FACE_OUTER_BOUND ( 'NONE', #147034, .T. ) ;
#217136 = ORIENTED_EDGE ( 'NONE', *, *, #70406, .F. ) ;
#217135 = DIRECTION ( 'NONE',  ( 0.000000000000000000, 0.000000000000000000, 1.000000000000000000 ) ) ;
#217138 = FACE_OUTER_BOUND ( 'NONE', #10265, .T. ) ;
#217137 = DIRECTION ( 'NONE',  ( 0.000000000000000000, 0.2128009952263604232, -0.9770955615653316162 ) ) ;
#217140 = EDGE_LOOP ( 'NONE', ( #156951, #227605, #53356, #76443 ) ) ;
#217139 = FACE_OUTER_BOUND ( 'NONE', #118892, .T. ) ;
#217141 = AXIS2_PLACEMENT_3D ( 'NONE', #122262, #201782, #242194 ) ;
#217142 = EDGE_LOOP ( 'NONE', ( #123955, #234283, #191091, #131407 ) ) ;
#217143 = CARTESIAN_POINT ( 'NONE',  ( -20.64999999999999858, 2.000000000011154189, -120.7753780772379315 ) ) ;
#217144 = FACE_OUTER_BOUND ( 'NONE', #39243, .T. ) ;
#217145 = ADVANCED_FACE ( 'NONE', ( #223981 ), #14346, .T. ) ;
#217147 = EDGE_CURVE ( 'NONE', #41849, #33512, #105649, .T. ) ;
#217146 = TOROIDAL_SURFACE ( 'NONE', #75726, 14.20833333333334103, 0.1000000000000000056 ) ;
#217148 = DIRECTION ( 'NONE',  ( 0.000000000000000000, 0.000000000000000000, -1.000000000000000000 ) ) ;
#217149 = AXIS2_PLACEMENT_3D ( 'NONE', #126295, #20808, #165445 ) ;
#217150 = CARTESIAN_POINT ( 'NONE',  ( -16.94445028196808778, 66.00793639031432747, -123.9157773061059231 ) ) ;
#217151 = CARTESIAN_POINT ( 'NONE',  ( 23.15000000000000213, 87.65000000001246860, -173.1231074845242688 ) ) ;
#217152 = EDGE_CURVE ( 'NONE', #133508, #69777, #55751, .T. ) ;
#217153 = CYLINDRICAL_SURFACE ( 'NONE', #157302, 0.1000000000000038219 ) ;
#217154 = VECTOR ( 'NONE', #5610, 1000.000000000000000 ) ;
#217155 = CYLINDRICAL_SURFACE ( 'NONE', #214662, 0.1000000000000000472 ) ;
#217157 = ORIENTED_EDGE ( 'NONE', *, *, #185848, .F. ) ;
#217156 = ADVANCED_FACE ( 'NONE', ( #32237 ), #93454, .T. ) ;
#217158 = ORIENTED_EDGE ( 'NONE', *, *, #46742, .T. ) ;
#217159 = DIRECTION ( 'NONE',  ( -1.000000000000000000, 0.000000000000000000, 0.000000000000000000 ) ) ;
#217160 = VECTOR ( 'NONE', #212369, 1000.000000000000000 ) ;
#217161 = VERTEX_POINT ( 'NONE', #50462 ) ;
#217162 = EDGE_CURVE ( 'NONE', #38009, #41827, #101551, .T. ) ;
#217163 = DIRECTION ( 'NONE',  ( 0.000000000000000000, 0.000000000000000000, 1.000000000000000000 ) ) ;
#217165 = EDGE_CURVE ( 'NONE', #59020, #244526, #53052, .T. ) ;
#217164 = AXIS2_PLACEMENT_3D ( 'NONE', #242515, #62606, #241253 ) ;
#217166 = CARTESIAN_POINT ( 'NONE',  ( 18.50211644919735221, 68.02921119886117651, -224.2090419302653856 ) ) ;
#217167 = CARTESIAN_POINT ( 'NONE',  ( -15.74999999999999645, 66.65000000001154490, -53.00158811269928094 ) ) ;
#217168 = CARTESIAN_POINT ( 'NONE',  ( -21.00023020733502221, -1.359983335743154331, -194.7555100259054086 ) ) ;
#217169 = ADVANCED_FACE ( 'NONE', ( #131307 ), #8803, .F. ) ;
#217170 = VERTEX_POINT ( 'NONE', #192574 ) ;
#217171 = CARTESIAN_POINT ( 'NONE',  ( -12.42749937872396337, 66.62931007840941788, -118.9966423578632657 ) ) ;
#217172 = EDGE_LOOP ( 'NONE', ( #215502, #128124, #212012, #21009 ) ) ;
#217174 = CIRCLE ( 'NONE', #29973, 0.1999999999999945155 ) ;
#217173 = CARTESIAN_POINT ( 'NONE',  ( -17.78241384941129155, 10.85557575279901066, -90.25096232753028858 ) ) ;
#217175 = VERTEX_POINT ( 'NONE', #191322 ) ;
#217176 = EDGE_CURVE ( 'NONE', #44902, #92180, #201526, .T. ) ;
#217177 = LINE ( 'NONE', #157254, #56465 ) ;
#217178 = EDGE_CURVE ( 'NONE', #132943, #237152, #176441, .T. ) ;
#217179 = DIRECTION ( 'NONE',  ( 0.000000000000000000, 5.204170427930272346E-14, -1.000000000000000000 ) ) ;
#217180 = CARTESIAN_POINT ( 'NONE',  ( 18.59999999999999076, 6.650000000011155876, -188.7499999999999716 ) ) ;
#217182 = ORIENTED_EDGE ( 'NONE', *, *, #24531, .F. ) ;
#217181 = EDGE_CURVE ( 'NONE', #119689, #135869, #172366, .T. ) ;
#217183 = FACE_OUTER_BOUND ( 'NONE', #58080, .T. ) ;
#217185 = ORIENTED_EDGE ( 'NONE', *, *, #14869, .F. ) ;
#217184 = CARTESIAN_POINT ( 'NONE',  ( 18.59999999999999787, -9.849999999999996092, 31.39999999999999858 ) ) ;
#217186 = AXIS2_PLACEMENT_3D ( 'NONE', #2554, #96508, #256830 ) ;
#217187 = CARTESIAN_POINT ( 'NONE',  ( 18.59999999999999432, -1.261786168553869603, -142.0864989635454947 ) ) ;
#217189 = VERTEX_POINT ( 'NONE', #107893 ) ;
#217188 = VECTOR ( 'NONE', #185013, 1000.000000000000114 ) ;
#217190 = CIRCLE ( 'NONE', #238046, 0.1000000000000000472 ) ;
#217191 = VECTOR ( 'NONE', #174741, 1000.000000000000000 ) ;
#217192 = PLANE ( 'NONE',  #103310 ) ;
#217193 = ORIENTED_EDGE ( 'NONE', *, *, #183013, .T. ) ;
#217194 = EDGE_CURVE ( 'NONE', #65618, #178845, #126528, .T. ) ;
#217195 = CARTESIAN_POINT ( 'NONE',  ( -21.44999999999999929, 68.75000000001253397, -182.2731074845244166 ) ) ;
#217196 = FACE_OUTER_BOUND ( 'NONE', #235941, .T. ) ;
#217197 = CARTESIAN_POINT ( 'NONE',  ( -16.93772744219066340, 66.00645889125922849, -56.92504551255470346 ) ) ;
#217198 = FACE_OUTER_BOUND ( 'NONE', #76335, .T. ) ;
#217199 = VERTEX_POINT ( 'NONE', #149618 ) ;
#217200 = CARTESIAN_POINT ( 'NONE',  ( -20.64999999999999858, 1.925233644870967487, -121.2697564668739005 ) ) ;
#217201 = CARTESIAN_POINT ( 'NONE',  ( 21.04999999999879634, 6.496686585778748579, -100.5146561185119225 ) ) ;
#217202 = DIRECTION ( 'NONE',  ( 1.000000000000000000, 0.000000000000000000, 0.000000000000000000 ) ) ;
#217203 = ORIENTED_EDGE ( 'NONE', *, *, #139614, .F. ) ;
#217205 = DIRECTION ( 'NONE',  ( 0.000000000000000000, -0.4088369013363280513, 0.9126074666063769270 ) ) ;
#217204 = CIRCLE ( 'NONE', #196559, 0.1000000000000002554 ) ;
#217206 = ORIENTED_EDGE ( 'NONE', *, *, #213281, .F. ) ;
#217207 = CARTESIAN_POINT ( 'NONE',  ( 21.14999999999999858, 69.35000000001228670, -157.8731074845244109 ) ) ;
#217208 = B_SPLINE_CURVE_WITH_KNOTS ( 'NONE', 3,
 ( #166758, #185002, #207140, #6346, #147148, #85864, #5046, #226681, #83299, #168046, #145858, #84562, #128889, #205845, #144572, #164162 ),
 .UNSPECIFIED., .F., .F.,
 ( 4, 3, 3, 3, 3, 4 ),
 ( 0.000000000000000000, 2.209833635978094077E-05, 5.595056164119032002E-05, 8.979992002654962630E-05, 0.0001236482757198868558, 0.0001574984039362969837 ),
 .UNSPECIFIED. ) ;
#217209 = EDGE_LOOP ( 'NONE', ( #174558, #46418, #207665, #213077 ) ) ;
#217210 = DIRECTION ( 'NONE',  ( -1.000000000000000000, 7.304098846218135653E-16, 4.639676173203994055E-30 ) ) ;
#217211 = LINE ( 'NONE', #176845, #81148 ) ;
#217213 = ORIENTED_EDGE ( 'NONE', *, *, #126454, .T. ) ;
#217212 = PLANE ( 'NONE',  #169640 ) ;
#217214 = CARTESIAN_POINT ( 'NONE',  ( -18.59999999999999787, 6.846123162363745074, -171.2377262668498759 ) ) ;
#217215 = VERTEX_POINT ( 'NONE', #207001 ) ;
#217216 = CIRCLE ( 'NONE', #133847, 0.1000000000000014488 ) ;
#217217 = FACE_OUTER_BOUND ( 'NONE', #179712, .T. ) ;
#217218 = CARTESIAN_POINT ( 'NONE',  ( -21.05000000000000071, 85.51932773110452501, -129.5501311079648872 ) ) ;
#217219 = ORIENTED_EDGE ( 'NONE', *, *, #15899, .F. ) ;
#217220 = EDGE_LOOP ( 'NONE', ( #105940, #90196, #39599, #245020 ) ) ;
#217221 = EDGE_CURVE ( 'NONE', #114829, #157279, #231714, .T. ) ;
#217222 = DIRECTION ( 'NONE',  ( -3.265361837132813093E-16, -1.000000000000000000, 7.445645354460596589E-46 ) ) ;
#217223 = CARTESIAN_POINT ( 'NONE',  ( -22.50875500270931795, -3.275978733247508323, -228.2735451763257402 ) ) ;
#217224 = VERTEX_POINT ( 'NONE', #113034 ) ;
#217225 = CARTESIAN_POINT ( 'NONE',  ( 21.13422380239121168, 10.19493587022274106, -228.0088647928831733 ) ) ;
#217226 = ADVANCED_FACE ( 'NONE', ( #132605 ), #168464, .F. ) ;
#217227 = VERTEX_POINT ( 'NONE', #251242 ) ;
#217228 = EDGE_LOOP ( 'NONE', ( #98607, #119776, #32788 ) ) ;
#217229 = AXIS2_PLACEMENT_3D ( 'NONE', #194918, #33296, #254812 ) ;
#217230 = LINE ( 'NONE', #22933, #93199 ) ;
#217231 = EDGE_CURVE ( 'NONE', #6807, #214648, #80898, .T. ) ;
#217233 = ORIENTED_EDGE ( 'NONE', *, *, #223594, .F. ) ;
#217232 = CARTESIAN_POINT ( 'NONE',  ( 20.94999999999999929, 4.850467289719617270, -12.03426740900167857 ) ) ;
#217234 = DIRECTION ( 'NONE',  ( -1.000000000000000000, -2.952720810173289112E-16, 0.000000000000000000 ) ) ;
#217235 = DIRECTION ( 'NONE',  ( -1.000000000000000000, -0.000000000000000000, -0.000000000000000000 ) ) ;
#217236 = CARTESIAN_POINT ( 'NONE',  ( -16.80100914604134132, 63.08371810292741344, -213.1612216948777530 ) ) ;
#217238 = CARTESIAN_POINT ( 'NONE',  ( 20.27550659511089037, 66.78395627750296626, -82.17310748452437963 ) ) ;
#217237 = CYLINDRICAL_SURFACE ( 'NONE', #235827, 11.80000000000000426 ) ;
#217240 = EDGE_CURVE ( 'NONE', #213658, #223475, #214196, .T. ) ;
#217239 = LINE ( 'NONE', #97270, #157187 ) ;
#217241 = DIRECTION ( 'NONE',  ( 0.000000000000000000, 0.2128009952263678062, -0.9770955615653298398 ) ) ;
#217242 = CIRCLE ( 'NONE', #134053, 0.9750000000000036415 ) ;
#217243 = FACE_OUTER_BOUND ( 'NONE', #169122, .T. ) ;
#217244 = AXIS2_PLACEMENT_3D ( 'NONE', #18772, #215679, #116601 ) ;
#217245 = CARTESIAN_POINT ( 'NONE',  ( 22.50046968638144307, -3.207446843257450109, -228.1445966768302469 ) ) ;
#217247 = VERTEX_POINT ( 'NONE', #11369 ) ;
#217246 = CIRCLE ( 'NONE', #237935, 0.09999999999999609201 ) ;
#217248 = EDGE_LOOP ( 'NONE', ( #229838, #245759, #137134 ) ) ;
#217249 = CARTESIAN_POINT ( 'NONE',  ( 18.49505832270841310, 85.43802806279519757, -162.8246343096303974 ) ) ;
#217251 = ORIENTED_EDGE ( 'NONE', *, *, #208423, .F. ) ;
#217250 = CARTESIAN_POINT ( 'NONE',  ( -21.44999999999999929, 11.70367352607683564, -220.1991933683510467 ) ) ;
#217252 = ORIENTED_EDGE ( 'NONE', *, *, #117734, .T. ) ;
#217253 = DIRECTION ( 'NONE',  ( 1.000000000000000000, 2.952720810173289112E-16, -0.000000000000000000 ) ) ;
#217254 = ORIENTED_EDGE ( 'NONE', *, *, #155090, .T. ) ;
#217255 = DIRECTION ( 'NONE',  ( 1.284434275755705296E-16, -0.7071067811865471286, -0.7071067811865479058 ) ) ;
#217256 = ORIENTED_EDGE ( 'NONE', *, *, #242833, .T. ) ;
#217257 = VECTOR ( 'NONE', #135300, 1000.000000000000000 ) ;
#217258 = FILL_AREA_STYLE ('',( #137727 ) ) ;
#217259 = DIRECTION ( 'NONE',  ( 1.000000000000000000, 2.952720810173289112E-16, -0.000000000000000000 ) ) ;
#217261 = ORIENTED_EDGE ( 'NONE', *, *, #116274, .F. ) ;
#217260 = ORIENTED_EDGE ( 'NONE', *, *, #160764, .F. ) ;
#217262 = ORIENTED_EDGE ( 'NONE', *, *, #60769, .F. ) ;
#217263 = ORIENTED_EDGE ( 'NONE', *, *, #197644, .T. ) ;
#217264 = CARTESIAN_POINT ( 'NONE',  ( -18.59999999999999787, -1.164121893230052995, -141.8148480855716684 ) ) ;
#217265 = DIRECTION ( 'NONE',  ( 0.7070776581708965169, 4.937903618720407826E-15, -0.7071359030027827286 ) ) ;
#217267 = ORIENTED_EDGE ( 'NONE', *, *, #111450, .T. ) ;
#217266 = DIRECTION ( 'NONE',  ( 0.000000000000000000, -0.4088369013363280513, 0.9126074666063772600 ) ) ;
#217268 = DIRECTION ( 'NONE',  ( 0.000000000000000000, 0.000000000000000000, 1.000000000000000000 ) ) ;
#217269 = DIRECTION ( 'NONE',  ( 0.000000000000000000, 0.000000000000000000, 1.000000000000000000 ) ) ;
#217271 = EDGE_LOOP ( 'NONE', ( #1165, #55089, #237830, #35630 ) ) ;
#217270 = CARTESIAN_POINT ( 'NONE',  ( 20.95496329884391784, 10.56743320610419623, -141.5743099322848479 ) ) ;
#217272 = DIRECTION ( 'NONE',  ( -1.000000000000000000, 3.265361837132813093E-16, 2.280189983783949500E-30 ) ) ;
#217273 = ORIENTED_EDGE ( 'NONE', *, *, #247089, .T. ) ;
#217274 = DIRECTION ( 'NONE',  ( 0.000000000000000000, -0.6728971962617172897, 0.7397360091702445128 ) ) ;
#217275 = ADVANCED_FACE ( 'NONE', ( #73939 ), #153498, .T. ) ;
#217277 = ORIENTED_EDGE ( 'NONE', *, *, #61753, .F. ) ;
#217276 = CARTESIAN_POINT ( 'NONE',  ( -20.85000000000000142, 1.115600667400684642E-11, -67.00000000000000000 ) ) ;
#217278 = CARTESIAN_POINT ( 'NONE',  ( 18.59999999999999432, -9.480686695267811714, -207.9411151687578183 ) ) ;
#217279 = FACE_OUTER_BOUND ( 'NONE', #37309, .T. ) ;
#217280 = VECTOR ( 'NONE', #235122, 1000.000000000000000 ) ;
#217281 = VECTOR ( 'NONE', #65629, 1000.000000000000000 ) ;
#217282 = EDGE_CURVE ( 'NONE', #63545, #106375, #170495, .T. ) ;
#217283 = CARTESIAN_POINT ( 'NONE',  ( 21.04386569057627909, 11.75000000001121059, -60.14283735177934886 ) ) ;
#217284 = CIRCLE ( 'NONE', #234050, 12.87499999999999822 ) ;
#217285 = VERTEX_POINT ( 'NONE', #210854 ) ;
#217287 = CARTESIAN_POINT ( 'NONE',  ( 21.14999999999999858, 69.74218538953552127, -69.62089777583315708 ) ) ;
#217286 = CARTESIAN_POINT ( 'NONE',  ( -18.39999999999999858, -9.500000000000005329, -6.999285677838848585 ) ) ;
#217288 = CARTESIAN_POINT ( 'NONE',  ( -22.50000000000000000, 11.65000000001113278, -100.5000000000000284 ) ) ;
#217289 = CYLINDRICAL_SURFACE ( 'NONE', #130711, 0.09999999999999939493 ) ;
#217290 = CARTESIAN_POINT ( 'NONE',  ( -22.47071067811865319, 7.720074744498064412, 0.09909245470260744093 ) ) ;
#217291 = VERTEX_POINT ( 'NONE', #136411 ) ;
#217292 = ORIENTED_EDGE ( 'NONE', *, *, #34104, .F. ) ;
#217293 = EDGE_LOOP ( 'NONE', ( #187363, #42941, #240545, #149154 ) ) ;
#217294 = EDGE_CURVE ( 'NONE', #193988, #129974, #64175, .T. ) ;
#217295 = LINE ( 'NONE', #81619, #113791 ) ;
#217296 = DIRECTION ( 'NONE',  ( 0.000000000000000000, -0.9654727137038715545, 0.2605042016806676242 ) ) ;
#217297 = VERTEX_POINT ( 'NONE', #253811 ) ;
#217298 = DIRECTION ( 'NONE',  ( 0.000000000000000000, 0.000000000000000000, -1.000000000000000000 ) ) ;
#217299 = EDGE_LOOP ( 'NONE', ( #202227, #249002, #17902, #43375 ) ) ;
#217300 = CARTESIAN_POINT ( 'NONE',  ( -0.8999999999999430678, 63.75000000001118394, -10.02310748452479139 ) ) ;
#217301 = DIRECTION ( 'NONE',  ( 0.000000000000000000, 0.2128009952263604510, -0.9770955615653315052 ) ) ;
#217302 = EDGE_CURVE ( 'NONE', #129607, #79153, #158603, .T. ) ;
#217303 = EDGE_CURVE ( 'NONE', #66482, #167847, #10206, .T. ) ;
#217304 = VECTOR ( 'NONE', #106419, 1000.000000000000000 ) ;
#217305 = ORIENTED_EDGE ( 'NONE', *, *, #144412, .T. ) ;
#217306 = EDGE_CURVE ( 'NONE', #114442, #243775, #72554, .T. ) ;
#217307 = DIRECTION ( 'NONE',  ( 4.408576920032447355E-17, -0.1350103645451876666, 0.9908441862701600211 ) ) ;
#217308 = ORIENTED_EDGE ( 'NONE', *, *, #139817, .F. ) ;
#217309 = ORIENTED_EDGE ( 'NONE', *, *, #127464, .F. ) ;
#217310 = EDGE_LOOP ( 'NONE', ( #97682, #79916, #173271 ) ) ;
#217311 = DIRECTION ( 'NONE',  ( 0.000000000000000000, -6.982962677686266711E-15, 1.000000000000000000 ) ) ;
#217312 = CARTESIAN_POINT ( 'NONE',  ( -18.59999999999999787, -26.43935341558978891, -118.6415086075074896 ) ) ;
#217313 = CARTESIAN_POINT ( 'NONE',  ( 21.05000000000000071, 76.00000000001213607, -136.5231074845243313 ) ) ;
#217314 = DIRECTION ( 'NONE',  ( 0.000000000000000000, 0.9770955615653313941, 0.2128009952263603677 ) ) ;
#217315 = DIRECTION ( 'NONE',  ( -1.000000000000000000, 3.265361837132813093E-16, 2.280189983783949500E-30 ) ) ;
#217316 = EDGE_CURVE ( 'NONE', #88042, #3049, #197425, .T. ) ;
#217317 = AXIS2_PLACEMENT_3D ( 'NONE', #49531, #190338, #29995 ) ;
#217319 = DIRECTION ( 'NONE',  ( 0.000000000000000000, 0.9770955615653548199, 0.2128009952262535920 ) ) ;
#217318 = CARTESIAN_POINT ( 'NONE',  ( 21.05000000000000071, 0.05148288189269902698, -161.1998201820867394 ) ) ;
#217320 = CARTESIAN_POINT ( 'NONE',  ( -23.25000000000000000, 10.33248238083634440, -72.59484654391314962 ) ) ;
#217322 = VERTEX_POINT ( 'NONE', #17760 ) ;
#217321 = CARTESIAN_POINT ( 'NONE',  ( -18.59999999999999787, 77.14957036958755054, -95.20719500002232394 ) ) ;
#217323 = CARTESIAN_POINT ( 'NONE',  ( -16.89268316805466341, 9.951721813253341153, -79.64424752145448849 ) ) ;
#217324 = VERTEX_POINT ( 'NONE', #156034 ) ;
#217325 = FACE_OUTER_BOUND ( 'NONE', #123419, .T. ) ;
#217326 = ORIENTED_EDGE ( 'NONE', *, *, #172499, .F. ) ;
#217327 = ORIENTED_EDGE ( 'NONE', *, *, #244213, .F. ) ;
#217328 = CARTESIAN_POINT ( 'NONE',  ( 18.59999999999999787, -10.80884033489985363, 6.000000000000001776 ) ) ;
#217329 = AXIS2_PLACEMENT_3D ( 'NONE', #224082, #45457, #8904 ) ;
#217330 = DIRECTION ( 'NONE',  ( 0.000000000000000000, -0.9999631594459053030, -0.008583690987162452199 ) ) ;
#217331 = CARTESIAN_POINT ( 'NONE',  ( -20.94999999999999929, 44.25095746879271985, -258.9156452930671435 ) ) ;
#217332 = ORIENTED_EDGE ( 'NONE', *, *, #158627, .F. ) ;
#217333 = VECTOR ( 'NONE', #72255, 1000.000000000000114 ) ;
#217334 = DIRECTION ( 'NONE',  ( 1.000000000000000000, -0.000000000000000000, 0.000000000000000000 ) ) ;
#217335 = AXIS2_PLACEMENT_3D ( 'NONE', #204563, #226687, #246269 ) ;
#217336 = ORIENTED_EDGE ( 'NONE', *, *, #244932, .F. ) ;
#217337 = VERTEX_POINT ( 'NONE', #98556 ) ;
#217338 = AXIS2_PLACEMENT_3D ( 'NONE', #76593, #57005, #113160 ) ;
#217339 = DIRECTION ( 'NONE',  ( 0.000000000000000000, 0.9955484899852913294, -0.09425075112701486457 ) ) ;
#217340 = EDGE_LOOP ( 'NONE', ( #179386, #102185, #79617, #60274, #84563 ) ) ;
#217341 = DIRECTION ( 'NONE',  ( 0.000000000000000000, -7.116814260417660624E-15, 1.000000000000000000 ) ) ;
#217342 = CARTESIAN_POINT ( 'NONE',  ( -22.50000000000000000, 64.25000000001237765, -170.0231074845244166 ) ) ;
#217343 = EDGE_LOOP ( 'NONE', ( #12496, #181086, #2392, #237685 ) ) ;
#217344 = CARTESIAN_POINT ( 'NONE',  ( -18.39999999999999858, -9.682403433465239573, -140.6568433774128266 ) ) ;
#217345 = DIRECTION ( 'NONE',  ( 0.000000000000000000, 0.4088369013363783999, -0.9126074666063545004 ) ) ;
#217346 = CARTESIAN_POINT ( 'NONE',  ( 20.99999999999999645, 66.25000000001261924, -190.8731074845244393 ) ) ;
#217347 = ORIENTED_EDGE ( 'NONE', *, *, #113490, .T. ) ;
#217348 = CIRCLE ( 'NONE', #42393, 1.899999999999997913 ) ;
#217350 = VECTOR ( 'NONE', #38400, 1000.000000000000000 ) ;
#217349 = CARTESIAN_POINT ( 'NONE',  ( -23.15000000000000213, 1.115600667400684642E-11, -100.5000000000000284 ) ) ;
#217351 = CARTESIAN_POINT ( 'NONE',  ( 21.05000000000000071, 71.14953271029224879, -90.98884007552265984 ) ) ;
#217352 = CARTESIAN_POINT ( 'NONE',  ( -22.50000000000000000, 25.98655542988603173, -254.2226763854395983 ) ) ;
#217353 = CIRCLE ( 'NONE', #9089, 0.1000000000000024342 ) ;
#217354 = EDGE_CURVE ( 'NONE', #40138, #148964, #92590, .T. ) ;
#217355 = VERTEX_POINT ( 'NONE', #76460 ) ;
#217356 = CIRCLE ( 'NONE', #121561, 4.150000000000009237 ) ;
#217358 = ORIENTED_EDGE ( 'NONE', *, *, #177621, .F. ) ;
#217357 = CARTESIAN_POINT ( 'NONE',  ( -23.49999999999994316, 83.90000000001120384, -37.27310748452479316 ) ) ;
#217359 = ORIENTED_EDGE ( 'NONE', *, *, #203986, .F. ) ;
#217360 = DIRECTION ( 'NONE',  ( 0.000000000000000000, -6.938893903907222067E-15, 1.000000000000000000 ) ) ;
#217362 = EDGE_CURVE ( 'NONE', #238448, #94706, #16518, .T. ) ;
#217361 = AXIS2_PLACEMENT_3D ( 'NONE', #38888, #197932, #178412 ) ;
#217363 = PLANE ( 'NONE',  #42084 ) ;
#217364 = DIRECTION ( 'NONE',  ( 1.000000000000000000, 0.000000000000000000, 0.000000000000000000 ) ) ;
#217365 = PLANE ( 'NONE',  #189784 ) ;
#217366 = DIRECTION ( 'NONE',  ( 0.000000000000000000, 1.000000000000000000, 6.982962677686266711E-15 ) ) ;
#217367 = CARTESIAN_POINT ( 'NONE',  ( -20.94999999999999929, -1.835341550213255957, -45.05515129256298223 ) ) ;
#217368 = ORIENTED_EDGE ( 'NONE', *, *, #253350, .F. ) ;
#217369 = CARTESIAN_POINT ( 'NONE',  ( -17.04295772865470937, 65.97510057475071221, -149.1731074845244507 ) ) ;
#217370 = LINE ( 'NONE', #59560, #123225 ) ;
#217371 = EDGE_CURVE ( 'NONE', #24982, #32549, #226656, .T. ) ;
#217372 = EDGE_CURVE ( 'NONE', #139747, #227184, #97451, .T. ) ;
#217373 = CARTESIAN_POINT ( 'NONE',  ( -18.50000000000000355, 77.31057150535087885, -241.6632115154811231 ) ) ;
#217374 = CARTESIAN_POINT ( 'NONE',  ( -23.15000000000000213, 1.115626384983466744E-11, -198.8999999999999773 ) ) ;
#217375 = VECTOR ( 'NONE', #83994, 1000.000000000000114 ) ;
#217376 = CIRCLE ( 'NONE', #104919, 11.90000000000000746 ) ;
#217377 = CARTESIAN_POINT ( 'NONE',  ( 22.39999999999999858, 7.790779598384538929, -133.9000000000000057 ) ) ;
#217378 = AXIS2_PLACEMENT_3D ( 'NONE', #183687, #70176, #5010 ) ;
#217379 = ORIENTED_EDGE ( 'NONE', *, *, #42190, .T. ) ;
#217380 = VERTEX_POINT ( 'NONE', #15234 ) ;
#217381 = CARTESIAN_POINT ( 'NONE',  ( 21.05000000000000071, 0.000000000000000000, -37.60000000000000142 ) ) ;
#217382 = LINE ( 'NONE', #177024, #130228 ) ;
#217383 = CYLINDRICAL_SURFACE ( 'NONE', #126815, 2.000000000000001776 ) ;
#217384 = DIRECTION ( 'NONE',  ( 0.000000000000000000, 0.9126074666063770380, 0.4088369013363281068 ) ) ;
#217385 = LINE ( 'NONE', #196550, #66333 ) ;
#217386 = EDGE_CURVE ( 'NONE', #171525, #204139, #245003, .T. ) ;
#217387 = ORIENTED_EDGE ( 'NONE', *, *, #41375, .F. ) ;
#217388 = CARTESIAN_POINT ( 'NONE',  ( -18.44362607810622379, 46.98013086100849733, -255.3267083682162593 ) ) ;
#217389 = EDGE_CURVE ( 'NONE', #144504, #211036, #251608, .T. ) ;
#217390 = FACE_OUTER_BOUND ( 'NONE', #187196, .T. ) ;
#217391 = ORIENTED_EDGE ( 'NONE', *, *, #155118, .F. ) ;
#217392 = CARTESIAN_POINT ( 'NONE',  ( -18.59999999999999787, -9.499999999988842703, -112.6500000000000483 ) ) ;
#217393 = PRODUCT_RELATED_PRODUCT_CATEGORY ( 'part', '', ( #162165 ) ) ;
#217394 = DIRECTION ( 'NONE',  ( 0.000000000000000000, -0.8814952561688430555, 0.4721928772777346239 ) ) ;
#217395 = VECTOR ( 'NONE', #88389, 1000.000000000000000 ) ;
#217396 = ORIENTED_EDGE ( 'NONE', *, *, #157163, .T. ) ;
#217397 = CARTESIAN_POINT ( 'NONE',  ( -21.04999999999994387, 74.83745509109094485, -44.02310748452479316 ) ) ;
#217398 = ADVANCED_FACE ( 'NONE', ( #217243 ), #257613, .T. ) ;
#217399 = ORIENTED_EDGE ( 'NONE', *, *, #245089, .F. ) ;
#217400 = EDGE_CURVE ( 'NONE', #63983, #197300, #101791, .T. ) ;
#217401 = DIRECTION ( 'NONE',  ( 1.000000000000000000, -0.000000000000000000, 0.000000000000000000 ) ) ;
#217402 = ADVANCED_FACE ( 'NONE', ( #138975 ), #60742, .F. ) ;
#217403 = CARTESIAN_POINT ( 'NONE',  ( 21.04999999999999716, 69.69981666374616225, -170.0744349168656129 ) ) ;
#217404 = LINE ( 'NONE', #118336, #245119 ) ;
#217405 = DIRECTION ( 'NONE',  ( 0.000000000000000000, 1.000000000000000000, -0.000000000000000000 ) ) ;
#217406 = FACE_OUTER_BOUND ( 'NONE', #53828, .T. ) ;
#217407 = CARTESIAN_POINT ( 'NONE',  ( 21.05000000000000071, 18.88692293749142337, -227.8658170387887481 ) ) ;
#217408 = DIRECTION ( 'NONE',  ( -0.7071067811865462405, -0.3338907855510745981, -0.6233112732207625184 ) ) ;
#217409 = PLANE ( 'NONE',  #222323 ) ;
#217410 = CARTESIAN_POINT ( 'NONE',  ( 20.94999999999999929, 67.23127455305835554, -235.8551265064784559 ) ) ;
#217411 = FACE_OUTER_BOUND ( 'NONE', #250954, .T. ) ;
#217412 = DIRECTION ( 'NONE',  ( 0.000000000000000000, 0.000000000000000000, -1.000000000000000000 ) ) ;
#217413 = DIRECTION ( 'NONE',  ( 1.734723475976817507E-14, -1.000000000000000000, 0.000000000000000000 ) ) ;
#217414 = DIRECTION ( 'NONE',  ( -0.000000000000000000, 0.000000000000000000, -1.000000000000000000 ) ) ;
#217415 = DIRECTION ( 'NONE',  ( -0.000000000000000000, 0.000000000000000000, -1.000000000000000000 ) ) ;
#217416 = AXIS2_PLACEMENT_3D ( 'NONE', #49661, #186623, #207471 ) ;
#217417 = VERTEX_POINT ( 'NONE', #45048 ) ;
#217418 = DIRECTION ( 'NONE',  ( 1.000000000000000000, 0.000000000000000000, 0.000000000000000000 ) ) ;
#217419 = CARTESIAN_POINT ( 'NONE',  ( 19.99999999999998934, 11.75000000001115907, -58.35000000000000142 ) ) ;
#217420 = CARTESIAN_POINT ( 'NONE',  ( -33.72168855820452649, 11.47316190337362585, -176.7499999999999716 ) ) ;
#217421 = VERTEX_POINT ( 'NONE', #140273 ) ;
#217422 = DIRECTION ( 'NONE',  ( 1.000000000000000000, 0.000000000000000000, -0.000000000000000000 ) ) ;
#217423 = EDGE_CURVE ( 'NONE', #16903, #106026, #239132, .T. ) ;
#217424 = FACE_OUTER_BOUND ( 'NONE', #225228, .T. ) ;
#217425 = EDGE_LOOP ( 'NONE', ( #209591, #257955, #224565, #171085, #121791, #219624, #101299, #258088, #252803, #162517, #47242, #65517, #95494, #126754, #235628, #51892, #77852, #150688 ) ) ;
#217426 = DIRECTION ( 'NONE',  ( -1.000000000000000000, -0.000000000000000000, -0.000000000000000000 ) ) ;
#217427 = CYLINDRICAL_SURFACE ( 'NONE', #5940, 0.5000000000000004441 ) ;
#217428 = VECTOR ( 'NONE', #226987, 1000.000000000000000 ) ;
#217429 = EDGE_LOOP ( 'NONE', ( #238288, #13910, #122804, #105830 ) ) ;
#217430 = VECTOR ( 'NONE', #44607, 1000.000000000000000 ) ;
#217431 = EDGE_LOOP ( 'NONE', ( #12082, #75062, #73573, #128401 ) ) ;
#217432 = CARTESIAN_POINT ( 'NONE',  ( -20.00857864376270001, 9.150000000011157653, -179.8499999999999943 ) ) ;
#217433 = EDGE_CURVE ( 'NONE', #11272, #152525, #189263, .T. ) ;
#217434 = ORIENTED_EDGE ( 'NONE', *, *, #167107, .F. ) ;
#217435 = CYLINDRICAL_SURFACE ( 'NONE', #145685, 0.1000000000000028644 ) ;
#217436 = CARTESIAN_POINT ( 'NONE',  ( -21.07928932188134041, 10.02993822722303818, -228.1074463178677263 ) ) ;
#217438 = CARTESIAN_POINT ( 'NONE',  ( -23.15000000000000213, 11.65000000001115588, -188.8499999999999659 ) ) ;
#217437 = UNCERTAINTY_MEASURE_WITH_UNIT (LENGTH_MEASURE( 1.000000000000000082E-05 ), #43531, 'distance_accuracy_value', 'NONE');
#217439 = ADVANCED_FACE ( 'NONE', ( #62059 ), #201546, .F. ) ;
#217440 = SPHERICAL_SURFACE ( 'NONE', #54518, 0.1000000000000000056 ) ;
#217441 = DIRECTION ( 'NONE',  ( 0.000000000000000000, 0.9908441862701782288, 0.1350103645450542456 ) ) ;
#217442 = DIRECTION ( 'NONE',  ( 0.000000000000000000, -1.000000000000000000, -2.891205793294679805E-16 ) ) ;
#217443 = AXIS2_PLACEMENT_3D ( 'NONE', #25793, #46617, #144427 ) ;
#217444 = PLANE ( 'NONE',  #242695 ) ;
#217446 = CARTESIAN_POINT ( 'NONE',  ( -20.94999999999999929, 1.835341550235567887, -45.15515129256298366 ) ) ;
#217445 = AXIS2_PLACEMENT_3D ( 'NONE', #246404, #203431, #44363 ) ;
#217447 = ADVANCED_FACE ( 'NONE', ( #82849 ), #106280, .T. ) ;
#217449 = ORIENTED_EDGE ( 'NONE', *, *, #145128, .T. ) ;
#217448 = DIRECTION ( 'NONE',  ( 0.000000000000000000, 0.000000000000000000, -1.000000000000000000 ) ) ;
#217450 = ORIENTED_EDGE ( 'NONE', *, *, #229017, .F. ) ;
#217452 = CARTESIAN_POINT ( 'NONE',  ( 21.05000000000000071, 0.000000000000000000, -33.50000000000000000 ) ) ;
#217451 = DIRECTION ( 'NONE',  ( 0.000000000000000000, -0.1298341882519953860, -0.9915357197604862671 ) ) ;
#217454 = VERTEX_POINT ( 'NONE', #81571 ) ;
#217453 = DIRECTION ( 'NONE',  ( 0.000000000000000000, 0.000000000000000000, -1.000000000000000000 ) ) ;
#217455 = ORIENTED_EDGE ( 'NONE', *, *, #186854, .T. ) ;
#217456 = CARTESIAN_POINT ( 'NONE',  ( 23.14999999999999503, 6.650000000011155876, -121.6500000000000341 ) ) ;
#217457 = CARTESIAN_POINT ( 'NONE',  ( 20.97107704358301916, 8.875478152032441059, -176.0589732293892382 ) ) ;
#217458 = EDGE_CURVE ( 'NONE', #96655, #209179, #200276, .T. ) ;
#217459 = EDGE_CURVE ( 'NONE', #208096, #67858, #1785, .T. ) ;
#217460 = FACE_OUTER_BOUND ( 'NONE', #141825, .T. ) ;
#217461 = CARTESIAN_POINT ( 'NONE',  ( 18.49713797159854423, -9.446482327578955562, -7.071458121610131542 ) ) ;
#217462 = DIRECTION ( 'NONE',  ( 0.000000000000000000, 0.000000000000000000, -1.000000000000000000 ) ) ;
#217463 = DIRECTION ( 'NONE',  ( 0.000000000000000000, 0.000000000000000000, 1.000000000000000000 ) ) ;
#217464 = CARTESIAN_POINT ( 'NONE',  ( -21.05000000000000071, 28.46617234522943107, -258.4921533293940570 ) ) ;
#217465 = AXIS2_PLACEMENT_3D ( 'NONE', #6454, #242501, #181273 ) ;
#217466 = AXIS2_PLACEMENT_3D ( 'NONE', #137532, #179274, #235356 ) ;
#217468 = VECTOR ( 'NONE', #64125, 1000.000000000000114 ) ;
#217467 = CYLINDRICAL_SURFACE ( 'NONE', #226971, 1.500000000000001332 ) ;
#217469 = ORIENTED_EDGE ( 'NONE', *, *, #171564, .F. ) ;
#217470 = ORIENTED_EDGE ( 'NONE', *, *, #7037, .T. ) ;
#217471 = DIRECTION ( 'NONE',  ( 1.000000000000000000, 0.000000000000000000, 0.000000000000000000 ) ) ;
#217472 = EDGE_CURVE ( 'NONE', #96731, #179633, #27024, .T. ) ;
#217473 = ORIENTED_EDGE ( 'NONE', *, *, #166916, .F. ) ;
#217474 = CARTESIAN_POINT ( 'NONE',  ( 20.94999999999999574, 79.00474222147506964, -236.0434322704576573 ) ) ;
#217476 = EDGE_CURVE ( 'NONE', #9522, #71022, #180879, .T. ) ;
#217475 = ORIENTED_EDGE ( 'NONE', *, *, #42670, .F. ) ;
#217477 = DIRECTION ( 'NONE',  ( 0.000000000000000000, 0.000000000000000000, 1.000000000000000000 ) ) ;
#217478 = DIRECTION ( 'NONE',  ( 0.000000000000000000, 0.9915357197604792727, -0.1298341882520475943 ) ) ;
#217479 = CARTESIAN_POINT ( 'NONE',  ( 18.69999999999999929, -9.849999999999994316, 30.00000000000000355 ) ) ;
#217480 = EDGE_CURVE ( 'NONE', #67927, #190104, #89277, .T. ) ;
#217482 = ORIENTED_EDGE ( 'NONE', *, *, #142978, .F. ) ;
#217481 = CARTESIAN_POINT ( 'NONE',  ( 18.59999999999999432, -9.480686695267811714, -207.9411151687578183 ) ) ;
#217483 = CARTESIAN_POINT ( 'NONE',  ( -20.85000000000000142, 11.75000000001115197, -127.2161343370219413 ) ) ;
#217484 = VERTEX_POINT ( 'NONE', #223670 ) ;
#217485 = DIRECTION ( 'NONE',  ( 1.000000000000000000, -0.000000000000000000, -0.000000000000000000 ) ) ;
#217486 = AXIS2_PLACEMENT_3D ( 'NONE', #7038, #65733, #246925 ) ;
#217487 = DIRECTION ( 'NONE',  ( -0.000000000000000000, 1.000000000000000000, 6.982962677686266711E-15 ) ) ;
#217488 = DIRECTION ( 'NONE',  ( 0.000000000000000000, 0.8887656589064600876, -0.4583618696494786149 ) ) ;
#217489 = EDGE_CURVE ( 'NONE', #114560, #77502, #76814, .T. ) ;
#217490 = DIRECTION ( 'NONE',  ( -1.000000000000000000, 0.000000000000000000, 0.000000000000000000 ) ) ;
#217491 = DIRECTION ( 'NONE',  ( 1.000000000000000000, 0.000000000000000000, 0.000000000000000000 ) ) ;
#217493 = VERTEX_POINT ( 'NONE', #24223 ) ;
#217492 = EDGE_CURVE ( 'NONE', #2987, #62655, #172550, .T. ) ;
#217494 = CARTESIAN_POINT ( 'NONE',  ( -18.47130263965443220, 85.47115558597528207, -29.33970271904725280 ) ) ;
#217495 = VERTEX_POINT ( 'NONE', #243236 ) ;
#217498 = ORIENTED_EDGE ( 'NONE', *, *, #90964, .T. ) ;
#217497 = DIRECTION ( 'NONE',  ( 0.000000000000000000, 0.1298341882519953583, 0.9915357197604862671 ) ) ;
#217496 = CARTESIAN_POINT ( 'NONE',  ( -20.64999999999999858, -6.488386256076841718, -212.2361678873109554 ) ) ;
#217499 = AXIS2_PLACEMENT_3D ( 'NONE', #13033, #96370, #35180 ) ;
#217500 = CARTESIAN_POINT ( 'NONE',  ( 22.39999999999999503, 76.10085836911075319, -114.7726746080137019 ) ) ;
#217501 = FACE_OUTER_BOUND ( 'NONE', #150610, .T. ) ;
#217502 = ORIENTED_EDGE ( 'NONE', *, *, #188313, .F. ) ;
#217503 = CARTESIAN_POINT ( 'NONE',  ( 18.52326479938734849, 85.64236444492715350, -129.8083500711180136 ) ) ;
#217504 = AXIS2_PLACEMENT_3D ( 'NONE', #181357, #255687, #39284 ) ;
#217505 = ADVANCED_FACE ( 'NONE', ( #64601 ), #126712, .F. ) ;
#217506 = CARTESIAN_POINT ( 'NONE',  ( -22.50000000000000000, -3.092988775432913506, -228.1437074281570858 ) ) ;
#217507 = EDGE_CURVE ( 'NONE', #220102, #118038, #255656, .T. ) ;
#217509 = VERTEX_POINT ( 'NONE', #125854 ) ;
#217508 = CARTESIAN_POINT ( 'NONE',  ( 18.49999999999999645, 76.00000000001267608, -203.5231074845243597 ) ) ;
#217510 = AXIS2_PLACEMENT_3D ( 'NONE', #192685, #34921, #173163 ) ;
#217511 = DIRECTION ( 'NONE',  ( -1.000000000000000000, -1.394253735153569469E-16, -2.602809386958778209E-16 ) ) ;
#217512 = AXIS2_PLACEMENT_3D ( 'NONE', #70661, #111037, #130591 ) ;
#217513 = ORIENTED_EDGE ( 'NONE', *, *, #82955, .F. ) ;
#217514 = VECTOR ( 'NONE', #34177, 1000.000000000000000 ) ;
#217515 = CARTESIAN_POINT ( 'NONE',  ( -13.39999999999994529, 67.72071067812984779, -21.02310748452479316 ) ) ;
#217516 = CARTESIAN_POINT ( 'NONE',  ( -23.25000000000000000, 4.150000000000001243, -12.35000000000000142 ) ) ;
#217517 = CARTESIAN_POINT ( 'NONE',  ( -20.54999999999999716, 1.115600667400684642E-11, -67.00000000000000000 ) ) ;
#217518 = ORIENTED_EDGE ( 'NONE', *, *, #11813, .T. ) ;
#217519 = CARTESIAN_POINT ( 'NONE',  ( -15.55912972643741199, 22.28907679569445932, -232.2212793431121440 ) ) ;
#217521 = ORIENTED_EDGE ( 'NONE', *, *, #160921, .T. ) ;
#217520 = TOROIDAL_SURFACE ( 'NONE', #51094, 12.97499999999999787, 0.1000000000000000056 ) ;
#217522 = DIRECTION ( 'NONE',  ( -0.000000000000000000, -1.000000000000000000, -0.000000000000000000 ) ) ;
#217523 = TOROIDAL_SURFACE ( 'NONE', #130230, 0.2000000000000000111, 0.1000000000000000056 ) ;
#217524 = CARTESIAN_POINT ( 'NONE',  ( 13.99999999999999822, 66.15000000001258229, -186.7731074845244450 ) ) ;
#217525 = CARTESIAN_POINT ( 'NONE',  ( -16.91049119928364419, 9.950000000011138823, -46.11827960680916760 ) ) ;
#217526 = ORIENTED_EDGE ( 'NONE', *, *, #28307, .T. ) ;
#217527 = CARTESIAN_POINT ( 'NONE',  ( 21.07189867249812210, 22.95831064513460973, -230.0453146669910325 ) ) ;
#217528 = CYLINDRICAL_SURFACE ( 'NONE', #101250, 0.1000000000000028644 ) ;
#217529 = CARTESIAN_POINT ( 'NONE',  ( -20.94999999999999929, 64.35000000001251408, -176.8069731475025321 ) ) ;
#217530 = VERTEX_POINT ( 'NONE', #26799 ) ;
#217531 = AXIS2_PLACEMENT_3D ( 'NONE', #240589, #184458, #200185 ) ;
#217532 = CARTESIAN_POINT ( 'NONE',  ( 5.899999999999996803, -11.65000000000000036, 13.90000000000000213 ) ) ;
#217534 = DIRECTION ( 'NONE',  ( 0.000000000000000000, -1.000000000000000000, 0.000000000000000000 ) ) ;
#217533 = AXIS2_PLACEMENT_3D ( 'NONE', #79421, #117292, #165074 ) ;
#217535 = EDGE_CURVE ( 'NONE', #138090, #5531, #143275, .T. ) ;
#217536 = EDGE_LOOP ( 'NONE', ( #95448, #4299, #21649, #128775 ) ) ;
#217537 = AXIS2_PLACEMENT_3D ( 'NONE', #44688, #244143, #124227 ) ;
#217538 = AXIS2_PLACEMENT_3D ( 'NONE', #72453, #91989, #49014 ) ;
#217539 = VERTEX_POINT ( 'NONE', #131004 ) ;
#217541 = EDGE_LOOP ( 'NONE', ( #75923, #95933, #72434, #227214, #107636, #28061, #179084, #119833, #124971, #63390, #257222 ) ) ;
#217540 = CYLINDRICAL_SURFACE ( 'NONE', #109590, 0.09999999999999939493 ) ;
#217542 = AXIS2_PLACEMENT_3D ( 'NONE', #245843, #146709, #150599 ) ;
#217545 = ORIENTED_EDGE ( 'NONE', *, *, #253648, .F. ) ;
#217544 = ORIENTED_EDGE ( 'NONE', *, *, #129500, .F. ) ;
#217543 = CARTESIAN_POINT ( 'NONE',  ( -21.12757541349819590, 0.005161215809727781600, 6.473380571251563964 ) ) ;
#217546 = CARTESIAN_POINT ( 'NONE',  ( 21.05000000000000071, 64.35000000001258513, -191.3731074845244393 ) ) ;
#217547 = CARTESIAN_POINT ( 'NONE',  ( -20.94788355080264353, 65.69792220476271893, -30.53355541284615526 ) ) ;
#217548 = DIRECTION ( 'NONE',  ( -1.000000000000000000, 0.000000000000000000, 0.000000000000000000 ) ) ;
#217549 = CARTESIAN_POINT ( 'NONE',  ( -16.80891096016299002, 12.41027476423438891, -211.2256307007121734 ) ) ;
#217551 = EDGE_CURVE ( 'NONE', #94408, #203994, #105838, .T. ) ;
#217550 = CARTESIAN_POINT ( 'NONE',  ( -23.15000000000000213, 85.00000000001179501, -79.41707660717668205 ) ) ;
#217552 = CARTESIAN_POINT ( 'NONE',  ( -18.59999999999999787, 78.57744179526842743, -232.8011145694030972 ) ) ;
#217553 = VECTOR ( 'NONE', #231919, 1000.000000000000000 ) ;
#217554 = FACE_OUTER_BOUND ( 'NONE', #215220, .T. ) ;
#217557 = LINE ( 'NONE', #20682, #30789 ) ;
#217556 = DIRECTION ( 'NONE',  ( 0.000000000000000000, 6.982962677686266711E-15, -1.000000000000000000 ) ) ;
#217555 = AXIS2_PLACEMENT_3D ( 'NONE', #200367, #201642, #256413 ) ;
#217558 = VERTEX_POINT ( 'NONE', #127155 ) ;
#217559 = ORIENTED_EDGE ( 'NONE', *, *, #142305, .F. ) ;
#217560 = DIRECTION ( 'NONE',  ( 1.000000000000000000, -0.000000000000000000, -0.000000000000000000 ) ) ;
#217562 = ORIENTED_EDGE ( 'NONE', *, *, #166125, .F. ) ;
#217561 = CARTESIAN_POINT ( 'NONE',  ( -18.59999999999999787, 1.115600667400684642E-11, -200.9999999999999432 ) ) ;
#217563 = ORIENTED_EDGE ( 'NONE', *, *, #40078, .F. ) ;
#217564 = DIRECTION ( 'NONE',  ( -1.000000000000000000, -0.000000000000000000, -0.000000000000000000 ) ) ;
#217565 = ORIENTED_EDGE ( 'NONE', *, *, #138949, .T. ) ;
#217566 = CARTESIAN_POINT ( 'NONE',  ( -22.59999999999999787, 0.1008583691098682150, -55.25043287651065782 ) ) ;
#217567 = B_SPLINE_CURVE_WITH_KNOTS ( 'NONE', 3,
 ( #233667, #156722, #154164, #36782, #155445, #212819, #35492, #175018, #194560, #215367 ),
 .UNSPECIFIED., .F., .F.,
 ( 4, 3, 3, 4 ),
 ( 0.000000000000000000, 0.0002000000000008537104, 0.001000000000082977483, 0.001967863649483329782 ),
 .UNSPECIFIED. ) ;
#217568 = VERTEX_POINT ( 'NONE', #87999 ) ;
#217569 = DIRECTION ( 'NONE',  ( 1.000000000000000000, 0.000000000000000000, 0.000000000000000000 ) ) ;
#217570 = FACE_OUTER_BOUND ( 'NONE', #131810, .T. ) ;
#217571 = AXIS2_PLACEMENT_3D ( 'NONE', #22997, #222412, #88039 ) ;
#217573 = EDGE_LOOP ( 'NONE', ( #247095, #227702, #44051, #138268 ) ) ;
#217572 = ORIENTED_EDGE ( 'NONE', *, *, #71335, .F. ) ;
#217574 = VERTEX_POINT ( 'NONE', #171458 ) ;
#217575 = CARTESIAN_POINT ( 'NONE',  ( -20.94999999999999929, 1.115600667400684642E-11, -134.0000000000000284 ) ) ;
#217576 = ORIENTED_EDGE ( 'NONE', *, *, #15101, .F. ) ;
#217577 = EDGE_LOOP ( 'NONE', ( #115210, #174991, #243680, #179666, #75844, #227108, #173378, #53012, #206349, #183500, #1860, #78980 ) ) ;
#217578 = CARTESIAN_POINT ( 'NONE',  ( 18.59999999999999076, 6.650000000011155876, -54.65000000000000568 ) ) ;
#217579 = AXIS2_PLACEMENT_3D ( 'NONE', #143646, #244026, #84925 ) ;
#217580 = ORIENTED_EDGE ( 'NONE', *, *, #48199, .F. ) ;
#217582 = DIRECTION ( 'NONE',  ( 0.000000000000000000, 0.000000000000000000, -1.000000000000000000 ) ) ;
#217581 = FACE_OUTER_BOUND ( 'NONE', #138823, .T. ) ;
#217583 = DIRECTION ( 'NONE',  ( -1.000000000000000000, 0.000000000000000000, 0.000000000000000000 ) ) ;
#217584 = DIRECTION ( 'NONE',  ( 0.000000000000000000, 0.000000000000000000, -1.000000000000000000 ) ) ;
#217585 = CARTESIAN_POINT ( 'NONE',  ( 23.25000000000000000, 87.75000000001246292, -181.7731074845242745 ) ) ;
#217586 = EDGE_LOOP ( 'NONE', ( #84922, #120132, #70230, #232643, #120179, #97336, #123374, #31032 ) ) ;
#217587 = VERTEX_POINT ( 'NONE', #248390 ) ;
#217588 = DIRECTION ( 'NONE',  ( 0.000000000000000000, 0.08413937888704772772, -0.9964539953858893018 ) ) ;
#217589 = CARTESIAN_POINT ( 'NONE',  ( -16.86420534634261514, 66.02938455442051691, -149.1047709352870356 ) ) ;
#217590 = PLANE ( 'NONE',  #87102 ) ;
#217591 = EDGE_CURVE ( 'NONE', #16549, #184365, #9769, .T. ) ;
#217592 = ORIENTED_EDGE ( 'NONE', *, *, #148378, .T. ) ;
#217593 = DIRECTION ( 'NONE',  ( 0.000000000000000000, -6.982962677686266711E-15, 1.000000000000000000 ) ) ;
#217594 = AXIS2_PLACEMENT_3D ( 'NONE', #18882, #257440, #80103 ) ;
#217595 = DIRECTION ( 'NONE',  ( -0.000000000000000000, 0.2617529984165031243, 0.9651348961777157509 ) ) ;
#217596 = DIRECTION ( 'NONE',  ( -0.000000000000000000, 3.469446951953635015E-14, 1.000000000000000000 ) ) ;
#217597 = EDGE_LOOP ( 'NONE', ( #65911, #61079, #91785, #73416 ) ) ;
#217598 = ORIENTED_EDGE ( 'NONE', *, *, #8179, .T. ) ;
#217599 = EDGE_CURVE ( 'NONE', #206540, #159653, #60060, .T. ) ;
#217600 = DIRECTION ( 'NONE',  ( 0.000000000000000000, 0.000000000000000000, -1.000000000000000000 ) ) ;
#217601 = DIRECTION ( 'NONE',  ( -1.000000000000000000, 0.000000000000000000, 0.000000000000000000 ) ) ;
#217602 = ORIENTED_EDGE ( 'NONE', *, *, #183258, .F. ) ;
#217603 = DIRECTION ( 'NONE',  ( 0.000000000000000000, 1.000000000000000000, 0.000000000000000000 ) ) ;
#217604 = EDGE_LOOP ( 'NONE', ( #69329, #18779, #248267, #108272 ) ) ;
#217605 = DIRECTION ( 'NONE',  ( 0.000000000000000000, 0.2128009952263604232, -0.9770955615653316162 ) ) ;
#217606 = DIRECTION ( 'NONE',  ( 0.000000000000000000, 0.000000000000000000, 1.000000000000000000 ) ) ;
#217608 = CARTESIAN_POINT ( 'NONE',  ( -22.49533356619863866, 55.97040697583999247, -232.8685561480747310 ) ) ;
#217607 = FACE_OUTER_BOUND ( 'NONE', #116302, .T. ) ;
#217609 = ADVANCED_FACE ( 'NONE', ( #231404 ), #68473, .F. ) ;
#217610 = CARTESIAN_POINT ( 'NONE',  ( -20.54999999999999716, 74.05981308412438580, -149.3522266955776843 ) ) ;
#217611 = AXIS2_PLACEMENT_3D ( 'NONE', #15360, #94866, #196536 ) ;
#217612 = EDGE_CURVE ( 'NONE', #124911, #174581, #250935, .T. ) ;
#217613 = DIRECTION ( 'NONE',  ( 0.000000000000000000, 0.000000000000000000, -1.000000000000000000 ) ) ;
#217615 = ORIENTED_EDGE ( 'NONE', *, *, #137615, .F. ) ;
#217614 = ORIENTED_EDGE ( 'NONE', *, *, #245428, .T. ) ;
#217616 = VERTEX_POINT ( 'NONE', #211840 ) ;
#217617 = AXIS2_PLACEMENT_3D ( 'NONE', #114699, #80685, #216360 ) ;
#217618 = FACE_OUTER_BOUND ( 'NONE', #198258, .T. ) ;
#217619 = LINE ( 'NONE', #238493, #115638 ) ;
#217620 =( BOUNDED_SURFACE ( )  B_SPLINE_SURFACE ( 3, 2, ( 
 ( #36106, #253839, #75246 ),
 ( #257635, #79035, #193895 ),
 ( #15263, #94774, #214721 ),
 ( #55614, #120788, #201572 ),
 ( #141601, #161178, #66889 ),
 ( #146401, #228546, #200300 ),
 ( #101142, #41255, #68175 ),
 ( #221127, #3358, #206403 ),
 ( #162472, #129432, #219852 ),
 ( #245539, #109851, #225926 ),
 ( #60771, #2077, #42497 ),
 ( #82876, #207702, #122047 ) ),
 .UNSPECIFIED., .F., .F., .F. ) 
 B_SPLINE_SURFACE_WITH_KNOTS ( ( 4, 2, 2, 2, 2, 4 ),
 ( 3, 3 ),
 ( 3.174653483277205090, 3.943930578431714018, 4.713207673586222946, 5.482484768740731873, 5.867123316317986337, 6.251761863895240801 ),
 ( 0.000000000000000000, 1.000000000000000000 ),
 .UNSPECIFIED. ) 
 GEOMETRIC_REPRESENTATION_ITEM ( )  RATIONAL_B_SPLINE_SURFACE ( (
 ( 1.000000000000000000, 0.8659465255642859738, 1.000000000000000000),
 ( 1.000000000000000000, 0.8648614068486716322, 1.000000000000000000),
 ( 1.000000000000000000, 0.8489031841325624939, 1.000000000000000000),
 ( 1.000000000000000000, 0.7927507630159957852, 1.000000000000000000),
 ( 1.000000000000000000, 0.7523013859024111349, 1.000000000000000000),
 ( 1.000000000000000000, 0.6616226951181095606, 1.000000000000000000),
 ( 1.000000000000000000, 0.6112214368682694632, 1.000000000000000000),
 ( 1.000000000000000000, 0.5507684314519089019, 1.000000000000000000),
 ( 1.000000000000000000, 0.5333267243155448423, 1.000000000000000000),
 ( 1.000000000000000000, 0.5084565446476616568, 1.000000000000000000),
 ( 1.000000000000000000, 0.5010722703453642790, 1.000000000000000000),
 ( 1.000000000000000000, 0.5001234037138547750, 1.000000000000000000) ) ) 
 REPRESENTATION_ITEM ( '' )  SURFACE ( )  );
#217621 = DIRECTION ( 'NONE',  ( 2.715809747126116508E-16, -1.000000000000000000, 0.000000000000000000 ) ) ;
#217622 = CARTESIAN_POINT ( 'NONE',  ( 20.94999999999999929, 84.66355140188136374, -146.0472086025916099 ) ) ;
#217623 = EDGE_CURVE ( 'NONE', #177617, #120136, #151886, .T. ) ;
#217625 = DIRECTION ( 'NONE',  ( 0.000000000000000000, 0.000000000000000000, -1.000000000000000000 ) ) ;
#217624 = CARTESIAN_POINT ( 'NONE',  ( 20.51284917709620359, 10.31088662284490631, -7.672473185591987210 ) ) ;
#217626 = EDGE_LOOP ( 'NONE', ( #98263, #234395, #49804, #103257 ) ) ;
#217627 = DIRECTION ( 'NONE',  ( 1.000000000000000000, 0.000000000000000000, 0.000000000000000000 ) ) ;
#217628 = ORIENTED_EDGE ( 'NONE', *, *, #218422, .T. ) ;
#217629 = CARTESIAN_POINT ( 'NONE',  ( -23.15000000000000213, -8.999999999988844479, -124.7060308773475867 ) ) ;
#217630 = ORIENTED_EDGE ( 'NONE', *, *, #153670, .T. ) ;
#217631 = VERTEX_POINT ( 'NONE', #168892 ) ;
#217632 = DIRECTION ( 'NONE',  ( 1.000000000000000000, 0.000000000000000000, 0.000000000000000000 ) ) ;
#217634 = AXIS2_PLACEMENT_3D ( 'NONE', #110155, #209255, #14929 ) ;
#217633 = CARTESIAN_POINT ( 'NONE',  ( -23.15000000000000213, 85.00000000001232081, -160.6291383618718385 ) ) ;
#217635 = DIRECTION ( 'NONE',  ( 0.000000000000000000, 0.000000000000000000, 1.000000000000000000 ) ) ;
#217636 = AXIS2_PLACEMENT_3D ( 'NONE', #112039, #173335, #54606 ) ;
#217637 = DIRECTION ( 'NONE',  ( 0.000000000000000000, -1.000000000000000000, -6.938893903907222067E-15 ) ) ;
#217638 = DIRECTION ( 'NONE',  ( 0.000000000000000000, -0.2617529984165031243, -0.9651348961777157509 ) ) ;
#217639 = ORIENTED_EDGE ( 'NONE', *, *, #190076, .F. ) ;
#217640 = ORIENTED_EDGE ( 'NONE', *, *, #164172, .F. ) ;
#217641 = DIRECTION ( 'NONE',  ( 0.000000000000000000, -1.000000000000000000, 0.000000000000000000 ) ) ;
#217642 = VECTOR ( 'NONE', #200821, 1000.000000000000000 ) ;
#217643 = LINE ( 'NONE', #117293, #173972 ) ;
#217644 = ORIENTED_EDGE ( 'NONE', *, *, #128742, .F. ) ;
#217645 = DIRECTION ( 'NONE',  ( 1.000000000000000000, 0.000000000000000000, 0.000000000000000000 ) ) ;
#217646 = DIRECTION ( 'NONE',  ( -4.239556034732056743E-17, -0.1298341882519953583, -0.9915357197604862671 ) ) ;
#217647 = DIRECTION ( 'NONE',  ( 1.000000000000000000, -0.000000000000000000, -0.000000000000000000 ) ) ;
#217648 = DIRECTION ( 'NONE',  ( 1.000000000000000000, -0.000000000000000000, -0.000000000000000000 ) ) ;
#217649 = CARTESIAN_POINT ( 'NONE',  ( 20.94999999999999574, 74.16465844978787914, -158.4679561919613775 ) ) ;
#217651 = EDGE_CURVE ( 'NONE', #168386, #30609, #205821, .T. ) ;
#217650 = DIRECTION ( 'NONE',  ( 1.000000000000000000, -0.000000000000000000, 0.000000000000000000 ) ) ;
#217652 = AXIS2_PLACEMENT_3D ( 'NONE', #251040, #16321, #116676 ) ;
#217655 = CARTESIAN_POINT ( 'NONE',  ( -20.94999999999999929, 11.65000000000000036, -7.014805770654001016 ) ) ;
#217654 = TOROIDAL_SURFACE ( 'NONE', #1361, 11.65000000000000036, 0.1000000000000000056 ) ;
#217653 = CARTESIAN_POINT ( 'NONE',  ( -20.64999999999999858, 68.75000000001185185, -90.77310748452435973 ) ) ;
#217657 = DIRECTION ( 'NONE',  ( 1.000000000000000000, 0.000000000000000000, 0.000000000000000000 ) ) ;
#217656 = VECTOR ( 'NONE', #249199, 1000.000000000000000 ) ;
#217658 = VECTOR ( 'NONE', #112840, 1000.000000000000000 ) ;
#217659 = PLANE ( 'NONE',  #129190 ) ;
#217661 = ORIENTED_EDGE ( 'NONE', *, *, #210810, .T. ) ;
#217660 = DIRECTION ( 'NONE',  ( 1.000000000000000000, 0.000000000000000000, 0.000000000000000000 ) ) ;
#217662 = ADVANCED_FACE ( 'NONE', ( #67183 ), #11061, .T. ) ;
#217663 = CARTESIAN_POINT ( 'NONE',  ( -23.15000000000000213, 11.65000000001115588, -88.35000000000003695 ) ) ;
#217664 = ORIENTED_EDGE ( 'NONE', *, *, #88853, .T. ) ;
#217665 = EDGE_CURVE ( 'NONE', #24108, #189878, #176791, .T. ) ;
#217666 = CARTESIAN_POINT ( 'NONE',  ( 18.50000000000000000, 85.40000000001208491, -129.2258477248609267 ) ) ;
#217667 = CARTESIAN_POINT ( 'NONE',  ( -1.739115166359751801E-14, 64.35000000001181775, -81.67310748452439384 ) ) ;
#217668 = CARTESIAN_POINT ( 'NONE',  ( 22.50497660315938120, 64.23170377028679923, -247.2158688254707215 ) ) ;
#217669 = VERTEX_POINT ( 'NONE', #8502 ) ;
#217670 = DIRECTION ( 'NONE',  ( 0.000000000000000000, 0.9915357197604804940, -0.1298341882520397950 ) ) ;
#217671 = ADVANCED_FACE ( 'NONE', ( #52743 ), #210117, .F. ) ;
#217672 = DIRECTION ( 'NONE',  ( -0.000000000000000000, -0.000000000000000000, -1.000000000000000000 ) ) ;
#217673 = DIRECTION ( 'NONE',  ( 0.000000000000000000, 1.000000000000000000, 6.982962677686266711E-15 ) ) ;
#217674 = CARTESIAN_POINT ( 'NONE',  ( 23.14999999999999503, 69.55000000001179217, -81.87310748452435405 ) ) ;
#217675 = LINE ( 'NONE', #39094, #132209 ) ;
#217676 = CARTESIAN_POINT ( 'NONE',  ( 21.05000000000000071, -8.999999999988842703, -57.60603087734755690 ) ) ;
#217677 = ORIENTED_EDGE ( 'NONE', *, *, #155352, .T. ) ;
#217678 = CARTESIAN_POINT ( 'NONE',  ( 18.59999999999999076, 1.835341550235567887, -45.05515129256298223 ) ) ;
#217680 = ORIENTED_EDGE ( 'NONE', *, *, #221798, .F. ) ;
#217679 = CARTESIAN_POINT ( 'NONE',  ( -21.05000000000000071, 1.736257131597397585, -11.56865232901749962 ) ) ;
#217681 = CARTESIAN_POINT ( 'NONE',  ( -20.64999999999999858, 69.05648948627110428, -235.0374527038057977 ) ) ;
#217682 = CIRCLE ( 'NONE', #105228, 0.09999999999999939493 ) ;
#217683 = EDGE_CURVE ( 'NONE', #253923, #76080, #118540, .T. ) ;
#217684 = DIRECTION ( 'NONE',  ( 0.000000000000000000, 0.9651348961777157509, -0.2617529984165031243 ) ) ;
#217685 = DIRECTION ( 'NONE',  ( 0.000000000000000000, 0.2617529984165152257, 0.9651348961777124202 ) ) ;
#217686 =( BOUNDED_CURVE ( )  B_SPLINE_CURVE ( 3, ( #69342, #28966, #189281, #19633 ),
 .UNSPECIFIED., .F., .F. ) 
 B_SPLINE_CURVE_WITH_KNOTS ( ( 4, 4 ),
 ( 0.06456096931748350753, 3.077031684272309775 ),
 .UNSPECIFIED. ) 
 CURVE ( )  GEOMETRIC_REPRESENTATION_ITEM ( )  RATIONAL_B_SPLINE_CURVE ( ( 1.000000000000000000, 0.3763440860215095940, 0.3763440860215095940, 1.000000000000000000 ) ) 
 REPRESENTATION_ITEM ( '' )  );
#217687 = ORIENTED_EDGE ( 'NONE', *, *, #251274, .T. ) ;
#217688 = DIRECTION ( 'NONE',  ( 0.000000000000000000, 0.8009761297185381546, -0.5986962832865355688 ) ) ;
#217689 = VECTOR ( 'NONE', #73721, 1000.000000000000000 ) ;
#217690 = EDGE_CURVE ( 'NONE', #140929, #32310, #247692, .T. ) ;
#217691 = SHAPE_DEFINITION_REPRESENTATION ( #242846, #141939 ) ;
#217692 = EDGE_CURVE ( 'NONE', #41172, #128036, #51858, .T. ) ;
#217694 = AXIS2_PLACEMENT_3D ( 'NONE', #168184, #9061, #127740 ) ;
#217693 = CARTESIAN_POINT ( 'NONE',  ( -18.54159361262954775, 85.46313213550493515, -95.97398526823127440 ) ) ;
#217695 = VERTEX_POINT ( 'NONE', #30648 ) ;
#217696 = VECTOR ( 'NONE', #157649, 1000.000000000000000 ) ;
#217697 = CARTESIAN_POINT ( 'NONE',  ( 20.85000000000000142, 74.44087353924872730, -232.6253149859214773 ) ) ;
#217698 = CARTESIAN_POINT ( 'NONE',  ( 16.87683809663750267, 22.97806745954241592, -230.9350634111226270 ) ) ;
#217699 = AXIS2_PLACEMENT_3D ( 'NONE', #11724, #185206, #87368 ) ;
#217700 = B_SPLINE_CURVE_WITH_KNOTS ( 'NONE', 3,
 ( #144839, #4052, #224379, #108303, #24930, #86130, #125297, #105693, #242660, #66607 ),
 .UNSPECIFIED., .F., .F.,
 ( 4, 2, 2, 2, 4 ),
 ( 0.000000000000000000, 0.0001584437871625043689, 0.0002376656807437589386, 0.0002772766275343880801, 0.0003168875743250173030 ),
 .UNSPECIFIED. ) ;
#217701 = AXIS2_PLACEMENT_3D ( 'NONE', #226457, #246056, #123538 ) ;
#217702 = EDGE_CURVE ( 'NONE', #70602, #114510, #205404, .T. ) ;
#217703 = CARTESIAN_POINT ( 'NONE',  ( -22.50000000000000000, 1.115600667400684642E-11, -167.4999999999999716 ) ) ;
#217704 = ORIENTED_EDGE ( 'NONE', *, *, #64401, .T. ) ;
#217705 = ORIENTED_EDGE ( 'NONE', *, *, #204674, .F. ) ;
#217706 = EDGE_CURVE ( 'NONE', #17556, #188870, #85152, .T. ) ;
#217707 = CARTESIAN_POINT ( 'NONE',  ( -22.39999999999999858, 76.10085836911075319, -114.7726746080137019 ) ) ;
#217708 = EDGE_CURVE ( 'NONE', #26810, #34583, #230103, .T. ) ;
#217710 = AXIS2_PLACEMENT_3D ( 'NONE', #224715, #164764, #223432 ) ;
#217709 = DIRECTION ( 'NONE',  ( -1.000000000000000000, 0.000000000000000000, 0.000000000000000000 ) ) ;
#217712 = CIRCLE ( 'NONE', #184411, 0.1000000000000002554 ) ;
#217711 = CARTESIAN_POINT ( 'NONE',  ( -21.05000000000000071, 1.115650877919449575E-11, -171.6000000000000227 ) ) ;
#217713 = DIRECTION ( 'NONE',  ( -1.000000000000000000, -0.000000000000000000, -0.000000000000000000 ) ) ;
#217714 = DIRECTION ( 'NONE',  ( 1.000000000000000000, -0.000000000000000000, -0.000000000000000000 ) ) ;
#217716 = DIRECTION ( 'NONE',  ( 0.000000000000000000, 0.000000000000000000, -1.000000000000000000 ) ) ;
#217715 = DIRECTION ( 'NONE',  ( 2.952720810173288619E-16, -1.000000000000000000, 0.000000000000000000 ) ) ;
#217717 = VECTOR ( 'NONE', #230065, 1000.000000000000000 ) ;
#217718 = CARTESIAN_POINT ( 'NONE',  ( 20.93302460841142931, 65.68434038414308418, -30.48668807260656521 ) ) ;
#217719 = CARTESIAN_POINT ( 'NONE',  ( 23.14999999999999858, 76.00000000001213607, -136.5231074845243313 ) ) ;
#217720 = FACE_OUTER_BOUND ( 'NONE', #142184, .T. ) ;
#217721 = FACE_OUTER_BOUND ( 'NONE', #217928, .T. ) ;
#217722 = ORIENTED_EDGE ( 'NONE', *, *, #21382, .T. ) ;
#217723 = ORIENTED_EDGE ( 'NONE', *, *, #148433, .T. ) ;
#217724 = CIRCLE ( 'NONE', #151120, 0.09999999999999363565 ) ;
#217725 = LINE ( 'NONE', #116093, #140972 ) ;
#217727 = DIRECTION ( 'NONE',  ( -0.000000000000000000, 7.272083257015735086E-15, -1.000000000000000000 ) ) ;
#217726 = CARTESIAN_POINT ( 'NONE',  ( 21.10320863425824811, 69.59972261355248691, -69.54812973575150181 ) ) ;
#217729 =( BOUNDED_CURVE ( )  B_SPLINE_CURVE ( 3, ( #73884, #52990, #112981, #30906 ),
 .UNSPECIFIED., .F., .F. ) 
 B_SPLINE_CURVE_WITH_KNOTS ( ( 4, 4 ),
 ( 1.570796326794901665, 3.141592653589768247 ),
 .UNSPECIFIED. ) 
 CURVE ( )  GEOMETRIC_REPRESENTATION_ITEM ( )  RATIONAL_B_SPLINE_CURVE ( ( 1.000000000000000000, 0.8047378541243720429, 0.8047378541243720429, 1.000000000000000000 ) ) 
 REPRESENTATION_ITEM ( '' )  );
#217728 = CIRCLE ( 'NONE', #105272, 12.77499999999999147 ) ;
#217730 = AXIS2_PLACEMENT_3D ( 'NONE', #204977, #208857, #48488 ) ;
#217731 = CIRCLE ( 'NONE', #163774, 0.5000000000000001110 ) ;
#217732 = EDGE_CURVE ( 'NONE', #166897, #209494, #101912, .T. ) ;
#217733 = CARTESIAN_POINT ( 'NONE',  ( -20.54999999999999716, 48.89266972451527948, -253.5637804087949121 ) ) ;
#217735 = EDGE_CURVE ( 'NONE', #78259, #4064, #31077, .T. ) ;
#217734 = DIRECTION ( 'NONE',  ( 1.000000000000000000, 1.541880601228652843E-16, 2.878400969107353907E-16 ) ) ;
#217736 = DIRECTION ( 'NONE',  ( 0.000000000000000000, 1.000000000000000000, 0.000000000000000000 ) ) ;
#217737 = ORIENTED_EDGE ( 'NONE', *, *, #182945, .F. ) ;
#217738 = EDGE_LOOP ( 'NONE', ( #196945, #206708, #175594, #61794 ) ) ;
#217739 = DIRECTION ( 'NONE',  ( 0.000000000000000000, 0.000000000000000000, 1.000000000000000000 ) ) ;
#217740 = ORIENTED_EDGE ( 'NONE', *, *, #188597, .F. ) ;
#217741 = DIRECTION ( 'NONE',  ( 0.000000000000000000, 0.000000000000000000, -1.000000000000000000 ) ) ;
#217742 = VECTOR ( 'NONE', #16783, 999.9999999999998863 ) ;
#217743 = CIRCLE ( 'NONE', #13759, 0.09999999999999134581 ) ;
#217744 = ORIENTED_EDGE ( 'NONE', *, *, #154628, .F. ) ;
#217745 = CARTESIAN_POINT ( 'NONE',  ( -21.05000000000000071, 40.58313652815211015, -247.7931640254992658 ) ) ;
#217746 = ORIENTED_EDGE ( 'NONE', *, *, #73844, .T. ) ;
#217747 = CARTESIAN_POINT ( 'NONE',  ( -20.85000000000000142, 6.933893972137497030, -137.7856458343736108 ) ) ;
#217748 = DIRECTION ( 'NONE',  ( -0.000000000000000000, -0.1350103645451876666, 0.9908441862701600211 ) ) ;
#217749 = CARTESIAN_POINT ( 'NONE',  ( 23.24999999999999645, 67.17743825834588733, -157.3731074845244109 ) ) ;
#217750 = ADVANCED_FACE ( 'NONE', ( #235238 ), #213105, .T. ) ;
#217751 = CARTESIAN_POINT ( 'NONE',  ( -18.50000000000000000, 77.35494420175976416, -241.6200040285045532 ) ) ;
#217752 = DIRECTION ( 'NONE',  ( 1.000000000000000000, 0.000000000000000000, 0.000000000000000000 ) ) ;
#217753 = DIRECTION ( 'NONE',  ( 0.000000000000000000, 0.000000000000000000, -1.000000000000000000 ) ) ;
#217754 = CARTESIAN_POINT ( 'NONE',  ( -15.55912972643741199, 67.50912972644950116, -123.9731074845243626 ) ) ;
#217755 = ADVANCED_FACE ( 'NONE', ( #14928 ), #39644, .T. ) ;
#217756 = ORIENTED_EDGE ( 'NONE', *, *, #209354, .T. ) ;
#217757 = CIRCLE ( 'NONE', #200655, 0.09999999999999939493 ) ;
#217759 = DIRECTION ( 'NONE',  ( 1.000000000000000000, -0.000000000000000000, -0.000000000000000000 ) ) ;
#217758 = CARTESIAN_POINT ( 'NONE',  ( 21.30000000000002558, 76.00000000001162448, -65.47310748452431994 ) ) ;
#217760 = ORIENTED_EDGE ( 'NONE', *, *, #8710, .F. ) ;
#217762 = ORIENTED_EDGE ( 'NONE', *, *, #37578, .T. ) ;
#217761 = CARTESIAN_POINT ( 'NONE',  ( 22.39999999999999503, 68.20922040163827660, -69.52310748452437394 ) ) ;
#217763 = VERTEX_POINT ( 'NONE', #76157 ) ;
#217764 = DIRECTION ( 'NONE',  ( -1.000000000000000000, 0.000000000000000000, 0.000000000000000000 ) ) ;
#217765 = CARTESIAN_POINT ( 'NONE',  ( -21.05000000000000071, -11.48912529307605901, -3.100000000000000533 ) ) ;
#217766 = EDGE_CURVE ( 'NONE', #55645, #109188, #168641, .T. ) ;
#217767 = CARTESIAN_POINT ( 'NONE',  ( -18.41431012584568450, 20.68648449445280235, -227.9633614482561370 ) ) ;
#217768 = CIRCLE ( 'NONE', #22181, 0.1000000000000028644 ) ;
#217769 = ORIENTED_EDGE ( 'NONE', *, *, #45737, .F. ) ;
#217770 = EDGE_CURVE ( 'NONE', #222470, #70015, #151862, .T. ) ;
#217771 = LINE ( 'NONE', #97814, #142172 ) ;
#217772 = CARTESIAN_POINT ( 'NONE',  ( -18.35663730107557257, 40.40958672937900076, -235.2982477752999273 ) ) ;
#217773 = CARTESIAN_POINT ( 'NONE',  ( -18.59999999999999787, 85.48068669529035901, -29.08199231576641353 ) ) ;
#217774 = ADVANCED_FACE ( 'NONE', ( #54033 ), #18563, .T. ) ;
#217775 = ORIENTED_EDGE ( 'NONE', *, *, #46308, .F. ) ;
#217776 = CYLINDRICAL_SURFACE ( 'NONE', #244134, 0.09999999999999156786 ) ;
#217777 = LINE ( 'NONE', #155296, #251724 ) ;
#217778 = EDGE_LOOP ( 'NONE', ( #142029, #78075, #182576, #71060 ) ) ;
#217779 = VERTEX_POINT ( 'NONE', #158312 ) ;
#217780 = CARTESIAN_POINT ( 'NONE',  ( -12.25000000000000178, 9.350000000011139178, -83.75000000000004263 ) ) ;
#217781 = ADVANCED_FACE ( 'NONE', ( #16222 ), #73633, .T. ) ;
#217782 = TOROIDAL_SURFACE ( 'NONE', #38749, 4.041421356237310469, 0.1000000000000000056 ) ;
#217783 = ORIENTED_EDGE ( 'NONE', *, *, #58822, .F. ) ;
#217784 = CARTESIAN_POINT ( 'NONE',  ( -16.91256925476570672, 9.985731158128174911, -12.53235751099471962 ) ) ;
#217786 = ADVANCED_FACE ( 'NONE', ( #176573 ), #237814, .T. ) ;
#217785 = ORIENTED_EDGE ( 'NONE', *, *, #181744, .F. ) ;
#217787 = LINE ( 'NONE', #82119, #100907 ) ;
#217788 = CARTESIAN_POINT ( 'NONE',  ( -18.59999999999999787, -1.164121893241208960, -41.41484808557160591 ) ) ;
#217789 = DIRECTION ( 'NONE',  ( 1.000000000000000000, 2.952720810173289112E-16, -0.000000000000000000 ) ) ;
#217790 = EDGE_CURVE ( 'NONE', #145739, #245180, #126319, .T. ) ;
#217791 = CARTESIAN_POINT ( 'NONE',  ( 20.95443524775735256, 60.89599939867935063, -225.2949451438352355 ) ) ;
#217792 = CARTESIAN_POINT ( 'NONE',  ( -16.89268316805465986, 66.04827818676963602, -82.16735500597883401 ) ) ;
#217793 = LINE ( 'NONE', #1320, #123928 ) ;
#217794 = CARTESIAN_POINT ( 'NONE',  ( -23.25000000000000000, 1.910280373842936141, -146.6313678551989597 ) ) ;
#217796 = ORIENTED_EDGE ( 'NONE', *, *, #138318, .F. ) ;
#217795 = ADVANCED_FACE ( 'NONE', ( #218219 ), #119156, .T. ) ;
#217799 = EDGE_CURVE ( 'NONE', #188486, #72511, #39437, .T. ) ;
#217798 = DIRECTION ( 'NONE',  ( -1.000000000000000000, 0.000000000000000000, 0.000000000000000000 ) ) ;
#217797 = LINE ( 'NONE', #163007, #241376 ) ;
#217801 = ORIENTED_EDGE ( 'NONE', *, *, #74067, .T. ) ;
#217800 = AXIS2_PLACEMENT_3D ( 'NONE', #196624, #96237, #76675 ) ;
#217804 = ORIENTED_EDGE ( 'NONE', *, *, #188874, .T. ) ;
#217803 = CARTESIAN_POINT ( 'NONE',  ( 18.59999999999999076, 10.20857864377385127, -88.35000000000003695 ) ) ;
#217802 = LINE ( 'NONE', #178739, #248895 ) ;
#217805 = ORIENTED_EDGE ( 'NONE', *, *, #241570, .F. ) ;
#217806 = CARTESIAN_POINT ( 'NONE',  ( 22.60000000000000142, 76.00000000001237765, -170.0231074845243597 ) ) ;
#217807 = CARTESIAN_POINT ( 'NONE',  ( 21.05000000000000071, 0.09843750001147391626, -60.70076908990778009 ) ) ;
#217809 = FACE_BOUND ( 'NONE', #144160, .T. ) ;
#217808 = AXIS2_PLACEMENT_3D ( 'NONE', #205465, #26872, #32994 ) ;
#217810 = ADVANCED_FACE ( 'NONE', ( #116583 ), #93155, .F. ) ;
#217811 = CARTESIAN_POINT ( 'NONE',  ( -20.94999999999999929, 64.40000000001209912, -129.5949042542488314 ) ) ;
#217812 = ORIENTED_EDGE ( 'NONE', *, *, #31721, .T. ) ;
#217813 = FACE_BOUND ( 'NONE', #117210, .T. ) ;
#217814 = CARTESIAN_POINT ( 'NONE',  ( -21.05000000000000071, -9.519327731081284938, -40.47297637655933755 ) ) ;
#217815 = EDGE_CURVE ( 'NONE', #68201, #127037, #55283, .T. ) ;
#217817 = CYLINDRICAL_SURFACE ( 'NONE', #146593, 0.1000000000000000472 ) ;
#217816 = CARTESIAN_POINT ( 'NONE',  ( 18.69999999999999929, -8.250000000000005329, -15.00000000000000000 ) ) ;
#217818 = EDGE_CURVE ( 'NONE', #97895, #215594, #81077, .T. ) ;
#217820 = ORIENTED_EDGE ( 'NONE', *, *, #120981, .F. ) ;
#217819 = CARTESIAN_POINT ( 'NONE',  ( -16.93935632781549572, 9.984730499736244269, -54.38966074871030543 ) ) ;
#217821 = VECTOR ( 'NONE', #192934, 1000.000000000000000 ) ;
#217822 = VECTOR ( 'NONE', #38594, 1000.000000000000000 ) ;
#217823 = ORIENTED_EDGE ( 'NONE', *, *, #200492, .F. ) ;
#217824 = LINE ( 'NONE', #36681, #238891 ) ;
#217825 = ORIENTED_EDGE ( 'NONE', *, *, #49097, .T. ) ;
#217826 = CARTESIAN_POINT ( 'NONE',  ( -22.50000000000000000, 11.65000000001113278, -67.00000000000004263 ) ) ;
#217827 = ORIENTED_EDGE ( 'NONE', *, *, #228776, .T. ) ;
#217828 = AXIS2_PLACEMENT_3D ( 'NONE', #133922, #114370, #195219 ) ;
#217830 = ADVANCED_FACE ( 'NONE', ( #163418 ), #106011, .F. ) ;
#217829 = DIRECTION ( 'NONE',  ( 1.000000000000000000, 0.000000000000000000, 0.000000000000000000 ) ) ;
#217831 = DIRECTION ( 'NONE',  ( 0.000000000000000000, 0.000000000000000000, 1.000000000000000000 ) ) ;
#217832 = EDGE_LOOP ( 'NONE', ( #199324, #41867, #8143, #184904 ) ) ;
#217833 = CARTESIAN_POINT ( 'NONE',  ( -21.65000000000000213, 9.949999999999985079, -20.75000000000000000 ) ) ;
#217834 = VECTOR ( 'NONE', #209062, 1000.000000000000000 ) ;
#217835 = TOROIDAL_SURFACE ( 'NONE', #51228, 0.4000000000000003553, 0.1000000000000000056 ) ;
#217836 = CIRCLE ( 'NONE', #134448, 0.09999999999999939493 ) ;
#217837 = CIRCLE ( 'NONE', #226194, 0.09999999999999939493 ) ;
#217838 = EDGE_CURVE ( 'NONE', #102301, #145985, #159650, .T. ) ;
#217839 = DIRECTION ( 'NONE',  ( -1.000000000000000000, -0.000000000000000000, -0.000000000000000000 ) ) ;
#217840 = ORIENTED_EDGE ( 'NONE', *, *, #220977, .T. ) ;
#217841 = ORIENTED_EDGE ( 'NONE', *, *, #211005, .F. ) ;
#217842 = VERTEX_POINT ( 'NONE', #22639 ) ;
#217843 = CARTESIAN_POINT ( 'NONE',  ( -21.44999999999999929, 68.65000000001222702, -148.8731074845244109 ) ) ;
#217844 = ADVANCED_FACE ( 'NONE', ( #240387 ), #222064, .F. ) ;
#217845 = VERTEX_POINT ( 'NONE', #64311 ) ;
#217847 = VERTEX_POINT ( 'NONE', #121736 ) ;
#217846 = LINE ( 'NONE', #3956, #84409 ) ;
#217848 = ORIENTED_EDGE ( 'NONE', *, *, #186666, .T. ) ;
#217851 = ORIENTED_EDGE ( 'NONE', *, *, #107060, .F. ) ;
#217850 = ORIENTED_EDGE ( 'NONE', *, *, #152647, .T. ) ;
#217849 = DIRECTION ( 'NONE',  ( 0.000000000000000000, -1.000000000000000000, -0.000000000000000000 ) ) ;
#217852 = CIRCLE ( 'NONE', #126292, 0.1000000000000011990 ) ;
#217853 = CIRCLE ( 'NONE', #109538, 0.1000000000000013933 ) ;
#217854 = ORIENTED_EDGE ( 'NONE', *, *, #212999, .T. ) ;
#217855 = CARTESIAN_POINT ( 'NONE',  ( -21.05000000000000071, 4.272272088314018390, -245.4186996786394843 ) ) ;
#217856 = ADVANCED_FACE ( 'NONE', ( #23929 ), #223367, .F. ) ;
#217857 = DIRECTION ( 'NONE',  ( -1.000000000000000000, 0.000000000000000000, 0.000000000000000000 ) ) ;
#217858 = DIRECTION ( 'NONE',  ( 0.000000000000000000, 0.3738317757009942399, -0.9274965247785252886 ) ) ;
#217859 = ORIENTED_EDGE ( 'NONE', *, *, #150823, .F. ) ;
#217860 = VECTOR ( 'NONE', #248354, 1000.000000000000000 ) ;
#217861 = DIRECTION ( 'NONE',  ( 0.000000000000000000, 0.1298341882520022972, 0.9915357197604853789 ) ) ;
#217862 = CIRCLE ( 'NONE', #238555, 3.999999999999996447 ) ;
#217864 = EDGE_LOOP ( 'NONE', ( #228394, #119010, #178219, #64934 ) ) ;
#217863 = DIRECTION ( 'NONE',  ( -6.938893903907222856E-15, 0.9770955615653313941, 0.2128009952263603677 ) ) ;
#217865 = DIRECTION ( 'NONE',  ( -1.000000000000000000, 0.000000000000000000, 0.000000000000000000 ) ) ;
#217867 = ORIENTED_EDGE ( 'NONE', *, *, #238325, .T. ) ;
#217866 = CARTESIAN_POINT ( 'NONE',  ( -16.87683809663752399, 42.27269979661959098, -221.1123729563994402 ) ) ;
#217868 = EDGE_LOOP ( 'NONE', ( #91805, #218472, #127502, #217095, #198461 ) ) ;
#217869 = AXIS2_PLACEMENT_3D ( 'NONE', #31415, #88757, #246558 ) ;
#217870 = FACE_OUTER_BOUND ( 'NONE', #219365, .T. ) ;
#217871 = DIRECTION ( 'NONE',  ( 0.000000000000000000, 0.000000000000000000, -1.000000000000000000 ) ) ;
#217872 = AXIS2_PLACEMENT_3D ( 'NONE', #29327, #205330, #26741 ) ;
#217873 = AXIS2_PLACEMENT_3D ( 'NONE', #109825, #5574, #188097 ) ;
#217875 = VERTEX_POINT ( 'NONE', #83824 ) ;
#217874 = CIRCLE ( 'NONE', #17975, 0.09999999999998898659 ) ;
#217876 = ORIENTED_EDGE ( 'NONE', *, *, #8912, .F. ) ;
#217877 = DIRECTION ( 'NONE',  ( -1.000000000000000000, -0.000000000000000000, -0.000000000000000000 ) ) ;
#217878 = CARTESIAN_POINT ( 'NONE',  ( -21.05000000000000071, 0.09779029131994597390, -161.2421853895238542 ) ) ;
#217879 = VECTOR ( 'NONE', #107505, 1000.000000000000000 ) ;
#217881 = ORIENTED_EDGE ( 'NONE', *, *, #144461, .F. ) ;
#217880 = ORIENTED_EDGE ( 'NONE', *, *, #255652, .F. ) ;
#217882 = ORIENTED_EDGE ( 'NONE', *, *, #246602, .F. ) ;
#217883 = CARTESIAN_POINT ( 'NONE',  ( -23.15000000000000213, -11.64999999998884483, -97.40000000000004832 ) ) ;
#217884 = ORIENTED_EDGE ( 'NONE', *, *, #114051, .T. ) ;
#217885 = ORIENTED_EDGE ( 'NONE', *, *, #58020, .F. ) ;
#217886 = CARTESIAN_POINT ( 'NONE',  ( 20.95289811251229750, 18.82242866597310282, -229.9079097911970280 ) ) ;
#217887 = VERTEX_POINT ( 'NONE', #201241 ) ;
#217888 = DIRECTION ( 'NONE',  ( 0.000000000000000000, 6.938893903907222067E-15, -1.000000000000000000 ) ) ;
#217889 = VECTOR ( 'NONE', #142310, 1000.000000000000000 ) ;
#217891 = CARTESIAN_POINT ( 'NONE',  ( -1.820710678118657944, 85.92928932189282420, -44.77310748452425315 ) ) ;
#217890 = DIRECTION ( 'NONE',  ( 1.000000000000000000, 0.000000000000000000, 0.000000000000000000 ) ) ;
#217893 = ORIENTED_EDGE ( 'NONE', *, *, #93580, .T. ) ;
#217892 = VECTOR ( 'NONE', #166528, 1000.000000000000000 ) ;
#217894 = ADVANCED_FACE ( 'NONE', ( #61743 ), #60238, .T. ) ;
#217896 = ORIENTED_EDGE ( 'NONE', *, *, #218552, .T. ) ;
#217895 = ORIENTED_EDGE ( 'NONE', *, *, #127185, .F. ) ;
#217897 = DIRECTION ( 'NONE',  ( 0.000000000000000000, 0.000000000000000000, -1.000000000000000000 ) ) ;
#217898 = DIRECTION ( 'NONE',  ( 0.000000000000000000, 0.000000000000000000, -1.000000000000000000 ) ) ;
#217899 = EDGE_LOOP ( 'NONE', ( #17008, #90913, #138349, #223909 ) ) ;
#217900 = AXIS2_PLACEMENT_3D ( 'NONE', #47894, #27096, #85708 ) ;
#217901 = CIRCLE ( 'NONE', #155426, 7.799999999999997158 ) ;
#217902 = ORIENTED_EDGE ( 'NONE', *, *, #122780, .T. ) ;
#217903 = ORIENTED_EDGE ( 'NONE', *, *, #144131, .F. ) ;
#217904 = ADVANCED_FACE ( 'NONE', ( #181696 ), #242938, .F. ) ;
#217905 = DIRECTION ( 'NONE',  ( 0.000000000000000000, 0.000000000000000000, -1.000000000000000000 ) ) ;
#217906 = ORIENTED_EDGE ( 'NONE', *, *, #22545, .F. ) ;
#217907 = CARTESIAN_POINT ( 'NONE',  ( -20.54999999999999716, 36.65892442174935439, -249.5511627012433848 ) ) ;
#217908 = CARTESIAN_POINT ( 'NONE',  ( 22.39999999999999503, 0.1000000000111554016, -92.70922040162665212 ) ) ;
#217909 = VERTEX_POINT ( 'NONE', #219518 ) ;
#217910 = DIRECTION ( 'NONE',  ( 0.7071067811865475727, 0.7071067811865475727, -0.000000000000000000 ) ) ;
#217911 = CARTESIAN_POINT ( 'NONE',  ( 18.52351027002947248, 85.64216290470727699, -129.8080605340145439 ) ) ;
#217913 = CARTESIAN_POINT ( 'NONE',  ( -16.97683810757273193, 9.950000000011137047, -120.7364232875395942 ) ) ;
#217912 = CARTESIAN_POINT ( 'NONE',  ( -33.80000000000000426, 3.175288713399618601, 33.00000000000000000 ) ) ;
#217914 = ADVANCED_FACE ( 'NONE', ( #103409 ), #139337, .T. ) ;
#217915 = DIRECTION ( 'NONE',  ( 1.000000000000000000, 0.000000000000000000, 0.000000000000000000 ) ) ;
#217916 = CARTESIAN_POINT ( 'NONE',  ( 18.49999999999999645, 77.83534155023700407, -191.9679561919613491 ) ) ;
#217917 = CARTESIAN_POINT ( 'NONE',  ( 21.10642757222115407, 65.27684371085369719, -157.7824099607392156 ) ) ;
#217918 = LINE ( 'NONE', #116294, #69511 ) ;
#217919 = CARTESIAN_POINT ( 'NONE',  ( 18.46921299892753865, -9.509378177812608968, -73.98657870937046255 ) ) ;
#217920 = DIRECTION ( 'NONE',  ( 1.000000000000000000, 0.000000000000000000, 0.000000000000000000 ) ) ;
#217922 = EDGE_CURVE ( 'NONE', #94361, #206526, #143453, .T. ) ;
#217921 = AXIS2_PLACEMENT_3D ( 'NONE', #195422, #114582, #153762 ) ;
#217924 = EDGE_LOOP ( 'NONE', ( #175513, #59394, #137841, #192836, #45751 ) ) ;
#217923 = VECTOR ( 'NONE', #138865, 1000.000000000000000 ) ;
#217925 = AXIS2_PLACEMENT_3D ( 'NONE', #183530, #238356, #119714 ) ;
#217926 = VECTOR ( 'NONE', #76451, 1000.000000000000000 ) ;
#217927 = ADVANCED_FACE ( 'NONE', ( #82551 ), #81274, .F. ) ;
#217929 = VERTEX_POINT ( 'NONE', #162147 ) ;
#217928 = EDGE_LOOP ( 'NONE', ( #198031, #141643, #128170, #92466 ) ) ;
#217930 = ORIENTED_EDGE ( 'NONE', *, *, #137092, .T. ) ;
#217931 = ORIENTED_EDGE ( 'NONE', *, *, #183866, .T. ) ;
#217932 = EDGE_CURVE ( 'NONE', #208514, #32089, #42191, .T. ) ;
#217933 = DIRECTION ( 'NONE',  ( -1.000000000000000000, 0.000000000000000000, 0.000000000000000000 ) ) ;
#217934 = CARTESIAN_POINT ( 'NONE',  ( -23.25000000000000000, 4.349999999999999645, -12.25000000000000000 ) ) ;
#217935 = EDGE_CURVE ( 'NONE', #217887, #163256, #202534, .T. ) ;
#217937 = FACE_OUTER_BOUND ( 'NONE', #228473, .T. ) ;
#217936 = CARTESIAN_POINT ( 'NONE',  ( 20.94999999999999929, -4.161311414658873886, -226.0656773515597706 ) ) ;
#217938 = ORIENTED_EDGE ( 'NONE', *, *, #43825, .F. ) ;
#217939 = DIRECTION ( 'NONE',  ( 0.000000000000000000, 1.000000000000000000, 0.000000000000000000 ) ) ;
#217940 = DIRECTION ( 'NONE',  ( -1.000000000000000000, -0.000000000000000000, -0.000000000000000000 ) ) ;
#217941 = ADVANCED_FACE ( 'NONE', ( #5589 ), #181076, .T. ) ;
#217942 = CARTESIAN_POINT ( 'NONE',  ( 21.13736287352038445, 8.046642376395153562, -113.1500000000000483 ) ) ;
#217943 = CARTESIAN_POINT ( 'NONE',  ( 18.41416235934318735, -9.499999999988846255, -73.60018939122205950 ) ) ;
#217944 = VERTEX_POINT ( 'NONE', #180412 ) ;
#217945 = DIRECTION ( 'NONE',  ( 0.000000000000000000, 0.9915357197604882655, -0.1298341882519793711 ) ) ;
#217946 = AXIS2_PLACEMENT_3D ( 'NONE', #14801, #173892, #245382 ) ;
#217947 = DIRECTION ( 'NONE',  ( 0.000000000000000000, -6.982962677686266711E-15, 1.000000000000000000 ) ) ;
#217948 = ORIENTED_EDGE ( 'NONE', *, *, #156553, .F. ) ;
#217949 = CARTESIAN_POINT ( 'NONE',  ( -20.64999999999999858, 63.44052078637213299, -222.1345147897817185 ) ) ;
#217950 = CARTESIAN_POINT ( 'NONE',  ( -18.40000000000000213, 64.51332499825421962, -93.77310748452438816 ) ) ;
#217951 = DIRECTION ( 'NONE',  ( 4.504528286903032433E-15, -0.1298341882520124002, -0.9915357197604841577 ) ) ;
#217952 = CARTESIAN_POINT ( 'NONE',  ( 21.14999999999999858, 69.35000000001156195, -57.37310748452436826 ) ) ;
#217953 = CARTESIAN_POINT ( 'NONE',  ( -18.40000000000000213, 68.12577260125452483, -210.9717008331155341 ) ) ;
#217954 = ORIENTED_EDGE ( 'NONE', *, *, #243883, .T. ) ;
#217955 = CARTESIAN_POINT ( 'NONE',  ( -20.54999999999999716, -11.74999999998884448, -150.7500000000000284 ) ) ;
#217956 = PLANE ( 'NONE',  #108999 ) ;
#217958 = EDGE_CURVE ( 'NONE', #15440, #41155, #164700, .T. ) ;
#217957 = CARTESIAN_POINT ( 'NONE',  ( 23.04999999999999716, 19.44861527341281615, -230.3234391047226666 ) ) ;
#217960 = FACE_BOUND ( 'NONE', #229211, .T. ) ;
#217959 = DIRECTION ( 'NONE',  ( 0.000000000000000000, -0.2128009952263603677, 0.9770955615653313941 ) ) ;
#217961 = CARTESIAN_POINT ( 'NONE',  ( -20.64999999999999858, 54.34471204062663219, -239.4366250215122420 ) ) ;
#217962 = FACE_OUTER_BOUND ( 'NONE', #255620, .T. ) ;
#217963 = LINE ( 'NONE', #99299, #130517 ) ;
#217964 = FACE_OUTER_BOUND ( 'NONE', #17106, .T. ) ;
#217965 = VECTOR ( 'NONE', #185456, 1000.000000000000000 ) ;
#217966 = ORIENTED_EDGE ( 'NONE', *, *, #220718, .F. ) ;
#217967 = CIRCLE ( 'NONE', #172247, 0.1000000000000028644 ) ;
#217968 = CIRCLE ( 'NONE', #38936, 0.1000000000000052097 ) ;
#217969 = ORIENTED_EDGE ( 'NONE', *, *, #60855, .F. ) ;
#217970 = ADVANCED_FACE ( 'NONE', ( #21358 ), #193164, .F. ) ;
#217971 = DIRECTION ( 'NONE',  ( -1.000000000000000000, -0.000000000000000000, -0.000000000000000000 ) ) ;
#217972 = ORIENTED_EDGE ( 'NONE', *, *, #169768, .T. ) ;
#217973 = DIRECTION ( 'NONE',  ( 1.000000000000000000, 0.000000000000000000, 0.000000000000000000 ) ) ;
#217975 = CARTESIAN_POINT ( 'NONE',  ( -18.60000000000000142, -9.321008403350132809, -174.7359382490778614 ) ) ;
#217974 = CIRCLE ( 'NONE', #147069, 11.65000000000000746 ) ;
#217976 = CARTESIAN_POINT ( 'NONE',  ( 23.14999999999999503, 64.35000000001150511, -48.17310748452440095 ) ) ;
#217977 = EDGE_LOOP ( 'NONE', ( #134203, #60419, #74408, #64350 ) ) ;
#217978 = EDGE_CURVE ( 'NONE', #158228, #227353, #147350, .T. ) ;
#217979 = CARTESIAN_POINT ( 'NONE',  ( -21.65000000000000213, 66.05000000001255955, -182.7731074845244450 ) ) ;
#217980 = CIRCLE ( 'NONE', #80606, 0.1000000000000026007 ) ;
#217981 = DIRECTION ( 'NONE',  ( 1.000000000000000000, 3.190570557967288949E-16, 6.948722487160392945E-17 ) ) ;
#217982 = LINE ( 'NONE', #160636, #115328 ) ;
#217983 = VECTOR ( 'NONE', #212434, 1000.000000000000000 ) ;
#217984 = DIRECTION ( 'NONE',  ( 0.000000000000000000, 0.000000000000000000, -1.000000000000000000 ) ) ;
#217985 = VERTEX_POINT ( 'NONE', #227228 ) ;
#217987 = CARTESIAN_POINT ( 'NONE',  ( 18.59999999999999076, 1.835341550235567887, -112.0551512925630249 ) ) ;
#217986 = CARTESIAN_POINT ( 'NONE',  ( -21.05000000000000071, 74.14897176987143723, -158.3691942151018850 ) ) ;
#217988 = DIRECTION ( 'NONE',  ( 0.000000000000000000, -2.664535259100396996E-15, 1.000000000000000000 ) ) ;
#217989 = EDGE_CURVE ( 'NONE', #213795, #200055, #97230, .T. ) ;
#217990 = DIRECTION ( 'NONE',  ( 0.000000000000000000, 0.000000000000000000, 1.000000000000000000 ) ) ;
#217991 = CARTESIAN_POINT ( 'NONE',  ( 20.94999999999999574, 1.162701749949165642, -142.1000000000000227 ) ) ;
#217992 = CARTESIAN_POINT ( 'NONE',  ( 23.14999999999999858, 76.00000000001212186, -134.5231074845243313 ) ) ;
#217993 = ORIENTED_EDGE ( 'NONE', *, *, #193288, .F. ) ;
#217994 = AXIS2_PLACEMENT_3D ( 'NONE', #75265, #72699, #152238 ) ;
#217995 = EDGE_CURVE ( 'NONE', #51091, #58399, #246785, .T. ) ;
#217996 = DIRECTION ( 'NONE',  ( 1.000000000000000000, 0.000000000000000000, 0.000000000000000000 ) ) ;
#217998 = CYLINDRICAL_SURFACE ( 'NONE', #21047, 0.09999999999999986677 ) ;
#217997 = AXIS2_PLACEMENT_3D ( 'NONE', #94398, #154426, #77395 ) ;
#217999 = EDGE_CURVE ( 'NONE', #240985, #179279, #105628, .T. ) ;
#218000 = AXIS2_PLACEMENT_3D ( 'NONE', #9621, #31796, #68325 ) ;
#218001 = ORIENTED_EDGE ( 'NONE', *, *, #250348, .T. ) ;
#218002 = DIRECTION ( 'NONE',  ( -1.000000000000000000, -0.000000000000000000, -0.000000000000000000 ) ) ;
#218003 = EDGE_LOOP ( 'NONE', ( #10414, #76797, #228148, #191864 ) ) ;
#218004 = DIRECTION ( 'NONE',  ( 0.000000000000000000, 0.000000000000000000, 1.000000000000000000 ) ) ;
#218005 = EDGE_CURVE ( 'NONE', #53814, #122630, #180497, .T. ) ;
#218006 = TOROIDAL_SURFACE ( 'NONE', #251340, 0.2000000000000000111, 0.1000000000000000056 ) ;
#218007 = DIRECTION ( 'NONE',  ( -0.000000000000000000, 1.000000000000000000, -0.000000000000000000 ) ) ;
#218008 = FACE_OUTER_BOUND ( 'NONE', #237781, .T. ) ;
#218009 = VERTEX_POINT ( 'NONE', #47288 ) ;
#218010 = ORIENTED_EDGE ( 'NONE', *, *, #197371, .T. ) ;
#218011 = AXIS2_PLACEMENT_3D ( 'NONE', #220621, #218022, #121552 ) ;
#218012 = CIRCLE ( 'NONE', #51411, 10.00000000000000178 ) ;
#218013 = CIRCLE ( 'NONE', #80647, 0.2000000000000057288 ) ;
#218014 = DIRECTION ( 'NONE',  ( 1.000000000000000000, 2.952720810173289112E-16, -0.000000000000000000 ) ) ;
#218015 = FACE_OUTER_BOUND ( 'NONE', #245144, .T. ) ;
#218016 = CARTESIAN_POINT ( 'NONE',  ( -16.93710578446435377, 63.01537210432839231, -213.3870536919253595 ) ) ;
#218017 = DIRECTION ( 'NONE',  ( 0.000000000000000000, 0.000000000000000000, -1.000000000000000000 ) ) ;
#218019 = DIRECTION ( 'NONE',  ( -0.000000000000000000, 0.01283462868039629209, -0.9999176327611372095 ) ) ;
#218018 = DIRECTION ( 'NONE',  ( -1.000000000000000000, 0.000000000000000000, 0.000000000000000000 ) ) ;
#218020 = CARTESIAN_POINT ( 'NONE',  ( 18.41416235934317314, -9.499999999988842703, -174.1001893912220169 ) ) ;
#218021 = LINE ( 'NONE', #257121, #139753 ) ;
#218022 = DIRECTION ( 'NONE',  ( 0.000000000000000000, -0.03181660087583042945, 0.9994937237965569876 ) ) ;
#218023 = EDGE_LOOP ( 'NONE', ( #127997, #99035, #255654, #17963 ) ) ;
#218024 = CARTESIAN_POINT ( 'NONE',  ( -22.50000000000000000, 1.115600667400684642E-11, -167.4999999999999716 ) ) ;
#218026 = EDGE_LOOP ( 'NONE', ( #42803, #36471, #39201, #195912 ) ) ;
#218025 = DIRECTION ( 'NONE',  ( -0.000000000000000000, -1.000000000000000000, 0.000000000000000000 ) ) ;
#218027 = LINE ( 'NONE', #255847, #230968 ) ;
#218028 = DIRECTION ( 'NONE',  ( 0.000000000000000000, -1.000000000000000000, 0.000000000000000000 ) ) ;
#218030 = DIRECTION ( 'NONE',  ( 1.000000000000000000, 0.000000000000000000, 0.000000000000000000 ) ) ;
#218029 = CYLINDRICAL_SURFACE ( 'NONE', #109441, 0.09999999999999108213 ) ;
#218031 = EDGE_CURVE ( 'NONE', #249805, #189336, #27786, .T. ) ;
#218032 = ORIENTED_EDGE ( 'NONE', *, *, #161265, .T. ) ;
#218034 = LINE ( 'NONE', #161962, #217468 ) ;
#218033 = FACE_OUTER_BOUND ( 'NONE', #76580, .T. ) ;
#218036 = ADVANCED_FACE ( 'NONE', ( #206392 ), #114013, .F. ) ;
#218035 = DIRECTION ( 'NONE',  ( 2.840903330521633255E-16, -0.8700118002898322711, 0.4930308989875231696 ) ) ;
#218037 = CARTESIAN_POINT ( 'NONE',  ( 21.05000000000000071, 70.50554186077093277, -228.5577520746950597 ) ) ;
#218038 = CARTESIAN_POINT ( 'NONE',  ( -22.39999999999999858, 76.00000000001213607, -136.5231074845242745 ) ) ;
#218039 = CARTESIAN_POINT ( 'NONE',  ( -18.50596464788227635, 10.30632246271647112, -139.5041836778896140 ) ) ;
#218040 = ORIENTED_EDGE ( 'NONE', *, *, #90985, .T. ) ;
#218041 = FACE_BOUND ( 'NONE', #112497, .T. ) ;
#218042 = VERTEX_POINT ( 'NONE', #29077 ) ;
#218043 = AXIS2_PLACEMENT_3D ( 'NONE', #215830, #37234, #56741 ) ;
#218044 = AXIS2_PLACEMENT_3D ( 'NONE', #246514, #183978, #9192 ) ;
#218045 = EDGE_CURVE ( 'NONE', #161554, #37930, #80701, .T. ) ;
#218046 = CARTESIAN_POINT ( 'NONE',  ( -18.39999999999999858, -9.500000000000005329, -40.10018939122204529 ) ) ;
#218047 = ORIENTED_EDGE ( 'NONE', *, *, #2174, .F. ) ;
#218048 = DIRECTION ( 'NONE',  ( 0.000000000000000000, 0.000000000000000000, -1.000000000000000000 ) ) ;
#218049 = TOROIDAL_SURFACE ( 'NONE', #59824, 0.2000000000000000111, 0.1000000000000000056 ) ;
#218050 = ORIENTED_EDGE ( 'NONE', *, *, #124153, .T. ) ;
#218051 =( BOUNDED_SURFACE ( )  B_SPLINE_SURFACE ( 3, 2, ( 
 ( #252474, #73891, #153444 ),
 ( #98500, #254988, #116834 ),
 ( #155985, #192525, #174294 ),
 ( #157270, #154707, #76403 ),
 ( #236765, #235482, #214636 ),
 ( #55533, #58114, #56821 ) ),
 .UNSPECIFIED., .F., .F., .T. ) 
 B_SPLINE_SURFACE_WITH_KNOTS ( ( 4, 2, 4 ),
 ( 3, 3 ),
 ( 0.0001792624049599534481, 0.0003686986002124667365, 0.0005581347954649799707 ),
 ( 0.000000000000000000, 1.000000000000000000 ),
 .UNSPECIFIED. ) 
 GEOMETRIC_REPRESENTATION_ITEM ( )  RATIONAL_B_SPLINE_SURFACE ( (
 ( 1.000000000000000000, 0.9238795325112859613, 1.000000000000000000),
 ( 1.000000000000000000, 0.9229318695239708825, 1.000000000000000000),
 ( 1.000000000000000000, 0.8926288119229073281, 1.000000000000000000),
 ( 1.000000000000000000, 0.8123777807272978269, 1.000000000000000000),
 ( 1.000000000000000000, 0.7629087100930436183, 1.000000000000000000),
 ( 1.000000000000000000, 0.7071067811865475727, 1.000000000000000000) ) ) 
 REPRESENTATION_ITEM ( '' )  SURFACE ( )  );
#218052 = CARTESIAN_POINT ( 'NONE',  ( -22.01447462590972748, 7.263800201241075172, -167.4009629999404183 ) ) ;
#218053 = CIRCLE ( 'NONE', #55715, 0.1000000000000081657 ) ;
#218054 = AXIS2_PLACEMENT_3D ( 'NONE', #254172, #79384, #157706 ) ;
#218055 = CARTESIAN_POINT ( 'NONE',  ( -18.39999999999999858, 85.60000000001211617, -129.9229180933022576 ) ) ;
#218056 = ORIENTED_EDGE ( 'NONE', *, *, #192364, .F. ) ;
#218057 = AXIS2_PLACEMENT_3D ( 'NONE', #214832, #151027, #134012 ) ;
#218058 = DIRECTION ( 'NONE',  ( 0.000000000000000000, -0.4088369013363280513, 0.9126074666063769270 ) ) ;
#218059 = DIRECTION ( 'NONE',  ( 1.000000000000000000, -0.000000000000000000, -0.000000000000000000 ) ) ;
#218060 = DIRECTION ( 'NONE',  ( -0.7071067811865487940, -0.7071067811865463515, -4.937700262164522799E-15 ) ) ;
#218062 = VECTOR ( 'NONE', #173367, 1000.000000000000000 ) ;
#218061 = DIRECTION ( 'NONE',  ( 0.000000000000000000, 0.9651348961777157509, -0.2617529984165031243 ) ) ;
#218063 = CARTESIAN_POINT ( 'NONE',  ( -23.25000000000000000, -11.74999999998884448, -21.75000000000000355 ) ) ;
#218064 = CIRCLE ( 'NONE', #26571, 0.1000000000000028644 ) ;
#218065 = SPHERICAL_SURFACE ( 'NONE', #23844, 0.1000000000000000056 ) ;
#218066 = EDGE_CURVE ( 'NONE', #184335, #52949, #126506, .T. ) ;
#218067 = ORIENTED_EDGE ( 'NONE', *, *, #29260, .F. ) ;
#218068 = DIRECTION ( 'NONE',  ( 0.000000000000000000, 0.4088369013363281068, -0.9126074666063770380 ) ) ;
#218069 = B_SPLINE_CURVE_WITH_KNOTS ( 'NONE', 3,
 ( #216391, #113448, #198118, #235952, #35232, #173483 ),
 .UNSPECIFIED., .F., .F.,
 ( 4, 2, 4 ),
 ( 0.000000000000000000, 0.0002113392456165983529, 0.0004226784912331967058 ),
 .UNSPECIFIED. ) ;
#218070 = ORIENTED_EDGE ( 'NONE', *, *, #252847, .T. ) ;
#218072 = EDGE_LOOP ( 'NONE', ( #51285, #145921, #128937, #149483 ) ) ;
#218071 = CARTESIAN_POINT ( 'NONE',  ( -16.87036670365549895, 66.01058118071021852, -90.50266760182643111 ) ) ;
#218073 = AXIS2_PLACEMENT_3D ( 'NONE', #12953, #135427, #231997 ) ;
#218074 = VERTEX_POINT ( 'NONE', #109840 ) ;
#218075 = CARTESIAN_POINT ( 'NONE',  ( 21.05000000000000071, 76.00000000001244871, -170.0231074845243597 ) ) ;
#218076 = CARTESIAN_POINT ( 'NONE',  ( -21.05000000000000071, 7.128833340094563376, -233.7327013124401276 ) ) ;
#218077 = DIRECTION ( 'NONE',  ( -1.000000000000000000, 0.000000000000000000, 0.000000000000000000 ) ) ;
#218078 = CARTESIAN_POINT ( 'NONE',  ( 18.59999999999999076, 6.982009704867611077, -104.1961521182563359 ) ) ;
#218079 = DIRECTION ( 'NONE',  ( 0.7071067811865474617, 0.2890913453342131012, -0.6453109281988449464 ) ) ;
#218080 = VERTEX_POINT ( 'NONE', #146390 ) ;
#218081 = EDGE_CURVE ( 'NONE', #195524, #251640, #30666, .T. ) ;
#218082 = CARTESIAN_POINT ( 'NONE',  ( -16.94225986326250322, 9.950000000011138823, -146.9467193756078700 ) ) ;
#218083 = DIRECTION ( 'NONE',  ( 0.000000000000000000, 6.308085367182471812E-16, 1.000000000000000000 ) ) ;
#218084 = ORIENTED_EDGE ( 'NONE', *, *, #133559, .T. ) ;
#218085 = EDGE_CURVE ( 'NONE', #93777, #118692, #222153, .T. ) ;
#218087 = ORIENTED_EDGE ( 'NONE', *, *, #30381, .F. ) ;
#218086 = DIRECTION ( 'NONE',  ( 0.000000000000000000, -0.1686199900910313187, 0.9856811345164828708 ) ) ;
#218088 = DIRECTION ( 'NONE',  ( -1.000000000000000000, 1.836970198721029934E-16, 1.282749433769087757E-30 ) ) ;
#218089 = AXIS2_PLACEMENT_3D ( 'NONE', #91218, #93767, #213718 ) ;
#218090 = EDGE_CURVE ( 'NONE', #155941, #182465, #243021, .T. ) ;
#218091 = CARTESIAN_POINT ( 'NONE',  ( -21.64999999999999858, 68.75000000001254818, -182.2731074845244166 ) ) ;
#218092 = ORIENTED_EDGE ( 'NONE', *, *, #79432, .F. ) ;
#218093 = AXIS2_PLACEMENT_3D ( 'NONE', #132588, #213389, #13930 ) ;
#218094 = CIRCLE ( 'NONE', #101555, 0.1000000000000094008 ) ;
#218095 = EDGE_CURVE ( 'NONE', #111006, #143109, #134679, .T. ) ;
#218096 = CARTESIAN_POINT ( 'NONE',  ( 22.39999999999999858, 0.3085173699977246109, -229.9658011520297975 ) ) ;
#218099 = EDGE_CURVE ( 'NONE', #237441, #183242, #108574, .T. ) ;
#218098 = EDGE_CURVE ( 'NONE', #93310, #31867, #30334, .T. ) ;
#218097 = EDGE_LOOP ( 'NONE', ( #127945, #31805, #256811, #90449 ) ) ;
#218100 = CARTESIAN_POINT ( 'NONE',  ( 21.14999999999999503, -11.64999999998883595, -170.3999999999999773 ) ) ;
#218101 = LINE ( 'NONE', #235126, #88987 ) ;
#218102 =( BOUNDED_CURVE ( )  B_SPLINE_CURVE ( 3, ( #44963, #82755, #161065, #123210 ),
 .UNSPECIFIED., .F., .F. ) 
 B_SPLINE_CURVE_WITH_KNOTS ( ( 4, 4 ),
 ( 0.3000847527772370071, 0.5497968875596834781 ),
 .UNSPECIFIED. ) 
 CURVE ( )  GEOMETRIC_REPRESENTATION_ITEM ( )  RATIONAL_B_SPLINE_CURVE ( ( 1.000000000000000000, 0.9948104011409417691, 0.9948104011409417691, 1.000000000000000000 ) ) 
 REPRESENTATION_ITEM ( '' )  );
#218103 = DIRECTION ( 'NONE',  ( 0.000000000000000000, 0.000000000000000000, 1.000000000000000000 ) ) ;
#218104 = AXIS2_PLACEMENT_3D ( 'NONE', #182919, #69393, #130628 ) ;
#218105 = CIRCLE ( 'NONE', #197277, 0.09999999999999741040 ) ;
#218107 = EDGE_CURVE ( 'NONE', #5240, #228447, #63967, .T. ) ;
#218106 = CIRCLE ( 'NONE', #163973, 11.80000000000000426 ) ;
#218108 = ADVANCED_FACE ( 'NONE', ( #49876 ), #129418, .T. ) ;
#218109 = ORIENTED_EDGE ( 'NONE', *, *, #177976, .F. ) ;
#218110 = FACE_OUTER_BOUND ( 'NONE', #157956, .T. ) ;
#218111 = VERTEX_POINT ( 'NONE', #177577 ) ;
#218112 = CARTESIAN_POINT ( 'NONE',  ( -20.65000000000000568, 68.75000000001226397, -149.1731074845244223 ) ) ;
#218113 = EDGE_CURVE ( 'NONE', #202021, #97694, #214097, .T. ) ;
#218114 = CARTESIAN_POINT ( 'NONE',  ( 23.24999999999999645, 58.31215475832291162, -223.8520309854405923 ) ) ;
#218116 = ORIENTED_EDGE ( 'NONE', *, *, #152698, .F. ) ;
#218115 = CARTESIAN_POINT ( 'NONE',  ( -21.98333005346336932, 1.115600667400684642E-11, -59.62592467094336968 ) ) ;
#218117 = CARTESIAN_POINT ( 'NONE',  ( -20.54999999999999716, 85.00000000001188027, -93.62913836187181005 ) ) ;
#218118 = CARTESIAN_POINT ( 'NONE',  ( 18.59999999999999076, 4.252251777740764460, -211.8999245327126744 ) ) ;
#218119 = CARTESIAN_POINT ( 'NONE',  ( 22.50000000000000000, 64.35042919246716053, -103.1231074845243825 ) ) ;
#218120 = LINE ( 'NONE', #179053, #237865 ) ;
#218121 = DIRECTION ( 'NONE',  ( 0.000000000000000000, 0.9770955615653543758, 0.2128009952262553683 ) ) ;
#218122 = CARTESIAN_POINT ( 'NONE',  ( -18.40000000000000568, 64.58541674041275371, -182.6731074845244223 ) ) ;
#218124 = EDGE_CURVE ( 'NONE', #91231, #95344, #227538, .T. ) ;
#218123 = CARTESIAN_POINT ( 'NONE',  ( -18.52186455169011481, 85.48101848145478243, -129.4980910066099398 ) ) ;
#218126 = VERTEX_POINT ( 'NONE', #13335 ) ;
#218125 = CARTESIAN_POINT ( 'NONE',  ( -21.40925344232282512, 69.34148114062169554, -136.6220576731439849 ) ) ;
#218127 = EDGE_CURVE ( 'NONE', #75842, #37875, #175020, .T. ) ;
#218128 = PLANE ( 'NONE',  #218185 ) ;
#218129 = AXIS2_PLACEMENT_3D ( 'NONE', #88529, #229361, #48136 ) ;
#218130 = VERTEX_POINT ( 'NONE', #74628 ) ;
#218131 = ORIENTED_EDGE ( 'NONE', *, *, #176572, .T. ) ;
#218133 = ADVANCED_FACE ( 'NONE', ( #92852 ), #55542, .F. ) ;
#218132 = DIRECTION ( 'NONE',  ( 0.000000000000000000, 1.000000000000000000, 0.000000000000000000 ) ) ;
#218134 = LINE ( 'NONE', #214311, #34853 ) ;
#218135 = ORIENTED_EDGE ( 'NONE', *, *, #98270, .F. ) ;
#218136 = CARTESIAN_POINT ( 'NONE',  ( -16.87683809663752399, 12.41403342719998726, -211.2428889513006993 ) ) ;
#218137 = DIRECTION ( 'NONE',  ( 0.000000000000000000, 0.000000000000000000, 1.000000000000000000 ) ) ;
#218138 = ADVANCED_FACE ( 'NONE', ( #191990 ), #152875, .T. ) ;
#218139 = ORIENTED_EDGE ( 'NONE', *, *, #13514, .F. ) ;
#218140 = AXIS2_PLACEMENT_3D ( 'NONE', #96595, #99166, #139577 ) ;
#218141 = CARTESIAN_POINT ( 'NONE',  ( -20.54999999999999716, -8.999999999988844479, -191.5060308773475413 ) ) ;
#218142 = VECTOR ( 'NONE', #108096, 1000.000000000000000 ) ;
#218143 = VECTOR ( 'NONE', #142274, 1000.000000000000000 ) ;
#218144 = CARTESIAN_POINT ( 'NONE',  ( -16.93658211146646408, 66.00589133767141448, -190.9274025544800963 ) ) ;
#218145 = VERTEX_POINT ( 'NONE', #173738 ) ;
#218146 = DIRECTION ( 'NONE',  ( 1.000000000000000000, 0.000000000000000000, 0.000000000000000000 ) ) ;
#218147 = VERTEX_POINT ( 'NONE', #36785 ) ;
#218149 = ADVANCED_FACE ( 'NONE', ( #54993 ), #51453, .T. ) ;
#218148 = CARTESIAN_POINT ( 'NONE',  ( -20.85000000000000142, -11.75000000000000000, -33.50000000000000000 ) ) ;
#218151 = ORIENTED_EDGE ( 'NONE', *, *, #6164, .T. ) ;
#218150 = CARTESIAN_POINT ( 'NONE',  ( -18.59999999999999787, 74.26374286841520700, -191.9544551555068779 ) ) ;
#218152 = DIRECTION ( 'NONE',  ( 0.000000000000000000, 0.000000000000000000, 1.000000000000000000 ) ) ;
#218153 = VERTEX_POINT ( 'NONE', #134534 ) ;
#218154 = ORIENTED_EDGE ( 'NONE', *, *, #92096, .F. ) ;
#218156 = ORIENTED_EDGE ( 'NONE', *, *, #186968, .F. ) ;
#218155 = ORIENTED_EDGE ( 'NONE', *, *, #151444, .T. ) ;
#218158 = CARTESIAN_POINT ( 'NONE',  ( 20.94999999999999574, 68.11887992016828264, -227.8068560890360175 ) ) ;
#218157 = VECTOR ( 'NONE', #26668, 1000.000000000000000 ) ;
#218159 = ORIENTED_EDGE ( 'NONE', *, *, #27309, .T. ) ;
#218160 = CARTESIAN_POINT ( 'NONE',  ( -18.79999999999999716, -1.212568896937008089, -8.000000000000000000 ) ) ;
#218161 = VERTEX_POINT ( 'NONE', #117559 ) ;
#218162 = AXIS2_PLACEMENT_3D ( 'NONE', #253926, #94858, #171880 ) ;
#218163 = CIRCLE ( 'NONE', #130698, 0.09999999999999939493 ) ;
#218164 = AXIS2_PLACEMENT_3D ( 'NONE', #156331, #235823, #134153 ) ;
#218165 = ORIENTED_EDGE ( 'NONE', *, *, #87150, .T. ) ;
#218166 = CARTESIAN_POINT ( 'NONE',  ( 18.59999999999999787, 7.783179459866048866, -245.3643104511423019 ) ) ;
#218167 = CARTESIAN_POINT ( 'NONE',  ( -23.15000000000000213, -8.596261682231830292, -158.0498724828497359 ) ) ;
#218169 = ORIENTED_EDGE ( 'NONE', *, *, #178367, .F. ) ;
#218168 = LINE ( 'NONE', #142495, #199137 ) ;
#218170 = DIRECTION ( 'NONE',  ( -1.000000000000000000, 0.000000000000000000, 0.000000000000000000 ) ) ;
#218171 = ORIENTED_EDGE ( 'NONE', *, *, #32155, .T. ) ;
#218172 = CARTESIAN_POINT ( 'NONE',  ( -18.52643265882458579, 65.68026841930924320, -130.9725740131889893 ) ) ;
#218173 = CARTESIAN_POINT ( 'NONE',  ( 21.13461538461538325, 67.11458296203782936, -157.6731074845244223 ) ) ;
#218174 = CARTESIAN_POINT ( 'NONE',  ( -23.25000000000000000, 64.35000000001180354, -81.67310748452439384 ) ) ;
#218175 = AXIS2_PLACEMENT_3D ( 'NONE', #205433, #144170, #228872 ) ;
#218176 = ORIENTED_EDGE ( 'NONE', *, *, #116274, .T. ) ;
#218177 = VECTOR ( 'NONE', #6218, 1000.000000000000000 ) ;
#218178 = DIRECTION ( 'NONE',  ( -1.000000000000000000, -0.000000000000000000, -0.000000000000000000 ) ) ;
#218179 = DIRECTION ( 'NONE',  ( 0.000000000000000000, 0.000000000000000000, 1.000000000000000000 ) ) ;
#218180 = DIRECTION ( 'NONE',  ( 1.000000000000000000, 0.000000000000000000, 0.000000000000000000 ) ) ;
#218181 = CIRCLE ( 'NONE', #205719, 12.87499999999999822 ) ;
#218182 = ORIENTED_EDGE ( 'NONE', *, *, #141707, .T. ) ;
#218183 = CARTESIAN_POINT ( 'NONE',  ( 20.99999999999999645, 13.96358247574307221, -219.2976327551816951 ) ) ;
#218184 = ORIENTED_EDGE ( 'NONE', *, *, #90771, .F. ) ;
#218185 = AXIS2_PLACEMENT_3D ( 'NONE', #197296, #172661, #216860 ) ;
#218186 = VERTEX_POINT ( 'NONE', #96676 ) ;
#218187 = DIRECTION ( 'NONE',  ( 0.000000000000000000, -0.3738317757008748909, -0.9274965247785733613 ) ) ;
#218189 = EDGE_LOOP ( 'NONE', ( #233693, #217327, #182533, #70183 ) ) ;
#218188 = AXIS2_PLACEMENT_3D ( 'NONE', #101726, #236132, #57475 ) ;
#218190 = EDGE_LOOP ( 'NONE', ( #100713, #194519, #229967, #190762 ) ) ;
#218191 = FACE_OUTER_BOUND ( 'NONE', #111720, .T. ) ;
#218192 = LINE ( 'NONE', #34480, #79284 ) ;
#218193 = VERTEX_POINT ( 'NONE', #14634 ) ;
#218194 = ORIENTED_EDGE ( 'NONE', *, *, #26610, .F. ) ;
#218195 = DIRECTION ( 'NONE',  ( 0.000000000000000000, -6.982962677686266711E-15, 1.000000000000000000 ) ) ;
#218196 = AXIS2_PLACEMENT_3D ( 'NONE', #95009, #256598, #252793 ) ;
#218197 = CIRCLE ( 'NONE', #168201, 12.87499999999999822 ) ;
#218198 = CARTESIAN_POINT ( 'NONE',  ( -20.64999999999999858, 74.00000000001180922, -82.34772940728642254 ) ) ;
#218199 = CIRCLE ( 'NONE', #226581, 0.09999999999999178990 ) ;
#218200 = ORIENTED_EDGE ( 'NONE', *, *, #232612, .F. ) ;
#218201 = EDGE_CURVE ( 'NONE', #58187, #248715, #114991, .T. ) ;
#218202 = ORIENTED_EDGE ( 'NONE', *, *, #28283, .F. ) ;
#218203 = VERTEX_POINT ( 'NONE', #236220 ) ;
#218204 = CARTESIAN_POINT ( 'NONE',  ( 21.05000000000000071, 69.45934304831143891, -203.4231074845244223 ) ) ;
#218205 = FACE_OUTER_BOUND ( 'NONE', #160355, .T. ) ;
#218206 = LINE ( 'NONE', #117841, #155797 ) ;
#218207 = FACE_OUTER_BOUND ( 'NONE', #255845, .T. ) ;
#218208 = ADVANCED_FACE ( 'NONE', ( #234950 ), #155448, .T. ) ;
#218209 = DIRECTION ( 'NONE',  ( -1.000000000000000000, -0.000000000000000000, -0.000000000000000000 ) ) ;
#218210 = ADVANCED_FACE ( 'NONE', ( #135824 ), #257022, .T. ) ;
#218211 = DIRECTION ( 'NONE',  ( 0.000000000000000000, 6.982962677686266711E-15, -1.000000000000000000 ) ) ;
#218212 = CIRCLE ( 'NONE', #105790, 0.8750000000000007772 ) ;
#218213 = B_SPLINE_CURVE_WITH_KNOTS ( 'NONE', 3,
 ( #129196, #10534, #172219, #30109, #109613, #251701, #110906 ),
 .UNSPECIFIED., .F., .F.,
 ( 4, 3, 4 ),
 ( 0.000000000000000000, 0.0007844235214594318627, 0.001767853679404347454 ),
 .UNSPECIFIED. ) ;
#218215 = CARTESIAN_POINT ( 'NONE',  ( -19.99999999999999645, 5.454087299794355914, 16.60000000000000142 ) ) ;
#218214 = DIRECTION ( 'NONE',  ( 1.186688945009009831E-16, -1.000000000000000000, 0.000000000000000000 ) ) ;
#218216 = DIRECTION ( 'NONE',  ( -1.000000000000000000, 3.265361837132813093E-16, 2.280189983783949500E-30 ) ) ;
#218217 = CARTESIAN_POINT ( 'NONE',  ( -16.87401514999228880, 23.03975626714240832, -230.9681084165865173 ) ) ;
#218218 = CIRCLE ( 'NONE', #122396, 0.09999999999999939493 ) ;
#218219 = FACE_OUTER_BOUND ( 'NONE', #255343, .T. ) ;
#218220 = CIRCLE ( 'NONE', #22640, 0.1000000000000124678 ) ;
#218221 = ORIENTED_EDGE ( 'NONE', *, *, #11888, .F. ) ;
#218222 = AXIS2_PLACEMENT_3D ( 'NONE', #250223, #49459, #11635 ) ;
#218223 = ADVANCED_FACE ( 'NONE', ( #215369 ), #255743, .T. ) ;
#218224 = CIRCLE ( 'NONE', #189038, 0.5000000000000022204 ) ;
#218226 = VERTEX_POINT ( 'NONE', #251933 ) ;
#218225 = LINE ( 'NONE', #254762, #157308 ) ;
#218227 = ADVANCED_FACE ( 'NONE', ( #77145 ), #138930, .T. ) ;
#218228 = LINE ( 'NONE', #39651, #249109 ) ;
#218229 = DIRECTION ( 'NONE',  ( 1.000000000000000000, 0.000000000000000000, 0.000000000000000000 ) ) ;
#218230 = VECTOR ( 'NONE', #55421, 1000.000000000000000 ) ;
#218231 = EDGE_CURVE ( 'NONE', #169886, #245309, #137133, .T. ) ;
#218232 = SURFACE_STYLE_USAGE ( .BOTH. , #138680 ) ;
#218233 = ORIENTED_EDGE ( 'NONE', *, *, #230271, .T. ) ;
#218234 = AXIS2_PLACEMENT_3D ( 'NONE', #130041, #88333, #208337 ) ;
#218235 = AXIS2_PLACEMENT_3D ( 'NONE', #51909, #114476, #53221 ) ;
#218236 = DIRECTION ( 'NONE',  ( 0.000000000000000000, 1.000000000000000000, 0.000000000000000000 ) ) ;
#218237 = ADVANCED_FACE ( 'NONE', ( #34207 ), #28451, .T. ) ;
#218238 = CIRCLE ( 'NONE', #147539, 4.099999999999992539 ) ;
#218239 = PRODUCT_DEFINITION_SHAPE ( 'NONE', 'NONE',  #258113 ) ;
#218240 = CARTESIAN_POINT ( 'NONE',  ( -17.01764560440512142, 9.950000000011138823, -54.25000000078541973 ) ) ;
#218241 = ORIENTED_EDGE ( 'NONE', *, *, #201347, .T. ) ;
#218242 = AXIS2_PLACEMENT_3D ( 'NONE', #226179, #63283, #26763 ) ;
#218243 = CARTESIAN_POINT ( 'NONE',  ( -21.14999999999999858, 11.75000000001115197, -140.7838656629781724 ) ) ;
#218244 = DIRECTION ( 'NONE',  ( 0.000000000000000000, 0.000000000000000000, 1.000000000000000000 ) ) ;
#218245 = EDGE_CURVE ( 'NONE', #231604, #14866, #72352, .T. ) ;
#218246 = CARTESIAN_POINT ( 'NONE',  ( -18.40000000000000213, 64.25000000001153921, -48.67310748452440805 ) ) ;
#218247 = SPHERICAL_SURFACE ( 'NONE', #95249, 0.1000000000000000056 ) ;
#218249 = VERTEX_POINT ( 'NONE', #101817 ) ;
#218248 = DIRECTION ( 'NONE',  ( 0.000000000000000000, -0.8660254037844377084, -0.5000000000000016653 ) ) ;
#218250 = B_SPLINE_CURVE_WITH_KNOTS ( 'NONE', 3,
 ( #100760, #154404, #233899, #122951, #184184, #44699, #26425, #86346, #61684, #124240, #102066, #5535, #241602 ),
 .UNSPECIFIED., .F., .F.,
 ( 4, 3, 3, 3, 4 ),
 ( -3.224855718277077941E-06, 0.000000000000000000, 6.199515528668320112E-06, 4.034952380127989350E-05, 7.452715123700383651E-05 ),
 .UNSPECIFIED. ) ;
#218251 = AXIS2_PLACEMENT_3D ( 'NONE', #193663, #6344, #205844 ) ;
#218253 = ORIENTED_EDGE ( 'NONE', *, *, #169580, .T. ) ;
#218252 = CARTESIAN_POINT ( 'NONE',  ( -18.46919391072061956, 85.67072438828961367, -96.34930395272469639 ) ) ;
#218254 = CARTESIAN_POINT ( 'NONE',  ( -22.49436431346200038, 11.64995094766461392, -167.4330964702777180 ) ) ;
#218255 = DIRECTION ( 'NONE',  ( -6.938893903907222856E-15, 1.000000000000000000, 2.891205793294679805E-16 ) ) ;
#218256 = FACE_OUTER_BOUND ( 'NONE', #244217, .T. ) ;
#218258 = EDGE_CURVE ( 'NONE', #208746, #24271, #218064, .T. ) ;
#218257 = DIRECTION ( 'NONE',  ( -0.000000000000000000, -0.9651348961777157509, 0.2617529984165031243 ) ) ;
#218259 = VECTOR ( 'NONE', #114313, 1000.000000000000114 ) ;
#218261 = CARTESIAN_POINT ( 'NONE',  ( -22.39999999999999858, 64.25000000001269029, -203.5231074845244166 ) ) ;
#218260 = CARTESIAN_POINT ( 'NONE',  ( 18.42555734704281889, 8.849919995194017730, -245.4285591738437802 ) ) ;
#218262 = LINE ( 'NONE', #137445, #74552 ) ;
#218263 = CARTESIAN_POINT ( 'NONE',  ( 22.60000000000000142, 0.1008583691098682150, -155.7504328765105868 ) ) ;
#218264 = DIRECTION ( 'NONE',  ( 0.7071067811865456854, -0.7071067811865493491, -0.000000000000000000 ) ) ;
#218265 = LINE ( 'NONE', #77464, #235033 ) ;
#218266 = SPHERICAL_SURFACE ( 'NONE', #126806, 0.1000000000000000056 ) ;
#218267 = CIRCLE ( 'NONE', #189075, 0.1000000000000055844 ) ;
#218269 = ORIENTED_EDGE ( 'NONE', *, *, #71044, .T. ) ;
#218268 = AXIS2_PLACEMENT_3D ( 'NONE', #255371, #37694, #198012 ) ;
#218270 = CARTESIAN_POINT ( 'NONE',  ( 21.07954640115298162, 0.06600770715069002870, -94.17071230397618820 ) ) ;
#218271 = EDGE_LOOP ( 'NONE', ( #30595, #85464, #119712, #52592 ) ) ;
#218272 = EDGE_LOOP ( 'NONE', ( #160113, #89917 ) ) ;
#218273 = CARTESIAN_POINT ( 'NONE',  ( -18.69999999999999929, -8.250000000000005329, 32.89999999999999858 ) ) ;
#218274 = DIRECTION ( 'NONE',  ( 1.000000000000000000, 0.000000000000000000, 0.000000000000000000 ) ) ;
#218275 = ORIENTED_EDGE ( 'NONE', *, *, #214767, .T. ) ;
#218276 = ORIENTED_EDGE ( 'NONE', *, *, #74139, .T. ) ;
#218277 =( LENGTH_UNIT ( ) NAMED_UNIT ( * ) SI_UNIT ( .MILLI., .METRE. ) );
#218279 = VERTEX_POINT ( 'NONE', #167 ) ;
#218278 = B_SPLINE_CURVE_WITH_KNOTS ( 'NONE', 3,
 ( #212648, #174842, #194381, #234762, #32755, #130518, #112268, #34037, #254305, #249205, #232222, #230935, #53563, #150117, #91410, #170991, #172272, #250467, #56097 ),
 .UNSPECIFIED., .F., .F.,
 ( 4, 3, 3, 3, 3, 3, 4 ),
 ( 0.000000000000000000, 1.655171619024644586E-05, 2.773500582848746404E-05, 5.941817267377038920E-05, 0.0001114174635873305049, 0.0001914169455916114393, 0.0002627181070750297790 ),
 .UNSPECIFIED. ) ;
#218280 = AXIS2_PLACEMENT_3D ( 'NONE', #162136, #42181, #142538 ) ;
#218281 = ORIENTED_EDGE ( 'NONE', *, *, #155063, .T. ) ;
#218282 = ADVANCED_FACE ( 'NONE', ( #181413 ), #205597, .F. ) ;
#218283 = DIRECTION ( 'NONE',  ( 0.000000000000000000, 0.4721928772777345129, 0.8814952561688431665 ) ) ;
#218284 = LINE ( 'NONE', #137470, #191039 ) ;
#218285 = CARTESIAN_POINT ( 'NONE',  ( 23.14999999999999503, 64.35000000001218723, -143.5379132551783812 ) ) ;
#218286 = ADVANCED_FACE ( 'NONE', ( #47956 ), #138382, .T. ) ;
#218287 = DIRECTION ( 'NONE',  ( 0.000000000000000000, 0.000000000000000000, -1.000000000000000000 ) ) ;
#218288 = CYLINDRICAL_SURFACE ( 'NONE', #66459, 0.1000000000000070832 ) ;
#218289 = CARTESIAN_POINT ( 'NONE',  ( 21.05000000000000426, 75.94851711813041106, -142.8232873024375351 ) ) ;
#218291 = VERTEX_POINT ( 'NONE', #120175 ) ;
#218290 = CARTESIAN_POINT ( 'NONE',  ( -22.32929514600008503, 75.90092432189779004, -77.10175504990083084 ) ) ;
#218293 = CARTESIAN_POINT ( 'NONE',  ( 20.85000000000000142, -11.64999999998883595, -64.10000000000000853 ) ) ;
#218292 = DIRECTION ( 'NONE',  ( 0.000000000000000000, 0.9770955615653310611, 0.2128009952263620608 ) ) ;
#218294 = EDGE_CURVE ( 'NONE', #247600, #192232, #238946, .T. ) ;
#218295 = DIRECTION ( 'NONE',  ( -0.000000000000000000, -0.000000000000000000, 1.000000000000000000 ) ) ;
#218296 = EDGE_CURVE ( 'NONE', #41545, #174999, #163128, .T. ) ;
#218297 = EDGE_LOOP ( 'NONE', ( #187544, #196583, #35430, #31910 ) ) ;
#218298 = SPHERICAL_SURFACE ( 'NONE', #114488, 0.1000000000000000056 ) ;
#218299 = DIRECTION ( 'NONE',  ( -1.000000000000000000, -0.000000000000000000, -0.000000000000000000 ) ) ;
#218300 = ORIENTED_EDGE ( 'NONE', *, *, #204758, .F. ) ;
#218301 = EDGE_CURVE ( 'NONE', #243832, #203823, #247294, .T. ) ;
#218303 = DIRECTION ( 'NONE',  ( 1.000000000000000000, 0.000000000000000000, 0.000000000000000000 ) ) ;
#218302 = DIRECTION ( 'NONE',  ( -1.000000000000000000, -8.674042436075353235E-17, -1.619280515896125144E-16 ) ) ;
#218304 = EDGE_CURVE ( 'NONE', #159614, #38886, #23636, .T. ) ;
#218305 = FACE_OUTER_BOUND ( 'NONE', #171049, .T. ) ;
#218306 = CARTESIAN_POINT ( 'NONE',  ( 20.04142135623730070, 16.72641738073392403, -222.5849938986771974 ) ) ;
#218307 = EDGE_CURVE ( 'NONE', #151151, #145162, #9981, .T. ) ;
#218308 = ORIENTED_EDGE ( 'NONE', *, *, #170709, .F. ) ;
#218309 = VECTOR ( 'NONE', #231303, 1000.000000000000000 ) ;
#218310 = CYLINDRICAL_SURFACE ( 'NONE', #211727, 2.000000000000001776 ) ;
#218311 = EDGE_CURVE ( 'NONE', #172722, #36165, #207049, .T. ) ;
#218312 = CARTESIAN_POINT ( 'NONE',  ( -18.43459694179556863, -0.7398119410654188099, -242.2185250903025349 ) ) ;
#218313 = CARTESIAN_POINT ( 'NONE',  ( 23.14999999999999858, 76.00000000001126921, -203.5231074845248997 ) ) ;
#218314 = EDGE_LOOP ( 'NONE', ( #56271, #99090, #186260, #129941 ) ) ;
#218315 = CARTESIAN_POINT ( 'NONE',  ( 23.25000000000000000, -9.600000000000006750, 11.75000000000000000 ) ) ;
#218316 = EDGE_CURVE ( 'NONE', #188486, #53873, #176590, .T. ) ;
#218317 = CARTESIAN_POINT ( 'NONE',  ( 21.33487959338958362, 6.725558151922348848, -167.4999999999999716 ) ) ;
#218318 = LINE ( 'NONE', #200071, #161710 ) ;
#218319 = EDGE_CURVE ( 'NONE', #197295, #131701, #155757, .T. ) ;
#218320 = VECTOR ( 'NONE', #127754, 1000.000000000000000 ) ;
#218321 = CARTESIAN_POINT ( 'NONE',  ( 20.94999999999999929, -8.999999999988842703, -191.5060308773475128 ) ) ;
#218322 = AXIS2_PLACEMENT_3D ( 'NONE', #212342, #174539, #114502 ) ;
#218323 = CYLINDRICAL_SURFACE ( 'NONE', #59601, 12.87499999999999822 ) ;
#218324 = AXIS2_PLACEMENT_3D ( 'NONE', #54423, #51837, #74031 ) ;
#218325 = AXIS2_PLACEMENT_3D ( 'NONE', #83213, #47960, #205752 ) ;
#218326 = ADVANCED_FACE ( 'NONE', ( #100529 ), #230757, .F. ) ;
#218328 = EDGE_LOOP ( 'NONE', ( #41626, #80955, #178635, #156989 ) ) ;
#218327 = CARTESIAN_POINT ( 'NONE',  ( -21.14999999999994174, 77.83551161375991967, -47.52760213295649550 ) ) ;
#218329 = LINE ( 'NONE', #16325, #14301 ) ;
#218330 = FACE_OUTER_BOUND ( 'NONE', #179234, .T. ) ;
#218331 = CARTESIAN_POINT ( 'NONE',  ( -18.50000000000000000, -9.399999999988850163, -74.29725975966333351 ) ) ;
#218332 = CARTESIAN_POINT ( 'NONE',  ( 20.94999999999999929, 0.000000000000000000, -35.40000000000000568 ) ) ;
#218333 = CARTESIAN_POINT ( 'NONE',  ( 20.95429693346638444, 10.54330487990667820, -175.0608825383128533 ) ) ;
#218334 = ADVANCED_FACE ( 'NONE', ( #83537 ), #61443, .F. ) ;
#218336 = ORIENTED_EDGE ( 'NONE', *, *, #24666, .F. ) ;
#218335 = CARTESIAN_POINT ( 'NONE',  ( -18.59999999999999787, 7.783179459866048866, -245.3643104511423303 ) ) ;
#218337 = CARTESIAN_POINT ( 'NONE',  ( 21.05000000000000071, 8.776282895292469632, -12.15000000000000036 ) ) ;
#218338 = ADVANCED_FACE ( 'NONE', ( #1454 ), #161855, .T. ) ;
#218339 = CARTESIAN_POINT ( 'NONE',  ( -21.05000000000000071, 61.95000000001210338, -131.0094124137634140 ) ) ;
#218340 = CARTESIAN_POINT ( 'NONE',  ( 20.94999999999999929, 67.49463558145296815, -195.5618716440587548 ) ) ;
#218341 = ORIENTED_EDGE ( 'NONE', *, *, #108712, .T. ) ;
#218342 = DIRECTION ( 'NONE',  ( -3.035766082959430717E-14, 0.000000000000000000, -1.000000000000000000 ) ) ;
#218343 = FACE_OUTER_BOUND ( 'NONE', #219302, .T. ) ;
#218344 = DIRECTION ( 'NONE',  ( 1.000000000000000000, 0.000000000000000000, 0.000000000000000000 ) ) ;
#218345 = DIRECTION ( 'NONE',  ( -1.000000000000000000, 0.000000000000000000, 0.000000000000000000 ) ) ;
#218346 = AXIS2_PLACEMENT_3D ( 'NONE', #150161, #13210, #129296 ) ;
#218347 = CARTESIAN_POINT ( 'NONE',  ( -18.42609945526421455, 78.23215990615727833, -231.5864509253183314 ) ) ;
#218348 = AXIS2_PLACEMENT_3D ( 'NONE', #74290, #131660, #175952 ) ;
#218349 = CYLINDRICAL_SURFACE ( 'NONE', #84281, 0.1000000000000055705 ) ;
#218351 = ORIENTED_EDGE ( 'NONE', *, *, #88255, .T. ) ;
#218350 = AXIS2_PLACEMENT_3D ( 'NONE', #45934, #225824, #161079 ) ;
#218352 = ORIENTED_EDGE ( 'NONE', *, *, #169322, .F. ) ;
#218353 = CIRCLE ( 'NONE', #10086, 0.1000000000000028644 ) ;
#218354 = CYLINDRICAL_SURFACE ( 'NONE', #222353, 0.1000000000000075273 ) ;
#218356 = DIRECTION ( 'NONE',  ( 0.000000000000000000, 0.000000000000000000, -1.000000000000000000 ) ) ;
#218355 = CIRCLE ( 'NONE', #168360, 0.09999999999999939493 ) ;
#218357 = FACE_OUTER_BOUND ( 'NONE', #229395, .T. ) ;
#218358 = CARTESIAN_POINT ( 'NONE',  ( 23.14999999999999858, 1.115600667400684642E-11, -200.9999999999999432 ) ) ;
#218359 = ORIENTED_EDGE ( 'NONE', *, *, #56260, .F. ) ;
#218360 = CARTESIAN_POINT ( 'NONE',  ( -18.40000000000000213, 64.52683809665056458, -179.3229367329901436 ) ) ;
#218361 = AXIS2_PLACEMENT_3D ( 'NONE', #236268, #19812, #141035 ) ;
#218362 = AXIS2_PLACEMENT_3D ( 'NONE', #47466, #124473, #125733 ) ;
#218363 = CARTESIAN_POINT ( 'NONE',  ( 21.00000000000000000, 9.750000000011153745, -121.6500000000000341 ) ) ;
#218364 = TOROIDAL_SURFACE ( 'NONE', #105937, 0.2000000000000000111, 0.1000000000000000056 ) ;
#218365 = CARTESIAN_POINT ( 'NONE',  ( -16.77683809663752257, 9.945835743204145984, -12.66394901910421034 ) ) ;
#218366 = CARTESIAN_POINT ( 'NONE',  ( -1.739115166359751170E-14, 34.53503747617445185, -235.1972745784239578 ) ) ;
#218367 = VECTOR ( 'NONE', #175737, 1000.000000000000000 ) ;
#218368 = DIRECTION ( 'NONE',  ( 1.000000000000000000, 0.000000000000000000, 0.000000000000000000 ) ) ;
#218369 = ORIENTED_EDGE ( 'NONE', *, *, #142713, .T. ) ;
#218370 = DIRECTION ( 'NONE',  ( -0.000000000000000000, -0.000000000000000000, -1.000000000000000000 ) ) ;
#218371 = AXIS2_PLACEMENT_3D ( 'NONE', #41484, #156313, #38911 ) ;
#218372 = ORIENTED_EDGE ( 'NONE', *, *, #144677, .F. ) ;
#218373 = CARTESIAN_POINT ( 'NONE',  ( 20.94999999999999929, 85.00000000001222134, -146.0170766071767332 ) ) ;
#218374 = ORIENTED_EDGE ( 'NONE', *, *, #254850, .T. ) ;
#218375 = DIRECTION ( 'NONE',  ( -0.000000000000000000, -0.2617529984165031243, -0.9651348961777157509 ) ) ;
#218376 = CARTESIAN_POINT ( 'NONE',  ( 18.49999999999999645, 1.728086936805617757, -20.38443500516777007 ) ) ;
#218377 = DIRECTION ( 'NONE',  ( 0.000000000000000000, 0.000000000000000000, -1.000000000000000000 ) ) ;
#218378 = VERTEX_POINT ( 'NONE', #62730 ) ;
#218380 = AXIS2_PLACEMENT_3D ( 'NONE', #213680, #18042, #234521 ) ;
#218379 = DIRECTION ( 'NONE',  ( 0.000000000000000000, -0.1350103645451807555, -0.9908441862701610203 ) ) ;
#218381 = CARTESIAN_POINT ( 'NONE',  ( 11.60000000000000142, -11.75000000000000000, 15.00000000000000355 ) ) ;
#218382 = CIRCLE ( 'NONE', #155892, 11.80000000000000959 ) ;
#218383 = ORIENTED_EDGE ( 'NONE', *, *, #146406, .F. ) ;
#218385 = CARTESIAN_POINT ( 'NONE',  ( -12.92414019175887319, 9.417632963117446465, -152.1489484657323032 ) ) ;
#218384 = AXIS2_PLACEMENT_3D ( 'NONE', #176722, #99705, #76301 ) ;
#218386 = EDGE_CURVE ( 'NONE', #46226, #227104, #97432, .T. ) ;
#218388 = ORIENTED_EDGE ( 'NONE', *, *, #50153, .F. ) ;
#218387 = DIRECTION ( 'NONE',  ( 3.265361837132813093E-16, -1.000000000000000000, -0.000000000000000000 ) ) ;
#218389 = CARTESIAN_POINT ( 'NONE',  ( -16.87036670365549895, 22.95364034536357423, -230.7688863709651628 ) ) ;
#218390 = CARTESIAN_POINT ( 'NONE',  ( -18.58693740092132884, 85.40643215026535984, -162.8982910280230385 ) ) ;
#218391 = EDGE_CURVE ( 'NONE', #7786, #249995, #71407, .T. ) ;
#218392 = EDGE_LOOP ( 'NONE', ( #256190, #156381, #70094, #60286 ) ) ;
#218393 = DIRECTION ( 'NONE',  ( 0.000000000000000000, 0.000000000000000000, -1.000000000000000000 ) ) ;
#218395 = ADVANCED_FACE ( 'NONE', ( #233049 ), #53095, .T. ) ;
#218394 = DIRECTION ( 'NONE',  ( 1.000000000000000000, -0.000000000000000000, 0.000000000000000000 ) ) ;
#218396 = CARTESIAN_POINT ( 'NONE',  ( -18.59999999999999787, 64.35000000001208775, -129.5083017138703667 ) ) ;
#218398 = ADVANCED_FACE ( 'NONE', ( #149661 ), #50509, .F. ) ;
#218397 = VERTEX_POINT ( 'NONE', #49250 ) ;
#218399 = LINE ( 'NONE', #39817, #154886 ) ;
#218400 = CARTESIAN_POINT ( 'NONE',  ( 21.05000000000000071, 76.00000000001173817, -72.42310748452430857 ) ) ;
#218401 = VECTOR ( 'NONE', #145937, 1000.000000000000000 ) ;
#218402 = ORIENTED_EDGE ( 'NONE', *, *, #182810, .T. ) ;
#218403 = CIRCLE ( 'NONE', #160194, 0.09999999999999939493 ) ;
#218405 = ORIENTED_EDGE ( 'NONE', *, *, #98773, .T. ) ;
#218404 = CIRCLE ( 'NONE', #156108, 0.1000000000000001027 ) ;
#218406 = ADVANCED_FACE ( 'NONE', ( #208351 ), #210892, .T. ) ;
#218407 = ORIENTED_EDGE ( 'NONE', *, *, #230112, .F. ) ;
#218408 = TOROIDAL_SURFACE ( 'NONE', #251758, 4.099999999999999645, 0.1000000000000000056 ) ;
#218409 = AXIS2_PLACEMENT_3D ( 'NONE', #60799, #118224, #197753 ) ;
#218410 = EDGE_LOOP ( 'NONE', ( #234857, #181704, #247664, #121410 ) ) ;
#218413 = ORIENTED_EDGE ( 'NONE', *, *, #51699, .T. ) ;
#218412 = CARTESIAN_POINT ( 'NONE',  ( -21.05000000000000071, 11.75000000001115552, -59.98519422934605672 ) ) ;
#218411 =( BOUNDED_CURVE ( )  B_SPLINE_CURVE ( 3, ( #156079, #139004, #99883, #179479 ),
 .UNSPECIFIED., .F., .F. ) 
 B_SPLINE_CURVE_WITH_KNOTS ( ( 4, 4 ),
 ( 3.192897208853993529, 4.712388980384689674 ),
 .UNSPECIFIED. ) 
 CURVE ( )  GEOMETRIC_REPRESENTATION_ITEM ( )  RATIONAL_B_SPLINE_CURVE ( ( 1.000000000000000000, 0.8166740347213228279, 0.8166740347213228279, 1.000000000000000000 ) ) 
 REPRESENTATION_ITEM ( '' )  );
#218415 = CIRCLE ( 'NONE', #126684, 0.09999999999999864553 ) ;
#218414 = CARTESIAN_POINT ( 'NONE',  ( -21.05000000000000071, 34.17451268998649283, -243.7608519714916326 ) ) ;
#218416 = DIRECTION ( 'NONE',  ( 0.000000000000000000, 0.000000000000000000, -1.000000000000000000 ) ) ;
#218417 = CYLINDRICAL_SURFACE ( 'NONE', #222688, 0.1000000000000028644 ) ;
#218418 = AXIS2_PLACEMENT_3D ( 'NONE', #54056, #34522, #150604 ) ;
#218419 = DIRECTION ( 'NONE',  ( 0.7071067811865474617, 0.7071067811865474617, -0.000000000000000000 ) ) ;
#218420 = AXIS2_PLACEMENT_3D ( 'NONE', #219360, #38186, #152036 ) ;
#218423 = EDGE_LOOP ( 'NONE', ( #116729, #187364, #128532, #109818 ) ) ;
#218422 = EDGE_CURVE ( 'NONE', #70430, #185866, #133916, .T. ) ;
#218421 = DIRECTION ( 'NONE',  ( 0.000000000000000000, 0.8814952561688425003, -0.4721928772777359007 ) ) ;
#218425 = ORIENTED_EDGE ( 'NONE', *, *, #229768, .T. ) ;
#218424 = CARTESIAN_POINT ( 'NONE',  ( 18.54999999999999716, 67.25000000001229239, -160.7731074845244166 ) ) ;
#218426 = DIRECTION ( 'NONE',  ( -0.000000000000000000, -6.982962677686266711E-15, 1.000000000000000000 ) ) ;
#218427 = VECTOR ( 'NONE', #131043, 1000.000000000000000 ) ;
#218428 = ORIENTED_EDGE ( 'NONE', *, *, #15350, .T. ) ;
#218429 = VERTEX_POINT ( 'NONE', #51796 ) ;
#218430 = EDGE_CURVE ( 'NONE', #32118, #252758, #168245, .T. ) ;
#218431 = DIRECTION ( 'NONE',  ( 0.000000000000000000, 6.982962677686266711E-15, -1.000000000000000000 ) ) ;
#218432 = LINE ( 'NONE', #167188, #126231 ) ;
#218433 = VECTOR ( 'NONE', #127693, 1000.000000000000000 ) ;
#218434 = DIRECTION ( 'NONE',  ( -1.000000000000000000, 7.801181613359271466E-16, 1.456333823655509297E-15 ) ) ;
#218435 = DIRECTION ( 'NONE',  ( 0.000000000000000000, -0.4088369013363281068, 0.9126074666063770380 ) ) ;
#218436 = FACE_OUTER_BOUND ( 'NONE', #191019, .T. ) ;
#218437 = AXIS2_PLACEMENT_3D ( 'NONE', #81092, #64119, #144916 ) ;
#218439 = EDGE_CURVE ( 'NONE', #252677, #42291, #76613, .T. ) ;
#218438 = LINE ( 'NONE', #162358, #165679 ) ;
#218440 = EDGE_CURVE ( 'NONE', #37642, #196167, #205799, .T. ) ;
#218441 = DIRECTION ( 'NONE',  ( -1.000000000000000000, 2.952720810173289112E-16, 2.061873921506763405E-30 ) ) ;
#218442 = VECTOR ( 'NONE', #117852, 1000.000000000000000 ) ;
#218443 = ORIENTED_EDGE ( 'NONE', *, *, #206567, .F. ) ;
#218444 = ORIENTED_EDGE ( 'NONE', *, *, #223029, .F. ) ;
#218445 = CARTESIAN_POINT ( 'NONE',  ( 23.14999999999999858, 71.22429906543278832, -148.3718755885703331 ) ) ;
#218446 = EDGE_CURVE ( 'NONE', #51379, #204053, #109213, .T. ) ;
#218447 = ORIENTED_EDGE ( 'NONE', *, *, #93583, .F. ) ;
#218448 = DIRECTION ( 'NONE',  ( 0.000000000000000000, 0.000000000000000000, -1.000000000000000000 ) ) ;
#218450 = AXIS2_PLACEMENT_3D ( 'NONE', #157679, #57221, #136772 ) ;
#218449 = DIRECTION ( 'NONE',  ( 0.000000000000000000, 0.000000000000000000, -1.000000000000000000 ) ) ;
#218451 = VECTOR ( 'NONE', #236827, 1000.000000000000114 ) ;
#218452 = CARTESIAN_POINT ( 'NONE',  ( 18.49999999999999289, 65.79142135624952914, -148.6731074845244223 ) ) ;
#218453 = CARTESIAN_POINT ( 'NONE',  ( 18.59999999999999076, 10.20857864377385127, -188.8499999999999659 ) ) ;
#218454 = ORIENTED_EDGE ( 'NONE', *, *, #207303, .F. ) ;
#218455 = DIRECTION ( 'NONE',  ( 0.000000000000000000, -0.9126074666063771490, -0.4088369013363278293 ) ) ;
#218456 = EDGE_LOOP ( 'NONE', ( #232218, #203799, #162821, #132166 ) ) ;
#218457 = EDGE_CURVE ( 'NONE', #242609, #164375, #250021, .T. ) ;
#218458 = FACE_OUTER_BOUND ( 'NONE', #12025, .T. ) ;
#218459 = ORIENTED_EDGE ( 'NONE', *, *, #128120, .T. ) ;
#218460 = DIRECTION ( 'NONE',  ( 0.000000000000000000, -0.9651348961777157509, 0.2617529984165031243 ) ) ;
#218461 = EDGE_CURVE ( 'NONE', #234608, #131461, #30858, .T. ) ;
#218462 = FACE_OUTER_BOUND ( 'NONE', #27349, .T. ) ;
#218463 = VERTEX_POINT ( 'NONE', #110501 ) ;
#218464 = DIRECTION ( 'NONE',  ( 0.000000000000000000, -6.982962677686266711E-15, 1.000000000000000000 ) ) ;
#218466 = ORIENTED_EDGE ( 'NONE', *, *, #52238, .F. ) ;
#218465 = FACE_OUTER_BOUND ( 'NONE', #85436, .T. ) ;
#218467 = DIRECTION ( 'NONE',  ( 0.000000000000000000, 0.2617529984165152257, 0.9651348961777124202 ) ) ;
#218468 = AXIS2_PLACEMENT_3D ( 'NONE', #153, #122711, #100517 ) ;
#218469 = VERTEX_POINT ( 'NONE', #132650 ) ;
#218470 = AXIS2_PLACEMENT_3D ( 'NONE', #241468, #159373, #81083 ) ;
#218471 = CARTESIAN_POINT ( 'NONE',  ( 20.94999999999999929, 71.00000000001199396, -115.0283735034374359 ) ) ;
#218472 = ORIENTED_EDGE ( 'NONE', *, *, #62645, .T. ) ;
#218473 = DIRECTION ( 'NONE',  ( -3.787827842127535236E-15, 0.7397360091702777085, 0.6728971962616808744 ) ) ;
#218474 = FACE_OUTER_BOUND ( 'NONE', #170679, .T. ) ;
#218475 = CARTESIAN_POINT ( 'NONE',  ( -18.59999999999999787, -9.480686695267820596, -207.9411151687578183 ) ) ;
#218476 = LINE ( 'NONE', #180663, #181193 ) ;
#218477 = CARTESIAN_POINT ( 'NONE',  ( -20.54999999999999716, 6.268811756569107274, -220.3853799378769622 ) ) ;
#218478 = ORIENTED_EDGE ( 'NONE', *, *, #67020, .F. ) ;
#218479 = CARTESIAN_POINT ( 'NONE',  ( -18.50000000000000000, 76.00000000001195133, -103.0231074845243171 ) ) ;
#218480 = CARTESIAN_POINT ( 'NONE',  ( -17.22361732159832215, 42.80650589791834193, -235.4613000926810855 ) ) ;
#218481 = CARTESIAN_POINT ( 'NONE',  ( 20.94999999999999929, 1.115600667400684642E-11, -102.5000000000000426 ) ) ;
#218482 = ORIENTED_EDGE ( 'NONE', *, *, #3501, .T. ) ;
#218483 = CARTESIAN_POINT ( 'NONE',  ( 21.93340585972025636, 7.156391548293796312, -199.4414142243540766 ) ) ;
#218484 = VERTEX_POINT ( 'NONE', #247449 ) ;
#218485 = VERTEX_POINT ( 'NONE', #131351 ) ;
#218486 = VECTOR ( 'NONE', #103989, 1000.000000000000000 ) ;
#218487 = STYLED_ITEM ( 'NONE', ( #43367 ), #198047 ) ;
#218488 = DIRECTION ( 'NONE',  ( -1.000000000000000000, -0.000000000000000000, 0.000000000000000000 ) ) ;
#218489 = CARTESIAN_POINT ( 'NONE',  ( -20.94999999999999929, 10.29270135741298731, -72.45736188715193293 ) ) ;
#218491 = ORIENTED_EDGE ( 'NONE', *, *, #104950, .F. ) ;
#218490 = CARTESIAN_POINT ( 'NONE',  ( 20.94999999999999929, 85.00000000001222134, -146.4170766071767389 ) ) ;
#218492 = DIRECTION ( 'NONE',  ( 1.000000000000000000, -0.000000000000000000, -0.000000000000000000 ) ) ;
#218493 = VERTEX_POINT ( 'NONE', #32286 ) ;
#218494 = DIRECTION ( 'NONE',  ( -0.000000000000000000, 1.000000000000000000, 2.891205793294679805E-16 ) ) ;
#218495 = DIRECTION ( 'NONE',  ( -1.000000000000000000, -0.000000000000000000, -0.000000000000000000 ) ) ;
#218496 = ORIENTED_EDGE ( 'NONE', *, *, #214781, .F. ) ;
#218497 = VERTEX_POINT ( 'NONE', #111806 ) ;
#218498 = DIRECTION ( 'NONE',  ( -3.265361837132813093E-16, -1.000000000000000000, -6.938893903907229955E-15 ) ) ;
#218500 = EDGE_CURVE ( 'NONE', #51561, #200730, #51641, .T. ) ;
#218499 = DIRECTION ( 'NONE',  ( 0.000000000000000000, -0.4999999999999478195, -0.8660254037844686836 ) ) ;
#218501 = ORIENTED_EDGE ( 'NONE', *, *, #144710, .F. ) ;
#218503 = CARTESIAN_POINT ( 'NONE',  ( 21.05000000000000071, 9.997527148596399016, -228.1702915402975407 ) ) ;
#218502 = AXIS2_PLACEMENT_3D ( 'NONE', #54294, #175561, #77700 ) ;
#218504 = CIRCLE ( 'NONE', #243468, 0.5000000000000004441 ) ;
#218505 = ORIENTED_EDGE ( 'NONE', *, *, #184387, .F. ) ;
#218506 = VERTEX_POINT ( 'NONE', #231755 ) ;
#218507 = AXIS2_PLACEMENT_3D ( 'NONE', #209419, #251100, #195022 ) ;
#218508 = DIRECTION ( 'NONE',  ( 0.000000000000000000, 0.000000000000000000, -1.000000000000000000 ) ) ;
#218509 = EDGE_CURVE ( 'NONE', #17154, #26810, #10131, .T. ) ;
#218511 = ORIENTED_EDGE ( 'NONE', *, *, #196082, .T. ) ;
#218510 = DIRECTION ( 'NONE',  ( 0.000000000000000000, -1.000000000000000000, 0.000000000000000000 ) ) ;
#218512 = EDGE_CURVE ( 'NONE', #257268, #123284, #118327, .T. ) ;
#218513 = DIRECTION ( 'NONE',  ( 0.000000000000000000, 0.000000000000000000, -1.000000000000000000 ) ) ;
#218514 = EDGE_CURVE ( 'NONE', #142484, #69302, #151669, .T. ) ;
#218515 = FACE_OUTER_BOUND ( 'NONE', #30489, .T. ) ;
#218516 = DIRECTION ( 'NONE',  ( -0.7071067811865475727, -0.7071067811865475727, 0.000000000000000000 ) ) ;
#218518 = DIRECTION ( 'NONE',  ( 1.000000000000000000, 0.000000000000000000, -0.000000000000000000 ) ) ;
#218517 = LINE ( 'NONE', #93449, #110940 ) ;
#218519 = DIRECTION ( 'NONE',  ( -5.603264701231743991E-32, -7.172728831056617961E-15, 1.000000000000000000 ) ) ;
#218520 = DIRECTION ( 'NONE',  ( -1.000000000000000000, 0.000000000000000000, 0.000000000000000000 ) ) ;
#218521 = CARTESIAN_POINT ( 'NONE',  ( 18.49505816908824229, 85.43787255322250473, -29.24545028285334780 ) ) ;
#218522 = AXIS2_PLACEMENT_3D ( 'NONE', #99887, #180751, #156083 ) ;
#218523 = CARTESIAN_POINT ( 'NONE',  ( -20.94999999999999929, 70.10000000001267040, -193.3040077198679967 ) ) ;
#218524 = AXIS2_PLACEMENT_3D ( 'NONE', #65190, #6497, #92449 ) ;
#218525 = ORIENTED_EDGE ( 'NONE', *, *, #213624, .T. ) ;
#218526 = VECTOR ( 'NONE', #217877, 1000.000000000000000 ) ;
#218527 = VECTOR ( 'NONE', #104206, 1000.000000000000000 ) ;
#218529 = ORIENTED_EDGE ( 'NONE', *, *, #225781, .F. ) ;
#218528 = DIRECTION ( 'NONE',  ( 0.000000000000000000, 0.000000000000000000, 1.000000000000000000 ) ) ;
#218531 = VERTEX_POINT ( 'NONE', #113083 ) ;
#218530 = B_SPLINE_CURVE_WITH_KNOTS ( 'NONE', 3,
 ( #45222, #25670, #203007, #143016, #102594, #183462, #3518, #246000, #242133, #4785, #47768, #105147, #68650, #63490, #88168, #222556 ),
 .UNSPECIFIED., .F., .F.,
 ( 4, 3, 3, 3, 3, 4 ),
 ( 0.000000000000000000, 2.372700795694925591E-05, 5.739057815867077772E-05, 9.073899019181627494E-05, 0.0001243544287365772689, 0.0001585386695601308422 ),
 .UNSPECIFIED. ) ;
#218532 = ADVANCED_FACE ( 'NONE', ( #192622 ), #13989, .F. ) ;
#218533 = FACE_OUTER_BOUND ( 'NONE', #36290, .T. ) ;
#218534 = ORIENTED_EDGE ( 'NONE', *, *, #228730, .T. ) ;
#218535 = CARTESIAN_POINT ( 'NONE',  ( 21.00000000000000000, 43.85220609964365224, -235.6449878604632886 ) ) ;
#218536 = AXIS2_PLACEMENT_3D ( 'NONE', #252704, #35003, #234427 ) ;
#218537 = CIRCLE ( 'NONE', #14589, 0.1000000000000096922 ) ;
#218538 = ORIENTED_EDGE ( 'NONE', *, *, #60314, .F. ) ;
#218539 = AXIS2_PLACEMENT_3D ( 'NONE', #257207, #99445, #179047 ) ;
#218540 = SURFACE_STYLE_USAGE ( .BOTH. , #204120 ) ;
#218541 = DIRECTION ( 'NONE',  ( 0.000000000000000000, 0.000000000000000000, 1.000000000000000000 ) ) ;
#218542 = CIRCLE ( 'NONE', #39552, 0.1000000000000013933 ) ;
#218544 = EDGE_LOOP ( 'NONE', ( #42327, #153713, #168835, #233676 ) ) ;
#218543 = VERTEX_POINT ( 'NONE', #255098 ) ;
#218545 = ORIENTED_EDGE ( 'NONE', *, *, #137543, .T. ) ;
#218546 = ORIENTED_EDGE ( 'NONE', *, *, #213233, .T. ) ;
#218548 = DIRECTION ( 'NONE',  ( 1.000000000000000000, 0.000000000000000000, 0.000000000000000000 ) ) ;
#218547 = CIRCLE ( 'NONE', #89568, 0.09999999999998898659 ) ;
#218549 = DIRECTION ( 'NONE',  ( 0.000000000000000000, 0.000000000000000000, 1.000000000000000000 ) ) ;
#218551 = EDGE_LOOP ( 'NONE', ( #207831, #60073, #143084, #203873 ) ) ;
#218550 = DIRECTION ( 'NONE',  ( 1.000000000000000000, 0.000000000000000000, 0.000000000000000000 ) ) ;
#218552 = EDGE_CURVE ( 'NONE', #8033, #2147, #140324, .T. ) ;
#218553 = CIRCLE ( 'NONE', #47871, 0.09999999999999939493 ) ;
#218554 = EDGE_CURVE ( 'NONE', #142448, #64371, #72541, .T. ) ;
#218555 = DIRECTION ( 'NONE',  ( -0.000000000000000000, 0.000000000000000000, -1.000000000000000000 ) ) ;
#218556 = DIRECTION ( 'NONE',  ( 1.000000000000000000, 0.000000000000000000, 0.000000000000000000 ) ) ;
#218558 = ORIENTED_EDGE ( 'NONE', *, *, #79863, .F. ) ;
#218557 = FACE_OUTER_BOUND ( 'NONE', #54696, .T. ) ;
#218559 = CYLINDRICAL_SURFACE ( 'NONE', #178653, 0.09999999999998898659 ) ;
#218560 = ORIENTED_EDGE ( 'NONE', *, *, #112314, .T. ) ;
#218561 = CIRCLE ( 'NONE', #255948, 2.100000000000002309 ) ;
#218562 = DIRECTION ( 'NONE',  ( 0.000000000000000000, -1.000000000000000000, -0.000000000000000000 ) ) ;
#218563 = CIRCLE ( 'NONE', #122925, 0.1000000000000124678 ) ;
#218565 = ORIENTED_EDGE ( 'NONE', *, *, #70406, .T. ) ;
#218564 = CARTESIAN_POINT ( 'NONE',  ( 21.14999999999999858, 1.115600667400684642E-11, -60.45934304829879835 ) ) ;
#218566 = DIRECTION ( 'NONE',  ( 1.000000000000000000, 0.000000000000000000, 0.000000000000000000 ) ) ;
#218567 = CARTESIAN_POINT ( 'NONE',  ( -20.65000000000000568, 70.35000000001190301, -93.77310748452434552 ) ) ;
#218569 = EDGE_CURVE ( 'NONE', #62106, #243885, #218238, .T. ) ;
#218568 = CARTESIAN_POINT ( 'NONE',  ( 21.05000000000000071, 10.48443348965288635, -74.45680580149196715 ) ) ;
#218570 = ORIENTED_EDGE ( 'NONE', *, *, #32436, .F. ) ;
#218572 = CARTESIAN_POINT ( 'NONE',  ( -16.88815647973234135, 44.13260157173010612, -235.2993095192094870 ) ) ;
#218571 = CARTESIAN_POINT ( 'NONE',  ( -16.85722902420150149, 9.950000000011138823, -46.26554747377067400 ) ) ;
#218573 = CARTESIAN_POINT ( 'NONE',  ( -12.68215100488890279, 66.60336962369413527, -85.11605009170608582 ) ) ;
#218574 = CARTESIAN_POINT ( 'NONE',  ( 18.41815437325346494, 85.49870985315384075, -163.4191616457223404 ) ) ;
#218575 = CARTESIAN_POINT ( 'NONE',  ( -20.64999999999999858, 1.115600667400684642E-11, -33.50000000000000000 ) ) ;
#218576 = LINE ( 'NONE', #161201, #142749 ) ;
#218577 = ORIENTED_EDGE ( 'NONE', *, *, #24733, .T. ) ;
#218578 = ORIENTED_EDGE ( 'NONE', *, *, #95062, .F. ) ;
#218579 = VERTEX_POINT ( 'NONE', #19104 ) ;
#218580 = CARTESIAN_POINT ( 'NONE',  ( 18.49999999999999289, 19.81721122307411420, -227.1998943584050039 ) ) ;
#218581 = ORIENTED_EDGE ( 'NONE', *, *, #184450, .F. ) ;
#218582 = LINE ( 'NONE', #196463, #226616 ) ;
#218583 = VERTEX_POINT ( 'NONE', #136465 ) ;
#218584 = DIRECTION ( 'NONE',  ( 1.000000000000000000, -0.000000000000000000, -0.000000000000000000 ) ) ;
#218585 = FACE_OUTER_BOUND ( 'NONE', #206080, .T. ) ;
#218586 = AXIS2_PLACEMENT_3D ( 'NONE', #226431, #106479, #210747 ) ;
#218587 = TOROIDAL_SURFACE ( 'NONE', #168598, 2.699999999999999734, 0.1000000000000000056 ) ;
#218588 = ORIENTED_EDGE ( 'NONE', *, *, #91006, .T. ) ;
#218589 = FACE_OUTER_BOUND ( 'NONE', #202161, .T. ) ;
#218590 = AXIS2_PLACEMENT_3D ( 'NONE', #92417, #169443, #109409 ) ;
#218591 = ORIENTED_EDGE ( 'NONE', *, *, #36816, .F. ) ;
#218592 = ORIENTED_EDGE ( 'NONE', *, *, #119745, .F. ) ;
#218593 = ORIENTED_EDGE ( 'NONE', *, *, #212096, .T. ) ;
#218594 = AXIS2_PLACEMENT_3D ( 'NONE', #137045, #159198, #178781 ) ;
#218595 = EDGE_CURVE ( 'NONE', #128950, #90426, #8062, .T. ) ;
#218596 = DIRECTION ( 'NONE',  ( 0.000000000000000000, -6.352154140967427193E-15, 1.000000000000000000 ) ) ;
#218597 = DIRECTION ( 'NONE',  ( 1.000000000000000000, 0.000000000000000000, 0.000000000000000000 ) ) ;
#218598 = AXIS2_PLACEMENT_3D ( 'NONE', #5316, #127874, #228263 ) ;
#218599 = DIRECTION ( 'NONE',  ( 1.000000000000000000, 0.000000000000000000, 0.000000000000000000 ) ) ;
#218600 = EDGE_CURVE ( 'NONE', #168958, #17700, #55630, .T. ) ;
#218601 = CARTESIAN_POINT ( 'NONE',  ( -23.25000000000000000, 87.65000000001246860, -181.7731074845242745 ) ) ;
#218602 = CARTESIAN_POINT ( 'NONE',  ( 14.88075390448864788, 66.56831044948793874, -118.2438174522883116 ) ) ;
#218603 = CARTESIAN_POINT ( 'NONE',  ( -23.15000000000000213, 68.69170246065380070, -214.2335597194317813 ) ) ;
#218604 = DIRECTION ( 'NONE',  ( 0.000000000000000000, 1.000000000000000000, 6.982962677686266711E-15 ) ) ;
#218606 = ORIENTED_EDGE ( 'NONE', *, *, #94963, .T. ) ;
#218605 = CARTESIAN_POINT ( 'NONE',  ( -23.49999999999994316, 83.90000000001120384, -34.77310748452479316 ) ) ;
#218607 = DIRECTION ( 'NONE',  ( 0.000000000000000000, -0.4721928772777350125, -0.8814952561688429444 ) ) ;
#218608 = ORIENTED_EDGE ( 'NONE', *, *, #218926, .F. ) ;
#218609 = EDGE_CURVE ( 'NONE', #252739, #92180, #105815, .T. ) ;
#218610 = CARTESIAN_POINT ( 'NONE',  ( -18.50000000000001066, -9.421308209727802918, -141.2423632140505561 ) ) ;
#218611 = EDGE_CURVE ( 'NONE', #191682, #201217, #172537, .T. ) ;
#218612 = ORIENTED_EDGE ( 'NONE', *, *, #125890, .T. ) ;
#218613 = ORIENTED_EDGE ( 'NONE', *, *, #135847, .T. ) ;
#218614 = DIRECTION ( 'NONE',  ( -1.000000000000000000, 5.945622153099073960E-16, -5.981866248895714834E-16 ) ) ;
#218615 = CIRCLE ( 'NONE', #143614, 3.999999999999996447 ) ;
#218616 = DIRECTION ( 'NONE',  ( 1.000000000000000000, -0.000000000000000000, -0.000000000000000000 ) ) ;
#218617 = CARTESIAN_POINT ( 'NONE',  ( -16.87368910959167678, 66.03872618332016486, -56.91061438788380400 ) ) ;
#218618 = VERTEX_POINT ( 'NONE', #116929 ) ;
#218619 = CIRCLE ( 'NONE', #210274, 0.09999999999998898659 ) ;
#218620 = ADVANCED_FACE ( 'NONE', ( #38680 ), #14286, .T. ) ;
#218621 = EDGE_CURVE ( 'NONE', #31271, #211413, #193344, .T. ) ;
#218622 = DIRECTION ( 'NONE',  ( -1.000000000000000000, 0.000000000000000000, 0.000000000000000000 ) ) ;
#218624 = ADVANCED_FACE ( 'NONE', ( #197744 ), #21195, .T. ) ;
#218623 = EDGE_CURVE ( 'NONE', #200055, #236931, #234297, .T. ) ;
#218625 = EDGE_LOOP ( 'NONE', ( #232865, #179021, #4034, #157191, #182414 ) ) ;
#218626 = ORIENTED_EDGE ( 'NONE', *, *, #111579, .T. ) ;
#218627 = CARTESIAN_POINT ( 'NONE',  ( -18.50000000000000000, 63.24832102809784118, -245.4188802514362635 ) ) ;
#218628 = ORIENTED_EDGE ( 'NONE', *, *, #225965, .T. ) ;
#218629 = CARTESIAN_POINT ( 'NONE',  ( 20.00000000000000355, 5.552655413246002425, 16.61686199900910310 ) ) ;
#218630 = CARTESIAN_POINT ( 'NONE',  ( -18.59999999999999787, 2.319530388122570841, -217.8268657444419887 ) ) ;
#218631 = ORIENTED_EDGE ( 'NONE', *, *, #46203, .F. ) ;
#218632 = DIRECTION ( 'NONE',  ( -0.000000000000000000, 0.9910465087640865089, 0.1335171055202867274 ) ) ;
#218634 = ADVANCED_FACE ( 'NONE', ( #201589 ), #161197, .T. ) ;
#218633 = CIRCLE ( 'NONE', #168808, 0.1999999999999987899 ) ;
#218635 = CARTESIAN_POINT ( 'NONE',  ( 22.59999985501178799, 11.74986979301414181, -133.9344013302005294 ) ) ;
#218636 = EDGE_LOOP ( 'NONE', ( #22796, #83494, #161095, #99156 ) ) ;
#218637 = DIRECTION ( 'NONE',  ( 0.000000000000000000, 6.982962677686266711E-15, -1.000000000000000000 ) ) ;
#218638 = ADVANCED_FACE ( 'NONE', ( #24267 ), #182041, .T. ) ;
#218639 = DIRECTION ( 'NONE',  ( 0.000000000000000000, 1.000000000000000000, 0.000000000000000000 ) ) ;
#218640 = CARTESIAN_POINT ( 'NONE',  ( -22.42253884134832376, 26.02661726287391986, -254.3121879182652663 ) ) ;
#218641 = EDGE_CURVE ( 'NONE', #166675, #57960, #181054, .T. ) ;
#218642 = EDGE_CURVE ( 'NONE', #69695, #58185, #213085, .T. ) ;
#218643 = AXIS2_PLACEMENT_3D ( 'NONE', #17188, #97958, #156 ) ;
#218644 = ORIENTED_EDGE ( 'NONE', *, *, #216870, .F. ) ;
#218645 = CIRCLE ( 'NONE', #160247, 0.1999999999999987899 ) ;
#218646 = EDGE_CURVE ( 'NONE', #115616, #196105, #251771, .T. ) ;
#218648 = EDGE_LOOP ( 'NONE', ( #18805, #104037, #220023, #38432 ) ) ;
#218647 = CARTESIAN_POINT ( 'NONE',  ( -21.04999999999994387, 74.73834681386826162, -44.00978271863746016 ) ) ;
#218649 = ORIENTED_EDGE ( 'NONE', *, *, #187537, .F. ) ;
#218650 = CARTESIAN_POINT ( 'NONE',  ( 21.13461538461538325, 67.11458296203758778, -124.1731074845243512 ) ) ;
#218651 = CARTESIAN_POINT ( 'NONE',  ( -22.49436431346200038, 12.57088205413893434, -223.4317334472834489 ) ) ;
#218652 = DIRECTION ( 'NONE',  ( -0.7071067811865217045, 0.3338907855512895928, 0.6233112732206752549 ) ) ;
#218653 = EDGE_CURVE ( 'NONE', #198535, #166946, #51840, .T. ) ;
#218654 = DIRECTION ( 'NONE',  ( 0.000000000000000000, 0.000000000000000000, 1.000000000000000000 ) ) ;
#218655 = DIRECTION ( 'NONE',  ( 0.000000000000000000, 0.000000000000000000, -1.000000000000000000 ) ) ;
#218656 = ORIENTED_EDGE ( 'NONE', *, *, #253117, .F. ) ;
#218657 = DIRECTION ( 'NONE',  ( 0.000000000000000000, 6.982962677686266711E-15, -1.000000000000000000 ) ) ;
#218658 = CARTESIAN_POINT ( 'NONE',  ( 20.94999999999999929, -9.399999999988844834, -124.1060308773475924 ) ) ;
#218660 = ADVANCED_FACE ( 'NONE', ( #224984 ), #101159, .T. ) ;
#218659 = FACE_OUTER_BOUND ( 'NONE', #17577, .T. ) ;
#218661 = CARTESIAN_POINT ( 'NONE',  ( 22.00356870140399579, 7.254242362511003961, -134.0000000000000000 ) ) ;
#218662 = AXIS2_PLACEMENT_3D ( 'NONE', #25531, #65931, #28112 ) ;
#218663 = CARTESIAN_POINT ( 'NONE',  ( 20.51284917709620359, 65.68911337716694732, -61.85063429893225617 ) ) ;
#218664 = EDGE_LOOP ( 'NONE', ( #189681, #19255, #250469, #237148 ) ) ;
#218665 = ORIENTED_EDGE ( 'NONE', *, *, #213310, .T. ) ;
#218666 = DIRECTION ( 'NONE',  ( 0.000000000000000000, -7.172728831056617961E-15, 1.000000000000000000 ) ) ;
#218667 = DIRECTION ( 'NONE',  ( 0.000000000000000000, -0.4999999999999949485, 0.8660254037844415942 ) ) ;
#218668 = DIRECTION ( 'NONE',  ( -1.000000000000000000, -2.952720810173289112E-16, 0.000000000000000000 ) ) ;
#218670 = CARTESIAN_POINT ( 'NONE',  ( 21.05000000000000071, 58.88775506787933978, -225.6504858384382999 ) ) ;
#218669 = AXIS2_PLACEMENT_3D ( 'NONE', #65082, #190181, #207178 ) ;
#218671 = CARTESIAN_POINT ( 'NONE',  ( -16.90137573187933739, 23.10008176225494481, -231.0004231328723563 ) ) ;
#218672 = EDGE_CURVE ( 'NONE', #79058, #193922, #31058, .T. ) ;
#218673 = ORIENTED_EDGE ( 'NONE', *, *, #154586, .F. ) ;
#218674 = FACE_OUTER_BOUND ( 'NONE', #233740, .T. ) ;
#218675 = LINE ( 'NONE', #4749, #142380 ) ;
#218676 = DIRECTION ( 'NONE',  ( 0.000000000000000000, 6.938893903907222067E-15, -1.000000000000000000 ) ) ;
#218677 = LINE ( 'NONE', #62198, #137105 ) ;
#218678 = VECTOR ( 'NONE', #222665, 1000.000000000000000 ) ;
#218679 = VECTOR ( 'NONE', #217672, 1000.000000000000000 ) ;
#218680 = ORIENTED_EDGE ( 'NONE', *, *, #235354, .T. ) ;
#218681 = CARTESIAN_POINT ( 'NONE',  ( -20.95613430942382749, 12.94008388437452162, -205.1996914945986248 ) ) ;
#218682 = ORIENTED_EDGE ( 'NONE', *, *, #199673, .T. ) ;
#218683 = FACE_OUTER_BOUND ( 'NONE', #16113, .T. ) ;
#218684 = CARTESIAN_POINT ( 'NONE',  ( 18.49999999999999289, 11.75000000001115907, -142.1000000000000227 ) ) ;
#218685 = DIRECTION ( 'NONE',  ( -1.000000000000000000, 0.000000000000000000, 0.000000000000000000 ) ) ;
#218686 = DIRECTION ( 'NONE',  ( -1.000000000000000000, 0.000000000000000000, 0.000000000000000000 ) ) ;
#218687 = CARTESIAN_POINT ( 'NONE',  ( -20.07928932188135107, 9.220710678129810489, -88.25000000000005684 ) ) ;
#218688 = CARTESIAN_POINT ( 'NONE',  ( 21.05000000000000071, 85.00000000001197975, -112.9170766071766820 ) ) ;
#218689 = DIRECTION ( 'NONE',  ( -0.000000000000000000, -0.000000000000000000, 1.000000000000000000 ) ) ;
#218690 = CARTESIAN_POINT ( 'NONE',  ( 23.24999999999999289, 11.65000000001116298, -122.2500000000000284 ) ) ;
#218691 = EDGE_CURVE ( 'NONE', #146731, #59304, #162491, .T. ) ;
#218692 = DIRECTION ( 'NONE',  ( 0.000000000000000000, -6.982962677686266711E-15, 1.000000000000000000 ) ) ;
#218693 = DIRECTION ( 'NONE',  ( -2.940209281316621016E-16, 1.000000000000000000, -4.704334850106593625E-15 ) ) ;
#218694 = DIRECTION ( 'NONE',  ( 0.000000000000000000, 0.000000000000000000, -1.000000000000000000 ) ) ;
#218695 = AXIS2_PLACEMENT_3D ( 'NONE', #192249, #17152, #160517 ) ;
#218696 = EDGE_CURVE ( 'NONE', #177630, #231520, #106321, .T. ) ;
#218697 = AXIS2_PLACEMENT_3D ( 'NONE', #3893, #199553, #164267 ) ;
#218698 = LINE ( 'NONE', #25660, #245389 ) ;
#218700 = DIRECTION ( 'NONE',  ( -0.000000000000000000, 0.7397360091702708251, 0.6728971962616883129 ) ) ;
#218699 = CIRCLE ( 'NONE', #256238, 0.09999999999999105438 ) ;
#218701 = AXIS2_PLACEMENT_3D ( 'NONE', #117502, #78359, #35433 ) ;
#218702 = ORIENTED_EDGE ( 'NONE', *, *, #6927, .F. ) ;
#218703 = CARTESIAN_POINT ( 'NONE',  ( -20.00857864376270001, 63.83985267992358104, -213.0213082169670145 ) ) ;
#218705 = EDGE_CURVE ( 'NONE', #53755, #170769, #126873, .T. ) ;
#218704 = CARTESIAN_POINT ( 'NONE',  ( 20.94999999999999929, 17.06838326776701109, -224.6250846885016870 ) ) ;
#218706 = CARTESIAN_POINT ( 'NONE',  ( 20.58091095332318332, 9.018470153363930208, -41.91865018215837324 ) ) ;
#218707 = EDGE_CURVE ( 'NONE', #79203, #211510, #26946, .T. ) ;
#218708 = ORIENTED_EDGE ( 'NONE', *, *, #66941, .F. ) ;
#218709 = DIRECTION ( 'NONE',  ( 1.000000000000000000, 0.000000000000000000, 0.000000000000000000 ) ) ;
#218710 = CARTESIAN_POINT ( 'NONE',  ( 18.59999999999999076, 30.76917518201224055, -234.8152055956155380 ) ) ;
#218711 = VERTEX_POINT ( 'NONE', #222409 ) ;
#218712 = CARTESIAN_POINT ( 'NONE',  ( 22.57320508075688892, 31.85509083104287598, -238.8280249686205536 ) ) ;
#218713 = ORIENTED_EDGE ( 'NONE', *, *, #179627, .T. ) ;
#218714 = AXIS2_PLACEMENT_3D ( 'NONE', #115882, #31252, #95021 ) ;
#218715 = CIRCLE ( 'NONE', #139604, 2.100000000000004530 ) ;
#218716 = EDGE_CURVE ( 'NONE', #140173, #53539, #43813, .T. ) ;
#218717 = AXIS2_PLACEMENT_3D ( 'NONE', #9943, #105142, #206860 ) ;
#218718 = VERTEX_POINT ( 'NONE', #232736 ) ;
#218719 = DIRECTION ( 'NONE',  ( 1.186688945009010077E-16, -1.000000000000000000, -0.000000000000000000 ) ) ;
#218720 = EDGE_LOOP ( 'NONE', ( #232625, #85177, #168258, #251104 ) ) ;
#218721 = DIRECTION ( 'NONE',  ( 0.000000000000000000, 0.000000000000000000, -1.000000000000000000 ) ) ;
#218723 = AXIS2_PLACEMENT_3D ( 'NONE', #100687, #204941, #202396 ) ;
#218722 = CARTESIAN_POINT ( 'NONE',  ( 21.12757541349815682, 34.00765740373876156, -243.6456173532155276 ) ) ;
#218725 = DIRECTION ( 'NONE',  ( 1.000000000000000000, 0.000000000000000000, 0.000000000000000000 ) ) ;
#218724 = AXIS2_PLACEMENT_3D ( 'NONE', #244704, #23131, #145604 ) ;
#218726 = AXIS2_PLACEMENT_3D ( 'NONE', #28059, #47573, #181973 ) ;
#218727 = DIRECTION ( 'NONE',  ( -4.336808689941752679E-15, 0.8660254037844482555, 0.4999999999999837907 ) ) ;
#218728 = DIRECTION ( 'NONE',  ( -0.000000000000000000, -0.000000000000000000, -1.000000000000000000 ) ) ;
#218729 = FACE_OUTER_BOUND ( 'NONE', #238807, .T. ) ;
#218730 = FACE_OUTER_BOUND ( 'NONE', #49795, .T. ) ;
#218732 = ORIENTED_EDGE ( 'NONE', *, *, #253753, .T. ) ;
#218731 = CARTESIAN_POINT ( 'NONE',  ( -18.59999996769639097, -9.363273769819228320, -40.68149391546575089 ) ) ;
#218733 = VERTEX_POINT ( 'NONE', #72378 ) ;
#218735 = CARTESIAN_POINT ( 'NONE',  ( -20.94999999999999929, 64.25000000001161027, -62.50830171387039513 ) ) ;
#218734 = CARTESIAN_POINT ( 'NONE',  ( 22.50927854361889047, -0.1008580735255082683, 11.74956712602691233 ) ) ;
#218738 = ORIENTED_EDGE ( 'NONE', *, *, #2504, .T. ) ;
#218737 = DIRECTION ( 'NONE',  ( -1.000000000000000000, 0.000000000000000000, 0.000000000000000000 ) ) ;
#218736 = CARTESIAN_POINT ( 'NONE',  ( 21.04999999999999716, 65.37127968600823635, -191.3731074845244109 ) ) ;
#218739 = ORIENTED_EDGE ( 'NONE', *, *, #185420, .F. ) ;
#218740 = EDGE_CURVE ( 'NONE', #154965, #117101, #170232, .T. ) ;
#218741 = DIRECTION ( 'NONE',  ( 0.000000000000000000, -0.000000000000000000, 1.000000000000000000 ) ) ;
#218742 = DIRECTION ( 'NONE',  ( -1.073024830501117725E-15, -0.000000000000000000, -1.000000000000000000 ) ) ;
#218743 = TOROIDAL_SURFACE ( 'NONE', #52158, 0.2000000000000000111, 0.1000000000000000056 ) ;
#218744 = CIRCLE ( 'NONE', #256284, 0.1000000000000051958 ) ;
#218745 = DIRECTION ( 'NONE',  ( 1.000000000000000000, 0.000000000000000000, -0.000000000000000000 ) ) ;
#218746 = PRESENTATION_STYLE_ASSIGNMENT (( #26686 ) ) ;
#218747 = LINE ( 'NONE', #143061, #156625 ) ;
#218748 = TOROIDAL_SURFACE ( 'NONE', #193834, 0.2000000000000000111, 0.1000000000000000056 ) ;
#218749 = DIRECTION ( 'NONE',  ( 1.186688945009010077E-16, -0.9770955615653315052, -0.2128009952263603954 ) ) ;
#218750 = AXIS2_PLACEMENT_3D ( 'NONE', #132513, #157236, #212062 ) ;
#218752 = EDGE_CURVE ( 'NONE', #8211, #97103, #129760, .T. ) ;
#218751 = CARTESIAN_POINT ( 'NONE',  ( 18.49999999999999289, 11.65000000000000036, -33.50000000000000000 ) ) ;
#218753 = EDGE_CURVE ( 'NONE', #100999, #77303, #193525, .T. ) ;
#218754 = DIRECTION ( 'NONE',  ( -4.336808689942053235E-15, -0.8660254037844482555, -0.4999999999999836797 ) ) ;
#218755 = EDGE_LOOP ( 'NONE', ( #252864, #118419, #113347, #207979 ) ) ;
#218756 = ORIENTED_EDGE ( 'NONE', *, *, #148181, .F. ) ;
#218757 = DIRECTION ( 'NONE',  ( -1.000000000000000000, -0.000000000000000000, -0.000000000000000000 ) ) ;
#218759 = ORIENTED_EDGE ( 'NONE', *, *, #222397, .T. ) ;
#218758 = B_SPLINE_CURVE_WITH_KNOTS ( 'NONE', 3,
 ( #133187, #212733, #34124, #113618, #94046, #17111, #253112 ),
 .UNSPECIFIED., .F., .F.,
 ( 4, 3, 4 ),
 ( 0.000000000000000000, 3.882884552234471334E-05, 5.798605692158473166E-05 ),
 .UNSPECIFIED. ) ;
#218760 = DIRECTION ( 'NONE',  ( 1.000000000000000000, 2.885090398161910739E-16, 6.283419270304611573E-17 ) ) ;
#218761 = ORIENTED_EDGE ( 'NONE', *, *, #11241, .F. ) ;
#218762 = DIRECTION ( 'NONE',  ( 1.000000000000000000, 0.000000000000000000, 0.000000000000000000 ) ) ;
#218763 = EDGE_CURVE ( 'NONE', #28813, #20729, #128483, .T. ) ;
#218764 = CARTESIAN_POINT ( 'NONE',  ( -12.33960340485503338, 48.63331072832804836, -233.9296379114950355 ) ) ;
#218765 = DIRECTION ( 'NONE',  ( 0.000000000000000000, -6.982962677686266711E-15, 1.000000000000000000 ) ) ;
#218766 = DIRECTION ( 'NONE',  ( 0.000000000000000000, -6.608470384673536035E-15, 1.000000000000000000 ) ) ;
#218767 = ADVANCED_FACE ( 'NONE', ( #231450 ), #105994, .T. ) ;
#218768 = LINE ( 'NONE', #137949, #187303 ) ;
#218769 = EDGE_LOOP ( 'NONE', ( #193171, #185933, #152126 ) ) ;
#218770 = ADVANCED_FACE ( 'NONE', ( #167630 ), #110113, .T. ) ;
#218771 = DIRECTION ( 'NONE',  ( 0.000000000000000000, 1.000000000000000000, 0.000000000000000000 ) ) ;
#218772 = CIRCLE ( 'NONE', #202236, 4.000000000000003553 ) ;
#218773 = DIRECTION ( 'NONE',  ( 1.000000000000000000, 0.000000000000000000, 0.000000000000000000 ) ) ;
#218774 = DIRECTION ( 'NONE',  ( 0.000000000000000000, 0.000000000000000000, -1.000000000000000000 ) ) ;
#218775 = AXIS2_PLACEMENT_3D ( 'NONE', #185783, #166254, #245764 ) ;
#218776 = CARTESIAN_POINT ( 'NONE',  ( -20.94999999999999929, 88.41227409416215721, -173.0231074845242745 ) ) ;
#218777 = ADVANCED_FACE ( 'NONE', ( #252263 ), #176777, .T. ) ;
#218778 = CYLINDRICAL_SURFACE ( 'NONE', #190769, 0.1000000000000028644 ) ;
#218779 = AXIS2_PLACEMENT_3D ( 'NONE', #195094, #114248, #213331 ) ;
#218780 = ORIENTED_EDGE ( 'NONE', *, *, #200676, .F. ) ;
#218781 = DIRECTION ( 'NONE',  ( -1.000000000000000000, -0.000000000000000000, 0.000000000000000000 ) ) ;
#218782 = ORIENTED_EDGE ( 'NONE', *, *, #209506, .T. ) ;
#218785 = ORIENTED_EDGE ( 'NONE', *, *, #84544, .F. ) ;
#218784 = FACE_OUTER_BOUND ( 'NONE', #228296, .T. ) ;
#218783 = DIRECTION ( 'NONE',  ( 1.000000000000000000, 0.000000000000000000, 0.000000000000000000 ) ) ;
#218786 = LINE ( 'NONE', #100109, #114565 ) ;
#218787 = VECTOR ( 'NONE', #28700, 999.9999999999998863 ) ;
#218788 = CARTESIAN_POINT ( 'NONE',  ( -23.25000000000000355, 28.17589918783267322, -238.5974746063260739 ) ) ;
#218789 = AXIS2_PLACEMENT_3D ( 'NONE', #153905, #134264, #174746 ) ;
#218790 = ORIENTED_EDGE ( 'NONE', *, *, #142385, .F. ) ;
#218791 = DIRECTION ( 'NONE',  ( 1.000000000000000000, 0.000000000000000000, 0.000000000000000000 ) ) ;
#218792 = EDGE_CURVE ( 'NONE', #145230, #240969, #6053, .T. ) ;
#218793 = DIRECTION ( 'NONE',  ( 1.000000000000000000, 0.000000000000000000, 0.000000000000000000 ) ) ;
#218794 = FACE_OUTER_BOUND ( 'NONE', #186904, .T. ) ;
#218795 = TOROIDAL_SURFACE ( 'NONE', #6988, 12.97499999999999609, 0.1000000000000000056 ) ;
#218796 = UNCERTAINTY_MEASURE_WITH_UNIT (LENGTH_MEASURE( 1.000000000000000082E-05 ), #159335, 'distance_accuracy_value', 'NONE');
#218798 = ORIENTED_EDGE ( 'NONE', *, *, #46503, .T. ) ;
#218797 = DIRECTION ( 'NONE',  ( 0.000000000000000000, 0.000000000000000000, 1.000000000000000000 ) ) ;
#218799 = VECTOR ( 'NONE', #68869, 1000.000000000000000 ) ;
#218800 = DIRECTION ( 'NONE',  ( 1.000000000000000000, 0.000000000000000000, 0.000000000000000000 ) ) ;
#218801 = CIRCLE ( 'NONE', #106370, 0.09999999999999939493 ) ;
#218802 = EDGE_LOOP ( 'NONE', ( #34897, #102090, #51182, #136336 ) ) ;
#218803 = CARTESIAN_POINT ( 'NONE',  ( -16.91256925476571382, 9.985731158139332209, -180.0323575109946717 ) ) ;
#218804 = CARTESIAN_POINT ( 'NONE',  ( -20.94999999999999929, 1.115600667400684642E-11, -134.0000000000000284 ) ) ;
#218805 = CARTESIAN_POINT ( 'NONE',  ( -16.77779411503079032, 44.14899187519263535, -235.2971511010943004 ) ) ;
#218806 = ORIENTED_EDGE ( 'NONE', *, *, #137376, .F. ) ;
#218807 = DIRECTION ( 'NONE',  ( 0.000000000000000000, -2.775557561562888827E-14, 1.000000000000000000 ) ) ;
#218808 = ORIENTED_EDGE ( 'NONE', *, *, #52879, .T. ) ;
#218809 = DIRECTION ( 'NONE',  ( 0.000000000000000000, 0.000000000000000000, 1.000000000000000000 ) ) ;
#218810 = CYLINDRICAL_SURFACE ( 'NONE', #97435, 1.749999999999998002 ) ;
#218811 = DIRECTION ( 'NONE',  ( 0.000000000000000000, 6.982962677686266711E-15, -1.000000000000000000 ) ) ;
#218812 = VECTOR ( 'NONE', #88611, 1000.000000000000000 ) ;
#218813 = ORIENTED_EDGE ( 'NONE', *, *, #144012, .F. ) ;
#218814 = DIRECTION ( 'NONE',  ( 0.000000000000000000, 6.982962677686267499E-15, -1.000000000000000000 ) ) ;
#218815 = DIRECTION ( 'NONE',  ( -1.000000000000000000, -0.000000000000000000, -0.000000000000000000 ) ) ;
#218816 = PLANE ( 'NONE',  #95900 ) ;
#218817 = ORIENTED_EDGE ( 'NONE', *, *, #57285, .T. ) ;
#218818 = CARTESIAN_POINT ( 'NONE',  ( 15.48841904831874849, 67.43841904833064405, -90.37310748452436826 ) ) ;
#218819 = LINE ( 'NONE', #119758, #85865 ) ;
#218820 = VERTEX_POINT ( 'NONE', #228871 ) ;
#218821 = DIRECTION ( 'NONE',  ( 0.7071359030027593029, 0.000000000000000000, 0.7070776581709197206 ) ) ;
#218822 = AXIS2_PLACEMENT_3D ( 'NONE', #255421, #76833, #55967 ) ;
#218823 = AXIS2_PLACEMENT_3D ( 'NONE', #52607, #228705, #31807 ) ;
#218824 = ORIENTED_EDGE ( 'NONE', *, *, #207622, .T. ) ;
#218825 = CARTESIAN_POINT ( 'NONE',  ( 23.15000000000000213, 87.75000000001222134, -148.6731074845242802 ) ) ;
#218826 = ORIENTED_EDGE ( 'NONE', *, *, #107499, .T. ) ;
#218828 = ORIENTED_EDGE ( 'NONE', *, *, #35605, .F. ) ;
#218827 = DIRECTION ( 'NONE',  ( 0.000000000000000000, -0.4930308989875170078, -0.8700118002898356018 ) ) ;
#218829 = EDGE_CURVE ( 'NONE', #9664, #241306, #168938, .T. ) ;
#218832 = ORIENTED_EDGE ( 'NONE', *, *, #22295, .F. ) ;
#218831 = ORIENTED_EDGE ( 'NONE', *, *, #228149, .F. ) ;
#218830 = CARTESIAN_POINT ( 'NONE',  ( -21.08035267497491816, 0.08268862477602348382, 6.331706839783040941 ) ) ;
#218833 = EDGE_CURVE ( 'NONE', #209723, #152770, #71093, .T. ) ;
#218834 = CARTESIAN_POINT ( 'NONE',  ( -2.995603634470829482E-16, -11.74999999998884448, -146.2500000000000284 ) ) ;
#218835 = EDGE_CURVE ( 'NONE', #254325, #79894, #185139, .T. ) ;
#218836 = CARTESIAN_POINT ( 'NONE',  ( -20.88420186297724257, 65.66974365629616273, -30.43601455626050978 ) ) ;
#218837 = CARTESIAN_POINT ( 'NONE',  ( -18.69999999999999929, -8.250000000000005329, -15.00000000000000000 ) ) ;
#218838 = CARTESIAN_POINT ( 'NONE',  ( -23.15000000000000213, 76.00000000001165290, -69.52310748452431710 ) ) ;
#218839 = DIRECTION ( 'NONE',  ( 0.000000000000000000, -0.7071067811865479058, 0.7071067811865472397 ) ) ;
#218840 = CIRCLE ( 'NONE', #85723, 0.1000000000000028644 ) ;
#218841 = CARTESIAN_POINT ( 'NONE',  ( 21.05000000000000071, 65.57661458509973329, -196.0310555606543517 ) ) ;
#218842 = CARTESIAN_POINT ( 'NONE',  ( -18.59999999999999787, 67.74990736105834799, -227.9721689390126755 ) ) ;
#218844 = DIRECTION ( 'NONE',  ( -1.000000000000000000, -9.012599976027990443E-15, -6.882867235861669241E-14 ) ) ;
#218843 = CARTESIAN_POINT ( 'NONE',  ( 23.24999999999999289, 69.55000000001203375, -114.7731074845243455 ) ) ;
#218845 = VERTEX_POINT ( 'NONE', #227572 ) ;
#218846 = ORIENTED_EDGE ( 'NONE', *, *, #104620, .F. ) ;
#218847 = DIRECTION ( 'NONE',  ( 3.469446951953728416E-14, -0.1022405907414316584, -0.9947597004326437231 ) ) ;
#218848 = VECTOR ( 'NONE', #195014, 1000.000000000000000 ) ;
#218850 = ORIENTED_EDGE ( 'NONE', *, *, #49680, .T. ) ;
#218849 = DIRECTION ( 'NONE',  ( 0.000000000000000000, -0.4721928772777334582, -0.8814952561688437216 ) ) ;
#218851 = CARTESIAN_POINT ( 'NONE',  ( -20.64999999999999858, 2.500000000011154633, -187.7753780772378889 ) ) ;
#218852 = ORIENTED_EDGE ( 'NONE', *, *, #204659, .F. ) ;
#218853 = EDGE_CURVE ( 'NONE', #40869, #218579, #64331, .T. ) ;
#218854 = ORIENTED_EDGE ( 'NONE', *, *, #135415, .T. ) ;
#218855 = CARTESIAN_POINT ( 'NONE',  ( -15.55912972643740488, 67.50912972644943011, -115.5731074845243569 ) ) ;
#218856 = ADVANCED_FACE ( 'NONE', ( #9812 ), #47780, .T. ) ;
#218857 = VERTEX_POINT ( 'NONE', #35821 ) ;
#218858 = CARTESIAN_POINT ( 'NONE',  ( -20.64999999999999858, 36.65892442174472876, -249.5511627012454596 ) ) ;
#218859 = DIRECTION ( 'NONE',  ( -0.000000000000000000, -0.000000000000000000, 1.000000000000000000 ) ) ;
#218862 = ORIENTED_EDGE ( 'NONE', *, *, #218319, .F. ) ;
#218861 = ORIENTED_EDGE ( 'NONE', *, *, #94440, .F. ) ;
#218860 = TOROIDAL_SURFACE ( 'NONE', #127115, 7.800000000000000711, 0.1000000000000000056 ) ;
#218863 = AXIS2_PLACEMENT_3D ( 'NONE', #195938, #39444, #255839 ) ;
#218864 = ORIENTED_EDGE ( 'NONE', *, *, #2422, .T. ) ;
#218865 = SPHERICAL_SURFACE ( 'NONE', #136215, 0.1000000000000000056 ) ;
#218866 = VERTEX_POINT ( 'NONE', #38374 ) ;
#218867 = ORIENTED_EDGE ( 'NONE', *, *, #45224, .F. ) ;
#218868 = EDGE_CURVE ( 'NONE', #12339, #190986, #68616, .T. ) ;
#218870 = ORIENTED_EDGE ( 'NONE', *, *, #60162, .T. ) ;
#218869 = CARTESIAN_POINT ( 'NONE',  ( 23.14999999999998437, 4.050000000011155343, -67.00000000000004263 ) ) ;
#218871 = ADVANCED_FACE ( 'NONE', ( #198720 ), #85134, .T. ) ;
#218872 = EDGE_CURVE ( 'NONE', #1827, #89024, #254791, .T. ) ;
#218873 = CARTESIAN_POINT ( 'NONE',  ( 20.95566103547454517, 65.38175234906526612, -162.3912672915438407 ) ) ;
#218874 = FACE_BOUND ( 'NONE', #29766, .T. ) ;
#218875 = DIRECTION ( 'NONE',  ( 1.000000000000000000, 0.000000000000000000, 0.000000000000000000 ) ) ;
#218876 = CARTESIAN_POINT ( 'NONE',  ( -21.78635804494510708, 7.035661485164336426, -66.90099493449235979 ) ) ;
#218877 = VERTEX_POINT ( 'NONE', #237851 ) ;
#218878 = ORIENTED_EDGE ( 'NONE', *, *, #40001, .T. ) ;
#218879 = FACE_OUTER_BOUND ( 'NONE', #19147, .T. ) ;
#218880 = CARTESIAN_POINT ( 'NONE',  ( 23.15000000000000213, -11.74999999998883560, -197.8999999999999773 ) ) ;
#218881 = DIRECTION ( 'NONE',  ( 0.000000000000000000, -6.467318590049456648E-15, 1.000000000000000000 ) ) ;
#218882 = EDGE_CURVE ( 'NONE', #146650, #60369, #218265, .T. ) ;
#218883 = VECTOR ( 'NONE', #223013, 1000.000000000000000 ) ;
#218884 = ORIENTED_EDGE ( 'NONE', *, *, #84584, .F. ) ;
#218885 = LINE ( 'NONE', #58525, #65336 ) ;
#218886 = VECTOR ( 'NONE', #117116, 1000.000000000000000 ) ;
#218887 = AXIS2_PLACEMENT_3D ( 'NONE', #222145, #224729, #29162 ) ;
#218888 = VECTOR ( 'NONE', #246432, 1000.000000000000000 ) ;
#218889 = DIRECTION ( 'NONE',  ( 0.000000000000000000, 0.000000000000000000, -1.000000000000000000 ) ) ;
#218890 = CARTESIAN_POINT ( 'NONE',  ( -13.77178122865953469, 12.43384112479209591, -213.6551227491177940 ) ) ;
#218891 = ORIENTED_EDGE ( 'NONE', *, *, #148020, .F. ) ;
#218892 = ORIENTED_EDGE ( 'NONE', *, *, #94470, .T. ) ;
#218893 = PRESENTATION_LAYER_ASSIGNMENT (  '', '', ( #152303 ) ) ;
#218894 = LINE ( 'NONE', #160252, #142527 ) ;
#218895 = DIRECTION ( 'NONE',  ( 0.000000000000000000, 0.2128009952263601179, -0.9770955615653315052 ) ) ;
#218896 = ORIENTED_EDGE ( 'NONE', *, *, #29348, .F. ) ;
#218897 = CARTESIAN_POINT ( 'NONE',  ( -21.05000000000000071, 66.10573665986746050, -240.0052065600425237 ) ) ;
#218898 = ORIENTED_EDGE ( 'NONE', *, *, #66261, .F. ) ;
#218899 = DIRECTION ( 'NONE',  ( -1.000000000000000000, 0.000000000000000000, 0.000000000000000000 ) ) ;
#218900 = DIRECTION ( 'NONE',  ( 0.000000000000000000, 0.000000000000000000, 1.000000000000000000 ) ) ;
#218902 = CARTESIAN_POINT ( 'NONE',  ( -20.90851465518105456, 68.09306500613196533, -224.1549646960459370 ) ) ;
#218901 = LINE ( 'NONE', #100223, #11595 ) ;
#218903 = DIRECTION ( 'NONE',  ( 0.000000000000000000, 6.938893903907222067E-15, -1.000000000000000000 ) ) ;
#218904 = ADVANCED_FACE ( 'NONE', ( #215698 ), #115327, .F. ) ;
#218905 = CARTESIAN_POINT ( 'NONE',  ( -20.94999999999999929, 7.128833340094563376, -233.7327013124401276 ) ) ;
#218906 = ORIENTED_EDGE ( 'NONE', *, *, #124741, .F. ) ;
#218907 = CARTESIAN_POINT ( 'NONE',  ( -18.58735405345342429, 85.56647862034827767, -62.70039283825828846 ) ) ;
#218908 = CIRCLE ( 'NONE', #94011, 11.65000000000001457 ) ;
#218910 = ORIENTED_EDGE ( 'NONE', *, *, #21103, .T. ) ;
#218909 = ORIENTED_EDGE ( 'NONE', *, *, #14973, .T. ) ;
#218911 = ORIENTED_EDGE ( 'NONE', *, *, #75139, .T. ) ;
#218912 = CIRCLE ( 'NONE', #35787, 0.09999999999999939493 ) ;
#218913 = EDGE_CURVE ( 'NONE', #106796, #73651, #247498, .T. ) ;
#218914 = CARTESIAN_POINT ( 'NONE',  ( -16.94389599338511943, 66.00880201025724148, -157.4154626827142067 ) ) ;
#218915 = DIRECTION ( 'NONE',  ( 0.000000000000000000, -0.9673461469267405910, 0.2534589355812664757 ) ) ;
#218916 = DIRECTION ( 'NONE',  ( -1.000000000000000000, -0.000000000000000000, -0.000000000000000000 ) ) ;
#218917 = DIRECTION ( 'NONE',  ( 0.000000000000000000, 0.9915357197604883766, -0.1298341882519788160 ) ) ;
#218918 = VECTOR ( 'NONE', #93008, 1000.000000000000000 ) ;
#218919 = DIRECTION ( 'NONE',  ( 0.000000000000000000, 7.056502275159890832E-15, -1.000000000000000000 ) ) ;
#218921 = CARTESIAN_POINT ( 'NONE',  ( -14.56556274378147009, 66.55344247693928139, -87.93316553017845649 ) ) ;
#218920 = CARTESIAN_POINT ( 'NONE',  ( 20.74897398619109268, 10.59569302166641336, -7.679311456256082913 ) ) ;
#218922 = ORIENTED_EDGE ( 'NONE', *, *, #108468, .F. ) ;
#218923 = CARTESIAN_POINT ( 'NONE',  ( -16.85312964099708211, 66.08639531794378286, -48.92029177809394014 ) ) ;
#218924 = ORIENTED_EDGE ( 'NONE', *, *, #225598, .T. ) ;
#218925 = VECTOR ( 'NONE', #104243, 1000.000000000000000 ) ;
#218926 = EDGE_CURVE ( 'NONE', #204622, #151116, #118515, .T. ) ;
#218927 = CARTESIAN_POINT ( 'NONE',  ( 18.59999999999999787, 1.851028230152016674, -179.1539132694224463 ) ) ;
#218929 = EDGE_CURVE ( 'NONE', #137741, #96910, #200627, .T. ) ;
#218928 = CIRCLE ( 'NONE', #102193, 11.70000000000000284 ) ;
#218930 = AXIS2_PLACEMENT_3D ( 'NONE', #151555, #130667, #172418 ) ;
#218931 = EDGE_LOOP ( 'NONE', ( #85246, #153845, #246763, #121780, #224871, #190628, #125353, #101015, #164785, #81750 ) ) ;
#218932 = EDGE_LOOP ( 'NONE', ( #112545, #81433, #27091, #116624 ) ) ;
#218933 = DIRECTION ( 'NONE',  ( 1.000000000000000000, 0.000000000000000000, 0.000000000000000000 ) ) ;
#218934 = FACE_OUTER_BOUND ( 'NONE', #58503, .T. ) ;
#218935 = CARTESIAN_POINT ( 'NONE',  ( 18.59999999999998366, 7.128833340094563376, -233.7327013124401276 ) ) ;
#218936 = CARTESIAN_POINT ( 'NONE',  ( 15.74999999999999645, 9.350000000011139178, -83.75000000000004263 ) ) ;
#218937 = ADVANCED_FACE ( 'NONE', ( #16267 ), #179196, .T. ) ;
#218938 = AXIS2_PLACEMENT_3D ( 'NONE', #32884, #211482, #189355 ) ;
#218939 = FACE_OUTER_BOUND ( 'NONE', #16069, .T. ) ;
#218940 = ADVANCED_FACE ( 'NONE', ( #235271 ), #210097, .F. ) ;
#218941 = ORIENTED_EDGE ( 'NONE', *, *, #127082, .T. ) ;
#218942 = ORIENTED_EDGE ( 'NONE', *, *, #216403, .T. ) ;
#218943 = VECTOR ( 'NONE', #113185, 1000.000000000000000 ) ;
#218944 = DIRECTION ( 'NONE',  ( 1.000000000000000000, 0.000000000000000000, 0.000000000000000000 ) ) ;
#218945 = ORIENTED_EDGE ( 'NONE', *, *, #109583, .F. ) ;
#218946 = LINE ( 'NONE', #237242, #39776 ) ;
#218947 = FACE_OUTER_BOUND ( 'NONE', #220144, .T. ) ;
#218948 = AXIS2_PLACEMENT_3D ( 'NONE', #112256, #133091, #212636 ) ;
#218949 = CARTESIAN_POINT ( 'NONE',  ( -23.25000000000000000, 76.00000000001267608, -203.5231074845243597 ) ) ;
#218950 = VECTOR ( 'NONE', #227006, 1000.000000000000000 ) ;
#218951 = CARTESIAN_POINT ( 'NONE',  ( 23.14999999999999858, 0.000000000000000000, -33.50000000000000000 ) ) ;
#218952 = CARTESIAN_POINT ( 'NONE',  ( -21.05000000000000071, 64.25000000001196554, -110.0379132551783243 ) ) ;
#218953 = FACE_OUTER_BOUND ( 'NONE', #104365, .T. ) ;
#218955 = CARTESIAN_POINT ( 'NONE',  ( -21.44999999999999929, 68.65000000001222702, -148.7731074845244166 ) ) ;
#218954 = DIRECTION ( 'NONE',  ( -1.000000000000000000, -0.000000000000000000, -0.000000000000000000 ) ) ;
#218956 = DIRECTION ( 'NONE',  ( 0.000000000000000000, 0.000000000000000000, -1.000000000000000000 ) ) ;
#218957 = DIRECTION ( 'NONE',  ( 0.000000000000000000, -0.9126074666063545004, -0.4088369013363783999 ) ) ;
#218958 = EDGE_CURVE ( 'NONE', #177256, #139796, #72748, .T. ) ;
#218959 = DIRECTION ( 'NONE',  ( 0.000000000000000000, 0.000000000000000000, -1.000000000000000000 ) ) ;
#218960 = FACE_OUTER_BOUND ( 'NONE', #9640, .T. ) ;
#218961 = EDGE_CURVE ( 'NONE', #245391, #48041, #139317, .T. ) ;
#218962 = ORIENTED_EDGE ( 'NONE', *, *, #82963, .T. ) ;
#218963 = ADVANCED_FACE ( 'NONE', ( #184290 ), #21401, .T. ) ;
#218964 = CARTESIAN_POINT ( 'NONE',  ( -21.10000000000000142, -11.75000000000000000, 12.09999999999999609 ) ) ;
#218965 = ORIENTED_EDGE ( 'NONE', *, *, #99782, .T. ) ;
#218966 = CARTESIAN_POINT ( 'NONE',  ( 20.99142135623731065, 11.60000000001116049, -93.57179676972454274 ) ) ;
#218967 = CARTESIAN_POINT ( 'NONE',  ( -18.34374000495060386, 11.47316190337362585, -109.7500000000000284 ) ) ;
#218968 = DIRECTION ( 'NONE',  ( 1.000000000000000000, 0.000000000000000000, 0.000000000000000000 ) ) ;
#218969 = EDGE_CURVE ( 'NONE', #2619, #77581, #124333, .T. ) ;
#218971 = ORIENTED_EDGE ( 'NONE', *, *, #233497, .F. ) ;
#218970 = AXIS2_PLACEMENT_3D ( 'NONE', #218160, #119096, #20010 ) ;
#218972 = CARTESIAN_POINT ( 'NONE',  ( 21.15000000000005187, 64.35000000001120668, -3.123107484524795474 ) ) ;
#218973 = AXIS2_PLACEMENT_3D ( 'NONE', #241037, #102768, #81909 ) ;
#218974 = AXIS2_PLACEMENT_3D ( 'NONE', #171689, #88235, #148236 ) ;
#218976 = EDGE_CURVE ( 'NONE', #123658, #167394, #81061, .T. ) ;
#218975 = CARTESIAN_POINT ( 'NONE',  ( 21.05000000000000071, 1.360870587192041681, -8.072997927090961312 ) ) ;
#218977 = DIRECTION ( 'NONE',  ( 0.000000000000000000, 6.982962677686266711E-15, -1.000000000000000000 ) ) ;
#218978 = DIRECTION ( 'NONE',  ( 0.000000000000000000, 0.5000000000000144329, 0.8660254037844302699 ) ) ;
#218979 = DIRECTION ( 'NONE',  ( 1.000000000000000000, -0.000000000000000000, 0.000000000000000000 ) ) ;
#218980 = CARTESIAN_POINT ( 'NONE',  ( 20.85000000000000142, 0.000000000000000000, -33.50000000000000000 ) ) ;
#218981 = VECTOR ( 'NONE', #27089, 1000.000000000000000 ) ;
#218982 = VERTEX_POINT ( 'NONE', #23964 ) ;
#218983 = CARTESIAN_POINT ( 'NONE',  ( -20.94999999999999929, 28.58935552370083144, -258.2621935127861548 ) ) ;
#218985 = EDGE_LOOP ( 'NONE', ( #108726, #4284, #108226, #18439 ) ) ;
#218984 = DIRECTION ( 'NONE',  ( 0.000000000000000000, -0.9893560106964500722, 0.1455152366551550613 ) ) ;
#218986 = CARTESIAN_POINT ( 'NONE',  ( -21.64999999999999858, 60.84284427644114146, -221.0155524357444108 ) ) ;
#218987 = CARTESIAN_POINT ( 'NONE',  ( 21.03670563405601968, 23.01071051840566284, -230.1870050808868768 ) ) ;
#218988 = EDGE_CURVE ( 'NONE', #139774, #162824, #226828, .T. ) ;
#218989 = CIRCLE ( 'NONE', #160770, 0.09999999999999939493 ) ;
#218990 = EDGE_LOOP ( 'NONE', ( #85070, #193232, #76123, #211489 ) ) ;
#218991 = DIRECTION ( 'NONE',  ( 1.000000000000000000, -0.000000000000000000, -0.000000000000000000 ) ) ;
#218992 = EDGE_CURVE ( 'NONE', #84197, #179303, #141321, .T. ) ;
#218993 = CIRCLE ( 'NONE', #214706, 0.09999999999999938105 ) ;
#218994 = PRODUCT_CONTEXT ( 'NONE', #230605, 'mechanical' ) ;
#218995 = CYLINDRICAL_SURFACE ( 'NONE', #221284, 2.000000000000003109 ) ;
#218996 = AXIS2_PLACEMENT_3D ( 'NONE', #175719, #253929, #196531 ) ;
#218997 = ORIENTED_EDGE ( 'NONE', *, *, #58654, .T. ) ;
#218998 = CARTESIAN_POINT ( 'NONE',  ( 23.24999999999999645, 79.90000000001190017, -103.0231074845242745 ) ) ;
#218999 = CARTESIAN_POINT ( 'NONE',  ( 23.25000000000000000, -11.74999999998883560, -122.2500000000000284 ) ) ;
#219000 = CARTESIAN_POINT ( 'NONE',  ( -21.05000000000000071, 5.900000000011162093, -157.2809002353436654 ) ) ;
#219001 = EDGE_LOOP ( 'NONE', ( #67456, #256991, #32882, #115531, #202135, #215947, #56312, #40884, #235096, #77104, #141964, #222071, #203488, #152015, #98014, #104252 ) ) ;
#219002 = CIRCLE ( 'NONE', #23413, 0.1000000000000028644 ) ;
#219003 = ORIENTED_EDGE ( 'NONE', *, *, #14309, .T. ) ;
#219004 = CYLINDRICAL_SURFACE ( 'NONE', #30810, 4.049999999999998046 ) ;
#219005 = DIRECTION ( 'NONE',  ( 0.000000000000000000, 0.000000000000000000, -1.000000000000000000 ) ) ;
#219006 = CARTESIAN_POINT ( 'NONE',  ( 21.14999999999998082, -11.74999999998884448, -100.5000000000000284 ) ) ;
#219007 = CARTESIAN_POINT ( 'NONE',  ( 18.59999999999999076, 65.79142135624984178, -182.1731074845244223 ) ) ;
#219008 = DIRECTION ( 'NONE',  ( 0.000000000000000000, -1.000000000000000000, 0.000000000000000000 ) ) ;
#219009 = LINE ( 'NONE', #202031, #13896 ) ;
#219011 = DIRECTION ( 'NONE',  ( 0.000000000000000000, 1.000000000000000000, 0.000000000000000000 ) ) ;
#219010 = CARTESIAN_POINT ( 'NONE',  ( -20.94999999999999929, 77.16270174995034381, -161.9231074845243370 ) ) ;
#219012 = LINE ( 'NONE', #196885, #123411 ) ;
#219013 = CARTESIAN_POINT ( 'NONE',  ( -23.15000000000000213, 64.25000000001196554, -110.0379132551783243 ) ) ;
#219014 = FACE_OUTER_BOUND ( 'NONE', #129566, .T. ) ;
#219015 = CARTESIAN_POINT ( 'NONE',  ( 12.25000000000000000, 9.849999999999981881, -16.74999999999999645 ) ) ;
#219016 = ORIENTED_EDGE ( 'NONE', *, *, #185484, .T. ) ;
#219017 = CIRCLE ( 'NONE', #214924, 0.1999999999999987899 ) ;
#219018 = ADVANCED_FACE ( 'NONE', ( #103453 ), #205122, .F. ) ;
#219019 = ORIENTED_EDGE ( 'NONE', *, *, #248643, .F. ) ;
#219020 = AXIS2_PLACEMENT_3D ( 'NONE', #250810, #216815, #113875 ) ;
#219021 = AXIS2_PLACEMENT_3D ( 'NONE', #198072, #98945, #199381 ) ;
#219022 = CARTESIAN_POINT ( 'NONE',  ( 23.24999999999999289, 6.450000000000001066, 11.75000000000000000 ) ) ;
#219024 = DIRECTION ( 'NONE',  ( 0.000000000000000000, 0.2617529984165033463, 0.9651348961777157509 ) ) ;
#219023 = CARTESIAN_POINT ( 'NONE',  ( -21.98333005346336577, 76.00000000001273293, -210.8971828135810540 ) ) ;
#219025 = PLANE ( 'NONE',  #172815 ) ;
#219026 = SPHERICAL_SURFACE ( 'NONE', #152347, 0.1000000000000000056 ) ;
#219027 = ORIENTED_EDGE ( 'NONE', *, *, #254563, .T. ) ;
#219028 = CARTESIAN_POINT ( 'NONE',  ( 18.39999999999999503, 70.35000000001180354, -78.77310748452434552 ) ) ;
#219029 = ORIENTED_EDGE ( 'NONE', *, *, #92128, .T. ) ;
#219030 = CARTESIAN_POINT ( 'NONE',  ( -16.86445178670615874, 51.65108416207809938, -231.9186532702945556 ) ) ;
#219031 = CIRCLE ( 'NONE', #2550, 6.258578643762703564 ) ;
#219032 = ORIENTED_EDGE ( 'NONE', *, *, #61929, .F. ) ;
#219033 = EDGE_CURVE ( 'NONE', #162036, #6351, #220849, .T. ) ;
#219034 = CARTESIAN_POINT ( 'NONE',  ( -18.54270223418607344, -9.624105502871746154, -73.74093505040742969 ) ) ;
#219035 = CIRCLE ( 'NONE', #256586, 0.09999999999999938105 ) ;
#219036 = CARTESIAN_POINT ( 'NONE',  ( -19.89999999999999858, 1.350000000000000089, 16.60000000000000142 ) ) ;
#219037 = CIRCLE ( 'NONE', #65107, 0.09999999999999939493 ) ;
#219038 = EDGE_LOOP ( 'NONE', ( #55115, #219281, #114817, #115671 ) ) ;
#219039 = CARTESIAN_POINT ( 'NONE',  ( -18.59999999999999787, -1.835341550213255957, -78.55515129256302487 ) ) ;
#219040 = ORIENTED_EDGE ( 'NONE', *, *, #137624, .T. ) ;
#219041 = FACE_OUTER_BOUND ( 'NONE', #216304, .T. ) ;
#219042 = CYLINDRICAL_SURFACE ( 'NONE', #136995, 0.09999999999998898659 ) ;
#219043 = DIRECTION ( 'NONE',  ( 1.000000000000000000, 0.000000000000000000, 0.000000000000000000 ) ) ;
#219044 = CARTESIAN_POINT ( 'NONE',  ( -18.50000000000000000, 18.37021030142088662, -237.6367305148568221 ) ) ;
#219045 = CARTESIAN_POINT ( 'NONE',  ( 18.39999999999999858, 85.50000000001240608, -163.4229180933022576 ) ) ;
#219047 = FACE_OUTER_BOUND ( 'NONE', #45376, .T. ) ;
#219046 = CARTESIAN_POINT ( 'NONE',  ( 19.97071067811864609, 64.27928932189355749, -145.3731074845244109 ) ) ;
#219048 = CARTESIAN_POINT ( 'NONE',  ( 21.14999999999999503, 64.35000000001237197, -169.9231074845244507 ) ) ;
#219050 = ORIENTED_EDGE ( 'NONE', *, *, #199680, .T. ) ;
#219049 = CARTESIAN_POINT ( 'NONE',  ( 20.97107704358301916, 67.12452184799079191, -127.9641342551351215 ) ) ;
#219052 = CARTESIAN_POINT ( 'NONE',  ( -16.87683809663752399, 66.15000000001201386, -116.4254715027206686 ) ) ;
#219051 = DIRECTION ( 'NONE',  ( 0.000000000000000000, 0.000000000000000000, 1.000000000000000000 ) ) ;
#219053 = ORIENTED_EDGE ( 'NONE', *, *, #7372, .T. ) ;
#219055 = VERTEX_POINT ( 'NONE', #3071 ) ;
#219054 = CARTESIAN_POINT ( 'NONE',  ( 18.59999999999997655, 64.25000000001170974, -69.52310748452438816 ) ) ;
#219056 = AXIS2_PLACEMENT_3D ( 'NONE', #122989, #8174, #121713 ) ;
#219057 = ORIENTED_EDGE ( 'NONE', *, *, #61764, .F. ) ;
#219058 = DIRECTION ( 'NONE',  ( -1.000000000000000000, 0.000000000000000000, 0.000000000000000000 ) ) ;
#219059 = DIRECTION ( 'NONE',  ( 0.000000000000000000, 0.000000000000000000, -1.000000000000000000 ) ) ;
#219060 = CARTESIAN_POINT ( 'NONE',  ( 18.59999999999999787, 77.83534155023646406, -124.9679561919613064 ) ) ;
#219061 = ORIENTED_EDGE ( 'NONE', *, *, #8237, .T. ) ;
#219062 = DIRECTION ( 'NONE',  ( -0.000000000000000000, -0.000000000000000000, -1.000000000000000000 ) ) ;
#219063 = CARTESIAN_POINT ( 'NONE',  ( -20.00857864376270001, 22.33586458086958615, -231.4986017528744071 ) ) ;
#219064 = CARTESIAN_POINT ( 'NONE',  ( -23.15000000000000213, 7.128833340094563376, -233.7327013124401276 ) ) ;
#219065 = CARTESIAN_POINT ( 'NONE',  ( -16.94107738177414291, 10.01423928514777373, -154.9500000000000455 ) ) ;
#219066 = DIRECTION ( 'NONE',  ( -0.000000000000000000, -0.1350103645451718737, 0.9908441862701622416 ) ) ;
#219067 = ADVANCED_FACE ( 'NONE', ( #120506 ), #104721, .T. ) ;
#219069 = AXIS2_PLACEMENT_3D ( 'NONE', #105618, #146048, #67803 ) ;
#219068 = DIRECTION ( 'NONE',  ( 1.000000000000000000, -0.000000000000000000, -0.000000000000000000 ) ) ;
#219070 = ORIENTED_EDGE ( 'NONE', *, *, #81067, .F. ) ;
#219071 = VERTEX_POINT ( 'NONE', #183031 ) ;
#219073 = CARTESIAN_POINT ( 'NONE',  ( -16.94107738177414291, 10.01423928514777373, -188.4499999999999886 ) ) ;
#219072 = AXIS2_PLACEMENT_3D ( 'NONE', #132516, #136326, #232924 ) ;
#219074 = VECTOR ( 'NONE', #204549, 1000.000000000000000 ) ;
#219075 = AXIS2_PLACEMENT_3D ( 'NONE', #42787, #124899, #84426 ) ;
#219076 = ORIENTED_EDGE ( 'NONE', *, *, #217732, .F. ) ;
#219077 = CARTESIAN_POINT ( 'NONE',  ( -17.80356949363960339, 10.87673139700207869, -10.28692697577638171 ) ) ;
#219078 = ORIENTED_EDGE ( 'NONE', *, *, #156772, .T. ) ;
#219079 = DIRECTION ( 'NONE',  ( 1.000000000000000000, 0.000000000000000000, 0.000000000000000000 ) ) ;
#219080 = ADVANCED_FACE ( 'NONE', ( #42229 ), #85332, .F. ) ;
#219081 = DIRECTION ( 'NONE',  ( 0.000000000000000000, -0.4088369013363280513, 0.9126074666063769270 ) ) ;
#219082 = LINE ( 'NONE', #23503, #242917 ) ;
#219083 = ADVANCED_FACE ( 'NONE', ( #200019 ), #10370, .F. ) ;
#219084 = DIRECTION ( 'NONE',  ( 0.000000000000000000, 0.000000000000000000, -1.000000000000000000 ) ) ;
#219085 = CARTESIAN_POINT ( 'NONE',  ( -23.25000000000000355, 64.25000000001190870, -93.77310748452438816 ) ) ;
#219086 = EDGE_CURVE ( 'NONE', #177620, #112295, #35514, .T. ) ;
#219087 = CARTESIAN_POINT ( 'NONE',  ( -22.45437739390953524, 1.115486826172573664E-11, -88.85042918840584036 ) ) ;
#219088 = DIRECTION ( 'NONE',  ( -7.304098846218134667E-16, -1.000000000000000000, 0.000000000000000000 ) ) ;
#219089 = ORIENTED_EDGE ( 'NONE', *, *, #251682, .F. ) ;
#219090 = CYLINDRICAL_SURFACE ( 'NONE', #27297, 0.1000000000000028644 ) ;
#219091 = AXIS2_PLACEMENT_3D ( 'NONE', #10592, #215199, #131808 ) ;
#219092 = ORIENTED_EDGE ( 'NONE', *, *, #139230, .T. ) ;
#219095 = ORIENTED_EDGE ( 'NONE', *, *, #233998, .F. ) ;
#219094 = DIRECTION ( 'NONE',  ( 0.000000000000000000, 0.4721928772776568528, 0.8814952561688845778 ) ) ;
#219093 = DIRECTION ( 'NONE',  ( 1.000000000000000000, 0.000000000000000000, 0.000000000000000000 ) ) ;
#219096 = ORIENTED_EDGE ( 'NONE', *, *, #79196, .T. ) ;
#219097 = DIRECTION ( 'NONE',  ( 0.000000000000000000, 0.000000000000000000, -1.000000000000000000 ) ) ;
#219098 = AXIS2_PLACEMENT_3D ( 'NONE', #215884, #252449, #116812 ) ;
#219099 = CARTESIAN_POINT ( 'NONE',  ( 21.04999999999999716, -0.01759718699747322632, -60.55922910633812251 ) ) ;
#219100 = CARTESIAN_POINT ( 'NONE',  ( 18.59999999999999787, -10.64999999999999325, 33.00000000000000000 ) ) ;
#219101 = DIRECTION ( 'NONE',  ( -1.000000000000000000, 0.000000000000000000, 0.000000000000000000 ) ) ;
#219102 = EDGE_LOOP ( 'NONE', ( #236309, #49945, #153410, #136490 ) ) ;
#219103 = CARTESIAN_POINT ( 'NONE',  ( 19.81427058490547211, 16.66812670693539289, -222.7000331208559203 ) ) ;
#219104 = AXIS2_PLACEMENT_3D ( 'NONE', #112285, #133121, #156565 ) ;
#219105 = EDGE_CURVE ( 'NONE', #20887, #72537, #162193, .T. ) ;
#219106 = DIRECTION ( 'NONE',  ( 0.000000000000000000, -0.4930308989875248349, -0.8700118002898312719 ) ) ;
#219107 = AXIS2_PLACEMENT_3D ( 'NONE', #8708, #69987, #128665 ) ;
#219109 = CARTESIAN_POINT ( 'NONE',  ( 20.95325940946048249, 10.52339007069628707, -7.564462129240085986 ) ) ;
#219108 = CARTESIAN_POINT ( 'NONE',  ( -22.39999999999999858, 7.790779598384560245, -167.4999999999999716 ) ) ;
#219110 = AXIS2_PLACEMENT_3D ( 'NONE', #190364, #169543, #52096 ) ;
#219112 = ORIENTED_EDGE ( 'NONE', *, *, #212986, .F. ) ;
#219111 = CARTESIAN_POINT ( 'NONE',  ( -23.15000000000000213, 1.148907358139439339E-11, -201.0000000000015064 ) ) ;
#219113 = EDGE_LOOP ( 'NONE', ( #255885, #173291, #164910, #148087, #105659 ) ) ;
#219114 = VECTOR ( 'NONE', #41221, 1000.000000000000000 ) ;
#219115 = DIRECTION ( 'NONE',  ( -1.000000000000000000, -2.952720810173289112E-16, 0.000000000000000000 ) ) ;
#219116 = EDGE_LOOP ( 'NONE', ( #233850, #126104, #174864 ) ) ;
#219117 = CARTESIAN_POINT ( 'NONE',  ( -21.64999999999999858, 68.65000000001187175, -90.67310748452436542 ) ) ;
#219118 = ORIENTED_EDGE ( 'NONE', *, *, #88032, .T. ) ;
#219119 = CIRCLE ( 'NONE', #110992, 1.500000000000001332 ) ;
#219120 = CARTESIAN_POINT ( 'NONE',  ( -20.85000000000000142, 11.65000000001115232, -127.2161343370219413 ) ) ;
#219121 = CARTESIAN_POINT ( 'NONE',  ( 23.04999999999999716, 11.31241850904329205, -211.4828089347303433 ) ) ;
#219122 = FACE_OUTER_BOUND ( 'NONE', #229469, .T. ) ;
#219124 = ORIENTED_EDGE ( 'NONE', *, *, #154416, .T. ) ;
#219123 = VECTOR ( 'NONE', #138947, 1000.000000000000000 ) ;
#219125 = DIRECTION ( 'NONE',  ( -1.000000000000000000, -0.000000000000000000, -0.000000000000000000 ) ) ;
#219126 = CIRCLE ( 'NONE', #7324, 0.5000000000000004441 ) ;
#219127 = CARTESIAN_POINT ( 'NONE',  ( 18.39999999999997371, 11.75000000001113953, -109.7500000000000426 ) ) ;
#219128 = ADVANCED_FACE ( 'NONE', ( #185581 ), #123050, .T. ) ;
#219129 = ORIENTED_EDGE ( 'NONE', *, *, #99439, .T. ) ;
#219130 = VERTEX_POINT ( 'NONE', #145154 ) ;
#219131 = VERTEX_POINT ( 'NONE', #224695 ) ;
#219132 = CARTESIAN_POINT ( 'NONE',  ( -23.15000000000000213, 11.75000000001116263, -179.6499999999999773 ) ) ;
#219133 = ORIENTED_EDGE ( 'NONE', *, *, #226193, .F. ) ;
#219135 = VERTEX_POINT ( 'NONE', #6941 ) ;
#219134 = DIRECTION ( 'NONE',  ( 1.000000000000000000, -0.000000000000000000, -0.000000000000000000 ) ) ;
#219136 =( REPRESENTATION_RELATIONSHIP ('NONE','NONE', #36900, #213520 ) REPRESENTATION_RELATIONSHIP_WITH_TRANSFORMATION ( #48062 )SHAPE_REPRESENTATION_RELATIONSHIP( ) );
#219137 = EDGE_CURVE ( 'NONE', #129914, #21223, #166047, .T. ) ;
#219138 = ORIENTED_EDGE ( 'NONE', *, *, #137384, .T. ) ;
#219139 = VECTOR ( 'NONE', #76707, 999.9999999999998863 ) ;
#219141 = B_SPLINE_CURVE_WITH_KNOTS ( 'NONE', 3,
 ( #223978, #186149, #124900, #126155, #27107, #204412, #105287, #106586, #7507, #87020, #73934, #88296, #29673, #72642, #208294, #93450, #169185, #33541, #230409, #13939, #28399, #252523, #248692, #153495, #51743, #113030, #148309, #92175, #229130, #50457 ),
 .UNSPECIFIED., .F., .F.,
 ( 4, 2, 2, 2, 2, 2, 2, 2, 2, 2, 2, 2, 2, 2, 4 ),
 ( 0.000000000000000000, 0.0003422764154113352953, 0.0006845528308226705907, 0.001026829246234005994, 0.001369105661645341181, 0.002053658492468010688, 0.002738211323290680194, 0.003080487738702015164, 0.003422764154113349267, 0.003765040569524684237, 0.004107316984936018774, 0.004449593400347354177, 0.004791869815758687846, 0.005134146231170023250, 0.005476422646581357787 ),
 .UNSPECIFIED. ) ;
#219140 = AXIS2_PLACEMENT_3D ( 'NONE', #105462, #185037, #205878 ) ;
#219144 = EDGE_LOOP ( 'NONE', ( #212750, #56647, #182475, #246709 ) ) ;
#219143 = ORIENTED_EDGE ( 'NONE', *, *, #224634, .F. ) ;
#219142 = DIRECTION ( 'NONE',  ( 1.000000000000000000, 0.000000000000000000, 0.000000000000000000 ) ) ;
#219145 = EDGE_CURVE ( 'NONE', #99179, #154587, #57715, .T. ) ;
#219147 = EDGE_CURVE ( 'NONE', #56434, #215032, #90320, .T. ) ;
#219146 = AXIS2_PLACEMENT_3D ( 'NONE', #191371, #92226, #171815 ) ;
#219148 = CIRCLE ( 'NONE', #106721, 0.09999999999999939493 ) ;
#219149 = VERTEX_POINT ( 'NONE', #111189 ) ;
#219150 = CYLINDRICAL_SURFACE ( 'NONE', #218701, 0.09999999999999939493 ) ;
#219151 = DIRECTION ( 'NONE',  ( 0.000000000000000000, 0.000000000000000000, -1.000000000000000000 ) ) ;
#219152 = TOROIDAL_SURFACE ( 'NONE', #111026, 11.65000000000000036, 0.1000000000000000056 ) ;
#219153 = CARTESIAN_POINT ( 'NONE',  ( 21.07928932188134397, 75.90110485435833709, -209.8516241409176928 ) ) ;
#219154 = ORIENTED_EDGE ( 'NONE', *, *, #182613, .T. ) ;
#219155 = DIRECTION ( 'NONE',  ( 0.000000000000000000, 1.000000000000000000, -1.224646799147353207E-16 ) ) ;
#219157 = ADVANCED_FACE ( 'NONE', ( #29128 ), #229848, .F. ) ;
#219156 =( BOUNDED_SURFACE ( )  B_SPLINE_SURFACE ( 3, 2, ( 
 ( #107229, #206344, #90216 ),
 ( #185491, #109790, #108517 ),
 ( #169823, #164651, #27739 ),
 ( #246730, #70707, #249330 ),
 ( #69412, #229749, #225861 ),
 ( #130645, #49824, #128088 ) ),
 .UNSPECIFIED., .F., .F., .F. ) 
 B_SPLINE_SURFACE_WITH_KNOTS ( ( 4, 2, 4 ),
 ( 3, 3 ),
 ( 0.0001300404313046710908, 0.0003183318589266637198, 0.0005066232865486563217 ),
 ( 0.000000000000000000, 1.000000000000000000 ),
 .UNSPECIFIED. ) 
 GEOMETRIC_REPRESENTATION_ITEM ( )  RATIONAL_B_SPLINE_SURFACE ( (
 ( 1.000000000000000000, 0.7071067811865475727, 1.000000000000000000),
 ( 1.000000000000000000, 0.7625113560532659207, 1.000000000000000000),
 ( 1.000000000000000000, 0.8126073484698599358, 1.000000000000000000),
 ( 1.000000000000000000, 0.8923049332723309579, 1.000000000000000000),
 ( 1.000000000000000000, 0.9231914937776042329, 1.000000000000000000),
 ( 1.000000000000000000, 0.9238795325112945100, 1.000000000000000000) ) ) 
 REPRESENTATION_ITEM ( '' )  SURFACE ( )  );
#219159 = ORIENTED_EDGE ( 'NONE', *, *, #808, .F. ) ;
#219158 = CARTESIAN_POINT ( 'NONE',  ( 22.47071067811865319, 0.09909245471376171288, -59.27992525550200043 ) ) ;
#219160 = CARTESIAN_POINT ( 'NONE',  ( -18.50000000000000000, 67.65998959290220682, -227.8609496483021530 ) ) ;
#219162 = EDGE_LOOP ( 'NONE', ( #100987, #233570, #220482, #141233 ) ) ;
#219161 = DIRECTION ( 'NONE',  ( 0.000000000000000000, 0.000000000000000000, 1.000000000000000000 ) ) ;
#219163 = EDGE_CURVE ( 'NONE', #197646, #152480, #43674, .T. ) ;
#219164 = AXIS2_PLACEMENT_3D ( 'NONE', #243269, #35816, #210581 ) ;
#219165 = EDGE_LOOP ( 'NONE', ( #202900, #219817, #28716, #56681, #122158 ) ) ;
#219166 = EDGE_CURVE ( 'NONE', #237439, #169837, #72073, .T. ) ;
#219167 = CIRCLE ( 'NONE', #31780, 4.150000000000001243 ) ;
#219168 = DIRECTION ( 'NONE',  ( 0.000000000000000000, 0.9126074666063769270, 0.4088369013363280513 ) ) ;
#219169 = CIRCLE ( 'NONE', #235931, 7.899999999999990585 ) ;
#219170 = ORIENTED_EDGE ( 'NONE', *, *, #149795, .F. ) ;
#219171 = ORIENTED_EDGE ( 'NONE', *, *, #257809, .T. ) ;
#219172 = CARTESIAN_POINT ( 'NONE',  ( 16.87683809663750267, 9.950000000011138823, -79.65000000000003411 ) ) ;
#219173 = DIRECTION ( 'NONE',  ( -1.000000000000000000, 0.000000000000000000, 0.000000000000000000 ) ) ;
#219175 = ORIENTED_EDGE ( 'NONE', *, *, #174616, .F. ) ;
#219174 = VERTEX_POINT ( 'NONE', #9506 ) ;
#219176 = ORIENTED_EDGE ( 'NONE', *, *, #121162, .F. ) ;
#219177 = CARTESIAN_POINT ( 'NONE',  ( 21.05000000000000071, 61.94127660284455317, -221.8315191551248517 ) ) ;
#219178 = ORIENTED_EDGE ( 'NONE', *, *, #81043, .T. ) ;
#219179 = ORIENTED_EDGE ( 'NONE', *, *, #245424, .F. ) ;
#219180 = ADVANCED_FACE ( 'NONE', ( #208999 ), #130746, .T. ) ;
#219181 = CARTESIAN_POINT ( 'NONE',  ( 18.45139536634708932, 85.48608172029364027, -163.3825958667137002 ) ) ;
#219182 = CIRCLE ( 'NONE', #215105, 11.65000000000000746 ) ;
#219183 = VERTEX_POINT ( 'NONE', #27830 ) ;
#219184 = ADVANCED_FACE ( 'NONE', ( #190754 ), #107322, .T. ) ;
#219185 = CARTESIAN_POINT ( 'NONE',  ( -16.94107738177415712, 12.45552124806248706, -211.1315092113344463 ) ) ;
#219186 = EDGE_CURVE ( 'NONE', #183814, #149811, #247861, .T. ) ;
#219188 = DIRECTION ( 'NONE',  ( -1.000000000000000000, 0.000000000000000000, -0.000000000000000000 ) ) ;
#219187 = SPHERICAL_SURFACE ( 'NONE', #177983, 0.1000000000000000056 ) ;
#219189 = VERTEX_POINT ( 'NONE', #66918 ) ;
#219191 = VERTEX_POINT ( 'NONE', #51176 ) ;
#219190 = ORIENTED_EDGE ( 'NONE', *, *, #40306, .T. ) ;
#219192 = CARTESIAN_POINT ( 'NONE',  ( -18.40000000000000213, 70.35000000001261355, -190.8731074845244109 ) ) ;
#219193 = CARTESIAN_POINT ( 'NONE',  ( 20.95512820512820440, 10.62384868372303615, -175.1649135690875880 ) ) ;
#219194 = B_SPLINE_CURVE_WITH_KNOTS ( 'NONE', 3,
 ( #219108, #180016, #100430, #103010, #19652, #242533, #82148 ),
 .UNSPECIFIED., .F., .F.,
 ( 4, 3, 4 ),
 ( 0.000000000000000000, 0.0009834301579439998740, 0.001767853679402675614 ),
 .UNSPECIFIED. ) ;
#219195 = EDGE_LOOP ( 'NONE', ( #196800, #139252, #77744, #180237 ) ) ;
#219196 = TOROIDAL_SURFACE ( 'NONE', #223284, 4.149999999999999467, 0.1000000000000000056 ) ;
#219197 = AXIS2_PLACEMENT_3D ( 'NONE', #226281, #206745, #177905 ) ;
#219198 = AXIS2_PLACEMENT_3D ( 'NONE', #238650, #219066, #23488 ) ;
#219199 = AXIS2_PLACEMENT_3D ( 'NONE', #190069, #130078, #253874 ) ;
#219200 = VERTEX_POINT ( 'NONE', #168646 ) ;
#219201 = ADVANCED_FACE ( 'NONE', ( #47335 ), #8244, .T. ) ;
#219202 = ORIENTED_EDGE ( 'NONE', *, *, #210509, .T. ) ;
#219203 = EDGE_CURVE ( 'NONE', #20798, #180781, #87751, .T. ) ;
#219204 = DIRECTION ( 'NONE',  ( -3.469446951953635015E-14, 1.000000000000000000, 0.000000000000000000 ) ) ;
#219205 = ORIENTED_EDGE ( 'NONE', *, *, #21879, .F. ) ;
#219206 = DIRECTION ( 'NONE',  ( 0.000000000000000000, 0.000000000000000000, -1.000000000000000000 ) ) ;
#219207 = CARTESIAN_POINT ( 'NONE',  ( 21.05000000000000071, 34.10212115774099573, -243.5992592859234378 ) ) ;
#219208 = ORIENTED_EDGE ( 'NONE', *, *, #252956, .F. ) ;
#219209 = DIRECTION ( 'NONE',  ( -3.469446951953749873E-14, -0.4088369013363783999, 0.9126074666063545004 ) ) ;
#219210 = CARTESIAN_POINT ( 'NONE',  ( -16.94107738177415357, 10.01423928514777728, -46.04999999999999716 ) ) ;
#219212 = CARTESIAN_POINT ( 'NONE',  ( -16.77431908686106254, 9.945805754529134290, -121.3358392176502747 ) ) ;
#219211 = DIRECTION ( 'NONE',  ( 1.000000000000000000, 0.000000000000000000, 0.000000000000000000 ) ) ;
#219213 = CARTESIAN_POINT ( 'NONE',  ( -23.15000000000000213, 87.48912529308852015, -173.1231074845242688 ) ) ;
#219214 = CARTESIAN_POINT ( 'NONE',  ( 21.05000000000000071, -1.249999999988843369, -74.90000000000004832 ) ) ;
#219215 = FACE_OUTER_BOUND ( 'NONE', #113835, .T. ) ;
#219216 = DIRECTION ( 'NONE',  ( 1.000000000000000000, 0.000000000000000000, 0.000000000000000000 ) ) ;
#219217 = EDGE_CURVE ( 'NONE', #131589, #84718, #246831, .T. ) ;
#219218 = DIRECTION ( 'NONE',  ( 1.000000000000000000, 0.000000000000000000, 0.000000000000000000 ) ) ;
#219219 = DIRECTION ( 'NONE',  ( 1.000000000000000000, 0.000000000000000000, 0.000000000000000000 ) ) ;
#219220 = CIRCLE ( 'NONE', #211040, 0.1000000000000020595 ) ;
#219221 = AXIS2_PLACEMENT_3D ( 'NONE', #95321, #213989, #135715 ) ;
#219222 = VERTEX_POINT ( 'NONE', #44361 ) ;
#219224 = ORIENTED_EDGE ( 'NONE', *, *, #44938, .F. ) ;
#219223 = ORIENTED_EDGE ( 'NONE', *, *, #37969, .F. ) ;
#219225 = AXIS2_PLACEMENT_3D ( 'NONE', #122550, #119999, #101647 ) ;
#219226 = VERTEX_POINT ( 'NONE', #203428 ) ;
#219227 = ORIENTED_EDGE ( 'NONE', *, *, #109352, .F. ) ;
#219228 = DIRECTION ( 'NONE',  ( 0.000000000000000000, 0.2128009952263485993, -0.9770955615653341697 ) ) ;
#219229 = CARTESIAN_POINT ( 'NONE',  ( -18.50000000000000355, 43.02787096365918984, -254.3959382439171577 ) ) ;
#219231 = DIRECTION ( 'NONE',  ( 0.000000000000000000, 0.9999631594459053030, 0.008583690987162899758 ) ) ;
#219230 = LINE ( 'NONE', #217936, #232532 ) ;
#219232 = CARTESIAN_POINT ( 'NONE',  ( -20.94999999999994600, 65.35000000001120668, -3.023107484524792277 ) ) ;
#219233 = ORIENTED_EDGE ( 'NONE', *, *, #224780, .T. ) ;
#219234 = EDGE_CURVE ( 'NONE', #252932, #207854, #23540, .T. ) ;
#219235 = CARTESIAN_POINT ( 'NONE',  ( 20.95000000000005613, 67.85000000001119247, -51.02310748452479316 ) ) ;
#219236 =( NAMED_UNIT ( * ) PLANE_ANGLE_UNIT ( ) SI_UNIT ( $, .RADIAN. ) );
#219237 = CARTESIAN_POINT ( 'NONE',  ( 21.05000000000000071, -11.64999999998883595, -36.39999999999999858 ) ) ;
#219238 = CYLINDRICAL_SURFACE ( 'NONE', #55822, 0.09999999999998898659 ) ;
#219239 = EDGE_CURVE ( 'NONE', #140955, #207631, #24818, .T. ) ;
#219240 = CARTESIAN_POINT ( 'NONE',  ( 18.39999999999999858, -9.499999999988842703, -73.60018939122203108 ) ) ;
#219241 = ORIENTED_EDGE ( 'NONE', *, *, #49621, .F. ) ;
#219242 = CARTESIAN_POINT ( 'NONE',  ( -23.25000000000000000, 87.75000000001215028, -136.5231074845242745 ) ) ;
#219243 = EDGE_CURVE ( 'NONE', #154288, #214314, #238020, .T. ) ;
#219244 = CARTESIAN_POINT ( 'NONE',  ( -21.05000000000000071, -0.02110330804789880416, -94.19548367073602435 ) ) ;
#219245 = EDGE_CURVE ( 'NONE', #229005, #75163, #68796, .T. ) ;
#219246 = VERTEX_POINT ( 'NONE', #3939 ) ;
#219247 = DIRECTION ( 'NONE',  ( 0.000000000000000000, 0.000000000000000000, 1.000000000000000000 ) ) ;
#219248 = LINE ( 'NONE', #61475, #19630 ) ;
#219249 = CARTESIAN_POINT ( 'NONE',  ( -21.04999999999994387, 76.00000000001119815, -40.17310748452479174 ) ) ;
#219250 = CARTESIAN_POINT ( 'NONE',  ( -23.49999999999994316, 74.83745509109094485, -44.02310748452479316 ) ) ;
#219251 = ADVANCED_FACE ( 'NONE', ( #82156 ), #26081, .F. ) ;
#219252 = CIRCLE ( 'NONE', #65132, 0.09999999999998898659 ) ;
#219253 = DIRECTION ( 'NONE',  ( 0.000000000000000000, -7.056502275159890043E-15, 1.000000000000000000 ) ) ;
#219254 = EDGE_LOOP ( 'NONE', ( #133714, #157787, #198339, #229899 ) ) ;
#219255 = DIRECTION ( 'NONE',  ( 0.000000000000000000, 0.000000000000000000, -1.000000000000000000 ) ) ;
#219256 = CARTESIAN_POINT ( 'NONE',  ( -20.85000000000000142, 11.65000000001115232, -200.9999999999999432 ) ) ;
#219257 = DIRECTION ( 'NONE',  ( 0.7071067811865127117, 0.7071067811865821007, 0.000000000000000000 ) ) ;
#219259 = DIRECTION ( 'NONE',  ( -0.000000000000000000, -6.982962677686266711E-15, 1.000000000000000000 ) ) ;
#219258 = DIRECTION ( 'NONE',  ( -1.000000000000000000, -0.000000000000000000, 1.073024830501117725E-15 ) ) ;
#219260 = DIRECTION ( 'NONE',  ( 0.000000000000000000, 6.982962677686266711E-15, -1.000000000000000000 ) ) ;
#219261 = AXIS2_PLACEMENT_3D ( 'NONE', #79495, #41689, #16990 ) ;
#219262 = FILL_AREA_STYLE_COLOUR ( '', #237337 ) ;
#219263 = DIRECTION ( 'NONE',  ( 0.000000000000000000, 0.000000000000000000, -1.000000000000000000 ) ) ;
#219264 = CARTESIAN_POINT ( 'NONE',  ( -20.94999999999999929, 76.00000000001149658, -47.72310748452432705 ) ) ;
#219265 = CIRCLE ( 'NONE', #48571, 1.900000000000012790 ) ;
#219266 = ORIENTED_EDGE ( 'NONE', *, *, #71151, .T. ) ;
#219267 = AXIS2_PLACEMENT_3D ( 'NONE', #146682, #226208, #148002 ) ;
#219268 = EDGE_CURVE ( 'NONE', #139739, #32735, #214524, .T. ) ;
#219269 = B_SPLINE_CURVE_WITH_KNOTS ( 'NONE', 3,
 ( #30872, #205609, #90796, #145633 ),
 .UNSPECIFIED., .F., .F.,
 ( 4, 4 ),
 ( 0.000000000000000000, 0.001767853679387143117 ),
 .UNSPECIFIED. ) ;
#219270 = EDGE_CURVE ( 'NONE', #181952, #207975, #56116, .T. ) ;
#219271 =( BOUNDED_CURVE ( )  B_SPLINE_CURVE ( 3, ( #150395, #147821, #30447, #229916 ),
 .UNSPECIFIED., .F., .F. ) 
 B_SPLINE_CURVE_WITH_KNOTS ( ( 4, 4 ),
 ( 4.712388980384689674, 6.283185307179586232 ),
 .UNSPECIFIED. ) 
 CURVE ( )  GEOMETRIC_REPRESENTATION_ITEM ( )  RATIONAL_B_SPLINE_CURVE ( ( 1.000000000000000000, 0.8047378541243649375, 0.8047378541243649375, 1.000000000000000000 ) ) 
 REPRESENTATION_ITEM ( '' )  );
#219272 = ORIENTED_EDGE ( 'NONE', *, *, #129127, .F. ) ;
#219273 = ORIENTED_EDGE ( 'NONE', *, *, #199185, .T. ) ;
#219274 = EDGE_CURVE ( 'NONE', #82520, #99517, #218619, .T. ) ;
#219275 = CYLINDRICAL_SURFACE ( 'NONE', #192713, 0.09999999999999939493 ) ;
#219276 = CARTESIAN_POINT ( 'NONE',  ( 18.59999999999999432, 0.5876173420563333138, -209.1618981382189588 ) ) ;
#219277 = CARTESIAN_POINT ( 'NONE',  ( -18.51991288638513566, -9.392436789662129470, -174.6432664039591600 ) ) ;
#219278 = EDGE_CURVE ( 'NONE', #222610, #231369, #235095, .T. ) ;
#219279 = DIRECTION ( 'NONE',  ( 1.000000000000000000, 0.000000000000000000, 0.000000000000000000 ) ) ;
#219280 = CIRCLE ( 'NONE', #202709, 0.09999999999999939493 ) ;
#219281 = ORIENTED_EDGE ( 'NONE', *, *, #42730, .T. ) ;
#219282 = CARTESIAN_POINT ( 'NONE',  ( -20.90000000000000213, 1.885425182446133885, -11.49641995933507843 ) ) ;
#219283 = VECTOR ( 'NONE', #204040, 1000.000000000000000 ) ;
#219284 = CARTESIAN_POINT ( 'NONE',  ( -23.15000000000000213, 1.115600667400684642E-11, -200.9999999999999432 ) ) ;
#219285 = CARTESIAN_POINT ( 'NONE',  ( -22.47071067811865319, 75.90090754530939421, -110.7431822290223806 ) ) ;
#219286 = ADVANCED_FACE ( 'NONE', ( #46894 ), #123896, .F. ) ;
#219287 = AXIS2_PLACEMENT_3D ( 'NONE', #216976, #119190, #157040 ) ;
#219288 = FACE_OUTER_BOUND ( 'NONE', #82521, .T. ) ;
#219290 = ORIENTED_EDGE ( 'NONE', *, *, #253350, .T. ) ;
#219289 = CARTESIAN_POINT ( 'NONE',  ( -16.89935556175728593, 9.950000000011264945, -187.8603236371162950 ) ) ;
#219292 = CARTESIAN_POINT ( 'NONE',  ( -18.44085059012131822, 11.51401249349495970, -158.2403053191215463 ) ) ;
#219291 = LINE ( 'NONE', #4102, #92265 ) ;
#219293 = DIRECTION ( 'NONE',  ( -0.000000000000000000, 0.7397360091702708251, 0.6728971962616883129 ) ) ;
#219294 = EDGE_CURVE ( 'NONE', #217247, #12219, #241283, .T. ) ;
#219295 = AXIS2_PLACEMENT_3D ( 'NONE', #42389, #240590, #661 ) ;
#219296 = CARTESIAN_POINT ( 'NONE',  ( -20.07928932188135107, 13.53153662663944523, -219.8011042742668337 ) ) ;
#219298 = EDGE_LOOP ( 'NONE', ( #35000, #244211, #53865, #74604 ) ) ;
#219297 = CIRCLE ( 'NONE', #90105, 0.09999999999998715472 ) ;
#219299 = EDGE_CURVE ( 'NONE', #254689, #215277, #243823, .T. ) ;
#219300 = CARTESIAN_POINT ( 'NONE',  ( -20.85000000000000142, 76.32388570108174974, -36.06551789521033413 ) ) ;
#219301 = CYLINDRICAL_SURFACE ( 'NONE', #227324, 0.1000000000000106914 ) ;
#219302 = EDGE_LOOP ( 'NONE', ( #105271, #212544, #148248, #72402 ) ) ;
#219303 = LINE ( 'NONE', #163202, #91869 ) ;
#219304 = CYLINDRICAL_SURFACE ( 'NONE', #230572, 0.1000000000000028644 ) ;
#219305 = ORIENTED_EDGE ( 'NONE', *, *, #164724, .F. ) ;
#219306 = AXIS2_PLACEMENT_3D ( 'NONE', #92844, #171158, #189390 ) ;
#219307 = CARTESIAN_POINT ( 'NONE',  ( 18.39999999999999503, 64.25000000001224976, -149.1731074845244507 ) ) ;
#219308 = AXIS2_PLACEMENT_3D ( 'NONE', #5737, #22791, #60587 ) ;
#219309 = CYLINDRICAL_SURFACE ( 'NONE', #215820, 0.09999999999999939493 ) ;
#219310 = DIRECTION ( 'NONE',  ( 0.000000000000000000, 0.000000000000000000, 1.000000000000000000 ) ) ;
#219311 = EDGE_CURVE ( 'NONE', #117760, #52759, #201881, .T. ) ;
#219312 = ORIENTED_EDGE ( 'NONE', *, *, #95062, .T. ) ;
#219313 = VERTEX_POINT ( 'NONE', #245117 ) ;
#219314 = CARTESIAN_POINT ( 'NONE',  ( -20.54999999999999716, 66.65000000001180069, -81.87310748452438247 ) ) ;
#219315 = CARTESIAN_POINT ( 'NONE',  ( -16.89155683852818157, 62.92151589033651504, -213.7331200518002845 ) ) ;
#219316 = CARTESIAN_POINT ( 'NONE',  ( 21.00000000000000000, 9.750000000011153745, -45.85000000000000142 ) ) ;
#219317 = AXIS2_PLACEMENT_3D ( 'NONE', #192572, #252525, #54325 ) ;
#219319 = DIRECTION ( 'NONE',  ( 0.000000000000000000, 0.000000000000000000, -1.000000000000000000 ) ) ;
#219318 = CARTESIAN_POINT ( 'NONE',  ( -22.39999999999999503, 76.00000000001219291, -144.3138870828977076 ) ) ;
#219320 = CARTESIAN_POINT ( 'NONE',  ( -18.35235881385853318, 58.57909272559864178, -223.9244268894767629 ) ) ;
#219321 = CARTESIAN_POINT ( 'NONE',  ( 20.02499999999999858, 66.25000000001223555, -148.8731074845244393 ) ) ;
#219322 = CARTESIAN_POINT ( 'NONE',  ( -22.50000000000000000, 64.35012909624795441, -136.6056273753972903 ) ) ;
#219323 = VERTEX_POINT ( 'NONE', #66480 ) ;
#219324 = DIRECTION ( 'NONE',  ( 0.000000000000000000, 0.000000000000000000, 1.000000000000000000 ) ) ;
#219326 = ORIENTED_EDGE ( 'NONE', *, *, #211355, .T. ) ;
#219325 = DIRECTION ( 'NONE',  ( 1.000000000000000000, -0.000000000000000000, -0.000000000000000000 ) ) ;
#219327 = CARTESIAN_POINT ( 'NONE',  ( 20.95325940946048249, 65.47660992931635349, -195.9586453552843466 ) ) ;
#219328 = DIRECTION ( 'NONE',  ( 0.000000000000000000, -0.008583690987162452199, 0.9999631594459053030 ) ) ;
#219330 = DIRECTION ( 'NONE',  ( 0.000000000000000000, 0.2617529984165036239, 0.9651348961777156399 ) ) ;
#219329 = DIRECTION ( 'NONE',  ( 0.000000000000000000, 0.4088369013363306603, -0.9126074666063758167 ) ) ;
#219331 = EDGE_CURVE ( 'NONE', #94835, #235074, #89442, .T. ) ;
#219332 = ORIENTED_EDGE ( 'NONE', *, *, #134225, .T. ) ;
#219333 = DIRECTION ( 'NONE',  ( -1.000000000000000000, -2.952720810173289112E-16, 0.000000000000000000 ) ) ;
#219334 = LINE ( 'NONE', #195952, #45590 ) ;
#219335 = DIRECTION ( 'NONE',  ( 0.000000000000000000, -1.000000000000000000, -0.000000000000000000 ) ) ;
#219336 = CARTESIAN_POINT ( 'NONE',  ( 20.95000000000005613, 67.75000000001118394, -3.123107484524795474 ) ) ;
#219337 = CARTESIAN_POINT ( 'NONE',  ( -15.06720934482786234, 66.58230930894947619, -185.3815067877598324 ) ) ;
#219338 = EDGE_LOOP ( 'NONE', ( #59237, #163830, #72976, #101762 ) ) ;
#219339 = CYLINDRICAL_SURFACE ( 'NONE', #226148, 14.30833333333333890 ) ;
#219340 = VECTOR ( 'NONE', #126096, 1000.000000000000114 ) ;
#219341 = VERTEX_POINT ( 'NONE', #225519 ) ;
#219342 = AXIS2_PLACEMENT_3D ( 'NONE', #230365, #51700, #210806 ) ;
#219343 = CIRCLE ( 'NONE', #177694, 0.1000000000000028644 ) ;
#219344 = AXIS2_PLACEMENT_3D ( 'NONE', #99484, #179089, #239028 ) ;
#219345 = CARTESIAN_POINT ( 'NONE',  ( -21.45000000000000284, 7.708578643773852157, -121.7500000000000426 ) ) ;
#219346 = ORIENTED_EDGE ( 'NONE', *, *, #255090, .F. ) ;
#219347 = EDGE_CURVE ( 'NONE', #135358, #190027, #126447, .T. ) ;
#219348 = DIRECTION ( 'NONE',  ( 1.000000000000000000, 0.000000000000000000, 0.000000000000000000 ) ) ;
#219349 = EDGE_LOOP ( 'NONE', ( #216802, #225883, #227594 ) ) ;
#219350 = AXIS2_PLACEMENT_3D ( 'NONE', #200600, #75542, #199326 ) ;
#219351 = DIRECTION ( 'NONE',  ( -1.000000000000000000, 0.000000000000000000, 0.000000000000000000 ) ) ;
#219352 = DIRECTION ( 'NONE',  ( 1.000000000000000000, 0.000000000000000000, -0.000000000000000000 ) ) ;
#219353 = ORIENTED_EDGE ( 'NONE', *, *, #136604, .F. ) ;
#219354 = AXIS2_PLACEMENT_3D ( 'NONE', #497, #196148, #159602 ) ;
#219355 = CARTESIAN_POINT ( 'NONE',  ( -16.83794479845801817, 9.926357419362647150, -87.69644470422234406 ) ) ;
#219357 = VECTOR ( 'NONE', #152541, 1000.000000000000000 ) ;
#219356 = DIRECTION ( 'NONE',  ( -1.000000000000000000, 0.000000000000000000, 0.000000000000000000 ) ) ;
#219358 = DIRECTION ( 'NONE',  ( -1.000000000000000000, 0.000000000000000000, 0.000000000000000000 ) ) ;
#219359 = AXIS2_PLACEMENT_3D ( 'NONE', #41683, #79489, #181198 ) ;
#219360 = CARTESIAN_POINT ( 'NONE',  ( -21.04999999999999716, 47.00127771169579916, -255.4372249185379928 ) ) ;
#219361 = DIRECTION ( 'NONE',  ( 0.000000000000000000, 0.2617529984165039569, 0.9651348961777155289 ) ) ;
#219362 = DIRECTION ( 'NONE',  ( -0.000000000000000000, 0.4721928772777345684, 0.8814952561688429444 ) ) ;
#219363 = VERTEX_POINT ( 'NONE', #186438 ) ;
#219364 = DIRECTION ( 'NONE',  ( -1.000000000000000000, 0.000000000000000000, 0.000000000000000000 ) ) ;
#219365 = EDGE_LOOP ( 'NONE', ( #79060, #956, #89626, #77887 ) ) ;
#219367 = ORIENTED_EDGE ( 'NONE', *, *, #219503, .T. ) ;
#219366 = CARTESIAN_POINT ( 'NONE',  ( 23.24999999999999645, 5.000000000011153745, -155.0947339810869323 ) ) ;
#219368 = ORIENTED_EDGE ( 'NONE', *, *, #233065, .F. ) ;
#219369 = FACE_OUTER_BOUND ( 'NONE', #202613, .T. ) ;
#219370 = FACE_OUTER_BOUND ( 'NONE', #65680, .T. ) ;
#219371 = CARTESIAN_POINT ( 'NONE',  ( -18.59999999999999787, 38.29773864426885410, -236.0513742605307925 ) ) ;
#219372 = CARTESIAN_POINT ( 'NONE',  ( 21.11344571971201134, 60.18902167132765157, -221.2568027326728384 ) ) ;
#219373 = CARTESIAN_POINT ( 'NONE',  ( 21.05000000000000071, 87.65000000001144542, -38.92310748452424463 ) ) ;
#219374 = VERTEX_POINT ( 'NONE', #181309 ) ;
#219375 = FACE_OUTER_BOUND ( 'NONE', #242682, .T. ) ;
#219376 = CARTESIAN_POINT ( 'NONE',  ( 20.94999999999999929, -8.730841121484166578, -191.4019252810156217 ) ) ;
#219377 = ORIENTED_EDGE ( 'NONE', *, *, #138970, .T. ) ;
#219378 = ADVANCED_FACE ( 'NONE', ( #70361 ), #192855, .F. ) ;
#219379 = CARTESIAN_POINT ( 'NONE',  ( 18.50000000000000000, -9.399999999988823518, -174.7972597596632340 ) ) ;
#219380 = FACE_OUTER_BOUND ( 'NONE', #192217, .T. ) ;
#219381 = VERTEX_POINT ( 'NONE', #89876 ) ;
#219382 = AXIS2_PLACEMENT_3D ( 'NONE', #239149, #21410, #183038 ) ;
#219383 = AXIS2_PLACEMENT_3D ( 'NONE', #86615, #200177, #4523 ) ;
#219384 = VECTOR ( 'NONE', #215718, 1000.000000000000000 ) ;
#219385 = DIRECTION ( 'NONE',  ( -1.000000000000000000, -0.000000000000000000, -0.000000000000000000 ) ) ;
#219386 = ORIENTED_EDGE ( 'NONE', *, *, #61932, .T. ) ;
#219387 = LINE ( 'NONE', #117735, #8723 ) ;
#219388 = EDGE_CURVE ( 'NONE', #255868, #42929, #190292, .T. ) ;
#219389 = FACE_OUTER_BOUND ( 'NONE', #91587, .T. ) ;
#219390 = CARTESIAN_POINT ( 'NONE',  ( 20.99551997958375082, 64.25000000001249134, -176.8714483468348533 ) ) ;
#219391 = ADVANCED_FACE ( 'NONE', ( #149889 ), #33815, .T. ) ;
#219392 = DIRECTION ( 'NONE',  ( 0.000000000000000000, -0.5341055959867045955, 0.8454177738465681324 ) ) ;
#219393 = CIRCLE ( 'NONE', #248060, 11.69999999999998863 ) ;
#219394 = VECTOR ( 'NONE', #107376, 1000.000000000000000 ) ;
#219395 = EDGE_CURVE ( 'NONE', #229408, #56338, #227007, .T. ) ;
#219396 = VERTEX_POINT ( 'NONE', #229412 ) ;
#219397 = DIRECTION ( 'NONE',  ( 0.000000000000000000, -6.982962677686266711E-15, 1.000000000000000000 ) ) ;
#219398 = CIRCLE ( 'NONE', #106980, 0.1000000000000028644 ) ;
#219399 = ORIENTED_EDGE ( 'NONE', *, *, #191621, .F. ) ;
#219400 = CARTESIAN_POINT ( 'NONE',  ( 18.39999999999999858, 37.94390843806124991, -261.1300795796834109 ) ) ;
#219401 = PLANE ( 'NONE',  #4166 ) ;
#219403 = ORIENTED_EDGE ( 'NONE', *, *, #77126, .T. ) ;
#219402 = CYLINDRICAL_SURFACE ( 'NONE', #83669, 0.09999999999998898659 ) ;
#219404 = DIRECTION ( 'NONE',  ( -1.000000000000000000, 0.000000000000000000, 0.000000000000000000 ) ) ;
#219405 = EDGE_CURVE ( 'NONE', #247452, #248444, #28685, .T. ) ;
#219406 = FACE_OUTER_BOUND ( 'NONE', #247785, .T. ) ;
#219407 = DIRECTION ( 'NONE',  ( 0.000000000000000000, -6.982962677686266711E-15, 1.000000000000000000 ) ) ;
#219408 = CARTESIAN_POINT ( 'NONE',  ( -16.87683809663752399, 9.850000000011144508, -80.40236401819635148 ) ) ;
#219409 = DIRECTION ( 'NONE',  ( 1.000000000000000000, -0.000000000000000000, -0.000000000000000000 ) ) ;
#219410 = FACE_OUTER_BOUND ( 'NONE', #217864, .T. ) ;
#219412 = ORIENTED_EDGE ( 'NONE', *, *, #192042, .T. ) ;
#219411 = CARTESIAN_POINT ( 'NONE',  ( -21.05000000000000071, -11.38316329222462464, -203.4791315943886048 ) ) ;
#219413 = EDGE_CURVE ( 'NONE', #37087, #89611, #230700, .T. ) ;
#219414 = AXIS2_PLACEMENT_3D ( 'NONE', #213120, #151893, #37086 ) ;
#219415 = CARTESIAN_POINT ( 'NONE',  ( 22.88900146558018989, 67.29609520889904672, -90.37310748452436826 ) ) ;
#219416 = ORIENTED_EDGE ( 'NONE', *, *, #118507, .T. ) ;
#219417 = EDGE_LOOP ( 'NONE', ( #157351, #143436, #94825, #61904 ) ) ;
#219418 = FACE_OUTER_BOUND ( 'NONE', #163388, .T. ) ;
#219419 = CARTESIAN_POINT ( 'NONE',  ( 21.13461538461538325, 23.02743022372036918, -230.2075788195831763 ) ) ;
#219420 = CIRCLE ( 'NONE', #65319, 0.2000000000000000944 ) ;
#219421 = ORIENTED_EDGE ( 'NONE', *, *, #22146, .T. ) ;
#219422 = CARTESIAN_POINT ( 'NONE',  ( -20.94999999999999929, -11.39257802170567224, -3.073949579831933843 ) ) ;
#219423 = EDGE_CURVE ( 'NONE', #250224, #192087, #143617, .T. ) ;
#219424 = DIRECTION ( 'NONE',  ( 0.000000000000000000, 0.000000000000000000, -1.000000000000000000 ) ) ;
#219425 = CIRCLE ( 'NONE', #177777, 0.09999999999999939493 ) ;
#219426 = ORIENTED_EDGE ( 'NONE', *, *, #32846, .T. ) ;
#219427 = CIRCLE ( 'NONE', #57109, 0.1000000000000053069 ) ;
#219428 = DIRECTION ( 'NONE',  ( 0.000000000000000000, -2.775557561562888827E-14, 1.000000000000000000 ) ) ;
#219429 = DIRECTION ( 'NONE',  ( -1.000000000000000000, 0.000000000000000000, 0.000000000000000000 ) ) ;
#219430 = MECHANICAL_DESIGN_GEOMETRIC_PRESENTATION_REPRESENTATION (  '', ( #202701 ), #98608 ) ;
#219431 = EDGE_CURVE ( 'NONE', #111551, #81780, #93736, .T. ) ;
#219432 = ORIENTED_EDGE ( 'NONE', *, *, #54123, .T. ) ;
#219433 = VERTEX_POINT ( 'NONE', #127746 ) ;
#219435 = CARTESIAN_POINT ( 'NONE',  ( 23.14999999999999147, 76.00000000001213607, -136.5231074845242745 ) ) ;
#219434 = CIRCLE ( 'NONE', #252761, 0.1999999999999987899 ) ;
#219436 = ORIENTED_EDGE ( 'NONE', *, *, #242116, .T. ) ;
#219437 = DIRECTION ( 'NONE',  ( 1.186688945009010077E-16, 0.4088369013363281623, -0.9126074666063771490 ) ) ;
#219438 = AXIS2_PLACEMENT_3D ( 'NONE', #132705, #75317, #32342 ) ;
#219439 = ORIENTED_EDGE ( 'NONE', *, *, #82897, .F. ) ;
#219441 = ORIENTED_EDGE ( 'NONE', *, *, #150171, .F. ) ;
#219440 = DIRECTION ( 'NONE',  ( -6.938893903907222067E-15, 1.000000000000000000, 0.000000000000000000 ) ) ;
#219442 = ADVANCED_FACE ( 'NONE', ( #172037 ), #72932, .F. ) ;
#219443 = FACE_OUTER_BOUND ( 'NONE', #92238, .T. ) ;
#219444 = ORIENTED_EDGE ( 'NONE', *, *, #30815, .F. ) ;
#219445 = CARTESIAN_POINT ( 'NONE',  ( -21.46681500597866332, 1.115542391533913547E-11, -93.64248884057226974 ) ) ;
#219446 = ORIENTED_EDGE ( 'NONE', *, *, #151648, .F. ) ;
#219448 = ORIENTED_EDGE ( 'NONE', *, *, #175841, .T. ) ;
#219447 = EDGE_LOOP ( 'NONE', ( #156451, #164657, #138129, #113528 ) ) ;
#219449 = DIRECTION ( 'NONE',  ( 0.000000000000000000, 2.168404344971021884E-15, 1.000000000000000000 ) ) ;
#219450 = ORIENTED_EDGE ( 'NONE', *, *, #73468, .T. ) ;
#219451 = EDGE_CURVE ( 'NONE', #117271, #16498, #147920, .T. ) ;
#219452 = FACE_OUTER_BOUND ( 'NONE', #112904, .T. ) ;
#219454 = ORIENTED_EDGE ( 'NONE', *, *, #177165, .F. ) ;
#219453 = VECTOR ( 'NONE', #135614, 1000.000000000000000 ) ;
#219455 = EDGE_CURVE ( 'NONE', #256947, #117242, #71629, .T. ) ;
#219456 = AXIS2_PLACEMENT_3D ( 'NONE', #127430, #167869, #229102 ) ;
#219457 = VECTOR ( 'NONE', #17232, 1000.000000000000114 ) ;
#219458 = ORIENTED_EDGE ( 'NONE', *, *, #113053, .T. ) ;
#219459 =( GEOMETRIC_REPRESENTATION_CONTEXT ( 3 ) GLOBAL_UNCERTAINTY_ASSIGNED_CONTEXT ( ( #152071 ) ) GLOBAL_UNIT_ASSIGNED_CONTEXT ( ( #358, #103297, #79873 ) ) REPRESENTATION_CONTEXT ( 'NONE', 'WORKASPACE' ) );
#219460 = FACE_OUTER_BOUND ( 'NONE', #233135, .T. ) ;
#219461 = LINE ( 'NONE', #222019, #18177 ) ;
#219462 = EDGE_CURVE ( 'NONE', #6661, #91518, #85506, .T. ) ;
#219464 = EDGE_LOOP ( 'NONE', ( #38851, #207250, #76751, #29976, #65606 ) ) ;
#219463 = CARTESIAN_POINT ( 'NONE',  ( 22.39999999999999503, -2.598867842139048090, -189.5410128746472083 ) ) ;
#219465 = LINE ( 'NONE', #160822, #143926 ) ;
#219466 = EDGE_LOOP ( 'NONE', ( #214787, #156330, #75950, #156155 ) ) ;
#219467 = CIRCLE ( 'NONE', #19584, 0.1000000000000124678 ) ;
#219468 = CARTESIAN_POINT ( 'NONE',  ( -18.55807992284872299, 65.67101464000523947, -130.9404391622479977 ) ) ;
#219469 = TOROIDAL_SURFACE ( 'NONE', #107046, 11.70000000000000107, 0.1000000000000000056 ) ;
#219470 = LINE ( 'NONE', #182947, #135545 ) ;
#219472 = ORIENTED_EDGE ( 'NONE', *, *, #252316, .T. ) ;
#219471 = EDGE_CURVE ( 'NONE', #144130, #163114, #43860, .T. ) ;
#219474 = EDGE_CURVE ( 'NONE', #165247, #233834, #131323, .T. ) ;
#219473 = FACE_OUTER_BOUND ( 'NONE', #16728, .T. ) ;
#219475 = DIRECTION ( 'NONE',  ( 1.000000000000000000, 0.000000000000000000, 0.000000000000000000 ) ) ;
#219477 = DIRECTION ( 'NONE',  ( 2.952720810173289112E-16, 1.000000000000000000, 6.467318590049456648E-15 ) ) ;
#219476 = B_SPLINE_CURVE_WITH_KNOTS ( 'NONE', 3,
 ( #199024, #159917, #36116, #218564 ),
 .UNSPECIFIED., .F., .F.,
 ( 4, 4 ),
 ( 0.000000000000000000, 0.001767853679387103869 ),
 .UNSPECIFIED. ) ;
#219478 = B_SPLINE_CURVE_WITH_KNOTS ( 'NONE', 3,
 ( #25383, #144009, #223537, #239275, #60615, #69641 ),
 .UNSPECIFIED., .F., .F.,
 ( 4, 2, 4 ),
 ( 0.000000000000000000, 0.0001569047307838624609, 0.0003138094615677249218 ),
 .UNSPECIFIED. ) ;
#219479 = ORIENTED_EDGE ( 'NONE', *, *, #51382, .F. ) ;
#219480 = CARTESIAN_POINT ( 'NONE',  ( -18.40000000000000213, 53.37686160793744961, -235.8706811220569932 ) ) ;
#219481 = EDGE_LOOP ( 'NONE', ( #70445, #200897, #221728, #84023 ) ) ;
#219482 = ORIENTED_EDGE ( 'NONE', *, *, #57355, .T. ) ;
#219483 = VECTOR ( 'NONE', #175013, 1000.000000000000000 ) ;
#219484 = DIRECTION ( 'NONE',  ( 0.000000000000000000, -0.8814952561688423893, 0.4721928772777359007 ) ) ;
#219485 = EDGE_CURVE ( 'NONE', #125182, #4469, #187731, .T. ) ;
#219486 = VERTEX_POINT ( 'NONE', #250249 ) ;
#219487 = VERTEX_POINT ( 'NONE', #148592 ) ;
#219488 = CARTESIAN_POINT ( 'NONE',  ( -16.90137573187933739, 9.950000000011135270, -79.78841742409694859 ) ) ;
#219489 = LINE ( 'NONE', #89927, #37634 ) ;
#219490 = ORIENTED_EDGE ( 'NONE', *, *, #172077, .T. ) ;
#219491 = ORIENTED_EDGE ( 'NONE', *, *, #15509, .T. ) ;
#219492 = FACE_OUTER_BOUND ( 'NONE', #125250, .T. ) ;
#219493 = ADVANCED_FACE ( 'NONE', ( #129029 ), #131583, .F. ) ;
#219494 = CYLINDRICAL_SURFACE ( 'NONE', #131584, 11.80000000000000426 ) ;
#219495 = ORIENTED_EDGE ( 'NONE', *, *, #136107, .T. ) ;
#219496 = AXIS2_PLACEMENT_3D ( 'NONE', #37071, #196123, #117850 ) ;
#219497 = EDGE_LOOP ( 'NONE', ( #90212, #33552, #127600, #254208 ) ) ;
#219498 = ORIENTED_EDGE ( 'NONE', *, *, #115475, .F. ) ;
#219499 = VECTOR ( 'NONE', #174340, 999.9999999999998863 ) ;
#219500 = CARTESIAN_POINT ( 'NONE',  ( -22.59999999999999787, 0.1008583691098682150, -155.7504328765105868 ) ) ;
#219501 = EDGE_CURVE ( 'NONE', #19663, #131047, #160594, .T. ) ;
#219502 = DIRECTION ( 'NONE',  ( 0.000000000000000000, 0.9126074666063602736, 0.4088369013363654103 ) ) ;
#219503 = EDGE_CURVE ( 'NONE', #96682, #154226, #2479, .T. ) ;
#219504 = CARTESIAN_POINT ( 'NONE',  ( -16.77828822459933633, 14.15263002279597693, -219.2435359409537625 ) ) ;
#219505 = FACE_OUTER_BOUND ( 'NONE', #4345, .T. ) ;
#219506 = AXIS2_PLACEMENT_3D ( 'NONE', #31872, #188349, #86647 ) ;
#219507 = CARTESIAN_POINT ( 'NONE',  ( 22.39999999999999503, 0.2612980822699583205, -230.0539506776466681 ) ) ;
#219508 = DIRECTION ( 'NONE',  ( -1.000000000000000000, 0.000000000000000000, 0.000000000000000000 ) ) ;
#219509 = AXIS2_PLACEMENT_3D ( 'NONE', #181658, #145075, #2993 ) ;
#219510 = CARTESIAN_POINT ( 'NONE',  ( -19.99999999999999645, 5.488301202077012775, 16.50000000000000000 ) ) ;
#219512 = CYLINDRICAL_SURFACE ( 'NONE', #16232, 0.09999999999999939493 ) ;
#219511 = CARTESIAN_POINT ( 'NONE',  ( -20.94999999999999929, 77.16412189325258453, -28.30825939895270693 ) ) ;
#219514 = CIRCLE ( 'NONE', #136106, 4.100000000000000533 ) ;
#219513 = FACE_OUTER_BOUND ( 'NONE', #142262, .T. ) ;
#219515 = AXIS2_PLACEMENT_3D ( 'NONE', #147080, #127537, #227921 ) ;
#219516 = CARTESIAN_POINT ( 'NONE',  ( -16.83233564386406655, 23.07933777265768782, -231.0117482525610626 ) ) ;
#219517 = ADVANCED_FACE ( 'NONE', ( #162885 ), #143288, .F. ) ;
#219518 = CARTESIAN_POINT ( 'NONE',  ( -18.79999999999999716, -11.75000000000000000, 32.89999999999999858 ) ) ;
#219519 = DIRECTION ( 'NONE',  ( 1.000000000000000000, 0.000000000000000000, 0.000000000000000000 ) ) ;
#219521 = ORIENTED_EDGE ( 'NONE', *, *, #20376, .F. ) ;
#219520 = VECTOR ( 'NONE', #143176, 1000.000000000000000 ) ;
#219523 = EDGE_LOOP ( 'NONE', ( #171302, #205725, #245506, #231375 ) ) ;
#219522 = DIRECTION ( 'NONE',  ( 0.000000000000000000, 0.8660254037844377084, 0.5000000000000016653 ) ) ;
#219524 = CARTESIAN_POINT ( 'NONE',  ( -23.15000000000000213, 87.48912529308798014, -106.0231074845242176 ) ) ;
#219525 = CARTESIAN_POINT ( 'NONE',  ( 21.07928932188134397, 0.09889514566555242248, -127.6714833436067238 ) ) ;
#219526 = AXIS2_PLACEMENT_3D ( 'NONE', #235894, #156410, #134224 ) ;
#219527 = CARTESIAN_POINT ( 'NONE',  ( -22.43310005002225438, 64.17650015117389728, -247.0971464675484413 ) ) ;
#219528 = ORIENTED_EDGE ( 'NONE', *, *, #188905, .F. ) ;
#219529 = CIRCLE ( 'NONE', #44765, 2.000000000000001776 ) ;
#219530 = EDGE_CURVE ( 'NONE', #238989, #193535, #106712, .T. ) ;
#219531 = CARTESIAN_POINT ( 'NONE',  ( 23.15000000000000213, 87.75000000001205080, -124.3731074845242119 ) ) ;
#219532 = EDGE_CURVE ( 'NONE', #103174, #213687, #67601, .T. ) ;
#219533 = CARTESIAN_POINT ( 'NONE',  ( -20.94999999999999929, 1.835341550235567887, -145.6551512925629766 ) ) ;
#219534 = ORIENTED_EDGE ( 'NONE', *, *, #22545, .T. ) ;
#219535 = AXIS2_PLACEMENT_3D ( 'NONE', #151737, #232555, #72187 ) ;
#219536 = CARTESIAN_POINT ( 'NONE',  ( -20.94999999999999929, 11.60000000001115339, -140.9282032302755852 ) ) ;
#219537 = DIRECTION ( 'NONE',  ( 0.000000000000000000, 0.000000000000000000, 1.000000000000000000 ) ) ;
#219538 = DIRECTION ( 'NONE',  ( -1.000000000000000000, -0.000000000000000000, -0.000000000000000000 ) ) ;
#219539 = EDGE_CURVE ( 'NONE', #122037, #60900, #239670, .T. ) ;
#219540 = CARTESIAN_POINT ( 'NONE',  ( 20.94999999999999929, 40.74071615341952679, -237.9411309446948337 ) ) ;
#219542 = ORIENTED_EDGE ( 'NONE', *, *, #23563, .F. ) ;
#219541 = DIRECTION ( 'NONE',  ( -0.000000000000000000, -0.000000000000000000, -1.000000000000000000 ) ) ;
#219544 = VERTEX_POINT ( 'NONE', #205834 ) ;
#219543 = CARTESIAN_POINT ( 'NONE',  ( -18.54260524012588007, 85.62421939008567051, -96.28233443875350872 ) ) ;
#219546 = ADVANCED_FACE ( 'NONE', ( #144562 ), #164152, .F. ) ;
#219545 = DIRECTION ( 'NONE',  ( -1.000000000000000000, 0.000000000000000000, 0.000000000000000000 ) ) ;
#219547 = CARTESIAN_POINT ( 'NONE',  ( -18.50000000000000000, 77.73625713160897988, -57.95445515550681392 ) ) ;
#219548 = CARTESIAN_POINT ( 'NONE',  ( 18.49999999999999645, 74.26374286841520700, -191.9544551555068779 ) ) ;
#219549 = CARTESIAN_POINT ( 'NONE',  ( -15.52965525596986929, 9.375538102059156387, -183.3698758809907474 ) ) ;
#219551 = DIRECTION ( 'NONE',  ( 0.000000000000000000, 0.000000000000000000, 1.000000000000000000 ) ) ;
#219550 = CARTESIAN_POINT ( 'NONE',  ( -16.91256925476570672, 66.01426884188362010, -82.05546499551910244 ) ) ;
#219553 = EDGE_CURVE ( 'NONE', #62069, #21878, #147135, .T. ) ;
#219552 = CARTESIAN_POINT ( 'NONE',  ( 18.49999999999996803, 7.070967871809997973, -104.2465642218683541 ) ) ;
#219554 = DIRECTION ( 'NONE',  ( -1.000000000000000000, -4.163336342344362270E-13, 8.326672684688724540E-13 ) ) ;
#219555 = FACE_OUTER_BOUND ( 'NONE', #11772, .T. ) ;
#219556 = VECTOR ( 'NONE', #79463, 1000.000000000000000 ) ;
#219557 = AXIS2_PLACEMENT_3D ( 'NONE', #28511, #3761, #187561 ) ;
#219558 = CARTESIAN_POINT ( 'NONE',  ( -21.14999999999999858, 79.23417978893665747, -236.1056577391152587 ) ) ;
#219559 = CIRCLE ( 'NONE', #52967, 11.65000000000000036 ) ;
#219560 = AXIS2_PLACEMENT_3D ( 'NONE', #78160, #22071, #241124 ) ;
#219561 = ORIENTED_EDGE ( 'NONE', *, *, #208362, .F. ) ;
#219562 = EDGE_CURVE ( 'NONE', #16612, #44305, #97990, .T. ) ;
#219563 = DIRECTION ( 'NONE',  ( 1.000000000000000000, 0.000000000000000000, 0.000000000000000000 ) ) ;
#219565 = EDGE_CURVE ( 'NONE', #134711, #102952, #135601, .T. ) ;
#219564 = EDGE_CURVE ( 'NONE', #34850, #161554, #244955, .T. ) ;
#219566 = ORIENTED_EDGE ( 'NONE', *, *, #99096, .T. ) ;
#219567 = EDGE_LOOP ( 'NONE', ( #16083, #1411, #220892, #253036 ) ) ;
#219568 = CARTESIAN_POINT ( 'NONE',  ( 20.75572585718184726, 67.11768327161587422, -94.52584908581822276 ) ) ;
#219569 = DIRECTION ( 'NONE',  ( -1.000000000000000000, -2.952720810173289112E-16, 0.000000000000000000 ) ) ;
#219570 = ORIENTED_EDGE ( 'NONE', *, *, #232251, .T. ) ;
#219571 = ORIENTED_EDGE ( 'NONE', *, *, #47644, .T. ) ;
#219572 = VECTOR ( 'NONE', #35374, 1000.000000000000000 ) ;
#219573 = AXIS2_PLACEMENT_3D ( 'NONE', #50638, #31139, #29844 ) ;
#219574 = VERTEX_POINT ( 'NONE', #166746 ) ;
#219575 = ADVANCED_FACE ( 'NONE', ( #81997 ), #25926, .T. ) ;
#219576 = EDGE_CURVE ( 'NONE', #159934, #161458, #101563, .T. ) ;
#219577 = ORIENTED_EDGE ( 'NONE', *, *, #229107, .F. ) ;
#219578 = CARTESIAN_POINT ( 'NONE',  ( -18.59999999999999787, -10.64999999999999325, 31.39999999999999858 ) ) ;
#219579 = LINE ( 'NONE', #155800, #24449 ) ;
#219580 = VECTOR ( 'NONE', #151782, 1000.000000000000114 ) ;
#219581 = DIRECTION ( 'NONE',  ( 0.000000000000000000, 0.5469332180710856361, -0.8371762388950170219 ) ) ;
#219582 = CARTESIAN_POINT ( 'NONE',  ( -21.05000000000000071, 28.24160076078326753, -259.1231640893983581 ) ) ;
#219583 = DIRECTION ( 'NONE',  ( 1.000000000000000000, 0.000000000000000000, 0.000000000000000000 ) ) ;
#219584 = ADVANCED_FACE ( 'NONE', ( #181155 ), #65034, .T. ) ;
#219585 = CARTESIAN_POINT ( 'NONE',  ( -20.64999999999999858, 1.940186915899009490, -113.3291192110533672 ) ) ;
#219586 = CARTESIAN_POINT ( 'NONE',  ( 21.05000000000000071, 75.96798630682417297, -142.7819502080616303 ) ) ;
#219588 = ORIENTED_EDGE ( 'NONE', *, *, #258058, .T. ) ;
#219587 = CARTESIAN_POINT ( 'NONE',  ( -21.04999999999994387, 65.15000000001120384, -51.02310748452479316 ) ) ;
#219590 = DIRECTION ( 'NONE',  ( -1.000000000000000000, 0.000000000000000000, 0.000000000000000000 ) ) ;
#219589 = CARTESIAN_POINT ( 'NONE',  ( -16.84419801905645286, 66.05000000001223270, -149.1925973307465085 ) ) ;
#219591 = DIRECTION ( 'NONE',  ( 0.000000000000000000, 0.2617529984165033463, 0.9651348961777157509 ) ) ;
#219592 = EDGE_CURVE ( 'NONE', #224075, #59451, #206359, .T. ) ;
#219593 = VERTEX_POINT ( 'NONE', #83290 ) ;
#219594 = CARTESIAN_POINT ( 'NONE',  ( -18.47653818581420637, 8.940896014627114141, -245.4411290137018113 ) ) ;
#219595 = SURFACE_STYLE_FILL_AREA ( #1826 ) ;
#219596 = VERTEX_POINT ( 'NONE', #125026 ) ;
#219597 = EDGE_CURVE ( 'NONE', #176803, #167022, #118884, .T. ) ;
#219599 = CARTESIAN_POINT ( 'NONE',  ( 20.94999999999999929, 8.531609279343539853, -209.3937462695851366 ) ) ;
#219598 = DIRECTION ( 'NONE',  ( -0.000000000000000000, 0.9876197685951241256, 0.1568667991644932258 ) ) ;
#219600 = TOROIDAL_SURFACE ( 'NONE', #32195, 12.97499999999999609, 0.1000000000000000056 ) ;
#219601 = CARTESIAN_POINT ( 'NONE',  ( -16.85697194749126027, 66.09145628588818511, -82.45811175213816568 ) ) ;
#219602 = LINE ( 'NONE', #97055, #159518 ) ;
#219603 = EDGE_LOOP ( 'NONE', ( #101372, #84723, #30194, #152306, #199840 ) ) ;
#219604 = CARTESIAN_POINT ( 'NONE',  ( 21.13422380239055087, 6.493326514816704531, -67.00000000000004263 ) ) ;
#219605 = CARTESIAN_POINT ( 'NONE',  ( -18.59999999999999787, 74.13328508995456900, -91.27043223824230722 ) ) ;
#219606 = DIRECTION ( 'NONE',  ( 0.000000000000000000, 0.000000000000000000, 1.000000000000000000 ) ) ;
#219607 = DIRECTION ( 'NONE',  ( 0.000000000000000000, -7.086529944415886769E-15, 1.000000000000000000 ) ) ;
#219609 = EDGE_CURVE ( 'NONE', #137324, #60290, #145847, .T. ) ;
#219608 = DIRECTION ( 'NONE',  ( 0.000000000000000000, 0.000000000000000000, 1.000000000000000000 ) ) ;
#219610 = ORIENTED_EDGE ( 'NONE', *, *, #181564, .F. ) ;
#219611 = AXIS2_PLACEMENT_3D ( 'NONE', #206813, #50283, #128561 ) ;
#219612 = DIRECTION ( 'NONE',  ( 0.000000000000000000, 0.9126074666063844765, 0.4088369013363114535 ) ) ;
#219613 = CIRCLE ( 'NONE', #215346, 11.69999999999999574 ) ;
#219615 = EDGE_CURVE ( 'NONE', #22587, #216057, #27234, .T. ) ;
#219614 = DIRECTION ( 'NONE',  ( 0.000000000000000000, 1.000000000000000000, 7.272083257015735086E-15 ) ) ;
#219616 = LINE ( 'NONE', #41018, #165804 ) ;
#219617 = CYLINDRICAL_SURFACE ( 'NONE', #34262, 0.09999999999999939493 ) ;
#219618 = AXIS2_PLACEMENT_3D ( 'NONE', #94655, #95928, #174247 ) ;
#219620 = PLANE ( 'NONE',  #253263 ) ;
#219619 = TOROIDAL_SURFACE ( 'NONE', #15672, 12.77499999999999858, 0.1000000000000000056 ) ;
#219621 = CARTESIAN_POINT ( 'NONE',  ( -21.05000000000000071, -11.64999999998884483, -67.00000000000004263 ) ) ;
#219622 = PRODUCT_DEFINITION_FORMATION_WITH_SPECIFIED_SOURCE ( 'ANY', '', #130599, .NOT_KNOWN. ) ;
#219624 = ORIENTED_EDGE ( 'NONE', *, *, #110111, .T. ) ;
#219623 = CARTESIAN_POINT ( 'NONE',  ( 21.05095171578076574, 8.776179878782192745, -179.6658732766378535 ) ) ;
#219625 = DIRECTION ( 'NONE',  ( 0.000000000000000000, 0.000000000000000000, -1.000000000000000000 ) ) ;
#219626 = CIRCLE ( 'NONE', #65506, 0.09999999999999971412 ) ;
#219627 = CARTESIAN_POINT ( 'NONE',  ( -21.55000000000000071, 7.350000000011155166, -179.7499999999999716 ) ) ;
#219628 = DIRECTION ( 'NONE',  ( 1.000000000000000000, 0.000000000000000000, 0.000000000000000000 ) ) ;
#219629 = CARTESIAN_POINT ( 'NONE',  ( -18.59999999999999787, 1.115600667400684642E-11, -134.0000000000000000 ) ) ;
#219630 = ADVANCED_FACE ( 'NONE', ( #11504 ), #8923, .F. ) ;
#219631 = CIRCLE ( 'NONE', #107206, 0.1000000000000064587 ) ;
#219632 = LINE ( 'NONE', #41031, #129557 ) ;
#219634 = ORIENTED_EDGE ( 'NONE', *, *, #180240, .F. ) ;
#219633 = DIRECTION ( 'NONE',  ( 0.000000000000000000, -0.4088369013363297166, 0.9126074666063763718 ) ) ;
#219635 = CARTESIAN_POINT ( 'NONE',  ( 23.15000000000000213, -11.74999999998883560, -146.1500000000000341 ) ) ;
#219636 = CYLINDRICAL_SURFACE ( 'NONE', #17817, 0.09999999999999939493 ) ;
#219637 = DIRECTION ( 'NONE',  ( -0.000000000000000000, -0.9770955615653316162, -0.2128009952263604232 ) ) ;
#219638 = ORIENTED_EDGE ( 'NONE', *, *, #156023, .T. ) ;
#219639 = LINE ( 'NONE', #159688, #9519 ) ;
#219640 = CARTESIAN_POINT ( 'NONE',  ( 21.07928932188134397, 75.90110485435778287, -176.3516241409230929 ) ) ;
#219641 = DIRECTION ( 'NONE',  ( 0.000000000000000000, 0.000000000000000000, -1.000000000000000000 ) ) ;
#219642 = DIRECTION ( 'NONE',  ( 0.000000000000000000, 0.9684149032218615227, -0.2493442905257554076 ) ) ;
#219643 = CIRCLE ( 'NONE', #98812, 0.1000000000000028644 ) ;
#219644 = CARTESIAN_POINT ( 'NONE',  ( 21.05000000000000071, -1.835341550213257733, -45.05515129256298223 ) ) ;
#219645 = AXIS2_PLACEMENT_3D ( 'NONE', #187123, #110125, #7159 ) ;
#219646 = ORIENTED_EDGE ( 'NONE', *, *, #254311, .T. ) ;
#219647 = VERTEX_POINT ( 'NONE', #248826 ) ;
#219648 = TOROIDAL_SURFACE ( 'NONE', #169643, 0.2000000000000000111, 0.1000000000000000056 ) ;
#219649 = DIRECTION ( 'NONE',  ( 0.000000000000000000, 1.000000000000000000, -0.000000000000000000 ) ) ;
#219651 = CARTESIAN_POINT ( 'NONE',  ( -20.94999999999999929, 64.40000000001263913, -196.5949042542488883 ) ) ;
#219650 = CIRCLE ( 'NONE', #124380, 0.1999999999999987899 ) ;
#219652 = AXIS2_PLACEMENT_3D ( 'NONE', #23518, #1327, #181293 ) ;
#219653 = CARTESIAN_POINT ( 'NONE',  ( -16.77683809663752257, 66.05000000001153637, -48.67310748452439384 ) ) ;
#219654 = DIRECTION ( 'NONE',  ( 0.000000000000000000, 0.000000000000000000, -1.000000000000000000 ) ) ;
#219655 = VERTEX_POINT ( 'NONE', #32370 ) ;
#219656 = AXIS2_PLACEMENT_3D ( 'NONE', #118442, #197952, #19327 ) ;
#219657 = DIRECTION ( 'NONE',  ( 0.000000000000000000, 0.000000000000000000, 1.000000000000000000 ) ) ;
#219658 = FACE_OUTER_BOUND ( 'NONE', #13832, .T. ) ;
#219659 = DIRECTION ( 'NONE',  ( -0.000000000000000000, 7.272083257015735086E-15, -1.000000000000000000 ) ) ;
#219660 = CARTESIAN_POINT ( 'NONE',  ( -20.94999999999994600, 67.73741572762334329, -25.54575917482290848 ) ) ;
#219661 = CARTESIAN_POINT ( 'NONE',  ( -16.97683810757273193, 9.949999999999983302, -20.23642328753963682 ) ) ;
#219662 = VECTOR ( 'NONE', #91280, 1000.000000000000000 ) ;
#219663 = AXIS2_PLACEMENT_3D ( 'NONE', #39451, #219325, #198484 ) ;
#219664 = AXIS2_PLACEMENT_3D ( 'NONE', #256113, #16311, #78802 ) ;
#219665 = ORIENTED_EDGE ( 'NONE', *, *, #208396, .F. ) ;
#219667 = ORIENTED_EDGE ( 'NONE', *, *, #184442, .F. ) ;
#219666 = DIRECTION ( 'NONE',  ( 1.000000000000000000, 0.000000000000000000, 0.000000000000000000 ) ) ;
#219668 = ORIENTED_EDGE ( 'NONE', *, *, #236990, .T. ) ;
#219669 = CARTESIAN_POINT ( 'NONE',  ( -16.87372397896795206, 9.880599536641732072, -20.35072451003573946 ) ) ;
#219670 = ORIENTED_EDGE ( 'NONE', *, *, #68971, .T. ) ;
#219671 = CARTESIAN_POINT ( 'NONE',  ( -21.05000000000000071, 1.115527483754042032E-11, -26.95934304829876282 ) ) ;
#219672 = DIRECTION ( 'NONE',  ( 0.000000000000000000, 0.000000000000000000, -1.000000000000000000 ) ) ;
#219673 = FACE_OUTER_BOUND ( 'NONE', #73412, .T. ) ;
#219674 = VERTEX_POINT ( 'NONE', #29806 ) ;
#219675 = DIRECTION ( 'NONE',  ( 1.000000000000000000, 0.000000000000000000, 0.000000000000000000 ) ) ;
#219676 = CYLINDRICAL_SURFACE ( 'NONE', #222034, 0.1000000000000098310 ) ;
#219677 = ORIENTED_EDGE ( 'NONE', *, *, #223430, .F. ) ;
#219678 = CARTESIAN_POINT ( 'NONE',  ( 22.59999985501178799, 11.74986979301414181, -100.4344013302006005 ) ) ;
#219679 = AXIS2_PLACEMENT_3D ( 'NONE', #87105, #47985, #188784 ) ;
#219681 = ORIENTED_EDGE ( 'NONE', *, *, #91337, .T. ) ;
#219680 = DIRECTION ( 'NONE',  ( 1.000000000000000000, 2.171475777237622503E-16, -9.970532993647777410E-16 ) ) ;
#219682 = EDGE_CURVE ( 'NONE', #107353, #39176, #31090, .T. ) ;
#219683 = CARTESIAN_POINT ( 'NONE',  ( -23.25000000000000000, 1.115600667400684642E-11, -100.5000000000000284 ) ) ;
#219684 = CIRCLE ( 'NONE', #44735, 0.1000000000000028644 ) ;
#219685 = DIRECTION ( 'NONE',  ( -1.000000000000000000, 0.000000000000000000, 0.000000000000000000 ) ) ;
#219686 = CONICAL_SURFACE ( 'NONE', #103160, 4.000000000000000000, 0.7853981633974489451 ) ;
#219687 = ORIENTED_EDGE ( 'NONE', *, *, #81930, .T. ) ;
#219688 = CIRCLE ( 'NONE', #257240, 0.09999999999999939493 ) ;
#219689 = PLANE ( 'NONE',  #187804 ) ;
#219690 = DIRECTION ( 'NONE',  ( -1.000000000000000000, -0.000000000000000000, -0.000000000000000000 ) ) ;
#219691 = ORIENTED_EDGE ( 'NONE', *, *, #119559, .F. ) ;
#219692 = SPHERICAL_SURFACE ( 'NONE', #238233, 0.1000000000000000056 ) ;
#219693 = EDGE_CURVE ( 'NONE', #232936, #23864, #251373, .T. ) ;
#219694 = CARTESIAN_POINT ( 'NONE',  ( 13.12229106158772751, 49.47508301341328263, -233.4759538034894319 ) ) ;
#219695 = DIRECTION ( 'NONE',  ( -1.000000000000000000, 0.000000000000000000, 0.000000000000000000 ) ) ;
#219696 = AXIS2_PLACEMENT_3D ( 'NONE', #196700, #178461, #96304 ) ;
#219697 = EDGE_CURVE ( 'NONE', #124122, #6716, #229264, .T. ) ;
#219698 = ORIENTED_EDGE ( 'NONE', *, *, #154423, .F. ) ;
#219699 = AXIS2_PLACEMENT_3D ( 'NONE', #126261, #166717, #186259 ) ;
#219700 = CIRCLE ( 'NONE', #128332, 11.80000000000001137 ) ;
#219701 = AXIS2_PLACEMENT_3D ( 'NONE', #33424, #210737, #51625 ) ;
#219702 = EDGE_LOOP ( 'NONE', ( #124803, #50424, #52382, #219765 ) ) ;
#219703 = EDGE_CURVE ( 'NONE', #191212, #196725, #185504, .T. ) ;
#219704 = ORIENTED_EDGE ( 'NONE', *, *, #116788, .T. ) ;
#219705 = EDGE_CURVE ( 'NONE', #78372, #182093, #139692, .T. ) ;
#219706 = DIRECTION ( 'NONE',  ( 0.7071067811865474617, 0.7071067811865474617, 0.000000000000000000 ) ) ;
#219707 = CARTESIAN_POINT ( 'NONE',  ( 21.04999999999999716, 8.871279686006799281, -45.64999999999999858 ) ) ;
#219709 = VERTEX_POINT ( 'NONE', #12796 ) ;
#219708 = CARTESIAN_POINT ( 'NONE',  ( -19.89999999999999858, 5.586869315528661062, 16.41686199900910736 ) ) ;
#219710 = FACE_OUTER_BOUND ( 'NONE', #10742, .T. ) ;
#219711 = CARTESIAN_POINT ( 'NONE',  ( 21.05000000000000071, 87.48912529308769592, -66.42310748452423752 ) ) ;
#219712 = EDGE_CURVE ( 'NONE', #142261, #47754, #27324, .T. ) ;
#219713 = CARTESIAN_POINT ( 'NONE',  ( -22.50000000000000000, 11.36547683798380959, -198.4402660583092199 ) ) ;
#219714 = DIRECTION ( 'NONE',  ( 0.000000000000000000, 0.000000000000000000, 1.000000000000000000 ) ) ;
#219715 = DIRECTION ( 'NONE',  ( 1.000000000000000000, -3.151514657663852580E-16, 8.547182517843351137E-17 ) ) ;
#219716 = AXIS2_PLACEMENT_3D ( 'NONE', #46178, #41077, #22801 ) ;
#219717 = CARTESIAN_POINT ( 'NONE',  ( -21.44999999999999929, 68.85000000001254250, -182.2731074845244166 ) ) ;
#219719 = ORIENTED_EDGE ( 'NONE', *, *, #240870, .F. ) ;
#219718 = CARTESIAN_POINT ( 'NONE',  ( 20.85000000000000142, 43.35377423437995503, -245.1717807829448930 ) ) ;
#219721 = ORIENTED_EDGE ( 'NONE', *, *, #165798, .F. ) ;
#219720 = LINE ( 'NONE', #20259, #40378 ) ;
#219722 = CARTESIAN_POINT ( 'NONE',  ( 21.72449340488910252, 65.71604372252048165, -60.27310748452440237 ) ) ;
#219723 = EDGE_CURVE ( 'NONE', #202898, #62992, #189613, .T. ) ;
#219724 = ORIENTED_EDGE ( 'NONE', *, *, #11649, .T. ) ;
#219725 = ORIENTED_EDGE ( 'NONE', *, *, #140112, .F. ) ;
#219726 = CYLINDRICAL_SURFACE ( 'NONE', #30829, 0.8750000000000007772 ) ;
#219727 = DIRECTION ( 'NONE',  ( 0.000000000000000000, 0.1350103645451876666, 0.9908441862701600211 ) ) ;
#219728 = AXIS2_PLACEMENT_3D ( 'NONE', #233522, #190550, #195688 ) ;
#219729 = EDGE_CURVE ( 'NONE', #242995, #60888, #218801, .T. ) ;
#219730 = DIRECTION ( 'NONE',  ( -1.000000000000000000, 0.000000000000000000, 0.000000000000000000 ) ) ;
#219731 = DIRECTION ( 'NONE',  ( -1.000000000000000000, 0.000000000000000000, 0.000000000000000000 ) ) ;
#219732 = ADVANCED_FACE ( 'NONE', ( #148440 ), #102251, .T. ) ;
#219733 = DIRECTION ( 'NONE',  ( 0.000000000000000000, 0.000000000000000000, 1.000000000000000000 ) ) ;
#219734 = SPHERICAL_SURFACE ( 'NONE', #169788, 0.1000000000000000056 ) ;
#219735 = EDGE_CURVE ( 'NONE', #131441, #82237, #23210, .T. ) ;
#219736 = FACE_OUTER_BOUND ( 'NONE', #232636, .T. ) ;
#219737 = ORIENTED_EDGE ( 'NONE', *, *, #91006, .F. ) ;
#219738 = VERTEX_POINT ( 'NONE', #227968 ) ;
#219739 = DIRECTION ( 'NONE',  ( 1.000000000000000000, 0.000000000000000000, 0.000000000000000000 ) ) ;
#219740 = CIRCLE ( 'NONE', #57429, 0.09999999999999681366 ) ;
#219741 = ORIENTED_EDGE ( 'NONE', *, *, #86016, .F. ) ;
#219743 = DIRECTION ( 'NONE',  ( -1.000000000000000000, 0.000000000000000000, -0.000000000000000000 ) ) ;
#219742 = CIRCLE ( 'NONE', #190758, 0.1000000000000028644 ) ;
#219744 = CARTESIAN_POINT ( 'NONE',  ( 18.55807992284871588, 68.10318897902124036, -224.1464165264002588 ) ) ;
#219745 = CARTESIAN_POINT ( 'NONE',  ( -21.10000000000000142, 11.99999999999999822, 11.90000000000000036 ) ) ;
#219746 = CARTESIAN_POINT ( 'NONE',  ( 18.49999999999999289, 6.450000000011156587, -110.5170271704400591 ) ) ;
#219747 = EDGE_CURVE ( 'NONE', #156798, #221299, #208428, .T. ) ;
#219748 = ORIENTED_EDGE ( 'NONE', *, *, #193118, .F. ) ;
#219749 = CARTESIAN_POINT ( 'NONE',  ( -15.75000000000001421, 66.65000000001205649, -119.6588398769083454 ) ) ;
#219750 = ORIENTED_EDGE ( 'NONE', *, *, #194804, .F. ) ;
#219751 = CARTESIAN_POINT ( 'NONE',  ( 22.50000000000000000, 7.128833340093095217, -233.7327013124392749 ) ) ;
#219752 = VERTEX_POINT ( 'NONE', #233130 ) ;
#219753 = CARTESIAN_POINT ( 'NONE',  ( 23.14999999999999503, 11.75000000001115552, -121.7500000000000426 ) ) ;
#219754 = CARTESIAN_POINT ( 'NONE',  ( 14.45204356427542791, 9.450668889178684751, -182.5555464902073197 ) ) ;
#219755 = AXIS2_PLACEMENT_3D ( 'NONE', #178418, #98809, #59694 ) ;
#219756 = ORIENTED_EDGE ( 'NONE', *, *, #30530, .T. ) ;
#219757 = FACE_OUTER_BOUND ( 'NONE', #6658, .T. ) ;
#219759 = EDGE_LOOP ( 'NONE', ( #158870, #216774, #99948, #41870 ) ) ;
#219758 = DIRECTION ( 'NONE',  ( -0.000000000000000000, -0.2128009952263604232, 0.9770955615653316162 ) ) ;
#219760 = DIRECTION ( 'NONE',  ( 0.000000000000000000, -0.9910827722268050755, 0.1332476588733589318 ) ) ;
#219761 = ORIENTED_EDGE ( 'NONE', *, *, #100583, .T. ) ;
#219762 = EDGE_CURVE ( 'NONE', #188219, #44233, #72780, .T. ) ;
#219763 = CIRCLE ( 'NONE', #3275, 11.65000000000000036 ) ;
#219764 = DIRECTION ( 'NONE',  ( 0.000000000000000000, 0.000000000000000000, -1.000000000000000000 ) ) ;
#219765 = ORIENTED_EDGE ( 'NONE', *, *, #198870, .F. ) ;
#219766 = DIRECTION ( 'NONE',  ( -1.000000000000000000, 0.000000000000000000, 0.000000000000000000 ) ) ;
#219767 = CARTESIAN_POINT ( 'NONE',  ( 19.97071067695834046, 64.27928932305417220, -178.8468540517208396 ) ) ;
#219768 = ADVANCED_FACE ( 'NONE', ( #250101 ), #202260, .T. ) ;
#219769 = DIRECTION ( 'NONE',  ( -1.000000000000000000, 0.000000000000000000, 0.000000000000000000 ) ) ;
#219770 = DIRECTION ( 'NONE',  ( 0.000000000000000000, 0.9893560106964510714, -0.1455152366551481502 ) ) ;
#219771 = CARTESIAN_POINT ( 'NONE',  ( -21.07971444708686093, 0.08782343632898161057, -60.67020791837349236 ) ) ;
#219773 = EDGE_LOOP ( 'NONE', ( #69484, #224556, #79813, #130616, #191814 ) ) ;
#219772 = EDGE_CURVE ( 'NONE', #102720, #214056, #56305, .T. ) ;
#219774 = EDGE_CURVE ( 'NONE', #202021, #38916, #89619, .T. ) ;
#219775 = LINE ( 'NONE', #86665, #56999 ) ;
#219776 = LINE ( 'NONE', #178119, #11968 ) ;
#219777 = FACE_OUTER_BOUND ( 'NONE', #132404, .T. ) ;
#219778 = EDGE_CURVE ( 'NONE', #159949, #138157, #122972, .T. ) ;
#219779 = CIRCLE ( 'NONE', #203037, 11.74999999999999645 ) ;
#219780 = ORIENTED_EDGE ( 'NONE', *, *, #50571, .T. ) ;
#219781 = CARTESIAN_POINT ( 'NONE',  ( 20.90851465518105456, 68.09306500613196533, -224.1549646960459370 ) ) ;
#219783 = ADVANCED_FACE ( 'NONE', ( #55699 ), #156159, .T. ) ;
#219782 = ORIENTED_EDGE ( 'NONE', *, *, #771, .F. ) ;
#219784 = DIRECTION ( 'NONE',  ( -1.000000000000000000, 4.625929269271478222E-14, 0.000000000000000000 ) ) ;
#219785 = TOROIDAL_SURFACE ( 'NONE', #249041, 7.791421356237316687, 0.1000000000000000056 ) ;
#219786 = ORIENTED_EDGE ( 'NONE', *, *, #112350, .T. ) ;
#219787 = CARTESIAN_POINT ( 'NONE',  ( -21.40925344232282512, 69.34148114062223556, -203.6220576731440417 ) ) ;
#219788 = CARTESIAN_POINT ( 'NONE',  ( -20.94983749550516450, 10.29766095125292402, -72.47436639332755703 ) ) ;
#219789 = EDGE_CURVE ( 'NONE', #190881, #219055, #169146, .T. ) ;
#219790 = ORIENTED_EDGE ( 'NONE', *, *, #171541, .T. ) ;
#219792 = ORIENTED_EDGE ( 'NONE', *, *, #124774, .F. ) ;
#219791 = CARTESIAN_POINT ( 'NONE',  ( -18.59999999999999787, 66.65000000001157332, -57.17310748452438673 ) ) ;
#219793 = FACE_OUTER_BOUND ( 'NONE', #79081, .T. ) ;
#219794 = VERTEX_POINT ( 'NONE', #137830 ) ;
#219795 = CIRCLE ( 'NONE', #24015, 0.09999999999998898659 ) ;
#219796 = DIRECTION ( 'NONE',  ( -0.000000000000000000, 1.000000000000000000, 0.000000000000000000 ) ) ;
#219797 = CARTESIAN_POINT ( 'NONE',  ( -20.85000000000000142, 64.35000000001191722, -103.0231074845243882 ) ) ;
#219798 = ORIENTED_EDGE ( 'NONE', *, *, #35537, .F. ) ;
#219799 = AXIS2_PLACEMENT_3D ( 'NONE', #127675, #104230, #45563 ) ;
#219800 = VERTEX_POINT ( 'NONE', #136545 ) ;
#219801 = DIRECTION ( 'NONE',  ( 0.000000000000000000, -0.2128009952263485993, 0.9770955615653341697 ) ) ;
#219802 = DIRECTION ( 'NONE',  ( -0.000000000000000000, 1.000000000000000000, 6.982962677686266711E-15 ) ) ;
#219803 = ORIENTED_EDGE ( 'NONE', *, *, #126166, .T. ) ;
#219804 = CARTESIAN_POINT ( 'NONE',  ( -20.54999999999999716, 19.93396995659180249, -235.7707092203739307 ) ) ;
#219805 = AXIS2_PLACEMENT_3D ( 'NONE', #192483, #175508, #16434 ) ;
#219806 = VECTOR ( 'NONE', #243271, 1000.000000000000114 ) ;
#219808 = ORIENTED_EDGE ( 'NONE', *, *, #68806, .F. ) ;
#219807 = AXIS2_PLACEMENT_3D ( 'NONE', #195044, #73821, #152069 ) ;
#219809 = EDGE_LOOP ( 'NONE', ( #122936, #144816, #214249 ) ) ;
#219810 = EDGE_CURVE ( 'NONE', #173014, #129045, #216088, .T. ) ;
#219812 = CARTESIAN_POINT ( 'NONE',  ( 20.94999999999999574, 69.60000000001157616, -59.59268285446279378 ) ) ;
#219811 = AXIS2_PLACEMENT_3D ( 'NONE', #210263, #167296, #69473 ) ;
#219813 = AXIS2_PLACEMENT_3D ( 'NONE', #213178, #72416, #151958 ) ;
#219814 = EDGE_CURVE ( 'NONE', #86681, #201690, #106545, .T. ) ;
#219815 = EDGE_CURVE ( 'NONE', #149532, #38617, #37482, .T. ) ;
#219817 = ORIENTED_EDGE ( 'NONE', *, *, #173297, .T. ) ;
#219816 = CARTESIAN_POINT ( 'NONE',  ( -20.94999999999999929, 0.2561057921033771945, -66.96510355832775474 ) ) ;
#219818 = CARTESIAN_POINT ( 'NONE',  ( 21.05000000000000071, 8.776282895303632259, -45.65000000000000568 ) ) ;
#219819 = DIRECTION ( 'NONE',  ( 0.000000000000000000, -0.4088369013363281068, 0.9126074666063770380 ) ) ;
#219820 = DIRECTION ( 'NONE',  ( -1.000000000000000000, -2.952720810173289112E-16, 0.000000000000000000 ) ) ;
#219822 = FACE_OUTER_BOUND ( 'NONE', #28838, .T. ) ;
#219821 = CARTESIAN_POINT ( 'NONE',  ( -20.00857864376270001, 9.150000000011157653, -88.25000000000005684 ) ) ;
#219823 = FACE_OUTER_BOUND ( 'NONE', #84740, .T. ) ;
#219824 = FACE_OUTER_BOUND ( 'NONE', #157338, .T. ) ;
#219825 = VECTOR ( 'NONE', #23768, 1000.000000000000114 ) ;
#219826 = DIRECTION ( 'NONE',  ( -1.000000000000000000, 0.000000000000000000, 0.000000000000000000 ) ) ;
#219827 = CARTESIAN_POINT ( 'NONE',  ( -16.77683809663752257, 42.27269979661959098, -221.1123729563994402 ) ) ;
#219828 = CIRCLE ( 'NONE', #19946, 0.1000000000000055844 ) ;
#219829 = ORIENTED_EDGE ( 'NONE', *, *, #37379, .F. ) ;
#219830 = CIRCLE ( 'NONE', #149135, 0.2000000000000057288 ) ;
#219831 = TOROIDAL_SURFACE ( 'NONE', #132352, 12.77500000000000036, 0.1000000000000000056 ) ;
#219832 = ORIENTED_EDGE ( 'NONE', *, *, #109994, .F. ) ;
#219833 = AXIS2_PLACEMENT_3D ( 'NONE', #211105, #190270, #113285 ) ;
#219834 = VERTEX_POINT ( 'NONE', #79138 ) ;
#219835 = CARTESIAN_POINT ( 'NONE',  ( 21.05000000000000071, 1.360870587203197646, -175.5729979270909382 ) ) ;
#219836 = ORIENTED_EDGE ( 'NONE', *, *, #159032, .T. ) ;
#219837 = TOROIDAL_SURFACE ( 'NONE', #128285, 0.6000000000000009770, 0.1000000000000000056 ) ;
#219838 = CARTESIAN_POINT ( 'NONE',  ( -16.89268316805466341, 9.951721813253341153, -146.6442475214544743 ) ) ;
#219839 = ORIENTED_EDGE ( 'NONE', *, *, #257376, .F. ) ;
#219840 = FILL_AREA_STYLE_COLOUR ( '', #214629 ) ;
#219841 = CARTESIAN_POINT ( 'NONE',  ( -21.05000000000000071, 11.64999999999999680, -0.1000000000000028644 ) ) ;
#219844 = VERTEX_POINT ( 'NONE', #117004 ) ;
#219843 = VERTEX_POINT ( 'NONE', #158729 ) ;
#219842 = AXIS2_PLACEMENT_3D ( 'NONE', #31966, #154493, #191043 ) ;
#219845 = ORIENTED_EDGE ( 'NONE', *, *, #194600, .F. ) ;
#219846 = CIRCLE ( 'NONE', #244789, 0.1999999999999935163 ) ;
#219847 = AXIS2_PLACEMENT_3D ( 'NONE', #169968, #188204, #228630 ) ;
#219848 = ORIENTED_EDGE ( 'NONE', *, *, #187158, .T. ) ;
#219849 = DIRECTION ( 'NONE',  ( 0.000000000000000000, 0.000000000000000000, 1.000000000000000000 ) ) ;
#219851 = ORIENTED_EDGE ( 'NONE', *, *, #160945, .T. ) ;
#219850 = DIRECTION ( 'NONE',  ( 1.000000000000000000, -0.000000000000000000, -0.000000000000000000 ) ) ;
#219852 = CARTESIAN_POINT ( 'NONE',  ( 20.54374330479336308, 39.41460512620965062, -236.8056672937158567 ) ) ;
#219853 = CARTESIAN_POINT ( 'NONE',  ( 13.43443725621852991, 12.44134409367007343, -213.7340784654985271 ) ) ;
#219855 = EDGE_LOOP ( 'NONE', ( #39179, #157095, #33561, #244271 ) ) ;
#219854 = CARTESIAN_POINT ( 'NONE',  ( 20.95539060131842746, 10.62386215766679776, -141.6537338136562028 ) ) ;
#219856 = CARTESIAN_POINT ( 'NONE',  ( -23.25000000000000000, 5.950000000011163692, -157.1942976949652007 ) ) ;
#219857 = ORIENTED_EDGE ( 'NONE', *, *, #75332, .F. ) ;
#219858 = DIRECTION ( 'NONE',  ( 0.000000000000000000, 0.9770955615653316162, 0.2128009952263604232 ) ) ;
#219860 = EDGE_LOOP ( 'NONE', ( #147948, #45611, #36381, #168229 ) ) ;
#219859 = DIRECTION ( 'NONE',  ( 1.000000000000000000, -0.000000000000000000, -0.000000000000000000 ) ) ;
#219861 = CIRCLE ( 'NONE', #107448, 0.09999999999998898659 ) ;
#219862 = DIRECTION ( 'NONE',  ( 1.000000000000000000, 0.000000000000000000, 0.000000000000000000 ) ) ;
#219864 = EDGE_CURVE ( 'NONE', #75688, #231797, #23407, .T. ) ;
#219863 = CARTESIAN_POINT ( 'NONE',  ( -15.31895204843005942, 27.34981073572249954, -233.9047583970293545 ) ) ;
#219865 = VECTOR ( 'NONE', #81934, 1000.000000000000000 ) ;
#219866 = CARTESIAN_POINT ( 'NONE',  ( 21.05000000000000426, 10.56275983746217406, -74.45681395791866919 ) ) ;
#219867 = ORIENTED_EDGE ( 'NONE', *, *, #250454, .T. ) ;
#219869 = CYLINDRICAL_SURFACE ( 'NONE', #199765, 0.09999999999998898659 ) ;
#219868 = DIRECTION ( 'NONE',  ( 1.000000000000000000, 0.000000000000000000, -6.938893903907270030E-14 ) ) ;
#219871 = ADVANCED_FACE ( 'NONE', ( #103513 ), #119062, .T. ) ;
#219870 = DIRECTION ( 'NONE',  ( 0.000000000000000000, 0.8814952561688418342, -0.4721928772777367889 ) ) ;
#219872 = VECTOR ( 'NONE', #135931, 1000.000000000000000 ) ;
#219873 = CARTESIAN_POINT ( 'NONE',  ( 22.47071067811865319, 7.720074744509199505, -133.9009075452974002 ) ) ;
#219874 = CARTESIAN_POINT ( 'NONE',  ( -16.97683809663752186, 66.15000000001207070, -123.1207434663278804 ) ) ;
#219875 = CARTESIAN_POINT ( 'NONE',  ( -23.25000000000000355, 64.19947762500697763, -225.4487242757812737 ) ) ;
#219876 = ORIENTED_EDGE ( 'NONE', *, *, #112567, .F. ) ;
#219877 = ORIENTED_EDGE ( 'NONE', *, *, #207793, .T. ) ;
#219879 = EDGE_LOOP ( 'NONE', ( #89937, #28438, #233648, #175277 ) ) ;
#219878 = AXIS2_PLACEMENT_3D ( 'NONE', #135820, #255738, #75864 ) ;
#219880 = ADVANCED_FACE ( 'NONE', ( #114440 ), #193992, .F. ) ;
#219881 = CARTESIAN_POINT ( 'NONE',  ( -21.05000000000000071, 1.115600667400684642E-11, -96.40000000000003411 ) ) ;
#219882 = ADVANCED_FACE ( 'NONE', ( #36204 ), #94862, .T. ) ;
#219883 = EDGE_LOOP ( 'NONE', ( #207844, #66193, #139759, #86343 ) ) ;
#219884 = CARTESIAN_POINT ( 'NONE',  ( 21.05000000000000071, 1.115600667400684642E-11, -79.15000000000004832 ) ) ;
#219885 = ORIENTED_EDGE ( 'NONE', *, *, #1587, .T. ) ;
#219886 = CARTESIAN_POINT ( 'NONE',  ( -18.58671080940900566, -7.675445184013033106, -209.9627843819515931 ) ) ;
#219887 = CARTESIAN_POINT ( 'NONE',  ( -21.53752568622122254, 75.90102553874163505, -176.8099153590727894 ) ) ;
#219888 = AXIS2_PLACEMENT_3D ( 'NONE', #223644, #2030, #81554 ) ;
#219889 = AXIS2_PLACEMENT_3D ( 'NONE', #219927, #101215, #2148 ) ;
#219890 = VECTOR ( 'NONE', #142606, 1000.000000000000000 ) ;
#219891 = ORIENTED_EDGE ( 'NONE', *, *, #92262, .T. ) ;
#219892 = AXIS2_PLACEMENT_3D ( 'NONE', #74820, #137306, #216845 ) ;
#219893 = DIRECTION ( 'NONE',  ( 1.000000000000000000, -0.000000000000000000, -0.000000000000000000 ) ) ;
#219894 = SURFACE_STYLE_FILL_AREA ( #3397 ) ;
#219895 = AXIS2_PLACEMENT_3D ( 'NONE', #72349, #127174, #131016 ) ;
#219896 = ORIENTED_EDGE ( 'NONE', *, *, #58183, .F. ) ;
#219897 = EDGE_CURVE ( 'NONE', #162084, #130647, #75343, .T. ) ;
#219898 = ORIENTED_EDGE ( 'NONE', *, *, #172772, .F. ) ;
#219899 = ADVANCED_FACE ( 'NONE', ( #256440 ), #227372, .T. ) ;
#219900 = ORIENTED_EDGE ( 'NONE', *, *, #229993, .T. ) ;
#219901 = DIRECTION ( 'NONE',  ( 0.000000000000000000, 0.000000000000000000, -1.000000000000000000 ) ) ;
#219902 = CARTESIAN_POINT ( 'NONE',  ( 18.49999999999999289, 64.35000000001201670, -114.7731074845243882 ) ) ;
#219903 = CARTESIAN_POINT ( 'NONE',  ( -16.94275863009466576, 66.01050395134919313, -56.91480486656551108 ) ) ;
#219904 = DIRECTION ( 'NONE',  ( -1.000000000000000000, -0.000000000000000000, 0.000000000000000000 ) ) ;
#219905 = CARTESIAN_POINT ( 'NONE',  ( -21.07946286933444568, 61.10282755137055233, -234.2724922642379681 ) ) ;
#219906 = DIRECTION ( 'NONE',  ( -1.000000000000000000, 0.000000000000000000, -0.000000000000000000 ) ) ;
#219908 = CARTESIAN_POINT ( 'NONE',  ( 18.49999999999998934, 10.25000000001115552, -158.7500000000000284 ) ) ;
#219907 = FACE_OUTER_BOUND ( 'NONE', #207022, .T. ) ;
#219909 = DIRECTION ( 'NONE',  ( 0.000000000000000000, -6.938893903907222067E-15, 1.000000000000000000 ) ) ;
#219911 = ORIENTED_EDGE ( 'NONE', *, *, #227326, .F. ) ;
#219910 = CYLINDRICAL_SURFACE ( 'NONE', #164844, 0.09999999999999939493 ) ;
#219912 = DIRECTION ( 'NONE',  ( -1.000000000000000000, -0.000000000000000000, -0.000000000000000000 ) ) ;
#219913 = CARTESIAN_POINT ( 'NONE',  ( -18.58693740092134306, -9.406432150241803569, -141.1248164565013781 ) ) ;
#219914 = ORIENTED_EDGE ( 'NONE', *, *, #44734, .T. ) ;
#219915 = ORIENTED_EDGE ( 'NONE', *, *, #190321, .F. ) ;
#219916 = CARTESIAN_POINT ( 'NONE',  ( 23.24999999999999645, 4.775700934590584090, -78.84876810404601599 ) ) ;
#219917 = CIRCLE ( 'NONE', #157604, 0.09999999999999864553 ) ;
#219918 = CARTESIAN_POINT ( 'NONE',  ( 21.14999999999999858, 76.00000000001237765, -169.9231074845243654 ) ) ;
#219919 = CARTESIAN_POINT ( 'NONE',  ( 19.97071067811865674, 64.27928932189281852, -44.87310748452440379 ) ) ;
#219920 = EDGE_LOOP ( 'NONE', ( #114651, #112970, #125721, #94613 ) ) ;
#219921 = ADVANCED_FACE ( 'NONE', ( #77858 ), #156505, .T. ) ;
#219922 = EDGE_CURVE ( 'NONE', #189431, #213725, #252303, .T. ) ;
#219923 = AXIS2_PLACEMENT_3D ( 'NONE', #70302, #149828, #35034 ) ;
#219924 = DIRECTION ( 'NONE',  ( 1.000000000000000000, 0.000000000000000000, 0.000000000000000000 ) ) ;
#219925 = EDGE_LOOP ( 'NONE', ( #239108, #108306, #127002, #209108, #87085, #45571 ) ) ;
#219926 = ORIENTED_EDGE ( 'NONE', *, *, #7805, .F. ) ;
#219927 = CARTESIAN_POINT ( 'NONE',  ( -18.59999999999999787, 7.021664781911246322, -70.83356540189728889 ) ) ;
#219928 = ORIENTED_EDGE ( 'NONE', *, *, #34622, .T. ) ;
#219929 = DIRECTION ( 'NONE',  ( 0.000000000000000000, -6.853228547068871147E-15, 1.000000000000000000 ) ) ;
#219930 = DIRECTION ( 'NONE',  ( 0.000000000000000000, 0.2617529984164506107, 0.9651348961777299618 ) ) ;
#219931 = LINE ( 'NONE', #36184, #215469 ) ;
#219932 = CARTESIAN_POINT ( 'NONE',  ( 20.90000000000000213, 1.885425182446133885, -11.49641995933507843 ) ) ;
#219934 = EDGE_CURVE ( 'NONE', #180782, #223140, #72987, .T. ) ;
#219933 = DIRECTION ( 'NONE',  ( 1.000000000000000000, 0.000000000000000000, 0.000000000000000000 ) ) ;
#219935 = ORIENTED_EDGE ( 'NONE', *, *, #86899, .T. ) ;
#219936 = ADVANCED_FACE ( 'NONE', ( #58289 ), #217365, .T. ) ;
#219937 = CARTESIAN_POINT ( 'NONE',  ( -20.64999999999999858, 46.05992536685982230, -240.5730681801377102 ) ) ;
#219938 = DIRECTION ( 'NONE',  ( 0.000000000000000000, 1.000000000000000000, 0.000000000000000000 ) ) ;
#219939 = ADVANCED_FACE ( 'NONE', ( #209054 ), #6993, .T. ) ;
#219940 = AXIS2_PLACEMENT_3D ( 'NONE', #173851, #152988, #36892 ) ;
#219942 = CIRCLE ( 'NONE', #57614, 0.8750000000000007772 ) ;
#219941 = CARTESIAN_POINT ( 'NONE',  ( -18.59999999999999787, 44.52640028187936849, -247.3006740988509193 ) ) ;
#219943 = AXIS2_PLACEMENT_3D ( 'NONE', #5894, #204101, #104970 ) ;
#219944 = AXIS2_PLACEMENT_3D ( 'NONE', #236611, #217040, #160956 ) ;
#219945 = ORIENTED_EDGE ( 'NONE', *, *, #106507, .F. ) ;
#219947 = ORIENTED_EDGE ( 'NONE', *, *, #241196, .F. ) ;
#219946 = DIRECTION ( 'NONE',  ( -0.000000000000000000, -0.000000000000000000, -1.000000000000000000 ) ) ;
#219948 = CARTESIAN_POINT ( 'NONE',  ( -20.94999999999999929, 77.84915357198768504, -57.91714086472724432 ) ) ;
#219949 = CARTESIAN_POINT ( 'NONE',  ( 20.85000000000000142, -4.990442493977157667, -233.3018263216538628 ) ) ;
#219950 = EDGE_CURVE ( 'NONE', #4559, #39036, #160777, .T. ) ;
#219951 = DIRECTION ( 'NONE',  ( -0.000000000000000000, 0.1350103645451876666, 0.9908441862701600211 ) ) ;
#219952 = CARTESIAN_POINT ( 'NONE',  ( 21.14999999999999503, -3.187427350888460076, -228.3200064793908837 ) ) ;
#219953 = DIRECTION ( 'NONE',  ( 2.694716079187274425E-16, 0.4088369013363281623, -0.9126074666063770380 ) ) ;
#219954 = CARTESIAN_POINT ( 'NONE',  ( -18.59999999999999787, 42.94327155031035659, -233.8606566173841372 ) ) ;
#219955 = ORIENTED_EDGE ( 'NONE', *, *, #37969, .T. ) ;
#219956 = EDGE_CURVE ( 'NONE', #98586, #182409, #19076, .T. ) ;
#219957 = CARTESIAN_POINT ( 'NONE',  ( 21.05000000000000071, 6.412126976762841046, -199.7058512474018244 ) ) ;
#219958 = CIRCLE ( 'NONE', #111821, 0.1999999999999987899 ) ;
#219959 = CARTESIAN_POINT ( 'NONE',  ( -18.44204374631832621, 77.15868121549257808, -241.8076815865107108 ) ) ;
#219960 = VECTOR ( 'NONE', #138223, 1000.000000000000000 ) ;
#219961 = DIRECTION ( 'NONE',  ( 1.000000000000000000, -0.000000000000000000, -0.000000000000000000 ) ) ;
#219962 = AXIS2_PLACEMENT_3D ( 'NONE', #204447, #62390, #124934 ) ;
#219963 = ORIENTED_EDGE ( 'NONE', *, *, #167176, .F. ) ;
#219964 = ORIENTED_EDGE ( 'NONE', *, *, #4536, .T. ) ;
#219965 = DIRECTION ( 'NONE',  ( 0.000000000000000000, 1.000000000000000000, 6.982962677686266711E-15 ) ) ;
#219966 = CARTESIAN_POINT ( 'NONE',  ( -18.59999999999999787, 64.35000000001161879, -62.50830171387039513 ) ) ;
#219967 = CARTESIAN_POINT ( 'NONE',  ( -21.05000000000000426, 69.52295361822282871, -203.4231074845244507 ) ) ;
#219968 = CARTESIAN_POINT ( 'NONE',  ( -20.85000000000000142, 77.83585931145526615, -58.01866831572577610 ) ) ;
#219969 =( BOUNDED_CURVE ( )  B_SPLINE_CURVE ( 3, ( #36850, #175093, #116367, #155515 ),
 .UNSPECIFIED., .F., .F. ) 
 B_SPLINE_CURVE_WITH_KNOTS ( ( 4, 4 ),
 ( 4.712388980384689674, 6.283185307179586232 ),
 .UNSPECIFIED. ) 
 CURVE ( )  GEOMETRIC_REPRESENTATION_ITEM ( )  RATIONAL_B_SPLINE_CURVE ( ( 1.000000000000000000, 0.8047378541243649375, 0.8047378541243649375, 1.000000000000000000 ) ) 
 REPRESENTATION_ITEM ( '' )  );
#219970 = VERTEX_POINT ( 'NONE', #30433 ) ;
#219971 = CARTESIAN_POINT ( 'NONE',  ( 22.88900146558018989, 67.29609520889918883, -115.6731074845243654 ) ) ;
#219972 = DIRECTION ( 'NONE',  ( -1.000000000000000000, 0.000000000000000000, 0.000000000000000000 ) ) ;
#219973 = FACE_OUTER_BOUND ( 'NONE', #219349, .T. ) ;
#219974 = LINE ( 'NONE', #238251, #124635 ) ;
#219975 = AXIS2_PLACEMENT_3D ( 'NONE', #46702, #83246, #126243 ) ;
#219976 = VECTOR ( 'NONE', #104335, 1000.000000000000000 ) ;
#219977 = ORIENTED_EDGE ( 'NONE', *, *, #207552, .F. ) ;
#219979 =( BOUNDED_CURVE ( )  B_SPLINE_CURVE ( 3, ( #61103, #97638, #160238, #41573 ),
 .UNSPECIFIED., .F., .F. ) 
 B_SPLINE_CURVE_WITH_KNOTS ( ( 4, 4 ),
 ( 1.570796326794908992, 2.617993877991481533 ),
 .UNSPECIFIED. ) 
 CURVE ( )  GEOMETRIC_REPRESENTATION_ITEM ( )  RATIONAL_B_SPLINE_CURVE ( ( 1.000000000000000000, 0.9106836025229633202, 0.9106836025229633202, 1.000000000000000000 ) ) 
 REPRESENTATION_ITEM ( '' )  );
#219978 = CARTESIAN_POINT ( 'NONE',  ( 20.10000000000000853, 3.461118860469513336, 28.84309995045515507 ) ) ;
#219980 = ORIENTED_EDGE ( 'NONE', *, *, #141792, .F. ) ;
#219981 = CARTESIAN_POINT ( 'NONE',  ( -21.05000000000000071, 75.96824164695655668, -75.78195460760348112 ) ) ;
#219982 = DIRECTION ( 'NONE',  ( 2.915501640297155269E-16, -1.000000000000000000, 0.000000000000000000 ) ) ;
#219983 = VECTOR ( 'NONE', #220637, 1000.000000000000000 ) ;
#219984 = CARTESIAN_POINT ( 'NONE',  ( -20.54999999999999716, 85.40000000001252545, -179.9170766071767389 ) ) ;
#219985 = CYLINDRICAL_SURFACE ( 'NONE', #78357, 0.1000000000000028644 ) ;
#219986 = FACE_OUTER_BOUND ( 'NONE', #103964, .T. ) ;
#219987 = FACE_OUTER_BOUND ( 'NONE', #250463, .T. ) ;
#219988 = DIRECTION ( 'NONE',  ( -1.000000000000000000, -0.000000000000000000, -0.000000000000000000 ) ) ;
#219989 = DIRECTION ( 'NONE',  ( 0.000000000000000000, 0.000000000000000000, -1.000000000000000000 ) ) ;
#219990 = CARTESIAN_POINT ( 'NONE',  ( 18.59999999999999076, 10.20857864377385127, -158.7500000000000284 ) ) ;
#219991 = FACE_OUTER_BOUND ( 'NONE', #12715, .T. ) ;
#219992 = ADVANCED_FACE ( 'NONE', ( #145213 ), #245616, .F. ) ;
#219993 = LINE ( 'NONE', #158771, #139561 ) ;
#219994 = FACE_OUTER_BOUND ( 'NONE', #111130, .T. ) ;
#219995 = AXIS2_PLACEMENT_3D ( 'NONE', #224563, #9370, #45937 ) ;
#219996 = VECTOR ( 'NONE', #189442, 1000.000000000000000 ) ;
#219997 = CIRCLE ( 'NONE', #199158, 0.09999999999999939493 ) ;
#219998 = FACE_OUTER_BOUND ( 'NONE', #46791, .T. ) ;
#219999 = CARTESIAN_POINT ( 'NONE',  ( 20.94999999999999574, -1.835341550213255957, -112.1551512925630050 ) ) ;
#220000 =( BOUNDED_SURFACE ( )  B_SPLINE_SURFACE ( 3, 2, ( 
 ( #206481, #183078, #42278 ),
 ( #147801, #4414, #102205 ),
 ( #22733, #121824, #205174 ),
 ( #3121, #83912, #85208 ) ),
 .UNSPECIFIED., .F., .F., .F. ) 
 B_SPLINE_SURFACE_WITH_KNOTS ( ( 4, 4 ),
 ( 3, 3 ),
 ( 1.355252715606880543E-20, 0.0003124336117481268005 ),
 ( 0.000000000000000000, 1.000000000000000000 ),
 .UNSPECIFIED. ) 
 GEOMETRIC_REPRESENTATION_ITEM ( )  RATIONAL_B_SPLINE_SURFACE ( (
 ( 1.000000000000000000, 0.7040654476016472429, 1.000000000000000000),
 ( 1.000000000000000000, 0.7039193538781700621, 1.000000000000000000),
 ( 1.000000000000000000, 0.7089171279145592974, 1.000000000000000000),
 ( 1.000000000000000000, 0.7071067811865506814, 1.000000000000000000) ) ) 
 REPRESENTATION_ITEM ( '' )  SURFACE ( )  );
#220001 = TOROIDAL_SURFACE ( 'NONE', #140908, 14.20833333333334103, 0.1000000000000000056 ) ;
#220002 = VERTEX_POINT ( 'NONE', #188208 ) ;
#220003 = FACE_OUTER_BOUND ( 'NONE', #245574, .T. ) ;
#220004 = LINE ( 'NONE', #145591, #200073 ) ;
#220006 = ADVANCED_FACE ( 'NONE', ( #46118 ), #207798, .T. ) ;
#220005 = CARTESIAN_POINT ( 'NONE',  ( 20.19326291201655366, 10.15606098791449519, -41.26186180760268485 ) ) ;
#220007 = ORIENTED_EDGE ( 'NONE', *, *, #59897, .F. ) ;
#220008 = CYLINDRICAL_SURFACE ( 'NONE', #234635, 0.1000000000000052097 ) ;
#220009 = ADVANCED_FACE ( 'NONE', ( #228639 ), #52390, .T. ) ;
#220010 = CIRCLE ( 'NONE', #91025, 0.5000000000000004441 ) ;
#220011 = EDGE_CURVE ( 'NONE', #196293, #7452, #56648, .T. ) ;
#220012 = DIRECTION ( 'NONE',  ( 0.000000000000000000, -0.9908441862701596881, 0.1350103645451904977 ) ) ;
#220013 = ORIENTED_EDGE ( 'NONE', *, *, #87388, .F. ) ;
#220014 = DIRECTION ( 'NONE',  ( -1.000000000000000000, -0.000000000000000000, -0.000000000000000000 ) ) ;
#220015 = CARTESIAN_POINT ( 'NONE',  ( 22.49999999999999645, 31.82071903192824180, -238.9531407059547803 ) ) ;
#220016 = VECTOR ( 'NONE', #101638, 1000.000000000000000 ) ;
#220017 = EDGE_LOOP ( 'NONE', ( #230208, #209201, #138222 ) ) ;
#220018 = VECTOR ( 'NONE', #5247, 1000.000000000000000 ) ;
#220019 = AXIS2_PLACEMENT_3D ( 'NONE', #60153, #96687, #137142 ) ;
#220020 = AXIS2_PLACEMENT_3D ( 'NONE', #114948, #10720, #131941 ) ;
#220021 = CIRCLE ( 'NONE', #45233, 11.70000000000000284 ) ;
#220023 = ORIENTED_EDGE ( 'NONE', *, *, #60219, .F. ) ;
#220022 = AXIS2_PLACEMENT_3D ( 'NONE', #249917, #174279, #212088 ) ;
#220024 = DIRECTION ( 'NONE',  ( 0.000000000000000000, 0.2617529984165152257, 0.9651348961777124202 ) ) ;
#220025 = EDGE_CURVE ( 'NONE', #80372, #230108, #81582, .T. ) ;
#220026 = ORIENTED_EDGE ( 'NONE', *, *, #192111, .F. ) ;
#220027 = EDGE_CURVE ( 'NONE', #26416, #89909, #202440, .T. ) ;
#220028 = VECTOR ( 'NONE', #22456, 1000.000000000000227 ) ;
#220029 = CARTESIAN_POINT ( 'NONE',  ( 21.05000000000000071, 0.05148288188168551049, 6.300179817914542291 ) ) ;
#220030 = PLANE ( 'NONE',  #236959 ) ;
#220032 = DIRECTION ( 'NONE',  ( 1.000000000000000000, 0.000000000000000000, 0.000000000000000000 ) ) ;
#220031 = UNCERTAINTY_MEASURE_WITH_UNIT (LENGTH_MEASURE( 1.000000000000000082E-05 ), #248138, 'distance_accuracy_value', 'NONE');
#220033 = CARTESIAN_POINT ( 'NONE',  ( 23.24999999999999289, 23.29878867550048938, -248.4686781323362084 ) ) ;
#220034 = FACE_OUTER_BOUND ( 'NONE', #139884, .T. ) ;
#220035 = DIRECTION ( 'NONE',  ( 1.000000000000000000, 0.000000000000000000, -0.000000000000000000 ) ) ;
#220036 = FACE_OUTER_BOUND ( 'NONE', #144961, .T. ) ;
#220037 = CARTESIAN_POINT ( 'NONE',  ( 22.00411653889213071, 0.7817229495155295638, -230.2203756341537257 ) ) ;
#220039 = ORIENTED_EDGE ( 'NONE', *, *, #32389, .T. ) ;
#220038 = CARTESIAN_POINT ( 'NONE',  ( -18.41799967126732795, -9.499999999988851584, -40.53206981325593006 ) ) ;
#220040 = VERTEX_POINT ( 'NONE', #44845 ) ;
#220042 = LINE ( 'NONE', #203034, #72899 ) ;
#220041 = CARTESIAN_POINT ( 'NONE',  ( -21.14999999999999858, 56.01362831242966678, -232.7091905853083347 ) ) ;
#220044 = ORIENTED_EDGE ( 'NONE', *, *, #3216, .T. ) ;
#220043 = CARTESIAN_POINT ( 'NONE',  ( 20.94999999999999574, 8.926614585098251453, -108.9716830192231498 ) ) ;
#220045 = VERTEX_POINT ( 'NONE', #186951 ) ;
#220046 = CARTESIAN_POINT ( 'NONE',  ( 23.14999999999999858, 4.813084112160684214, -155.5584822434762202 ) ) ;
#220047 = COLOUR_RGB ( '', 0.40784314, 0.44705882, 0.49803922) ;
#220048 = TOROIDAL_SURFACE ( 'NONE', #111918, 11.70000000000000107, 0.1000000000000000056 ) ;
#220049 = CARTESIAN_POINT ( 'NONE',  ( 20.44999100639894962, 10.43971070322319683, -175.2590757259704901 ) ) ;
#220050 = EDGE_CURVE ( 'NONE', #223036, #18401, #76172, .T. ) ;
#220051 = DIRECTION ( 'NONE',  ( -1.000000000000000000, 0.000000000000000000, -0.000000000000000000 ) ) ;
#220052 = CARTESIAN_POINT ( 'NONE',  ( -23.25000000000000000, 36.65892442174472876, -249.5511627012454596 ) ) ;
#220053 = DIRECTION ( 'NONE',  ( 1.000000000000000000, 0.000000000000000000, 0.000000000000000000 ) ) ;
#220054 = FACE_OUTER_BOUND ( 'NONE', #72269, .T. ) ;
#220055 = DIRECTION ( 'NONE',  ( 0.000000000000000000, -0.8700118002898321601, 0.4930308989875230030 ) ) ;
#220056 = AXIS2_PLACEMENT_3D ( 'NONE', #113453, #256762, #16938 ) ;
#220057 = AXIS2_PLACEMENT_3D ( 'NONE', #14004, #93521, #80021 ) ;
#220058 = EDGE_CURVE ( 'NONE', #179506, #29920, #210627, .T. ) ;
#220059 = DIRECTION ( 'NONE',  ( -0.000000000000000000, 0.8814952561688430555, -0.4721928772777346239 ) ) ;
#220060 = ORIENTED_EDGE ( 'NONE', *, *, #111253, .T. ) ;
#220061 = ORIENTED_EDGE ( 'NONE', *, *, #24088, .T. ) ;
#220062 = DIRECTION ( 'NONE',  ( -1.000000000000000000, 0.000000000000000000, 0.000000000000000000 ) ) ;
#220063 = AXIS2_PLACEMENT_3D ( 'NONE', #46795, #205879, #5083 ) ;
#220064 = ORIENTED_EDGE ( 'NONE', *, *, #141732, .T. ) ;
#220065 = CARTESIAN_POINT ( 'NONE',  ( 21.11825140030075332, 0.007203620643842375236, -27.05459243457999818 ) ) ;
#220066 = ORIENTED_EDGE ( 'NONE', *, *, #47547, .T. ) ;
#220067 = CARTESIAN_POINT ( 'NONE',  ( 21.05000000000000071, 87.65000000001215597, -139.4231074845242802 ) ) ;
#220068 = AXIS2_PLACEMENT_3D ( 'NONE', #7905, #61439, #140990 ) ;
#220069 = DIRECTION ( 'NONE',  ( 0.000000000000000000, -0.3427706569149662763, 0.9394191166662954062 ) ) ;
#220070 = CARTESIAN_POINT ( 'NONE',  ( -23.15000000000000213, 1.115600667400684642E-11, -200.9999999999999432 ) ) ;
#220071 = DIRECTION ( 'NONE',  ( 0.000000000000000000, 0.9651348961777149738, -0.2617529984165058998 ) ) ;
#220072 = CARTESIAN_POINT ( 'NONE',  ( -21.12757541349819590, 75.99483878420299732, -209.9964880557759273 ) ) ;
#220073 = ORIENTED_EDGE ( 'NONE', *, *, #84324, .F. ) ;
#220074 = AXIS2_PLACEMENT_3D ( 'NONE', #139974, #5599, #120476 ) ;
#220075 = FACE_OUTER_BOUND ( 'NONE', #144920, .T. ) ;
#220076 = ORIENTED_EDGE ( 'NONE', *, *, #7992, .T. ) ;
#220077 = EDGE_CURVE ( 'NONE', #36405, #109174, #88636, .T. ) ;
#220078 = CARTESIAN_POINT ( 'NONE',  ( -22.39999999999999858, 68.20922040163873135, -136.6231074845243540 ) ) ;
#220079 = AXIS2_PLACEMENT_3D ( 'NONE', #48676, #104771, #243026 ) ;
#220081 = CARTESIAN_POINT ( 'NONE',  ( -23.15000000000000213, 87.65000000001192859, -106.1231074845242262 ) ) ;
#220080 = VECTOR ( 'NONE', #24971, 1000.000000000000000 ) ;
#220082 = CARTESIAN_POINT ( 'NONE',  ( 0.9000000000000546452, 67.72071067812984779, -6.052396806406134644 ) ) ;
#220083 = CIRCLE ( 'NONE', #78427, 0.1000000000000015737 ) ;
#220084 = SPHERICAL_SURFACE ( 'NONE', #132281, 0.1000000000000000056 ) ;
#220085 = ORIENTED_EDGE ( 'NONE', *, *, #172724, .T. ) ;
#220086 = FACE_OUTER_BOUND ( 'NONE', #205447, .T. ) ;
#220087 = ORIENTED_EDGE ( 'NONE', *, *, #920, .T. ) ;
#220090 = ORIENTED_EDGE ( 'NONE', *, *, #174829, .F. ) ;
#220089 = FACE_OUTER_BOUND ( 'NONE', #195429, .T. ) ;
#220088 = CARTESIAN_POINT ( 'NONE',  ( 18.49999999999998934, 47.07326788871596790, -255.0992659944398042 ) ) ;
#220091 = AXIS2_PLACEMENT_3D ( 'NONE', #110766, #190328, #102081 ) ;
#220092 = DIRECTION ( 'NONE',  ( 7.304098846218134667E-16, 0.4088369013363281068, -0.9126074666063770380 ) ) ;
#220093 = EDGE_CURVE ( 'NONE', #248011, #235587, #147807, .T. ) ;
#220094 = DIRECTION ( 'NONE',  ( 1.000000000000000000, -2.952720810173289112E-16, -2.061873921506763405E-30 ) ) ;
#220095 = ORIENTED_EDGE ( 'NONE', *, *, #18017, .F. ) ;
#220097 = EDGE_CURVE ( 'NONE', #47300, #166855, #226012, .T. ) ;
#220096 = CARTESIAN_POINT ( 'NONE',  ( 18.50000000000001421, 85.48068669529106955, -129.5819923157664562 ) ) ;
#220098 = EDGE_CURVE ( 'NONE', #229760, #231169, #239864, .T. ) ;
#220099 = CARTESIAN_POINT ( 'NONE',  ( -22.46246831459151494, -3.130120236468494355, -228.2124027741761552 ) ) ;
#220100 = EDGE_CURVE ( 'NONE', #144042, #72959, #12164, .T. ) ;
#220102 = VERTEX_POINT ( 'NONE', #173831 ) ;
#220101 = CARTESIAN_POINT ( 'NONE',  ( -18.59999999999999787, 64.35000000001161879, -62.60830171387041077 ) ) ;
#220103 = AXIS2_PLACEMENT_3D ( 'NONE', #169399, #248904, #132812 ) ;
#220104 = CARTESIAN_POINT ( 'NONE',  ( 18.39999999999999858, 85.40000000001204228, -114.7731074845242460 ) ) ;
#220106 = ORIENTED_EDGE ( 'NONE', *, *, #256211, .T. ) ;
#220105 = EDGE_CURVE ( 'NONE', #125207, #47181, #143973, .T. ) ;
#220107 = CARTESIAN_POINT ( 'NONE',  ( 21.00023020733438983, 61.06322362754158917, -234.1822973190417088 ) ) ;
#220108 = CARTESIAN_POINT ( 'NONE',  ( -18.50000000000000000, -9.421290279512383847, -140.8238821790260999 ) ) ;
#220109 = EDGE_CURVE ( 'NONE', #115416, #137749, #175113, .T. ) ;
#220110 = VERTEX_POINT ( 'NONE', #151683 ) ;
#220111 = DIRECTION ( 'NONE',  ( -1.000000000000000000, 0.000000000000000000, 0.000000000000000000 ) ) ;
#220114 = ADVANCED_FACE ( 'NONE', ( #229901 ), #51232, .F. ) ;
#220113 = ADVANCED_FACE ( 'NONE', ( #31737 ), #210348, .T. ) ;
#220112 = ORIENTED_EDGE ( 'NONE', *, *, #33328, .F. ) ;
#220115 = CARTESIAN_POINT ( 'NONE',  ( 21.05000000000000071, -11.64999999998883595, -136.9000000000000341 ) ) ;
#220116 = LINE ( 'NONE', #143118, #30864 ) ;
#220117 = DIRECTION ( 'NONE',  ( 0.000000000000000000, -6.467318590049456648E-15, 1.000000000000000000 ) ) ;
#220118 = ORIENTED_EDGE ( 'NONE', *, *, #26354, .T. ) ;
#220119 = DIRECTION ( 'NONE',  ( 0.000000000000000000, 0.000000000000000000, 1.000000000000000000 ) ) ;
#220120 = CARTESIAN_POINT ( 'NONE',  ( 20.95000000000005258, 65.35000000001120668, -3.123107484524795474 ) ) ;
#220121 = EDGE_CURVE ( 'NONE', #182231, #256176, #64867, .T. ) ;
#220122 = CARTESIAN_POINT ( 'NONE',  ( -20.94560253601877164, 64.25000000001250555, -177.0130239720093925 ) ) ;
#220123 = EDGE_LOOP ( 'NONE', ( #173043, #163435, #134800, #199940 ) ) ;
#220124 = CIRCLE ( 'NONE', #174572, 0.2000000000000057288 ) ;
#220126 = AXIS2_PLACEMENT_3D ( 'NONE', #154452, #233948, #117842 ) ;
#220125 = DIRECTION ( 'NONE',  ( 0.000000000000000000, 0.000000000000000000, 1.000000000000000000 ) ) ;
#220127 = CARTESIAN_POINT ( 'NONE',  ( 21.05000000000000071, 8.013878543493270001, -211.9507248933737458 ) ) ;
#220129 = ORIENTED_EDGE ( 'NONE', *, *, #217489, .T. ) ;
#220128 = EDGE_CURVE ( 'NONE', #179165, #120381, #20328, .T. ) ;
#220130 = VECTOR ( 'NONE', #53834, 1000.000000000000114 ) ;
#220132 = ADVANCED_FACE ( 'NONE', ( #34299 ), #55082, .F. ) ;
#220131 = CARTESIAN_POINT ( 'NONE',  ( 20.94999999999999929, 4.999999999999997335, -12.40526601891309788 ) ) ;
#220133 = EDGE_LOOP ( 'NONE', ( #124443, #35729, #31946, #142209 ) ) ;
#220134 = VERTEX_POINT ( 'NONE', #111239 ) ;
#220135 = EDGE_CURVE ( 'NONE', #10380, #63695, #127419, .T. ) ;
#220136 = CARTESIAN_POINT ( 'NONE',  ( -21.05000000000000071, -11.48912529306490349, -170.5999999999999659 ) ) ;
#220137 = CIRCLE ( 'NONE', #199291, 0.1000000000000026007 ) ;
#220138 = ORIENTED_EDGE ( 'NONE', *, *, #117742, .T. ) ;
#220140 = VERTEX_POINT ( 'NONE', #92949 ) ;
#220139 = LINE ( 'NONE', #100148, #134515 ) ;
#220141 = EDGE_CURVE ( 'NONE', #62035, #255544, #114949, .T. ) ;
#220144 = EDGE_LOOP ( 'NONE', ( #23286, #234904, #123583, #43879 ) ) ;
#220143 = ORIENTED_EDGE ( 'NONE', *, *, #62629, .F. ) ;
#220142 = CARTESIAN_POINT ( 'NONE',  ( -21.05000000000000071, 11.60000000001115517, -127.0717967697245143 ) ) ;
#220146 = TOROIDAL_SURFACE ( 'NONE', #182745, 0.4000000000000009104, 0.1000000000000000056 ) ;
#220145 = DIRECTION ( 'NONE',  ( -1.000000000000000000, -0.000000000000000000, -0.000000000000000000 ) ) ;
#220147 = CIRCLE ( 'NONE', #216027, 0.1000000000000124678 ) ;
#220148 = DIRECTION ( 'NONE',  ( 1.186688945009009831E-16, -1.000000000000000000, 0.000000000000000000 ) ) ;
#220149 = DIRECTION ( 'NONE',  ( 0.000000000000000000, -1.000000000000000000, -1.387778780781442047E-14 ) ) ;
#220150 = VECTOR ( 'NONE', #101649, 1000.000000000000114 ) ;
#220151 = FACE_OUTER_BOUND ( 'NONE', #45127, .T. ) ;
#220152 = DIRECTION ( 'NONE',  ( 0.000000000000000000, 0.8660254037844420383, -0.4999999999999941713 ) ) ;
#220153 = CARTESIAN_POINT ( 'NONE',  ( 20.95595624212450048, 65.37610879691844445, -195.8934745703976432 ) ) ;
#220154 = DIRECTION ( 'NONE',  ( 1.000000000000000000, 0.000000000000000000, 0.000000000000000000 ) ) ;
#220155 = AXIS2_PLACEMENT_3D ( 'NONE', #60465, #1775, #81293 ) ;
#220156 = DIRECTION ( 'NONE',  ( 1.000000000000000000, 0.000000000000000000, 0.000000000000000000 ) ) ;
#220157 = EDGE_LOOP ( 'NONE', ( #174311, #24075, #75778, #102706, #123959 ) ) ;
#220158 = ORIENTED_EDGE ( 'NONE', *, *, #69972, .T. ) ;
#220160 = ORIENTED_EDGE ( 'NONE', *, *, #158241, .T. ) ;
#220159 = FACE_OUTER_BOUND ( 'NONE', #198212, .T. ) ;
#220161 = CARTESIAN_POINT ( 'NONE',  ( -21.05000000000000071, -11.75000000000000000, -30.50000000000000000 ) ) ;
#220162 = ORIENTED_EDGE ( 'NONE', *, *, #224707, .T. ) ;
#220163 = CARTESIAN_POINT ( 'NONE',  ( -18.59999999999999787, 64.25000000001173817, -81.27310748452440237 ) ) ;
#220164 = VERTEX_POINT ( 'NONE', #113802 ) ;
#220165 = CARTESIAN_POINT ( 'NONE',  ( -23.25000000000000000, 85.60000000001188880, -93.12913836187179584 ) ) ;
#220166 = VERTEX_POINT ( 'NONE', #130792 ) ;
#220167 = CARTESIAN_POINT ( 'NONE',  ( -16.91776028072577631, 66.03659960638205462, -82.14808346982226794 ) ) ;
#220168 = SPHERICAL_SURFACE ( 'NONE', #28029, 0.1000000000000000056 ) ;
#220169 = CIRCLE ( 'NONE', #157668, 0.2000000000000000944 ) ;
#220170 = CIRCLE ( 'NONE', #178695, 0.09999999999999363565 ) ;
#220171 = AXIS2_PLACEMENT_3D ( 'NONE', #202987, #3494, #120920 ) ;
#220173 = VERTEX_POINT ( 'NONE', #172549 ) ;
#220172 = ORIENTED_EDGE ( 'NONE', *, *, #168825, .T. ) ;
#220174 = ORIENTED_EDGE ( 'NONE', *, *, #185100, .F. ) ;
#220175 = ORIENTED_EDGE ( 'NONE', *, *, #9294, .T. ) ;
#220176 = EDGE_LOOP ( 'NONE', ( #172420, #219112, #63466, #186305 ) ) ;
#220177 = CYLINDRICAL_SURFACE ( 'NONE', #230364, 4.049999999999998046 ) ;
#220179 = ORIENTED_EDGE ( 'NONE', *, *, #134150, .F. ) ;
#220178 = CARTESIAN_POINT ( 'NONE',  ( -18.59999999999999787, -1.149570369564537842, -208.8159124845019221 ) ) ;
#220180 = AXIS2_PLACEMENT_3D ( 'NONE', #64946, #224017, #166660 ) ;
#220182 = CARTESIAN_POINT ( 'NONE',  ( 20.95576188350343116, 65.39101945504891944, -162.4118737617701242 ) ) ;
#220181 = CARTESIAN_POINT ( 'NONE',  ( 23.14999999999999858, 1.115600667400684642E-11, -33.50000000000000000 ) ) ;
#220183 = CARTESIAN_POINT ( 'NONE',  ( -22.39999999999999858, 64.27847795353595473, -247.1247091181747066 ) ) ;
#220184 = CYLINDRICAL_SURFACE ( 'NONE', #106522, 0.09999999999999939493 ) ;
#220185 = CARTESIAN_POINT ( 'NONE',  ( -22.01447462590972748, 7.263800201241075172, -66.90096299994051776 ) ) ;
#220186 = ORIENTED_EDGE ( 'NONE', *, *, #42276, .F. ) ;
#220187 = ORIENTED_EDGE ( 'NONE', *, *, #30834, .F. ) ;
#220188 = DIRECTION ( 'NONE',  ( 0.000000000000000000, 0.000000000000000000, 1.000000000000000000 ) ) ;
#220189 = DIRECTION ( 'NONE',  ( 0.000000000000000000, 1.000000000000000000, -6.308085367188393199E-16 ) ) ;
#220191 = EDGE_CURVE ( 'NONE', #14799, #38057, #102428, .T. ) ;
#220190 = DIRECTION ( 'NONE',  ( -0.7071067811865486830, 0.3338907855510728218, 0.6233112732207607420 ) ) ;
#220192 = EDGE_LOOP ( 'NONE', ( #154, #189496, #114047, #94296 ) ) ;
#220193 = AXIS2_PLACEMENT_3D ( 'NONE', #19668, #137037, #80893 ) ;
#220195 = CARTESIAN_POINT ( 'NONE',  ( 23.14999999999999858, 5.000000000011153745, -179.9052660189130677 ) ) ;
#220194 = CIRCLE ( 'NONE', #120268, 0.09999999999998898659 ) ;
#220196 = EDGE_CURVE ( 'NONE', #208658, #16708, #232492, .T. ) ;
#220197 = CIRCLE ( 'NONE', #216079, 0.1000000000000035305 ) ;
#220198 = LINE ( 'NONE', #84477, #76167 ) ;
#220199 = CARTESIAN_POINT ( 'NONE',  ( -20.54999999999999716, 65.49732036650624423, -236.6319166190174883 ) ) ;
#220200 = VECTOR ( 'NONE', #242424, 999.9999999999998863 ) ;
#220201 = VERTEX_POINT ( 'NONE', #14732 ) ;
#220202 = ORIENTED_EDGE ( 'NONE', *, *, #210895, .T. ) ;
#220203 = ADVANCED_FACE ( 'NONE', ( #94232 ), #253304, .F. ) ;
#220204 = CARTESIAN_POINT ( 'NONE',  ( -21.14999999999999858, 1.148907358139439339E-11, -201.0000000000015064 ) ) ;
#220206 = EDGE_CURVE ( 'NONE', #224018, #174229, #2688, .T. ) ;
#220205 = CARTESIAN_POINT ( 'NONE',  ( -18.59999999999999787, 1.162701749949165642, -75.00000000000004263 ) ) ;
#220207 = ORIENTED_EDGE ( 'NONE', *, *, #51178, .F. ) ;
#220208 = DIRECTION ( 'NONE',  ( 0.000000000000000000, 0.000000000000000000, 1.000000000000000000 ) ) ;
#220209 = ORIENTED_EDGE ( 'NONE', *, *, #59660, .T. ) ;
#220210 = CARTESIAN_POINT ( 'NONE',  ( -20.54999999999999716, 76.00000000001267608, -203.5231074845243597 ) ) ;
#220211 = CARTESIAN_POINT ( 'NONE',  ( -16.81744102076748959, 9.950000000011138823, -87.85000000000005116 ) ) ;
#220213 = DIRECTION ( 'NONE',  ( -0.000000000000000000, 1.000000000000000000, -0.000000000000000000 ) ) ;
#220212 = FACE_OUTER_BOUND ( 'NONE', #42492, .T. ) ;
#220214 = CIRCLE ( 'NONE', #199937, 0.1000000000000056677 ) ;
#220215 = CIRCLE ( 'NONE', #70391, 0.09999999999998898659 ) ;
#220216 = CARTESIAN_POINT ( 'NONE',  ( 18.59999999999999076, 61.95000000001208917, -131.0094124137634140 ) ) ;
#220217 = CARTESIAN_POINT ( 'NONE',  ( -16.87851181299898684, 66.04995707600411947, -90.37325099989129740 ) ) ;
#220218 = ORIENTED_EDGE ( 'NONE', *, *, #228911, .T. ) ;
#220219 = AXIS2_PLACEMENT_3D ( 'NONE', #25685, #62242, #239600 ) ;
#220220 = CARTESIAN_POINT ( 'NONE',  ( 18.39999999999999858, -9.519327731081283162, -40.47297637655933755 ) ) ;
#220221 = ADVANCED_FACE ( 'NONE', ( #62814, #139762 ), #21152, .T. ) ;
#220224 = ORIENTED_EDGE ( 'NONE', *, *, #61038, .T. ) ;
#220223 = ORIENTED_EDGE ( 'NONE', *, *, #20517, .T. ) ;
#220222 = AXIS2_PLACEMENT_3D ( 'NONE', #199707, #58856, #21075 ) ;
#220225 = ORIENTED_EDGE ( 'NONE', *, *, #102475, .F. ) ;
#220227 = ADVANCED_FACE ( 'NONE', ( #218015 ), #240184, .T. ) ;
#220226 = AXIS2_PLACEMENT_3D ( 'NONE', #124095, #82348, #185340 ) ;
#220228 = AXIS2_PLACEMENT_3D ( 'NONE', #187829, #130390, #170873 ) ;
#220229 = EDGE_LOOP ( 'NONE', ( #161673, #220632, #145569 ) ) ;
#220230 = AXIS2_PLACEMENT_3D ( 'NONE', #216632, #174994, #256997 ) ;
#220231 = DIRECTION ( 'NONE',  ( 1.000000000000000000, 0.000000000000000000, -0.000000000000000000 ) ) ;
#220232 = CARTESIAN_POINT ( 'NONE',  ( -22.39999999999999858, 76.10085836911045476, -81.27267460801371612 ) ) ;
#220233 = CARTESIAN_POINT ( 'NONE',  ( 18.50000000000000000, 9.122720154857379526, -245.4644708025848558 ) ) ;
#220234 = DIRECTION ( 'NONE',  ( -1.000000000000000000, 0.000000000000000000, 0.000000000000000000 ) ) ;
#220235 = DIRECTION ( 'NONE',  ( 1.000000000000000000, 0.000000000000000000, 0.000000000000000000 ) ) ;
#220237 = CARTESIAN_POINT ( 'NONE',  ( 20.95595012432476523, 58.98502654666104661, -225.7485087577998399 ) ) ;
#220236 = CARTESIAN_POINT ( 'NONE',  ( 21.05000000000000071, 5.500000000011153745, -88.09473398108696074 ) ) ;
#220239 = ORIENTED_EDGE ( 'NONE', *, *, #73665, .F. ) ;
#220238 = LINE ( 'NONE', #101517, #235369 ) ;
#220240 = DIRECTION ( 'NONE',  ( -3.265361837132813093E-16, -1.000000000000000000, -6.938893903907229955E-15 ) ) ;
#220241 = VERTEX_POINT ( 'NONE', #19856 ) ;
#220242 = DIRECTION ( 'NONE',  ( 0.000000000000000000, 0.000000000000000000, -1.000000000000000000 ) ) ;
#220243 = ORIENTED_EDGE ( 'NONE', *, *, #200160, .F. ) ;
#220244 = VERTEX_POINT ( 'NONE', #39436 ) ;
#220245 = DIRECTION ( 'NONE',  ( 0.000000000000000000, 0.000000000000000000, -1.000000000000000000 ) ) ;
#220246 = CARTESIAN_POINT ( 'NONE',  ( 21.14999999999999858, 42.98415524044398950, -233.9519173640447889 ) ) ;
#220247 = CARTESIAN_POINT ( 'NONE',  ( -21.05000000000000071, 18.90448995781211750, -232.7802074516171444 ) ) ;
#220248 = EDGE_CURVE ( 'NONE', #253340, #216920, #215093, .T. ) ;
#220249 = CARTESIAN_POINT ( 'NONE',  ( 12.84233041328156055, 9.410538608540026217, -82.43268799714094541 ) ) ;
#220250 = ADVANCED_FACE ( 'NONE', ( #40725 ), #262, .T. ) ;
#220251 = VECTOR ( 'NONE', #31894, 1000.000000000000000 ) ;
#220252 = AXIS2_PLACEMENT_3D ( 'NONE', #174168, #211980, #175432 ) ;
#220253 = CARTESIAN_POINT ( 'NONE',  ( 21.87500000000000355, 63.38346053167636995, -212.7939182281409956 ) ) ;
#220254 = ORIENTED_EDGE ( 'NONE', *, *, #20280, .T. ) ;
#220255 = VERTEX_POINT ( 'NONE', #38137 ) ;
#220256 = FACE_OUTER_BOUND ( 'NONE', #4988, .T. ) ;
#220257 = ORIENTED_EDGE ( 'NONE', *, *, #182724, .T. ) ;
#220258 = LINE ( 'NONE', #200687, #193691 ) ;
#220259 = CARTESIAN_POINT ( 'NONE',  ( -20.64999999999999858, 4.350000000011156054, -179.7499999999999716 ) ) ;
#220260 = DIRECTION ( 'NONE',  ( -1.000000000000000000, 7.304098846218134667E-16, 5.100424963727256530E-30 ) ) ;
#220261 = CARTESIAN_POINT ( 'NONE',  ( -17.11825945287481332, 9.950000000011138823, -188.2499999999999716 ) ) ;
#220263 = EDGE_CURVE ( 'NONE', #107478, #34312, #81076, .T. ) ;
#220262 = DIRECTION ( 'NONE',  ( -2.915501640297154283E-16, 1.000000000000000000, 0.000000000000000000 ) ) ;
#220264 = CARTESIAN_POINT ( 'NONE',  ( 23.25000000000000000, 87.75000000001259082, -191.3731074845242688 ) ) ;
#220265 = CIRCLE ( 'NONE', #166293, 0.1000000000000056677 ) ;
#220266 = DIRECTION ( 'NONE',  ( 0.000000000000000000, -6.982962677686266711E-15, 1.000000000000000000 ) ) ;
#220267 = DIRECTION ( 'NONE',  ( 1.000000000000000000, 0.000000000000000000, 0.000000000000000000 ) ) ;
#220268 = ADVANCED_FACE ( 'NONE', ( #156817 ), #27696, .T. ) ;
#220269 = AXIS2_PLACEMENT_3D ( 'NONE', #191868, #70637, #13212 ) ;
#220270 = CARTESIAN_POINT ( 'NONE',  ( 18.49999999999999289, 65.58283456529608202, -178.6731074851066410 ) ) ;
#220271 = CARTESIAN_POINT ( 'NONE',  ( 20.94999999999999929, -9.500000000000000000, -23.60603087734755690 ) ) ;
#220272 = AXIS2_PLACEMENT_3D ( 'NONE', #103879, #119637, #163889 ) ;
#220273 = ADVANCED_FACE ( 'NONE', ( #61539 ), #177663, .T. ) ;
#220274 = LINE ( 'NONE', #128871, #44796 ) ;
#220275 = VECTOR ( 'NONE', #227266, 1000.000000000000000 ) ;
#220276 = EDGE_CURVE ( 'NONE', #159242, #187404, #57660, .T. ) ;
#220277 = EDGE_LOOP ( 'NONE', ( #156879, #10900, #143813, #255334 ) ) ;
#220278 = CARTESIAN_POINT ( 'NONE',  ( 20.95575313997065336, 10.61455330328599089, -41.12129070194482239 ) ) ;
#220279 = ORIENTED_EDGE ( 'NONE', *, *, #155455, .F. ) ;
#220280 = EDGE_CURVE ( 'NONE', #81295, #70011, #40148, .T. ) ;
#220281 = CARTESIAN_POINT ( 'NONE',  ( 20.94999999999999929, 1.115600667400684642E-11, -167.5000000000000284 ) ) ;
#220282 = CARTESIAN_POINT ( 'NONE',  ( 18.59999999999999432, 0.6770221356676882074, -212.8807256103264649 ) ) ;
#220283 = CYLINDRICAL_SURFACE ( 'NONE', #135294, 2.000000000000001776 ) ;
#220284 = AXIS2_PLACEMENT_3D ( 'NONE', #33341, #34607, #231515 ) ;
#220285 = ORIENTED_EDGE ( 'NONE', *, *, #250256, .F. ) ;
#220286 = DIRECTION ( 'NONE',  ( 0.000000000000000000, 0.000000000000000000, 1.000000000000000000 ) ) ;
#220287 = EDGE_CURVE ( 'NONE', #178738, #170516, #152590, .T. ) ;
#220288 = CIRCLE ( 'NONE', #107830, 11.65000000000000746 ) ;
#220289 = DIRECTION ( 'NONE',  ( -1.020425574104004196E-15, -0.000000000000000000, -1.000000000000000000 ) ) ;
#220290 = CARTESIAN_POINT ( 'NONE',  ( 23.14999999999999858, 11.60000000001116227, -60.07179676972450011 ) ) ;
#220291 = FACE_OUTER_BOUND ( 'NONE', #34908, .T. ) ;
#220292 = CARTESIAN_POINT ( 'NONE',  ( -16.93658211146644987, 9.994108662352344297, -121.4042950699557082 ) ) ;
#220293 = FACE_OUTER_BOUND ( 'NONE', #192789, .T. ) ;
#220294 = ORIENTED_EDGE ( 'NONE', *, *, #199683, .T. ) ;
#220295 = LINE ( 'NONE', #65051, #212510 ) ;
#220297 = ORIENTED_EDGE ( 'NONE', *, *, #164779, .F. ) ;
#220296 = FACE_OUTER_BOUND ( 'NONE', #57806, .T. ) ;
#220298 = DIRECTION ( 'NONE',  ( 0.000000000000000000, -1.445602896647339410E-16, 1.000000000000000000 ) ) ;
#220299 = EDGE_CURVE ( 'NONE', #79795, #159346, #201042, .T. ) ;
#220300 = DIRECTION ( 'NONE',  ( 0.000000000000000000, -1.000000000000000000, -0.000000000000000000 ) ) ;
#220301 = ORIENTED_EDGE ( 'NONE', *, *, #219147, .F. ) ;
#220302 = DIRECTION ( 'NONE',  ( 0.000000000000000000, 0.1350103645451835865, 0.9908441862701605762 ) ) ;
#220303 = APPLICATION_PROTOCOL_DEFINITION ( 'draft international standard', 'automotive_design', 1998, #24210 ) ;
#220304 = CARTESIAN_POINT ( 'NONE',  ( 23.14999999999999858, 1.115600667400684642E-11, -67.00000000000004263 ) ) ;
#220305 = VERTEX_POINT ( 'NONE', #79786 ) ;
#220306 = DIRECTION ( 'NONE',  ( 1.000000000000000000, 0.000000000000000000, 0.000000000000000000 ) ) ;
#220307 = CARTESIAN_POINT ( 'NONE',  ( 15.31784899511109188, 9.396630376328875656, -185.4070573928183308 ) ) ;
#220308 = DIRECTION ( 'NONE',  ( 0.000000000000000000, 0.2128009952263485993, -0.9770955615653341697 ) ) ;
#220309 = ORIENTED_EDGE ( 'NONE', *, *, #120297, .T. ) ;
#220310 = ORIENTED_EDGE ( 'NONE', *, *, #140288, .F. ) ;
#220311 = CYLINDRICAL_SURFACE ( 'NONE', #251359, 0.09999999999998898659 ) ;
#220312 = DIRECTION ( 'NONE',  ( 1.000000000000000000, 0.000000000000000000, 0.000000000000000000 ) ) ;
#220313 = DIRECTION ( 'NONE',  ( 0.000000000000000000, -0.9876013379310930596, -0.1569827930593520049 ) ) ;
#220314 = LINE ( 'NONE', #16986, #136123 ) ;
#220315 = DIRECTION ( 'NONE',  ( 1.000000000000000000, 0.000000000000000000, 0.000000000000000000 ) ) ;
#220316 = CARTESIAN_POINT ( 'NONE',  ( 20.94999999999999929, 85.50000000001222134, -146.4170766071767389 ) ) ;
#220318 = CARTESIAN_POINT ( 'NONE',  ( -23.15000000000000213, 87.65000000001172964, -72.62310748452422615 ) ) ;
#220317 = DIRECTION ( 'NONE',  ( 0.000000000000000000, -1.186135710069610235E-15, 1.000000000000000000 ) ) ;
#220319 = VECTOR ( 'NONE', #134039, 1000.000000000000000 ) ;
#220321 = CARTESIAN_POINT ( 'NONE',  ( 20.85882249326303040, 65.66751761918619934, -30.42826094061123854 ) ) ;
#220320 = CIRCLE ( 'NONE', #107867, 0.09999999999999993616 ) ;
#220322 = FACE_OUTER_BOUND ( 'NONE', #69410, .T. ) ;
#220323 = CARTESIAN_POINT ( 'NONE',  ( -20.64999999999999858, 84.66355140188177586, -193.9990063664569959 ) ) ;
#220324 = AXIS2_PLACEMENT_3D ( 'NONE', #135291, #113181, #227020 ) ;
#220326 = CARTESIAN_POINT ( 'NONE',  ( -18.59999999999999787, 63.93636616954134411, -213.0474835168086827 ) ) ;
#220325 = VECTOR ( 'NONE', #253533, 1000.000000000000000 ) ;
#220327 = ORIENTED_EDGE ( 'NONE', *, *, #65994, .F. ) ;
#220328 = ORIENTED_EDGE ( 'NONE', *, *, #148032, .T. ) ;
#220329 = FACE_OUTER_BOUND ( 'NONE', #43155, .T. ) ;
#220331 = LINE ( 'NONE', #58650, #124464 ) ;
#220330 = FACE_OUTER_BOUND ( 'NONE', #164306, .T. ) ;
#220332 = CIRCLE ( 'NONE', #32915, 0.09999999999999741040 ) ;
#220333 = CARTESIAN_POINT ( 'NONE',  ( -21.14999999999999858, 65.49889199258218753, -241.8691648588935266 ) ) ;
#220334 = CARTESIAN_POINT ( 'NONE',  ( -21.14999999999999503, 12.95327426846188779, -205.2602563699350355 ) ) ;
#220336 = EDGE_CURVE ( 'NONE', #31313, #170158, #119243, .T. ) ;
#220335 = CARTESIAN_POINT ( 'NONE',  ( -20.64999999999999858, 76.00000000001246292, -172.0231074845243597 ) ) ;
#220337 = EDGE_LOOP ( 'NONE', ( #40895, #199526, #158658, #205495, #252152, #176050, #84134, #203175, #234504 ) ) ;
#220338 = LINE ( 'NONE', #121272, #1591 ) ;
#220339 = EDGE_LOOP ( 'NONE', ( #234308, #98450, #111148, #132823 ) ) ;
#220340 = ADVANCED_FACE ( 'NONE', ( #238896 ), #60237, .F. ) ;
#220341 = CONICAL_SURFACE ( 'NONE', #145480, 4.049999999999998934, 0.7853981633974604915 ) ;
#220343 = EDGE_CURVE ( 'NONE', #25429, #58178, #199785, .T. ) ;
#220342 = AXIS2_PLACEMENT_3D ( 'NONE', #208720, #169623, #186585 ) ;
#220345 = AXIS2_PLACEMENT_3D ( 'NONE', #88516, #168129, #243767 ) ;
#220344 = CARTESIAN_POINT ( 'NONE',  ( -16.85718274719440046, 51.68725577354657474, -231.8871841270915013 ) ) ;
#220346 = ORIENTED_EDGE ( 'NONE', *, *, #120018, .T. ) ;
#220347 = FACE_OUTER_BOUND ( 'NONE', #194205, .T. ) ;
#220348 = AXIS2_PLACEMENT_3D ( 'NONE', #198410, #60172, #82283 ) ;
#220349 = LINE ( 'NONE', #17017, #142194 ) ;
#220350 = VERTEX_POINT ( 'NONE', #161939 ) ;
#220351 = DIRECTION ( 'NONE',  ( 1.000000000000000000, 0.000000000000000000, 0.000000000000000000 ) ) ;
#220352 = ADVANCED_FACE ( 'NONE', ( #167089 ), #223160, .T. ) ;
#220353 = ORIENTED_EDGE ( 'NONE', *, *, #45841, .F. ) ;
#220354 = DIRECTION ( 'NONE',  ( -7.304098846218134667E-16, 1.000000000000000000, 6.982962677686266711E-15 ) ) ;
#220355 = CARTESIAN_POINT ( 'NONE',  ( -22.39999999999999503, 68.20922040163824818, -69.52310748452435973 ) ) ;
#220356 = CARTESIAN_POINT ( 'NONE',  ( -20.54999999999999716, 36.65892442174472876, -249.5511627012454596 ) ) ;
#220357 = CARTESIAN_POINT ( 'NONE',  ( -20.65000000000000568, 5.649999999999983480, -12.65000000000000213 ) ) ;
#220358 = CARTESIAN_POINT ( 'NONE',  ( -18.40000000000000213, 11.47316190337364183, -54.45000000000000284 ) ) ;
#220360 = CARTESIAN_POINT ( 'NONE',  ( 18.55807992284871588, 65.67101464000523947, -130.9404391622479977 ) ) ;
#220359 = CARTESIAN_POINT ( 'NONE',  ( -22.39999999999999858, 7.790779598384560245, -134.0000000000000000 ) ) ;
#220361 = LINE ( 'NONE', #41733, #223886 ) ;
#220363 = ORIENTED_EDGE ( 'NONE', *, *, #84751, .T. ) ;
#220362 = CARTESIAN_POINT ( 'NONE',  ( 20.86036036209898015, 65.37895722344113381, -128.8567590660221356 ) ) ;
#220365 = DIRECTION ( 'NONE',  ( 3.265361837132812600E-16, -0.9770955615653313941, -0.2128009952263603677 ) ) ;
#220364 = CARTESIAN_POINT ( 'NONE',  ( -20.64999999999999858, 73.60000000001180354, -82.74772940728642823 ) ) ;
#220366 = ORIENTED_EDGE ( 'NONE', *, *, #9995, .T. ) ;
#220368 = ORIENTED_EDGE ( 'NONE', *, *, #169195, .F. ) ;
#220367 = CARTESIAN_POINT ( 'NONE',  ( -22.39999999999999858, 55.96127771274636586, -232.9022175645438892 ) ) ;
#220369 = CIRCLE ( 'NONE', #195434, 0.3999999999999959699 ) ;
#220370 = ORIENTED_EDGE ( 'NONE', *, *, #92120, .T. ) ;
#220371 = LINE ( 'NONE', #59976, #3425 ) ;
#220372 = CARTESIAN_POINT ( 'NONE',  ( -21.95218792049438505, 30.04628837005676445, -252.4050306439679048 ) ) ;
#220373 = LINE ( 'NONE', #22180, #180807 ) ;
#220374 = VERTEX_POINT ( 'NONE', #129216 ) ;
#220375 = ADVANCED_FACE ( 'NONE', ( #30134 ), #67951, .F. ) ;
#220377 = EDGE_CURVE ( 'NONE', #195498, #81754, #73474, .T. ) ;
#220376 = DIRECTION ( 'NONE',  ( 1.000000000000000000, 0.000000000000000000, 0.000000000000000000 ) ) ;
#220378 = AXIS2_PLACEMENT_3D ( 'NONE', #232712, #9790, #172764 ) ;
#220379 = CARTESIAN_POINT ( 'NONE',  ( 20.94999999999999574, 48.04585786805223080, -246.4610531646956417 ) ) ;
#220380 = CARTESIAN_POINT ( 'NONE',  ( -21.05000000000000071, 76.00000000001145395, -40.12310748452431852 ) ) ;
#220381 = DIRECTION ( 'NONE',  ( 0.000000000000000000, 0.000000000000000000, -1.000000000000000000 ) ) ;
#220382 = EDGE_CURVE ( 'NONE', #153695, #223817, #48493, .T. ) ;
#220383 = DIRECTION ( 'NONE',  ( 0.000000000000000000, 0.000000000000000000, -1.000000000000000000 ) ) ;
#220384 = ORIENTED_EDGE ( 'NONE', *, *, #28063, .F. ) ;
#220385 = VERTEX_POINT ( 'NONE', #44549 ) ;
#220386 = AXIS2_PLACEMENT_3D ( 'NONE', #167676, #54111, #247174 ) ;
#220387 = CARTESIAN_POINT ( 'NONE',  ( 23.15000000000000213, -4.914013037343258894, -233.1828366659746905 ) ) ;
#220388 = AXIS2_PLACEMENT_3D ( 'NONE', #246904, #207823, #168718 ) ;
#220389 = VERTEX_POINT ( 'NONE', #182782 ) ;
#220390 = FACE_OUTER_BOUND ( 'NONE', #235376, .T. ) ;
#220391 = VERTEX_POINT ( 'NONE', #127934 ) ;
#220392 = DIRECTION ( 'NONE',  ( 0.000000000000000000, 0.000000000000000000, -1.000000000000000000 ) ) ;
#220393 = CARTESIAN_POINT ( 'NONE',  ( -20.94999999999999929, 68.87972903831429505, -99.36354444268502561 ) ) ;
#220394 = FACE_OUTER_BOUND ( 'NONE', #124448, .T. ) ;
#220395 = DIRECTION ( 'NONE',  ( -1.000000000000000000, 1.652117596168391700E-15, 0.000000000000000000 ) ) ;
#220396 = DIRECTION ( 'NONE',  ( 0.000000000000000000, 0.000000000000000000, 1.000000000000000000 ) ) ;
#220397 = VERTEX_POINT ( 'NONE', #224449 ) ;
#220398 = AXIS2_PLACEMENT_3D ( 'NONE', #176317, #216698, #255785 ) ;
#220399 = ADVANCED_FACE ( 'NONE', ( #45820 ), #204879, .F. ) ;
#220400 = DIRECTION ( 'NONE',  ( 0.000000000000000000, 0.2617529984164856383, 0.9651348961777204138 ) ) ;
#220401 = DIRECTION ( 'NONE',  ( -0.1538461538461484146, -0.9880948137434723000, 0.000000000000000000 ) ) ;
#220402 = DIRECTION ( 'NONE',  ( 0.000000000000000000, 0.000000000000000000, 1.000000000000000000 ) ) ;
#220403 = ORIENTED_EDGE ( 'NONE', *, *, #67883, .F. ) ;
#220405 = FACE_OUTER_BOUND ( 'NONE', #238658, .T. ) ;
#220404 = FACE_OUTER_BOUND ( 'NONE', #60156, .T. ) ;
#220406 = VERTEX_POINT ( 'NONE', #187910 ) ;
#220408 = ORIENTED_EDGE ( 'NONE', *, *, #137085, .T. ) ;
#220407 = DIRECTION ( 'NONE',  ( -0.000000000000000000, 0.9126074666063770380, 0.4088369013363281068 ) ) ;
#220409 = VECTOR ( 'NONE', #232102, 1000.000000000000000 ) ;
#220410 = EDGE_LOOP ( 'NONE', ( #8229, #34722, #211854, #198710 ) ) ;
#220411 = DIRECTION ( 'NONE',  ( -0.000000000000000000, 1.000000000000000000, -0.000000000000000000 ) ) ;
#220412 = CIRCLE ( 'NONE', #212028, 0.1000000000000028644 ) ;
#220413 = TOROIDAL_SURFACE ( 'NONE', #132922, 11.70000000000000107, 0.1000000000000000056 ) ;
#220414 = CIRCLE ( 'NONE', #53802, 0.09999999999999935330 ) ;
#220415 = SPHERICAL_SURFACE ( 'NONE', #44463, 0.1000000000000000056 ) ;
#220416 = EDGE_CURVE ( 'NONE', #203922, #20026, #69365, .T. ) ;
#220417 = DIRECTION ( 'NONE',  ( 0.000000000000000000, -6.467318590049456648E-15, 1.000000000000000000 ) ) ;
#220418 = EDGE_LOOP ( 'NONE', ( #180382, #228177, #2892 ) ) ;
#220419 = LINE ( 'NONE', #22224, #122089 ) ;
#220420 = CIRCLE ( 'NONE', #162157, 0.2000000000000027867 ) ;
#220421 = ADVANCED_FACE ( 'NONE', ( #147493 ), #27584, .F. ) ;
#220423 = DIRECTION ( 'NONE',  ( 0.000000000000000000, -0.9915357197604853789, 0.1298341882520022694 ) ) ;
#220422 = DIRECTION ( 'NONE',  ( -0.000000000000000000, 0.9126074666063771490, 0.4088369013363281623 ) ) ;
#220424 = ADVANCED_FACE ( 'NONE', ( #69254 ), #203610, .F. ) ;
#220426 = VERTEX_POINT ( 'NONE', #5379 ) ;
#220425 = DIRECTION ( 'NONE',  ( -1.000000000000000000, 0.000000000000000000, -0.000000000000000000 ) ) ;
#220427 = ORIENTED_EDGE ( 'NONE', *, *, #153882, .T. ) ;
#220428 = CARTESIAN_POINT ( 'NONE',  ( 22.45305468355010703, -2.598867842140088591, -189.5410128746470946 ) ) ;
#220429 = ADVANCED_FACE ( 'NONE', ( #64105 ), #177532, .T. ) ;
#220430 = DIRECTION ( 'NONE',  ( -1.000000000000000000, 0.000000000000000000, 0.000000000000000000 ) ) ;
#220432 = EDGE_CURVE ( 'NONE', #141245, #11304, #219169, .T. ) ;
#220431 = ORIENTED_EDGE ( 'NONE', *, *, #171032, .F. ) ;
#220433 = DIRECTION ( 'NONE',  ( 1.000000000000000000, 0.000000000000000000, -0.000000000000000000 ) ) ;
#220434 = ORIENTED_EDGE ( 'NONE', *, *, #55293, .T. ) ;
#220435 = CARTESIAN_POINT ( 'NONE',  ( -20.54999999999999716, 73.50000000001254818, -183.2477294072864709 ) ) ;
#220436 = LINE ( 'NONE', #121367, #170161 ) ;
#220437 = CARTESIAN_POINT ( 'NONE',  ( 20.93284271247462414, 64.25000000001219291, -143.5379132551784096 ) ) ;
#220438 = EDGE_CURVE ( 'NONE', #78303, #3356, #123505, .T. ) ;
#220439 = ORIENTED_EDGE ( 'NONE', *, *, #25711, .T. ) ;
#220440 = DIRECTION ( 'NONE',  ( -0.7071067811865460184, -0.6824534298470606997, 0.1850873201761399356 ) ) ;
#220441 = AXIS2_PLACEMENT_3D ( 'NONE', #80850, #60006, #219084 ) ;
#220442 = ADVANCED_FACE ( 'NONE', ( #186630 ), #87496, .T. ) ;
#220443 = TOROIDAL_SURFACE ( 'NONE', #174519, 0.2000000000000000111, 0.1000000000000000056 ) ;
#220444 = DIRECTION ( 'NONE',  ( 0.000000000000000000, 0.000000000000000000, -1.000000000000000000 ) ) ;
#220445 = ADVANCED_FACE ( 'NONE', ( #88775 ), #240041, .T. ) ;
#220446 = ADVANCED_FACE ( 'NONE', ( #168393 ), #155231, .F. ) ;
#220447 = AXIS2_PLACEMENT_3D ( 'NONE', #253247, #74668, #30378 ) ;
#220448 = B_SPLINE_CURVE_WITH_KNOTS ( 'NONE', 3,
 ( #248651, #33502, #111709, #231676, #249940, #28362, #71323, #212108, #112998, #152147 ),
 .UNSPECIFIED., .F., .F.,
 ( 4, 3, 3, 4 ),
 ( 4.906538933386797396E-18, 0.0002000000000002859679, 0.001000000000045107602, 0.001967863649472130407 ),
 .UNSPECIFIED. ) ;
#220449 = ORIENTED_EDGE ( 'NONE', *, *, #241044, .T. ) ;
#220450 = ORIENTED_EDGE ( 'NONE', *, *, #237408, .T. ) ;
#220451 = ORIENTED_EDGE ( 'NONE', *, *, #228944, .T. ) ;
#220452 = EDGE_CURVE ( 'NONE', #59275, #43988, #169669, .T. ) ;
#220453 = DIRECTION ( 'NONE',  ( -1.000000000000000000, -0.000000000000000000, -0.000000000000000000 ) ) ;
#220454 = VERTEX_POINT ( 'NONE', #54793 ) ;
#220456 = ORIENTED_EDGE ( 'NONE', *, *, #129260, .F. ) ;
#220455 = DIRECTION ( 'NONE',  ( 1.000000000000000000, -0.000000000000000000, -0.000000000000000000 ) ) ;
#220458 = EDGE_CURVE ( 'NONE', #201739, #158454, #189962, .T. ) ;
#220457 = VERTEX_POINT ( 'NONE', #131776 ) ;
#220459 = CIRCLE ( 'NONE', #8077, 0.09999999999999939493 ) ;
#220460 = ADVANCED_FACE ( 'NONE', ( #211321 ), #174809, .T. ) ;
#220463 = VERTEX_POINT ( 'NONE', #113498 ) ;
#220462 = ORIENTED_EDGE ( 'NONE', *, *, #30172, .F. ) ;
#220461 = DIRECTION ( 'NONE',  ( 1.000000000000000000, 0.000000000000000000, -0.000000000000000000 ) ) ;
#220464 = AXIS2_PLACEMENT_3D ( 'NONE', #154115, #152819, #111085 ) ;
#220465 = EDGE_CURVE ( 'NONE', #247920, #6886, #32723, .T. ) ;
#220466 = EDGE_LOOP ( 'NONE', ( #114178, #2741, #121581, #57161 ) ) ;
#220467 = FACE_OUTER_BOUND ( 'NONE', #87959, .T. ) ;
#220468 = CIRCLE ( 'NONE', #153876, 0.5000000000000008882 ) ;
#220469 = DIRECTION ( 'NONE',  ( -1.073024830501117725E-15, 6.982962677686266711E-15, -1.000000000000000000 ) ) ;
#220470 = DIRECTION ( 'NONE',  ( 0.000000000000000000, -0.8814952561688429444, 0.4721928772777349570 ) ) ;
#220471 = ORIENTED_EDGE ( 'NONE', *, *, #185841, .F. ) ;
#220472 = DIRECTION ( 'NONE',  ( 1.000000000000000000, 0.000000000000000000, 0.000000000000000000 ) ) ;
#220474 = ORIENTED_EDGE ( 'NONE', *, *, #68866, .F. ) ;
#220473 = CARTESIAN_POINT ( 'NONE',  ( 21.53551880898956838, 6.784797761427480367, -167.4010302654283180 ) ) ;
#220475 = DIRECTION ( 'NONE',  ( -0.000000000000000000, -0.000000000000000000, -1.000000000000000000 ) ) ;
#220477 = ORIENTED_EDGE ( 'NONE', *, *, #100253, .F. ) ;
#220476 = DIRECTION ( 'NONE',  ( -4.336808689941751890E-15, -0.8660254037844445918, -0.4999999999999897304 ) ) ;
#220478 = EDGE_CURVE ( 'NONE', #32249, #257642, #193049, .T. ) ;
#220479 = ORIENTED_EDGE ( 'NONE', *, *, #114824, .T. ) ;
#220480 = DIRECTION ( 'NONE',  ( -1.000000000000000000, 0.000000000000000000, 0.000000000000000000 ) ) ;
#220481 = CARTESIAN_POINT ( 'NONE',  ( -20.15000000000000568, 9.291421356248463326, -146.3500000000000227 ) ) ;
#220482 = ORIENTED_EDGE ( 'NONE', *, *, #252656, .T. ) ;
#220483 = ORIENTED_EDGE ( 'NONE', *, *, #202973, .F. ) ;
#220484 = CIRCLE ( 'NONE', #112170, 0.2000000000000057288 ) ;
#220485 = CARTESIAN_POINT ( 'NONE',  ( -16.87333278164158656, 9.882609784590076885, -180.6331678061535797 ) ) ;
#220486 = CARTESIAN_POINT ( 'NONE',  ( -21.05000000000000071, 0.03175835306662712354, -161.2411528769235929 ) ) ;
#220488 = ORIENTED_EDGE ( 'NONE', *, *, #72104, .T. ) ;
#220487 = ORIENTED_EDGE ( 'NONE', *, *, #84640, .F. ) ;
#220489 = ORIENTED_EDGE ( 'NONE', *, *, #103505, .T. ) ;
#220490 = CARTESIAN_POINT ( 'NONE',  ( -21.14999999999999858, 11.65000000001115588, -174.2838656629781156 ) ) ;
#220491 = ORIENTED_EDGE ( 'NONE', *, *, #147968, .F. ) ;
#220492 = ORIENTED_EDGE ( 'NONE', *, *, #16207, .F. ) ;
#220493 = DIRECTION ( 'NONE',  ( 0.000000000000000000, -0.4930308989875248349, -0.8700118002898312719 ) ) ;
#220494 = ORIENTED_EDGE ( 'NONE', *, *, #43570, .T. ) ;
#220496 = CARTESIAN_POINT ( 'NONE',  ( 18.52165635395179066, -9.481150711270972309, -107.5248375828625740 ) ) ;
#220495 = DIRECTION ( 'NONE',  ( 0.000000000000000000, -6.982962677686266711E-15, 1.000000000000000000 ) ) ;
#220497 = VERTEX_POINT ( 'NONE', #93931 ) ;
#220499 = VERTEX_POINT ( 'NONE', #13126 ) ;
#220498 = ORIENTED_EDGE ( 'NONE', *, *, #137823, .F. ) ;
#220501 = AXIS2_PLACEMENT_3D ( 'NONE', #7355, #106429, #185997 ) ;
#220500 = DIRECTION ( 'NONE',  ( -0.000000000000000000, -1.265107689135680095E-16, 1.000000000000000000 ) ) ;
#220503 = ADVANCED_FACE ( 'NONE', ( #10561 ), #65063, .T. ) ;
#220502 = DIRECTION ( 'NONE',  ( -0.000000000000000000, 0.2617529984165031243, 0.9651348961777157509 ) ) ;
#220504 = VECTOR ( 'NONE', #1125, 1000.000000000000000 ) ;
#220505 = CIRCLE ( 'NONE', #37345, 0.09999999999999939493 ) ;
#220506 = CIRCLE ( 'NONE', #199671, 0.1000000000000028644 ) ;
#220507 = ORIENTED_EDGE ( 'NONE', *, *, #68782, .T. ) ;
#220508 = EDGE_CURVE ( 'NONE', #182741, #58501, #98334, .T. ) ;
#220509 = AXIS2_PLACEMENT_3D ( 'NONE', #252975, #118632, #96453 ) ;
#220510 = CARTESIAN_POINT ( 'NONE',  ( 23.14999999999999858, 76.00000000001190870, -103.0231074845243029 ) ) ;
#220511 = ORIENTED_EDGE ( 'NONE', *, *, #91630, .F. ) ;
#220512 = ORIENTED_EDGE ( 'NONE', *, *, #111450, .F. ) ;
#220513 = DIRECTION ( 'NONE',  ( 0.000000000000000000, 0.000000000000000000, -1.000000000000000000 ) ) ;
#220514 = ORIENTED_EDGE ( 'NONE', *, *, #129148, .T. ) ;
#220515 = DIRECTION ( 'NONE',  ( 1.000000000000000000, -0.000000000000000000, 0.000000000000000000 ) ) ;
#220516 = VERTEX_POINT ( 'NONE', #153963 ) ;
#220517 = LINE ( 'NONE', #215361, #52230 ) ;
#220518 = CARTESIAN_POINT ( 'NONE',  ( 21.14999999999999858, -0.09999999998884338825, -134.0000000000000000 ) ) ;
#220520 = CARTESIAN_POINT ( 'NONE',  ( -16.80070461187883879, 9.950000000011266721, -121.3530361708397010 ) ) ;
#220519 = DIRECTION ( 'NONE',  ( 0.000000000000000000, 1.000000000000000000, -6.308085367188393199E-16 ) ) ;
#220521 = DIRECTION ( 'NONE',  ( 0.000000000000000000, 0.9126074666064696306, 0.4088369013361213278 ) ) ;
#220522 = AXIS2_PLACEMENT_3D ( 'NONE', #41219, #164985, #3322 ) ;
#220524 = CARTESIAN_POINT ( 'NONE',  ( 18.59999999999999076, 14.90151243843702566, -203.3975529985363551 ) ) ;
#220523 = VECTOR ( 'NONE', #209679, 1000.000000000000114 ) ;
#220525 = DIRECTION ( 'NONE',  ( 0.000000000000000000, 0.8700118002898322711, -0.4930308989875231140 ) ) ;
#220526 = CIRCLE ( 'NONE', #216214, 11.79999999999999893 ) ;
#220527 = CARTESIAN_POINT ( 'NONE',  ( -20.54999999999999716, 47.74660456829661825, -241.9541913331436263 ) ) ;
#220528 = DIRECTION ( 'NONE',  ( -0.000000000000000000, -0.000000000000000000, 1.000000000000000000 ) ) ;
#220529 = EDGE_CURVE ( 'NONE', #100799, #254615, #131707, .T. ) ;
#220530 = ORIENTED_EDGE ( 'NONE', *, *, #168054, .T. ) ;
#220532 = ORIENTED_EDGE ( 'NONE', *, *, #161341, .F. ) ;
#220531 = ORIENTED_EDGE ( 'NONE', *, *, #5499, .F. ) ;
#220533 = ORIENTED_EDGE ( 'NONE', *, *, #107077, .T. ) ;
#220534 = VERTEX_POINT ( 'NONE', #92640 ) ;
#220535 = DIRECTION ( 'NONE',  ( -1.000000000000000000, 0.000000000000000000, 0.000000000000000000 ) ) ;
#220536 = DIRECTION ( 'NONE',  ( 1.000000000000000000, 0.000000000000000000, 0.000000000000000000 ) ) ;
#220537 = CARTESIAN_POINT ( 'NONE',  ( -14.77738660682463667, 9.436552840004420517, -15.17795547276031520 ) ) ;
#220538 = LINE ( 'NONE', #252250, #128735 ) ;
#220539 = ORIENTED_EDGE ( 'NONE', *, *, #132995, .F. ) ;
#220540 = CARTESIAN_POINT ( 'NONE',  ( -23.25000000000000000, 77.85161776048053639, -57.91991776492063337 ) ) ;
#220541 = DIRECTION ( 'NONE',  ( -0.000000000000000000, 0.6132151058540549204, -0.7899159663865520375 ) ) ;
#220542 = DIRECTION ( 'NONE',  ( 1.000000000000000000, 0.000000000000000000, 0.000000000000000000 ) ) ;
#220543 = CYLINDRICAL_SURFACE ( 'NONE', #187416, 0.09999999999999939493 ) ;
#220544 = EDGE_LOOP ( 'NONE', ( #26978, #83400, #92858, #46323 ) ) ;
#220545 = AXIS2_PLACEMENT_3D ( 'NONE', #29872, #89797, #113221 ) ;
#220546 = DIRECTION ( 'NONE',  ( -3.265361837132813093E-16, 1.000000000000000000, 0.000000000000000000 ) ) ;
#220547 = ORIENTED_EDGE ( 'NONE', *, *, #231477, .F. ) ;
#220548 = LINE ( 'NONE', #241403, #41475 ) ;
#220549 = DIRECTION ( 'NONE',  ( 0.000000000000000000, 6.982962677686266711E-15, -1.000000000000000000 ) ) ;
#220550 = CARTESIAN_POINT ( 'NONE',  ( 23.40000000000004476, 84.00000000001119815, -37.18565239344504647 ) ) ;
#220551 = CARTESIAN_POINT ( 'NONE',  ( 18.59999999999999076, 10.20857864377385127, -121.8500000000000369 ) ) ;
#220552 = VERTEX_POINT ( 'NONE', #233471 ) ;
#220553 = CARTESIAN_POINT ( 'NONE',  ( -21.14999999999999858, 6.540656951701240729, -0.09999999999999939493 ) ) ;
#220555 = ADVANCED_FACE ( 'NONE', ( #56068 ), #213881, .F. ) ;
#220554 = DIRECTION ( 'NONE',  ( 1.000000000000000000, 0.000000000000000000, 0.000000000000000000 ) ) ;
#220556 = DIRECTION ( 'NONE',  ( -0.000000000000000000, 6.982962677686266711E-15, -1.000000000000000000 ) ) ;
#220558 = DIRECTION ( 'NONE',  ( -1.000000000000000000, 0.000000000000000000, 0.000000000000000000 ) ) ;
#220557 = DIRECTION ( 'NONE',  ( 0.000000000000000000, 0.2128009952263602844, -0.9770955615653315052 ) ) ;
#220559 = CARTESIAN_POINT ( 'NONE',  ( 20.95512820512820440, 10.62384868372303615, -45.65000000000000568 ) ) ;
#220560 = ADVANCED_FACE ( 'NONE', ( #75675 ), #194350, .T. ) ;
#220561 = CARTESIAN_POINT ( 'NONE',  ( -23.25000000000000000, 27.82649702422227733, -239.8850763025288870 ) ) ;
#220562 = LINE ( 'NONE', #22380, #205522 ) ;
#220563 = CARTESIAN_POINT ( 'NONE',  ( 18.50000000000000000, -9.399999999988843058, -207.8820418481726620 ) ) ;
#220564 = CIRCLE ( 'NONE', #4073, 0.09999999999999105438 ) ;
#220566 = ORIENTED_EDGE ( 'NONE', *, *, #219922, .F. ) ;
#220565 = DIRECTION ( 'NONE',  ( -0.000000000000000000, 0.8660254037844502539, 0.4999999999999799050 ) ) ;
#220567 = VECTOR ( 'NONE', #92686, 1000.000000000000000 ) ;
#220568 = ORIENTED_EDGE ( 'NONE', *, *, #131970, .T. ) ;
#220569 = EDGE_CURVE ( 'NONE', #102057, #88538, #135615, .T. ) ;
#220570 = AXIS2_PLACEMENT_3D ( 'NONE', #174114, #194933, #253587 ) ;
#220571 = EDGE_CURVE ( 'NONE', #3343, #42984, #248582, .T. ) ;
#220572 = AXIS2_PLACEMENT_3D ( 'NONE', #237250, #191734, #114736 ) ;
#220573 = EDGE_CURVE ( 'NONE', #177869, #169137, #173642, .T. ) ;
#220574 = CONICAL_SURFACE ( 'NONE', #108146, 4.299999999999956302, 0.7853981633974466137 ) ;
#220575 = CARTESIAN_POINT ( 'NONE',  ( -23.15000000000000213, 1.115649653272650466E-11, -171.5000000000000284 ) ) ;
#220576 = CARTESIAN_POINT ( 'NONE',  ( -18.57399277249657032, 65.66887361445283489, -30.43298459182691929 ) ) ;
#220577 = EDGE_CURVE ( 'NONE', #49989, #162629, #190496, .T. ) ;
#220578 = CARTESIAN_POINT ( 'NONE',  ( -21.05000000000000071, 76.00000000001222134, -148.2231074845243199 ) ) ;
#220579 = ORIENTED_EDGE ( 'NONE', *, *, #87750, .F. ) ;
#220580 = CIRCLE ( 'NONE', #237334, 0.09999999999999939493 ) ;
#220581 = CARTESIAN_POINT ( 'NONE',  ( -20.94999999999999929, -11.41227409413852989, -103.5000000000000426 ) ) ;
#220582 = AXIS2_PLACEMENT_3D ( 'NONE', #219990, #103872, #106434 ) ;
#220583 = CIRCLE ( 'NONE', #8206, 11.70000000000000284 ) ;
#220584 = DIRECTION ( 'NONE',  ( 0.000000000000000000, 0.000000000000000000, 1.000000000000000000 ) ) ;
#220585 = CARTESIAN_POINT ( 'NONE',  ( -18.52643265882458579, 65.68026841930900162, -97.47257401318891823 ) ) ;
#220586 = STYLED_ITEM ( 'NONE', ( #69801 ), #192084 ) ;
#220587 = AXIS2_PLACEMENT_3D ( 'NONE', #59657, #80496, #235748 ) ;
#220588 = DIRECTION ( 'NONE',  ( 0.000000000000000000, 0.000000000000000000, 1.000000000000000000 ) ) ;
#220590 = ORIENTED_EDGE ( 'NONE', *, *, #6719, .F. ) ;
#220589 = CARTESIAN_POINT ( 'NONE',  ( 18.59999999999999076, 1.115600667400684642E-11, -200.9999999999999432 ) ) ;
#220592 = DIRECTION ( 'NONE',  ( -0.000000000000000000, 0.9770955615653313941, 0.2128009952263603954 ) ) ;
#220591 = FACE_OUTER_BOUND ( 'NONE', #178319, .T. ) ;
#220593 = VECTOR ( 'NONE', #144166, 1000.000000000000000 ) ;
#220594 = EDGE_CURVE ( 'NONE', #62956, #90545, #31434, .T. ) ;
#220595 = CARTESIAN_POINT ( 'NONE',  ( 20.94999999999999929, 1.115600667400684642E-11, -146.9749999999999943 ) ) ;
#220596 = DIRECTION ( 'NONE',  ( 0.000000000000000000, 0.000000000000000000, -1.000000000000000000 ) ) ;
#220597 = EDGE_LOOP ( 'NONE', ( #227926, #4552, #17781, #146140, #45685, #241712, #199677, #77320, #243909, #252078, #51464, #191375, #143024, #43831, #192923, #11372, #135477, #91817, #14187, #96052, #111074, #187987 ) ) ;
#220598 = DIRECTION ( 'NONE',  ( 1.000000000000000000, 0.000000000000000000, 0.000000000000000000 ) ) ;
#220599 = CARTESIAN_POINT ( 'NONE',  ( 23.24999999999999645, 3.899999999999999467, -33.50000000000000000 ) ) ;
#220600 = DIRECTION ( 'NONE',  ( -0.5932847527679310229, -0.8049926720990042694, -4.984624513800578906E-15 ) ) ;
#220601 = EDGE_LOOP ( 'NONE', ( #192731, #167843, #110180, #248289 ) ) ;
#220602 = FACE_OUTER_BOUND ( 'NONE', #211008, .T. ) ;
#220603 = CARTESIAN_POINT ( 'NONE',  ( 23.24999999999999289, 11.75000000001116263, -100.6000000000000369 ) ) ;
#220605 = EDGE_LOOP ( 'NONE', ( #230273, #186461, #89145, #189792 ) ) ;
#220604 = AXIS2_PLACEMENT_3D ( 'NONE', #168289, #185237, #148694 ) ;
#220606 = DIRECTION ( 'NONE',  ( 0.000000000000000000, 6.982962677686266711E-15, -1.000000000000000000 ) ) ;
#220607 = CARTESIAN_POINT ( 'NONE',  ( 21.14999999999999858, 11.65000000001115943, -67.10000000000005116 ) ) ;
#220608 = CARTESIAN_POINT ( 'NONE',  ( -22.41119224318417125, 1.115600667400684642E-11, -122.3504291924552234 ) ) ;
#220609 = VERTEX_POINT ( 'NONE', #100326 ) ;
#220610 = ORIENTED_EDGE ( 'NONE', *, *, #113454, .T. ) ;
#220611 = AXIS2_PLACEMENT_3D ( 'NONE', #162672, #122260, #161399 ) ;
#220612 = DIRECTION ( 'NONE',  ( 0.000000000000000000, 6.982962677686266711E-15, -1.000000000000000000 ) ) ;
#220613 = CARTESIAN_POINT ( 'NONE',  ( 20.94999999999999929, 76.00000000001213607, -136.5231074845243313 ) ) ;
#220614 = CARTESIAN_POINT ( 'NONE',  ( 21.05000000000000071, 10.54375127550676616, -141.5563878086650504 ) ) ;
#220615 = DIRECTION ( 'NONE',  ( -1.000000000000000000, 0.000000000000000000, 0.000000000000000000 ) ) ;
#220616 = TOROIDAL_SURFACE ( 'NONE', #158117, 0.2000000000000000111, 0.1000000000000000056 ) ;
#220618 = DIRECTION ( 'NONE',  ( -3.469446951953604722E-14, -0.9999176327611370985, -0.01283462868040260302 ) ) ;
#220617 = CYLINDRICAL_SURFACE ( 'NONE', #257355, 0.09999999999999986677 ) ;
#220619 = CARTESIAN_POINT ( 'NONE',  ( -21.14999999999999858, 26.06832281015329755, -254.4051978787608732 ) ) ;
#220620 = LINE ( 'NONE', #99359, #181109 ) ;
#220621 = CARTESIAN_POINT ( 'NONE',  ( -20.94999999999999929, 18.82290990851282331, -233.3604470821920529 ) ) ;
#220622 = ORIENTED_EDGE ( 'NONE', *, *, #24830, .T. ) ;
#220623 = CARTESIAN_POINT ( 'NONE',  ( -18.40000000000000213, 11.75000000001113953, -113.1500000000000341 ) ) ;
#220624 = AXIS2_PLACEMENT_3D ( 'NONE', #238527, #97701, #114737 ) ;
#220625 = EDGE_CURVE ( 'NONE', #144144, #176263, #59919, .T. ) ;
#220627 = VERTEX_POINT ( 'NONE', #99041 ) ;
#220626 = FACE_OUTER_BOUND ( 'NONE', #27660, .T. ) ;
#220628 = DIRECTION ( 'NONE',  ( 3.616040088954497272E-32, -1.224646799147352961E-16, 1.000000000000000000 ) ) ;
#220629 = DIRECTION ( 'NONE',  ( 0.000000000000000000, -1.000000000000000000, -6.982962677686265922E-15 ) ) ;
#220631 = CARTESIAN_POINT ( 'NONE',  ( 20.85000000000000142, 1.115600667400684642E-11, -134.0000000000000284 ) ) ;
#220630 = CARTESIAN_POINT ( 'NONE',  ( -23.25000000000000000, 19.16534496950139399, -238.0132401564540032 ) ) ;
#220632 = ORIENTED_EDGE ( 'NONE', *, *, #102341, .F. ) ;
#220634 = FACE_OUTER_BOUND ( 'NONE', #33616, .T. ) ;
#220633 = CARTESIAN_POINT ( 'NONE',  ( -16.77180007708461673, 66.05000000001157900, -56.88749336556956848 ) ) ;
#220635 = DIRECTION ( 'NONE',  ( -1.000000000000000000, 2.952720810173289112E-16, 2.061873921506763405E-30 ) ) ;
#220636 = CARTESIAN_POINT ( 'NONE',  ( 23.14999999999999147, 67.23127455305841238, -235.8551265064783991 ) ) ;
#220637 = DIRECTION ( 'NONE',  ( 0.000000000000000000, 0.9651348961777157509, -0.2617529984165031243 ) ) ;
#220639 = EDGE_CURVE ( 'NONE', #85598, #200718, #200739, .T. ) ;
#220638 = DIRECTION ( 'NONE',  ( 0.000000000000000000, -0.2617529984165031243, -0.9651348961777157509 ) ) ;
#220640 = ORIENTED_EDGE ( 'NONE', *, *, #33816, .F. ) ;
#220641 = DIRECTION ( 'NONE',  ( 1.186688945009009831E-16, -1.000000000000000000, 0.000000000000000000 ) ) ;
#220643 = ORIENTED_EDGE ( 'NONE', *, *, #112127, .T. ) ;
#220642 = VECTOR ( 'NONE', #63140, 1000.000000000000000 ) ;
#220644 = TOROIDAL_SURFACE ( 'NONE', #104083, 0.9750000000000019762, 0.1000000000000000056 ) ;
#220645 = ADVANCED_FACE ( 'NONE', ( #20844 ), #139466, .T. ) ;
#220646 = EDGE_CURVE ( 'NONE', #65963, #29575, #231366, .T. ) ;
#220647 = FACE_OUTER_BOUND ( 'NONE', #15003, .T. ) ;
#220648 = EDGE_LOOP ( 'NONE', ( #139845, #109522, #134119, #71761 ) ) ;
#220649 = CARTESIAN_POINT ( 'NONE',  ( 15.74999999999999645, 9.849999999999981881, -16.74999999999999645 ) ) ;
#220650 = CIRCLE ( 'NONE', #158150, 0.1000000000000028644 ) ;
#220651 = ORIENTED_EDGE ( 'NONE', *, *, #135961, .T. ) ;
#220652 = DIRECTION ( 'NONE',  ( 1.000000000000000000, 7.304098846218163263E-16, -4.217023435051627211E-16 ) ) ;
#220653 = CARTESIAN_POINT ( 'NONE',  ( -23.15000000000000213, -11.88052908492542770, -191.5620167057819287 ) ) ;
#220654 = ORIENTED_EDGE ( 'NONE', *, *, #2191, .T. ) ;
#220655 = EDGE_CURVE ( 'NONE', #70783, #94097, #119952, .T. ) ;
#220656 = EDGE_CURVE ( 'NONE', #211293, #68795, #220314, .T. ) ;
#220657 = CARTESIAN_POINT ( 'NONE',  ( -23.15000000000000213, -8.999999999988846255, -177.3939691226524076 ) ) ;
#220658 = CARTESIAN_POINT ( 'NONE',  ( -21.07928932188134397, 65.47931918658504458, -241.9371126717015841 ) ) ;
#220659 = DIRECTION ( 'NONE',  ( 0.000000000000000000, 0.000000000000000000, -1.000000000000000000 ) ) ;
#220660 = CARTESIAN_POINT ( 'NONE',  ( -22.39999999999999858, 76.00000000001195133, -103.1231074845243114 ) ) ;
#220662 = AXIS2_PLACEMENT_3D ( 'NONE', #71256, #92071, #171655 ) ;
#220661 = LINE ( 'NONE', #22479, #12287 ) ;
#220663 = AXIS2_PLACEMENT_3D ( 'NONE', #218114, #61632, #177755 ) ;
#220664 = CARTESIAN_POINT ( 'NONE',  ( 13.54556439290364622, 62.05118075326792848, -218.8501529344108292 ) ) ;
#220665 = ORIENTED_EDGE ( 'NONE', *, *, #82955, .T. ) ;
#220666 = CARTESIAN_POINT ( 'NONE',  ( 23.24999999999999645, 70.40000000001187175, -90.61784146561124942 ) ) ;
#220667 = VERTEX_POINT ( 'NONE', #258093 ) ;
#220669 = ORIENTED_EDGE ( 'NONE', *, *, #134290, .T. ) ;
#220668 = DIRECTION ( 'NONE',  ( -1.000000000000000000, 0.000000000000000000, 0.000000000000000000 ) ) ;
#220670 = ORIENTED_EDGE ( 'NONE', *, *, #235489, .T. ) ;
#220671 = CARTESIAN_POINT ( 'NONE',  ( -18.59999999999999787, -1.835341550213255957, -112.1551512925630050 ) ) ;
#220672 = CARTESIAN_POINT ( 'NONE',  ( 15.74999999999999645, 66.65000000001258229, -186.7731074845244166 ) ) ;
#220673 = CARTESIAN_POINT ( 'NONE',  ( 20.94999999999999929, 70.15000000001252545, -180.1556047088023149 ) ) ;
#220674 = ADVANCED_FACE ( 'NONE', ( #18253 ), #179909, .F. ) ;
#220675 = CARTESIAN_POINT ( 'NONE',  ( -21.14999999999999858, 76.00000000001195133, -103.0231074845243171 ) ) ;
#220676 = ORIENTED_EDGE ( 'NONE', *, *, #119559, .T. ) ;
#220677 = EDGE_CURVE ( 'NONE', #146049, #16439, #231864, .T. ) ;
#220678 = EDGE_CURVE ( 'NONE', #243492, #15384, #6980, .T. ) ;
#220679 = CARTESIAN_POINT ( 'NONE',  ( 21.00000000000000000, 66.25000000001206502, -124.1731074845243654 ) ) ;
#220680 = CARTESIAN_POINT ( 'NONE',  ( -16.87683809663753109, 66.13508622147386973, -156.7473918488857692 ) ) ;
#220681 = ORIENTED_EDGE ( 'NONE', *, *, #251367, .F. ) ;
#220682 = CARTESIAN_POINT ( 'NONE',  ( -20.88420186297724257, 10.33025634371521662, -39.08709292826387838 ) ) ;
#220683 = CIRCLE ( 'NONE', #187362, 12.87499999999999822 ) ;
#220684 = AXIS2_PLACEMENT_3D ( 'NONE', #252256, #14961, #138699 ) ;
#220685 = AXIS2_PLACEMENT_3D ( 'NONE', #194703, #138516, #155585 ) ;
#220686 = DIRECTION ( 'NONE',  ( 0.000000000000000000, -0.9915357197604982575, 0.1298341882519033486 ) ) ;
#220687 = ORIENTED_EDGE ( 'NONE', *, *, #250758, .F. ) ;
#220688 = CARTESIAN_POINT ( 'NONE',  ( -16.96982749440708460, 9.950000000011137047, -147.1247784088109256 ) ) ;
#220689 = AXIS2_PLACEMENT_3D ( 'NONE', #196545, #53191, #191460 ) ;
#220690 = CARTESIAN_POINT ( 'NONE',  ( 18.59999999999999432, 44.52640028187936849, -247.3006740988509193 ) ) ;
#220691 = ORIENTED_EDGE ( 'NONE', *, *, #78201, .T. ) ;
#220692 = CARTESIAN_POINT ( 'NONE',  ( 18.59999999999999787, -10.35479209691423996, -127.7565409830737906 ) ) ;
#220693 = CARTESIAN_POINT ( 'NONE',  ( -11.60000000000000320, -8.250000000000005329, 10.95857864376268864 ) ) ;
#220695 = DIRECTION ( 'NONE',  ( -1.000000000000000000, -2.885090398161910739E-16, -6.283419270304611573E-17 ) ) ;
#220694 =( REPRESENTATION_RELATIONSHIP ('NONE','NONE', #36900, #73451 ) REPRESENTATION_RELATIONSHIP_WITH_TRANSFORMATION ( #50615 )SHAPE_REPRESENTATION_RELATIONSHIP( ) );
#220696 = DIRECTION ( 'NONE',  ( 0.000000000000000000, 0.2617529984165035684, 0.9651348961777156399 ) ) ;
#220697 = AXIS2_PLACEMENT_3D ( 'NONE', #197800, #178277, #79123 ) ;
#220698 = EDGE_CURVE ( 'NONE', #181313, #91518, #11263, .T. ) ;
#220699 = AXIS2_PLACEMENT_3D ( 'NONE', #122595, #97842, #100417 ) ;
#220700 = CARTESIAN_POINT ( 'NONE',  ( -23.15000000000000213, 49.36776662947724503, -253.7196102226803021 ) ) ;
#220701 = TOROIDAL_SURFACE ( 'NONE', #99855, 12.77499999999999858, 0.1000000000000000056 ) ;
#220702 = ORIENTED_EDGE ( 'NONE', *, *, #192808, .T. ) ;
#220703 = ORIENTED_EDGE ( 'NONE', *, *, #45197, .F. ) ;
#220704 = DIRECTION ( 'NONE',  ( -1.000000000000000000, 0.000000000000000000, 0.000000000000000000 ) ) ;
#220705 = EDGE_CURVE ( 'NONE', #132009, #101907, #159070, .T. ) ;
#220706 = DIRECTION ( 'NONE',  ( 1.000000000000000000, -1.836970198721029934E-16, -1.282749433769087582E-30 ) ) ;
#220709 = ORIENTED_EDGE ( 'NONE', *, *, #251581, .F. ) ;
#220708 = CARTESIAN_POINT ( 'NONE',  ( 21.13461538461538680, 10.61458296203669427, -146.2500000000000568 ) ) ;
#220707 =( BOUNDED_SURFACE ( )  B_SPLINE_SURFACE ( 3, 2, ( 
 ( #111845, #135231, #93549 ),
 ( #252616, #114404, #253899 ),
 ( #193952, #136508, #75306 ),
 ( #154840, #115691, #195252 ),
 ( #16609, #96102, #255137 ),
 ( #76548, #156129, #235619 ) ),
 .UNSPECIFIED., .F., .F., .F. ) 
 B_SPLINE_SURFACE_WITH_KNOTS ( ( 4, 2, 4 ),
 ( 3, 3 ),
 ( 0.0001300404313046710908, 0.0003183318589266656172, 0.0005066232865486601164 ),
 ( 0.000000000000000000, 1.000000000000000000 ),
 .UNSPECIFIED. ) 
 GEOMETRIC_REPRESENTATION_ITEM ( )  RATIONAL_B_SPLINE_SURFACE ( (
 ( 1.000000000000000000, 0.7071067811865475727, 1.000000000000000000),
 ( 1.000000000000000000, 0.7625113560542993163, 1.000000000000000000),
 ( 1.000000000000000000, 0.8126073484684785964, 1.000000000000000000),
 ( 1.000000000000000000, 0.8923049332736345818, 1.000000000000000000),
 ( 1.000000000000000000, 0.9231914937766407814, 1.000000000000000000),
 ( 1.000000000000000000, 0.9238795325112909573, 1.000000000000000000) ) ) 
 REPRESENTATION_ITEM ( '' )  SURFACE ( )  );
#220710 = CARTESIAN_POINT ( 'NONE',  ( -22.50000000000000000, 76.00000000001237765, -170.0231074845243597 ) ) ;
#220711 = CARTESIAN_POINT ( 'NONE',  ( 23.14999999999999147, 80.15000000001214175, -136.5231074845242460 ) ) ;
#220712 = CARTESIAN_POINT ( 'NONE',  ( 18.39999999999997371, 64.25000000001190870, -93.77310748452438816 ) ) ;
#220713 = ADVANCED_FACE ( 'NONE', ( #2521 ), #1231, .T. ) ;
#220714 = FACE_OUTER_BOUND ( 'NONE', #64610, .T. ) ;
#220715 = CARTESIAN_POINT ( 'NONE',  ( -18.40000000000000213, 85.50000000001209344, -129.5237453873441211 ) ) ;
#220717 = ORIENTED_EDGE ( 'NONE', *, *, #105413, .T. ) ;
#220716 = CARTESIAN_POINT ( 'NONE',  ( 20.85000000000000142, -1.263275465217258198, -41.40186466674640542 ) ) ;
#220718 = EDGE_CURVE ( 'NONE', #82125, #256377, #202788, .T. ) ;
#220719 = TOROIDAL_SURFACE ( 'NONE', #124858, 0.2000000000000000111, 0.1000000000000000056 ) ;
#220721 = ADVANCED_FACE ( 'NONE', ( #39122 ), #176072, .F. ) ;
#220720 = CARTESIAN_POINT ( 'NONE',  ( -18.59999999999999787, -1.164121893230052995, -74.91484808557160591 ) ) ;
#220723 = EDGE_CURVE ( 'NONE', #189375, #38731, #97756, .T. ) ;
#220722 = ORIENTED_EDGE ( 'NONE', *, *, #130609, .F. ) ;
#220724 = ORIENTED_EDGE ( 'NONE', *, *, #123563, .F. ) ;
#220725 = CIRCLE ( 'NONE', #108309, 0.09999999999999609201 ) ;
#220726 = DIRECTION ( 'NONE',  ( 1.000000000000000000, 0.000000000000000000, -0.000000000000000000 ) ) ;
#220727 = DIRECTION ( 'NONE',  ( 0.000000000000000000, -7.086529944415886769E-15, 1.000000000000000000 ) ) ;
#220728 = ORIENTED_EDGE ( 'NONE', *, *, #160933, .T. ) ;
#220729 = DIRECTION ( 'NONE',  ( 1.000000000000000000, 0.000000000000000000, -0.000000000000000000 ) ) ;
#220730 = CARTESIAN_POINT ( 'NONE',  ( -18.51991288638499356, 85.39243678968496454, -62.37984108056530630 ) ) ;
#220731 = ORIENTED_EDGE ( 'NONE', *, *, #133598, .F. ) ;
#220732 = CIRCLE ( 'NONE', #8368, 0.5000000000000004441 ) ;
#220734 = EDGE_CURVE ( 'NONE', #239491, #109070, #190163, .T. ) ;
#220733 = DIRECTION ( 'NONE',  ( 0.000000000000000000, 0.2211802418851293583, -0.9752329468386697897 ) ) ;
#220736 = ADVANCED_FACE ( 'NONE', ( #203311 ), #185024, .F. ) ;
#220735 = AXIS2_PLACEMENT_3D ( 'NONE', #18292, #36612, #215212 ) ;
#220737 = CARTESIAN_POINT ( 'NONE',  ( -20.54999999999999716, 85.00000000001159606, -60.12913836187181715 ) ) ;
#220738 = VERTEX_POINT ( 'NONE', #48078 ) ;
#220739 = VERTEX_POINT ( 'NONE', #182478 ) ;
#220740 = ORIENTED_EDGE ( 'NONE', *, *, #239586, .T. ) ;
#220741 = EDGE_CURVE ( 'NONE', #117253, #184932, #224142, .T. ) ;
#220742 = LINE ( 'NONE', #199914, #233689 ) ;
#220743 = EDGE_LOOP ( 'NONE', ( #163364, #3233, #226165, #138103 ) ) ;
#220745 = VERTEX_POINT ( 'NONE', #23419 ) ;
#220744 = FACE_OUTER_BOUND ( 'NONE', #23517, .T. ) ;
#220746 = AXIS2_PLACEMENT_3D ( 'NONE', #63095, #141358, #142624 ) ;
#220747 = CIRCLE ( 'NONE', #224999, 0.09999999999999939493 ) ;
#220748 = DIRECTION ( 'NONE',  ( 1.000000000000000000, 0.000000000000000000, 0.000000000000000000 ) ) ;
#220749 = ORIENTED_EDGE ( 'NONE', *, *, #224421, .F. ) ;
#220750 = CARTESIAN_POINT ( 'NONE',  ( -22.47071067811865319, 0.09909245471376178227, -92.77992525550196490 ) ) ;
#220752 = ORIENTED_EDGE ( 'NONE', *, *, #53447, .F. ) ;
#220751 = EDGE_CURVE ( 'NONE', #125507, #234183, #102896, .T. ) ;
#220754 = VERTEX_POINT ( 'NONE', #187614 ) ;
#220753 = VERTEX_POINT ( 'NONE', #63797 ) ;
#220755 = ADVANCED_FACE ( 'NONE', ( #166783 ), #207170, .T. ) ;
#220756 = DIRECTION ( 'NONE',  ( 1.000000000000000000, -0.000000000000000000, -0.000000000000000000 ) ) ;
#220757 = ORIENTED_EDGE ( 'NONE', *, *, #140100, .F. ) ;
#220758 = VECTOR ( 'NONE', #225982, 1000.000000000000000 ) ;
#220759 = CIRCLE ( 'NONE', #70764, 0.09999999999999939493 ) ;
#220760 = AXIS2_PLACEMENT_3D ( 'NONE', #33964, #192997, #75631 ) ;
#220761 = AXIS2_PLACEMENT_3D ( 'NONE', #61771, #25233, #123039 ) ;
#220762 = VECTOR ( 'NONE', #44498, 1000.000000000000000 ) ;
#220763 = EDGE_CURVE ( 'NONE', #191501, #196430, #115302, .T. ) ;
#220764 = ORIENTED_EDGE ( 'NONE', *, *, #172367, .T. ) ;
#220766 = AXIS2_PLACEMENT_3D ( 'NONE', #1787, #23959, #63049 ) ;
#220765 = DIRECTION ( 'NONE',  ( 0.000000000000000000, -0.8660254037844411501, -0.4999999999999956701 ) ) ;
#220767 = FACE_OUTER_BOUND ( 'NONE', #147978, .T. ) ;
#220769 = VERTEX_POINT ( 'NONE', #27276 ) ;
#220768 = FACE_OUTER_BOUND ( 'NONE', #244177, .T. ) ;
#220770 = ORIENTED_EDGE ( 'NONE', *, *, #7623, .T. ) ;
#220771 = CARTESIAN_POINT ( 'NONE',  ( -16.94107738177414291, 65.98576071487489969, -48.57310748452439952 ) ) ;
#220772 = DIRECTION ( 'NONE',  ( 1.000000000000000000, 0.000000000000000000, 0.000000000000000000 ) ) ;
#220773 = EDGE_CURVE ( 'NONE', #103755, #20245, #244995, .T. ) ;
#220774 = ORIENTED_EDGE ( 'NONE', *, *, #109751, .F. ) ;
#220775 = DIRECTION ( 'NONE',  ( -1.000000000000000000, 0.000000000000000000, 0.000000000000000000 ) ) ;
#220776 = DIRECTION ( 'NONE',  ( 0.7071067811865475727, 0.7071067811865475727, 0.000000000000000000 ) ) ;
#220777 = FACE_OUTER_BOUND ( 'NONE', #33578, .T. ) ;
#220778 = ORIENTED_EDGE ( 'NONE', *, *, #219474, .T. ) ;
#220779 = DIRECTION ( 'NONE',  ( -1.000000000000000000, 0.000000000000000000, 0.000000000000000000 ) ) ;
#220780 = ORIENTED_EDGE ( 'NONE', *, *, #196870, .T. ) ;
#220781 = ORIENTED_EDGE ( 'NONE', *, *, #83550, .T. ) ;
#220782 = ORIENTED_EDGE ( 'NONE', *, *, #108909, .F. ) ;
#220783 = ORIENTED_EDGE ( 'NONE', *, *, #36107, .T. ) ;
#220784 = CARTESIAN_POINT ( 'NONE',  ( -18.40000000000000213, 11.48667500176882328, -42.75000000000000000 ) ) ;
#220785 = ORIENTED_EDGE ( 'NONE', *, *, #53115, .T. ) ;
#220786 = FACE_OUTER_BOUND ( 'NONE', #121388, .T. ) ;
#220787 = EDGE_LOOP ( 'NONE', ( #231502, #16235, #222230, #203833, #245172, #21270 ) ) ;
#220788 = CARTESIAN_POINT ( 'NONE',  ( -20.64999999999999858, 73.50000000001199396, -116.2477294072864140 ) ) ;
#220789 = CARTESIAN_POINT ( 'NONE',  ( -20.85000000000000142, 76.00000000001170974, -69.52310748452431710 ) ) ;
#220790 = AXIS2_PLACEMENT_3D ( 'NONE', #109756, #85033, #49791 ) ;
#220791 = VERTEX_POINT ( 'NONE', #246291 ) ;
#220792 = VECTOR ( 'NONE', #35115, 1000.000000000000000 ) ;
#220793 = ORIENTED_EDGE ( 'NONE', *, *, #8782, .T. ) ;
#220794 = ORIENTED_EDGE ( 'NONE', *, *, #173914, .T. ) ;
#220795 = CIRCLE ( 'NONE', #54384, 0.09999999999999739653 ) ;
#220796 =( BOUNDED_CURVE ( )  B_SPLINE_CURVE ( 3, ( #200572, #221395, #138013, #38948 ),
 .UNSPECIFIED., .F., .F. ) 
 B_SPLINE_CURVE_WITH_KNOTS ( ( 4, 4 ),
 ( 2.589852378279005940, 2.850972632318389710 ),
 .UNSPECIFIED. ) 
 CURVE ( )  GEOMETRIC_REPRESENTATION_ITEM ( )  RATIONAL_B_SPLINE_CURVE ( ( 1.000000000000000000, 0.9943260843901262636, 0.9943260843901262636, 1.000000000000000000 ) ) 
 REPRESENTATION_ITEM ( '' )  );
#220797 = ADVANCED_FACE ( 'NONE', ( #67642 ), #83323, .T. ) ;
#220798 = CARTESIAN_POINT ( 'NONE',  ( 21.05000000000000071, 69.58602111852471239, -203.4373083682504273 ) ) ;
#220799 = CARTESIAN_POINT ( 'NONE',  ( -16.77683809663752257, 14.15196434607590348, -219.2423291894720307 ) ) ;
#220800 = FACE_OUTER_BOUND ( 'NONE', #216353, .T. ) ;
#220801 = CYLINDRICAL_SURFACE ( 'NONE', #82717, 0.1000000000000098310 ) ;
#220802 = LINE ( 'NONE', #42184, #98459 ) ;
#220803 = CARTESIAN_POINT ( 'NONE',  ( -33.72168855820452649, 33.92263863280957281, -235.0698407953532296 ) ) ;
#220804 = AXIS2_PLACEMENT_3D ( 'NONE', #55594, #13952, #229144 ) ;
#220806 = CARTESIAN_POINT ( 'NONE',  ( 21.10320863425824811, 6.400277386470322405, -100.4749777487729006 ) ) ;
#220805 = FACE_OUTER_BOUND ( 'NONE', #19767, .T. ) ;
#220807 = CYLINDRICAL_SURFACE ( 'NONE', #57372, 4.000000000000002665 ) ;
#220808 = FACE_OUTER_BOUND ( 'NONE', #227157, .T. ) ;
#220809 = CARTESIAN_POINT ( 'NONE',  ( 21.05000000000000071, 1.115600667400684642E-11, -134.0000000000000284 ) ) ;
#220810 = EDGE_CURVE ( 'NONE', #127836, #231419, #256735, .T. ) ;
#220811 = CARTESIAN_POINT ( 'NONE',  ( -18.39999999999999858, 11.74999999999998224, -9.250000000000001776 ) ) ;
#220812 = AXIS2_PLACEMENT_3D ( 'NONE', #164715, #120480, #139984 ) ;
#220813 = ORIENTED_EDGE ( 'NONE', *, *, #209491, .T. ) ;
#220814 = AXIS2_PLACEMENT_3D ( 'NONE', #1035, #122304, #257904 ) ;
#220816 = ORIENTED_EDGE ( 'NONE', *, *, #79604, .T. ) ;
#220815 = DIRECTION ( 'NONE',  ( -1.000000000000000000, 0.000000000000000000, 0.000000000000000000 ) ) ;
#220817 = VERTEX_POINT ( 'NONE', #24699 ) ;
#220818 = DIRECTION ( 'NONE',  ( -0.000000000000000000, -1.000000000000000000, 0.000000000000000000 ) ) ;
#220819 = CARTESIAN_POINT ( 'NONE',  ( -23.15000000000000213, 2.600000000011156054, -88.75000000000004263 ) ) ;
#220820 = CARTESIAN_POINT ( 'NONE',  ( -21.14999999999994174, 64.35000000001120668, -30.12310748452479103 ) ) ;
#220821 = ORIENTED_EDGE ( 'NONE', *, *, #247947, .T. ) ;
#220822 =( NAMED_UNIT ( * ) PLANE_ANGLE_UNIT ( ) SI_UNIT ( $, .RADIAN. ) );
#220824 = VECTOR ( 'NONE', #184891, 1000.000000000000000 ) ;
#220823 = DIRECTION ( 'NONE',  ( -1.000000000000000000, -0.000000000000000000, -0.000000000000000000 ) ) ;
#220825 = AXIS2_PLACEMENT_3D ( 'NONE', #48175, #110723, #28675 ) ;
#220826 = CARTESIAN_POINT ( 'NONE',  ( -33.72168855820451938, 9.950000000000001066, -20.85000000000005471 ) ) ;
#220827 = ORIENTED_EDGE ( 'NONE', *, *, #113908, .F. ) ;
#220828 = CARTESIAN_POINT ( 'NONE',  ( -21.03571358705729466, 11.75000000001115374, -140.8251068220585864 ) ) ;
#220829 = CARTESIAN_POINT ( 'NONE',  ( 21.05000000000000071, 0.09779029131994770863, -60.74218538952391810 ) ) ;
#220830 = DIRECTION ( 'NONE',  ( 0.000000000000000000, -1.000000000000000000, 0.000000000000000000 ) ) ;
#220831 = FACE_OUTER_BOUND ( 'NONE', #161736, .T. ) ;
#220833 = ORIENTED_EDGE ( 'NONE', *, *, #63763, .T. ) ;
#220832 = CARTESIAN_POINT ( 'NONE',  ( -20.54999999999999716, 68.85000000001225828, -153.2731074845244166 ) ) ;
#220835 = VERTEX_POINT ( 'NONE', #242418 ) ;
#220834 = LINE ( 'NONE', #164730, #64907 ) ;
#220836 = FACE_OUTER_BOUND ( 'NONE', #173212, .T. ) ;
#220837 = CARTESIAN_POINT ( 'NONE',  ( 18.59999999999999076, 64.35000000001147669, -44.67310748452440095 ) ) ;
#220838 = LINE ( 'NONE', #181728, #252598 ) ;
#220839 = CARTESIAN_POINT ( 'NONE',  ( -15.39946565075089779, 9.389534562357860992, -183.1748093043898962 ) ) ;
#220840 = TOROIDAL_SURFACE ( 'NONE', #95930, 0.2000000000000000111, 0.1000000000000000056 ) ;
#220843 = CARTESIAN_POINT ( 'NONE',  ( -20.94999999999999929, 44.58277672189309015, -247.4925639031954745 ) ) ;
#220842 = CIRCLE ( 'NONE', #241700, 12.77500000000000036 ) ;
#220841 = CARTESIAN_POINT ( 'NONE',  ( -17.73285935859622953, 65.14201819621573009, -79.76454567473506074 ) ) ;
#220844 = CARTESIAN_POINT ( 'NONE',  ( 20.94999999999999929, 5.000000000011153745, -54.99473398108690958 ) ) ;
#220846 = EDGE_CURVE ( 'NONE', #104861, #189061, #140226, .T. ) ;
#220845 = CARTESIAN_POINT ( 'NONE',  ( 23.24999999999999645, 67.17743825834619997, -190.8731074845244109 ) ) ;
#220847 = AXIS2_PLACEMENT_3D ( 'NONE', #186928, #87775, #167366 ) ;
#220848 =( NAMED_UNIT ( * ) SI_UNIT ( $, .STERADIAN. ) SOLID_ANGLE_UNIT ( ) );
#220849 = LINE ( 'NONE', #142583, #243573 ) ;
#220850 = CARTESIAN_POINT ( 'NONE',  ( 21.10320863425824811, 10.12894173882548365, -228.0790718293079067 ) ) ;
#220851 = ORIENTED_EDGE ( 'NONE', *, *, #154511, .T. ) ;
#220852 = CARTESIAN_POINT ( 'NONE',  ( -21.59142135623730852, 68.15000000001253966, -182.3731074845244109 ) ) ;
#220853 = AXIS2_PLACEMENT_3D ( 'NONE', #141705, #221231, #218666 ) ;
#220854 = EDGE_LOOP ( 'NONE', ( #83872, #104105, #60744, #208920 ) ) ;
#220855 = ORIENTED_EDGE ( 'NONE', *, *, #134512, .F. ) ;
#220856 = EDGE_CURVE ( 'NONE', #233400, #190315, #136113, .T. ) ;
#220857 = CARTESIAN_POINT ( 'NONE',  ( -21.05000000000000071, 11.59999999999999787, -26.57179676972450011 ) ) ;
#220858 = EDGE_LOOP ( 'NONE', ( #64318, #126787, #230811, #206246 ) ) ;
#220859 = ADVANCED_FACE ( 'NONE', ( #183749 ), #42954, .T. ) ;
#220860 = AXIS2_PLACEMENT_3D ( 'NONE', #69245, #10549, #246568 ) ;
#220861 = ORIENTED_EDGE ( 'NONE', *, *, #101765, .F. ) ;
#220862 = EDGE_CURVE ( 'NONE', #21614, #136482, #165477, .T. ) ;
#220863 = ORIENTED_EDGE ( 'NONE', *, *, #180891, .T. ) ;
#220864 = CARTESIAN_POINT ( 'NONE',  ( -23.15000000000000213, 1.148907358139439339E-11, -201.0000000000015064 ) ) ;
#220865 = ORIENTED_EDGE ( 'NONE', *, *, #165751, .F. ) ;
#220866 = DIRECTION ( 'NONE',  ( 1.000000000000000000, 0.000000000000000000, -0.000000000000000000 ) ) ;
#220867 = FACE_OUTER_BOUND ( 'NONE', #241760, .T. ) ;
#220868 = LINE ( 'NONE', #244281, #96884 ) ;
#220869 = CARTESIAN_POINT ( 'NONE',  ( -18.50000000000000000, 85.40000000001232650, -162.7258477248610120 ) ) ;
#220870 = CARTESIAN_POINT ( 'NONE',  ( 22.60000000000000142, 76.00000000001165290, -69.52310748452431710 ) ) ;
#220871 = SPHERICAL_SURFACE ( 'NONE', #125098, 0.1000000000000000056 ) ;
#220872 = DIRECTION ( 'NONE',  ( 1.000000000000000000, 0.000000000000000000, 0.000000000000000000 ) ) ;
#220874 = VERTEX_POINT ( 'NONE', #46779 ) ;
#220873 = DIRECTION ( 'NONE',  ( 1.000000000000000000, 0.000000000000000000, 0.000000000000000000 ) ) ;
#220876 = CARTESIAN_POINT ( 'NONE',  ( 18.58719872626880232, 85.56664439761000551, -29.20062928812724223 ) ) ;
#220875 = FACE_OUTER_BOUND ( 'NONE', #217116, .T. ) ;
#220877 = EDGE_CURVE ( 'NONE', #99784, #74339, #243717, .T. ) ;
#220878 = CARTESIAN_POINT ( 'NONE',  ( -18.50000000000000000, -1.164121893230052995, -74.91484808557160591 ) ) ;
#220879 = EDGE_LOOP ( 'NONE', ( #256185, #220026, #251825, #209913, #12696 ) ) ;
#220880 = DIRECTION ( 'NONE',  ( 1.000000000000000000, 0.000000000000000000, 0.000000000000000000 ) ) ;
#220881 = SURFACE_SIDE_STYLE ('',( #219595 ) ) ;
#220882 = ORIENTED_EDGE ( 'NONE', *, *, #24733, .F. ) ;
#220884 = CARTESIAN_POINT ( 'NONE',  ( -23.25000000000000000, 31.85509083104287598, -238.8280249686205536 ) ) ;
#220883 = CARTESIAN_POINT ( 'NONE',  ( 18.39999999999999503, 53.37686160793744961, -235.8706811220569932 ) ) ;
#220885 = AXIS2_PLACEMENT_3D ( 'NONE', #132183, #228734, #29278 ) ;
#220886 = CARTESIAN_POINT ( 'NONE',  ( -16.89935556175729303, 66.05000000001182059, -82.66278384740907370 ) ) ;
#220887 = ORIENTED_EDGE ( 'NONE', *, *, #44279, .T. ) ;
#220888 = CARTESIAN_POINT ( 'NONE',  ( 21.05000000000000071, 6.304516329275136499, -67.02110330805874128 ) ) ;
#220890 = CARTESIAN_POINT ( 'NONE',  ( -15.75000000000000355, 9.350000000011140955, -83.75000000000004263 ) ) ;
#220889 = AXIS2_PLACEMENT_3D ( 'NONE', #87765, #47353, #64375 ) ;
#220891 = FACE_OUTER_BOUND ( 'NONE', #177124, .T. ) ;
#220892 = ORIENTED_EDGE ( 'NONE', *, *, #17357, .F. ) ;
#220893 = ADVANCED_FACE ( 'NONE', ( #144596 ), #7686, .F. ) ;
#220894 = DIRECTION ( 'NONE',  ( 0.000000000000000000, -0.8814952561688430555, 0.4721928772777345684 ) ) ;
#220895 = DIRECTION ( 'NONE',  ( 1.000000000000000000, 0.000000000000000000, 0.000000000000000000 ) ) ;
#220896 = DIRECTION ( 'NONE',  ( 0.000000000000000000, 0.000000000000000000, -1.000000000000000000 ) ) ;
#220897 = AXIS2_PLACEMENT_3D ( 'NONE', #206861, #50330, #189868 ) ;
#220898 = CARTESIAN_POINT ( 'NONE',  ( 22.50000000000000000, 0.1000000000111554016, -155.8504291924551808 ) ) ;
#220900 = CARTESIAN_POINT ( 'NONE',  ( -18.44362607810622023, 85.49049615809714453, -162.9651536176772026 ) ) ;
#220899 = AXIS2_PLACEMENT_3D ( 'NONE', #37259, #78903, #235419 ) ;
#220901 = EDGE_CURVE ( 'NONE', #216625, #208580, #61155, .T. ) ;
#220903 = EDGE_LOOP ( 'NONE', ( #177499, #28179, #30927, #213907 ) ) ;
#220902 = CARTESIAN_POINT ( 'NONE',  ( -22.94999999999999929, -1.300000000000000044, -7.900000000000000355 ) ) ;
#220904 = CARTESIAN_POINT ( 'NONE',  ( 21.05000000000000071, 8.776282895303632259, -142.5586289951409640 ) ) ;
#220905 = CARTESIAN_POINT ( 'NONE',  ( -18.59999999999999787, 64.35000000001161879, -62.50830171387039513 ) ) ;
#220906 = DIRECTION ( 'NONE',  ( 0.000000000000000000, 7.109473446599835262E-15, -1.000000000000000000 ) ) ;
#220907 = CARTESIAN_POINT ( 'NONE',  ( -16.27683809663750480, 66.65000000001263913, -194.2731074845244166 ) ) ;
#220909 = ORIENTED_EDGE ( 'NONE', *, *, #208820, .T. ) ;
#220908 = CARTESIAN_POINT ( 'NONE',  ( -18.50000000000000000, 61.57587952878036930, -212.2000740415318774 ) ) ;
#220910 = FACE_OUTER_BOUND ( 'NONE', #28709, .T. ) ;
#220911 = AXIS2_PLACEMENT_3D ( 'NONE', #65365, #82331, #6670 ) ;
#220912 = CARTESIAN_POINT ( 'NONE',  ( -23.15000000000000213, 49.57218508014541669, -254.1759139559835035 ) ) ;
#220913 = LINE ( 'NONE', #138782, #232310 ) ;
#220915 = EDGE_CURVE ( 'NONE', #168958, #165708, #152352, .T. ) ;
#220914 = CIRCLE ( 'NONE', #158593, 0.1000000000000053069 ) ;
#220916 = ORIENTED_EDGE ( 'NONE', *, *, #64609, .F. ) ;
#220917 = CARTESIAN_POINT ( 'NONE',  ( -13.11924609551134502, 66.56831044948815190, -151.7438174522883401 ) ) ;
#220918 = LINE ( 'NONE', #1864, #46093 ) ;
#220919 = EDGE_CURVE ( 'NONE', #227883, #188779, #213564, .T. ) ;
#220920 = DIRECTION ( 'NONE',  ( -1.000000000000000000, -2.885090398161910739E-16, -6.283419270304611573E-17 ) ) ;
#220922 = CARTESIAN_POINT ( 'NONE',  ( -16.88783316861814399, 9.950000000011137047, -87.74773595802028581 ) ) ;
#220921 = AXIS2_PLACEMENT_3D ( 'NONE', #186284, #7640, #67600 ) ;
#220923 = AXIS2_PLACEMENT_3D ( 'NONE', #79529, #20894, #57402 ) ;
#220925 = ORIENTED_EDGE ( 'NONE', *, *, #238222, .F. ) ;
#220924 = AXIS2_PLACEMENT_3D ( 'NONE', #154859, #75325, #153602 ) ;
#220926 = EDGE_LOOP ( 'NONE', ( #219935, #195555, #95653, #60508 ) ) ;
#220927 = AXIS2_PLACEMENT_3D ( 'NONE', #196496, #17856, #97368 ) ;
#220928 = AXIS2_PLACEMENT_3D ( 'NONE', #8906, #247516, #147116 ) ;
#220929 = CARTESIAN_POINT ( 'NONE',  ( 21.07016717457010913, -1.345102501103334403, -194.8238367621760574 ) ) ;
#220930 = DIRECTION ( 'NONE',  ( -0.000000000000000000, -0.000000000000000000, 1.000000000000000000 ) ) ;
#220931 = ADVANCED_FACE ( 'NONE', ( #188881 ), #251418, .F. ) ;
#220932 = DIRECTION ( 'NONE',  ( 0.000000000000000000, 0.2617529984165030688, 0.9651348961777157509 ) ) ;
#220933 = DIRECTION ( 'NONE',  ( 1.000000000000000000, -7.304098846218133681E-16, 4.607487905232622991E-31 ) ) ;
#220934 = EDGE_LOOP ( 'NONE', ( #240279, #233675, #46923, #186755, #158849 ) ) ;
#220935 = CARTESIAN_POINT ( 'NONE',  ( -23.25000000000000000, 11.65000000001115588, -88.35000000000003695 ) ) ;
#220936 = EDGE_CURVE ( 'NONE', #232566, #185866, #194458, .T. ) ;
#220938 = ADVANCED_FACE ( 'NONE', ( #233165 ), #211015, .T. ) ;
#220937 = CARTESIAN_POINT ( 'NONE',  ( 20.97250901189795158, 12.01224122581901277, -206.2280749500426111 ) ) ;
#220939 = DIRECTION ( 'NONE',  ( -1.000000000000000000, -0.000000000000000000, -0.000000000000000000 ) ) ;
#220940 = B_SPLINE_CURVE_WITH_KNOTS ( 'NONE', 3,
 ( #74034, #154845, #113124, #150972, #34907, #170588, #14040, #153587, #191412, #195257, #51841, #132699, #11472, #96107, #92264, #250070, #71453, #255142, #230512 ),
 .UNSPECIFIED., .F., .F.,
 ( 4, 3, 3, 3, 3, 3, 4 ),
 ( 1.387778780781445676E-17, 2.646747978908895087E-05, 5.271166642129234721E-05, 9.008788829885287059E-05, 0.0001426648776561089771, 0.0001897378458659771045, 0.0001917382627806340850 ),
 .UNSPECIFIED. ) ;
#220941 = CYLINDRICAL_SURFACE ( 'NONE', #116159, 0.09999999999999939493 ) ;
#220942 = CARTESIAN_POINT ( 'NONE',  ( -16.82542659449979539, 9.934499891427430285, -20.75536439997388527 ) ) ;
#220943 = CARTESIAN_POINT ( 'NONE',  ( 18.59999999999999076, 65.50857864377445594, -78.17310748452437963 ) ) ;
#220944 = ORIENTED_EDGE ( 'NONE', *, *, #126436, .F. ) ;
#220946 = EDGE_LOOP ( 'NONE', ( #178108, #115444, #49112, #50620 ) ) ;
#220945 = CARTESIAN_POINT ( 'NONE',  ( -20.85000000000000142, 87.75000000001173817, -72.42310748452422331 ) ) ;
#220947 = ADVANCED_FACE ( 'NONE', ( #71524 ), #174510, .F. ) ;
#220948 = ORIENTED_EDGE ( 'NONE', *, *, #33615, .T. ) ;
#220949 = CARTESIAN_POINT ( 'NONE',  ( 20.94999999999999574, 43.04635563724865932, -239.7315875678428370 ) ) ;
#220950 = ORIENTED_EDGE ( 'NONE', *, *, #66202, .T. ) ;
#220951 = DIRECTION ( 'NONE',  ( 1.000000000000000000, 0.000000000000000000, 0.000000000000000000 ) ) ;
#220952 = CARTESIAN_POINT ( 'NONE',  ( -23.25000000000000000, 68.97833521811159585, -65.68954208262705663 ) ) ;
#220953 = LINE ( 'NONE', #201398, #149963 ) ;
#220954 = B_SPLINE_CURVE_WITH_KNOTS ( 'NONE', 3,
 ( #16652, #195305, #118314, #81701, #238243, #76603, #219967, #19203 ),
 .UNSPECIFIED., .F., .F.,
 ( 4, 2, 2, 4 ),
 ( 0.000000000000000000, 9.550056980122538541E-05, 0.0001910011396024507708, 0.0003820022792049804173 ),
 .UNSPECIFIED. ) ;
#220955 = ORIENTED_EDGE ( 'NONE', *, *, #110532, .F. ) ;
#220956 = ADVANCED_FACE ( 'NONE', ( #229299 ), #14113, .F. ) ;
#220957 = EDGE_CURVE ( 'NONE', #255695, #52077, #114473, .T. ) ;
#220958 = CYLINDRICAL_SURFACE ( 'NONE', #61523, 0.1000000000000118433 ) ;
#220959 = FACE_OUTER_BOUND ( 'NONE', #247850, .T. ) ;
#220961 = ORIENTED_EDGE ( 'NONE', *, *, #177110, .T. ) ;
#220960 = VECTOR ( 'NONE', #174939, 1000.000000000000000 ) ;
#220962 = CARTESIAN_POINT ( 'NONE',  ( -16.87036670365548474, 9.989418819312801290, -54.47956011730205006 ) ) ;
#220964 = VERTEX_POINT ( 'NONE', #89763 ) ;
#220963 = DIRECTION ( 'NONE',  ( -1.020425574104003999E-15, 0.2128009952263603677, -0.9770955615653313941 ) ) ;
#220965 = CIRCLE ( 'NONE', #4297, 11.75000000000000000 ) ;
#220966 = DIRECTION ( 'NONE',  ( 0.000000000000000000, 0.000000000000000000, -1.000000000000000000 ) ) ;
#220967 = DIRECTION ( 'NONE',  ( -0.000000000000000000, -6.982962677686266711E-15, 1.000000000000000000 ) ) ;
#220968 = AXIS2_PLACEMENT_3D ( 'NONE', #72288, #189656, #170135 ) ;
#220969 = EDGE_LOOP ( 'NONE', ( #91567, #83504, #86061, #156193 ) ) ;
#220970 = CARTESIAN_POINT ( 'NONE',  ( -16.77683809663752257, 9.945835743215301505, -79.66394901910425119 ) ) ;
#220971 = CARTESIAN_POINT ( 'NONE',  ( 21.05000000000000071, 71.14953271029297355, -191.4888400755227167 ) ) ;
#220972 = CIRCLE ( 'NONE', #146522, 4.000000000000003553 ) ;
#220973 = DIRECTION ( 'NONE',  ( 1.000000000000000000, 0.000000000000000000, 0.000000000000000000 ) ) ;
#220974 = ORIENTED_EDGE ( 'NONE', *, *, #88734, .T. ) ;
#220975 = DIRECTION ( 'NONE',  ( 0.000000000000000000, -0.8660254037844411501, -0.4999999999999956701 ) ) ;
#220976 = ADVANCED_FACE ( 'NONE', ( #170652 ), #207094, .T. ) ;
#220977 = EDGE_CURVE ( 'NONE', #200038, #177863, #73830, .T. ) ;
#220978 = DIRECTION ( 'NONE',  ( -4.336808689941751890E-15, -0.8660254037844445918, -0.4999999999999897304 ) ) ;
#220979 = DIRECTION ( 'NONE',  ( 0.000000000000000000, 0.000000000000000000, 1.000000000000000000 ) ) ;
#220980 = AXIS2_PLACEMENT_3D ( 'NONE', #233656, #156708, #35477 ) ;
#220981 = ORIENTED_EDGE ( 'NONE', *, *, #133496, .F. ) ;
#220982 = EDGE_CURVE ( 'NONE', #47325, #105460, #110623, .T. ) ;
#220983 = AXIS2_PLACEMENT_3D ( 'NONE', #30066, #225637, #109556 ) ;
#220984 = VECTOR ( 'NONE', #239463, 1000.000000000000000 ) ;
#220986 = ORIENTED_EDGE ( 'NONE', *, *, #96503, .F. ) ;
#220985 = AXIS2_PLACEMENT_3D ( 'NONE', #210859, #209578, #10089 ) ;
#220987 = ORIENTED_EDGE ( 'NONE', *, *, #196574, .F. ) ;
#220988 = CARTESIAN_POINT ( 'NONE',  ( 18.51697539158856642, 10.31565961586830760, -39.03641941191783360 ) ) ;
#220989 = DIRECTION ( 'NONE',  ( -0.000000000000000000, -6.982962677686266711E-15, 1.000000000000000000 ) ) ;
#220991 = ORIENTED_EDGE ( 'NONE', *, *, #75850, .T. ) ;
#220990 = CARTESIAN_POINT ( 'NONE',  ( 20.94999999999999929, 1.115600667400684642E-11, -167.5000000000000284 ) ) ;
#220992 = CARTESIAN_POINT ( 'NONE',  ( 20.94999999999999929, 5.399999999999998579, -23.60603087734755690 ) ) ;
#220993 = LINE ( 'NONE', #42372, #36597 ) ;
#220994 = FACE_OUTER_BOUND ( 'NONE', #246846, .T. ) ;
#220995 = FACE_OUTER_BOUND ( 'NONE', #251648, .T. ) ;
#220996 = LINE ( 'NONE', #65790, #154502 ) ;
#220997 = ADVANCED_FACE ( 'NONE', ( #113191 ), #51907, .T. ) ;
#220998 = DIRECTION ( 'NONE',  ( 0.000000000000000000, 6.982962677686266711E-15, -1.000000000000000000 ) ) ;
#221000 = ORIENTED_EDGE ( 'NONE', *, *, #74192, .T. ) ;
#220999 = DIRECTION ( 'NONE',  ( 0.000000000000000000, 1.000000000000000000, 6.853228547068871147E-15 ) ) ;
#221002 = VERTEX_POINT ( 'NONE', #248857 ) ;
#221001 = LINE ( 'NONE', #22845, #173661 ) ;
#221003 = LINE ( 'NONE', #106186, #137131 ) ;
#221004 = AXIS2_PLACEMENT_3D ( 'NONE', #2304, #240943, #62299 ) ;
#221005 = ORIENTED_EDGE ( 'NONE', *, *, #121148, .T. ) ;
#221006 = EDGE_CURVE ( 'NONE', #141753, #252297, #152955, .T. ) ;
#221007 = ORIENTED_EDGE ( 'NONE', *, *, #20013, .F. ) ;
#221008 = CARTESIAN_POINT ( 'NONE',  ( 23.14999999999999858, 28.08470566095357057, -239.2860081655328770 ) ) ;
#221009 = CARTESIAN_POINT ( 'NONE',  ( -20.64999999999999858, 2.000000000011154189, -154.2753780772379173 ) ) ;
#221010 = PLANE ( 'NONE',  #194386 ) ;
#221011 = EDGE_CURVE ( 'NONE', #56619, #35302, #219529, .T. ) ;
#221012 = CARTESIAN_POINT ( 'NONE',  ( -20.85000000000000142, 69.15387683765909799, -65.78538121767449809 ) ) ;
#221013 = CARTESIAN_POINT ( 'NONE',  ( 20.22894356738409627, 66.72150177717490749, -195.2545845782749154 ) ) ;
#221014 = ADVANCED_FACE ( 'NONE', ( #132777 ), #212310, .F. ) ;
#221015 = CARTESIAN_POINT ( 'NONE',  ( 20.94999999999999929, 67.23127455305835554, -235.8551265064784559 ) ) ;
#221016 = AXIS2_PLACEMENT_3D ( 'NONE', #47484, #226111, #43658 ) ;
#221017 = VERTEX_POINT ( 'NONE', #158763 ) ;
#221018 = ORIENTED_EDGE ( 'NONE', *, *, #223502, .F. ) ;
#221019 = AXIS2_PLACEMENT_3D ( 'NONE', #218949, #61168, #3762 ) ;
#221020 = EDGE_CURVE ( 'NONE', #47754, #78772, #236297, .T. ) ;
#221021 = CIRCLE ( 'NONE', #208591, 0.1000000000000000472 ) ;
#221022 = ORIENTED_EDGE ( 'NONE', *, *, #1862, .T. ) ;
#221023 = DIRECTION ( 'NONE',  ( 1.000000000000000000, 0.000000000000000000, 0.000000000000000000 ) ) ;
#221025 = EDGE_CURVE ( 'NONE', #244526, #190309, #238261, .T. ) ;
#221024 = CARTESIAN_POINT ( 'NONE',  ( -13.43673303185028800, 66.55335100938270898, -54.43394418860121675 ) ) ;
#221026 = AXIS2_PLACEMENT_3D ( 'NONE', #254586, #120281, #78533 ) ;
#221028 = EDGE_CURVE ( 'NONE', #37949, #18904, #194641, .T. ) ;
#221027 = ADVANCED_FACE ( 'NONE', ( #217406 ), #101269, .F. ) ;
#221029 = DIRECTION ( 'NONE',  ( 0.7071067811865388020, -0.7071067811865561215, 0.000000000000000000 ) ) ;
#221030 = EDGE_LOOP ( 'NONE', ( #82437, #89050, #18171, #223968 ) ) ;
#221031 = LINE ( 'NONE', #64534, #44344 ) ;
#221032 = ORIENTED_EDGE ( 'NONE', *, *, #128591, .T. ) ;
#221033 = EDGE_CURVE ( 'NONE', #96528, #55246, #190346, .T. ) ;
#221034 = CARTESIAN_POINT ( 'NONE',  ( -20.94999999999999929, -10.56629024491939894, -206.4738935375009703 ) ) ;
#221035 = EDGE_LOOP ( 'NONE', ( #626, #146917, #67510, #26370 ) ) ;
#221036 = AXIS2_PLACEMENT_3D ( 'NONE', #138165, #19537, #118648 ) ;
#221037 = DIRECTION ( 'NONE',  ( 0.000000000000000000, -0.8814952561688430555, 0.4721928772777346239 ) ) ;
#221038 = DIRECTION ( 'NONE',  ( -1.000000000000000000, -2.952720810173289112E-16, 0.000000000000000000 ) ) ;
#221039 = VERTEX_POINT ( 'NONE', #178327 ) ;
#221040 = DIRECTION ( 'NONE',  ( 0.000000000000000000, -0.8068669527896844551, -0.5907332058517525963 ) ) ;
#221042 = EDGE_LOOP ( 'NONE', ( #240296, #139894, #130012, #51099 ) ) ;
#221041 = DIRECTION ( 'NONE',  ( 2.940209281316621016E-16, 1.000000000000000000, 9.408669700213187250E-15 ) ) ;
#221043 = EDGE_CURVE ( 'NONE', #148888, #169963, #77885, .T. ) ;
#221044 = LINE ( 'NONE', #204054, #18879 ) ;
#221045 = EDGE_CURVE ( 'NONE', #247963, #222383, #17928, .T. ) ;
#221046 = ORIENTED_EDGE ( 'NONE', *, *, #172170, .F. ) ;
#221047 = EDGE_CURVE ( 'NONE', #124745, #183616, #135303, .T. ) ;
#221048 = CARTESIAN_POINT ( 'NONE',  ( -20.54999999999999716, 16.34561257290783942, -251.9995012668252343 ) ) ;
#221049 = ORIENTED_EDGE ( 'NONE', *, *, #193202, .F. ) ;
#221050 = CYLINDRICAL_SURFACE ( 'NONE', #136876, 0.1000000000000028644 ) ;
#221052 = CARTESIAN_POINT ( 'NONE',  ( 22.49066049874202022, 26.00400106736331196, -254.2626983329210475 ) ) ;
#221051 = VECTOR ( 'NONE', #193680, 1000.000000000000000 ) ;
#221054 = ADVANCED_FACE ( 'NONE', ( #96176 ), #252858, .T. ) ;
#221053 = DIRECTION ( 'NONE',  ( 1.000000000000000000, 0.000000000000000000, -0.000000000000000000 ) ) ;
#221055 = CARTESIAN_POINT ( 'NONE',  ( 21.15000000000005542, 83.98667523412385094, -34.76145429838185663 ) ) ;
#221056 = CARTESIAN_POINT ( 'NONE',  ( -13.12432614554023935, 66.56923500459026855, -188.2925700897739887 ) ) ;
#221057 = ADVANCED_FACE ( 'NONE', ( #100008, #57033 ), #36247, .F. ) ;
#221058 = VECTOR ( 'NONE', #154563, 1000.000000000000000 ) ;
#221059 = ORIENTED_EDGE ( 'NONE', *, *, #143010, .T. ) ;
#221060 = DIRECTION ( 'NONE',  ( 1.000000000000000000, 0.000000000000000000, -0.000000000000000000 ) ) ;
#221061 = DIRECTION ( 'NONE',  ( 0.000000000000000000, 0.000000000000000000, -1.000000000000000000 ) ) ;
#221062 = DIRECTION ( 'NONE',  ( 0.000000000000000000, -0.9915357197604792727, 0.1298341882520475943 ) ) ;
#221063 = EDGE_LOOP ( 'NONE', ( #92519, #180689, #30049, #249222, #11683 ) ) ;
#221064 = CARTESIAN_POINT ( 'NONE',  ( -21.07954763557533084, 75.93412408139347747, -109.3523984745629463 ) ) ;
#221065 = EDGE_LOOP ( 'NONE', ( #232290, #218534, #49148, #61592 ) ) ;
#221066 = DIRECTION ( 'NONE',  ( 0.000000000000000000, -1.000000000000000000, 0.000000000000000000 ) ) ;
#221067 = VERTEX_POINT ( 'NONE', #177042 ) ;
#221068 = DIRECTION ( 'NONE',  ( -2.602085213965226419E-14, -6.982962677686266711E-15, 1.000000000000000000 ) ) ;
#221069 = DIRECTION ( 'NONE',  ( -0.000000000000000000, -0.000000000000000000, -1.000000000000000000 ) ) ;
#221070 = ORIENTED_EDGE ( 'NONE', *, *, #212836, .T. ) ;
#221071 = AXIS2_PLACEMENT_3D ( 'NONE', #217976, #36837, #117620 ) ;
#221073 = ORIENTED_EDGE ( 'NONE', *, *, #252478, .T. ) ;
#221072 = LINE ( 'NONE', #141540, #182254 ) ;
#221074 = ADVANCED_FACE ( 'NONE', ( #219986 ), #236995, .T. ) ;
#221075 = CYLINDRICAL_SURFACE ( 'NONE', #33958, 11.79999999999999716 ) ;
#221076 = ORIENTED_EDGE ( 'NONE', *, *, #211278, .T. ) ;
#221077 = FACE_OUTER_BOUND ( 'NONE', #114903, .T. ) ;
#221078 = DIRECTION ( 'NONE',  ( -1.000000000000000000, -0.000000000000000000, -0.000000000000000000 ) ) ;
#221079 = EDGE_LOOP ( 'NONE', ( #253897, #49338 ) ) ;
#221081 = VERTEX_POINT ( 'NONE', #196570 ) ;
#221080 = EDGE_CURVE ( 'NONE', #248454, #119221, #144526, .T. ) ;
#221082 = CARTESIAN_POINT ( 'NONE',  ( -21.05000000000000071, -1.835341550213255957, -179.0551512925629538 ) ) ;
#221083 = CARTESIAN_POINT ( 'NONE',  ( -18.50000000000000000, 9.250000000000001776, -12.34999999999999964 ) ) ;
#221084 = CARTESIAN_POINT ( 'NONE',  ( 20.04142135623730070, 64.25000000001148237, -44.87310748452440379 ) ) ;
#221085 = CIRCLE ( 'NONE', #75388, 0.1000000000000028644 ) ;
#221086 = AXIS2_PLACEMENT_3D ( 'NONE', #244424, #223561, #241853 ) ;
#221087 = ORIENTED_EDGE ( 'NONE', *, *, #148072, .T. ) ;
#221088 = ORIENTED_EDGE ( 'NONE', *, *, #206597, .F. ) ;
#221089 = CIRCLE ( 'NONE', #100281, 0.1999999999999905742 ) ;
#221090 = DIRECTION ( 'NONE',  ( -1.000000000000000000, 0.000000000000000000, 0.000000000000000000 ) ) ;
#221091 = AXIS2_PLACEMENT_3D ( 'NONE', #155209, #254252, #37823 ) ;
#221092 = EDGE_CURVE ( 'NONE', #150252, #200951, #97445, .T. ) ;
#221093 = AXIS2_PLACEMENT_3D ( 'NONE', #4108, #83607, #44534 ) ;
#221094 = AXIS2_PLACEMENT_3D ( 'NONE', #149507, #64800, #183479 ) ;
#221096 = ORIENTED_EDGE ( 'NONE', *, *, #240229, .F. ) ;
#221095 = DIRECTION ( 'NONE',  ( 1.000000000000000000, 3.265361837132813093E-16, -0.000000000000000000 ) ) ;
#221097 = FACE_OUTER_BOUND ( 'NONE', #110414, .T. ) ;
#221098 = CARTESIAN_POINT ( 'NONE',  ( -22.50000000000000000, 75.90000000001172964, -81.17267829206912211 ) ) ;
#221099 = DIRECTION ( 'NONE',  ( 0.000000000000000000, 0.9126074666063660468, 0.4088369013363524762 ) ) ;
#221101 = LINE ( 'NONE', #239402, #244977 ) ;
#221100 = CARTESIAN_POINT ( 'NONE',  ( -16.94107738177415712, 65.98576071487524075, -90.47310748452437679 ) ) ;
#221102 = DIRECTION ( 'NONE',  ( 1.000000000000000000, -0.000000000000000000, -0.000000000000000000 ) ) ;
#221103 = LINE ( 'NONE', #4619, #231823 ) ;
#221104 = CARTESIAN_POINT ( 'NONE',  ( -16.87368910959167678, 60.91865946774127849, -221.0749760015432344 ) ) ;
#221105 = EDGE_CURVE ( 'NONE', #257159, #155298, #20529, .T. ) ;
#221106 = AXIS2_PLACEMENT_3D ( 'NONE', #26917, #142954, #106397 ) ;
#221107 = CARTESIAN_POINT ( 'NONE',  ( 20.94999999999999929, 4.850467289730776344, -88.46573259099837117 ) ) ;
#221108 = VECTOR ( 'NONE', #92730, 1000.000000000000000 ) ;
#221109 = AXIS2_PLACEMENT_3D ( 'NONE', #148108, #106384, #68574 ) ;
#221110 = AXIS2_PLACEMENT_3D ( 'NONE', #248472, #107668, #71137 ) ;
#221112 = ORIENTED_EDGE ( 'NONE', *, *, #95384, .T. ) ;
#221111 = AXIS2_PLACEMENT_3D ( 'NONE', #228013, #169364, #48083 ) ;
#221113 = VERTEX_POINT ( 'NONE', #255209 ) ;
#221114 = DIRECTION ( 'NONE',  ( 0.000000000000000000, 0.000000000000000000, 1.000000000000000000 ) ) ;
#221115 = ORIENTED_EDGE ( 'NONE', *, *, #254348, .T. ) ;
#221116 = DIRECTION ( 'NONE',  ( -0.000000000000000000, 1.000000000000000000, -0.000000000000000000 ) ) ;
#221117 = CIRCLE ( 'NONE', #137725, 0.09999999999998802902 ) ;
#221118 = ORIENTED_EDGE ( 'NONE', *, *, #117028, .F. ) ;
#221120 = EDGE_LOOP ( 'NONE', ( #172146, #3348, #202394, #151343 ) ) ;
#221119 = VERTEX_POINT ( 'NONE', #76624 ) ;
#221121 = VERTEX_POINT ( 'NONE', #905 ) ;
#221122 = EDGE_LOOP ( 'NONE', ( #71014, #135450, #12397, #107289, #249620, #110115, #29299, #44569, #111422, #23216 ) ) ;
#221123 = DIRECTION ( 'NONE',  ( 0.000000000000000000, -0.2617529984164506107, -0.9651348961777299618 ) ) ;
#221124 = CARTESIAN_POINT ( 'NONE',  ( -21.12757541349819590, 75.99483878420227256, -109.4964880557758704 ) ) ;
#221126 = ORIENTED_EDGE ( 'NONE', *, *, #224797, .T. ) ;
#221125 = DIRECTION ( 'NONE',  ( 0.000000000000000000, 0.000000000000000000, 1.000000000000000000 ) ) ;
#221127 = CARTESIAN_POINT ( 'NONE',  ( 20.51284917709620359, 39.44540980133907482, -237.0045804191218792 ) ) ;
#221128 = CARTESIAN_POINT ( 'NONE',  ( 19.75857864376268935, 11.75000000001116440, -158.7500000000000284 ) ) ;
#221130 = ORIENTED_EDGE ( 'NONE', *, *, #39785, .T. ) ;
#221129 = DIRECTION ( 'NONE',  ( 1.000000000000000000, 0.000000000000000000, 0.000000000000000000 ) ) ;
#221131 = CARTESIAN_POINT ( 'NONE',  ( -21.95218792049438861, 0.09902843981107177507, -59.79849243875336384 ) ) ;
#221133 = ORIENTED_EDGE ( 'NONE', *, *, #138324, .F. ) ;
#221132 = B_SPLINE_CURVE_WITH_KNOTS ( 'NONE', 3,
 ( #137166, #173786, #172497, #253252, #176320, #255788, #72074, #134576 ),
 .UNSPECIFIED., .F., .F.,
 ( 4, 2, 2, 4 ),
 ( 0.000000000000000000, 0.0002181133598169265018, 0.0003271700397253585820, 0.0004362267196337907163 ),
 .UNSPECIFIED. ) ;
#221134 = DIRECTION ( 'NONE',  ( 0.2834754621636358940, -0.2834754621636437211, 0.9161240771326893961 ) ) ;
#221135 = CIRCLE ( 'NONE', #158641, 0.09999999999998898659 ) ;
#221137 = EDGE_LOOP ( 'NONE', ( #256304, #145120, #216927, #212275, #34232, #155817, #101325, #159722, #68983, #109459, #77264, #193219 ) ) ;
#221136 = CARTESIAN_POINT ( 'NONE',  ( -16.94107738177415712, 65.98576071487543970, -123.9731074845243626 ) ) ;
#221138 = CARTESIAN_POINT ( 'NONE',  ( 23.14999999999999503, 64.35000000001258513, -191.3731074845244393 ) ) ;
#221139 = CARTESIAN_POINT ( 'NONE',  ( -15.75000000000000711, 26.40960863751540444, -233.4539077120826960 ) ) ;
#221140 = EDGE_CURVE ( 'NONE', #162728, #199385, #57705, .T. ) ;
#221141 = DIRECTION ( 'NONE',  ( 0.000000000000000000, 3.469446951953614189E-14, 1.000000000000000000 ) ) ;
#221142 = ORIENTED_EDGE ( 'NONE', *, *, #187682, .F. ) ;
#221144 = DIRECTION ( 'NONE',  ( 0.7071067811865475727, -0.7071067811865475727, -4.937700262164531476E-15 ) ) ;
#221143 = DIRECTION ( 'NONE',  ( 1.000000000000000000, 0.000000000000000000, 0.000000000000000000 ) ) ;
#221145 = DIRECTION ( 'NONE',  ( 1.000000000000000000, 0.000000000000000000, 0.000000000000000000 ) ) ;
#221146 = CARTESIAN_POINT ( 'NONE',  ( 18.50000000000000711, 85.42107434499938279, -163.1986354250934710 ) ) ;
#221147 = CARTESIAN_POINT ( 'NONE',  ( 20.85000000000000142, 68.97833521811131163, -32.18954208262707795 ) ) ;
#221148 = CARTESIAN_POINT ( 'NONE',  ( -16.95709691156226384, 44.14466031266160684, -235.2948197039139870 ) ) ;
#221149 = VERTEX_POINT ( 'NONE', #156198 ) ;
#221150 = VERTEX_POINT ( 'NONE', #83009 ) ;
#221151 = ORIENTED_EDGE ( 'NONE', *, *, #114256, .T. ) ;
#221153 = AXIS2_PLACEMENT_3D ( 'NONE', #248457, #28149, #88060 ) ;
#221152 = DIRECTION ( 'NONE',  ( 1.000000000000000000, 0.000000000000000000, 0.000000000000000000 ) ) ;
#221154 = VERTEX_POINT ( 'NONE', #43919 ) ;
#221155 = DIRECTION ( 'NONE',  ( -0.000000000000000000, -0.000000000000000000, -1.000000000000000000 ) ) ;
#221156 = VERTEX_POINT ( 'NONE', #145576 ) ;
#221157 = EDGE_CURVE ( 'NONE', #236966, #81210, #65424, .T. ) ;
#221158 = CARTESIAN_POINT ( 'NONE',  ( -20.64999999999999858, 68.75000000001158185, -57.17310748452437252 ) ) ;
#221159 = DIRECTION ( 'NONE',  ( 1.000000000000000000, -1.186688945009010077E-16, -8.286604613020808509E-31 ) ) ;
#221160 = EDGE_CURVE ( 'NONE', #52893, #105073, #230894, .T. ) ;
#221161 = ORIENTED_EDGE ( 'NONE', *, *, #59936, .F. ) ;
#221162 = DIRECTION ( 'NONE',  ( 0.000000000000000000, 6.938893903907222067E-15, -1.000000000000000000 ) ) ;
#221163 = CIRCLE ( 'NONE', #54583, 11.65000000000001457 ) ;
#221164 = ADVANCED_FACE ( 'NONE', ( #105130 ), #7357, .F. ) ;
#221165 = ORIENTED_EDGE ( 'NONE', *, *, #248812, .T. ) ;
#221166 = ORIENTED_EDGE ( 'NONE', *, *, #28086, .F. ) ;
#221167 = VERTEX_POINT ( 'NONE', #23098 ) ;
#221168 = AXIS2_PLACEMENT_3D ( 'NONE', #129406, #48579, #130684 ) ;
#221169 = ADVANCED_FACE ( 'NONE', ( #84270 ), #19658, .F. ) ;
#221170 = PLANE ( 'NONE',  #171146 ) ;
#221171 = CARTESIAN_POINT ( 'NONE',  ( 22.43288208788031568, 75.99510014512738110, -215.1727593282434441 ) ) ;
#221172 = DIRECTION ( 'NONE',  ( 0.000000000000000000, -6.982962677686266711E-15, 1.000000000000000000 ) ) ;
#221174 = ADVANCED_FACE ( 'NONE', ( #64761 ), #67332, .T. ) ;
#221173 = DIRECTION ( 'NONE',  ( 0.000000000000000000, 2.664535259100315349E-15, -1.000000000000000000 ) ) ;
#221175 = CARTESIAN_POINT ( 'NONE',  ( 18.59999999999999432, 13.66123737402873495, -238.6633470470287648 ) ) ;
#221176 = DIRECTION ( 'NONE',  ( 0.000000000000000000, -1.000000000000000000, -6.982962677686266711E-15 ) ) ;
#221178 = DIRECTION ( 'NONE',  ( 1.000000000000000000, 0.000000000000000000, 0.000000000000000000 ) ) ;
#221177 = CARTESIAN_POINT ( 'NONE',  ( -23.15000000000000213, 85.50000000001159606, -59.62913836187181005 ) ) ;
#221179 = CARTESIAN_POINT ( 'NONE',  ( -14.00000000000000178, 26.54497872210690090, -232.9592037335782209 ) ) ;
#221181 = ORIENTED_EDGE ( 'NONE', *, *, #89165, .F. ) ;
#221180 = DIRECTION ( 'NONE',  ( 0.000000000000000000, 0.1568667991644355497, -0.9876197685951332295 ) ) ;
#221182 = CARTESIAN_POINT ( 'NONE',  ( 21.14999999999999858, 69.45934304831071415, -103.0231074845243597 ) ) ;
#221183 = EDGE_CURVE ( 'NONE', #54887, #210905, #146847, .T. ) ;
#221184 = CARTESIAN_POINT ( 'NONE',  ( 20.46382478191414833, 67.09862044130970560, -161.4773793896413565 ) ) ;
#221185 = ORIENTED_EDGE ( 'NONE', *, *, #124829, .T. ) ;
#221186 = DIRECTION ( 'NONE',  ( -1.000000000000000000, -0.000000000000000000, -0.000000000000000000 ) ) ;
#221187 = DIRECTION ( 'NONE',  ( 0.000000000000000000, 0.2128009952263604510, -0.9770955615653315052 ) ) ;
#221188 = DIRECTION ( 'NONE',  ( -0.000000000000000000, 1.000000000000000000, -0.000000000000000000 ) ) ;
#221189 = ORIENTED_EDGE ( 'NONE', *, *, #123417, .F. ) ;
#221190 = ADVANCED_FACE ( 'NONE', ( #47750 ), #244478, .F. ) ;
#221191 = CIRCLE ( 'NONE', #142083, 0.3999999999999975797 ) ;
#221192 = DIRECTION ( 'NONE',  ( -0.000000000000000000, 1.000000000000000000, 0.000000000000000000 ) ) ;
#221193 = DIRECTION ( 'NONE',  ( 0.000000000000000000, 0.000000000000000000, -1.000000000000000000 ) ) ;
#221194 = EDGE_LOOP ( 'NONE', ( #72521, #117414, #148333, #191243 ) ) ;
#221195 = ORIENTED_EDGE ( 'NONE', *, *, #42703, .T. ) ;
#221196 = CARTESIAN_POINT ( 'NONE',  ( -23.25000000000000000, 2.600000000011156054, -154.2753780772379173 ) ) ;
#221197 = ORIENTED_EDGE ( 'NONE', *, *, #134778, .T. ) ;
#221198 = DIRECTION ( 'NONE',  ( -1.000000000000000000, 0.000000000000000000, 0.000000000000000000 ) ) ;
#221199 = CARTESIAN_POINT ( 'NONE',  ( 20.09999999999999787, 66.25000000001210765, -127.2731074845243597 ) ) ;
#221200 = DIRECTION ( 'NONE',  ( 0.000000000000000000, 0.000000000000000000, 1.000000000000000000 ) ) ;
#221201 = DIRECTION ( 'NONE',  ( -1.000000000000000000, 0.000000000000000000, 0.000000000000000000 ) ) ;
#221202 = ORIENTED_EDGE ( 'NONE', *, *, #187735, .F. ) ;
#221203 = EDGE_CURVE ( 'NONE', #209826, #38549, #232042, .T. ) ;
#221204 = DIRECTION ( 'NONE',  ( -1.000000000000000000, 0.000000000000000000, 0.000000000000000000 ) ) ;
#221205 = AXIS2_PLACEMENT_3D ( 'NONE', #212982, #150462, #151755 ) ;
#221207 = DIRECTION ( 'NONE',  ( 1.000000000000000000, -0.000000000000000000, 0.000000000000000000 ) ) ;
#221206 = CIRCLE ( 'NONE', #8844, 0.5000000000000004441 ) ;
#221208 = AXIS2_PLACEMENT_3D ( 'NONE', #122144, #60867, #62170 ) ;
#221209 = DIRECTION ( 'NONE',  ( 1.000000000000000000, 0.000000000000000000, 0.000000000000000000 ) ) ;
#221210 = FACE_OUTER_BOUND ( 'NONE', #157719, .T. ) ;
#221211 = EDGE_LOOP ( 'NONE', ( #164746, #183552 ) ) ;
#221212 = EDGE_CURVE ( 'NONE', #142560, #104329, #183441, .T. ) ;
#221214 = ORIENTED_EDGE ( 'NONE', *, *, #247314, .T. ) ;
#221213 = DIRECTION ( 'NONE',  ( 3.265361837132813093E-16, 1.000000000000000000, 6.982962677686266711E-15 ) ) ;
#221215 = CARTESIAN_POINT ( 'NONE',  ( -21.04999999999965610, 34.03619476471878613, -243.8226196603530980 ) ) ;
#221216 = DIRECTION ( 'NONE',  ( 0.000000000000000000, -0.000000000000000000, -1.000000000000000000 ) ) ;
#221217 = DIRECTION ( 'NONE',  ( -0.000000000000000000, -1.000000000000000000, 8.673617379884045333E-16 ) ) ;
#221218 = CARTESIAN_POINT ( 'NONE',  ( 21.33487959338958362, 10.30459399514276519, -227.8041537064418947 ) ) ;
#221219 = CARTESIAN_POINT ( 'NONE',  ( -16.88815647973234135, 66.04916738069633197, -123.8758904211983634 ) ) ;
#221220 = CIRCLE ( 'NONE', #17251, 0.09999999999998898659 ) ;
#221221 = ORIENTED_EDGE ( 'NONE', *, *, #16495, .T. ) ;
#221222 = CARTESIAN_POINT ( 'NONE',  ( 21.03675099975491136, 61.89177620496869991, -221.6362106908973431 ) ) ;
#221223 = DIRECTION ( 'NONE',  ( -1.000000000000000000, 0.000000000000000000, 0.000000000000000000 ) ) ;
#221224 = FACE_OUTER_BOUND ( 'NONE', #240197, .T. ) ;
#221225 = DIRECTION ( 'NONE',  ( 0.000000000000000000, 0.9915357197604792727, -0.1298341882520473722 ) ) ;
#221226 = CARTESIAN_POINT ( 'NONE',  ( 22.49999999999999645, 11.36146383068193622, -198.4232501820394816 ) ) ;
#221227 = CARTESIAN_POINT ( 'NONE',  ( -20.00857864376270001, 66.85000000001205933, -124.2731074845243597 ) ) ;
#221228 = ADVANCED_FACE ( 'NONE', ( #182158 ), #198697, .T. ) ;
#221229 = VERTEX_POINT ( 'NONE', #142993 ) ;
#221230 = ORIENTED_EDGE ( 'NONE', *, *, #155188, .T. ) ;
#221231 = DIRECTION ( 'NONE',  ( -0.000000000000000000, 1.000000000000000000, 7.172728831056617961E-15 ) ) ;
#221232 = DIRECTION ( 'NONE',  ( 0.000000000000000000, -6.467318590049456648E-15, 1.000000000000000000 ) ) ;
#221233 = DIRECTION ( 'NONE',  ( 0.000000000000000000, 0.000000000000000000, 1.000000000000000000 ) ) ;
#221234 = CARTESIAN_POINT ( 'NONE',  ( 20.85000000106584750, 17.15319076756267691, -224.5445635972164951 ) ) ;
#221235 = CIRCLE ( 'NONE', #212889, 11.64999999999999325 ) ;
#221236 = ADVANCED_FACE ( 'NONE', ( #184704 ), #127978, .T. ) ;
#221237 = VERTEX_POINT ( 'NONE', #242112 ) ;
#221238 = FACE_OUTER_BOUND ( 'NONE', #202733, .T. ) ;
#221239 = CARTESIAN_POINT ( 'NONE',  ( 21.14999999999999858, 69.35000000001156195, -57.17310748452436542 ) ) ;
#221240 = CIRCLE ( 'NONE', #75538, 0.09999999999998898659 ) ;
#221241 = EDGE_CURVE ( 'NONE', #101254, #31810, #36415, .T. ) ;
#221243 = ADVANCED_FACE ( 'NONE', ( #248536 ), #249828, .T. ) ;
#221242 = DIRECTION ( 'NONE',  ( 0.000000000000000000, 0.000000000000000000, -1.000000000000000000 ) ) ;
#221244 = CARTESIAN_POINT ( 'NONE',  ( 18.59999999999999076, 10.20857864377385127, -188.7499999999999716 ) ) ;
#221245 = ORIENTED_EDGE ( 'NONE', *, *, #160181, .F. ) ;
#221246 = DIRECTION ( 'NONE',  ( -0.000000000000000000, 6.982962677686266711E-15, -1.000000000000000000 ) ) ;
#221247 = EDGE_CURVE ( 'NONE', #192659, #103735, #54180, .T. ) ;
#221248 = AXIS2_PLACEMENT_3D ( 'NONE', #51879, #68922, #48046 ) ;
#221249 = ORIENTED_EDGE ( 'NONE', *, *, #37055, .T. ) ;
#221250 = DIRECTION ( 'NONE',  ( -1.000000000000000000, 1.186688945009010077E-16, 8.286604613020808509E-31 ) ) ;
#221251 = LINE ( 'NONE', #218684, #63150 ) ;
#221252 = CARTESIAN_POINT ( 'NONE',  ( -21.05000000000000071, 10.12484234394027816, -228.1850061131911218 ) ) ;
#221253 = CARTESIAN_POINT ( 'NONE',  ( 18.49999999999999289, 65.70729864260985664, -64.06574559737245522 ) ) ;
#221254 = DIRECTION ( 'NONE',  ( 0.000000000000000000, -0.2818822000686748708, 0.9594490217225944972 ) ) ;
#221255 = FACE_OUTER_BOUND ( 'NONE', #245783, .T. ) ;
#221257 = DIRECTION ( 'NONE',  ( 0.000000000000000000, -0.2617529984165031243, -0.9651348961777157509 ) ) ;
#221256 = AXIS2_PLACEMENT_3D ( 'NONE', #246809, #51156, #86427 ) ;
#221258 = DIRECTION ( 'NONE',  ( 1.000000000000000000, 0.000000000000000000, 0.000000000000000000 ) ) ;
#221259 = DIRECTION ( 'NONE',  ( 0.000000000000000000, -6.982962677686266711E-15, 1.000000000000000000 ) ) ;
#221260 = CARTESIAN_POINT ( 'NONE',  ( 20.85000000000000142, 64.35000000001190301, -103.0231074845243882 ) ) ;
#221261 = FACE_OUTER_BOUND ( 'NONE', #194130, .T. ) ;
#221262 = LINE ( 'NONE', #66051, #52168 ) ;
#221263 = AXIS2_PLACEMENT_3D ( 'NONE', #32468, #92390, #192796 ) ;
#221264 = VECTOR ( 'NONE', #144687, 1000.000000000000000 ) ;
#221265 = DIRECTION ( 'NONE',  ( 0.000000000000000000, 0.4088369013363783999, -0.9126074666063545004 ) ) ;
#221266 = CARTESIAN_POINT ( 'NONE',  ( -18.59999999999999787, 74.83729825007431202, -161.9231074845243654 ) ) ;
#221267 = EDGE_CURVE ( 'NONE', #13290, #222515, #12520, .T. ) ;
#221268 = VERTEX_POINT ( 'NONE', #88145 ) ;
#221269 = AXIS2_PLACEMENT_3D ( 'NONE', #76277, #16339, #95830 ) ;
#221270 = DIRECTION ( 'NONE',  ( 0.000000000000000000, -6.467318590049456648E-15, 1.000000000000000000 ) ) ;
#221271 = LINE ( 'NONE', #183458, #8535 ) ;
#221272 = EDGE_CURVE ( 'NONE', #9660, #213491, #165892, .T. ) ;
#221273 = EDGE_CURVE ( 'NONE', #245627, #83974, #234090, .T. ) ;
#221274 = AXIS2_PLACEMENT_3D ( 'NONE', #130896, #12263, #34398 ) ;
#221275 = ORIENTED_EDGE ( 'NONE', *, *, #138912, .F. ) ;
#221276 = CARTESIAN_POINT ( 'NONE',  ( 21.14999999999999858, 64.35000000001186038, -90.87310748452438247 ) ) ;
#221277 = CARTESIAN_POINT ( 'NONE',  ( -18.37013991200266361, 11.49974761622313579, -191.7930230105170892 ) ) ;
#221278 = VERTEX_POINT ( 'NONE', #29525 ) ;
#221279 = LINE ( 'NONE', #161345, #217100 ) ;
#221280 = CARTESIAN_POINT ( 'NONE',  ( -18.40000000000000213, 65.08943781962308606, -222.1672656287770451 ) ) ;
#221281 = VECTOR ( 'NONE', #62550, 1000.000000000000000 ) ;
#221282 = ORIENTED_EDGE ( 'NONE', *, *, #188386, .F. ) ;
#221283 = MECHANICAL_DESIGN_GEOMETRIC_PRESENTATION_REPRESENTATION (  '', ( #33926 ), #171300 ) ;
#221284 = AXIS2_PLACEMENT_3D ( 'NONE', #80754, #40407, #122486 ) ;
#221285 = VERTEX_POINT ( 'NONE', #150727 ) ;
#221286 = DIRECTION ( 'NONE',  ( -4.408576920032447355E-17, -0.07893460099012300502, 0.9968797965484754720 ) ) ;
#221287 = EDGE_LOOP ( 'NONE', ( #73974, #74857, #380, #119704 ) ) ;
#221288 = CARTESIAN_POINT ( 'NONE',  ( -21.05000000000000071, 76.00000000001237765, -170.0231074845243597 ) ) ;
#221289 = DIRECTION ( 'NONE',  ( 1.000000000000000000, 0.000000000000000000, 0.000000000000000000 ) ) ;
#221290 = CARTESIAN_POINT ( 'NONE',  ( 21.14999999999999503, 76.00000000001195133, -103.0231074845243171 ) ) ;
#221291 = CARTESIAN_POINT ( 'NONE',  ( -18.59999999999999787, -1.162701749938009677, -8.099999999999999645 ) ) ;
#221292 = FACE_OUTER_BOUND ( 'NONE', #189673, .T. ) ;
#221293 = EDGE_CURVE ( 'NONE', #250267, #136073, #140816, .T. ) ;
#221294 = DIRECTION ( 'NONE',  ( 0.000000000000000000, 0.000000000000000000, 1.000000000000000000 ) ) ;
#221295 = DIRECTION ( 'NONE',  ( 1.000000000000000000, 0.000000000000000000, 0.000000000000000000 ) ) ;
#221296 = DIRECTION ( 'NONE',  ( 1.000000000000000000, 0.000000000000000000, 0.000000000000000000 ) ) ;
#221298 = VERTEX_POINT ( 'NONE', #34654 ) ;
#221297 = DIRECTION ( 'NONE',  ( 1.000000000000000000, 0.000000000000000000, 0.000000000000000000 ) ) ;
#221299 = VERTEX_POINT ( 'NONE', #187299 ) ;
#221301 = FACE_OUTER_BOUND ( 'NONE', #150299, .T. ) ;
#221300 = CARTESIAN_POINT ( 'NONE',  ( 20.85000000000000142, 11.75000000001115907, -160.7161343370219129 ) ) ;
#221303 = ORIENTED_EDGE ( 'NONE', *, *, #257436, .T. ) ;
#221302 = CARTESIAN_POINT ( 'NONE',  ( 23.14999999999999858, 67.23127455305835554, -235.8551265064784559 ) ) ;
#221304 = ADVANCED_FACE ( 'NONE', ( #128597 ), #112883, .T. ) ;
#221305 = ORIENTED_EDGE ( 'NONE', *, *, #96776, .F. ) ;
#221306 = CARTESIAN_POINT ( 'NONE',  ( 18.59999999999999076, 6.400000000011158541, -43.43042463006157305 ) ) ;
#221307 = CARTESIAN_POINT ( 'NONE',  ( 20.41140022480670879, 10.41043084241175087, -175.1150013036360349 ) ) ;
#221308 = CARTESIAN_POINT ( 'NONE',  ( 22.39999999999999503, 0.1000000000111554016, -25.70922040162662014 ) ) ;
#221309 = FACE_OUTER_BOUND ( 'NONE', #180687, .T. ) ;
#221310 = ADVANCED_FACE ( 'NONE', ( #110309 ), #103188, .T. ) ;
#221311 = PLANE ( 'NONE',  #168624 ) ;
#221312 = CARTESIAN_POINT ( 'NONE',  ( -18.40000000000000213, 11.41458325961095177, -87.85000000000003695 ) ) ;
#221313 = CIRCLE ( 'NONE', #129750, 0.1000000000000000472 ) ;
#221314 = ADVANCED_FACE ( 'NONE', ( #52898 ), #171605, .F. ) ;
#221315 = DIRECTION ( 'NONE',  ( 0.000000000000000000, 0.000000000000000000, -1.000000000000000000 ) ) ;
#221316 = ORIENTED_EDGE ( 'NONE', *, *, #154609, .F. ) ;
#221317 = ORIENTED_EDGE ( 'NONE', *, *, #104446, .F. ) ;
#221318 = EDGE_CURVE ( 'NONE', #213795, #61667, #69915, .T. ) ;
#221319 = DIRECTION ( 'NONE',  ( 0.000000000000000000, 0.000000000000000000, 1.000000000000000000 ) ) ;
#221320 = EDGE_LOOP ( 'NONE', ( #4679, #304, #1322, #254909 ) ) ;
#221321 = DIRECTION ( 'NONE',  ( 1.000000000000000000, 0.000000000000000000, 0.000000000000000000 ) ) ;
#221322 = EDGE_LOOP ( 'NONE', ( #49563, #76089, #81889, #142799, #255750 ) ) ;
#221323 = CARTESIAN_POINT ( 'NONE',  ( 23.14999999999999147, 7.128833340093095217, -233.7327013124392749 ) ) ;
#221324 = EDGE_CURVE ( 'NONE', #218733, #162124, #253041, .T. ) ;
#221325 = AXIS2_PLACEMENT_3D ( 'NONE', #123073, #22706, #40986 ) ;
#221326 = EDGE_CURVE ( 'NONE', #59416, #248967, #248977, .T. ) ;
#221327 = CARTESIAN_POINT ( 'NONE',  ( -13.77083647240106679, 49.67554723225254776, -233.3568105763834524 ) ) ;
#221328 = FACE_OUTER_BOUND ( 'NONE', #141248, .T. ) ;
#221329 = DIRECTION ( 'NONE',  ( -0.8660254037844653530, 0.000000000000000000, 0.4999999999999539257 ) ) ;
#221330 = EDGE_LOOP ( 'NONE', ( #228788, #112565, #222998, #121793 ) ) ;
#221331 = FACE_OUTER_BOUND ( 'NONE', #55791, .T. ) ;
#221332 = ORIENTED_EDGE ( 'NONE', *, *, #30763, .F. ) ;
#221333 = DIRECTION ( 'NONE',  ( 0.000000000000000000, 0.000000000000000000, 1.000000000000000000 ) ) ;
#221334 = FACE_OUTER_BOUND ( 'NONE', #104391, .T. ) ;
#221335 = DIRECTION ( 'NONE',  ( 0.000000000000000000, -0.8777080977375715243, 0.4791956752370512551 ) ) ;
#221336 = FACE_OUTER_BOUND ( 'NONE', #197876, .T. ) ;
#221337 = ORIENTED_EDGE ( 'NONE', *, *, #92670, .T. ) ;
#221339 = CARTESIAN_POINT ( 'NONE',  ( -21.05000000000000071, 64.35000000001190301, -96.23924182154622997 ) ) ;
#221338 = AXIS2_PLACEMENT_3D ( 'NONE', #67914, #189150, #247837 ) ;
#221340 = ORIENTED_EDGE ( 'NONE', *, *, #91274, .F. ) ;
#221343 = ORIENTED_EDGE ( 'NONE', *, *, #152912, .T. ) ;
#221342 = CARTESIAN_POINT ( 'NONE',  ( 18.49999999999999645, 70.05000000001213323, -126.2174051794894893 ) ) ;
#221341 = LINE ( 'NONE', #177136, #124188 ) ;
#221344 = AXIS2_PLACEMENT_3D ( 'NONE', #86426, #103431, #223384 ) ;
#221345 = EDGE_CURVE ( 'NONE', #176003, #204625, #131154, .T. ) ;
#221346 = CARTESIAN_POINT ( 'NONE',  ( -21.05000000000000071, 1.750000000011155743, -45.16951155790164307 ) ) ;
#221347 = EDGE_CURVE ( 'NONE', #154466, #160229, #244662, .T. ) ;
#221348 = EDGE_LOOP ( 'NONE', ( #220301, #66821, #26470, #87464 ) ) ;
#221349 = VECTOR ( 'NONE', #63815, 1000.000000000000227 ) ;
#221350 = LINE ( 'NONE', #244771, #33637 ) ;
#221351 = ORIENTED_EDGE ( 'NONE', *, *, #226665, .F. ) ;
#221352 = CARTESIAN_POINT ( 'NONE',  ( 20.99999999999999645, 30.11188998467138234, -234.9833440560338147 ) ) ;
#221353 = FACE_OUTER_BOUND ( 'NONE', #32841, .T. ) ;
#221355 = VERTEX_POINT ( 'NONE', #38486 ) ;
#221354 = CARTESIAN_POINT ( 'NONE',  ( -18.60000000000000497, 9.036460724854876503, -245.3776971525634565 ) ) ;
#221356 = LINE ( 'NONE', #243506, #139261 ) ;
#221357 = EDGE_CURVE ( 'NONE', #203889, #162457, #97124, .T. ) ;
#221358 = CIRCLE ( 'NONE', #204804, 12.87500000000000000 ) ;
#221359 = ORIENTED_EDGE ( 'NONE', *, *, #63254, .T. ) ;
#221361 = EDGE_CURVE ( 'NONE', #110160, #214060, #118014, .T. ) ;
#221360 = DIRECTION ( 'NONE',  ( -0.000000000000000000, 1.000000000000000000, 6.982962677686267499E-15 ) ) ;
#221362 = DIRECTION ( 'NONE',  ( 0.000000000000000000, -0.2617529984165031243, -0.9651348961777157509 ) ) ;
#221363 = DIRECTION ( 'NONE',  ( -2.952720810173289112E-16, -0.4088369013363280513, 0.9126074666063769270 ) ) ;
#221364 = ORIENTED_EDGE ( 'NONE', *, *, #80276, .F. ) ;
#221365 = DIRECTION ( 'NONE',  ( -1.000000000000000000, -2.952720810173289112E-16, 0.000000000000000000 ) ) ;
#221366 = EDGE_LOOP ( 'NONE', ( #185014, #95433, #231685, #212218 ) ) ;
#221367 = DIRECTION ( 'NONE',  ( -1.000000000000000000, -0.000000000000000000, -0.000000000000000000 ) ) ;
#221368 = DIRECTION ( 'NONE',  ( -1.284434275755705789E-16, 0.7071067811865472397, 0.7071067811865479058 ) ) ;
#221369 = CYLINDRICAL_SURFACE ( 'NONE', #56012, 0.09999999999998898659 ) ;
#221371 = ORIENTED_EDGE ( 'NONE', *, *, #56023, .F. ) ;
#221370 = CARTESIAN_POINT ( 'NONE',  ( -16.90257928357874562, 9.954106821116520010, -146.6362854301137020 ) ) ;
#221372 = EDGE_CURVE ( 'NONE', #20245, #39697, #16372, .T. ) ;
#221373 = DIRECTION ( 'NONE',  ( 1.000000000000000000, 2.952720810173289112E-16, -0.000000000000000000 ) ) ;
#221374 = VECTOR ( 'NONE', #8069, 1000.000000000000000 ) ;
#221375 = AXIS2_PLACEMENT_3D ( 'NONE', #10806, #89041, #30383 ) ;
#221376 = DIRECTION ( 'NONE',  ( 0.000000000000000000, 0.000000000000000000, -1.000000000000000000 ) ) ;
#221377 = EDGE_LOOP ( 'NONE', ( #167883, #201821, #124680, #191645, #251904, #234758, #156370, #20702, #75609, #149402, #44704, #171216 ) ) ;
#221378 = AXIS2_PLACEMENT_3D ( 'NONE', #111265, #189524, #228660 ) ;
#221379 = ADVANCED_FACE ( 'NONE', ( #59282 ), #157172, .T. ) ;
#221380 = DIRECTION ( 'NONE',  ( 0.000000000000000000, -1.000000000000000000, 6.308085367188393199E-16 ) ) ;
#221381 = DIRECTION ( 'NONE',  ( 1.000000000000000000, 0.000000000000000000, -0.000000000000000000 ) ) ;
#221382 = ORIENTED_EDGE ( 'NONE', *, *, #176846, .F. ) ;
#221383 = CARTESIAN_POINT ( 'NONE',  ( 22.59999999999999432, 64.25043287652299284, -170.1239658536231616 ) ) ;
#221384 = ORIENTED_EDGE ( 'NONE', *, *, #154477, .F. ) ;
#221385 = CARTESIAN_POINT ( 'NONE',  ( 18.59999999999999787, 77.83534155023627932, -91.36795619196132634 ) ) ;
#221386 = ORIENTED_EDGE ( 'NONE', *, *, #34571, .T. ) ;
#221388 = ORIENTED_EDGE ( 'NONE', *, *, #171763, .T. ) ;
#221387 = CARTESIAN_POINT ( 'NONE',  ( -23.25000000000000000, 69.01799029515568407, -132.8269553662681233 ) ) ;
#221389 = ADVANCED_FACE ( 'NONE', ( #158459 ), #179304, .F. ) ;
#221390 = AXIS2_PLACEMENT_3D ( 'NONE', #243079, #125701, #205223 ) ;
#221393 = ORIENTED_EDGE ( 'NONE', *, *, #174157, .F. ) ;
#221392 = ORIENTED_EDGE ( 'NONE', *, *, #171039, .T. ) ;
#221391 = CARTESIAN_POINT ( 'NONE',  ( 21.05000000000000071, 1.115600667400684642E-11, -167.5000000000000284 ) ) ;
#221394 = DIRECTION ( 'NONE',  ( 0.000000000000000000, 0.9126074666063660468, 0.4088369013363524762 ) ) ;
#221395 = CARTESIAN_POINT ( 'NONE',  ( 17.74533788810830615, 10.81849979148195118, -110.8136226749475952 ) ) ;
#221397 = CARTESIAN_POINT ( 'NONE',  ( -16.85718274719399545, 9.976142314621760931, -20.93665366781759474 ) ) ;
#221396 = DIRECTION ( 'NONE',  ( 0.000000000000000000, -6.853228547068871147E-15, 1.000000000000000000 ) ) ;
#221398 = LINE ( 'NONE', #158910, #78429 ) ;
#221399 = DIRECTION ( 'NONE',  ( -1.000000000000000000, -7.304098846218164250E-16, 4.217023435051628197E-16 ) ) ;
#221400 = DIRECTION ( 'NONE',  ( 0.000000000000000000, -1.000000000000000000, -6.982962677686265922E-15 ) ) ;
#221402 = CARTESIAN_POINT ( 'NONE',  ( -20.64999999999999858, 76.00000000001185185, -90.04810748452430857 ) ) ;
#221401 = CARTESIAN_POINT ( 'NONE',  ( 18.39999999999999858, -9.599999999988845900, -207.6001893912220169 ) ) ;
#221403 = ORIENTED_EDGE ( 'NONE', *, *, #31623, .F. ) ;
#221404 = ORIENTED_EDGE ( 'NONE', *, *, #21809, .F. ) ;
#221405 = DIRECTION ( 'NONE',  ( 0.000000000000000000, 0.000000000000000000, -1.000000000000000000 ) ) ;
#221407 = VERTEX_POINT ( 'NONE', #78867 ) ;
#221406 = DIRECTION ( 'NONE',  ( -1.000000000000000000, -1.394253735153569469E-16, -2.602809386958778209E-16 ) ) ;
#221408 = ORIENTED_EDGE ( 'NONE', *, *, #194371, .F. ) ;
#221410 = CARTESIAN_POINT ( 'NONE',  ( -22.47007471830798409, 7.720710651926475876, 8.715969027246751475E-16 ) ) ;
#221409 = AXIS2_PLACEMENT_3D ( 'NONE', #208903, #36723, #159225 ) ;
#221411 = VERTEX_POINT ( 'NONE', #115440 ) ;
#221412 = CARTESIAN_POINT ( 'NONE',  ( -18.59999999999999787, 10.33248238083634440, -106.0948465439131922 ) ) ;
#221413 = AXIS2_PLACEMENT_3D ( 'NONE', #28823, #105706, #185283 ) ;
#221414 = ORIENTED_EDGE ( 'NONE', *, *, #36878, .F. ) ;
#221416 = VECTOR ( 'NONE', #130482, 1000.000000000000000 ) ;
#221415 = DIRECTION ( 'NONE',  ( 0.000000000000000000, 0.000000000000000000, -1.000000000000000000 ) ) ;
#221417 = CARTESIAN_POINT ( 'NONE',  ( -18.58735405345342784, -9.566478620325446158, -174.3227146462660357 ) ) ;
#221419 = ORIENTED_EDGE ( 'NONE', *, *, #208392, .F. ) ;
#221418 = EDGE_LOOP ( 'NONE', ( #11697, #72989, #81905, #188079 ) ) ;
#221420 = ORIENTED_EDGE ( 'NONE', *, *, #230058, .T. ) ;
#221422 = DIRECTION ( 'NONE',  ( 0.000000000000000000, -0.8660254037844459241, -0.4999999999999873990 ) ) ;
#221421 = AXIS2_PLACEMENT_3D ( 'NONE', #125342, #67928, #44526 ) ;
#221423 = ORIENTED_EDGE ( 'NONE', *, *, #42712, .F. ) ;
#221424 = ORIENTED_EDGE ( 'NONE', *, *, #37561, .T. ) ;
#221425 = CARTESIAN_POINT ( 'NONE',  ( -21.05000000000000071, -4.756823075239758225, -233.1486023682345490 ) ) ;
#221426 = VECTOR ( 'NONE', #255174, 1000.000000000000000 ) ;
#221428 = ORIENTED_EDGE ( 'NONE', *, *, #139690, .T. ) ;
#221427 = DIRECTION ( 'NONE',  ( 1.000000000000000000, -1.335000415235278971E-16, 2.979993593738921214E-16 ) ) ;
#221430 = CARTESIAN_POINT ( 'NONE',  ( -21.14999999999999858, 1.115600667400684642E-11, -127.4593430482987912 ) ) ;
#221429 = CARTESIAN_POINT ( 'NONE',  ( 23.14999999999999503, 64.35000000001204512, -124.2731074845243739 ) ) ;
#221431 = CARTESIAN_POINT ( 'NONE',  ( 21.12230431290520372, 0.005209851700162637655, -60.54243334670702836 ) ) ;
#221433 = DIRECTION ( 'NONE',  ( 2.659396599871503635E-15, 0.6132151058540549204, -0.7899159663865520375 ) ) ;
#221432 = B_SPLINE_CURVE_WITH_KNOTS ( 'NONE', 3,
 ( #35817, #95745, #76190, #155775, #38368, #59166, #193591, #218260, #34536, #117890 ),
 .UNSPECIFIED., .F., .F.,
 ( 4, 2, 2, 2, 4 ),
 ( 0.000000000000000000, 0.0001584437871625069168, 0.0002376656807437669617, 0.0002772766275343895438, 0.0003168875743250120988 ),
 .UNSPECIFIED. ) ;
#221434 = ORIENTED_EDGE ( 'NONE', *, *, #84728, .T. ) ;
#221435 = AXIS2_PLACEMENT_3D ( 'NONE', #104093, #147079, #162832 ) ;
#221436 = ORIENTED_EDGE ( 'NONE', *, *, #132131, .F. ) ;
#221437 = AXIS2_PLACEMENT_3D ( 'NONE', #149074, #108641, #245593 ) ;
#221438 = DIRECTION ( 'NONE',  ( -1.000000000000000000, 0.000000000000000000, 0.000000000000000000 ) ) ;
#221439 = PLANE ( 'NONE',  #228782 ) ;
#221440 = EDGE_CURVE ( 'NONE', #57391, #84649, #99709, .T. ) ;
#221442 = ORIENTED_EDGE ( 'NONE', *, *, #185782, .T. ) ;
#221441 = AXIS2_PLACEMENT_3D ( 'NONE', #37579, #195378, #256548 ) ;
#221443 = DIRECTION ( 'NONE',  ( 1.000000000000000000, 0.000000000000000000, 0.000000000000000000 ) ) ;
#221444 = DIRECTION ( 'NONE',  ( -1.000000000000000000, 0.000000000000000000, 0.000000000000000000 ) ) ;
#221445 = CARTESIAN_POINT ( 'NONE',  ( -15.75000000000000355, 12.70026017068886937, -215.3766613508543628 ) ) ;
#221446 = EDGE_LOOP ( 'NONE', ( #101502, #200752, #211718, #156086 ) ) ;
#221447 = ORIENTED_EDGE ( 'NONE', *, *, #25651, .F. ) ;
#221448 = VECTOR ( 'NONE', #236951, 1000.000000000000000 ) ;
#221449 = CARTESIAN_POINT ( 'NONE',  ( -20.54999999999999716, 2.000000000011154189, -180.2246219227620543 ) ) ;
#221450 = CARTESIAN_POINT ( 'NONE',  ( 23.14999999999999503, 8.980461154494404852, -187.0187154576991304 ) ) ;
#221451 = ORIENTED_EDGE ( 'NONE', *, *, #128981, .F. ) ;
#221452 = DIRECTION ( 'NONE',  ( 0.000000000000000000, 0.1350103645451876666, -0.9908441862701600211 ) ) ;
#221453 = ORIENTED_EDGE ( 'NONE', *, *, #166573, .T. ) ;
#221454 = DIRECTION ( 'NONE',  ( 1.000000000000000000, 0.000000000000000000, 0.000000000000000000 ) ) ;
#221456 = AXIS2_PLACEMENT_3D ( 'NONE', #43368, #163316, #147595 ) ;
#221455 = DIRECTION ( 'NONE',  ( -1.000000000000000000, 0.000000000000000000, -3.469446951953635015E-14 ) ) ;
#221458 = CARTESIAN_POINT ( 'NONE',  ( 18.59999999999999787, -1.362429037182151470, -208.8888812479211765 ) ) ;
#221457 = DIRECTION ( 'NONE',  ( 0.000000000000000000, 0.4721928772777346239, 0.8814952561688430555 ) ) ;
#221459 = EDGE_CURVE ( 'NONE', #205761, #195708, #124073, .T. ) ;
#221460 = LINE ( 'NONE', #63687, #11608 ) ;
#221461 = DIRECTION ( 'NONE',  ( 0.000000000000000000, 0.000000000000000000, -1.000000000000000000 ) ) ;
#221462 = ORIENTED_EDGE ( 'NONE', *, *, #219299, .T. ) ;
#221463 = CARTESIAN_POINT ( 'NONE',  ( -18.39999999999999858, 85.68240343348806221, -62.86626410711144786 ) ) ;
#221464 = AXIS2_PLACEMENT_3D ( 'NONE', #164878, #67060, #51311 ) ;
#221465 = VECTOR ( 'NONE', #114459, 1000.000000000000000 ) ;
#221466 = CIRCLE ( 'NONE', #121739, 11.65000000000000036 ) ;
#221468 = ORIENTED_EDGE ( 'NONE', *, *, #207785, .F. ) ;
#221467 = EDGE_LOOP ( 'NONE', ( #105781, #189951, #15690, #35550, #88613 ) ) ;
#221470 = VERTEX_POINT ( 'NONE', #217092 ) ;
#221469 = CIRCLE ( 'NONE', #183896, 0.09999999999999939493 ) ;
#221471 = ORIENTED_EDGE ( 'NONE', *, *, #155063, .F. ) ;
#221472 = ADVANCED_FACE ( 'NONE', ( #178013 ), #119309, .F. ) ;
#221473 = CARTESIAN_POINT ( 'NONE',  ( 18.59999999999999076, 18.18127959618848166, -237.5711165786817389 ) ) ;
#221474 = DIRECTION ( 'NONE',  ( 1.000000000000000000, 0.000000000000000000, 0.000000000000000000 ) ) ;
#221475 = DIRECTION ( 'NONE',  ( 0.000000000000000000, 0.1575844902526876978, 0.9875055080513731598 ) ) ;
#221477 = EDGE_CURVE ( 'NONE', #225728, #20618, #256173, .T. ) ;
#221476 = CARTESIAN_POINT ( 'NONE',  ( -18.40000000000000213, 11.75000000001113953, -188.3499999999999659 ) ) ;
#221478 = FACE_OUTER_BOUND ( 'NONE', #252444, .T. ) ;
#221479 =( BOUNDED_CURVE ( )  B_SPLINE_CURVE ( 3, ( #70048, #50431, #110427, #189975 ),
 .UNSPECIFIED., .F., .F. ) 
 B_SPLINE_CURVE_WITH_KNOTS ( ( 4, 4 ),
 ( 3.141592653589793116, 4.712388980384689674 ),
 .UNSPECIFIED. ) 
 CURVE ( )  GEOMETRIC_REPRESENTATION_ITEM ( )  RATIONAL_B_SPLINE_CURVE ( ( 1.000000000000000000, 0.8047378541243649375, 0.8047378541243649375, 1.000000000000000000 ) ) 
 REPRESENTATION_ITEM ( '' )  );
#221481 = FACE_OUTER_BOUND ( 'NONE', #196271, .T. ) ;
#221480 = CARTESIAN_POINT ( 'NONE',  ( -18.40000000000000213, 11.41458325961093756, -113.1500000000000483 ) ) ;
#221483 = ORIENTED_EDGE ( 'NONE', *, *, #148958, .F. ) ;
#221482 = CARTESIAN_POINT ( 'NONE',  ( -21.64999999999999858, 65.95000000001225260, -149.1731074845244223 ) ) ;
#221484 = DIRECTION ( 'NONE',  ( 0.000000000000000000, 0.000000000000000000, 1.000000000000000000 ) ) ;
#221485 = ORIENTED_EDGE ( 'NONE', *, *, #79965, .F. ) ;
#221486 = EDGE_CURVE ( 'NONE', #173183, #167224, #155888, .T. ) ;
#221487 = FACE_OUTER_BOUND ( 'NONE', #9615, .T. ) ;
#221488 = ORIENTED_EDGE ( 'NONE', *, *, #117959, .F. ) ;
#221489 = ORIENTED_EDGE ( 'NONE', *, *, #163986, .F. ) ;
#221490 = CARTESIAN_POINT ( 'NONE',  ( 21.05000000000000071, 5.000000000011153745, -155.0947339810869323 ) ) ;
#221491 = CARTESIAN_POINT ( 'NONE',  ( 20.94999999999999574, 74.75000000001207923, -128.5231074845243029 ) ) ;
#221492 = LINE ( 'NONE', #85814, #79464 ) ;
#221493 = CYLINDRICAL_SURFACE ( 'NONE', #83317, 0.09999999999999939493 ) ;
#221494 = EDGE_CURVE ( 'NONE', #146108, #151096, #197545, .T. ) ;
#221495 = VECTOR ( 'NONE', #202257, 1000.000000000000000 ) ;
#221496 = CARTESIAN_POINT ( 'NONE',  ( 23.24999999999999289, 11.75000000001116263, -112.6500000000000341 ) ) ;
#221497 = EDGE_LOOP ( 'NONE', ( #240899, #66558, #235849, #182696 ) ) ;
#221499 = VERTEX_POINT ( 'NONE', #236666 ) ;
#221498 = EDGE_CURVE ( 'NONE', #155708, #204919, #257098, .T. ) ;
#221500 =( BOUNDED_CURVE ( )  B_SPLINE_CURVE ( 3, ( #45167, #225067, #8619, #67300 ),
 .UNSPECIFIED., .F., .F. ) 
 B_SPLINE_CURVE_WITH_KNOTS ( ( 4, 4 ),
 ( 3.141592653589791784, 4.712388980384688786 ),
 .UNSPECIFIED. ) 
 CURVE ( )  GEOMETRIC_REPRESENTATION_ITEM ( )  RATIONAL_B_SPLINE_CURVE ( ( 1.000000000000000000, 0.8047378541243649375, 0.8047378541243649375, 1.000000000000000000 ) ) 
 REPRESENTATION_ITEM ( '' )  );
#221501 = CARTESIAN_POINT ( 'NONE',  ( -18.59999999999999787, -8.150000000000005684, 10.52591260281975138 ) ) ;
#221502 = ORIENTED_EDGE ( 'NONE', *, *, #225726, .F. ) ;
#221503 = DIRECTION ( 'NONE',  ( 0.000000000000000000, 1.000000000000000000, 6.352154140967427193E-15 ) ) ;
#221504 = CARTESIAN_POINT ( 'NONE',  ( 21.05000000000000071, 67.22371710471909978, -57.37310748452438247 ) ) ;
#221505 = LINE ( 'NONE', #182420, #66911 ) ;
#221506 = CARTESIAN_POINT ( 'NONE',  ( -23.15000000000000213, 6.396492353704923417, -220.9716372748161746 ) ) ;
#221507 = CARTESIAN_POINT ( 'NONE',  ( 21.22070241538126467, 0.09891903054618129965, -60.53005372713042220 ) ) ;
#221508 = LINE ( 'NONE', #65018, #146112 ) ;
#221509 = DIRECTION ( 'NONE',  ( 0.000000000000000000, 0.000000000000000000, 1.000000000000000000 ) ) ;
#221510 = CARTESIAN_POINT ( 'NONE',  ( -20.65000000000000568, 5.650000000011139001, -87.85000000000003695 ) ) ;
#221511 = ADVANCED_FACE ( 'NONE', ( #56719 ), #186436, .F. ) ;
#221512 = CARTESIAN_POINT ( 'NONE',  ( 18.59999999999999076, 65.50857864377520912, -178.7731074845244166 ) ) ;
#221513 = CARTESIAN_POINT ( 'NONE',  ( -22.49533356619863866, 11.65000000631534149, -133.9348774196772354 ) ) ;
#221514 = DIRECTION ( 'NONE',  ( 7.304098846218132695E-16, -0.4721928772777346794, -0.8814952561688431665 ) ) ;
#221515 =( BOUNDED_SURFACE ( )  B_SPLINE_SURFACE ( 3, 2, ( 
 ( #79190, #212328, #175766 ),
 ( #115771, #154929, #156210 ),
 ( #114487, #235705, #137876 ),
 ( #57048, #158776, #117059 ),
 ( #118350, #98731, #214865 ),
 ( #256497, #33717, #252699 ) ),
 .UNSPECIFIED., .F., .F., .F. ) 
 B_SPLINE_SURFACE_WITH_KNOTS ( ( 4, 2, 4 ),
 ( 3, 3 ),
 ( 0.0001342700090130156216, 0.0002909192928057487745, 0.0004475685765984819273 ),
 ( 0.000000000000000000, 1.000000000000000000 ),
 .UNSPECIFIED. ) 
 GEOMETRIC_REPRESENTATION_ITEM ( )  RATIONAL_B_SPLINE_SURFACE ( (
 ( 1.000000000000000000, 0.7250110520819876836, 1.000000000000000000),
 ( 1.000000000000000000, 0.7257599279134827608, 1.000000000000000000),
 ( 1.000000000000000000, 0.7137594617283012921, 1.000000000000000000),
 ( 1.000000000000000000, 0.6959270178810966767, 1.000000000000000000),
 ( 1.000000000000000000, 0.6919879549338106006, 1.000000000000000000),
 ( 1.000000000000000000, 0.7071067811865475727, 1.000000000000000000) ) ) 
 REPRESENTATION_ITEM ( '' )  SURFACE ( )  );
#221516 = ORIENTED_EDGE ( 'NONE', *, *, #172205, .F. ) ;
#221517 = DIRECTION ( 'NONE',  ( 0.000000000000000000, 0.000000000000000000, 1.000000000000000000 ) ) ;
#221518 = ORIENTED_EDGE ( 'NONE', *, *, #257505, .T. ) ;
#221519 = DIRECTION ( 'NONE',  ( 0.000000000000000000, 0.9999176327611370985, -0.01283462868041286391 ) ) ;
#221520 = CARTESIAN_POINT ( 'NONE',  ( -20.94999999999999929, 76.00000000001162448, -66.62310748452433984 ) ) ;
#221521 = DIRECTION ( 'NONE',  ( 0.000000000000000000, -8.232585987686539041E-15, 1.000000000000000000 ) ) ;
#221522 = VERTEX_POINT ( 'NONE', #37215 ) ;
#221523 = DIRECTION ( 'NONE',  ( 0.000000000000000000, 0.000000000000000000, 1.000000000000000000 ) ) ;
#221524 = FACE_BOUND ( 'NONE', #227132, .T. ) ;
#221525 = CARTESIAN_POINT ( 'NONE',  ( -23.25000000000000000, 6.396492353704923417, -220.9716372748161746 ) ) ;
#221526 = DIRECTION ( 'NONE',  ( -1.000000000000000000, 0.000000000000000000, 0.000000000000000000 ) ) ;
#221527 = DIRECTION ( 'NONE',  ( -1.000000000000000000, -0.000000000000000000, -0.000000000000000000 ) ) ;
#221528 = EDGE_CURVE ( 'NONE', #252116, #19033, #74030, .T. ) ;
#221529 = EDGE_CURVE ( 'NONE', #58261, #219055, #228127, .T. ) ;
#221530 = VERTEX_POINT ( 'NONE', #114159 ) ;
#221531 = DIRECTION ( 'NONE',  ( 1.000000000000000000, 0.000000000000000000, 0.000000000000000000 ) ) ;
#221533 = ORIENTED_EDGE ( 'NONE', *, *, #171165, .F. ) ;
#221532 = CARTESIAN_POINT ( 'NONE',  ( 21.30000000000002558, 1.115600667400684642E-11, -167.4999999999999716 ) ) ;
#221534 = DIRECTION ( 'NONE',  ( 1.000000000000000000, 0.000000000000000000, 0.000000000000000000 ) ) ;
#221535 = CARTESIAN_POINT ( 'NONE',  ( 21.14999999999999858, 11.65000000001115943, -67.10000000000005116 ) ) ;
#221537 = EDGE_CURVE ( 'NONE', #12734, #67154, #15759, .T. ) ;
#221536 = CARTESIAN_POINT ( 'NONE',  ( -23.15000000000000213, 42.98415524044398950, -233.9519173640447889 ) ) ;
#221538 = ADVANCED_FACE ( 'NONE', ( #244374 ), #146547, .T. ) ;
#221539 = VERTEX_POINT ( 'NONE', #200130 ) ;
#221540 = DIRECTION ( 'NONE',  ( 1.000000000000000000, 0.000000000000000000, 0.000000000000000000 ) ) ;
#221541 = CYLINDRICAL_SURFACE ( 'NONE', #233958, 4.000000000000003553 ) ;
#221542 = CIRCLE ( 'NONE', #109118, 14.30833333333333535 ) ;
#221543 = ADVANCED_FACE ( 'NONE', ( #102269 ), #65750, .T. ) ;
#221544 = ORIENTED_EDGE ( 'NONE', *, *, #28260, .T. ) ;
#221545 = DIRECTION ( 'NONE',  ( -1.000000000000000000, 0.000000000000000000, 0.000000000000000000 ) ) ;
#221546 = CARTESIAN_POINT ( 'NONE',  ( 21.05000000000000071, 65.27628289530463235, -136.5231074845243597 ) ) ;
#221547 = ADVANCED_FACE ( 'NONE', ( #201400 ), #104834, .T. ) ;
#221548 = EDGE_CURVE ( 'NONE', #34583, #254300, #125719, .T. ) ;
#221549 = EDGE_LOOP ( 'NONE', ( #51943, #204950, #218945, #138528 ) ) ;
#221550 = EDGE_CURVE ( 'NONE', #41396, #140330, #136507, .T. ) ;
#221551 = VERTEX_POINT ( 'NONE', #205242 ) ;
#221552 = CARTESIAN_POINT ( 'NONE',  ( 21.05000000000000071, 10.42338541492405390, -74.49205192387015018 ) ) ;
#221553 = FACE_OUTER_BOUND ( 'NONE', #98819, .T. ) ;
#221554 = DIRECTION ( 'NONE',  ( 0.000000000000000000, 0.000000000000000000, -1.000000000000000000 ) ) ;
#221555 = CARTESIAN_POINT ( 'NONE',  ( 21.14999999999999503, 1.115600667400684642E-11, -67.00000000000004263 ) ) ;
#221556 = EDGE_CURVE ( 'NONE', #74308, #142228, #100969, .T. ) ;
#221558 = CARTESIAN_POINT ( 'NONE',  ( 18.49999999999999645, 10.28015861706802347, -125.2245720712022319 ) ) ;
#221557 = CIRCLE ( 'NONE', #96843, 0.1999999999999945155 ) ;
#221559 = TOROIDAL_SURFACE ( 'NONE', #171730, 0.2000000000000000111, 0.1000000000000000056 ) ;
#221560 = LINE ( 'NONE', #121249, #63964 ) ;
#221562 = DIRECTION ( 'NONE',  ( 1.000000000000000000, 0.000000000000000000, -0.000000000000000000 ) ) ;
#221561 = CIRCLE ( 'NONE', #180095, 4.049999999999998046 ) ;
#221563 = DIRECTION ( 'NONE',  ( -0.000000000000000000, 1.000000000000000000, 6.982962677686266711E-15 ) ) ;
#221565 = EDGE_CURVE ( 'NONE', #241107, #17556, #5750, .T. ) ;
#221564 = DIRECTION ( 'NONE',  ( 0.000000000000000000, -0.1568667991644863147, -0.9876197685951252359 ) ) ;
#221566 = CARTESIAN_POINT ( 'NONE',  ( -20.54999999999999716, 7.150000000011155876, -54.65000000000000568 ) ) ;
#221568 = EDGE_CURVE ( 'NONE', #66968, #57845, #198876, .T. ) ;
#221567 = CARTESIAN_POINT ( 'NONE',  ( -16.86757978335471364, 9.965650379045438712, -146.5980046531675498 ) ) ;
#221569 = ORIENTED_EDGE ( 'NONE', *, *, #35781, .F. ) ;
#221570 = VERTEX_POINT ( 'NONE', #1902 ) ;
#221571 = FACE_OUTER_BOUND ( 'NONE', #207784, .T. ) ;
#221572 = SPHERICAL_SURFACE ( 'NONE', #70256, 0.1000000000000000056 ) ;
#221574 = FACE_OUTER_BOUND ( 'NONE', #75389, .T. ) ;
#221573 = FACE_OUTER_BOUND ( 'NONE', #238192, .T. ) ;
#221575 = ADVANCED_FACE ( 'NONE', ( #222228 ), #252665, .T. ) ;
#221576 = SPHERICAL_SURFACE ( 'NONE', #76903, 0.1000000000000000056 ) ;
#221577 = DIRECTION ( 'NONE',  ( 1.000000000000000000, -0.000000000000000000, -0.000000000000000000 ) ) ;
#221578 = DIRECTION ( 'NONE',  ( -1.000000000000000000, -1.394253735153568729E-16, -2.602809386958776729E-16 ) ) ;
#221579 = ADVANCED_FACE ( 'NONE', ( #63168 ), #220958, .T. ) ;
#221580 = ORIENTED_EDGE ( 'NONE', *, *, #164931, .F. ) ;
#221581 = EDGE_CURVE ( 'NONE', #247713, #103565, #82707, .T. ) ;
#221582 = CARTESIAN_POINT ( 'NONE',  ( 22.59999999999999076, 11.74987124438766273, -66.93457040898637445 ) ) ;
#221584 = ORIENTED_EDGE ( 'NONE', *, *, #56297, .T. ) ;
#221583 = AXIS2_PLACEMENT_3D ( 'NONE', #143972, #126992, #223505 ) ;
#221585 = CARTESIAN_POINT ( 'NONE',  ( -13.54036565897075306, 9.451541661385510551, -18.45387549883059464 ) ) ;
#221586 = ORIENTED_EDGE ( 'NONE', *, *, #235707, .T. ) ;
#221587 = CARTESIAN_POINT ( 'NONE',  ( -23.49999999999994316, 74.83745509109094485, -44.02310748452479316 ) ) ;
#221588 = AXIS2_PLACEMENT_3D ( 'NONE', #250620, #34190, #210242 ) ;
#221589 = CARTESIAN_POINT ( 'NONE',  ( 18.58725287972292506, 85.56662691070296489, -29.20060267875857818 ) ) ;
#221590 = VERTEX_POINT ( 'NONE', #163575 ) ;
#221591 = DIRECTION ( 'NONE',  ( 0.000000000000000000, -0.8814952561685701626, 0.4721928772782442163 ) ) ;
#221592 = CIRCLE ( 'NONE', #229994, 0.09999999999999939493 ) ;
#221593 = EDGE_LOOP ( 'NONE', ( #159375, #41921, #59046 ) ) ;
#221594 = DIRECTION ( 'NONE',  ( -0.000000000000000000, 0.2128009952263603677, -0.9770955615653313941 ) ) ;
#221595 = CARTESIAN_POINT ( 'NONE',  ( -15.55912972643740488, 52.21540900819563547, -233.2780816987436765 ) ) ;
#221597 = CIRCLE ( 'NONE', #38465, 0.09999999999999939493 ) ;
#221596 = DIRECTION ( 'NONE',  ( 1.000000000000000000, 0.000000000000000000, 0.000000000000000000 ) ) ;
#221598 = DIRECTION ( 'NONE',  ( 0.000000000000000000, -0.9908441862701605762, -0.1350103645451835310 ) ) ;
#221599 = CARTESIAN_POINT ( 'NONE',  ( -18.59999999999999787, -9.849999999999990763, 31.39999999999999858 ) ) ;
#221601 = CARTESIAN_POINT ( 'NONE',  ( -0.8999999999999437339, 64.35000000001120668, -7.323107484524790323 ) ) ;
#221600 = CARTESIAN_POINT ( 'NONE',  ( -16.97683809663754317, 66.05000000001258798, -183.2946366524139137 ) ) ;
#221602 = VECTOR ( 'NONE', #22229, 1000.000000000000000 ) ;
#221604 = DIRECTION ( 'NONE',  ( 1.000000000000000000, 0.000000000000000000, 0.000000000000000000 ) ) ;
#221603 = VECTOR ( 'NONE', #110928, 1000.000000000000000 ) ;
#221605 = AXIS2_PLACEMENT_3D ( 'NONE', #47260, #246755, #146362 ) ;
#221607 = EDGE_LOOP ( 'NONE', ( #77081, #239597, #245493, #130151 ) ) ;
#221606 = CARTESIAN_POINT ( 'NONE',  ( 20.75572585718182950, 67.11768327161469472, -128.0258490858113021 ) ) ;
#221609 = CARTESIAN_POINT ( 'NONE',  ( -23.25000000000000000, -3.187427350888460076, -228.3200064793908837 ) ) ;
#221608 = CARTESIAN_POINT ( 'NONE',  ( -16.89146115310545682, 9.951443245667611848, -188.3548224189541997 ) ) ;
#221610 = ORIENTED_EDGE ( 'NONE', *, *, #197743, .T. ) ;
#221612 = ORIENTED_EDGE ( 'NONE', *, *, #38695, .T. ) ;
#221611 = DIRECTION ( 'NONE',  ( 1.000000000000000000, 0.000000000000000000, 0.000000000000000000 ) ) ;
#221613 = ORIENTED_EDGE ( 'NONE', *, *, #222967, .F. ) ;
#221614 = CARTESIAN_POINT ( 'NONE',  ( 20.85000000000000142, 68.92903212821283887, -65.77654326265606244 ) ) ;
#221615 = CIRCLE ( 'NONE', #254885, 0.09999999999999939493 ) ;
#221616 = FACE_OUTER_BOUND ( 'NONE', #104475, .T. ) ;
#221617 = CARTESIAN_POINT ( 'NONE',  ( 21.14999999999999858, 76.00000000001219291, -143.0637644362255401 ) ) ;
#221618 = ORIENTED_EDGE ( 'NONE', *, *, #202215, .T. ) ;
#221619 = CARTESIAN_POINT ( 'NONE',  ( 21.05000000000000071, -8.663551401869154844, -23.97589888193268948 ) ) ;
#221620 = DIRECTION ( 'NONE',  ( -1.000000000000000000, 0.000000000000000000, 0.000000000000000000 ) ) ;
#221621 = CARTESIAN_POINT ( 'NONE',  ( -20.54999999999999716, 73.50000000001199396, -116.2477294072864140 ) ) ;
#221622 = DIRECTION ( 'NONE',  ( 0.000000000000000000, 1.000000000000000000, 6.982962677686266711E-15 ) ) ;
#221623 = AXIS2_PLACEMENT_3D ( 'NONE', #252601, #132677, #209639 ) ;
#221624 = CARTESIAN_POINT ( 'NONE',  ( -18.59999999999999787, 46.46967969402478360, -243.0849751855955674 ) ) ;
#221625 = CIRCLE ( 'NONE', #55033, 0.1000000000000028644 ) ;
#221626 = ADVANCED_FACE ( 'NONE', ( #44911 ), #124453, .F. ) ;
#221627 = CARTESIAN_POINT ( 'NONE',  ( -18.50000000000000000, 11.65000000001115232, -174.5148057706539930 ) ) ;
#221628 = TOROIDAL_SURFACE ( 'NONE', #17626, 4.099999999999999645, 0.1000000000000000056 ) ;
#221629 = CIRCLE ( 'NONE', #201000, 4.049999999999998046 ) ;
#221630 = ORIENTED_EDGE ( 'NONE', *, *, #167727, .F. ) ;
#221631 = ORIENTED_EDGE ( 'NONE', *, *, #188874, .F. ) ;
#221632 = EDGE_CURVE ( 'NONE', #141361, #28188, #127010, .T. ) ;
#221633 = CARTESIAN_POINT ( 'NONE',  ( -20.94999999999999929, 77.83534155023700407, -191.9679561919613491 ) ) ;
#221634 = AXIS2_PLACEMENT_3D ( 'NONE', #149101, #169976, #55086 ) ;
#221635 = VERTEX_POINT ( 'NONE', #249542 ) ;
#221636 = CARTESIAN_POINT ( 'NONE',  ( 20.85000000000000142, 42.20719072976272912, -239.1935934412594804 ) ) ;
#221637 = VERTEX_POINT ( 'NONE', #226077 ) ;
#221638 = DIRECTION ( 'NONE',  ( -1.000000000000000000, 0.000000000000000000, 0.000000000000000000 ) ) ;
#221639 = VECTOR ( 'NONE', #240808, 1000.000000000000000 ) ;
#221640 = EDGE_CURVE ( 'NONE', #200, #66243, #57397, .T. ) ;
#221641 = ADVANCED_FACE ( 'NONE', ( #194389 ), #168763, .T. ) ;
#221642 = DIRECTION ( 'NONE',  ( 0.000000000000000000, 0.8814952561688476074, -0.4721928772777262417 ) ) ;
#221643 = CARTESIAN_POINT ( 'NONE',  ( 20.94999999999999574, 1.835341550235567887, -112.0551512925630249 ) ) ;
#221644 = CIRCLE ( 'NONE', #109226, 0.1000000000000028644 ) ;
#221645 = LINE ( 'NONE', #105530, #129401 ) ;
#221646 = CARTESIAN_POINT ( 'NONE',  ( 20.95512840106819752, 10.62384869378447583, -179.7024792207988071 ) ) ;
#221647 = ORIENTED_EDGE ( 'NONE', *, *, #42305, .F. ) ;
#221648 = CARTESIAN_POINT ( 'NONE',  ( 18.59999999999999432, 85.48068669529082797, -96.08199231576637089 ) ) ;
#221649 = CARTESIAN_POINT ( 'NONE',  ( -16.87786941232800686, 66.04184528586756642, -182.6459216847304390 ) ) ;
#221650 = PLANE ( 'NONE',  #23979 ) ;
#221651 = CARTESIAN_POINT ( 'NONE',  ( -23.25000000000000000, 2.000000000011154189, -187.7753780772378889 ) ) ;
#221652 = VERTEX_POINT ( 'NONE', #30499 ) ;
#221654 = CARTESIAN_POINT ( 'NONE',  ( -23.25000000000000000, 64.25313205997782973, -247.2214437328673853 ) ) ;
#221653 = FACE_OUTER_BOUND ( 'NONE', #239677, .T. ) ;
#221655 = AXIS2_PLACEMENT_3D ( 'NONE', #107726, #245967, #131140 ) ;
#221656 = ORIENTED_EDGE ( 'NONE', *, *, #217665, .F. ) ;
#221659 = ORIENTED_EDGE ( 'NONE', *, *, #36201, .T. ) ;
#221658 = DIRECTION ( 'NONE',  ( 1.000000000000000000, 0.000000000000000000, 0.000000000000000000 ) ) ;
#221657 = CARTESIAN_POINT ( 'NONE',  ( -18.59999999999999787, 70.05000000001213323, -126.2174051794894893 ) ) ;
#221660 = AXIS2_PLACEMENT_3D ( 'NONE', #119665, #94942, #195365 ) ;
#221661 = ORIENTED_EDGE ( 'NONE', *, *, #175938, .T. ) ;
#221662 = CARTESIAN_POINT ( 'NONE',  ( -17.11825945287482753, 66.05000000001187743, -90.27310748452438816 ) ) ;
#221663 = ADVANCED_FACE ( 'NONE', ( #107443 ), #248245, .F. ) ;
#221664 = LINE ( 'NONE', #222954, #177749 ) ;
#221665 = DIRECTION ( 'NONE',  ( -1.000000000000000000, 0.000000000000000000, 0.000000000000000000 ) ) ;
#221666 = ORIENTED_EDGE ( 'NONE', *, *, #221763, .F. ) ;
#221667 = FACE_OUTER_BOUND ( 'NONE', #177067, .T. ) ;
#221668 = CARTESIAN_POINT ( 'NONE',  ( 20.94999999999999574, 4.384524567800934136, -245.2091454203640239 ) ) ;
#221670 = DIRECTION ( 'NONE',  ( 1.000000000000000000, 0.000000000000000000, 0.000000000000000000 ) ) ;
#221669 = CARTESIAN_POINT ( 'NONE',  ( 13.99999999999999822, 66.15000000001258229, -186.7731074845244450 ) ) ;
#221672 = ORIENTED_EDGE ( 'NONE', *, *, #231455, .F. ) ;
#221671 = CARTESIAN_POINT ( 'NONE',  ( -23.15000000000000213, 0.000000000000000000, 0.000000000000000000 ) ) ;
#221673 = EDGE_CURVE ( 'NONE', #233325, #167773, #234770, .T. ) ;
#221674 = VERTEX_POINT ( 'NONE', #206548 ) ;
#221676 = ADVANCED_FACE ( 'NONE', ( #188265 ), #150447, .T. ) ;
#221675 = DIRECTION ( 'NONE',  ( 1.000000000000000000, 0.000000000000000000, -0.000000000000000000 ) ) ;
#221677 = AXIS2_PLACEMENT_3D ( 'NONE', #121163, #200669, #159001 ) ;
#221678 = DIRECTION ( 'NONE',  ( -0.000000000000000000, -0.9651348961777157509, 0.2617529984165028467 ) ) ;
#221679 = CARTESIAN_POINT ( 'NONE',  ( -21.64999999999999858, 68.65000000001261071, -191.1731074845243938 ) ) ;
#221680 = EDGE_LOOP ( 'NONE', ( #138026, #39647, #76027, #86981, #64846 ) ) ;
#221681 = ORIENTED_EDGE ( 'NONE', *, *, #176217, .F. ) ;
#221682 = DIRECTION ( 'NONE',  ( 0.000000000000000000, 6.982962677686267499E-15, -1.000000000000000000 ) ) ;
#221683 = CARTESIAN_POINT ( 'NONE',  ( 22.50927854361893310, 76.10085807353982545, -114.7726746105512063 ) ) ;
#221684 = CYLINDRICAL_SURFACE ( 'NONE', #143333, 11.80000000000000426 ) ;
#221685 = ORIENTED_EDGE ( 'NONE', *, *, #11876, .T. ) ;
#221686 = EDGE_CURVE ( 'NONE', #195224, #91774, #78251, .T. ) ;
#221687 = DIRECTION ( 'NONE',  ( 0.000000000000000000, -1.000000000000000000, 0.000000000000000000 ) ) ;
#221688 = EDGE_CURVE ( 'NONE', #208072, #42380, #8359, .T. ) ;
#221689 = ADVANCED_FACE ( 'NONE', ( #167449 ), #149165, .F. ) ;
#221690 = CARTESIAN_POINT ( 'NONE',  ( -21.04999999999999716, -9.599999999988844124, -107.5320693966997112 ) ) ;
#221691 = B_SPLINE_CURVE_WITH_KNOTS ( 'NONE', 3,
 ( #73186, #225782, #48447, #217772, #136969, #254333, #35348 ),
 .UNSPECIFIED., .F., .F.,
 ( 4, 3, 4 ),
 ( 0.000000000000000000, 4.520325912680621513E-05, 5.794988040901376952E-05 ),
 .UNSPECIFIED. ) ;
#221693 = ORIENTED_EDGE ( 'NONE', *, *, #24505, .T. ) ;
#221692 = CONICAL_SURFACE ( 'NONE', #21815, 4.000000000000000000, 0.7853981633974487231 ) ;
#221694 = ORIENTED_EDGE ( 'NONE', *, *, #228741, .T. ) ;
#221695 = VERTEX_POINT ( 'NONE', #176108 ) ;
#221696 = CARTESIAN_POINT ( 'NONE',  ( -23.25000000000000000, 76.00000000001210765, -132.4731074845242915 ) ) ;
#221697 = ORIENTED_EDGE ( 'NONE', *, *, #110503, .T. ) ;
#221699 = ORIENTED_EDGE ( 'NONE', *, *, #112237, .T. ) ;
#221698 = DIRECTION ( 'NONE',  ( -1.000000000000000000, 0.000000000000000000, -0.000000000000000000 ) ) ;
#221700 = EDGE_CURVE ( 'NONE', #16800, #33205, #25815, .T. ) ;
#221701 = ORIENTED_EDGE ( 'NONE', *, *, #102941, .F. ) ;
#221704 = VERTEX_POINT ( 'NONE', #90436 ) ;
#221703 = ORIENTED_EDGE ( 'NONE', *, *, #27667, .T. ) ;
#221702 = CARTESIAN_POINT ( 'NONE',  ( -16.77779411503079032, 9.946101446935278645, -113.1630574176198678 ) ) ;
#221705 = EDGE_CURVE ( 'NONE', #68619, #90505, #15942, .T. ) ;
#221706 = VERTEX_POINT ( 'NONE', #246944 ) ;
#221707 = DIRECTION ( 'NONE',  ( 0.000000000000000000, -0.8814952561688429444, 0.4721928772777350680 ) ) ;
#221708 = CARTESIAN_POINT ( 'NONE',  ( 18.59999999999999076, 6.550000000011156231, -144.0170271704400307 ) ) ;
#221709 = VECTOR ( 'NONE', #185393, 1000.000000000000000 ) ;
#221710 = CARTESIAN_POINT ( 'NONE',  ( -16.89935556175677078, 14.05479797069542514, -218.7766119553601527 ) ) ;
#221711 = ORIENTED_EDGE ( 'NONE', *, *, #71037, .F. ) ;
#221712 = CIRCLE ( 'NONE', #246675, 0.1000000000000124678 ) ;
#221713 = DIRECTION ( 'NONE',  ( 0.000000000000000000, 0.2128009952263604787, -0.9770955615653313941 ) ) ;
#221715 = ORIENTED_EDGE ( 'NONE', *, *, #164468, .T. ) ;
#221714 = CARTESIAN_POINT ( 'NONE',  ( -20.85000000000000142, -1.164121893230052995, -108.3148480855716542 ) ) ;
#221716 = CARTESIAN_POINT ( 'NONE',  ( -16.77902162784673834, 9.946419257218995114, -180.1619912440693270 ) ) ;
#221718 = EDGE_LOOP ( 'NONE', ( #257543, #78365, #215519, #109801 ) ) ;
#221717 = LINE ( 'NONE', #185188, #139767 ) ;
#221719 = ORIENTED_EDGE ( 'NONE', *, *, #247269, .T. ) ;
#221720 = CARTESIAN_POINT ( 'NONE',  ( -20.54999999999999716, 74.00000000001205080, -123.7984855617622060 ) ) ;
#221721 = AXIS2_PLACEMENT_3D ( 'NONE', #151887, #16223, #133574 ) ;
#221722 = VECTOR ( 'NONE', #214969, 1000.000000000000000 ) ;
#221723 = EDGE_LOOP ( 'NONE', ( #110006, #95722, #19666, #2759 ) ) ;
#221724 = ORIENTED_EDGE ( 'NONE', *, *, #33728, .T. ) ;
#221725 = FACE_OUTER_BOUND ( 'NONE', #232385, .T. ) ;
#221726 = DIRECTION ( 'NONE',  ( 0.000000000000000000, -0.8660254037844377084, -0.5000000000000016653 ) ) ;
#221728 = ORIENTED_EDGE ( 'NONE', *, *, #25343, .F. ) ;
#221727 = EDGE_LOOP ( 'NONE', ( #30547, #162453, #222580, #3217 ) ) ;
#221729 = ORIENTED_EDGE ( 'NONE', *, *, #50259, .F. ) ;
#221730 = CARTESIAN_POINT ( 'NONE',  ( 19.97071067811864609, 11.72071067812981404, -158.6500000000000057 ) ) ;
#221731 = EDGE_LOOP ( 'NONE', ( #105312, #213819, #85069, #244442 ) ) ;
#221732 = VERTEX_POINT ( 'NONE', #174851 ) ;
#221734 = CARTESIAN_POINT ( 'NONE',  ( -21.64999999999999858, 10.05000000001113847, -121.2500000000000426 ) ) ;
#221733 = AXIS2_PLACEMENT_3D ( 'NONE', #63873, #224217, #83401 ) ;
#221736 = ORIENTED_EDGE ( 'NONE', *, *, #117642, .T. ) ;
#221735 = FACE_OUTER_BOUND ( 'NONE', #75526, .T. ) ;
#221737 = FACE_OUTER_BOUND ( 'NONE', #160037, .T. ) ;
#221739 = LINE ( 'NONE', #142225, #256605 ) ;
#221738 = CARTESIAN_POINT ( 'NONE',  ( -21.65000000000000213, 65.69159657275406516, -213.8343546826533839 ) ) ;
#221740 = ORIENTED_EDGE ( 'NONE', *, *, #157873, .T. ) ;
#221741 = AXIS2_PLACEMENT_3D ( 'NONE', #37362, #39937, #15229 ) ;
#221742 = VECTOR ( 'NONE', #110376, 1000.000000000000114 ) ;
#221744 = ORIENTED_EDGE ( 'NONE', *, *, #20926, .F. ) ;
#221743 = ORIENTED_EDGE ( 'NONE', *, *, #143716, .T. ) ;
#221745 = AXIS2_PLACEMENT_3D ( 'NONE', #211662, #252049, #113820 ) ;
#221746 = CARTESIAN_POINT ( 'NONE',  ( 23.14999999999999503, 11.65000000001116298, -160.5851942293460866 ) ) ;
#221747 = DIRECTION ( 'NONE',  ( 1.000000000000000000, -0.000000000000000000, 0.000000000000000000 ) ) ;
#221748 = ORIENTED_EDGE ( 'NONE', *, *, #216677, .T. ) ;
#221749 = CARTESIAN_POINT ( 'NONE',  ( -18.59999999999999787, 43.35377423437995503, -245.1717807829448930 ) ) ;
#221750 = ORIENTED_EDGE ( 'NONE', *, *, #137499, .F. ) ;
#221751 = ORIENTED_EDGE ( 'NONE', *, *, #15485, .F. ) ;
#221752 = SPHERICAL_SURFACE ( 'NONE', #233494, 0.1000000000000000056 ) ;
#221753 = ADVANCED_FACE ( 'NONE', ( #130858, #195673 ), #213922, .T. ) ;
#221754 = ORIENTED_EDGE ( 'NONE', *, *, #16367, .T. ) ;
#221755 = DIRECTION ( 'NONE',  ( 0.000000000000000000, 0.000000000000000000, 1.000000000000000000 ) ) ;
#221756 = DIRECTION ( 'NONE',  ( 0.000000000000000000, -0.4088369013363281068, 0.9126074666063770380 ) ) ;
#221757 = ORIENTED_EDGE ( 'NONE', *, *, #202196, .T. ) ;
#221758 = FACE_OUTER_BOUND ( 'NONE', #171810, .T. ) ;
#221759 = CARTESIAN_POINT ( 'NONE',  ( -20.54999999999999716, 9.350000000011156942, -155.2500000000000284 ) ) ;
#221761 = CARTESIAN_POINT ( 'NONE',  ( -21.05000000000000071, 43.44873802792533724, -245.1397081572968659 ) ) ;
#221760 = CARTESIAN_POINT ( 'NONE',  ( 20.94999999999999929, 1.115600667400684642E-11, -200.9999999999999432 ) ) ;
#221762 = CYLINDRICAL_SURFACE ( 'NONE', #156498, 0.5000000000000004441 ) ;
#221763 = EDGE_CURVE ( 'NONE', #134587, #47002, #40882, .T. ) ;
#221765 = EDGE_CURVE ( 'NONE', #14167, #104512, #159110, .T. ) ;
#221764 = CARTESIAN_POINT ( 'NONE',  ( -21.14999999999999858, 61.16604239671104892, -234.3115055913011417 ) ) ;
#221766 = CARTESIAN_POINT ( 'NONE',  ( 18.79999999999999716, 1.250000000000000000, 21.90000000000000213 ) ) ;
#221767 = DIRECTION ( 'NONE',  ( 1.000000000000000000, 0.000000000000000000, 0.000000000000000000 ) ) ;
#221768 = VECTOR ( 'NONE', #217255, 1000.000000000000000 ) ;
#221769 = EDGE_LOOP ( 'NONE', ( #170140, #37791, #104042, #145427, #91820, #182114 ) ) ;
#221770 = VECTOR ( 'NONE', #151248, 1000.000000000000000 ) ;
#221772 = VERTEX_POINT ( 'NONE', #78250 ) ;
#221771 = ORIENTED_EDGE ( 'NONE', *, *, #127393, .F. ) ;
#221773 = ORIENTED_EDGE ( 'NONE', *, *, #182837, .F. ) ;
#221774 = EDGE_CURVE ( 'NONE', #69086, #18420, #99084, .T. ) ;
#221775 = LINE ( 'NONE', #223082, #116044 ) ;
#221776 = VECTOR ( 'NONE', #231394, 1000.000000000000000 ) ;
#221777 = CARTESIAN_POINT ( 'NONE',  ( -20.94999999999999929, 87.65000000001192859, -100.1231074845242262 ) ) ;
#221779 = CARTESIAN_POINT ( 'NONE',  ( -21.14999999999999858, 11.75000000000000000, -0.1000000000000028644 ) ) ;
#221778 = FACE_OUTER_BOUND ( 'NONE', #194401, .T. ) ;
#221780 = CARTESIAN_POINT ( 'NONE',  ( 20.95263205890715952, 67.10425989211827869, -161.5335990775828066 ) ) ;
#221781 = VERTEX_POINT ( 'NONE', #217749 ) ;
#221782 = VECTOR ( 'NONE', #232790, 1000.000000000000000 ) ;
#221783 = FACE_OUTER_BOUND ( 'NONE', #100037, .T. ) ;
#221784 = LINE ( 'NONE', #44479, #229392 ) ;
#221785 = AXIS2_PLACEMENT_3D ( 'NONE', #228124, #230692, #54598 ) ;
#221786 = CARTESIAN_POINT ( 'NONE',  ( -21.05000000000000071, 77.07318729351892728, -199.5660544101962728 ) ) ;
#221787 = CIRCLE ( 'NONE', #47008, 0.1000000000000000333 ) ;
#221788 = CIRCLE ( 'NONE', #105240, 0.1000000000000028644 ) ;
#221789 = FACE_OUTER_BOUND ( 'NONE', #140806, .T. ) ;
#221790 = ORIENTED_EDGE ( 'NONE', *, *, #186164, .T. ) ;
#221791 = CIRCLE ( 'NONE', #26021, 0.09999999999999693856 ) ;
#221792 = CARTESIAN_POINT ( 'NONE',  ( 20.05000000000002913, 68.75000000001197975, -115.6731074845243512 ) ) ;
#221793 = AXIS2_PLACEMENT_3D ( 'NONE', #35058, #191552, #33779 ) ;
#221794 = CARTESIAN_POINT ( 'NONE',  ( -20.85000000000000142, -1.362429037193307435, -41.38888124792119783 ) ) ;
#221795 = ORIENTED_EDGE ( 'NONE', *, *, #143842, .T. ) ;
#221796 = EDGE_CURVE ( 'NONE', #201070, #226700, #237346, .T. ) ;
#221797 = CARTESIAN_POINT ( 'NONE',  ( 23.14999999999999503, 6.450000000011156587, -146.3500000000000227 ) ) ;
#221798 = EDGE_CURVE ( 'NONE', #169080, #147215, #58676, .T. ) ;
#221799 = DIRECTION ( 'NONE',  ( -1.000000000000000000, -0.000000000000000000, -0.000000000000000000 ) ) ;
#221800 = DIRECTION ( 'NONE',  ( 1.000000000000000000, 0.000000000000000000, 0.000000000000000000 ) ) ;
#221801 = DIRECTION ( 'NONE',  ( 1.000000000000000000, 0.000000000000000000, 0.000000000000000000 ) ) ;
#221803 = TOROIDAL_SURFACE ( 'NONE', #176069, 0.2000000000000000111, 0.1000000000000000056 ) ;
#221802 = CARTESIAN_POINT ( 'NONE',  ( -17.27223548803194575, 10.34539739140540604, -22.13360617919591533 ) ) ;
#221804 = VERTEX_POINT ( 'NONE', #99083 ) ;
#221805 = DIRECTION ( 'NONE',  ( -1.000000000000000000, 0.000000000000000000, 0.000000000000000000 ) ) ;
#221806 = DIRECTION ( 'NONE',  ( -2.940209281316618057E-16, 0.4721928772777340688, 0.8814952561688433885 ) ) ;
#221807 = CARTESIAN_POINT ( 'NONE',  ( 21.05000000000000071, 11.77895973109482419, -206.1023438919106070 ) ) ;
#221809 = SPHERICAL_SURFACE ( 'NONE', #241248, 0.1000000000000000056 ) ;
#221808 = CYLINDRICAL_SURFACE ( 'NONE', #99172, 0.1000000000000028644 ) ;
#221810 = LINE ( 'NONE', #7941, #137227 ) ;
#221811 = EDGE_CURVE ( 'NONE', #176792, #248456, #100364, .T. ) ;
#221812 = DIRECTION ( 'NONE',  ( -1.000000000000000000, -0.000000000000000000, 0.000000000000000000 ) ) ;
#221813 = VECTOR ( 'NONE', #202793, 1000.000000000000000 ) ;
#221814 = LINE ( 'NONE', #43211, #172838 ) ;
#221815 = FACE_BOUND ( 'NONE', #194810, .T. ) ;
#221817 = ORIENTED_EDGE ( 'NONE', *, *, #180898, .T. ) ;
#221816 = CARTESIAN_POINT ( 'NONE',  ( -21.05000000000000071, 26.06832281015329755, -254.4051978787608732 ) ) ;
#221818 = AXIS2_PLACEMENT_3D ( 'NONE', #204709, #185167, #229432 ) ;
#221819 = VECTOR ( 'NONE', #197210, 1000.000000000000000 ) ;
#221820 = ORIENTED_EDGE ( 'NONE', *, *, #182516, .F. ) ;
#221821 = CARTESIAN_POINT ( 'NONE',  ( -16.94107738177415712, 10.01423928514777728, -146.5500000000000114 ) ) ;
#221822 = ADVANCED_FACE ( 'NONE', ( #117390 ), #160398, .F. ) ;
#221823 = DIRECTION ( 'NONE',  ( 0.000000000000000000, -0.2128009952263604510, 0.9770955615653315052 ) ) ;
#221824 = CARTESIAN_POINT ( 'NONE',  ( 12.93225390519045703, 9.417651958852161442, -149.3587873924404619 ) ) ;
#221825 = ORIENTED_EDGE ( 'NONE', *, *, #243883, .F. ) ;
#221826 = VECTOR ( 'NONE', #193427, 1000.000000000000000 ) ;
#221828 = DIRECTION ( 'NONE',  ( 0.000000000000000000, 0.000000000000000000, -1.000000000000000000 ) ) ;
#221827 = CIRCLE ( 'NONE', #217555, 0.2000000000000053679 ) ;
#221829 = CARTESIAN_POINT ( 'NONE',  ( 20.12500000000000000, 9.750000000011153745, -108.6117712821143186 ) ) ;
#221830 = CARTESIAN_POINT ( 'NONE',  ( -21.00023020733502932, 76.00000000001200817, -109.4139767297926653 ) ) ;
#221831 = EDGE_CURVE ( 'NONE', #254615, #45873, #244842, .T. ) ;
#221832 = ADVANCED_FACE ( 'NONE', ( #62559 ), #138210, .F. ) ;
#221833 = VERTEX_POINT ( 'NONE', #216487 ) ;
#221834 = DIRECTION ( 'NONE',  ( -1.000000000000000000, 0.000000000000000000, -0.000000000000000000 ) ) ;
#221836 = ORIENTED_EDGE ( 'NONE', *, *, #243962, .T. ) ;
#221835 = DIRECTION ( 'NONE',  ( -1.000000000000000000, 1.772924042024179204E-16, -4.808324575169891715E-17 ) ) ;
#221838 = CARTESIAN_POINT ( 'NONE',  ( -12.25000000000000178, 9.850000000011133849, -150.7500000000000284 ) ) ;
#221837 = DIRECTION ( 'NONE',  ( -3.265361837132813093E-16, 1.000000000000000000, 0.000000000000000000 ) ) ;
#221839 = CARTESIAN_POINT ( 'NONE',  ( 20.74897398619119215, 65.40430697834587193, -162.3437960282675192 ) ) ;
#221841 = EDGE_CURVE ( 'NONE', #126698, #85598, #39163, .T. ) ;
#221840 = CARTESIAN_POINT ( 'NONE',  ( 18.49999999999999289, 34.53503747617446606, -235.1972745784239578 ) ) ;
#221842 = EDGE_CURVE ( 'NONE', #152529, #212362, #202069, .T. ) ;
#221843 = ORIENTED_EDGE ( 'NONE', *, *, #237002, .T. ) ;
#221844 = DIRECTION ( 'NONE',  ( 0.000000000000000000, 1.000000000000000000, 6.982962677686266711E-15 ) ) ;
#221845 = CARTESIAN_POINT ( 'NONE',  ( 20.05000000000002913, 68.75000000001257661, -190.8731074845244109 ) ) ;
#221846 = EDGE_LOOP ( 'NONE', ( #2722, #207201, #229109, #239527 ) ) ;
#221847 = CYLINDRICAL_SURFACE ( 'NONE', #37744, 0.1000000000000124678 ) ;
#221848 = AXIS2_PLACEMENT_3D ( 'NONE', #248436, #14972, #151926 ) ;
#221849 = ADVANCED_FACE ( 'NONE', ( #157847 ), #23460, .T. ) ;
#221850 = DIRECTION ( 'NONE',  ( 1.000000000000000000, 0.000000000000000000, 0.000000000000000000 ) ) ;
#221852 = EDGE_CURVE ( 'NONE', #93242, #256823, #207463, .T. ) ;
#221851 = EDGE_CURVE ( 'NONE', #251749, #257480, #18287, .T. ) ;
#221853 = CIRCLE ( 'NONE', #26088, 0.09999999999999939493 ) ;
#221854 = DIRECTION ( 'NONE',  ( 0.000000000000000000, -0.3488585713686159218, -0.9371753822965306346 ) ) ;
#221855 = DIRECTION ( 'NONE',  ( 0.000000000000000000, 0.000000000000000000, 1.000000000000000000 ) ) ;
#221856 = EDGE_LOOP ( 'NONE', ( #123702, #27310, #28319, #136500 ) ) ;
#221857 = EDGE_CURVE ( 'NONE', #211037, #178041, #45132, .T. ) ;
#221858 = ORIENTED_EDGE ( 'NONE', *, *, #55401, .T. ) ;
#221859 = LINE ( 'NONE', #66672, #163201 ) ;
#221860 = DIRECTION ( 'NONE',  ( 0.000000000000000000, 0.000000000000000000, 1.000000000000000000 ) ) ;
#221861 = DIRECTION ( 'NONE',  ( 1.000000000000000000, 0.000000000000000000, 0.000000000000000000 ) ) ;
#221862 = EDGE_CURVE ( 'NONE', #20618, #78065, #49216, .T. ) ;
#221863 = CARTESIAN_POINT ( 'NONE',  ( -20.64999999999999858, 71.65000000001187175, -90.67310748452433700 ) ) ;
#221864 = FACE_OUTER_BOUND ( 'NONE', #10732, .T. ) ;
#221865 = CARTESIAN_POINT ( 'NONE',  ( -16.87683809663752399, 12.47642768288813286, -211.9993005936843815 ) ) ;
#221866 = DIRECTION ( 'NONE',  ( 1.000000000000000000, 0.000000000000000000, 0.000000000000000000 ) ) ;
#221868 = EDGE_CURVE ( 'NONE', #6746, #27052, #20025, .T. ) ;
#221867 = CARTESIAN_POINT ( 'NONE',  ( -16.87683809663753109, 66.13508622147315918, -56.24739184888585442 ) ) ;
#221870 = ADVANCED_FACE ( 'NONE', ( #181238 ), #102940, .F. ) ;
#221869 = CYLINDRICAL_SURFACE ( 'NONE', #218011, 0.1000000000000012546 ) ;
#221871 = ORIENTED_EDGE ( 'NONE', *, *, #256831, .F. ) ;
#221872 = DIRECTION ( 'NONE',  ( 1.000000000000000000, 0.000000000000000000, 0.000000000000000000 ) ) ;
#221873 = VECTOR ( 'NONE', #82378, 1000.000000000000000 ) ;
#221875 = ORIENTED_EDGE ( 'NONE', *, *, #121322, .T. ) ;
#221874 = DIRECTION ( 'NONE',  ( 1.000000000000000000, -0.000000000000000000, -0.000000000000000000 ) ) ;
#221876 = CARTESIAN_POINT ( 'NONE',  ( -21.03922262424648082, 64.37609936600730975, -129.6638994416306616 ) ) ;
#221877 = DIRECTION ( 'NONE',  ( 0.000000000000000000, 0.000000000000000000, 1.000000000000000000 ) ) ;
#221879 = CARTESIAN_POINT ( 'NONE',  ( -20.94999999999999929, -11.48912529306490349, -136.9000000000000341 ) ) ;
#221878 = CARTESIAN_POINT ( 'NONE',  ( 22.00411653889209518, 75.90096189422524731, -110.2765503521647048 ) ) ;
#221880 = EDGE_CURVE ( 'NONE', #199490, #55232, #211548, .T. ) ;
#221881 = EDGE_LOOP ( 'NONE', ( #59826, #208458, #118246, #219078, #104645, #153093 ) ) ;
#221883 = FACE_OUTER_BOUND ( 'NONE', #189287, .T. ) ;
#221882 = CYLINDRICAL_SURFACE ( 'NONE', #226744, 0.1000000000000028644 ) ;
#221884 = LINE ( 'NONE', #185354, #70739 ) ;
#221885 = DIRECTION ( 'NONE',  ( 1.000000000000000000, 0.000000000000000000, 0.000000000000000000 ) ) ;
#221886 = DIRECTION ( 'NONE',  ( 1.441126678808781001E-14, 0.9876197685951252359, 0.1568667991644863424 ) ) ;
#221887 = LINE ( 'NONE', #161966, #140938 ) ;
#221888 = VERTEX_POINT ( 'NONE', #147220 ) ;
#221889 = EDGE_CURVE ( 'NONE', #2008, #80528, #185061, .T. ) ;
#221890 = ORIENTED_EDGE ( 'NONE', *, *, #26385, .F. ) ;
#221891 = EDGE_CURVE ( 'NONE', #128423, #242182, #228305, .T. ) ;
#221893 = AXIS2_PLACEMENT_3D ( 'NONE', #1861, #99672, #137527 ) ;
#221892 = DIRECTION ( 'NONE',  ( -1.000000000000000000, 0.000000000000000000, -0.000000000000000000 ) ) ;
#221894 = VERTEX_POINT ( 'NONE', #27320 ) ;
#221895 = CARTESIAN_POINT ( 'NONE',  ( -20.85000000000000142, 76.00000000001126921, -203.5231074845248997 ) ) ;
#221896 = ORIENTED_EDGE ( 'NONE', *, *, #235535, .F. ) ;
#221897 = AXIS2_PLACEMENT_3D ( 'NONE', #117104, #173277, #213626 ) ;
#221898 = CARTESIAN_POINT ( 'NONE',  ( 23.14999999999999858, 45.69057616835975466, -239.3688303688244616 ) ) ;
#221899 = TOROIDAL_SURFACE ( 'NONE', #238491, 0.2000000000000000111, 0.1000000000000000056 ) ;
#221900 = FACE_OUTER_BOUND ( 'NONE', #59177, .T. ) ;
#221901 = VERTEX_POINT ( 'NONE', #63840 ) ;
#221902 = EDGE_CURVE ( 'NONE', #48580, #105943, #78441, .T. ) ;
#221903 = CARTESIAN_POINT ( 'NONE',  ( -16.77683809663752257, 9.945835743215303282, -87.83605098089584828 ) ) ;
#221904 = CARTESIAN_POINT ( 'NONE',  ( -21.11833042828139284, 65.53725477864057325, -242.0741845493446078 ) ) ;
#221905 = DIRECTION ( 'NONE',  ( 0.000000000000000000, 0.1686199900910294591, -0.9856811345164832039 ) ) ;
#221906 = TOROIDAL_SURFACE ( 'NONE', #59582, 1.900000000000002576, 0.1000000000000000056 ) ;
#221908 = CARTESIAN_POINT ( 'NONE',  ( 22.39999999999999503, 0.3085173699977246109, -229.9658011520297975 ) ) ;
#221907 = AXIS2_PLACEMENT_3D ( 'NONE', #81836, #161438, #126119 ) ;
#221909 = DIRECTION ( 'NONE',  ( 1.000000000000000000, 0.000000000000000000, 0.000000000000000000 ) ) ;
#221910 = DIRECTION ( 'NONE',  ( 0.000000000000000000, 0.9999631594459053030, 0.008583690987162899758 ) ) ;
#221911 = DIRECTION ( 'NONE',  ( 0.000000000000000000, -0.8814952561688476074, 0.4721928772777262417 ) ) ;
#221912 = VERTEX_POINT ( 'NONE', #83367 ) ;
#221914 = DIRECTION ( 'NONE',  ( 1.000000000000000000, -2.952720810173289112E-16, -2.061873921506763405E-30 ) ) ;
#221913 = CARTESIAN_POINT ( 'NONE',  ( 23.24999999999999645, 64.25000000001190870, -93.77310748452438816 ) ) ;
#221915 = VERTEX_POINT ( 'NONE', #85931 ) ;
#221917 = ORIENTED_EDGE ( 'NONE', *, *, #166847, .T. ) ;
#221916 = CARTESIAN_POINT ( 'NONE',  ( 18.59999999999999432, 77.16270174995064224, -195.5231074845243313 ) ) ;
#221918 = ORIENTED_EDGE ( 'NONE', *, *, #195964, .F. ) ;
#221919 = FACE_BOUND ( 'NONE', #6718, .T. ) ;
#221920 = DIRECTION ( 'NONE',  ( -1.000000000000000000, -2.952720810173289112E-16, 0.000000000000000000 ) ) ;
#221921 = AXIS2_PLACEMENT_3D ( 'NONE', #256379, #140333, #216017 ) ;
#221922 = DIRECTION ( 'NONE',  ( 0.000000000000000000, 0.000000000000000000, -1.000000000000000000 ) ) ;
#221923 = ORIENTED_EDGE ( 'NONE', *, *, #51023, .T. ) ;
#221924 = FACE_OUTER_BOUND ( 'NONE', #140577, .T. ) ;
#221925 = CARTESIAN_POINT ( 'NONE',  ( 21.05000000000000071, 11.65000000001116298, -33.50000000000000000 ) ) ;
#221926 = CIRCLE ( 'NONE', #134622, 11.80000000000000426 ) ;
#221927 = ORIENTED_EDGE ( 'NONE', *, *, #163374, .F. ) ;
#221928 = AXIS2_PLACEMENT_3D ( 'NONE', #105879, #239321, #165908 ) ;
#221929 = CIRCLE ( 'NONE', #209475, 0.09999999999999939493 ) ;
#221930 = CARTESIAN_POINT ( 'NONE',  ( 18.58703555225034165, -9.406336740777783589, -174.6249446412465716 ) ) ;
#221931 = VECTOR ( 'NONE', #40296, 1000.000000000000000 ) ;
#221932 = ADVANCED_FACE ( 'NONE', ( #8995 ), #207215, .T. ) ;
#221933 = CARTESIAN_POINT ( 'NONE',  ( -21.05000000000000071, 7.128833340094563376, -233.7327013124401276 ) ) ;
#221934 = VERTEX_POINT ( 'NONE', #127669 ) ;
#221935 = EDGE_CURVE ( 'NONE', #80211, #113007, #11843, .T. ) ;
#221936 = CARTESIAN_POINT ( 'NONE',  ( 18.59999999999999076, 11.65000000000000391, -24.85000000000000142 ) ) ;
#221937 = DIRECTION ( 'NONE',  ( 1.000000000000000000, 0.000000000000000000, 0.000000000000000000 ) ) ;
#221938 = VERTEX_POINT ( 'NONE', #126375 ) ;
#221939 = CYLINDRICAL_SURFACE ( 'NONE', #191915, 0.09999999999999939493 ) ;
#221940 = EDGE_CURVE ( 'NONE', #177487, #22985, #219917, .T. ) ;
#221941 = EDGE_CURVE ( 'NONE', #227124, #109848, #103368, .T. ) ;
#221942 = DIRECTION ( 'NONE',  ( 0.000000000000000000, -0.9651348961777379554, 0.2617529984164210233 ) ) ;
#221943 = CARTESIAN_POINT ( 'NONE',  ( 21.05000000000000071, 5.000000000011153745, -155.4947339810869380 ) ) ;
#221944 = AXIS2_PLACEMENT_3D ( 'NONE', #141164, #257196, #220696 ) ;
#221945 = CYLINDRICAL_SURFACE ( 'NONE', #108231, 0.09999999999999976963 ) ;
#221946 = DIRECTION ( 'NONE',  ( 1.000000000000000000, 0.000000000000000000, 0.000000000000000000 ) ) ;
#221947 = CARTESIAN_POINT ( 'NONE',  ( 20.94788355080264353, 10.30207779525983014, -72.48955207167824710 ) ) ;
#221948 = VERTEX_POINT ( 'NONE', #128953 ) ;
#221950 = DIRECTION ( 'NONE',  ( -1.000000000000000000, 0.000000000000000000, -0.000000000000000000 ) ) ;
#221949 = DIRECTION ( 'NONE',  ( 0.000000000000000000, -0.9126074666063660468, -0.4088369013363524762 ) ) ;
#221951 = EDGE_LOOP ( 'NONE', ( #203303, #81142, #120439, #245514 ) ) ;
#221952 = AXIS2_PLACEMENT_3D ( 'NONE', #179407, #98516, #238069 ) ;
#221953 = LINE ( 'NONE', #240280, #235316 ) ;
#221954 = LINE ( 'NONE', #241550, #158327 ) ;
#221955 = AXIS2_PLACEMENT_3D ( 'NONE', #128133, #64299, #164689 ) ;
#221957 = ORIENTED_EDGE ( 'NONE', *, *, #107367, .T. ) ;
#221956 = CARTESIAN_POINT ( 'NONE',  ( 23.40000000000005542, 74.94272479589878344, -3.123107484524795474 ) ) ;
#221959 = ORIENTED_EDGE ( 'NONE', *, *, #5696, .F. ) ;
#221958 = CARTESIAN_POINT ( 'NONE',  ( -18.44448725179914206, 85.49008171549542112, -129.8941471904618368 ) ) ;
#221960 = LINE ( 'NONE', #124195, #189490 ) ;
#221961 = CARTESIAN_POINT ( 'NONE',  ( -20.85000000000000142, 77.83585931145526615, -58.01866831572577610 ) ) ;
#221962 = CARTESIAN_POINT ( 'NONE',  ( -16.83199030136658081, 9.930648033124620966, -79.77240102265751887 ) ) ;
#221963 = AXIS2_PLACEMENT_3D ( 'NONE', #97735, #135596, #92617 ) ;
#221964 = DIRECTION ( 'NONE',  ( 0.000000000000000000, 0.000000000000000000, -1.000000000000000000 ) ) ;
#221966 = ORIENTED_EDGE ( 'NONE', *, *, #101163, .T. ) ;
#221965 = FACE_OUTER_BOUND ( 'NONE', #193345, .T. ) ;
#221967 = TOROIDAL_SURFACE ( 'NONE', #67875, 0.2000000000000000111, 0.1000000000000000056 ) ;
#221968 = CIRCLE ( 'NONE', #209520, 4.049999999999998046 ) ;
#221969 = ADVANCED_FACE ( 'NONE', ( #104225 ), #115870, .F. ) ;
#221970 = VECTOR ( 'NONE', #29601, 999.9999999999998863 ) ;
#221971 = LINE ( 'NONE', #43373, #134972 ) ;
#221972 = ORIENTED_EDGE ( 'NONE', *, *, #107138, .F. ) ;
#221973 = ORIENTED_EDGE ( 'NONE', *, *, #76952, .F. ) ;
#221974 = CARTESIAN_POINT ( 'NONE',  ( -18.41418431465368144, 85.50000000001161027, -29.42291809330281183 ) ) ;
#221975 = DIRECTION ( 'NONE',  ( 0.000000000000000000, 0.000000000000000000, -1.000000000000000000 ) ) ;
#221976 = VECTOR ( 'NONE', #223132, 1000.000000000000000 ) ;
#221977 = EDGE_LOOP ( 'NONE', ( #184928, #171148, #178763, #60385, #30467, #133162 ) ) ;
#221978 = ADVANCED_FACE ( 'NONE', ( #205905 ), #24309, .T. ) ;
#221979 = DIRECTION ( 'NONE',  ( 0.000000000000000000, -0.9770955615653316162, -0.2128009952263604232 ) ) ;
#221980 = AXIS2_PLACEMENT_3D ( 'NONE', #25705, #90795, #6119 ) ;
#221981 = EDGE_CURVE ( 'NONE', #194795, #64660, #208504, .T. ) ;
#221982 = FACE_OUTER_BOUND ( 'NONE', #13955, .T. ) ;
#221983 = AXIS2_PLACEMENT_3D ( 'NONE', #160508, #240025, #61377 ) ;
#221984 = ORIENTED_EDGE ( 'NONE', *, *, #60524, .T. ) ;
#221985 = DIRECTION ( 'NONE',  ( -5.603264701231743991E-32, 1.897661533703520143E-16, -1.000000000000000000 ) ) ;
#221986 = CIRCLE ( 'NONE', #142881, 1.900000000000012790 ) ;
#221987 = CONICAL_SURFACE ( 'NONE', #38879, 6.249999999999995559, 0.7853981633974431720 ) ;
#221989 = TOROIDAL_SURFACE ( 'NONE', #80518, 12.77500000000000036, 0.1000000000000000056 ) ;
#221988 = CARTESIAN_POINT ( 'NONE',  ( -18.50000000000000000, 85.40000000001263913, -196.2258477248610120 ) ) ;
#221990 = EDGE_CURVE ( 'NONE', #229182, #202498, #43784, .T. ) ;
#221991 = VERTEX_POINT ( 'NONE', #246326 ) ;
#221992 = TOROIDAL_SURFACE ( 'NONE', #146989, 11.89999999999999858, 0.1000000000000000056 ) ;
#221993 = ORIENTED_EDGE ( 'NONE', *, *, #126909, .F. ) ;
#221994 = CARTESIAN_POINT ( 'NONE',  ( -23.15000000000000213, 66.17117490947157421, -239.7639228359981303 ) ) ;
#221995 = ORIENTED_EDGE ( 'NONE', *, *, #147764, .T. ) ;
#221996 = CARTESIAN_POINT ( 'NONE',  ( -16.83794237512073977, 23.10225113665113383, -231.0284041592679785 ) ) ;
#221997 = ORIENTED_EDGE ( 'NONE', *, *, #85734, .F. ) ;
#221999 = EDGE_LOOP ( 'NONE', ( #206654, #119605, #252238, #29590 ) ) ;
#221998 = LINE ( 'NONE', #4245, #46854 ) ;
#222000 = ADVANCED_FACE ( 'NONE', ( #49410 ), #36796, .F. ) ;
#222001 = EDGE_CURVE ( 'NONE', #61108, #27454, #190913, .T. ) ;
#222002 = DIRECTION ( 'NONE',  ( 1.000000000000000000, -0.000000000000000000, -0.000000000000000000 ) ) ;
#222003 = ORIENTED_EDGE ( 'NONE', *, *, #104922, .T. ) ;
#222004 = CARTESIAN_POINT ( 'NONE',  ( 22.50046968638162781, 0.04516984715002460293, -88.74995484552745495 ) ) ;
#222005 = ORIENTED_EDGE ( 'NONE', *, *, #99230, .T. ) ;
#222007 = ORIENTED_EDGE ( 'NONE', *, *, #1595, .F. ) ;
#222006 = ORIENTED_EDGE ( 'NONE', *, *, #218705, .F. ) ;
#222008 = DIRECTION ( 'NONE',  ( 1.000000000000000000, -0.000000000000000000, -0.000000000000000000 ) ) ;
#222009 = EDGE_CURVE ( 'NONE', #16173, #232481, #257449, .T. ) ;
#222010 = LINE ( 'NONE', #160813, #77317 ) ;
#222012 = EDGE_LOOP ( 'NONE', ( #93510, #181900, #163732, #165602, #15476, #174736, #4168, #191151, #196057 ) ) ;
#222011 = VECTOR ( 'NONE', #121026, 1000.000000000000000 ) ;
#222013 = AXIS2_PLACEMENT_3D ( 'NONE', #109061, #212043, #30850 ) ;
#222014 = CIRCLE ( 'NONE', #188716, 4.150000000000001243 ) ;
#222015 = VECTOR ( 'NONE', #107880, 1000.000000000000227 ) ;
#222016 = EDGE_LOOP ( 'NONE', ( #4380, #124953, #195670, #117999 ) ) ;
#222017 = CARTESIAN_POINT ( 'NONE',  ( 23.04999999999999716, 29.67396024497139706, -235.8008764811443712 ) ) ;
#222018 = EDGE_CURVE ( 'NONE', #155807, #98643, #107484, .T. ) ;
#222019 = CARTESIAN_POINT ( 'NONE',  ( -18.50000000000000000, -26.43935341558978891, -185.6415086075074328 ) ) ;
#222021 = VERTEX_POINT ( 'NONE', #151080 ) ;
#222020 = FACE_OUTER_BOUND ( 'NONE', #98949, .T. ) ;
#222022 = CYLINDRICAL_SURFACE ( 'NONE', #93867, 0.1000000000000098310 ) ;
#222023 = ORIENTED_EDGE ( 'NONE', *, *, #19743, .T. ) ;
#222024 = DIRECTION ( 'NONE',  ( 0.000000000000000000, -7.026728003956695223E-15, 1.000000000000000000 ) ) ;
#222025 = DIRECTION ( 'NONE',  ( 1.000000000000000000, 0.000000000000000000, 0.000000000000000000 ) ) ;
#222026 = ORIENTED_EDGE ( 'NONE', *, *, #242378, .F. ) ;
#222027 = DIRECTION ( 'NONE',  ( -4.336808689941751101E-15, 0.7397890806274315390, 0.6728388485992909951 ) ) ;
#222028 = DIRECTION ( 'NONE',  ( 0.000000000000000000, -0.1575844902526687130, -0.9875055080513762684 ) ) ;
#222029 = ORIENTED_EDGE ( 'NONE', *, *, #229825, .T. ) ;
#222030 = CARTESIAN_POINT ( 'NONE',  ( -16.94389599338511943, 66.00880201025681515, -90.41546268271413567 ) ) ;
#222031 = ORIENTED_EDGE ( 'NONE', *, *, #218609, .T. ) ;
#222033 = ORIENTED_EDGE ( 'NONE', *, *, #153268, .T. ) ;
#222032 = ORIENTED_EDGE ( 'NONE', *, *, #251492, .F. ) ;
#222034 = AXIS2_PLACEMENT_3D ( 'NONE', #41078, #134988, #44912 ) ;
#222035 = ORIENTED_EDGE ( 'NONE', *, *, #83281, .F. ) ;
#222036 = CARTESIAN_POINT ( 'NONE',  ( -16.86132326855785735, 9.950000000011135270, -79.69863578466836884 ) ) ;
#222037 = ORIENTED_EDGE ( 'NONE', *, *, #22227, .T. ) ;
#222038 = DIRECTION ( 'NONE',  ( 0.000000000000000000, 0.8700118002898321601, -0.4930308989875230030 ) ) ;
#222039 = ORIENTED_EDGE ( 'NONE', *, *, #210020, .T. ) ;
#222040 = DIRECTION ( 'NONE',  ( 0.000000000000000000, 0.000000000000000000, -1.000000000000000000 ) ) ;
#222041 = DIRECTION ( 'NONE',  ( 0.000000000000000000, 0.2617529984165028467, 0.9651348961777159730 ) ) ;
#222042 = ORIENTED_EDGE ( 'NONE', *, *, #76498, .F. ) ;
#222043 = ORIENTED_EDGE ( 'NONE', *, *, #113330, .T. ) ;
#222044 = AXIS2_PLACEMENT_3D ( 'NONE', #221643, #122582, #44325 ) ;
#222045 = VERTEX_POINT ( 'NONE', #194074 ) ;
#222046 = EDGE_CURVE ( 'NONE', #257455, #135756, #170267, .T. ) ;
#222047 = CIRCLE ( 'NONE', #251290, 0.09999999999999520384 ) ;
#222048 = CARTESIAN_POINT ( 'NONE',  ( -22.39999999999999858, -0.1008583690875579364, -155.7504328765105868 ) ) ;
#222049 = ORIENTED_EDGE ( 'NONE', *, *, #213121, .F. ) ;
#222050 = CARTESIAN_POINT ( 'NONE',  ( -21.05000000000000071, 4.384524567800934136, -245.2091454203640239 ) ) ;
#222051 = EDGE_CURVE ( 'NONE', #167344, #76552, #211055, .T. ) ;
#222052 = DIRECTION ( 'NONE',  ( -6.938893903907222856E-15, -0.4088369013363283289, 0.9126074666063768159 ) ) ;
#222053 = CARTESIAN_POINT ( 'NONE',  ( -20.64999999999999858, -9.399999999988850163, -43.39396912265245021 ) ) ;
#222054 = CARTESIAN_POINT ( 'NONE',  ( 21.56666275994539816, 0.9959460939976487737, -230.4474815061071240 ) ) ;
#222055 = CARTESIAN_POINT ( 'NONE',  ( -22.39999999999999858, 76.00000000001242029, -176.2731074845243597 ) ) ;
#222056 = DIRECTION ( 'NONE',  ( 1.000000000000000000, 2.952720810173289112E-16, -0.000000000000000000 ) ) ;
#222057 = EDGE_CURVE ( 'NONE', #142448, #13227, #135340, .T. ) ;
#222059 = CARTESIAN_POINT ( 'NONE',  ( 21.05000000000000071, -11.64999999998883595, -134.0000000000000000 ) ) ;
#222058 = DIRECTION ( 'NONE',  ( 0.000000000000000000, 0.000000000000000000, -1.000000000000000000 ) ) ;
#222061 = EDGE_CURVE ( 'NONE', #6622, #70888, #92373, .T. ) ;
#222060 = CARTESIAN_POINT ( 'NONE',  ( -20.94999999999999929, 87.65000000001235492, -167.1231074845242688 ) ) ;
#222062 = CARTESIAN_POINT ( 'NONE',  ( 20.09999999673965121, 4.627350251755220079, 22.02580456186781532 ) ) ;
#222063 = AXIS2_PLACEMENT_3D ( 'NONE', #72157, #36903, #34325 ) ;
#222064 = CYLINDRICAL_SURFACE ( 'NONE', #1404, 0.09999999999999939493 ) ;
#222065 = DIRECTION ( 'NONE',  ( 1.000000000000000000, -0.000000000000000000, 0.000000000000000000 ) ) ;
#222066 = CIRCLE ( 'NONE', #113763, 0.8750000000000007772 ) ;
#222067 = ORIENTED_EDGE ( 'NONE', *, *, #244269, .T. ) ;
#222068 = AXIS2_PLACEMENT_3D ( 'NONE', #11668, #35106, #95029 ) ;
#222070 = EDGE_LOOP ( 'NONE', ( #130586, #205668, #180260, #102669 ) ) ;
#222069 = CARTESIAN_POINT ( 'NONE',  ( 20.94999999999999574, 16.44800918141279311, -240.8068063186265135 ) ) ;
#222071 = ORIENTED_EDGE ( 'NONE', *, *, #174488, .T. ) ;
#222072 = EDGE_CURVE ( 'NONE', #227982, #227593, #203539, .T. ) ;
#222073 = DIRECTION ( 'NONE',  ( -0.000000000000000000, -0.000000000000000000, -1.000000000000000000 ) ) ;
#222074 = CARTESIAN_POINT ( 'NONE',  ( 20.77766267348356166, 10.44904239062959839, -141.5927089158778642 ) ) ;
#222075 = EDGE_CURVE ( 'NONE', #182052, #3876, #74396, .T. ) ;
#222076 = DIRECTION ( 'NONE',  ( 1.000000000000000000, 0.000000000000000000, 0.000000000000000000 ) ) ;
#222077 = EDGE_LOOP ( 'NONE', ( #250251, #45158, #78844, #27821 ) ) ;
#222078 = VECTOR ( 'NONE', #147054, 1000.000000000000000 ) ;
#222080 = AXIS2_PLACEMENT_3D ( 'NONE', #102085, #20031, #162109 ) ;
#222079 =( NAMED_UNIT ( * ) SI_UNIT ( $, .STERADIAN. ) SOLID_ANGLE_UNIT ( ) );
#222081 = PRODUCT_DEFINITION ( 'UNKNOWN', '', #165495, #105164 ) ;
#222083 = CIRCLE ( 'NONE', #43067, 0.2000000000000057288 ) ;
#222082 = DIRECTION ( 'NONE',  ( -1.000000000000000000, 0.000000000000000000, 0.000000000000000000 ) ) ;
#222084 = DIRECTION ( 'NONE',  ( 1.000000000000000000, -0.000000000000000000, -0.000000000000000000 ) ) ;
#222085 = ORIENTED_EDGE ( 'NONE', *, *, #92980, .T. ) ;
#222086 = DIRECTION ( 'NONE',  ( 0.000000000000000000, -1.000000000000000000, 0.000000000000000000 ) ) ;
#222087 = FACE_OUTER_BOUND ( 'NONE', #202690, .T. ) ;
#222088 = EDGE_CURVE ( 'NONE', #212939, #111810, #253413, .T. ) ;
#222089 = AXIS2_PLACEMENT_3D ( 'NONE', #80027, #179199, #115336 ) ;
#222090 = EDGE_CURVE ( 'NONE', #66196, #63643, #115800, .T. ) ;
#222091 = DIRECTION ( 'NONE',  ( 1.000000000000000000, 0.000000000000000000, 0.000000000000000000 ) ) ;
#222093 = VERTEX_POINT ( 'NONE', #91100 ) ;
#222092 = FACE_OUTER_BOUND ( 'NONE', #195943, .T. ) ;
#222094 = EDGE_CURVE ( 'NONE', #174607, #189423, #61886, .T. ) ;
#222095 = CARTESIAN_POINT ( 'NONE',  ( 20.94999999999999574, -11.41227409414968719, -3.000000000000002665 ) ) ;
#222097 = EDGE_LOOP ( 'NONE', ( #79705, #11044, #188892, #141092 ) ) ;
#222096 = DIRECTION ( 'NONE',  ( 0.000000000000000000, -0.9126074666063770380, -0.4088369013363281068 ) ) ;
#222098 = FACE_OUTER_BOUND ( 'NONE', #44571, .T. ) ;
#222100 = CARTESIAN_POINT ( 'NONE',  ( -23.25000000000000000, 11.65000000001115588, -88.75000000000004263 ) ) ;
#222099 = CIRCLE ( 'NONE', #172306, 0.09999999999998802902 ) ;
#222101 = AXIS2_PLACEMENT_3D ( 'NONE', #218710, #102598, #199169 ) ;
#222102 = CARTESIAN_POINT ( 'NONE',  ( -16.93302609847409457, 66.00331747920908754, -157.4367189891619034 ) ) ;
#222103 = CYLINDRICAL_SURFACE ( 'NONE', #152765, 0.1000000000000028644 ) ;
#222104 = AXIS2_PLACEMENT_3D ( 'NONE', #102219, #243051, #141380 ) ;
#222106 = FACE_OUTER_BOUND ( 'NONE', #228475, .T. ) ;
#222105 = CARTESIAN_POINT ( 'NONE',  ( -16.93658211146644987, 63.05737344118514187, -213.0636739456002147 ) ) ;
#222107 = CARTESIAN_POINT ( 'NONE',  ( -18.50000000000000000, -9.499999999988849808, -122.2500000000000284 ) ) ;
#222108 = FACE_OUTER_BOUND ( 'NONE', #29305, .T. ) ;
#222109 = EDGE_CURVE ( 'NONE', #219226, #22920, #114513, .T. ) ;
#222110 = CARTESIAN_POINT ( 'NONE',  ( -18.57399277249657032, 10.33112638555853913, -39.09012289269747953 ) ) ;
#222111 = DIRECTION ( 'NONE',  ( 1.000000000000000000, 0.000000000000000000, 0.000000000000000000 ) ) ;
#222112 = CARTESIAN_POINT ( 'NONE',  ( 20.94999999999999574, 6.550000000011159784, -177.3438220896831012 ) ) ;
#222113 = ORIENTED_EDGE ( 'NONE', *, *, #241856, .T. ) ;
#222114 = DIRECTION ( 'NONE',  ( -0.7071067811865475727, -0.7071067811865475727, -0.000000000000000000 ) ) ;
#222115 = ORIENTED_EDGE ( 'NONE', *, *, #192484, .F. ) ;
#222116 = EDGE_LOOP ( 'NONE', ( #166659, #238444, #228772, #257893, #247492 ) ) ;
#222117 = CARTESIAN_POINT ( 'NONE',  ( -21.02374657821575354, 11.60000000082034433, -26.57179677019813013 ) ) ;
#222118 = CARTESIAN_POINT ( 'NONE',  ( 23.24999999999999645, 70.40000000001180069, -81.92837350343744163 ) ) ;
#222119 = ORIENTED_EDGE ( 'NONE', *, *, #93708, .F. ) ;
#222121 = EDGE_CURVE ( 'NONE', #208712, #8349, #41061, .T. ) ;
#222120 = ORIENTED_EDGE ( 'NONE', *, *, #245502, .T. ) ;
#222122 = AXIS2_PLACEMENT_3D ( 'NONE', #42027, #236358, #141122 ) ;
#222123 = CIRCLE ( 'NONE', #18154, 7.799999999999993605 ) ;
#222124 = ORIENTED_EDGE ( 'NONE', *, *, #239772, .T. ) ;
#222125 = VECTOR ( 'NONE', #108414, 1000.000000000000000 ) ;
#222126 = DIRECTION ( 'NONE',  ( 0.000000000000000000, -0.8700118002898359348, 0.4930308989875165082 ) ) ;
#222127 = ORIENTED_EDGE ( 'NONE', *, *, #102304, .F. ) ;
#222128 = DIRECTION ( 'NONE',  ( 0.000000000000000000, -0.1350103645451876944, 0.9908441862701601321 ) ) ;
#222129 = DIRECTION ( 'NONE',  ( 0.000000000000000000, 0.2128009952263605065, -0.9770955615653313941 ) ) ;
#222130 = CARTESIAN_POINT ( 'NONE',  ( -16.77732147262506146, 66.05403306739317770, -82.18661624124851528 ) ) ;
#222131 = CARTESIAN_POINT ( 'NONE',  ( 20.94999999999999929, 76.00000000001247713, -174.1231074845243540 ) ) ;
#222132 = CARTESIAN_POINT ( 'NONE',  ( 18.39999999999999858, 85.51932773110452501, -129.5501311079648872 ) ) ;
#222133 = CIRCLE ( 'NONE', #30472, 0.09999999999999489853 ) ;
#222134 = EDGE_CURVE ( 'NONE', #51812, #222344, #103551, .T. ) ;
#222135 = CIRCLE ( 'NONE', #126306, 0.1000000000000017680 ) ;
#222136 = DIRECTION ( 'NONE',  ( 1.000000000000000000, 0.000000000000000000, 0.000000000000000000 ) ) ;
#222137 = CARTESIAN_POINT ( 'NONE',  ( -21.59142135623730852, 7.850000000011158718, -121.7500000000000426 ) ) ;
#222139 = ORIENTED_EDGE ( 'NONE', *, *, #223359, .F. ) ;
#222138 = DIRECTION ( 'NONE',  ( 0.000000000000000000, 0.000000000000000000, 1.000000000000000000 ) ) ;
#222141 = FACE_OUTER_BOUND ( 'NONE', #186130, .T. ) ;
#222140 = CARTESIAN_POINT ( 'NONE',  ( -20.54999999999999716, 47.91013932883114990, -242.3192343197862044 ) ) ;
#222142 = DIRECTION ( 'NONE',  ( 1.000000000000000000, 0.000000000000000000, 0.000000000000000000 ) ) ;
#222143 = VERTEX_POINT ( 'NONE', #111966 ) ;
#222144 = AXIS2_PLACEMENT_3D ( 'NONE', #194015, #113174, #191466 ) ;
#222145 = CARTESIAN_POINT ( 'NONE',  ( 21.05000000000005400, 65.35000000001120668, -4.423107484524790856 ) ) ;
#222146 = ADVANCED_FACE ( 'NONE', ( #190212 ), #153511, .F. ) ;
#222147 = ORIENTED_EDGE ( 'NONE', *, *, #55800, .F. ) ;
#222148 = CIRCLE ( 'NONE', #176414, 11.64999999999999680 ) ;
#222151 = CARTESIAN_POINT ( 'NONE',  ( -16.94445028196807002, 66.00793639031427062, -115.6304376629428106 ) ) ;
#222150 = CYLINDRICAL_SURFACE ( 'NONE', #212008, 14.30833333333333890 ) ;
#222149 = VECTOR ( 'NONE', #13315, 1000.000000000000000 ) ;
#222152 = CIRCLE ( 'NONE', #168067, 0.09999999999998898659 ) ;
#222153 = CIRCLE ( 'NONE', #213815, 0.09999999999999775735 ) ;
#222154 = CARTESIAN_POINT ( 'NONE',  ( 18.54999999999999716, 30.20632856012699108, -234.8070450048000737 ) ) ;
#222155 = VERTEX_POINT ( 'NONE', #70288 ) ;
#222156 = VECTOR ( 'NONE', #194781, 999.9999999999998863 ) ;
#222157 = ADVANCED_FACE ( 'NONE', ( #252723 ), #130208, .T. ) ;
#222158 = DIRECTION ( 'NONE',  ( -1.000000000000000000, -0.000000000000000000, -0.000000000000000000 ) ) ;
#222160 = EDGE_CURVE ( 'NONE', #209604, #112606, #250180, .T. ) ;
#222159 = CARTESIAN_POINT ( 'NONE',  ( -2.995603634470829482E-16, -11.74999999998884448, -158.7500000000000284 ) ) ;
#222161 = CARTESIAN_POINT ( 'NONE',  ( 23.14999999999999858, 1.115600667400684642E-11, -200.9999999999999432 ) ) ;
#222162 = DIRECTION ( 'NONE',  ( 0.000000000000000000, 0.000000000000000000, -1.000000000000000000 ) ) ;
#222163 = ORIENTED_EDGE ( 'NONE', *, *, #216443, .F. ) ;
#222164 = AXIS2_PLACEMENT_3D ( 'NONE', #28850, #108339, #228293 ) ;
#222165 = DIRECTION ( 'NONE',  ( -1.000000000000000000, 0.000000000000000000, 0.000000000000000000 ) ) ;
#222166 = AXIS2_PLACEMENT_3D ( 'NONE', #10080, #111753, #33544 ) ;
#222167 = SPHERICAL_SURFACE ( 'NONE', #3628, 0.1000000000000000056 ) ;
#222168 = CARTESIAN_POINT ( 'NONE',  ( 20.94999999999999929, 76.00000000001207923, -128.7231074845243484 ) ) ;
#222169 = DIRECTION ( 'NONE',  ( 0.000000000000000000, 1.000000000000000000, 2.891205793294679805E-16 ) ) ;
#222171 = EDGE_CURVE ( 'NONE', #45933, #48358, #251453, .T. ) ;
#222170 = CARTESIAN_POINT ( 'NONE',  ( 21.15000000000005187, 82.78482233730476025, -26.42994920107286916 ) ) ;
#222172 = CIRCLE ( 'NONE', #180701, 0.09999999999999939493 ) ;
#222173 = CIRCLE ( 'NONE', #109763, 0.1000000000000028644 ) ;
#222175 = VERTEX_POINT ( 'NONE', #231914 ) ;
#222174 = DIRECTION ( 'NONE',  ( 1.000000000000000000, 0.000000000000000000, 0.000000000000000000 ) ) ;
#222176 = AXIS2_PLACEMENT_3D ( 'NONE', #257757, #158745, #135281 ) ;
#222177 = CARTESIAN_POINT ( 'NONE',  ( 23.14999999999999858, 64.04577702392042227, -222.1950530992138226 ) ) ;
#222178 = CARTESIAN_POINT ( 'NONE',  ( -20.85000000000000142, -1.362429037182151470, -108.3888812479212476 ) ) ;
#222179 = DIRECTION ( 'NONE',  ( -0.7071067811865463515, 0.7071067811865487940, -0.000000000000000000 ) ) ;
#222180 = FACE_OUTER_BOUND ( 'NONE', #194210, .T. ) ;
#222181 = ADVANCED_FACE ( 'NONE', ( #33744 ), #28616, .F. ) ;
#222182 = DIRECTION ( 'NONE',  ( 1.000000000000000000, -0.000000000000000000, -0.000000000000000000 ) ) ;
#222184 = ORIENTED_EDGE ( 'NONE', *, *, #22322, .T. ) ;
#222183 = CARTESIAN_POINT ( 'NONE',  ( 21.04999999999908411, 67.22371710472090456, -57.36519848187187876 ) ) ;
#222185 = FACE_OUTER_BOUND ( 'NONE', #11984, .T. ) ;
#222186 = FACE_OUTER_BOUND ( 'NONE', #125739, .T. ) ;
#222187 = CARTESIAN_POINT ( 'NONE',  ( -23.15000000000000213, 0.000000000000000000, -35.60000000000000853 ) ) ;
#222188 = ORIENTED_EDGE ( 'NONE', *, *, #121224, .T. ) ;
#222189 = CARTESIAN_POINT ( 'NONE',  ( -14.56336952470178758, 66.55335465531700834, -151.6123010284242127 ) ) ;
#222190 = DIRECTION ( 'NONE',  ( -1.000000000000000000, 0.000000000000000000, 0.000000000000000000 ) ) ;
#222191 = EDGE_CURVE ( 'NONE', #131951, #52291, #178624, .T. ) ;
#222192 = DIRECTION ( 'NONE',  ( 1.000000000000000000, 0.000000000000000000, 0.000000000000000000 ) ) ;
#222193 = ITEM_DEFINED_TRANSFORMATION ( 'NONE', 'NONE', #156939,  #2425 ) ;
#222194 = EDGE_CURVE ( 'NONE', #190789, #243888, #175791, .T. ) ;
#222195 = DIRECTION ( 'NONE',  ( 0.000000000000000000, 0.2128009952263403282, -0.9770955615653358350 ) ) ;
#222196 = AXIS2_PLACEMENT_3D ( 'NONE', #254075, #33802, #135407 ) ;
#222197 = ORIENTED_EDGE ( 'NONE', *, *, #55829, .T. ) ;
#222198 = CARTESIAN_POINT ( 'NONE',  ( -16.82055514392389028, 9.950000000011137047, -87.82320192545805071 ) ) ;
#222199 = CIRCLE ( 'NONE', #143098, 0.1000000000000028644 ) ;
#222200 = CIRCLE ( 'NONE', #97101, 0.09999999999999736877 ) ;
#222201 = ORIENTED_EDGE ( 'NONE', *, *, #89513, .T. ) ;
#222202 = CYLINDRICAL_SURFACE ( 'NONE', #68279, 0.1000000000000028644 ) ;
#222203 = DIRECTION ( 'NONE',  ( 2.952720810173289112E-16, 1.000000000000000000, -6.088138035986627436E-46 ) ) ;
#222204 =( BOUNDED_SURFACE ( )  B_SPLINE_SURFACE ( 3, 2, ( 
 ( #240955, #64871, #80560 ),
 ( #220108, #141840, #144384 ),
 ( #44036, #27069, #239674 ),
 ( #21914, #84385, #63589 ),
 ( #145684, #223934, #122292 ),
 ( #45317, #163990, #83114 ),
 ( #126117, #244785, #160161 ),
 ( #106550, #123573, #182271 ),
 ( #121038, #101385, #200538 ),
 ( #66163, #180990, #124857 ) ),
 .UNSPECIFIED., .F., .F., .F. ) 
 B_SPLINE_SURFACE_WITH_KNOTS ( ( 4, 2, 2, 2, 4 ),
 ( 3, 3 ),
 ( 0.0001836757140119083063, 0.0004000170051583593783, 0.0005081876507315849414, 0.0005622729735181976416, 0.0006163582963048104503 ),
 ( 0.000000000000000000, 1.000000000000000000 ),
 .UNSPECIFIED. ) 
 GEOMETRIC_REPRESENTATION_ITEM ( )  RATIONAL_B_SPLINE_SURFACE ( (
 ( 1.000000000000000000, 0.7071067811865425767, 1.000000000000000000),
 ( 1.000000000000000000, 0.6461995200031245279, 1.000000000000000000),
 ( 1.000000000000000000, 0.5776453529547745935, 1.000000000000000000),
 ( 1.000000000000000000, 0.4585233068352737584, 1.000000000000000000),
 ( 1.000000000000000000, 0.4154092989937730462, 1.000000000000000000),
 ( 1.000000000000000000, 0.3550093145837215358, 1.000000000000000000),
 ( 1.000000000000000000, 0.3354498651689109545, 1.000000000000000000),
 ( 1.000000000000000000, 0.3060347992252169802, 1.000000000000000000),
 ( 1.000000000000000000, 0.2963555829629179739, 1.000000000000000000),
 ( 1.000000000000000000, 0.2966190024560962923, 1.000000000000000000) ) ) 
 REPRESENTATION_ITEM ( '' )  SURFACE ( )  );
#222205 = DIRECTION ( 'NONE',  ( 1.000000000000000000, 0.000000000000000000, 0.000000000000000000 ) ) ;
#222206 = CARTESIAN_POINT ( 'NONE',  ( -23.15000000000000213, 1.115600667400684642E-11, -71.15000000000004832 ) ) ;
#222207 = EDGE_LOOP ( 'NONE', ( #191128, #154734, #15651, #198629 ) ) ;
#222208 = ADVANCED_FACE ( 'NONE', ( #239601 ), #81764, .T. ) ;
#222209 = EDGE_CURVE ( 'NONE', #207654, #147896, #257623, .T. ) ;
#222210 = CARTESIAN_POINT ( 'NONE',  ( 20.95568717954149562, 10.60199405390297400, -175.1025083682686159 ) ) ;
#222211 = DIRECTION ( 'NONE',  ( -1.000000000000000000, -0.000000000000000000, -0.000000000000000000 ) ) ;
#222212 = DIRECTION ( 'NONE',  ( 1.000000000000000000, 0.000000000000000000, 0.000000000000000000 ) ) ;
#222213 = CARTESIAN_POINT ( 'NONE',  ( -20.94999999999999929, 64.25000000001190870, -96.00830171387039513 ) ) ;
#222214 = CARTESIAN_POINT ( 'NONE',  ( -16.87333278164143735, 9.882609784578759715, -20.36683219384677912 ) ) ;
#222215 = DIRECTION ( 'NONE',  ( -1.000000000000000000, -1.608698681449252075E-14, -3.503574203973550643E-15 ) ) ;
#222216 = EDGE_LOOP ( 'NONE', ( #253331, #201498, #37860, #174436 ) ) ;
#222218 = VERTEX_POINT ( 'NONE', #57077 ) ;
#222217 = DIRECTION ( 'NONE',  ( -0.000000000000000000, 0.000000000000000000, -1.000000000000000000 ) ) ;
#222219 = ORIENTED_EDGE ( 'NONE', *, *, #147322, .F. ) ;
#222221 = B_SPLINE_CURVE_WITH_KNOTS ( 'NONE', 3,
 ( #58428, #158864, #40207, #183545, #84376, #81827, #221354, #180978 ),
 .UNSPECIFIED., .F., .F.,
 ( 4, 2, 2, 4 ),
 ( 0.000000000000000000, 0.0001049670497870005311, 0.0002099340995740010623, 0.0004198681991479908488 ),
 .UNSPECIFIED. ) ;
#222220 = AXIS2_PLACEMENT_3D ( 'NONE', #76022, #155603, #56446 ) ;
#222222 = CARTESIAN_POINT ( 'NONE',  ( 20.94999999999999929, 76.00000000001244871, -170.0231074845243597 ) ) ;
#222223 = EDGE_LOOP ( 'NONE', ( #122779, #42993, #88977, #27881 ) ) ;
#222224 = CARTESIAN_POINT ( 'NONE',  ( 21.09096482362066993, 61.07927011738019019, -234.2275225987165754 ) ) ;
#222225 = DIRECTION ( 'NONE',  ( -4.391705002472927119E-16, -1.000000000000000000, -7.026728003956683390E-15 ) ) ;
#222226 = DIRECTION ( 'NONE',  ( 0.000000000000000000, 0.000000000000000000, 1.000000000000000000 ) ) ;
#222227 = EDGE_LOOP ( 'NONE', ( #138463, #133839, #25589, #73808 ) ) ;
#222228 = FACE_OUTER_BOUND ( 'NONE', #108048, .T. ) ;
#222229 = FACE_OUTER_BOUND ( 'NONE', #139322, .T. ) ;
#222230 = ORIENTED_EDGE ( 'NONE', *, *, #214482, .T. ) ;
#222231 = CARTESIAN_POINT ( 'NONE',  ( 22.48660254037844197, 11.65000000001115588, -100.4500000000000455 ) ) ;
#222233 = ORIENTED_EDGE ( 'NONE', *, *, #7311, .F. ) ;
#222232 = FACE_OUTER_BOUND ( 'NONE', #139779, .T. ) ;
#222234 = LINE ( 'NONE', #4486, #227416 ) ;
#222235 = CARTESIAN_POINT ( 'NONE',  ( -20.94999999999999929, 36.22908226166886436, -236.0480061918409547 ) ) ;
#222236 = AXIS2_PLACEMENT_3D ( 'NONE', #245734, #67091, #25414 ) ;
#222237 = EDGE_CURVE ( 'NONE', #168899, #18436, #165962, .T. ) ;
#222238 = AXIS2_PLACEMENT_3D ( 'NONE', #199506, #160388, #243743 ) ;
#222239 = EDGE_LOOP ( 'NONE', ( #216483, #162692, #86682, #71654 ) ) ;
#222240 = VECTOR ( 'NONE', #183315, 1000.000000000000000 ) ;
#222241 = FACE_OUTER_BOUND ( 'NONE', #222699, .T. ) ;
#222242 = CARTESIAN_POINT ( 'NONE',  ( 21.10642757222115051, 10.72315628916975250, -79.24069752378524356 ) ) ;
#222243 = CARTESIAN_POINT ( 'NONE',  ( -11.59999999999994458, 67.72071067812984779, -17.05239680640613642 ) ) ;
#222244 = ORIENTED_EDGE ( 'NONE', *, *, #142978, .T. ) ;
#222245 = DIRECTION ( 'NONE',  ( 1.186688945009009831E-16, 1.000000000000000000, 6.982962677686266711E-15 ) ) ;
#222246 = DIRECTION ( 'NONE',  ( 0.000000000000000000, 0.000000000000000000, -1.000000000000000000 ) ) ;
#222247 = ORIENTED_EDGE ( 'NONE', *, *, #256860, .F. ) ;
#222248 = TOROIDAL_SURFACE ( 'NONE', #109839, 4.041421356237307805, 0.1000000000000000056 ) ;
#222249 = EDGE_CURVE ( 'NONE', #46846, #202163, #199190, .T. ) ;
#222250 = CIRCLE ( 'NONE', #205702, 0.09999999999999609201 ) ;
#222251 = AXIS2_PLACEMENT_3D ( 'NONE', #247318, #64830, #186078 ) ;
#222252 = EDGE_LOOP ( 'NONE', ( #217521, #11496, #236652, #46115 ) ) ;
#222253 = AXIS2_PLACEMENT_3D ( 'NONE', #135436, #74232, #152475 ) ;
#222254 = ORIENTED_EDGE ( 'NONE', *, *, #253872, .T. ) ;
#222255 = CARTESIAN_POINT ( 'NONE',  ( 18.54148534481893762, 10.32532329026771123, -39.06993430183595706 ) ) ;
#222256 = LINE ( 'NONE', #184439, #29531 ) ;
#222258 = VERTEX_POINT ( 'NONE', #60945 ) ;
#222257 = CARTESIAN_POINT ( 'NONE',  ( -16.80468759584937288, 9.942153675145293690, -146.6900188662016546 ) ) ;
#222259 = DIRECTION ( 'NONE',  ( 1.000000000000000000, 0.000000000000000000, 0.000000000000000000 ) ) ;
#222260 = CARTESIAN_POINT ( 'NONE',  ( -20.94999999999999929, 5.900000000011102586, -110.7190997646564483 ) ) ;
#222261 = CARTESIAN_POINT ( 'NONE',  ( -20.54999999999999716, 70.76939748184450707, -215.3970883796142743 ) ) ;
#222262 = CARTESIAN_POINT ( 'NONE',  ( -16.88005004766534967, 51.61912858099893242, -231.9462398806007286 ) ) ;
#222263 = DIRECTION ( 'NONE',  ( 0.000000000000000000, 1.000000000000000000, 0.000000000000000000 ) ) ;
#222264 = CIRCLE ( 'NONE', #109856, 2.599999999999998312 ) ;
#222266 = ORIENTED_EDGE ( 'NONE', *, *, #189520, .F. ) ;
#222265 = CARTESIAN_POINT ( 'NONE',  ( 20.94999999999999574, 74.16465844978745281, -91.46795619196133487 ) ) ;
#222268 = ORIENTED_EDGE ( 'NONE', *, *, #80158, .F. ) ;
#222267 = CARTESIAN_POINT ( 'NONE',  ( 20.94999999999999929, -8.730841121484166578, -57.40192528101566438 ) ) ;
#222270 = CARTESIAN_POINT ( 'NONE',  ( -23.15000000000000213, 87.65000000001215597, -139.6231074845242688 ) ) ;
#222269 = CIRCLE ( 'NONE', #143172, 0.09999999999999939493 ) ;
#222271 = ORIENTED_EDGE ( 'NONE', *, *, #117861, .F. ) ;
#222272 = DIRECTION ( 'NONE',  ( 0.000000000000000000, 0.2128009952263601456, -0.9770955615653316162 ) ) ;
#222273 = DIRECTION ( 'NONE',  ( 1.000000000000000000, 0.000000000000000000, 0.000000000000000000 ) ) ;
#222274 = VECTOR ( 'NONE', #181740, 1000.000000000000000 ) ;
#222275 = CARTESIAN_POINT ( 'NONE',  ( -23.15000000000000213, 49.57218508014541669, -254.1759139559835035 ) ) ;
#222276 = FACE_OUTER_BOUND ( 'NONE', #42344, .T. ) ;
#222277 = CARTESIAN_POINT ( 'NONE',  ( 20.97217846901852312, 67.12455827530294528, -195.0218798005872145 ) ) ;
#222278 = CIRCLE ( 'NONE', #255587, 0.1999999999999945155 ) ;
#222279 = ORIENTED_EDGE ( 'NONE', *, *, #133197, .T. ) ;
#222281 = AXIS2_PLACEMENT_3D ( 'NONE', #3818, #42949, #65071 ) ;
#222280 = DIRECTION ( 'NONE',  ( 0.000000000000000000, 0.9274965247785529332, 0.3738317757009255171 ) ) ;
#222282 = VERTEX_POINT ( 'NONE', #156236 ) ;
#222283 = ORIENTED_EDGE ( 'NONE', *, *, #84670, .T. ) ;
#222284 = CARTESIAN_POINT ( 'NONE',  ( -21.55000000000000071, 68.65000000001229807, -157.6731074845243938 ) ) ;
#222285 = EDGE_CURVE ( 'NONE', #138829, #101113, #161357, .T. ) ;
#222286 = ORIENTED_EDGE ( 'NONE', *, *, #4302, .T. ) ;
#222287 = CARTESIAN_POINT ( 'NONE',  ( -12.47155713865592475, 66.62433047358575777, -53.65531747513846739 ) ) ;
#222288 =( BOUNDED_CURVE ( )  B_SPLINE_CURVE ( 3, ( #57769, #40822, #156917, #257216 ),
 .UNSPECIFIED., .F., .T. ) 
 B_SPLINE_CURVE_WITH_KNOTS ( ( 4, 4 ),
 ( 3.141592653589791784, 4.712388980384688786 ),
 .UNSPECIFIED. ) 
 CURVE ( )  GEOMETRIC_REPRESENTATION_ITEM ( )  RATIONAL_B_SPLINE_CURVE ( ( 1.000000000000000000, 0.8047378541243649375, 0.8047378541243649375, 1.000000000000000000 ) ) 
 REPRESENTATION_ITEM ( '' )  );
#222289 = CARTESIAN_POINT ( 'NONE',  ( 20.94999999999999929, 5.500000000011153745, -54.59473398108690390 ) ) ;
#222290 = ADVANCED_FACE ( 'NONE', ( #98756 ), #178364, .F. ) ;
#222291 = ORIENTED_EDGE ( 'NONE', *, *, #189432, .F. ) ;
#222292 = DIRECTION ( 'NONE',  ( 1.000000000000000000, 0.000000000000000000, 0.000000000000000000 ) ) ;
#222293 = ORIENTED_EDGE ( 'NONE', *, *, #182313, .T. ) ;
#222294 = CARTESIAN_POINT ( 'NONE',  ( -14.87779219673428699, 9.430633469083952392, -48.73176579482408499 ) ) ;
#222295 = VERTEX_POINT ( 'NONE', #16712 ) ;
#222296 = EDGE_CURVE ( 'NONE', #232305, #235554, #139183, .T. ) ;
#222297 = DIRECTION ( 'NONE',  ( 2.952720810173289112E-16, -1.000000000000000000, 0.000000000000000000 ) ) ;
#222298 = CIRCLE ( 'NONE', #18331, 4.000000000000000000 ) ;
#222299 = DIRECTION ( 'NONE',  ( 0.000000000000000000, -0.2128009952263403282, 0.9770955615653358350 ) ) ;
#222300 = ORIENTED_EDGE ( 'NONE', *, *, #133410, .T. ) ;
#222301 = CIRCLE ( 'NONE', #97409, 0.1000000000000028644 ) ;
#222302 = DIRECTION ( 'NONE',  ( 0.000000000000000000, 2.168404344970946942E-15, 1.000000000000000000 ) ) ;
#222303 = EDGE_CURVE ( 'NONE', #175608, #217189, #3607, .T. ) ;
#222305 = ORIENTED_EDGE ( 'NONE', *, *, #54911, .F. ) ;
#222304 = LINE ( 'NONE', #123239, #226291 ) ;
#222306 = CIRCLE ( 'NONE', #197390, 12.97499999999998366 ) ;
#222307 = CARTESIAN_POINT ( 'NONE',  ( -22.39999999999999858, 76.10085836911147794, -215.2726746080137445 ) ) ;
#222308 = ORIENTED_EDGE ( 'NONE', *, *, #45806, .F. ) ;
#222309 = AXIS2_PLACEMENT_3D ( 'NONE', #109223, #49257, #15292 ) ;
#222310 = LINE ( 'NONE', #38579, #223925 ) ;
#222311 = EDGE_LOOP ( 'NONE', ( #51755, #98387, #25262, #228358 ) ) ;
#222312 = DIRECTION ( 'NONE',  ( -1.000000000000000000, 0.000000000000000000, -0.000000000000000000 ) ) ;
#222313 = ADVANCED_FACE ( 'NONE', ( #117087 ), #257816, .F. ) ;
#222314 = CARTESIAN_POINT ( 'NONE',  ( 20.01093837587850288, 64.25000000001250555, -178.7687100499268240 ) ) ;
#222315 = DIRECTION ( 'NONE',  ( -1.000000000000000000, 0.000000000000000000, -0.000000000000000000 ) ) ;
#222316 = FACE_OUTER_BOUND ( 'NONE', #23596, .T. ) ;
#222317 = VECTOR ( 'NONE', #59578, 1000.000000000000000 ) ;
#222318 = CARTESIAN_POINT ( 'NONE',  ( -13.43673303185030221, 66.55335100938371795, -188.4339441886012025 ) ) ;
#222319 = DIRECTION ( 'NONE',  ( 1.000000000000000000, 0.000000000000000000, 0.000000000000000000 ) ) ;
#222320 = AXIS2_PLACEMENT_3D ( 'NONE', #234280, #76489, #250007 ) ;
#222321 = ORIENTED_EDGE ( 'NONE', *, *, #79344, .F. ) ;
#222322 = CARTESIAN_POINT ( 'NONE',  ( -20.94999999999999929, 68.97833521811233481, -166.1895420826271277 ) ) ;
#222323 = AXIS2_PLACEMENT_3D ( 'NONE', #201711, #197855, #236999 ) ;
#222324 = DIRECTION ( 'NONE',  ( 2.952720810173289112E-16, 1.000000000000000000, 6.467318590049456648E-15 ) ) ;
#222325 = CARTESIAN_POINT ( 'NONE',  ( 21.07928932188134397, 6.328516656404468144, -100.4011048543456468 ) ) ;
#222327 = CARTESIAN_POINT ( 'NONE',  ( 21.22070241538126467, 1.472315254537094553, -230.5904421098591968 ) ) ;
#222326 = VECTOR ( 'NONE', #31011, 1000.000000000000000 ) ;
#222328 = ORIENTED_EDGE ( 'NONE', *, *, #13192, .T. ) ;
#222329 = CARTESIAN_POINT ( 'NONE',  ( -21.07928932188134041, 75.90110485435761234, -109.3516241409176075 ) ) ;
#222330 = ORIENTED_EDGE ( 'NONE', *, *, #107077, .F. ) ;
#222331 = CARTESIAN_POINT ( 'NONE',  ( 13.22261339317536333, 9.436552840015579591, -115.6779554727603312 ) ) ;
#222333 = ORIENTED_EDGE ( 'NONE', *, *, #165324, .T. ) ;
#222332 = CIRCLE ( 'NONE', #118330, 0.09999999999999824307 ) ;
#222334 = FACE_OUTER_BOUND ( 'NONE', #245173, .T. ) ;
#222335 = DIRECTION ( 'NONE',  ( 0.000000000000000000, -4.562560375171877784E-14, 1.000000000000000000 ) ) ;
#222336 = ORIENTED_EDGE ( 'NONE', *, *, #109984, .F. ) ;
#222338 = VERTEX_POINT ( 'NONE', #42673 ) ;
#222337 = CARTESIAN_POINT ( 'NONE',  ( -20.94999999999994245, 67.85000000001119247, -3.123107484524795474 ) ) ;
#222339 = DIRECTION ( 'NONE',  ( 1.000000000000000000, -7.304098846218134667E-16, -5.100424963727256530E-30 ) ) ;
#222340 = ORIENTED_EDGE ( 'NONE', *, *, #140296, .F. ) ;
#222341 = TOROIDAL_SURFACE ( 'NONE', #164135, 0.2000000000000000111, 0.1000000000000000056 ) ;
#222342 = CARTESIAN_POINT ( 'NONE',  ( 21.15000000000005187, 77.85126707825561709, -47.62635315998165453 ) ) ;
#222343 = DIRECTION ( 'NONE',  ( 0.000000000000000000, 0.9594490217226113726, 0.2818822000686178608 ) ) ;
#222344 = VERTEX_POINT ( 'NONE', #97482 ) ;
#222345 = ORIENTED_EDGE ( 'NONE', *, *, #171384, .T. ) ;
#222346 = CIRCLE ( 'NONE', #72373, 0.09999999999999939493 ) ;
#222347 = CARTESIAN_POINT ( 'NONE',  ( -20.54999999999999716, 73.60000000001157616, -56.29848556176223440 ) ) ;
#222348 = CARTESIAN_POINT ( 'NONE',  ( -16.89268316805466341, 66.04827818676987761, -123.8788599630699281 ) ) ;
#222350 = EDGE_LOOP ( 'NONE', ( #170025, #255938, #89043, #6560 ) ) ;
#222349 = AXIS2_PLACEMENT_3D ( 'NONE', #2701, #101778, #144770 ) ;
#222351 = ORIENTED_EDGE ( 'NONE', *, *, #178234, .F. ) ;
#222352 = EDGE_CURVE ( 'NONE', #257429, #4495, #45312, .T. ) ;
#222353 = AXIS2_PLACEMENT_3D ( 'NONE', #136242, #20191, #37195 ) ;
#222354 = CARTESIAN_POINT ( 'NONE',  ( 18.59999999999999076, 65.79142135624910281, -81.77310748452437394 ) ) ;
#222355 = EDGE_CURVE ( 'NONE', #81533, #224911, #87667, .T. ) ;
#222357 = ORIENTED_EDGE ( 'NONE', *, *, #37735, .T. ) ;
#222356 = LINE ( 'NONE', #164982, #26622 ) ;
#222358 = DIRECTION ( 'NONE',  ( 0.5000000000001140199, 0.1842910678166251592, -0.8461895782405347566 ) ) ;
#222359 = CYLINDRICAL_SURFACE ( 'NONE', #256474, 0.09999999999999939493 ) ;
#222360 = CARTESIAN_POINT ( 'NONE',  ( -23.25000000000000000, 76.00000000001170974, -69.52310748452431710 ) ) ;
#222362 = LINE ( 'NONE', #240674, #116003 ) ;
#222361 = CARTESIAN_POINT ( 'NONE',  ( -18.37013991200266005, 64.50025238380011672, -127.3161304950415058 ) ) ;
#222364 = ADVANCED_FACE ( 'NONE', ( #68667 ), #174355, .F. ) ;
#222363 = CARTESIAN_POINT ( 'NONE',  ( -20.93302460841142931, 65.68434038414410736, -164.4866880726065972 ) ) ;
#222365 = DIRECTION ( 'NONE',  ( 0.000000000000000000, 1.000000000000000000, 6.853228547068871147E-15 ) ) ;
#222366 = DIRECTION ( 'NONE',  ( 0.000000000000000000, 1.000000000000000000, 6.938893903907222067E-15 ) ) ;
#222367 = VECTOR ( 'NONE', #231310, 1000.000000000000000 ) ;
#222368 = DIRECTION ( 'NONE',  ( 0.000000000000000000, 0.000000000000000000, 1.000000000000000000 ) ) ;
#222369 = VECTOR ( 'NONE', #93361, 1000.000000000000227 ) ;
#222370 = VECTOR ( 'NONE', #158301, 1000.000000000000000 ) ;
#222371 = VERTEX_POINT ( 'NONE', #203023 ) ;
#222372 = B_SPLINE_CURVE_WITH_KNOTS ( 'NONE', 3,
 ( #219177, #82210, #3990, #122684, #78386, #18423, #21020, #19724, #40597, #41865, #199654, #161814, #157982, #177540, #100493, #180078 ),
 .UNSPECIFIED., .F., .F.,
 ( 4, 3, 3, 3, 3, 4 ),
 ( 0.000000000000000000, 2.372700795692865946E-05, 5.739057815865495515E-05, 9.073899019180231584E-05, 0.0001243544287365729863, 0.0001585386695601217349 ),
 .UNSPECIFIED. ) ;
#222373 = VERTEX_POINT ( 'NONE', #145610 ) ;
#222374 = DIRECTION ( 'NONE',  ( 1.000000000000000000, 0.000000000000000000, 0.000000000000000000 ) ) ;
#222375 = EDGE_CURVE ( 'NONE', #101099, #187124, #236831, .T. ) ;
#222376 = ORIENTED_EDGE ( 'NONE', *, *, #174078, .T. ) ;
#222377 = CARTESIAN_POINT ( 'NONE',  ( -16.87435696428308063, 9.950002462943377424, -146.6499917651665896 ) ) ;
#222378 = EDGE_CURVE ( 'NONE', #64314, #26511, #195182, .T. ) ;
#222379 = ORIENTED_EDGE ( 'NONE', *, *, #154771, .T. ) ;
#222380 = CARTESIAN_POINT ( 'NONE',  ( 18.39999999999997371, 33.92263863280957281, -235.0698407953532296 ) ) ;
#222381 = ORIENTED_EDGE ( 'NONE', *, *, #145636, .F. ) ;
#222382 = DIRECTION ( 'NONE',  ( 1.000000000000000000, -0.000000000000000000, -0.000000000000000000 ) ) ;
#222383 = VERTEX_POINT ( 'NONE', #24426 ) ;
#222384 = ORIENTED_EDGE ( 'NONE', *, *, #206725, .F. ) ;
#222385 = ADVANCED_FACE ( 'NONE', ( #165192 ), #88187, .T. ) ;
#222386 = CARTESIAN_POINT ( 'NONE',  ( -23.15000000000000213, 4.250000000011156409, -188.7499999999999716 ) ) ;
#222387 = CIRCLE ( 'NONE', #55802, 0.2000000000000057288 ) ;
#222388 = FACE_OUTER_BOUND ( 'NONE', #36707, .T. ) ;
#222390 = ORIENTED_EDGE ( 'NONE', *, *, #85818, .T. ) ;
#222389 = CARTESIAN_POINT ( 'NONE',  ( -23.15000000000000213, 11.65000000001115588, -179.7499999999999716 ) ) ;
#222391 = EDGE_CURVE ( 'NONE', #44944, #178909, #167789, .T. ) ;
#222392 = CARTESIAN_POINT ( 'NONE',  ( 5.899999999999996803, -11.75000000000000000, 13.90000000000000213 ) ) ;
#222394 = ORIENTED_EDGE ( 'NONE', *, *, #222088, .F. ) ;
#222393 = CARTESIAN_POINT ( 'NONE',  ( 20.95462737510932882, 10.55678195165489441, -141.5699500565623055 ) ) ;
#222395 = CARTESIAN_POINT ( 'NONE',  ( -21.30740335185486245, 0.09893452578700702438, -60.44334207797204073 ) ) ;
#222397 = EDGE_CURVE ( 'NONE', #224848, #96608, #128523, .T. ) ;
#222396 = ORIENTED_EDGE ( 'NONE', *, *, #231385, .T. ) ;
#222398 = DIRECTION ( 'NONE',  ( 1.000000000000000000, 0.000000000000000000, 0.000000000000000000 ) ) ;
#222400 = ORIENTED_EDGE ( 'NONE', *, *, #104047, .F. ) ;
#222399 = CARTESIAN_POINT ( 'NONE',  ( 18.49999999999999645, 1.162701749949165642, -75.10000000000003695 ) ) ;
#222401 = CYLINDRICAL_SURFACE ( 'NONE', #118028, 0.1000000000000028644 ) ;
#222402 = CARTESIAN_POINT ( 'NONE',  ( -21.29999999999995808, 40.35498466150055918, -247.8953732508333587 ) ) ;
#222403 = DIRECTION ( 'NONE',  ( -0.000000000000000000, 0.1350103645451974088, -0.9908441862701587999 ) ) ;
#222404 = ORIENTED_EDGE ( 'NONE', *, *, #118735, .F. ) ;
#222406 = CARTESIAN_POINT ( 'NONE',  ( 20.30466543256828160, 9.304236939266628426, -108.7536626513920197 ) ) ;
#222405 = CARTESIAN_POINT ( 'NONE',  ( -23.15000000000000213, 0.000000000000000000, -33.50000000000000000 ) ) ;
#222407 = CARTESIAN_POINT ( 'NONE',  ( -20.15000000000000568, 9.291421356248463326, -179.7499999999999716 ) ) ;
#222408 = AXIS2_PLACEMENT_3D ( 'NONE', #58757, #233581, #35407 ) ;
#222409 = CARTESIAN_POINT ( 'NONE',  ( 21.13461538461538325, 10.61458296203669249, -146.3500000000000227 ) ) ;
#222410 = AXIS2_PLACEMENT_3D ( 'NONE', #30828, #110333, #225128 ) ;
#222411 = DIRECTION ( 'NONE',  ( -1.000000000000000000, -0.000000000000000000, 0.000000000000000000 ) ) ;
#222412 = DIRECTION ( 'NONE',  ( -1.000000000000000000, 0.000000000000000000, -0.000000000000000000 ) ) ;
#222413 = ORIENTED_EDGE ( 'NONE', *, *, #5820, .T. ) ;
#222414 = VERTEX_POINT ( 'NONE', #6099 ) ;
#222415 = ORIENTED_EDGE ( 'NONE', *, *, #99075, .F. ) ;
#222416 = CIRCLE ( 'NONE', #110022, 0.09999999999999939493 ) ;
#222417 = CARTESIAN_POINT ( 'NONE',  ( -18.59999999999999787, 4.193200906077805712, -212.0298262072164164 ) ) ;
#222419 = VERTEX_POINT ( 'NONE', #66087 ) ;
#222418 = ADVANCED_FACE ( 'NONE', ( #244710 ), #183478, .T. ) ;
#222420 = CARTESIAN_POINT ( 'NONE',  ( 23.14999999999999858, 1.115600667400684642E-11, -67.00000000000000000 ) ) ;
#222421 = ORIENTED_EDGE ( 'NONE', *, *, #23685, .F. ) ;
#222422 = ADVANCED_FACE ( 'NONE', ( #243438 ), #206885, .F. ) ;
#222423 = CARTESIAN_POINT ( 'NONE',  ( 18.50000000000000000, -7.695243320584908453, -209.8393003250734523 ) ) ;
#222424 = DIRECTION ( 'NONE',  ( -1.000000000000000000, 0.000000000000000000, 0.000000000000000000 ) ) ;
#222426 = ADVANCED_FACE ( 'NONE', ( #102615 ), #223859, .T. ) ;
#222425 = ORIENTED_EDGE ( 'NONE', *, *, #22240, .F. ) ;
#222427 = AXIS2_PLACEMENT_3D ( 'NONE', #202409, #66760, #65459 ) ;
#222428 = DIRECTION ( 'NONE',  ( 0.000000000000000000, 0.000000000000000000, -1.000000000000000000 ) ) ;
#222429 = CIRCLE ( 'NONE', #118430, 0.1000000000000124678 ) ;
#222430 = ORIENTED_EDGE ( 'NONE', *, *, #159249, .T. ) ;
#222431 = ORIENTED_EDGE ( 'NONE', *, *, #147450, .T. ) ;
#222432 = AXIS2_PLACEMENT_3D ( 'NONE', #254382, #32840, #13248 ) ;
#222434 = ORIENTED_EDGE ( 'NONE', *, *, #27548, .T. ) ;
#222433 = B_SPLINE_CURVE_WITH_KNOTS ( 'NONE', 3,
 ( #5061, #243705, #239868, #61218, #39112, #140752, #118649, #59908, #220307, #228958, #224129, #32062, #171578, #211972, #65066, #251067, #230233, #189830, #111578, #29506, #149439, #144586, #69904, #45503, #50294, #132427, #92002, #12493, #90713, #30779 ),
 .UNSPECIFIED., .F., .F.,
 ( 4, 2, 2, 2, 2, 2, 2, 2, 2, 2, 2, 2, 2, 2, 4 ),
 ( 0.000000000000000000, 0.0003422764154113552447, 0.0006845528308227104893, 0.001026829246234067794, 0.001369105661645424882, 0.002053658492468080510, 0.002738211323290736139, 0.003080487738702061135, 0.003422764154113386997, 0.003765040569524712426, 0.004107316984936037856, 0.004449593400347363718, 0.004791869815758688714, 0.005134146231170014577, 0.005476422646581339572 ),
 .UNSPECIFIED. ) ;
#222435 = AXIS2_PLACEMENT_3D ( 'NONE', #15208, #17739, #212124 ) ;
#222436 = DIRECTION ( 'NONE',  ( 0.000000000000000000, 0.000000000000000000, 1.000000000000000000 ) ) ;
#222437 = CARTESIAN_POINT ( 'NONE',  ( -21.05000000000000071, 1.148907358139439339E-11, -201.0000000000015064 ) ) ;
#222438 = DIRECTION ( 'NONE',  ( -0.000000000000000000, 1.000000000000000000, -0.000000000000000000 ) ) ;
#222439 = AXIS2_PLACEMENT_3D ( 'NONE', #120284, #199803, #100644 ) ;
#222440 = DIRECTION ( 'NONE',  ( 1.000000000000000000, 0.000000000000000000, 0.000000000000000000 ) ) ;
#222441 = LINE ( 'NONE', #204180, #10939 ) ;
#222442 = CARTESIAN_POINT ( 'NONE',  ( -23.15000000000000213, 64.25000000001156764, -57.37310748452440379 ) ) ;
#222444 = CARTESIAN_POINT ( 'NONE',  ( 20.04142135623730070, 2.319530388122574394, -217.8268657444419887 ) ) ;
#222443 = FACE_OUTER_BOUND ( 'NONE', #111269, .T. ) ;
#222445 = DIRECTION ( 'NONE',  ( 0.000000000000000000, 0.000000000000000000, -1.000000000000000000 ) ) ;
#222447 = ORIENTED_EDGE ( 'NONE', *, *, #5730, .F. ) ;
#222446 = DIRECTION ( 'NONE',  ( 0.000000000000000000, 0.000000000000000000, 1.000000000000000000 ) ) ;
#222449 = CARTESIAN_POINT ( 'NONE',  ( 18.59999999999999076, -1.851617760457748618, -78.60318971960367662 ) ) ;
#222448 = CARTESIAN_POINT ( 'NONE',  ( -16.87331047859649757, 9.950000000011138823, -188.3499999999999659 ) ) ;
#222450 = CARTESIAN_POINT ( 'NONE',  ( 20.94999999999999574, -11.64999999999999147, -3.100000000000001865 ) ) ;
#222451 = VERTEX_POINT ( 'NONE', #26993 ) ;
#222452 = CYLINDRICAL_SURFACE ( 'NONE', #246317, 0.09999999999999939493 ) ;
#222454 = CIRCLE ( 'NONE', #64268, 0.2000000000000057288 ) ;
#222453 = DIRECTION ( 'NONE',  ( 0.000000000000000000, 0.000000000000000000, -1.000000000000000000 ) ) ;
#222456 = EDGE_CURVE ( 'NONE', #115127, #247461, #232603, .T. ) ;
#222455 = FACE_OUTER_BOUND ( 'NONE', #52370, .T. ) ;
#222457 = CIRCLE ( 'NONE', #176710, 0.2000000000000057288 ) ;
#222458 = ORIENTED_EDGE ( 'NONE', *, *, #147919, .F. ) ;
#222459 = AXIS2_PLACEMENT_3D ( 'NONE', #189886, #111630, #248569 ) ;
#222460 = EDGE_CURVE ( 'NONE', #118577, #24660, #166157, .T. ) ;
#222461 = CIRCLE ( 'NONE', #197356, 0.9000000000000014655 ) ;
#222462 = CARTESIAN_POINT ( 'NONE',  ( -20.54999999999999716, 2.500000000011154633, -53.77537807723790309 ) ) ;
#222463 = CARTESIAN_POINT ( 'NONE',  ( 20.27550659511089037, 9.216043722520002035, -121.3500000000000227 ) ) ;
#222464 = VERTEX_POINT ( 'NONE', #107781 ) ;
#222465 = ORIENTED_EDGE ( 'NONE', *, *, #108987, .T. ) ;
#222466 = EDGE_CURVE ( 'NONE', #159346, #245418, #187339, .T. ) ;
#222467 = AXIS2_PLACEMENT_3D ( 'NONE', #178436, #140548, #40209 ) ;
#222469 = EDGE_CURVE ( 'NONE', #132417, #28509, #74008, .T. ) ;
#222468 = DIRECTION ( 'NONE',  ( 0.000000000000000000, 0.3896596508880098009, 0.9209589331071360574 ) ) ;
#222470 = VERTEX_POINT ( 'NONE', #242152 ) ;
#222471 = CARTESIAN_POINT ( 'NONE',  ( 23.15000000000000213, 87.65000000001195701, -103.0231074845242318 ) ) ;
#222472 = CARTESIAN_POINT ( 'NONE',  ( -18.48179518608866445, -9.518325300483311935, -174.3897055767653512 ) ) ;
#222473 = DIRECTION ( 'NONE',  ( -1.000000000000000000, 2.849773892568378313E-16, -7.728835255496647986E-17 ) ) ;
#222474 = CARTESIAN_POINT ( 'NONE',  ( -21.65000000000000213, 7.250000000011138646, -87.85000000000003695 ) ) ;
#222475 = ORIENTED_EDGE ( 'NONE', *, *, #134535, .F. ) ;
#222476 = AXIS2_PLACEMENT_3D ( 'NONE', #237098, #178433, #200531 ) ;
#222477 = EDGE_CURVE ( 'NONE', #242536, #61026, #161471, .T. ) ;
#222478 = AXIS2_PLACEMENT_3D ( 'NONE', #199143, #217401, #17924 ) ;
#222479 = CARTESIAN_POINT ( 'NONE',  ( 21.05000000000000071, 5.400000000011154988, -79.40526601891313874 ) ) ;
#222480 = LINE ( 'NONE', #148109, #237442 ) ;
#222481 = DIRECTION ( 'NONE',  ( 0.000000000000000000, 1.000000000000000000, 0.000000000000000000 ) ) ;
#222482 = DIRECTION ( 'NONE',  ( 0.000000000000000000, -6.982962677686266711E-15, 1.000000000000000000 ) ) ;
#222483 = EDGE_CURVE ( 'NONE', #130735, #31072, #66156, .T. ) ;
#222484 = ORIENTED_EDGE ( 'NONE', *, *, #85959, .T. ) ;
#222485 = EDGE_CURVE ( 'NONE', #156163, #116539, #152828, .T. ) ;
#222487 = EDGE_LOOP ( 'NONE', ( #223874, #190358, #128155 ) ) ;
#222486 = DIRECTION ( 'NONE',  ( 0.000000000000000000, -0.9910827722268049644, 0.1332476588733589318 ) ) ;
#222488 = CARTESIAN_POINT ( 'NONE',  ( 18.49999999999998934, 54.96412023489455834, -230.1191065505896063 ) ) ;
#222489 = CARTESIAN_POINT ( 'NONE',  ( 18.50000000000000000, -7.714568254029292582, -236.5586399380298985 ) ) ;
#222490 = EDGE_CURVE ( 'NONE', #143687, #250542, #186415, .T. ) ;
#222491 = LINE ( 'NONE', #184666, #212761 ) ;
#222492 = DIRECTION ( 'NONE',  ( 1.000000000000000000, 0.000000000000000000, 0.000000000000000000 ) ) ;
#222493 = DIRECTION ( 'NONE',  ( 0.000000000000000000, 0.000000000000000000, -1.000000000000000000 ) ) ;
#222494 = DIRECTION ( 'NONE',  ( 1.000000000000000000, -0.000000000000000000, -0.000000000000000000 ) ) ;
#222495 = VERTEX_POINT ( 'NONE', #229027 ) ;
#222496 = CARTESIAN_POINT ( 'NONE',  ( 20.85000000000000142, 76.00000000001239187, -162.2231074845243768 ) ) ;
#222497 = AXIS2_PLACEMENT_3D ( 'NONE', #10607, #253051, #69304 ) ;
#222498 = CARTESIAN_POINT ( 'NONE',  ( -21.04999999999994387, 65.35000000001120668, -4.623107484524796362 ) ) ;
#222499 = CARTESIAN_POINT ( 'NONE',  ( 15.07585980824113037, 9.417632963117446465, -51.64894846573224640 ) ) ;
#222501 = VECTOR ( 'NONE', #79580, 1000.000000000000000 ) ;
#222500 = SPHERICAL_SURFACE ( 'NONE', #29952, 0.1000000000000000056 ) ;
#222502 = AXIS2_PLACEMENT_3D ( 'NONE', #40146, #218727, #139185 ) ;
#222503 = ADVANCED_FACE ( 'NONE', ( #32125 ), #98872, .T. ) ;
#222504 = DIRECTION ( 'NONE',  ( -0.000000000000000000, -0.000000000000000000, -1.000000000000000000 ) ) ;
#222505 = CYLINDRICAL_SURFACE ( 'NONE', #44970, 0.1000000000000033362 ) ;
#222506 = EDGE_LOOP ( 'NONE', ( #13012, #242610, #198154, #4271, #20378, #162069 ) ) ;
#222507 = ORIENTED_EDGE ( 'NONE', *, *, #97780, .T. ) ;
#222508 = DIRECTION ( 'NONE',  ( 0.000000000000000000, 0.2617529984165152257, 0.9651348961777124202 ) ) ;
#222509 = AXIS2_PLACEMENT_3D ( 'NONE', #80857, #203402, #220402 ) ;
#222510 = CARTESIAN_POINT ( 'NONE',  ( -16.27683809663751191, 66.65000000001262492, -190.9731074845244336 ) ) ;
#222511 = EDGE_CURVE ( 'NONE', #146352, #117463, #41241, .T. ) ;
#222512 = DIRECTION ( 'NONE',  ( 0.000000000000000000, 0.9126074666063660468, 0.4088369013363524762 ) ) ;
#222513 = AXIS2_PLACEMENT_3D ( 'NONE', #72388, #112782, #189747 ) ;
#222514 = CARTESIAN_POINT ( 'NONE',  ( -16.92989143108098204, 23.18300089227618344, -231.0448406408646917 ) ) ;
#222515 = VERTEX_POINT ( 'NONE', #129902 ) ;
#222517 = EDGE_CURVE ( 'NONE', #116136, #177617, #170379, .T. ) ;
#222516 = DIRECTION ( 'NONE',  ( 0.000000000000000000, -6.982962677686266711E-15, 1.000000000000000000 ) ) ;
#222518 = TOROIDAL_SURFACE ( 'NONE', #255814, 0.2000000000000000111, 0.1000000000000000056 ) ;
#222519 = EDGE_CURVE ( 'NONE', #212431, #13073, #50350, .T. ) ;
#222521 = VECTOR ( 'NONE', #139000, 1000.000000000000000 ) ;
#222520 = DIRECTION ( 'NONE',  ( 0.000000000000000000, -3.729655473350132098E-14, -1.000000000000000000 ) ) ;
#222522 = CARTESIAN_POINT ( 'NONE',  ( 23.14999999999998437, 1.115600667400684642E-11, -167.4999999999999716 ) ) ;
#222523 = AXIS2_PLACEMENT_3D ( 'NONE', #28246, #149466, #26959 ) ;
#222524 = AXIS2_PLACEMENT_3D ( 'NONE', #34540, #158355, #155779 ) ;
#222525 = PRODUCT_DEFINITION_SHAPE ( 'NONE', 'NONE',  #258124 ) ;
#222526 = CARTESIAN_POINT ( 'NONE',  ( 18.52928932188133970, 63.76258513157054608, -209.3739165141045078 ) ) ;
#222527 = ORIENTED_EDGE ( 'NONE', *, *, #136757, .F. ) ;
#222528 = CYLINDRICAL_SURFACE ( 'NONE', #115083, 0.1000000000000028644 ) ;
#222529 = ORIENTED_EDGE ( 'NONE', *, *, #117676, .F. ) ;
#222530 = EDGE_CURVE ( 'NONE', #256921, #5569, #211352, .T. ) ;
#222531 = PLANE ( 'NONE',  #84909 ) ;
#222532 = CARTESIAN_POINT ( 'NONE',  ( -18.40000000000000213, 11.75000000001113953, -91.25000000000005684 ) ) ;
#222534 = AXIS2_PLACEMENT_3D ( 'NONE', #76264, #198781, #117970 ) ;
#222533 = CARTESIAN_POINT ( 'NONE',  ( -21.04999999999839133, 10.20950081962639544, -228.0124793259371359 ) ) ;
#222535 = CARTESIAN_POINT ( 'NONE',  ( 18.49999999999998934, 19.85039924724470950, -169.7803030578013477 ) ) ;
#222536 = DIRECTION ( 'NONE',  ( 1.000000000000000000, 0.000000000000000000, 0.000000000000000000 ) ) ;
#222537 = LINE ( 'NONE', #226381, #14602 ) ;
#222538 = CARTESIAN_POINT ( 'NONE',  ( -18.59999999999999787, 0.000000000000000000, -33.50000000000000000 ) ) ;
#222539 = CARTESIAN_POINT ( 'NONE',  ( -18.39999999999999858, -9.682403433465239573, -107.1568433774128408 ) ) ;
#222540 = DIRECTION ( 'NONE',  ( 0.000000000000000000, -6.982962677686266711E-15, 1.000000000000000000 ) ) ;
#222541 = EDGE_CURVE ( 'NONE', #90288, #63948, #249864, .T. ) ;
#222542 = VECTOR ( 'NONE', #29677, 1000.000000000000000 ) ;
#222543 = DIRECTION ( 'NONE',  ( 1.000000000000000000, 0.000000000000000000, 0.000000000000000000 ) ) ;
#222544 = DIRECTION ( 'NONE',  ( 1.284434275755705296E-16, -0.7071067811865471286, -0.7071067811865479058 ) ) ;
#222545 = DIRECTION ( 'NONE',  ( 0.000000000000000000, 4.510281037540195239E-13, 1.000000000000000000 ) ) ;
#222546 = AXIS2_PLACEMENT_3D ( 'NONE', #72997, #117227, #152533 ) ;
#222547 = CARTESIAN_POINT ( 'NONE',  ( -20.95000000000000284, 56.06656052939784729, -228.0911609752645575 ) ) ;
#222548 = CARTESIAN_POINT ( 'NONE',  ( -20.85000000000000142, 42.92545512184477730, -254.1955779480491344 ) ) ;
#222549 = CIRCLE ( 'NONE', #226848, 6.258578643762696458 ) ;
#222550 = ORIENTED_EDGE ( 'NONE', *, *, #15821, .T. ) ;
#222551 = DIRECTION ( 'NONE',  ( 0.000000000000000000, -1.000000000000000000, -6.982962677686265922E-15 ) ) ;
#222552 = DIRECTION ( 'NONE',  ( -1.000000000000000000, -0.000000000000000000, -0.000000000000000000 ) ) ;
#222553 = EDGE_CURVE ( 'NONE', #215460, #251832, #49084, .T. ) ;
#222554 = ORIENTED_EDGE ( 'NONE', *, *, #100010, .T. ) ;
#222555 = FACE_OUTER_BOUND ( 'NONE', #165841, .T. ) ;
#222556 = CARTESIAN_POINT ( 'NONE',  ( 21.14999999999999858, 67.21339244341217523, -157.7731074845244166 ) ) ;
#222557 = CARTESIAN_POINT ( 'NONE',  ( -18.41431012584567739, 11.48747202921933308, -191.7732360131016662 ) ) ;
#222558 = VERTEX_POINT ( 'NONE', #109056 ) ;
#222559 = CARTESIAN_POINT ( 'NONE',  ( -16.87036670365548474, 9.989418819312801290, -188.4795601173020145 ) ) ;
#222560 = CARTESIAN_POINT ( 'NONE',  ( -18.39999999999999858, 85.50000000001161027, -62.49103808782458458 ) ) ;
#222561 = EDGE_CURVE ( 'NONE', #219130, #236185, #252408, .T. ) ;
#222562 = VERTEX_POINT ( 'NONE', #128646 ) ;
#222563 = AXIS2_PLACEMENT_3D ( 'NONE', #148995, #228525, #72019 ) ;
#222564 = VERTEX_POINT ( 'NONE', #150765 ) ;
#222565 = CARTESIAN_POINT ( 'NONE',  ( -23.25000000000000000, -11.64999999998884483, -197.9999999999999432 ) ) ;
#222566 = VECTOR ( 'NONE', #229908, 1000.000000000000114 ) ;
#222567 = ORIENTED_EDGE ( 'NONE', *, *, #24385, .T. ) ;
#222568 = CARTESIAN_POINT ( 'NONE',  ( -23.25000000000000000, 1.115600667400684642E-11, -100.5000000000000426 ) ) ;
#222569 = DIRECTION ( 'NONE',  ( -1.000000000000000000, 0.000000000000000000, 0.000000000000000000 ) ) ;
#222570 = DIRECTION ( 'NONE',  ( 0.000000000000000000, 1.000000000000000000, 0.000000000000000000 ) ) ;
#222572 = CARTESIAN_POINT ( 'NONE',  ( 20.85000000000000142, -1.835859311432481045, -78.50443916879852679 ) ) ;
#222571 = PRODUCT_DEFINITION_CONTEXT ( 'detailed design', #42461, 'design' ) ;
#222573 = DIRECTION ( 'NONE',  ( 1.000000000000000000, 0.000000000000000000, 0.000000000000000000 ) ) ;
#222574 = DIRECTION ( 'NONE',  ( 0.000000000000000000, -1.000000000000000000, 0.000000000000000000 ) ) ;
#222575 = CARTESIAN_POINT ( 'NONE',  ( 21.72449340488909897, 65.71604372252112114, -149.1731074845244507 ) ) ;
#222576 = CARTESIAN_POINT ( 'NONE',  ( 20.94999999999999929, 0.000000000000000000, -37.60000000000000142 ) ) ;
#222577 = DIRECTION ( 'NONE',  ( -1.000000000000000000, -0.000000000000000000, -0.000000000000000000 ) ) ;
#222579 = ORIENTED_EDGE ( 'NONE', *, *, #187792, .F. ) ;
#222578 = CARTESIAN_POINT ( 'NONE',  ( 18.41832399655374886, 87.08727404907521930, -199.6327534953675240 ) ) ;
#222580 = ORIENTED_EDGE ( 'NONE', *, *, #257539, .F. ) ;
#222581 = CARTESIAN_POINT ( 'NONE',  ( -20.64999999999999858, 7.150000000011155876, -88.15000000000004832 ) ) ;
#222583 = ORIENTED_EDGE ( 'NONE', *, *, #156479, .T. ) ;
#222582 = CARTESIAN_POINT ( 'NONE',  ( -16.85722902420167557, 60.96960266377776350, -220.9302088364852068 ) ) ;
#222584 = ORIENTED_EDGE ( 'NONE', *, *, #109214, .F. ) ;
#222585 = DIRECTION ( 'NONE',  ( 0.000000000000000000, -2.664535259100396996E-15, 1.000000000000000000 ) ) ;
#222586 = CARTESIAN_POINT ( 'NONE',  ( 20.97250901189795513, 10.62456803371303593, -175.1645457169669555 ) ) ;
#222587 = TOROIDAL_SURFACE ( 'NONE', #110171, 11.65000000000000036, 0.1000000000000000056 ) ;
#222588 = DIRECTION ( 'NONE',  ( 1.000000000000000000, -0.000000000000000000, -0.000000000000000000 ) ) ;
#222589 = CARTESIAN_POINT ( 'NONE',  ( 18.49999999999999645, 65.87552587769046397, -245.8195358697090001 ) ) ;
#222590 = DIRECTION ( 'NONE',  ( 1.000000000000000000, 1.159508501126949290E-16, 2.525285885220369759E-17 ) ) ;
#222591 = CARTESIAN_POINT ( 'NONE',  ( -23.15000000000000213, 30.43677443282724937, -239.5249545687858870 ) ) ;
#222592 = EDGE_CURVE ( 'NONE', #244844, #48052, #73823, .T. ) ;
#222593 = CARTESIAN_POINT ( 'NONE',  ( -20.64999999999999858, 76.00000000001205080, -123.6481074845242887 ) ) ;
#222594 = VERTEX_POINT ( 'NONE', #171649 ) ;
#222595 = ORIENTED_EDGE ( 'NONE', *, *, #24379, .F. ) ;
#222596 = CARTESIAN_POINT ( 'NONE',  ( 20.94999999999999929, 87.48912529308749697, -39.12310748452424747 ) ) ;
#222597 = VECTOR ( 'NONE', #55873, 1000.000000000000000 ) ;
#222598 = CIRCLE ( 'NONE', #80962, 3.999999999999994671 ) ;
#222599 = ORIENTED_EDGE ( 'NONE', *, *, #158665, .F. ) ;
#222600 = CARTESIAN_POINT ( 'NONE',  ( 21.04999999999999716, 0.05148288189283987265, -27.19982018208539998 ) ) ;
#222601 = ORIENTED_EDGE ( 'NONE', *, *, #88866, .T. ) ;
#222602 = CARTESIAN_POINT ( 'NONE',  ( -16.85312964099708566, 9.913604682078865693, -154.6028157064305049 ) ) ;
#222603 = CIRCLE ( 'NONE', #193437, 0.09999999999999230338 ) ;
#222604 = CIRCLE ( 'NONE', #85224, 1.900000000000012790 ) ;
#222605 = FACE_OUTER_BOUND ( 'NONE', #233761, .T. ) ;
#222606 =( GEOMETRIC_REPRESENTATION_CONTEXT ( 3 ) GLOBAL_UNCERTAINTY_ASSIGNED_CONTEXT ( ( #133757 ) ) GLOBAL_UNIT_ASSIGNED_CONTEXT ( ( #103423, #220822, #162163 ) ) REPRESENTATION_CONTEXT ( 'NONE', 'WORKASPACE' ) );
#222607 = ADVANCED_FACE ( 'NONE', ( #111635 ), #12559, .T. ) ;
#222608 = DIRECTION ( 'NONE',  ( 1.000000000000000000, 0.000000000000000000, 0.000000000000000000 ) ) ;
#222609 = DIRECTION ( 'NONE',  ( 1.000000000000000000, 7.304098846218135653E-16, 0.000000000000000000 ) ) ;
#222610 = VERTEX_POINT ( 'NONE', #132485 ) ;
#222611 = CARTESIAN_POINT ( 'NONE',  ( -21.05000000000000071, 11.63687328910405938, -6.821759213324853022 ) ) ;
#222612 = ORIENTED_EDGE ( 'NONE', *, *, #107470, .T. ) ;
#222613 = EDGE_CURVE ( 'NONE', #37705, #37503, #254189, .T. ) ;
#222614 = CARTESIAN_POINT ( 'NONE',  ( 22.49806830649814060, 0.07746431633666325811, -122.3501103451609424 ) ) ;
#222615 = DIRECTION ( 'NONE',  ( 1.000000000000000000, 0.000000000000000000, 0.000000000000000000 ) ) ;
#222617 = AXIS2_PLACEMENT_3D ( 'NONE', #57116, #254048, #213654 ) ;
#222616 = DIRECTION ( 'NONE',  ( 0.000000000000000000, 0.000000000000000000, -1.000000000000000000 ) ) ;
#222618 = DIRECTION ( 'NONE',  ( 2.952720810173289605E-16, -0.9770955615653315052, -0.2128009952263610061 ) ) ;
#222619 = VERTEX_POINT ( 'NONE', #208187 ) ;
#222620 = CARTESIAN_POINT ( 'NONE',  ( -20.94999999999999929, 64.40000000001188596, -96.09490425424883142 ) ) ;
#222621 = EDGE_CURVE ( 'NONE', #91601, #225500, #99456, .T. ) ;
#222623 = VERTEX_POINT ( 'NONE', #195045 ) ;
#222622 = TOROIDAL_SURFACE ( 'NONE', #172807, 4.099999999999999645, 0.1000000000000000056 ) ;
#222626 = ORIENTED_EDGE ( 'NONE', *, *, #96917, .T. ) ;
#222625 = DIRECTION ( 'NONE',  ( -1.000000000000000000, 0.000000000000000000, -0.000000000000000000 ) ) ;
#222624 = DIRECTION ( 'NONE',  ( -1.000000000000000000, -1.836970198721029934E-16, -3.186635328391151676E-31 ) ) ;
#222627 = FACE_OUTER_BOUND ( 'NONE', #28872, .T. ) ;
#222629 = ORIENTED_EDGE ( 'NONE', *, *, #2199, .F. ) ;
#222628 = VECTOR ( 'NONE', #190296, 1000.000000000000114 ) ;
#222630 = AXIS2_PLACEMENT_3D ( 'NONE', #167572, #227506, #11042 ) ;
#222631 = EDGE_CURVE ( 'NONE', #125182, #34168, #153123, .T. ) ;
#222632 = FACE_OUTER_BOUND ( 'NONE', #126946, .T. ) ;
#222633 = ORIENTED_EDGE ( 'NONE', *, *, #35184, .F. ) ;
#222635 = DIRECTION ( 'NONE',  ( 0.000000000000000000, 0.000000000000000000, 1.000000000000000000 ) ) ;
#222634 = AXIS2_PLACEMENT_3D ( 'NONE', #116097, #216459, #172258 ) ;
#222636 = CARTESIAN_POINT ( 'NONE',  ( -16.93521499325732549, 9.994786119814678571, -54.40710854109355665 ) ) ;
#222637 = EDGE_CURVE ( 'NONE', #69624, #157880, #58057, .T. ) ;
#222638 = DIRECTION ( 'NONE',  ( 0.000000000000000000, 0.2617529984164506107, 0.9651348961777299618 ) ) ;
#222639 = CARTESIAN_POINT ( 'NONE',  ( -18.54118089899632693, -9.463537631836942410, -74.04857759786816018 ) ) ;
#222640 = CIRCLE ( 'NONE', #68554, 11.89999999999999858 ) ;
#222641 = AXIS2_PLACEMENT_3D ( 'NONE', #17961, #200466, #97477 ) ;
#222642 = DIRECTION ( 'NONE',  ( 1.000000000000000000, 0.000000000000000000, 0.000000000000000000 ) ) ;
#222643 = AXIS2_PLACEMENT_3D ( 'NONE', #164593, #43361, #5476 ) ;
#222644 = EDGE_CURVE ( 'NONE', #130981, #121226, #199462, .T. ) ;
#222645 = ORIENTED_EDGE ( 'NONE', *, *, #9503, .F. ) ;
#222646 = CARTESIAN_POINT ( 'NONE',  ( -21.05000000000000071, -1.261786168553869603, -108.5864989635455089 ) ) ;
#222647 = CARTESIAN_POINT ( 'NONE',  ( 18.49999999999999645, -1.835341550213255957, -78.55515129256302487 ) ) ;
#222648 = TOROIDAL_SURFACE ( 'NONE', #110236, 0.6000000000000009770, 0.1000000000000000056 ) ;
#222650 = B_SPLINE_CURVE_WITH_KNOTS ( 'NONE', 3,
 ( #81947, #203214, #119858, #100234, #3729, #102806, #139369, #141952, #218914, #1142 ),
 .UNSPECIFIED., .F., .F.,
 ( 4, 3, 3, 4 ),
 ( 1.883833020489685736E-15, 3.877043166999269576E-05, 7.336897548476537185E-05, 7.659383120240726740E-05 ),
 .UNSPECIFIED. ) ;
#222649 = FACE_OUTER_BOUND ( 'NONE', #130682, .T. ) ;
#222651 = VERTEX_POINT ( 'NONE', #76337 ) ;
#222652 = LINE ( 'NONE', #44038, #92748 ) ;
#222653 = ORIENTED_EDGE ( 'NONE', *, *, #203975, .F. ) ;
#222654 = CARTESIAN_POINT ( 'NONE',  ( -20.85000000000000142, 76.00000000001142553, -36.02310748452432421 ) ) ;
#222655 = TOROIDAL_SURFACE ( 'NONE', #118651, 0.6000000000000013101, 0.1000000000000000056 ) ;
#222656 = DIRECTION ( 'NONE',  ( -0.000000000000000000, -1.000000000000000000, 6.308085367188393199E-16 ) ) ;
#222657 = FACE_BOUND ( 'NONE', #71239, .T. ) ;
#222659 = ORIENTED_EDGE ( 'NONE', *, *, #191264, .F. ) ;
#222658 = CYLINDRICAL_SURFACE ( 'NONE', #102929, 0.1000000000000002554 ) ;
#222660 = DIRECTION ( 'NONE',  ( 0.000000000000000000, 0.000000000000000000, -1.000000000000000000 ) ) ;
#222661 = CIRCLE ( 'NONE', #77117, 0.1000000000000024342 ) ;
#222662 = AXIS2_PLACEMENT_3D ( 'NONE', #24451, #105195, #184771 ) ;
#222663 = EDGE_CURVE ( 'NONE', #231485, #135981, #18942, .T. ) ;
#222664 = CARTESIAN_POINT ( 'NONE',  ( -20.94999999999999929, -11.74999999998884448, -103.6000000000000369 ) ) ;
#222665 = DIRECTION ( 'NONE',  ( -1.000000000000000000, -7.304098846218134667E-16, 0.000000000000000000 ) ) ;
#222666 = ORIENTED_EDGE ( 'NONE', *, *, #142418, .T. ) ;
#222667 = DIRECTION ( 'NONE',  ( -0.000000000000000000, -0.1298341882519953583, -0.9915357197604862671 ) ) ;
#222668 = LINE ( 'NONE', #86997, #218981 ) ;
#222669 = ORIENTED_EDGE ( 'NONE', *, *, #4331, .T. ) ;
#222670 = CARTESIAN_POINT ( 'NONE',  ( 22.49999999999999645, 64.35012909624819599, -170.1056273753973755 ) ) ;
#222671 = EDGE_LOOP ( 'NONE', ( #185384, #215027, #36743 ) ) ;
#222672 = ADVANCED_FACE ( 'NONE', ( #159757 ), #28218, .T. ) ;
#222673 = FACE_OUTER_BOUND ( 'NONE', #166975, .T. ) ;
#222675 = ORIENTED_EDGE ( 'NONE', *, *, #169165, .F. ) ;
#222674 = CARTESIAN_POINT ( 'NONE',  ( -23.15000000000000213, 71.85000000001228670, -157.6731074845243654 ) ) ;
#222678 = ORIENTED_EDGE ( 'NONE', *, *, #77629, .F. ) ;
#222677 = VERTEX_POINT ( 'NONE', #135022 ) ;
#222676 = DIRECTION ( 'NONE',  ( 0.000000000000000000, 0.9654727137038726648, -0.2605042016806632943 ) ) ;
#222679 = AXIS2_PLACEMENT_3D ( 'NONE', #53273, #113237, #192788 ) ;
#222680 = CARTESIAN_POINT ( 'NONE',  ( -17.22361732159832215, 10.34515565861359221, -78.37078452586717958 ) ) ;
#222681 = DIRECTION ( 'NONE',  ( 0.000000000000000000, 0.000000000000000000, -1.000000000000000000 ) ) ;
#222682 = AXIS2_PLACEMENT_3D ( 'NONE', #179692, #40199, #21893 ) ;
#222683 = CYLINDRICAL_SURFACE ( 'NONE', #177544, 0.09999999999998898659 ) ;
#222685 = CARTESIAN_POINT ( 'NONE',  ( -20.85000000000000142, 7.021664781911246322, -104.2335654018973372 ) ) ;
#222684 = DIRECTION ( 'NONE',  ( 1.000000000000000000, 0.000000000000000000, 0.000000000000000000 ) ) ;
#222687 = ADVANCED_FACE ( 'NONE', ( #56758, #140164, #136301 ), #116766, .F. ) ;
#222686 = CARTESIAN_POINT ( 'NONE',  ( -21.44999999999999929, 7.349999999999998757, -12.34999999999999964 ) ) ;
#222688 = AXIS2_PLACEMENT_3D ( 'NONE', #38527, #21540, #161049 ) ;
#222689 = FACE_OUTER_BOUND ( 'NONE', #119493, .T. ) ;
#222690 = EDGE_CURVE ( 'NONE', #178423, #186245, #32306, .T. ) ;
#222691 = CARTESIAN_POINT ( 'NONE',  ( 21.05000000000000071, 87.39257802171739797, -72.59705706435616435 ) ) ;
#222692 = CARTESIAN_POINT ( 'NONE',  ( -18.59999999999999787, 74.73821383144729680, -161.9366085209788935 ) ) ;
#222693 = ORIENTED_EDGE ( 'NONE', *, *, #64657, .F. ) ;
#222695 = ORIENTED_EDGE ( 'NONE', *, *, #214254, .F. ) ;
#222694 = AXIS2_PLACEMENT_3D ( 'NONE', #128369, #168818, #64529 ) ;
#222696 = DIRECTION ( 'NONE',  ( 0.000000000000000000, 1.000000000000000000, 0.000000000000000000 ) ) ;
#222698 = ORIENTED_EDGE ( 'NONE', *, *, #131227, .F. ) ;
#222697 = CARTESIAN_POINT ( 'NONE',  ( 22.50000000000000000, 7.128833340093095217, -233.7327013124392749 ) ) ;
#222699 = EDGE_LOOP ( 'NONE', ( #192578, #123232, #122557, #128621, #47073, #158799, #216338, #161977, #195821, #92963, #171500, #252082, #128722, #94626, #245210, #202402 ) ) ;
#222700 = DIRECTION ( 'NONE',  ( -1.000000000000000000, 0.000000000000000000, -0.000000000000000000 ) ) ;
#222701 = ADVANCED_FACE ( 'NONE', ( #155923 ), #118051, .F. ) ;
#222702 = ORIENTED_EDGE ( 'NONE', *, *, #175107, .F. ) ;
#222703 = CARTESIAN_POINT ( 'NONE',  ( 19.75857864376268935, 11.65000000000000391, -24.85000000000000142 ) ) ;
#222704 = AXIS2_PLACEMENT_3D ( 'NONE', #78742, #256054, #138692 ) ;
#222705 = EDGE_CURVE ( 'NONE', #171172, #147844, #81461, .T. ) ;
#222706 = EDGE_CURVE ( 'NONE', #220552, #73178, #223799, .T. ) ;
#222707 = VERTEX_POINT ( 'NONE', #20252 ) ;
#222708 = AXIS2_PLACEMENT_3D ( 'NONE', #171209, #249423, #109885 ) ;
#222709 = DIRECTION ( 'NONE',  ( 0.000000000000000000, 0.000000000000000000, 1.000000000000000000 ) ) ;
#222710 = DIRECTION ( 'NONE',  ( 2.710505431213777355E-16, 1.000000000000000000, 6.982962677686266711E-15 ) ) ;
#222711 = CIRCLE ( 'NONE', #189425, 0.4999999999999944489 ) ;
#222713 = ORIENTED_EDGE ( 'NONE', *, *, #244313, .F. ) ;
#222712 = ORIENTED_EDGE ( 'NONE', *, *, #249005, .F. ) ;
#222714 = ORIENTED_EDGE ( 'NONE', *, *, #153945, .F. ) ;
#222715 = CARTESIAN_POINT ( 'NONE',  ( -20.64999999999999858, 36.65892442174935439, -249.5511627012433848 ) ) ;
#222716 = ORIENTED_EDGE ( 'NONE', *, *, #233309, .F. ) ;
#222717 = ORIENTED_EDGE ( 'NONE', *, *, #253503, .T. ) ;
#222718 = EDGE_CURVE ( 'NONE', #195198, #232010, #59324, .T. ) ;
#222719 = CARTESIAN_POINT ( 'NONE',  ( 18.79999999999999716, 7.800000000000000711, 1.212568896937007867 ) ) ;
#222720 = CARTESIAN_POINT ( 'NONE',  ( 21.05000000000000071, 71.18691588786246882, -114.9646252410481537 ) ) ;
#222722 = VERTEX_POINT ( 'NONE', #80174 ) ;
#222721 = CARTESIAN_POINT ( 'NONE',  ( 18.50000000000000355, -9.421074344975995274, -107.3244720594301356 ) ) ;
#222723 = AXIS2_PLACEMENT_3D ( 'NONE', #161954, #185348, #100636 ) ;
#222725 = CARTESIAN_POINT ( 'NONE',  ( 20.95556889135987788, 65.37805641227723186, -162.3807132626669159 ) ) ;
#222724 = DIRECTION ( 'NONE',  ( -0.000000000000000000, -6.982962677686266711E-15, 1.000000000000000000 ) ) ;
#222726 = CARTESIAN_POINT ( 'NONE',  ( 20.94999999999999574, 87.41227409416133298, -66.52310748452423184 ) ) ;
#222728 = ORIENTED_EDGE ( 'NONE', *, *, #100861, .T. ) ;
#222727 = DIRECTION ( 'NONE',  ( 0.000000000000000000, 0.000000000000000000, 1.000000000000000000 ) ) ;
#222729 = CARTESIAN_POINT ( 'NONE',  ( -17.78241384941336989, 10.85557575280576792, -177.7490376724458088 ) ) ;
#222730 = ORIENTED_EDGE ( 'NONE', *, *, #93376, .F. ) ;
#222731 = CARTESIAN_POINT ( 'NONE',  ( -2.995603634470891112E-16, 6.650000000011155876, -188.7499999999999716 ) ) ;
#222732 = ORIENTED_EDGE ( 'NONE', *, *, #20308, .F. ) ;
#222733 = CARTESIAN_POINT ( 'NONE',  ( 22.47071067811865319, 68.27992525551434255, -170.1221999392270163 ) ) ;
#222734 = CARTESIAN_POINT ( 'NONE',  ( -20.54999999999999716, -3.363022478626109368, -226.2703567425896267 ) ) ;
#222735 = EDGE_LOOP ( 'NONE', ( #38172, #55449, #41906, #142447 ) ) ;
#222736 = CARTESIAN_POINT ( 'NONE',  ( 21.08804281139605408, 10.62183430185232069, -45.84999996737845862 ) ) ;
#222737 = AXIS2_PLACEMENT_3D ( 'NONE', #238792, #139656, #197075 ) ;
#222738 = DIRECTION ( 'NONE',  ( -0.000000000000000000, 1.000000000000000000, -0.000000000000000000 ) ) ;
#222739 = CIRCLE ( 'NONE', #26970, 0.1000000000000029476 ) ;
#222740 = DIRECTION ( 'NONE',  ( 0.000000000000000000, 0.5000000000000209832, 0.8660254037844264952 ) ) ;
#222741 = ORIENTED_EDGE ( 'NONE', *, *, #191424, .T. ) ;
#222742 = ORIENTED_EDGE ( 'NONE', *, *, #229735, .F. ) ;
#222743 = DIRECTION ( 'NONE',  ( 1.000000000000000000, 0.000000000000000000, 0.000000000000000000 ) ) ;
#222744 = DIRECTION ( 'NONE',  ( 1.000000000000000000, -0.000000000000000000, -0.000000000000000000 ) ) ;
#222746 = ORIENTED_EDGE ( 'NONE', *, *, #249878, .T. ) ;
#222745 = EDGE_CURVE ( 'NONE', #32887, #201638, #69900, .T. ) ;
#222747 = CARTESIAN_POINT ( 'NONE',  ( -16.87683809663752399, 21.23804903844422043, -113.1500000000000341 ) ) ;
#222748 = EDGE_LOOP ( 'NONE', ( #57690, #143487, #144719, #183823 ) ) ;
#222749 = EDGE_CURVE ( 'NONE', #223519, #194690, #232217, .T. ) ;
#222750 = CARTESIAN_POINT ( 'NONE',  ( -22.40000000000000213, 1.115486826172573664E-11, -55.24956710754144495 ) ) ;
#222751 = DIRECTION ( 'NONE',  ( 0.000000000000000000, 0.2617529984165029022, 0.9651348961777158619 ) ) ;
#222753 = DIRECTION ( 'NONE',  ( 0.000000000000000000, -1.000000000000000000, 0.000000000000000000 ) ) ;
#222752 = CARTESIAN_POINT ( 'NONE',  ( -21.29999999999995808, 1.115600667400684642E-11, -71.05000000000003979 ) ) ;
#222754 = LINE ( 'NONE', #119845, #219865 ) ;
#222755 = CARTESIAN_POINT ( 'NONE',  ( 18.59999999999999787, -1.362429037182151470, -108.3888812479212476 ) ) ;
#222757 = ADVANCED_FACE ( 'NONE', ( #35965 ), #257502, .F. ) ;
#222756 = ORIENTED_EDGE ( 'NONE', *, *, #17544, .T. ) ;
#222758 = CARTESIAN_POINT ( 'NONE',  ( 18.48197441911631955, -9.517954794695798526, -207.8902116422065092 ) ) ;
#222759 = AXIS2_PLACEMENT_3D ( 'NONE', #239442, #120795, #17801 ) ;
#222761 = ORIENTED_EDGE ( 'NONE', *, *, #169699, .F. ) ;
#222760 = ORIENTED_EDGE ( 'NONE', *, *, #221529, .T. ) ;
#222762 = ORIENTED_EDGE ( 'NONE', *, *, #152535, .T. ) ;
#222763 = VERTEX_POINT ( 'NONE', #196298 ) ;
#222764 = DIRECTION ( 'NONE',  ( -1.000000000000000000, 0.000000000000000000, 0.000000000000000000 ) ) ;
#222765 = CARTESIAN_POINT ( 'NONE',  ( -18.44362607810621668, -7.771182065979212794, -209.9158824246631241 ) ) ;
#222766 = AXIS2_PLACEMENT_3D ( 'NONE', #227027, #147499, #204886 ) ;
#222767 = DIRECTION ( 'NONE',  ( 1.000000000000000000, 0.000000000000000000, 0.000000000000000000 ) ) ;
#222768 = CARTESIAN_POINT ( 'NONE',  ( 20.90000000000000213, 7.900000000000000355, -1.212568896937008089 ) ) ;
#222770 = FACE_OUTER_BOUND ( 'NONE', #43450, .T. ) ;
#222769 = FACE_OUTER_BOUND ( 'NONE', #169638, .T. ) ;
#222772 = ORIENTED_EDGE ( 'NONE', *, *, #213226, .T. ) ;
#222771 = CARTESIAN_POINT ( 'NONE',  ( 18.43466021071402139, 77.15162984240767230, -241.8142968757794335 ) ) ;
#222773 = CARTESIAN_POINT ( 'NONE',  ( -21.04999999999676774, 6.497017786442108367, -167.5145456905664219 ) ) ;
#222774 = ORIENTED_EDGE ( 'NONE', *, *, #206244, .T. ) ;
#222775 = CARTESIAN_POINT ( 'NONE',  ( 21.95218792049437795, 33.62430829188672021, -243.0194996105014411 ) ) ;
#222776 = EDGE_LOOP ( 'NONE', ( #45541, #142511, #53719, #6430, #136899, #156406 ) ) ;
#222777 = EDGE_LOOP ( 'NONE', ( #254235, #51800, #101902, #21771 ) ) ;
#222778 = CARTESIAN_POINT ( 'NONE',  ( 21.05000000000000071, 6.477067021124756963, -0.09999999999999967248 ) ) ;
#222779 = CARTESIAN_POINT ( 'NONE',  ( -16.80621392010904813, 66.05779742250376785, -48.71269944994133283 ) ) ;
#222780 = DIRECTION ( 'NONE',  ( -0.000000000000000000, -0.4088369013363281623, 0.9126074666063771490 ) ) ;
#222781 = ADVANCED_FACE ( 'NONE', ( #236701 ), #115666, .T. ) ;
#222782 = VECTOR ( 'NONE', #73548, 1000.000000000000000 ) ;
#222783 = FACE_OUTER_BOUND ( 'NONE', #234935, .T. ) ;
#222784 = ORIENTED_EDGE ( 'NONE', *, *, #75517, .T. ) ;
#222785 = ORIENTED_EDGE ( 'NONE', *, *, #16719, .F. ) ;
#222787 = EDGE_CURVE ( 'NONE', #58814, #185550, #217125, .T. ) ;
#222786 = CARTESIAN_POINT ( 'NONE',  ( -20.94999999999999929, -1.162701749926853712, -142.1000000000000227 ) ) ;
#222788 = ORIENTED_EDGE ( 'NONE', *, *, #130836, .T. ) ;
#222789 = LINE ( 'NONE', #27210, #177143 ) ;
#222790 = DIRECTION ( 'NONE',  ( 1.000000000000000000, 0.000000000000000000, 0.000000000000000000 ) ) ;
#222791 = CARTESIAN_POINT ( 'NONE',  ( -18.50000000000000000, 1.115600667400684642E-11, -100.5000000000000284 ) ) ;
#222792 = CARTESIAN_POINT ( 'NONE',  ( -20.94999999999999929, -1.835341550213255957, -145.5551512925629822 ) ) ;
#222793 = LINE ( 'NONE', #208407, #240360 ) ;
#222794 = CARTESIAN_POINT ( 'NONE',  ( -16.80438519320023616, 66.05022090354351860, -90.37236920360311387 ) ) ;
#222795 = DIRECTION ( 'NONE',  ( 0.000000000000000000, 0.000000000000000000, -1.000000000000000000 ) ) ;
#222796 = ADVANCED_FACE ( 'NONE', ( #125749 ), #123197, .T. ) ;
#222797 = FACE_OUTER_BOUND ( 'NONE', #28014, .T. ) ;
#222798 = CARTESIAN_POINT ( 'NONE',  ( 20.94999999999999929, 74.16465844978819177, -191.9679561919613775 ) ) ;
#222799 = CARTESIAN_POINT ( 'NONE',  ( 18.52928932188133970, 65.72071067813116940, -178.8731074845244109 ) ) ;
#222801 = EDGE_CURVE ( 'NONE', #254838, #201469, #61940, .T. ) ;
#222800 = CARTESIAN_POINT ( 'NONE',  ( -18.59999999999999787, 85.32100840337318459, -95.78716923544635620 ) ) ;
#222802 = AXIS2_PLACEMENT_3D ( 'NONE', #95983, #236782, #213367 ) ;
#222803 = CARTESIAN_POINT ( 'NONE',  ( -20.85000000000000142, 65.66751761918668251, -97.42826094061121012 ) ) ;
#222804 = AXIS2_PLACEMENT_3D ( 'NONE', #234479, #18000, #231944 ) ;
#222805 = AXIS2_PLACEMENT_3D ( 'NONE', #129799, #110230, #230184 ) ;
#222806 = CIRCLE ( 'NONE', #101986, 0.1000000000000001860 ) ;
#222807 = EDGE_CURVE ( 'NONE', #52329, #4150, #245604, .T. ) ;
#222808 = VERTEX_POINT ( 'NONE', #240573 ) ;
#222810 = ADVANCED_FACE ( 'NONE', ( #142737 ), #102303, .T. ) ;
#222809 = EDGE_CURVE ( 'NONE', #221156, #41586, #201438, .T. ) ;
#222811 = MECHANICAL_DESIGN_GEOMETRIC_PRESENTATION_REPRESENTATION (  '', ( #243672 ), #160315 ) ;
#222812 = CARTESIAN_POINT ( 'NONE',  ( -16.88005004766534967, 30.20667229816764987, -234.8071151212674863 ) ) ;
#222813 = ORIENTED_EDGE ( 'NONE', *, *, #165099, .F. ) ;
#222814 = LINE ( 'NONE', #65033, #58609 ) ;
#222815 = CARTESIAN_POINT ( 'NONE',  ( -20.54999999999999716, 71.75000000001156764, -57.17310748452435121 ) ) ;
#222816 = CARTESIAN_POINT ( 'NONE',  ( 20.95512820512820440, 61.84489010471549619, -221.8053782964821323 ) ) ;
#222817 = VERTEX_POINT ( 'NONE', #166211 ) ;
#222818 = DIRECTION ( 'NONE',  ( 1.000000000000000000, 0.000000000000000000, 0.000000000000000000 ) ) ;
#222819 = CARTESIAN_POINT ( 'NONE',  ( 21.05000000000000071, 87.65000000001164437, -69.52310748452424605 ) ) ;
#222820 = CARTESIAN_POINT ( 'NONE',  ( -23.25000000000000000, 4.350000000011156054, -155.3500000000000227 ) ) ;
#222821 = CARTESIAN_POINT ( 'NONE',  ( -18.50000000000000000, 76.00000000001267608, -203.5231074845243597 ) ) ;
#222822 = EDGE_CURVE ( 'NONE', #247693, #92943, #3213, .T. ) ;
#222823 = CYLINDRICAL_SURFACE ( 'NONE', #30681, 0.09999999999999939493 ) ;
#222824 = EDGE_CURVE ( 'NONE', #141973, #97847, #7331, .T. ) ;
#222825 = AXIS2_PLACEMENT_3D ( 'NONE', #81838, #117167, #196684 ) ;
#222826 = LINE ( 'NONE', #44218, #161328 ) ;
#222827 = CIRCLE ( 'NONE', #10466, 0.5000000000000004441 ) ;
#222828 = AXIS2_PLACEMENT_3D ( 'NONE', #113206, #71543, #191495 ) ;
#222829 = VERTEX_POINT ( 'NONE', #202722 ) ;
#222830 = CARTESIAN_POINT ( 'NONE',  ( -18.39999999999999858, 86.89640087696872683, -199.6396878666313341 ) ) ;
#222832 = VERTEX_POINT ( 'NONE', #222260 ) ;
#222831 = DIRECTION ( 'NONE',  ( 0.000000000000000000, -0.4999999999999689138, -0.8660254037844565822 ) ) ;
#222833 = CARTESIAN_POINT ( 'NONE',  ( 22.59999999999999432, 0.1008583691098678542, -122.2504328765106152 ) ) ;
#222834 = EDGE_CURVE ( 'NONE', #241392, #255132, #245713, .T. ) ;
#222835 = DIRECTION ( 'NONE',  ( -0.000000000000000000, -0.6052030477778852502, -0.7960711469211522173 ) ) ;
#222836 = DIRECTION ( 'NONE',  ( 0.000000000000000000, -0.1335171055202867274, 0.9910465087640866200 ) ) ;
#222837 = ORIENTED_EDGE ( 'NONE', *, *, #94315, .F. ) ;
#222838 = CARTESIAN_POINT ( 'NONE',  ( -22.49072729836729678, 75.94351806727860321, -148.1731157336792535 ) ) ;
#222839 = VECTOR ( 'NONE', #66742, 1000.000000000000000 ) ;
#222840 = CONTEXT_DEPENDENT_SHAPE_REPRESENTATION ( #219136, #157924 ) ;
#222841 = CIRCLE ( 'NONE', #35447, 0.09999999999999609201 ) ;
#222842 = CIRCLE ( 'NONE', #39721, 0.09999999999999939493 ) ;
#222843 = EDGE_CURVE ( 'NONE', #33602, #74587, #141467, .T. ) ;
#222844 = CARTESIAN_POINT ( 'NONE',  ( -20.94999999999994600, 65.15000000001120384, -3.123107484524795474 ) ) ;
#222845 = ORIENTED_EDGE ( 'NONE', *, *, #148815, .F. ) ;
#222846 = DIRECTION ( 'NONE',  ( 1.000000000000000000, -0.000000000000000000, -0.000000000000000000 ) ) ;
#222847 = DIRECTION ( 'NONE',  ( -1.000000000000000000, 0.000000000000000000, 0.000000000000000000 ) ) ;
#222848 = EDGE_CURVE ( 'NONE', #235855, #156630, #4515, .T. ) ;
#222849 = VECTOR ( 'NONE', #25164, 1000.000000000000000 ) ;
#222850 = DIRECTION ( 'NONE',  ( 1.000000000000000000, -0.000000000000000000, -0.000000000000000000 ) ) ;
#222851 = ORIENTED_EDGE ( 'NONE', *, *, #114006, .F. ) ;
#222852 = EDGE_LOOP ( 'NONE', ( #66933, #16162, #214078, #99882 ) ) ;
#222853 = EDGE_CURVE ( 'NONE', #164389, #16503, #220993, .T. ) ;
#222854 = FACE_OUTER_BOUND ( 'NONE', #8154, .T. ) ;
#222855 = AXIS2_PLACEMENT_3D ( 'NONE', #242565, #220461, #100466 ) ;
#222856 = LINE ( 'NONE', #165473, #67263 ) ;
#222857 = DIRECTION ( 'NONE',  ( -1.000000000000000000, -0.000000000000000000, -0.000000000000000000 ) ) ;
#222858 = CIRCLE ( 'NONE', #193835, 4.050000000000000711 ) ;
#222859 = CARTESIAN_POINT ( 'NONE',  ( 20.85000000000000142, 76.00000000001170974, -69.52310748452431710 ) ) ;
#222860 = DIRECTION ( 'NONE',  ( 1.000000000000000000, 0.000000000000000000, 0.000000000000000000 ) ) ;
#222861 = CARTESIAN_POINT ( 'NONE',  ( 21.05000000000000071, 76.00000000001237765, -170.0231074845243597 ) ) ;
#222862 = CARTESIAN_POINT ( 'NONE',  ( -23.15000000000000213, -8.663551401858001100, -90.97589888193274987 ) ) ;
#222864 = DIRECTION ( 'NONE',  ( 0.000000000000000000, 0.000000000000000000, 1.000000000000000000 ) ) ;
#222863 = CARTESIAN_POINT ( 'NONE',  ( 20.95203847575071521, 65.49893946073788698, -95.45603613590083114 ) ) ;
#222865 = EDGE_CURVE ( 'NONE', #111551, #184113, #104869, .T. ) ;
#222866 = DIRECTION ( 'NONE',  ( 0.000000000000000000, 0.000000000000000000, 1.000000000000000000 ) ) ;
#222867 = DIRECTION ( 'NONE',  ( 1.000000000000000000, 0.000000000000000000, 0.000000000000000000 ) ) ;
#222868 = DIRECTION ( 'NONE',  ( 1.000000000000000000, 0.000000000000000000, -0.000000000000000000 ) ) ;
#222869 = CARTESIAN_POINT ( 'NONE',  ( 20.95325940946048249, 18.76594065868512118, -228.0282680241705293 ) ) ;
#222870 = EDGE_LOOP ( 'NONE', ( #175964, #236741, #171422, #100167 ) ) ;
#222871 = ORIENTED_EDGE ( 'NONE', *, *, #50601, .F. ) ;
#222872 = LINE ( 'NONE', #23432, #160913 ) ;
#222873 = DIRECTION ( 'NONE',  ( 0.000000000000000000, 0.000000000000000000, 1.000000000000000000 ) ) ;
#222875 = LINE ( 'NONE', #117371, #116084 ) ;
#222874 = FACE_OUTER_BOUND ( 'NONE', #6242, .T. ) ;
#222876 = FACE_OUTER_BOUND ( 'NONE', #24815, .T. ) ;
#222877 = CARTESIAN_POINT ( 'NONE',  ( -20.94999999999999929, 10.29270135741298731, -139.4573618871519614 ) ) ;
#222878 = EDGE_CURVE ( 'NONE', #30979, #68928, #187049, .T. ) ;
#222879 = CARTESIAN_POINT ( 'NONE',  ( -18.59999999999999787, -1.866714910046153308, -45.25267524628200988 ) ) ;
#222880 = FACE_OUTER_BOUND ( 'NONE', #241745, .T. ) ;
#222881 = ORIENTED_EDGE ( 'NONE', *, *, #8996, .T. ) ;
#222882 = CIRCLE ( 'NONE', #35487, 0.09999999999999178990 ) ;
#222883 = VECTOR ( 'NONE', #59376, 1000.000000000000000 ) ;
#222884 = CARTESIAN_POINT ( 'NONE',  ( 13.99999999999999822, 66.15000000001185754, -86.27310748452437394 ) ) ;
#222885 = VERTEX_POINT ( 'NONE', #145309 ) ;
#222886 = PLANE ( 'NONE',  #143132 ) ;
#222887 = VECTOR ( 'NONE', #177761, 999.9999999999998863 ) ;
#222888 = LINE ( 'NONE', #165510, #179817 ) ;
#222889 = AXIS2_PLACEMENT_3D ( 'NONE', #210172, #133195, #190617 ) ;
#222890 = CIRCLE ( 'NONE', #256151, 0.1999999999999987899 ) ;
#222891 = ORIENTED_EDGE ( 'NONE', *, *, #247314, .F. ) ;
#222892 = CARTESIAN_POINT ( 'NONE',  ( -18.51024323315077424, 18.37846419038447010, -236.9325101954433137 ) ) ;
#222893 = EDGE_LOOP ( 'NONE', ( #200125, #38005, #120039, #128760 ) ) ;
#222894 = DIRECTION ( 'NONE',  ( -1.000000000000000000, 0.000000000000000000, 0.000000000000000000 ) ) ;
#222896 = AXIS2_PLACEMENT_3D ( 'NONE', #56314, #75899, #25889 ) ;
#222895 = CARTESIAN_POINT ( 'NONE',  ( 21.14999999999999858, 1.115600667400684642E-11, -146.1500000000000341 ) ) ;
#222897 = DIRECTION ( 'NONE',  ( 0.000000000000000000, 0.000000000000000000, -1.000000000000000000 ) ) ;
#222898 = CARTESIAN_POINT ( 'NONE',  ( -18.49513951962167013, 77.27548444980108400, -241.6969386449946740 ) ) ;
#222899 = CARTESIAN_POINT ( 'NONE',  ( 20.73486653747088582, 68.75000000001155342, -56.87310748452436826 ) ) ;
#222900 = FACE_OUTER_BOUND ( 'NONE', #199614, .T. ) ;
#222901 = AXIS2_PLACEMENT_3D ( 'NONE', #53176, #132733, #33670 ) ;
#222902 = DIRECTION ( 'NONE',  ( 0.000000000000000000, 6.982962677686266711E-15, -1.000000000000000000 ) ) ;
#222903 = LINE ( 'NONE', #202076, #153896 ) ;
#222905 = ORIENTED_EDGE ( 'NONE', *, *, #192687, .F. ) ;
#222904 = CARTESIAN_POINT ( 'NONE',  ( 21.08750232978087524, 65.27513661400244871, -191.2942493115248510 ) ) ;
#222907 = DIRECTION ( 'NONE',  ( 1.000000000000000000, -0.000000000000000000, -0.000000000000000000 ) ) ;
#222906 = CARTESIAN_POINT ( 'NONE',  ( -18.54118089899630561, 85.46353763186074559, -196.4745298866561711 ) ) ;
#222908 = ORIENTED_EDGE ( 'NONE', *, *, #80202, .T. ) ;
#222910 = EDGE_LOOP ( 'NONE', ( #258073, #173390, #186359, #82381 ) ) ;
#222909 = CARTESIAN_POINT ( 'NONE',  ( -23.39999999999994529, 76.00000000001119815, -36.02310748452479316 ) ) ;
#222911 = ORIENTED_EDGE ( 'NONE', *, *, #223994, .F. ) ;
#222912 = CARTESIAN_POINT ( 'NONE',  ( 18.58685178364169488, 85.40673308381587958, -62.39868701543652918 ) ) ;
#222913 = DIRECTION ( 'NONE',  ( 0.000000000000000000, -8.881784197001832136E-16, -1.000000000000000000 ) ) ;
#222914 = DIRECTION ( 'NONE',  ( 0.000000000000000000, -1.000000000000000000, 0.000000000000000000 ) ) ;
#222915 = ORIENTED_EDGE ( 'NONE', *, *, #300, .F. ) ;
#222916 = DIRECTION ( 'NONE',  ( -0.000000000000000000, 0.4791956752371485107, 0.8777080977375185666 ) ) ;
#222917 = DIRECTION ( 'NONE',  ( 0.000000000000000000, 6.982962677686267499E-15, -1.000000000000000000 ) ) ;
#222919 = CARTESIAN_POINT ( 'NONE',  ( -16.77683809663752257, 23.65833333334447985, -184.2499999999999716 ) ) ;
#222918 = AXIS2_PLACEMENT_3D ( 'NONE', #72284, #73588, #209205 ) ;
#222920 = CARTESIAN_POINT ( 'NONE',  ( 21.14999999999999858, 64.35000000001156195, -57.37310748452439668 ) ) ;
#222921 = DIRECTION ( 'NONE',  ( 0.7070776581708965169, 0.000000000000000000, 0.7071359030027827286 ) ) ;
#222922 = EDGE_CURVE ( 'NONE', #92448, #236459, #46214, .T. ) ;
#222923 = DIRECTION ( 'NONE',  ( 1.000000000000000000, 0.000000000000000000, 0.000000000000000000 ) ) ;
#222924 = EDGE_LOOP ( 'NONE', ( #144098, #238991, #210289, #175722 ) ) ;
#222925 = ORIENTED_EDGE ( 'NONE', *, *, #66364, .T. ) ;
#222926 = DIRECTION ( 'NONE',  ( 0.000000000000000000, 0.000000000000000000, 1.000000000000000000 ) ) ;
#222927 = AXIS2_PLACEMENT_3D ( 'NONE', #121134, #216342, #200642 ) ;
#222928 = ORIENTED_EDGE ( 'NONE', *, *, #129149, .F. ) ;
#222929 = CIRCLE ( 'NONE', #27356, 3.999999999999998224 ) ;
#222930 = DIRECTION ( 'NONE',  ( 0.000000000000000000, 0.01562500000001045344, 0.9998779222360096863 ) ) ;
#222931 = ORIENTED_EDGE ( 'NONE', *, *, #29701, .F. ) ;
#222932 = DIRECTION ( 'NONE',  ( 0.000000000000000000, 0.2617529984164506107, 0.9651348961777299618 ) ) ;
#222933 = CARTESIAN_POINT ( 'NONE',  ( -18.59999999999999787, 11.65000000001115232, -107.5148057706540357 ) ) ;
#222934 = DIRECTION ( 'NONE',  ( 1.000000000000000000, -7.304098846218134667E-16, -5.100424963727255829E-30 ) ) ;
#222935 = ADVANCED_FACE ( 'NONE', ( #181888 ), #94994, .T. ) ;
#222936 = CARTESIAN_POINT ( 'NONE',  ( 23.24999999999999289, 69.35000000001180354, -81.67310748452436542 ) ) ;
#222937 = CARTESIAN_POINT ( 'NONE',  ( -18.59999999999999787, -10.80884033489985363, 6.100000000000002309 ) ) ;
#222938 = ORIENTED_EDGE ( 'NONE', *, *, #238282, .F. ) ;
#222939 = EDGE_CURVE ( 'NONE', #67174, #230022, #82741, .T. ) ;
#222940 = DIRECTION ( 'NONE',  ( 1.000000000000000000, 0.000000000000000000, -0.000000000000000000 ) ) ;
#222941 = DIRECTION ( 'NONE',  ( -0.000000000000000000, 0.000000000000000000, 1.000000000000000000 ) ) ;
#222942 = CARTESIAN_POINT ( 'NONE',  ( -21.14250536705909411, 1.115600667400684642E-11, -26.98182782311924655 ) ) ;
#222943 = DIRECTION ( 'NONE',  ( 1.000000000000000000, 0.000000000000000000, -0.000000000000000000 ) ) ;
#222944 = ORIENTED_EDGE ( 'NONE', *, *, #132758, .T. ) ;
#222945 = CIRCLE ( 'NONE', #27181, 0.09999999999999939493 ) ;
#222947 = CARTESIAN_POINT ( 'NONE',  ( -21.05000000000000071, 1.835341550235567887, -45.15515129256298366 ) ) ;
#222946 = DIRECTION ( 'NONE',  ( 0.000000000000000000, -0.2617529984165031243, -0.9651348961777157509 ) ) ;
#222948 = ORIENTED_EDGE ( 'NONE', *, *, #106028, .F. ) ;
#222951 = EDGE_LOOP ( 'NONE', ( #218511, #192874, #9031, #2720 ) ) ;
#222950 =( NAMED_UNIT ( * ) PLANE_ANGLE_UNIT ( ) SI_UNIT ( $, .RADIAN. ) );
#222949 = DIRECTION ( 'NONE',  ( 0.000000000000000000, 0.000000000000000000, 1.000000000000000000 ) ) ;
#222952 = EDGE_LOOP ( 'NONE', ( #9730, #155783, #181207, #134407, #84437, #125124, #108799 ) ) ;
#222953 = CARTESIAN_POINT ( 'NONE',  ( 20.94999999999999929, 67.22371710472012296, -191.3731074845244109 ) ) ;
#222954 = CARTESIAN_POINT ( 'NONE',  ( -23.25000000000000000, 16.02417409648692725, -219.3605785455116006 ) ) ;
#222955 = EDGE_CURVE ( 'NONE', #255897, #135478, #3395, .T. ) ;
#222956 = DIRECTION ( 'NONE',  ( -0.000000000000000000, 0.000000000000000000, 1.000000000000000000 ) ) ;
#222957 = VECTOR ( 'NONE', #99050, 1000.000000000000000 ) ;
#222958 = ORIENTED_EDGE ( 'NONE', *, *, #5488, .F. ) ;
#222959 = DIRECTION ( 'NONE',  ( -1.000000000000000000, 0.000000000000000000, 0.000000000000000000 ) ) ;
#222960 = ADVANCED_FACE ( 'NONE', ( #52636 ), #211739, .F. ) ;
#222961 = CYLINDRICAL_SURFACE ( 'NONE', #177817, 0.5000000000000004441 ) ;
#222962 = ADVANCED_FACE ( 'NONE', ( #68365 ), #129621, .T. ) ;
#222964 = DIRECTION ( 'NONE',  ( -1.000000000000000000, -0.000000000000000000, -0.000000000000000000 ) ) ;
#222963 = LINE ( 'NONE', #178757, #96896 ) ;
#222966 = ORIENTED_EDGE ( 'NONE', *, *, #195381, .F. ) ;
#222965 = CARTESIAN_POINT ( 'NONE',  ( -18.40000000000000213, 70.35000000001230092, -157.3731074845244109 ) ) ;
#222967 = EDGE_CURVE ( 'NONE', #97608, #236182, #193459, .T. ) ;
#222968 = ORIENTED_EDGE ( 'NONE', *, *, #181241, .F. ) ;
#222969 = CARTESIAN_POINT ( 'NONE',  ( 19.75857864376269291, 64.35000000001177511, -78.27310748452438816 ) ) ;
#222970 = CARTESIAN_POINT ( 'NONE',  ( 22.50497660315937765, -2.577283117375421817, -189.5360782167620073 ) ) ;
#222971 = AXIS2_PLACEMENT_3D ( 'NONE', #247062, #86691, #68450 ) ;
#222972 = VECTOR ( 'NONE', #83291, 1000.000000000000000 ) ;
#222973 = DIRECTION ( 'NONE',  ( -1.000000000000000000, 1.652117596168391700E-15, 0.000000000000000000 ) ) ;
#222974 = ORIENTED_EDGE ( 'NONE', *, *, #162726, .T. ) ;
#222975 = DIRECTION ( 'NONE',  ( 0.000000000000000000, 7.056502275159890832E-15, -1.000000000000000000 ) ) ;
#222976 = EDGE_CURVE ( 'NONE', #180734, #120848, #227125, .T. ) ;
#222977 = ORIENTED_EDGE ( 'NONE', *, *, #198849, .T. ) ;
#222978 = CARTESIAN_POINT ( 'NONE',  ( -23.15000000000000213, 76.00000000001195133, -103.0231074845243171 ) ) ;
#222979 = DIRECTION ( 'NONE',  ( 0.000000000000000000, 0.2617529984165033463, 0.9651348961777157509 ) ) ;
#222980 = CARTESIAN_POINT ( 'NONE',  ( 22.00411653962166625, 7.253442868381227093, -33.40096189421769424 ) ) ;
#222981 = ORIENTED_EDGE ( 'NONE', *, *, #98678, .F. ) ;
#222982 = FACE_OUTER_BOUND ( 'NONE', #236148, .T. ) ;
#222983 = ADVANCED_FACE ( 'NONE', ( #250831 ), #78240, .F. ) ;
#222984 = CIRCLE ( 'NONE', #18970, 0.09999999999999939493 ) ;
#222985 = CARTESIAN_POINT ( 'NONE',  ( 20.04999999999999716, 64.24389422848746278, -213.4417251850286164 ) ) ;
#222986 = CIRCLE ( 'NONE', #185583, 3.900000000000020783 ) ;
#222987 = CIRCLE ( 'NONE', #110574, 0.2000000000000058675 ) ;
#222988 = TOROIDAL_SURFACE ( 'NONE', #23111, 11.65000000000000036, 0.1000000000000000056 ) ;
#222989 = ORIENTED_EDGE ( 'NONE', *, *, #15416, .T. ) ;
#222990 = ORIENTED_EDGE ( 'NONE', *, *, #17527, .T. ) ;
#222991 = ORIENTED_EDGE ( 'NONE', *, *, #225396, .F. ) ;
#222992 = CARTESIAN_POINT ( 'NONE',  ( -20.98284271247461064, 6.322468214605803993, 12.11686199900910488 ) ) ;
#222993 = ORIENTED_EDGE ( 'NONE', *, *, #164632, .T. ) ;
#222995 = ORIENTED_EDGE ( 'NONE', *, *, #245230, .T. ) ;
#222994 = DIRECTION ( 'NONE',  ( 1.000000000000000000, 0.000000000000000000, 0.000000000000000000 ) ) ;
#222996 = VERTEX_POINT ( 'NONE', #232599 ) ;
#222999 = VERTEX_POINT ( 'NONE', #87889 ) ;
#222998 = ORIENTED_EDGE ( 'NONE', *, *, #257768, .F. ) ;
#222997 = FACE_OUTER_BOUND ( 'NONE', #185437, .T. ) ;
#223000 = DIRECTION ( 'NONE',  ( -1.000000000000000000, -0.000000000000000000, -0.000000000000000000 ) ) ;
#223001 = ORIENTED_EDGE ( 'NONE', *, *, #51077, .F. ) ;
#223002 = CARTESIAN_POINT ( 'NONE',  ( -18.59999999999999787, 9.350000000011156942, -88.35000000000003695 ) ) ;
#223003 = CARTESIAN_POINT ( 'NONE',  ( 21.04999999999999716, 69.69554417806426727, -103.0020720079842391 ) ) ;
#223004 = EDGE_CURVE ( 'NONE', #230108, #116223, #133470, .T. ) ;
#223005 = CARTESIAN_POINT ( 'NONE',  ( -18.46154800491017056, 86.89228561700184628, -199.5792417787053807 ) ) ;
#223006 = AXIS2_PLACEMENT_3D ( 'NONE', #166866, #246369, #67728 ) ;
#223007 = ORIENTED_EDGE ( 'NONE', *, *, #14671, .T. ) ;
#223008 = CARTESIAN_POINT ( 'NONE',  ( -20.85000000000000142, 43.35377423437995503, -245.1717807829448930 ) ) ;
#223010 = ORIENTED_EDGE ( 'NONE', *, *, #242280, .F. ) ;
#223009 = DIRECTION ( 'NONE',  ( 0.000000000000000000, 0.000000000000000000, -1.000000000000000000 ) ) ;
#223012 = CARTESIAN_POINT ( 'NONE',  ( -16.87304349924914604, 14.17879107892816215, -219.2907450666499471 ) ) ;
#223011 = CIRCLE ( 'NONE', #94027, 11.80000000000000426 ) ;
#223014 = ORIENTED_EDGE ( 'NONE', *, *, #88743, .F. ) ;
#223013 = DIRECTION ( 'NONE',  ( -1.652117596168391700E-15, -1.000000000000000000, 0.000000000000000000 ) ) ;
#223015 = EDGE_CURVE ( 'NONE', #171663, #5154, #30538, .T. ) ;
#223017 = EDGE_CURVE ( 'NONE', #121084, #206913, #207897, .T. ) ;
#223016 =( BOUNDED_CURVE ( )  B_SPLINE_CURVE ( 3, ( #155589, #235094, #116432, #195976 ),
 .UNSPECIFIED., .F., .F. ) 
 B_SPLINE_CURVE_WITH_KNOTS ( ( 4, 4 ),
 ( 0.5235987755982174363, 1.570796326794896558 ),
 .UNSPECIFIED. ) 
 CURVE ( )  GEOMETRIC_REPRESENTATION_ITEM ( )  RATIONAL_B_SPLINE_CURVE ( ( 1.000000000000000000, 0.9106836025229455567, 0.9106836025229455567, 1.000000000000000000 ) ) 
 REPRESENTATION_ITEM ( '' )  );
#223018 = ORIENTED_EDGE ( 'NONE', *, *, #140149, .T. ) ;
#223019 = B_SPLINE_CURVE_WITH_KNOTS ( 'NONE', 3,
 ( #253406, #38230, #218115, #119047 ),
 .UNSPECIFIED., .F., .F.,
 ( 4, 4 ),
 ( 0.000000000000000000, 0.001767853679387133359 ),
 .UNSPECIFIED. ) ;
#223020 = VECTOR ( 'NONE', #26026, 1000.000000000000000 ) ;
#223021 = AXIS2_PLACEMENT_3D ( 'NONE', #179985, #238661, #241242 ) ;
#223022 = CIRCLE ( 'NONE', #127351, 0.6000000000000033085 ) ;
#223023 = EDGE_CURVE ( 'NONE', #214758, #97941, #244824, .T. ) ;
#223024 = EDGE_CURVE ( 'NONE', #217291, #199045, #128334, .T. ) ;
#223025 = ORIENTED_EDGE ( 'NONE', *, *, #45499, .T. ) ;
#223026 = ORIENTED_EDGE ( 'NONE', *, *, #209204, .F. ) ;
#223027 = LINE ( 'NONE', #182645, #143540 ) ;
#223029 = EDGE_CURVE ( 'NONE', #73178, #207360, #172650, .T. ) ;
#223028 = CARTESIAN_POINT ( 'NONE',  ( -21.14999999999999858, 11.75000000001115552, -67.10000000000005116 ) ) ;
#223030 = ADVANCED_FACE ( 'NONE', ( #108767 ), #157394, .F. ) ;
#223033 = EDGE_LOOP ( 'NONE', ( #79798, #188290, #63886 ) ) ;
#223032 = ORIENTED_EDGE ( 'NONE', *, *, #151126, .T. ) ;
#223031 = AXIS2_PLACEMENT_3D ( 'NONE', #170488, #190000, #12667 ) ;
#223034 = ORIENTED_EDGE ( 'NONE', *, *, #71539, .T. ) ;
#223035 = DIRECTION ( 'NONE',  ( 0.000000000000000000, 0.000000000000000000, 1.000000000000000000 ) ) ;
#223036 = VERTEX_POINT ( 'NONE', #51329 ) ;
#223037 = AXIS2_PLACEMENT_3D ( 'NONE', #74732, #231217, #214207 ) ;
#223038 = ORIENTED_EDGE ( 'NONE', *, *, #168728, .T. ) ;
#223039 = ADVANCED_FACE ( 'NONE', ( #16115 ), #116479, .F. ) ;
#223040 = FACE_OUTER_BOUND ( 'NONE', #25460, .T. ) ;
#223042 = ORIENTED_EDGE ( 'NONE', *, *, #57315, .F. ) ;
#223041 = LINE ( 'NONE', #84783, #47579 ) ;
#223043 = DIRECTION ( 'NONE',  ( 0.000000000000000000, 0.9910827722268055195, 0.1332476588733540468 ) ) ;
#223044 = AXIS2_PLACEMENT_3D ( 'NONE', #123925, #163066, #104323 ) ;
#223046 = FACE_OUTER_BOUND ( 'NONE', #111629, .T. ) ;
#223045 = CYLINDRICAL_SURFACE ( 'NONE', #128085, 0.1000000000000028644 ) ;
#223047 = ORIENTED_EDGE ( 'NONE', *, *, #152746, .T. ) ;
#223049 = ORIENTED_EDGE ( 'NONE', *, *, #135045, .T. ) ;
#223048 = ORIENTED_EDGE ( 'NONE', *, *, #224582, .F. ) ;
#223050 = CARTESIAN_POINT ( 'NONE',  ( -21.04999999999999716, 76.08574093704612551, -209.9369337733373015 ) ) ;
#223051 = SURFACE_STYLE_FILL_AREA ( #63988 ) ;
#223052 = ORIENTED_EDGE ( 'NONE', *, *, #195068, .F. ) ;
#223053 =( BOUNDED_SURFACE ( )  B_SPLINE_SURFACE ( 3, 2, ( 
 ( #87423, #126568, #165714 ),
 ( #5296, #242647, #245238 ),
 ( #66598, #101832, #225631 ),
 ( #144826, #146121, #82265 ) ),
 .UNSPECIFIED., .F., .F., .F. ) 
 B_SPLINE_SURFACE_WITH_KNOTS ( ( 4, 4 ),
 ( 3, 3 ),
 ( 4.712388980384689674, 5.765869716888459173 ),
 ( 0.000000000000000000, 1.000000000000000000 ),
 .UNSPECIFIED. ) 
 GEOMETRIC_REPRESENTATION_ITEM ( )  RATIONAL_B_SPLINE_SURFACE ( (
 ( 1.000000000000000000, 0.7071067811865475727, 1.000000000000000000),
 ( 1.000000000000000000, 0.7953136715913045052, 1.000000000000000000),
 ( 1.000000000000000000, 0.8646876308615548679, 1.000000000000000000),
 ( 1.000000000000000000, 0.8984936768950610997, 1.000000000000000000) ) ) 
 REPRESENTATION_ITEM ( '' )  SURFACE ( )  );
#223054 = EDGE_CURVE ( 'NONE', #168030, #108506, #74194, .T. ) ;
#223055 = CARTESIAN_POINT ( 'NONE',  ( -21.55000000000000071, 9.712035112405693837, -211.5243229699422614 ) ) ;
#223056 = ORIENTED_EDGE ( 'NONE', *, *, #153555, .F. ) ;
#223057 = ORIENTED_EDGE ( 'NONE', *, *, #172724, .F. ) ;
#223058 = DIRECTION ( 'NONE',  ( -0.7071067811865389130, 0.1850873201762231746, 0.6824534298470456006 ) ) ;
#223060 = EDGE_CURVE ( 'NONE', #252099, #206043, #32503, .T. ) ;
#223059 = ORIENTED_EDGE ( 'NONE', *, *, #83448, .F. ) ;
#223061 = CARTESIAN_POINT ( 'NONE',  ( -20.94684162601830124, 11.75000000001115374, -107.3416439990470224 ) ) ;
#223062 = DIRECTION ( 'NONE',  ( -1.000000000000000000, -7.166229603267617241E-16, -4.447280054184918885E-16 ) ) ;
#223063 = VERTEX_POINT ( 'NONE', #158213 ) ;
#223064 = EDGE_CURVE ( 'NONE', #55133, #235552, #57384, .T. ) ;
#223065 = CARTESIAN_POINT ( 'NONE',  ( -23.25000000000000355, 65.95000000001158469, -56.77310748452439526 ) ) ;
#223066 = DIRECTION ( 'NONE',  ( 1.000000000000000000, 1.070816960479510500E-16, -0.000000000000000000 ) ) ;
#223068 = FACE_OUTER_BOUND ( 'NONE', #8438, .T. ) ;
#223067 = CYLINDRICAL_SURFACE ( 'NONE', #98648, 0.5000000000000004441 ) ;
#223069 = DIRECTION ( 'NONE',  ( -2.252264143451594314E-15, -0.1298341882520124002, -0.9915357197604841577 ) ) ;
#223070 = AXIS2_PLACEMENT_3D ( 'NONE', #148879, #228418, #193139 ) ;
#223071 = DIRECTION ( 'NONE',  ( -1.000000000000000000, -0.000000000000000000, 0.000000000000000000 ) ) ;
#223072 = CARTESIAN_POINT ( 'NONE',  ( 20.04999999999999716, 22.41143600680915426, -231.9928577185252152 ) ) ;
#223073 = CIRCLE ( 'NONE', #110648, 0.09999999999998898659 ) ;
#223074 = DIRECTION ( 'NONE',  ( -1.000000000000000000, 0.000000000000000000, -0.000000000000000000 ) ) ;
#223075 = DIRECTION ( 'NONE',  ( 0.000000000000000000, 0.9968797965484670343, 0.07893460099023182075 ) ) ;
#223076 = AXIS2_PLACEMENT_3D ( 'NONE', #196345, #116818, #13868 ) ;
#223077 = ORIENTED_EDGE ( 'NONE', *, *, #85777, .F. ) ;
#223078 = VECTOR ( 'NONE', #130302, 1000.000000000000000 ) ;
#223080 = EDGE_LOOP ( 'NONE', ( #99489, #52247, #5234, #2643 ) ) ;
#223079 = VERTEX_POINT ( 'NONE', #57766 ) ;
#223081 = ORIENTED_EDGE ( 'NONE', *, *, #52512, .F. ) ;
#223082 = CARTESIAN_POINT ( 'NONE',  ( -18.50000000000000000, 9.250000000011157297, -88.15000000000004832 ) ) ;
#223083 = FACE_OUTER_BOUND ( 'NONE', #109486, .T. ) ;
#223084 = VECTOR ( 'NONE', #208674, 1000.000000000000000 ) ;
#223086 = DIRECTION ( 'NONE',  ( 1.000000000000000000, 7.304098846218133681E-16, -4.217023435051677501E-16 ) ) ;
#223085 = CARTESIAN_POINT ( 'NONE',  ( 20.73486653747088226, 45.23934133962701765, -237.7629717664446503 ) ) ;
#223087 = CARTESIAN_POINT ( 'NONE',  ( 0.9000000000000535350, 64.25000000001119815, -7.323107484524790323 ) ) ;
#223089 = VERTEX_POINT ( 'NONE', #59026 ) ;
#223088 = AXIS2_PLACEMENT_3D ( 'NONE', #35850, #211918, #192341 ) ;
#223090 = DIRECTION ( 'NONE',  ( 1.000000000000000000, -0.000000000000000000, 0.000000000000000000 ) ) ;
#223091 = FACE_OUTER_BOUND ( 'NONE', #179933, .T. ) ;
#223092 = AXIS2_PLACEMENT_3D ( 'NONE', #47393, #128241, #205185 ) ;
#223093 = DIRECTION ( 'NONE',  ( 0.000000000000000000, -0.8164390028469705740, 0.5774316882803059992 ) ) ;
#223094 = LINE ( 'NONE', #66604, #53940 ) ;
#223095 = ORIENTED_EDGE ( 'NONE', *, *, #18746, .F. ) ;
#223096 = DIRECTION ( 'NONE',  ( 0.000000000000000000, 1.000000000000000000, 2.891205793294679805E-16 ) ) ;
#223097 = DIRECTION ( 'NONE',  ( -2.252264143451594314E-15, -0.1298341882520124002, -0.9915357197604841577 ) ) ;
#223098 = ORIENTED_EDGE ( 'NONE', *, *, #126989, .T. ) ;
#223099 = DIRECTION ( 'NONE',  ( 0.7071067811865474617, -0.7071067811865474617, -5.142139384388980375E-15 ) ) ;
#223100 = DIRECTION ( 'NONE',  ( 0.000000000000000000, 0.000000000000000000, -1.000000000000000000 ) ) ;
#223101 = AXIS2_PLACEMENT_3D ( 'NONE', #93763, #216274, #211154 ) ;
#223102 = DIRECTION ( 'NONE',  ( 0.000000000000000000, 1.192622389734062135E-14, -1.000000000000000000 ) ) ;
#223103 = CARTESIAN_POINT ( 'NONE',  ( -20.94999999999999929, 14.72981487416292623, -236.4853282537515895 ) ) ;
#223104 = CARTESIAN_POINT ( 'NONE',  ( 22.39999999999999503, 11.65000000001116298, -67.10000000000005116 ) ) ;
#223105 = CARTESIAN_POINT ( 'NONE',  ( -17.80356949363898877, 10.87673139700146763, -23.21307302422549768 ) ) ;
#223106 = EDGE_LOOP ( 'NONE', ( #59377, #13220, #244334, #165896 ) ) ;
#223107 = CARTESIAN_POINT ( 'NONE',  ( -20.54999999999999716, 1.115600667400684642E-11, -121.1250000000000426 ) ) ;
#223108 = DIRECTION ( 'NONE',  ( 1.000000000000000000, 0.000000000000000000, 0.000000000000000000 ) ) ;
#223109 = FACE_OUTER_BOUND ( 'NONE', #197049, .T. ) ;
#223110 = EDGE_CURVE ( 'NONE', #71927, #14083, #174160, .T. ) ;
#223112 = CARTESIAN_POINT ( 'NONE',  ( 19.97071067811864609, 64.27928932189330169, -111.7731074845243739 ) ) ;
#223111 = CARTESIAN_POINT ( 'NONE',  ( 20.94999999999999574, 67.07338541492450190, -61.05142446530125966 ) ) ;
#223113 = LINE ( 'NONE', #225660, #28953 ) ;
#223114 =( NAMED_UNIT ( * ) PLANE_ANGLE_UNIT ( ) SI_UNIT ( $, .RADIAN. ) );
#223116 = ADVANCED_FACE ( 'NONE', ( #119050 ), #173930, .T. ) ;
#223115 = FACE_OUTER_BOUND ( 'NONE', #188838, .T. ) ;
#223117 = CARTESIAN_POINT ( 'NONE',  ( 18.42636655943171320, -9.496944315759474620, -207.6090805711554879 ) ) ;
#223118 = AXIS2_PLACEMENT_3D ( 'NONE', #68543, #209317, #8568 ) ;
#223121 = ORIENTED_EDGE ( 'NONE', *, *, #245277, .T. ) ;
#223120 = VECTOR ( 'NONE', #60801, 1000.000000000000000 ) ;
#223119 = DIRECTION ( 'NONE',  ( -1.000000000000000000, -1.541880601228652843E-16, -2.878400969107353907E-16 ) ) ;
#223122 = AXIS2_PLACEMENT_3D ( 'NONE', #48757, #86578, #147881 ) ;
#223123 = AXIS2_PLACEMENT_3D ( 'NONE', #106053, #159986, #21746 ) ;
#223124 = EDGE_CURVE ( 'NONE', #82861, #167877, #65775, .T. ) ;
#223125 = EDGE_CURVE ( 'NONE', #106564, #209692, #194982, .T. ) ;
#223126 = LINE ( 'NONE', #83129, #154233 ) ;
#223127 = DIRECTION ( 'NONE',  ( -0.000000000000000000, 0.1350103645451835865, 0.9908441862701605762 ) ) ;
#223128 = CARTESIAN_POINT ( 'NONE',  ( 15.39793903038208178, 9.389686005666810331, -149.6728435063513132 ) ) ;
#223129 = CIRCLE ( 'NONE', #173123, 0.09999999999998898659 ) ;
#223130 = VERTEX_POINT ( 'NONE', #155638 ) ;
#223131 = ADVANCED_FACE ( 'NONE', ( #78614 ), #211532, .T. ) ;
#223132 = DIRECTION ( 'NONE',  ( 1.000000000000000000, 0.000000000000000000, 0.000000000000000000 ) ) ;
#223133 = EDGE_CURVE ( 'NONE', #149012, #249539, #115192, .T. ) ;
#223134 = CARTESIAN_POINT ( 'NONE',  ( -15.75000000000000355, 9.350000000011140955, -50.25000000000000711 ) ) ;
#223135 = DIRECTION ( 'NONE',  ( 0.000000000000000000, 1.000000000000000000, 1.265107689135680095E-16 ) ) ;
#223136 = CIRCLE ( 'NONE', #6480, 0.09999999999999939493 ) ;
#223137 = EDGE_LOOP ( 'NONE', ( #34050, #115703, #62693, #198140 ) ) ;
#223138 = DIRECTION ( 'NONE',  ( 0.000000000000000000, 1.000000000000000000, 0.000000000000000000 ) ) ;
#223140 = VERTEX_POINT ( 'NONE', #56476 ) ;
#223139 = LINE ( 'NONE', #182757, #100798 ) ;
#223142 = CARTESIAN_POINT ( 'NONE',  ( 21.07928932188134397, 0.09889514565439641580, 6.328516656393307294 ) ) ;
#223141 = DIRECTION ( 'NONE',  ( 1.000000000000000000, 0.000000000000000000, 0.000000000000000000 ) ) ;
#223143 = VERTEX_POINT ( 'NONE', #176469 ) ;
#223144 = DIRECTION ( 'NONE',  ( 0.000000000000000000, 0.000000000000000000, -1.000000000000000000 ) ) ;
#223145 = EDGE_CURVE ( 'NONE', #123340, #81862, #255927, .T. ) ;
#223146 = CARTESIAN_POINT ( 'NONE',  ( 21.05000000000000071, 67.22371735104096047, -128.0355151060064145 ) ) ;
#223147 = VERTEX_POINT ( 'NONE', #253409 ) ;
#223148 = DIRECTION ( 'NONE',  ( 0.000000000000000000, 0.000000000000000000, 1.000000000000000000 ) ) ;
#223149 = EDGE_CURVE ( 'NONE', #139621, #218429, #223976, .T. ) ;
#223150 = CIRCLE ( 'NONE', #252361, 0.2000000000000048406 ) ;
#223151 = CARTESIAN_POINT ( 'NONE',  ( 18.50000000000000711, 54.95667902235472724, -229.8578999281555753 ) ) ;
#223152 = DIRECTION ( 'NONE',  ( 0.000000000000000000, 1.897661533703519897E-16, -1.000000000000000000 ) ) ;
#223153 = DIRECTION ( 'NONE',  ( 1.000000000000000000, 0.000000000000000000, 0.000000000000000000 ) ) ;
#223154 = ORIENTED_EDGE ( 'NONE', *, *, #242088, .F. ) ;
#223155 = ORIENTED_EDGE ( 'NONE', *, *, #57620, .F. ) ;
#223156 = EDGE_CURVE ( 'NONE', #255700, #144708, #233857, .T. ) ;
#223157 = CARTESIAN_POINT ( 'NONE',  ( 18.59999999999999432, -1.835859311432481045, -212.5044391687984842 ) ) ;
#223158 = EDGE_CURVE ( 'NONE', #77934, #211293, #230865, .T. ) ;
#223159 = DIRECTION ( 'NONE',  ( -0.000000000000000000, 1.000000000000000000, 6.982962677686266711E-15 ) ) ;
#223160 = CYLINDRICAL_SURFACE ( 'NONE', #198331, 0.1000000000000106914 ) ;
#223161 = DIRECTION ( 'NONE',  ( 0.000000000000000000, 0.000000000000000000, 1.000000000000000000 ) ) ;
#223162 = CARTESIAN_POINT ( 'NONE',  ( -18.40000000000000213, 11.33174054713631662, -79.65000000000004832 ) ) ;
#223165 = CARTESIAN_POINT ( 'NONE',  ( 20.94999999999999929, 64.35000000001170406, -69.52310748452438816 ) ) ;
#223164 = CIRCLE ( 'NONE', #114850, 0.09999999999999520384 ) ;
#223163 = CYLINDRICAL_SURFACE ( 'NONE', #111670, 0.09999999999999939493 ) ;
#223166 = ADVANCED_FACE ( 'NONE', ( #250397 ), #71791, .T. ) ;
#223167 = CARTESIAN_POINT ( 'NONE',  ( -18.50000000000000000, 76.00000000001142553, -36.02310748452432421 ) ) ;
#223168 = VECTOR ( 'NONE', #69686, 1000.000000000000000 ) ;
#223169 = DIRECTION ( 'NONE',  ( 1.224646799147353207E-16, -1.000000000000000000, -6.982962677686266711E-15 ) ) ;
#223170 = CARTESIAN_POINT ( 'NONE',  ( -18.49346865148373098, 47.07686520425682630, -255.2314089849770937 ) ) ;
#223171 = VECTOR ( 'NONE', #255172, 1000.000000000000000 ) ;
#223172 = DIRECTION ( 'NONE',  ( -3.265361837132813093E-16, -1.000000000000000000, -7.026728003956683390E-15 ) ) ;
#223173 = AXIS2_PLACEMENT_3D ( 'NONE', #6211, #222684, #64903 ) ;
#223175 = VERTEX_POINT ( 'NONE', #10519 ) ;
#223174 = DIRECTION ( 'NONE',  ( 0.000000000000000000, -0.8660254037844383745, 0.5000000000000003331 ) ) ;
#223176 = CARTESIAN_POINT ( 'NONE',  ( 20.95545211741311320, 65.41358668846868341, -195.9369606249361198 ) ) ;
#223177 = DIRECTION ( 'NONE',  ( -1.000000000000000000, 0.000000000000000000, 0.000000000000000000 ) ) ;
#223179 = CARTESIAN_POINT ( 'NONE',  ( -20.65000000000000568, 7.250000000011138646, -113.1500000000000341 ) ) ;
#223178 = CARTESIAN_POINT ( 'NONE',  ( 18.59999999999999076, 1.115600667400684642E-11, -167.5000000000000284 ) ) ;
#223180 = ORIENTED_EDGE ( 'NONE', *, *, #25859, .F. ) ;
#223181 = DIRECTION ( 'NONE',  ( 0.7071067811865475727, 0.6909108974501237954, 0.1504730267678056066 ) ) ;
#223182 = CARTESIAN_POINT ( 'NONE',  ( 21.00000000000000000, 30.46448808713892831, -235.1722212069449256 ) ) ;
#223183 = EDGE_CURVE ( 'NONE', #236853, #26557, #107469, .T. ) ;
#223184 = CARTESIAN_POINT ( 'NONE',  ( 21.13461538461538325, 65.38541703798651383, -124.1731074845243654 ) ) ;
#223185 = LINE ( 'NONE', #146217, #257522 ) ;
#223186 = CARTESIAN_POINT ( 'NONE',  ( -14.56336952470178758, 66.55335465531733519, -185.1123010284241843 ) ) ;
#223187 = VERTEX_POINT ( 'NONE', #233433 ) ;
#223188 = VERTEX_POINT ( 'NONE', #211282 ) ;
#223189 = ADVANCED_FACE ( 'NONE', ( #35243 ), #103171, .T. ) ;
#223190 = DIRECTION ( 'NONE',  ( 0.000000000000000000, 0.000000000000000000, -1.000000000000000000 ) ) ;
#223191 = ORIENTED_EDGE ( 'NONE', *, *, #3966, .F. ) ;
#223192 = CARTESIAN_POINT ( 'NONE',  ( 20.02499999999999858, 30.37633856152204359, -235.1250019192171408 ) ) ;
#223193 = AXIS2_PLACEMENT_3D ( 'NONE', #104514, #184082, #44583 ) ;
#223194 = ORIENTED_EDGE ( 'NONE', *, *, #44962, .T. ) ;
#223195 = LINE ( 'NONE', #141118, #172736 ) ;
#223196 = AXIS2_PLACEMENT_3D ( 'NONE', #84348, #161397, #41456 ) ;
#223197 = DIRECTION ( 'NONE',  ( 4.408576920032447355E-17, -0.1350103645451876666, -0.9908441862701600211 ) ) ;
#223198 = CARTESIAN_POINT ( 'NONE',  ( -21.04386569057571421, 62.86478208612209073, -207.0655967136950721 ) ) ;
#223200 = ORIENTED_EDGE ( 'NONE', *, *, #66518, .F. ) ;
#223199 = CIRCLE ( 'NONE', #64987, 0.09999999999999939493 ) ;
#223201 = VECTOR ( 'NONE', #213631, 1000.000000000000000 ) ;
#223202 = CARTESIAN_POINT ( 'NONE',  ( 16.87683809663749557, 9.950000000011131718, -121.3500000000000369 ) ) ;
#223204 = DIRECTION ( 'NONE',  ( 1.000000000000000000, -0.000000000000000000, -0.000000000000000000 ) ) ;
#223203 = CIRCLE ( 'NONE', #252412, 11.80000000000000426 ) ;
#223205 = DIRECTION ( 'NONE',  ( 0.000000000000000000, -0.07847809223012357227, -0.9969158384938622275 ) ) ;
#223206 = LINE ( 'NONE', #95871, #95651 ) ;
#223207 = DIRECTION ( 'NONE',  ( 1.000000000000000000, 0.000000000000000000, 0.000000000000000000 ) ) ;
#223208 = DIRECTION ( 'NONE',  ( -1.000000000000000000, 0.000000000000000000, 0.000000000000000000 ) ) ;
#223209 = CARTESIAN_POINT ( 'NONE',  ( 20.94999999999999574, 13.63177590472475487, -238.5351604075707144 ) ) ;
#223210 = EDGE_LOOP ( 'NONE', ( #6158, #216930, #191596, #238239 ) ) ;
#223212 = CARTESIAN_POINT ( 'NONE',  ( -18.50000000000000000, 66.75000000001205080, -124.1731074845243654 ) ) ;
#223211 = DIRECTION ( 'NONE',  ( 4.408576920032447355E-17, -0.8490545835447252943, -0.5283051335749947564 ) ) ;
#223213 = ORIENTED_EDGE ( 'NONE', *, *, #74399, .F. ) ;
#223215 = VERTEX_POINT ( 'NONE', #252960 ) ;
#223214 = LINE ( 'NONE', #257163, #198082 ) ;
#223216 = AXIS2_PLACEMENT_3D ( 'NONE', #33538, #50454, #149611 ) ;
#223217 = ORIENTED_EDGE ( 'NONE', *, *, #198365, .T. ) ;
#223218 = DIRECTION ( 'NONE',  ( -0.000000000000000000, 0.000000000000000000, 1.000000000000000000 ) ) ;
#223219 = DIRECTION ( 'NONE',  ( 0.000000000000000000, -0.9770955615653312831, -0.2128009952263614224 ) ) ;
#223220 = AXIS2_PLACEMENT_3D ( 'NONE', #231869, #53211, #132771 ) ;
#223221 = CARTESIAN_POINT ( 'NONE',  ( 20.95512840106819752, 60.17186297114481874, -221.2972637402838245 ) ) ;
#223222 = CARTESIAN_POINT ( 'NONE',  ( 23.15000000000000213, 30.69873658968802133, -264.9868732779115703 ) ) ;
#223223 = EDGE_LOOP ( 'NONE', ( #210621, #240508, #234723, #154064 ) ) ;
#223224 = DIRECTION ( 'NONE',  ( 1.000000000000000000, 0.000000000000000000, 0.000000000000000000 ) ) ;
#223225 = CARTESIAN_POINT ( 'NONE',  ( -23.15000000000000213, 74.08971962618045382, -149.1544753397233194 ) ) ;
#223226 = CIRCLE ( 'NONE', #110800, 0.1000000000000055844 ) ;
#223227 = ORIENTED_EDGE ( 'NONE', *, *, #25309, .T. ) ;
#223228 = CARTESIAN_POINT ( 'NONE',  ( -20.94999675878240808, 10.29307482167955357, -38.95864214669402514 ) ) ;
#223229 = ADVANCED_FACE ( 'NONE', ( #189147 ), #49345, .T. ) ;
#223230 = CIRCLE ( 'NONE', #244083, 0.1000000000000033223 ) ;
#223231 = CARTESIAN_POINT ( 'NONE',  ( -23.15000000000000213, 74.00000000001223555, -149.1477294072864765 ) ) ;
#223232 = EDGE_LOOP ( 'NONE', ( #103084, #81420, #171846, #203448 ) ) ;
#223233 = DIRECTION ( 'NONE',  ( 0.000000000000000000, 0.000000000000000000, -1.000000000000000000 ) ) ;
#223234 = ORIENTED_EDGE ( 'NONE', *, *, #137639, .F. ) ;
#223235 = CARTESIAN_POINT ( 'NONE',  ( 21.05000000000000071, 7.300274141770061398, -211.7264450054621534 ) ) ;
#223236 = ORIENTED_EDGE ( 'NONE', *, *, #75687, .T. ) ;
#223237 = FACE_OUTER_BOUND ( 'NONE', #105200, .T. ) ;
#223238 = EDGE_CURVE ( 'NONE', #104039, #180952, #213844, .T. ) ;
#223239 = CARTESIAN_POINT ( 'NONE',  ( 18.50000000000000000, -9.399999999988843058, -107.3820418481727188 ) ) ;
#223240 = DIRECTION ( 'NONE',  ( 0.000000000000000000, 0.000000000000000000, 1.000000000000000000 ) ) ;
#223241 = CARTESIAN_POINT ( 'NONE',  ( -22.00411653962173375, 7.066231425286666479, -199.3596904452039382 ) ) ;
#223242 = CIRCLE ( 'NONE', #110827, 0.1000000000000028644 ) ;
#223243 = ADVANCED_FACE ( 'NONE', ( #73090 ), #190711, .T. ) ;
#223244 = EDGE_CURVE ( 'NONE', #168568, #189415, #61682, .T. ) ;
#223245 = AXIS2_PLACEMENT_3D ( 'NONE', #144382, #4870, #244783 ) ;
#223246 = AXIS2_PLACEMENT_3D ( 'NONE', #244886, #150932, #205757 ) ;
#223247 = AXIS2_PLACEMENT_3D ( 'NONE', #95652, #175246, #196056 ) ;
#223248 = DIRECTION ( 'NONE',  ( 0.000000000000000000, 1.000000000000000000, 6.982962677686266711E-15 ) ) ;
#223249 = DIRECTION ( 'NONE',  ( 0.000000000000000000, 0.000000000000000000, -1.000000000000000000 ) ) ;
#223250 = CARTESIAN_POINT ( 'NONE',  ( 20.94999999999999929, 10.29288807859936838, -72.45800201601217339 ) ) ;
#223251 = ORIENTED_EDGE ( 'NONE', *, *, #159794, .F. ) ;
#223253 = CARTESIAN_POINT ( 'NONE',  ( -23.15000000000000213, 1.115600667400684642E-11, -154.6250000000000284 ) ) ;
#223252 = CARTESIAN_POINT ( 'NONE',  ( -21.05000000000000071, 69.52192177891774350, -169.9231075492199352 ) ) ;
#223254 = AXIS2_PLACEMENT_3D ( 'NONE', #36379, #178459, #79305 ) ;
#223255 = VERTEX_POINT ( 'NONE', #91342 ) ;
#223256 = DIRECTION ( 'NONE',  ( -0.000000000000000000, -6.982962677686266711E-15, 1.000000000000000000 ) ) ;
#223257 = ADVANCED_FACE ( 'NONE', ( #152621 ), #240754, .T. ) ;
#223258 = CARTESIAN_POINT ( 'NONE',  ( 20.94999999999999929, 43.24695311518262031, -245.0026972281755491 ) ) ;
#223260 = ORIENTED_EDGE ( 'NONE', *, *, #177318, .T. ) ;
#223259 = DIRECTION ( 'NONE',  ( 0.000000000000000000, 0.000000000000000000, 1.000000000000000000 ) ) ;
#223262 = ORIENTED_EDGE ( 'NONE', *, *, #4786, .F. ) ;
#223261 = CARTESIAN_POINT ( 'NONE',  ( -18.39999999999999858, 85.50000000001210765, -129.9229180933022576 ) ) ;
#223263 = CARTESIAN_POINT ( 'NONE',  ( -18.50000000000000000, 11.64999999999999680, -7.014805770654001016 ) ) ;
#223265 = DIRECTION ( 'NONE',  ( -1.000000000000000000, 0.000000000000000000, 0.000000000000000000 ) ) ;
#223264 = VECTOR ( 'NONE', #224979, 1000.000000000000114 ) ;
#223266 = FACE_OUTER_BOUND ( 'NONE', #134164, .T. ) ;
#223267 = CARTESIAN_POINT ( 'NONE',  ( 20.94999999999999929, 84.66355140188063899, -45.54720860259157433 ) ) ;
#223268 = CIRCLE ( 'NONE', #123503, 0.09999999999999520384 ) ;
#223270 = ORIENTED_EDGE ( 'NONE', *, *, #23743, .T. ) ;
#223269 = CARTESIAN_POINT ( 'NONE',  ( 20.95512828230159030, 67.12384868768700130, -157.8206772190212916 ) ) ;
#223271 = AXIS2_PLACEMENT_3D ( 'NONE', #193359, #152971, #212909 ) ;
#223272 = DIRECTION ( 'NONE',  ( 4.239556034732056743E-17, 0.1298341882519953860, 0.9915357197604862671 ) ) ;
#223273 = ORIENTED_EDGE ( 'NONE', *, *, #195026, .F. ) ;
#223274 = ADVANCED_FACE ( 'NONE', ( #151327 ), #228289, .F. ) ;
#223275 = ORIENTED_EDGE ( 'NONE', *, *, #63294, .F. ) ;
#223276 = VECTOR ( 'NONE', #143145, 1000.000000000000000 ) ;
#223277 = FACE_OUTER_BOUND ( 'NONE', #38770, .T. ) ;
#223278 = CARTESIAN_POINT ( 'NONE',  ( 18.49999999999998934, 69.55000000001230376, -160.0060803140843859 ) ) ;
#223279 = ORIENTED_EDGE ( 'NONE', *, *, #208004, .F. ) ;
#223280 = FACE_OUTER_BOUND ( 'NONE', #221330, .T. ) ;
#223282 = EDGE_CURVE ( 'NONE', #23304, #8981, #36784, .T. ) ;
#223281 = CARTESIAN_POINT ( 'NONE',  ( -16.88495309932523369, 9.954627058484017965, -180.1345486738118780 ) ) ;
#223283 = ORIENTED_EDGE ( 'NONE', *, *, #255058, .T. ) ;
#223284 = AXIS2_PLACEMENT_3D ( 'NONE', #46085, #228602, #248149 ) ;
#223285 = CIRCLE ( 'NONE', #119263, 0.1000000000000026007 ) ;
#223286 = DIRECTION ( 'NONE',  ( -1.000000000000000000, -2.952720810173289112E-16, 0.000000000000000000 ) ) ;
#223287 = VECTOR ( 'NONE', #152571, 999.9999999999998863 ) ;
#223288 = CARTESIAN_POINT ( 'NONE',  ( -23.25000000000000355, 70.35000000001160458, -60.27310748452436684 ) ) ;
#223289 = ORIENTED_EDGE ( 'NONE', *, *, #187853, .T. ) ;
#223290 = ORIENTED_EDGE ( 'NONE', *, *, #244257, .T. ) ;
#223291 = CARTESIAN_POINT ( 'NONE',  ( -18.59999999999999787, 1.835341550235567887, -112.1551512925630192 ) ) ;
#223292 = VERTEX_POINT ( 'NONE', #247833 ) ;
#223293 = DIRECTION ( 'NONE',  ( 0.000000000000000000, -1.000000000000000000, -6.982962677686265922E-15 ) ) ;
#223294 = ORIENTED_EDGE ( 'NONE', *, *, #49861, .T. ) ;
#223296 = ORIENTED_EDGE ( 'NONE', *, *, #72082, .F. ) ;
#223295 = DIRECTION ( 'NONE',  ( 1.000000000000000000, 0.000000000000000000, 0.000000000000000000 ) ) ;
#223297 = DIRECTION ( 'NONE',  ( 0.000000000000000000, 0.000000000000000000, 1.000000000000000000 ) ) ;
#223298 = ORIENTED_EDGE ( 'NONE', *, *, #42790, .F. ) ;
#223299 = EDGE_CURVE ( 'NONE', #172948, #14805, #155587, .T. ) ;
#223300 = CARTESIAN_POINT ( 'NONE',  ( 22.40000000000010516, 1.019545479467800000E-11, -88.74956710754109679 ) ) ;
#223301 = ORIENTED_EDGE ( 'NONE', *, *, #229565, .F. ) ;
#223303 = EDGE_LOOP ( 'NONE', ( #91211, #64523, #215823, #188726 ) ) ;
#223302 = ORIENTED_EDGE ( 'NONE', *, *, #53180, .T. ) ;
#223304 = CARTESIAN_POINT ( 'NONE',  ( 21.05000000000000071, 69.45934304831089889, -136.5231074845243313 ) ) ;
#223305 = VECTOR ( 'NONE', #249133, 1000.000000000000000 ) ;
#223306 = CARTESIAN_POINT ( 'NONE',  ( -20.94999999999999929, 56.24810294282605128, -228.0242159533278254 ) ) ;
#223307 = AXIS2_PLACEMENT_3D ( 'NONE', #220551, #142286, #139705 ) ;
#223308 = EDGE_LOOP ( 'NONE', ( #202008, #151360, #4285, #83749 ) ) ;
#223309 = EDGE_CURVE ( 'NONE', #237217, #27502, #124239, .T. ) ;
#223310 = ADVANCED_FACE ( 'NONE', ( #135571 ), #196835, .F. ) ;
#223311 = ORIENTED_EDGE ( 'NONE', *, *, #4678, .F. ) ;
#223312 = DIRECTION ( 'NONE',  ( 0.000000000000000000, -0.8700118002898357128, 0.4930308989875171188 ) ) ;
#223313 = LINE ( 'NONE', #145066, #255450 ) ;
#223315 = VERTEX_POINT ( 'NONE', #98998 ) ;
#223314 = CARTESIAN_POINT ( 'NONE',  ( -18.34374000495059676, 64.52683809664901560, -45.27310748452439526 ) ) ;
#223316 = CARTESIAN_POINT ( 'NONE',  ( -23.25000000000000000, 71.65000000001207070, -124.3731074845243256 ) ) ;
#223317 = VERTEX_POINT ( 'NONE', #237267 ) ;
#223318 = EDGE_CURVE ( 'NONE', #22582, #106308, #200705, .T. ) ;
#223320 = ADVANCED_FACE ( 'NONE', ( #58603 ), #258060, .T. ) ;
#223319 = CARTESIAN_POINT ( 'NONE',  ( 18.59999999999999076, 6.550000000011156231, -110.5170271704400591 ) ) ;
#223321 = CARTESIAN_POINT ( 'NONE',  ( 20.27550659511089037, 66.78395627750339258, -149.1731074845244223 ) ) ;
#223322 = VERTEX_POINT ( 'NONE', #179870 ) ;
#223323 = DIRECTION ( 'NONE',  ( 1.000000000000000000, 0.000000000000000000, 0.000000000000000000 ) ) ;
#223324 = FACE_OUTER_BOUND ( 'NONE', #243610, .T. ) ;
#223325 = EDGE_CURVE ( 'NONE', #114232, #55645, #58979, .T. ) ;
#223326 = ORIENTED_EDGE ( 'NONE', *, *, #208820, .F. ) ;
#223327 = FACE_OUTER_BOUND ( 'NONE', #11677, .T. ) ;
#223328 = ORIENTED_EDGE ( 'NONE', *, *, #113245, .F. ) ;
#223329 = EDGE_CURVE ( 'NONE', #237621, #233645, #36963, .T. ) ;
#223330 = TOROIDAL_SURFACE ( 'NONE', #61019, 0.2000000000000000111, 0.1000000000000000056 ) ;
#223332 = EDGE_CURVE ( 'NONE', #64966, #245973, #16942, .T. ) ;
#223331 = EDGE_CURVE ( 'NONE', #223130, #177869, #103541, .T. ) ;
#223334 = ORIENTED_EDGE ( 'NONE', *, *, #31567, .F. ) ;
#223333 = VERTEX_POINT ( 'NONE', #118617 ) ;
#223335 = ORIENTED_EDGE ( 'NONE', *, *, #195271, .F. ) ;
#223336 = DIRECTION ( 'NONE',  ( -1.000000000000000000, -0.000000000000000000, 0.000000000000000000 ) ) ;
#223337 = ORIENTED_EDGE ( 'NONE', *, *, #106194, .F. ) ;
#223338 = FACE_OUTER_BOUND ( 'NONE', #181937, .T. ) ;
#223339 = ORIENTED_EDGE ( 'NONE', *, *, #39156, .T. ) ;
#223340 = CARTESIAN_POINT ( 'NONE',  ( -16.92570016628983609, 66.04121104227165517, -48.64375815456339325 ) ) ;
#223341 = CARTESIAN_POINT ( 'NONE',  ( -18.34374000495059676, 64.52683809665003878, -179.2731074845244450 ) ) ;
#223342 = ORIENTED_EDGE ( 'NONE', *, *, #159089, .F. ) ;
#223343 = ADVANCED_FACE ( 'NONE', ( #136870 ), #128501, .T. ) ;
#223344 = ORIENTED_EDGE ( 'NONE', *, *, #27298, .T. ) ;
#223345 = CIRCLE ( 'NONE', #85958, 0.09999999999999939493 ) ;
#223346 = EDGE_CURVE ( 'NONE', #42531, #180924, #158809, .T. ) ;
#223347 = EDGE_CURVE ( 'NONE', #200249, #177586, #119913, .T. ) ;
#223348 = ORIENTED_EDGE ( 'NONE', *, *, #253647, .F. ) ;
#223349 = VECTOR ( 'NONE', #50286, 1000.000000000000000 ) ;
#223350 = AXIS2_PLACEMENT_3D ( 'NONE', #207993, #71052, #106276 ) ;
#223351 = MECHANICAL_DESIGN_GEOMETRIC_PRESENTATION_REPRESENTATION (  '', ( #127516 ), #194170 ) ;
#223352 = EDGE_CURVE ( 'NONE', #29761, #118692, #95186, .T. ) ;
#223353 = LINE ( 'NONE', #124281, #84577 ) ;
#223354 = VERTEX_POINT ( 'NONE', #121201 ) ;
#223355 = CARTESIAN_POINT ( 'NONE',  ( -21.05000000000000071, 76.00000000001126921, -203.5231074845248997 ) ) ;
#223356 = CARTESIAN_POINT ( 'NONE',  ( 21.05000000000000071, 43.51422117117169108, -240.0698702536254530 ) ) ;
#223357 = DIRECTION ( 'NONE',  ( 0.000000000000000000, -0.8068669527897506244, -0.5907332058516622242 ) ) ;
#223358 = DIRECTION ( 'NONE',  ( 0.000000000000000000, 0.000000000000000000, -1.000000000000000000 ) ) ;
#223359 = EDGE_CURVE ( 'NONE', #94374, #124226, #32693, .T. ) ;
#223360 = CARTESIAN_POINT ( 'NONE',  ( 21.05000000000000071, 65.43728505328384415, -162.5663053788799743 ) ) ;
#223361 = DIRECTION ( 'NONE',  ( 1.000000000000000000, 0.000000000000000000, 0.000000000000000000 ) ) ;
#223362 = CYLINDRICAL_SURFACE ( 'NONE', #102247, 0.1000000000000028644 ) ;
#223364 = CARTESIAN_POINT ( 'NONE',  ( 21.11101077988997332, 6.423684734737197921, -100.4847147310857167 ) ) ;
#223363 = DIRECTION ( 'NONE',  ( 0.000000000000000000, -0.2617529984165045120, -0.9651348961777153068 ) ) ;
#223365 = DIRECTION ( 'NONE',  ( -2.840903330521632269E-16, -0.8700118002898356018, 0.4930308989875170078 ) ) ;
#223366 = DIRECTION ( 'NONE',  ( -1.000000000000000000, -7.304098846218105085E-16, -4.217023435051676515E-16 ) ) ;
#223367 = CYLINDRICAL_SURFACE ( 'NONE', #68634, 0.09999999999999986677 ) ;
#223368 = FACE_OUTER_BOUND ( 'NONE', #26848, .T. ) ;
#223369 = ORIENTED_EDGE ( 'NONE', *, *, #7808, .F. ) ;
#223370 = TOROIDAL_SURFACE ( 'NONE', #94375, 0.2000000000000000111, 0.1000000000000000056 ) ;
#223372 = ORIENTED_EDGE ( 'NONE', *, *, #113015, .F. ) ;
#223371 = DIRECTION ( 'NONE',  ( 0.000000000000000000, 0.000000000000000000, -1.000000000000000000 ) ) ;
#223373 = CIRCLE ( 'NONE', #110968, 0.09999999999998898659 ) ;
#223374 = VERTEX_POINT ( 'NONE', #24167 ) ;
#223375 = DIRECTION ( 'NONE',  ( 0.000000000000000000, -0.9651348961777157509, 0.2617529984165031243 ) ) ;
#223376 = CARTESIAN_POINT ( 'NONE',  ( -20.54999999999999716, 74.00000000001254818, -183.2477294072864709 ) ) ;
#223377 = AXIS2_PLACEMENT_3D ( 'NONE', #94651, #115498, #212057 ) ;
#223378 = LINE ( 'NONE', #8216, #157092 ) ;
#223379 = ORIENTED_EDGE ( 'NONE', *, *, #220191, .F. ) ;
#223380 = DIRECTION ( 'NONE',  ( 0.7071067811865475727, 0.7071067811865475727, 2.044391222244500083E-16 ) ) ;
#223381 = DIRECTION ( 'NONE',  ( -6.938893903907222856E-15, -1.000000000000000000, -7.272083257015735086E-15 ) ) ;
#223382 = VERTEX_POINT ( 'NONE', #60686 ) ;
#223384 = DIRECTION ( 'NONE',  ( 0.000000000000000000, -6.608470384673536035E-15, 1.000000000000000000 ) ) ;
#223383 = VECTOR ( 'NONE', #256023, 999.9999999999998863 ) ;
#223385 = CARTESIAN_POINT ( 'NONE',  ( 22.16821283564876666, 68.44102665923090001, -69.52310748452437394 ) ) ;
#223386 = AXIS2_PLACEMENT_3D ( 'NONE', #55333, #236563, #74967 ) ;
#223387 = FACE_OUTER_BOUND ( 'NONE', #150144, .T. ) ;
#223388 = AXIS2_PLACEMENT_3D ( 'NONE', #46462, #221246, #81718 ) ;
#223389 = CARTESIAN_POINT ( 'NONE',  ( 18.59999999999999076, 11.65000000001115943, -192.3499999999999659 ) ) ;
#223391 = VERTEX_POINT ( 'NONE', #64551 ) ;
#223390 = CARTESIAN_POINT ( 'NONE',  ( -21.14999999999999858, -10.76604040606818025, -206.3127087229280789 ) ) ;
#223393 = LINE ( 'NONE', #222095, #186025 ) ;
#223392 = VECTOR ( 'NONE', #219796, 1000.000000000000000 ) ;
#223395 = ORIENTED_EDGE ( 'NONE', *, *, #39946, .F. ) ;
#223394 = CARTESIAN_POINT ( 'NONE',  ( -16.27683809663751191, 9.349999999999978328, -9.249999999999966249 ) ) ;
#223396 = CARTESIAN_POINT ( 'NONE',  ( 18.49999999999999645, 1.162701749949165642, -142.1000000000000227 ) ) ;
#223397 = CARTESIAN_POINT ( 'NONE',  ( 18.59999999999999432, -1.135018845899022466, -108.2169768834323662 ) ) ;
#223398 = ORIENTED_EDGE ( 'NONE', *, *, #215010, .F. ) ;
#223399 = CARTESIAN_POINT ( 'NONE',  ( 23.14999999999998437, -11.74999999998884448, -134.0000000000000000 ) ) ;
#223400 = DIRECTION ( 'NONE',  ( 0.7071359030028288029, 0.000000000000000000, 0.7070776581708504427 ) ) ;
#223401 = ADVANCED_FACE ( 'NONE', ( #5846 ), #221050, .T. ) ;
#223403 = DIRECTION ( 'NONE',  ( 1.000000000000000000, 0.000000000000000000, 0.000000000000000000 ) ) ;
#223402 = CARTESIAN_POINT ( 'NONE',  ( -16.93294127766158752, 63.05522583286660421, -213.0365540695144944 ) ) ;
#223404 = CARTESIAN_POINT ( 'NONE',  ( 22.60000000000000142, 64.25043287652255231, -103.1239658536231047 ) ) ;
#223405 = CARTESIAN_POINT ( 'NONE',  ( 20.95346350065193519, 40.79338854218204347, -237.9607482723631051 ) ) ;
#223406 = AXIS2_PLACEMENT_3D ( 'NONE', #50460, #130004, #209567 ) ;
#223407 = CARTESIAN_POINT ( 'NONE',  ( -18.59117750673696889, 10.33248238082519066, -39.09484654391314962 ) ) ;
#223408 = DIRECTION ( 'NONE',  ( 1.000000000000000000, -2.986185139342070877E-16, 6.665775143889692774E-16 ) ) ;
#223409 = EDGE_CURVE ( 'NONE', #101582, #174818, #157587, .T. ) ;
#223410 = DIRECTION ( 'NONE',  ( 1.000000000000000000, 0.000000000000000000, 0.000000000000000000 ) ) ;
#223411 = EDGE_LOOP ( 'NONE', ( #128102, #247021, #6036, #237184 ) ) ;
#223412 = DIRECTION ( 'NONE',  ( 0.000000000000000000, 0.000000000000000000, 1.000000000000000000 ) ) ;
#223413 = ORIENTED_EDGE ( 'NONE', *, *, #170637, .T. ) ;
#223414 = ORIENTED_EDGE ( 'NONE', *, *, #214919, .F. ) ;
#223415 = EDGE_CURVE ( 'NONE', #172696, #242555, #90891, .T. ) ;
#223416 = CARTESIAN_POINT ( 'NONE',  ( -20.85000000106584750, 11.74999999999999645, -26.65550465647363154 ) ) ;
#223417 = EDGE_CURVE ( 'NONE', #102432, #11614, #28605, .T. ) ;
#223418 = DIRECTION ( 'NONE',  ( 4.239556034732057360E-17, 0.1298341882519953860, 0.9915357197604862671 ) ) ;
#223419 = ORIENTED_EDGE ( 'NONE', *, *, #144375, .F. ) ;
#223420 = SHAPE_REPRESENTATION ( 'Snap Open Cable Crossbars 2', ( #2425 ), #32042 ) ;
#223421 = AXIS2_PLACEMENT_3D ( 'NONE', #95957, #236749, #137643 ) ;
#223422 = AXIS2_PLACEMENT_3D ( 'NONE', #63274, #41180, #166272 ) ;
#223423 = ORIENTED_EDGE ( 'NONE', *, *, #251837, .F. ) ;
#223424 = AXIS2_PLACEMENT_3D ( 'NONE', #43499, #82578, #142571 ) ;
#223425 = CIRCLE ( 'NONE', #94264, 12.87499999999999467 ) ;
#223426 = ORIENTED_EDGE ( 'NONE', *, *, #38928, .F. ) ;
#223427 = CARTESIAN_POINT ( 'NONE',  ( 19.97071067811864609, 64.27928932189355749, -145.2731074845244450 ) ) ;
#223428 = ORIENTED_EDGE ( 'NONE', *, *, #48219, .F. ) ;
#223429 = VECTOR ( 'NONE', #8162, 1000.000000000000114 ) ;
#223430 = EDGE_CURVE ( 'NONE', #51735, #229756, #149371, .T. ) ;
#223431 = DIRECTION ( 'NONE',  ( -1.000000000000000000, 0.000000000000000000, 0.000000000000000000 ) ) ;
#223432 = DIRECTION ( 'NONE',  ( 0.000000000000000000, 0.8700118002898356018, -0.4930308989875170078 ) ) ;
#223433 = ADVANCED_FACE ( 'NONE', ( #44998 ), #161104, .F. ) ;
#223434 = CARTESIAN_POINT ( 'NONE',  ( -22.50000000000000000, 11.65000000001115588, -167.4999999999999716 ) ) ;
#223435 = CARTESIAN_POINT ( 'NONE',  ( -22.10000000000000497, 6.223900101154156594, 12.09999999999999964 ) ) ;
#223436 = CARTESIAN_POINT ( 'NONE',  ( 20.85000000000000142, 6.982009704867603972, -104.1961521182563359 ) ) ;
#223437 = FACE_OUTER_BOUND ( 'NONE', #223730, .T. ) ;
#223439 = ORIENTED_EDGE ( 'NONE', *, *, #87234, .T. ) ;
#223438 = DIRECTION ( 'NONE',  ( -0.000000000000000000, 1.000000000000000000, 6.982962677686267499E-15 ) ) ;
#223441 = DIRECTION ( 'NONE',  ( -3.265361837132813093E-16, 1.000000000000000000, 0.000000000000000000 ) ) ;
#223440 = CARTESIAN_POINT ( 'NONE',  ( 20.95561247346651967, 65.40499263480805325, -61.92932471754276236 ) ) ;
#223442 = CARTESIAN_POINT ( 'NONE',  ( -21.05000000000000071, -1.835341550213255957, -145.5551512925629822 ) ) ;
#223443 = CIRCLE ( 'NONE', #173635, 0.1000000000000028644 ) ;
#223444 = ORIENTED_EDGE ( 'NONE', *, *, #142834, .F. ) ;
#223445 = CARTESIAN_POINT ( 'NONE',  ( -15.70407651835961005, 9.355806591641286474, -116.7911025315462012 ) ) ;
#223446 = PLANE ( 'NONE',  #50055 ) ;
#223448 = ORIENTED_EDGE ( 'NONE', *, *, #43215, .T. ) ;
#223447 = AXIS2_PLACEMENT_3D ( 'NONE', #216315, #37717, #14305 ) ;
#223450 = CARTESIAN_POINT ( 'NONE',  ( 18.59999999999999076, -1.835859311432481045, -212.5044391687984842 ) ) ;
#223449 = PLANE ( 'NONE',  #170539 ) ;
#223451 = CARTESIAN_POINT ( 'NONE',  ( -22.59999999999999787, 64.25043287652226809, -69.62396585362311896 ) ) ;
#223452 = EDGE_CURVE ( 'NONE', #232431, #32139, #57570, .T. ) ;
#223453 = EDGE_LOOP ( 'NONE', ( #179465, #199761, #119654, #230126 ) ) ;
#223454 =( LENGTH_UNIT ( ) NAMED_UNIT ( * ) SI_UNIT ( .MILLI., .METRE. ) );
#223455 = CARTESIAN_POINT ( 'NONE',  ( 20.94999999999999929, 85.00000000001207923, -126.6291383618717816 ) ) ;
#223456 = CARTESIAN_POINT ( 'NONE',  ( -18.39999999999999858, 85.60000000001167564, -62.92291809330219365 ) ) ;
#223457 = CIRCLE ( 'NONE', #156878, 14.20833333333333748 ) ;
#223458 = DIRECTION ( 'NONE',  ( 0.000000000000000000, 0.000000000000000000, 1.000000000000000000 ) ) ;
#223459 = ORIENTED_EDGE ( 'NONE', *, *, #190725, .T. ) ;
#223460 = ORIENTED_EDGE ( 'NONE', *, *, #206013, .F. ) ;
#223461 = ADVANCED_FACE ( 'NONE', ( #141519 ), #240627, .T. ) ;
#223462 = EDGE_CURVE ( 'NONE', #117567, #130245, #7716, .T. ) ;
#223463 = CARTESIAN_POINT ( 'NONE',  ( -16.87242674293849021, 66.05000000001255955, -182.6720172381520797 ) ) ;
#223464 = CARTESIAN_POINT ( 'NONE',  ( 21.05000000000000071, 10.42338541491290727, -7.492051923870097774 ) ) ;
#223465 = DIRECTION ( 'NONE',  ( -1.020425574104004196E-15, -1.210927747993693964E-31, 1.000000000000000000 ) ) ;
#223466 = DIRECTION ( 'NONE',  ( 0.000000000000000000, -1.000000000000000000, -6.982962677686266711E-15 ) ) ;
#223467 = VECTOR ( 'NONE', #86172, 1000.000000000000000 ) ;
#223468 = AXIS2_PLACEMENT_3D ( 'NONE', #216996, #78765, #138716 ) ;
#223469 = FACE_OUTER_BOUND ( 'NONE', #187760, .T. ) ;
#223470 = AXIS2_PLACEMENT_3D ( 'NONE', #184452, #85329, #164900 ) ;
#223471 = AXIS2_PLACEMENT_3D ( 'NONE', #247468, #45420, #243616 ) ;
#223472 = DIRECTION ( 'NONE',  ( 1.000000000000000000, 0.000000000000000000, -0.000000000000000000 ) ) ;
#223473 = EDGE_CURVE ( 'NONE', #58429, #110957, #53495, .T. ) ;
#223475 = VERTEX_POINT ( 'NONE', #4564 ) ;
#223474 = DIRECTION ( 'NONE',  ( 0.000000000000000000, -0.8660254037844377084, -0.5000000000000016653 ) ) ;
#223476 = CARTESIAN_POINT ( 'NONE',  ( -21.15000000000000213, 6.540656951712399803, -33.50000000000000000 ) ) ;
#223477 = FACE_OUTER_BOUND ( 'NONE', #62291, .T. ) ;
#223478 = CARTESIAN_POINT ( 'NONE',  ( -16.97683809663752186, 66.05000000001160743, -60.27310748452439526 ) ) ;
#223479 = CARTESIAN_POINT ( 'NONE',  ( 20.94999999999999929, 62.96536896499190306, -207.0767526245058150 ) ) ;
#223481 = ORIENTED_EDGE ( 'NONE', *, *, #243284, .T. ) ;
#223480 = CARTESIAN_POINT ( 'NONE',  ( 6.000000000000061284, 64.75000000001119815, -22.12310748452479103 ) ) ;
#223482 = DIRECTION ( 'NONE',  ( -2.952720810173289112E-16, 1.000000000000000000, 0.000000000000000000 ) ) ;
#223483 = CARTESIAN_POINT ( 'NONE',  ( -20.54999999999999716, 30.18746141061095045, -235.4776000216846796 ) ) ;
#223484 = EDGE_CURVE ( 'NONE', #61629, #225362, #199246, .T. ) ;
#223485 = CARTESIAN_POINT ( 'NONE',  ( 18.59999999999999076, 21.17283678855157802, -243.7231193059830332 ) ) ;
#223486 = CARTESIAN_POINT ( 'NONE',  ( -18.59999999999999787, -21.97324378644421117, -224.3523082604776562 ) ) ;
#223487 = ORIENTED_EDGE ( 'NONE', *, *, #21386, .F. ) ;
#223488 = DIRECTION ( 'NONE',  ( 0.000000000000000000, 0.000000000000000000, -1.000000000000000000 ) ) ;
#223489 = CARTESIAN_POINT ( 'NONE',  ( -16.92280123533721792, 66.05000000001201954, -115.8737397986094493 ) ) ;
#223490 = DIRECTION ( 'NONE',  ( 0.000000000000000000, 1.000000000000000000, 0.000000000000000000 ) ) ;
#223491 = EDGE_CURVE ( 'NONE', #208753, #165812, #243185, .T. ) ;
#223492 = AXIS2_PLACEMENT_3D ( 'NONE', #223757, #107672, #225033 ) ;
#223493 = VECTOR ( 'NONE', #108000, 1000.000000000000000 ) ;
#223495 = VECTOR ( 'NONE', #174915, 1000.000000000000000 ) ;
#223494 = PLANE ( 'NONE',  #146722 ) ;
#223496 = VERTEX_POINT ( 'NONE', #25444 ) ;
#223497 = DIRECTION ( 'NONE',  ( 0.000000000000000000, -1.000000000000000000, 0.000000000000000000 ) ) ;
#223498 = EDGE_LOOP ( 'NONE', ( #97908, #247526, #38156, #64931 ) ) ;
#223500 = DIRECTION ( 'NONE',  ( 1.000000000000000000, 0.000000000000000000, 0.000000000000000000 ) ) ;
#223499 = AXIS2_PLACEMENT_3D ( 'NONE', #154336, #149173, #233831 ) ;
#223501 = DIRECTION ( 'NONE',  ( 1.000000000000000000, 0.000000000000000000, 0.000000000000000000 ) ) ;
#223502 = EDGE_CURVE ( 'NONE', #14172, #248822, #82674, .T. ) ;
#223503 = DIRECTION ( 'NONE',  ( 1.000000000000000000, 0.000000000000000000, -0.000000000000000000 ) ) ;
#223504 = VERTEX_POINT ( 'NONE', #121967 ) ;
#223505 = DIRECTION ( 'NONE',  ( 1.000000000000000000, 0.000000000000000000, 0.000000000000000000 ) ) ;
#223506 = DIRECTION ( 'NONE',  ( 0.000000000000000000, 0.9998779222360102414, 0.01562499999996356907 ) ) ;
#223507 = DIRECTION ( 'NONE',  ( 0.000000000000000000, 0.000000000000000000, 1.000000000000000000 ) ) ;
#223508 = CARTESIAN_POINT ( 'NONE',  ( 23.14999999999999858, 4.775700934590591196, -155.6512318959540551 ) ) ;
#223509 = VECTOR ( 'NONE', #88010, 1000.000000000000000 ) ;
#223510 = FACE_OUTER_BOUND ( 'NONE', #115007, .T. ) ;
#223511 = ORIENTED_EDGE ( 'NONE', *, *, #72639, .T. ) ;
#223513 = ORIENTED_EDGE ( 'NONE', *, *, #240691, .F. ) ;
#223512 = DIRECTION ( 'NONE',  ( 0.000000000000000000, 1.000000000000000000, 0.000000000000000000 ) ) ;
#223514 = VERTEX_POINT ( 'NONE', #201489 ) ;
#223515 = CARTESIAN_POINT ( 'NONE',  ( -16.85312964099708921, 9.913604682067711948, -20.60281570643044802 ) ) ;
#223516 = ORIENTED_EDGE ( 'NONE', *, *, #219451, .T. ) ;
#223517 = CARTESIAN_POINT ( 'NONE',  ( 21.11833042828126139, 61.00849935111920530, -234.1748126302079243 ) ) ;
#223518 = PLANE ( 'NONE',  #147098 ) ;
#223519 = VERTEX_POINT ( 'NONE', #179389 ) ;
#223520 = DIRECTION ( 'NONE',  ( 0.000000000000000000, 0.000000000000000000, -1.000000000000000000 ) ) ;
#223521 = FACE_OUTER_BOUND ( 'NONE', #97118, .T. ) ;
#223522 = VECTOR ( 'NONE', #88424, 1000.000000000000000 ) ;
#223523 = VERTEX_POINT ( 'NONE', #701 ) ;
#223524 = CARTESIAN_POINT ( 'NONE',  ( -16.88460203013675809, 9.954759003246870463, -54.36589180953823330 ) ) ;
#223526 = ORIENTED_EDGE ( 'NONE', *, *, #201825, .T. ) ;
#223525 = DIRECTION ( 'NONE',  ( 0.000000000000000000, -0.9126074666063660468, -0.4088369013363524762 ) ) ;
#223527 = LINE ( 'NONE', #243104, #164886 ) ;
#223528 = CARTESIAN_POINT ( 'NONE',  ( 21.14999999999999858, 64.25000000001244871, -181.7731074845244450 ) ) ;
#223529 = TOROIDAL_SURFACE ( 'NONE', #215175, 0.2000000000000000111, 0.1000000000000000056 ) ;
#223530 = AXIS2_PLACEMENT_3D ( 'NONE', #160243, #217593, #179793 ) ;
#223531 = ADVANCED_FACE ( 'NONE', ( #80228 ), #159824, .T. ) ;
#223532 = ORIENTED_EDGE ( 'NONE', *, *, #48499, .T. ) ;
#223533 = DIRECTION ( 'NONE',  ( -0.000000000000000000, 6.982962677686266711E-15, -1.000000000000000000 ) ) ;
#223534 = DIRECTION ( 'NONE',  ( 1.000000000000000000, 0.000000000000000000, 0.000000000000000000 ) ) ;
#223535 = CARTESIAN_POINT ( 'NONE',  ( -20.00857864376270001, 9.250000000011157297, -45.85000000000000142 ) ) ;
#223536 = ORIENTED_EDGE ( 'NONE', *, *, #254991, .F. ) ;
#223537 = CARTESIAN_POINT ( 'NONE',  ( 22.57856590037849287, 76.00412833007679581, -181.7731659471998000 ) ) ;
#223538 = AXIS2_PLACEMENT_3D ( 'NONE', #244933, #66307, #174440 ) ;
#223539 = EDGE_CURVE ( 'NONE', #95156, #130026, #180660, .T. ) ;
#223540 = DIRECTION ( 'NONE',  ( 1.000000000000000000, 0.000000000000000000, 0.000000000000000000 ) ) ;
#223541 = EDGE_CURVE ( 'NONE', #106114, #54036, #170065, .T. ) ;
#223542 = ORIENTED_EDGE ( 'NONE', *, *, #74252, .T. ) ;
#223543 = ADVANCED_FACE ( 'NONE', ( #89246 ), #30592, .T. ) ;
#223544 = CIRCLE ( 'NONE', #256828, 0.09999999999998898659 ) ;
#223545 = VECTOR ( 'NONE', #15850, 1000.000000000000000 ) ;
#223546 = ORIENTED_EDGE ( 'NONE', *, *, #179152, .T. ) ;
#223547 = FACE_OUTER_BOUND ( 'NONE', #178576, .T. ) ;
#223548 = VECTOR ( 'NONE', #242672, 1000.000000000000000 ) ;
#223549 = ORIENTED_EDGE ( 'NONE', *, *, #25542, .T. ) ;
#223550 = DIRECTION ( 'NONE',  ( -0.000000000000000000, 0.1350103645451649625, -0.9908441862701631297 ) ) ;
#223551 = EDGE_CURVE ( 'NONE', #52627, #195996, #29326, .T. ) ;
#223552 = DIRECTION ( 'NONE',  ( 1.000000000000000000, 0.000000000000000000, 0.000000000000000000 ) ) ;
#223554 = EDGE_LOOP ( 'NONE', ( #116254, #180397, #115978, #80488 ) ) ;
#223553 = DIRECTION ( 'NONE',  ( 6.938893903907030216E-14, 0.000000000000000000, 1.000000000000000000 ) ) ;
#223555 = CARTESIAN_POINT ( 'NONE',  ( 18.59999999999997655, 64.65966496992309942, -200.4475097531309586 ) ) ;
#223557 = AXIS2_PLACEMENT_3D ( 'NONE', #248294, #68381, #205297 ) ;
#223556 = DIRECTION ( 'NONE',  ( 0.000000000000000000, 0.9964539953858966292, 0.08413937888696096379 ) ) ;
#223558 = CARTESIAN_POINT ( 'NONE',  ( 18.50000000000000000, -9.399999999988843058, -174.3820418481727188 ) ) ;
#223559 = AXIS2_PLACEMENT_3D ( 'NONE', #223376, #242947, #126865 ) ;
#223560 = DIRECTION ( 'NONE',  ( -3.265361837132812600E-16, 0.4721928772777346239, 0.8814952561688430555 ) ) ;
#223561 = DIRECTION ( 'NONE',  ( 1.000000000000000000, -0.000000000000000000, -0.000000000000000000 ) ) ;
#223562 = CARTESIAN_POINT ( 'NONE',  ( 23.14999999999999858, 7.128833340093095217, -233.7327013124392749 ) ) ;
#223563 = DIRECTION ( 'NONE',  ( 0.000000000000000000, -1.000000000000000000, 0.000000000000000000 ) ) ;
#223565 = VERTEX_POINT ( 'NONE', #168843 ) ;
#223564 = DIRECTION ( 'NONE',  ( 0.000000000000000000, 0.000000000000000000, -1.000000000000000000 ) ) ;
#223566 = DIRECTION ( 'NONE',  ( 1.000000000000000000, 0.000000000000000000, 0.000000000000000000 ) ) ;
#223567 = ORIENTED_EDGE ( 'NONE', *, *, #55832, .F. ) ;
#223568 = DIRECTION ( 'NONE',  ( 1.000000000000000000, 0.000000000000000000, 0.000000000000000000 ) ) ;
#223569 = AXIS2_PLACEMENT_3D ( 'NONE', #232391, #186833, #148998 ) ;
#223570 = CIRCLE ( 'NONE', #111169, 0.1000000000000026007 ) ;
#223571 = AXIS2_PLACEMENT_3D ( 'NONE', #59271, #82697, #159712 ) ;
#223572 = DIRECTION ( 'NONE',  ( 0.000000000000000000, 0.000000000000000000, -1.000000000000000000 ) ) ;
#223573 = DIRECTION ( 'NONE',  ( -2.978066053179067751E-16, 0.9770955615653316162, 0.2128009952263596738 ) ) ;
#223574 = EDGE_CURVE ( 'NONE', #136977, #100199, #220083, .T. ) ;
#223575 = EDGE_CURVE ( 'NONE', #28671, #86933, #99263, .T. ) ;
#223576 = DIRECTION ( 'NONE',  ( 0.000000000000000000, -0.9908441862701596881, -0.1350103645451904977 ) ) ;
#223577 = CARTESIAN_POINT ( 'NONE',  ( 20.97438252431638972, 67.07457649393661825, -195.0507367955136431 ) ) ;
#223578 = ORIENTED_EDGE ( 'NONE', *, *, #165984, .F. ) ;
#223579 = CARTESIAN_POINT ( 'NONE',  ( 18.50000000000000000, 78.21362219944488459, -231.2727646510690533 ) ) ;
#223580 = DIRECTION ( 'NONE',  ( 0.000000000000000000, 0.8096735173027155286, -0.5868805631290315850 ) ) ;
#223581 = CIRCLE ( 'NONE', #77850, 11.75000000000000000 ) ;
#223582 = EDGE_CURVE ( 'NONE', #7699, #132399, #68415, .T. ) ;
#223583 = EDGE_LOOP ( 'NONE', ( #24166, #236606, #238253 ) ) ;
#223584 = CARTESIAN_POINT ( 'NONE',  ( 21.05000000000000071, 70.15000000001198543, -113.1556047088022581 ) ) ;
#223585 = CARTESIAN_POINT ( 'NONE',  ( -16.92989143108098915, 61.00021111735996016, -220.8173494352598425 ) ) ;
#223586 = VERTEX_POINT ( 'NONE', #127098 ) ;
#223587 = DIRECTION ( 'NONE',  ( 0.000000000000000000, 0.000000000000000000, 1.000000000000000000 ) ) ;
#223588 = ORIENTED_EDGE ( 'NONE', *, *, #207289, .F. ) ;
#223589 = DIRECTION ( 'NONE',  ( 0.000000000000000000, 0.1332476588733448597, 0.9910827722268067408 ) ) ;
#223590 = ORIENTED_EDGE ( 'NONE', *, *, #161018, .T. ) ;
#223591 = CIRCLE ( 'NONE', #65406, 0.09999999999999939493 ) ;
#223592 = FACE_OUTER_BOUND ( 'NONE', #9978, .T. ) ;
#223593 = VECTOR ( 'NONE', #155697, 1000.000000000000000 ) ;
#223594 = EDGE_CURVE ( 'NONE', #95316, #35530, #190954, .T. ) ;
#223595 = CARTESIAN_POINT ( 'NONE',  ( -20.85000000000000142, -1.164121893230052995, -74.91484808557160591 ) ) ;
#223596 = CIRCLE ( 'NONE', #57003, 4.000000000000003553 ) ;
#223597 = AXIS2_PLACEMENT_3D ( 'NONE', #244909, #45431, #208378 ) ;
#223598 = ORIENTED_EDGE ( 'NONE', *, *, #85609, .T. ) ;
#223599 = DIRECTION ( 'NONE',  ( 0.000000000000000000, -0.8700118002898359348, 0.4930308989875165082 ) ) ;
#223601 = ORIENTED_EDGE ( 'NONE', *, *, #219814, .F. ) ;
#223600 = DIRECTION ( 'NONE',  ( 0.000000000000000000, -1.000000000000000000, -0.000000000000000000 ) ) ;
#223602 = DIRECTION ( 'NONE',  ( 0.000000000000000000, -0.5859227990963362664, -0.8103668758649469339 ) ) ;
#223603 = EDGE_LOOP ( 'NONE', ( #235890, #107234, #164639 ) ) ;
#223604 = VECTOR ( 'NONE', #23598, 1000.000000000000000 ) ;
#223605 = ADVANCED_FACE ( 'NONE', ( #12316 ), #247031, .F. ) ;
#223606 = ORIENTED_EDGE ( 'NONE', *, *, #15830, .T. ) ;
#223607 = CARTESIAN_POINT ( 'NONE',  ( -23.25000000000000000, 64.35000000001173248, -81.27310748452440237 ) ) ;
#223608 = CARTESIAN_POINT ( 'NONE',  ( 22.39999999999999503, 26.02743912001966464, -254.3139371321002216 ) ) ;
#223609 = DIRECTION ( 'NONE',  ( 0.000000000000000000, 0.000000000000000000, 1.000000000000000000 ) ) ;
#223610 = EDGE_CURVE ( 'NONE', #148687, #196126, #132600, .T. ) ;
#223611 = EDGE_CURVE ( 'NONE', #132097, #198523, #106228, .T. ) ;
#223612 = TOROIDAL_SURFACE ( 'NONE', #127402, 0.2000000000000000111, 0.1000000000000000056 ) ;
#223613 = DIRECTION ( 'NONE',  ( 1.000000000000000000, 0.000000000000000000, 0.000000000000000000 ) ) ;
#223614 = DIRECTION ( 'NONE',  ( 0.000000000000000000, -6.608470384673547079E-15, 1.000000000000000000 ) ) ;
#223615 = AXIS2_PLACEMENT_3D ( 'NONE', #32406, #173219, #208466 ) ;
#223616 = EDGE_LOOP ( 'NONE', ( #30737, #67585, #69610, #151894 ) ) ;
#223617 = B_SPLINE_CURVE_WITH_KNOTS ( 'NONE', 3,
 ( #26358, #68041, #203706, #5470 ),
 .UNSPECIFIED., .F., .F.,
 ( 4, 4 ),
 ( 0.000000000000000000, 0.001767853679387130974 ),
 .UNSPECIFIED. ) ;
#223618 = DIRECTION ( 'NONE',  ( 1.000000000000000000, 0.000000000000000000, -0.000000000000000000 ) ) ;
#223619 = DIRECTION ( 'NONE',  ( 0.000000000000000000, -1.000000000000000000, -6.982962677686265922E-15 ) ) ;
#223620 = CARTESIAN_POINT ( 'NONE',  ( -23.25000000000000000, 77.83585931145546510, -91.51866831572576189 ) ) ;
#223621 = CARTESIAN_POINT ( 'NONE',  ( -23.15000000000000213, 1.925233644870967487, -54.26975646687386501 ) ) ;
#223622 = ORIENTED_EDGE ( 'NONE', *, *, #251186, .T. ) ;
#223623 = CARTESIAN_POINT ( 'NONE',  ( 20.93975676684922504, 68.05374558910872906, -224.1882283518532120 ) ) ;
#223624 = ORIENTED_EDGE ( 'NONE', *, *, #36252, .F. ) ;
#223625 = CARTESIAN_POINT ( 'NONE',  ( 15.70340296795547808, 9.355888454513701546, -116.7886428967780574 ) ) ;
#223627 = ORIENTED_EDGE ( 'NONE', *, *, #80233, .T. ) ;
#223626 = CIRCLE ( 'NONE', #207099, 14.20833333333333748 ) ;
#223629 = EDGE_CURVE ( 'NONE', #223036, #228001, #107645, .T. ) ;
#223628 = ADVANCED_FACE ( 'NONE', ( #108808 ), #186785, .T. ) ;
#223630 = EDGE_CURVE ( 'NONE', #126961, #121672, #174337, .T. ) ;
#223631 = DIRECTION ( 'NONE',  ( 0.000000000000000000, 1.000000000000000000, 0.000000000000000000 ) ) ;
#223632 = LINE ( 'NONE', #78971, #168701 ) ;
#223633 = ORIENTED_EDGE ( 'NONE', *, *, #40887, .T. ) ;
#223635 = EDGE_LOOP ( 'NONE', ( #239989, #254622, #99094, #161711 ) ) ;
#223634 = CARTESIAN_POINT ( 'NONE',  ( -20.94999999999999929, 1.115600667400684642E-11, -167.5000000000000284 ) ) ;
#223636 = CARTESIAN_POINT ( 'NONE',  ( -20.94999999999999929, 18.27574494880468592, -237.6039235467692947 ) ) ;
#223637 = VERTEX_POINT ( 'NONE', #130954 ) ;
#223638 = ADVANCED_FACE ( 'NONE', ( #210497 ), #125806, .T. ) ;
#223639 = DIRECTION ( 'NONE',  ( 0.000000000000000000, 0.2617529984165055668, 0.9651348961777149738 ) ) ;
#223640 = DIRECTION ( 'NONE',  ( 0.000000000000000000, 0.000000000000000000, 1.000000000000000000 ) ) ;
#223641 = ORIENTED_EDGE ( 'NONE', *, *, #1930, .F. ) ;
#223642 = ADVANCED_FACE ( 'NONE', ( #67124 ), #146639, .T. ) ;
#223643 = FACE_OUTER_BOUND ( 'NONE', #126463, .T. ) ;
#223644 = CARTESIAN_POINT ( 'NONE',  ( 22.39999999999999503, 0.1000000000111554016, -161.2499999999999716 ) ) ;
#223645 = VECTOR ( 'NONE', #159047, 1000.000000000000000 ) ;
#223646 = CIRCLE ( 'NONE', #198546, 0.1000000000000002831 ) ;
#223648 = EDGE_CURVE ( 'NONE', #194778, #195203, #22712, .T. ) ;
#223647 = CIRCLE ( 'NONE', #73859, 11.75000000000000000 ) ;
#223649 = CIRCLE ( 'NONE', #169558, 0.09999999999999939493 ) ;
#223650 = ADVANCED_FACE ( 'NONE', ( #9711 ), #133520, .F. ) ;
#223651 = ORIENTED_EDGE ( 'NONE', *, *, #66632, .T. ) ;
#223652 = VERTEX_POINT ( 'NONE', #132238 ) ;
#223653 = DIRECTION ( 'NONE',  ( 0.000000000000000000, 0.000000000000000000, -1.000000000000000000 ) ) ;
#223654 = EDGE_CURVE ( 'NONE', #216065, #113349, #53674, .T. ) ;
#223656 = ORIENTED_EDGE ( 'NONE', *, *, #7672, .F. ) ;
#223655 = CARTESIAN_POINT ( 'NONE',  ( -33.72168855820452649, 20.70020979027691155, -227.9869476361872103 ) ) ;
#223657 = EDGE_CURVE ( 'NONE', #79346, #224301, #249507, .T. ) ;
#223658 = DIRECTION ( 'NONE',  ( 0.000000000000000000, 0.000000000000000000, -1.000000000000000000 ) ) ;
#223659 = CARTESIAN_POINT ( 'NONE',  ( -18.59999999999999787, 68.97833521811233481, -166.1895420826271277 ) ) ;
#223660 = EDGE_CURVE ( 'NONE', #15847, #207603, #91091, .T. ) ;
#223661 = CARTESIAN_POINT ( 'NONE',  ( -20.54999999999999716, 1.999999999999998224, -13.22462192276210224 ) ) ;
#223664 = DIRECTION ( 'NONE',  ( 1.000000000000000000, 0.000000000000000000, -0.000000000000000000 ) ) ;
#223663 = VECTOR ( 'NONE', #152748, 1000.000000000000000 ) ;
#223662 = CARTESIAN_POINT ( 'NONE',  ( -16.94445028196808778, 66.00793639031412852, -90.41577730610593733 ) ) ;
#223665 = CARTESIAN_POINT ( 'NONE',  ( -20.85000000000000142, 65.66751761918722252, -164.4282609406112670 ) ) ;
#223667 = EDGE_CURVE ( 'NONE', #184576, #39196, #49586, .T. ) ;
#223666 = DIRECTION ( 'NONE',  ( -1.000000000000000000, 0.000000000000000000, 0.000000000000000000 ) ) ;
#223668 = TOROIDAL_SURFACE ( 'NONE', #223123, 0.2000000000000000111, 0.1000000000000000056 ) ;
#223669 = CIRCLE ( 'NONE', #248626, 0.09999999999999528710 ) ;
#223670 = CARTESIAN_POINT ( 'NONE',  ( -21.05000000000000071, -11.29603075032412995, -103.5478991596638991 ) ) ;
#223671 = CARTESIAN_POINT ( 'NONE',  ( -23.15000000000000213, 76.00000000001145395, -39.92310748452432279 ) ) ;
#223672 = ORIENTED_EDGE ( 'NONE', *, *, #242095, .F. ) ;
#223673 = AXIS2_PLACEMENT_3D ( 'NONE', #195052, #73833, #252417 ) ;
#223674 = ORIENTED_EDGE ( 'NONE', *, *, #219562, .T. ) ;
#223675 = CARTESIAN_POINT ( 'NONE',  ( -23.25000000000000355, 5.650000000011139001, -143.2500000000000284 ) ) ;
#223676 = VERTEX_POINT ( 'NONE', #73580 ) ;
#223677 = ADVANCED_FACE ( 'NONE', ( #216896 ), #37017, .T. ) ;
#223678 = EDGE_CURVE ( 'NONE', #74886, #227850, #74870, .T. ) ;
#223679 = CARTESIAN_POINT ( 'NONE',  ( -18.50000000000000000, -1.164121893230052995, -208.9148480855715775 ) ) ;
#223680 = ORIENTED_EDGE ( 'NONE', *, *, #194839, .F. ) ;
#223681 = CARTESIAN_POINT ( 'NONE',  ( 20.94999999999999929, -1.835859311432481045, -112.0044391687985694 ) ) ;
#223683 = ORIENTED_EDGE ( 'NONE', *, *, #116504, .F. ) ;
#223682 = AXIS2_PLACEMENT_3D ( 'NONE', #254766, #59144, #40938 ) ;
#223684 = LINE ( 'NONE', #185857, #79760 ) ;
#223685 = ORIENTED_EDGE ( 'NONE', *, *, #242490, .T. ) ;
#223686 = ORIENTED_EDGE ( 'NONE', *, *, #256647, .F. ) ;
#223687 = LINE ( 'NONE', #29399, #58846 ) ;
#223688 = FACE_OUTER_BOUND ( 'NONE', #151794, .T. ) ;
#223690 = ORIENTED_EDGE ( 'NONE', *, *, #31567, .T. ) ;
#223689 = DIRECTION ( 'NONE',  ( 0.000000000000000000, 0.2128009952263485993, -0.9770955615653341697 ) ) ;
#223691 = CARTESIAN_POINT ( 'NONE',  ( 21.05000000000000071, -1.236118717437887371, -194.8647072476926212 ) ) ;
#223693 = ORIENTED_EDGE ( 'NONE', *, *, #126464, .T. ) ;
#223692 = DIRECTION ( 'NONE',  ( 0.000000000000000000, 0.000000000000000000, 1.000000000000000000 ) ) ;
#223694 = CARTESIAN_POINT ( 'NONE',  ( 19.97071067811865674, 11.72071067812981937, -125.1500000000000341 ) ) ;
#223695 = VERTEX_POINT ( 'NONE', #155687 ) ;
#223697 = CARTESIAN_POINT ( 'NONE',  ( -16.88853107394619357, 9.950878483358135185, -121.3529363468922639 ) ) ;
#223696 = AXIS2_PLACEMENT_3D ( 'NONE', #209375, #170300, #54144 ) ;
#223699 = VERTEX_POINT ( 'NONE', #34457 ) ;
#223698 = CYLINDRICAL_SURFACE ( 'NONE', #177198, 0.09999999999999939493 ) ;
#223700 = CARTESIAN_POINT ( 'NONE',  ( -20.94999999999999929, -11.29603075032412995, -103.5478991596638991 ) ) ;
#223701 = CARTESIAN_POINT ( 'NONE',  ( -12.25000000000000533, 26.41090933635395288, -233.4546044608430293 ) ) ;
#223702 = DIRECTION ( 'NONE',  ( 1.836970198721029934E-16, -1.000000000000000000, -0.000000000000000000 ) ) ;
#223703 = AXIS2_PLACEMENT_3D ( 'NONE', #78856, #158449, #121874 ) ;
#223704 = ORIENTED_EDGE ( 'NONE', *, *, #200124, .F. ) ;
#223705 = EDGE_CURVE ( 'NONE', #192537, #102565, #145242, .T. ) ;
#223707 = FACE_OUTER_BOUND ( 'NONE', #256376, .T. ) ;
#223706 = CARTESIAN_POINT ( 'NONE',  ( -23.15000000000000213, 4.959819536546777642E-16, 4.049999999999998934 ) ) ;
#223708 = CARTESIAN_POINT ( 'NONE',  ( 18.52928932304149967, 10.27928932305266407, -91.67625343280367645 ) ) ;
#223709 = DIRECTION ( 'NONE',  ( 0.000000000000000000, -1.000000000000000000, -6.982962677686265922E-15 ) ) ;
#223710 = TOROIDAL_SURFACE ( 'NONE', #7231, 0.2000000000000000111, 0.1000000000000000056 ) ;
#223711 = VECTOR ( 'NONE', #87068, 1000.000000000000000 ) ;
#223712 = ADVANCED_FACE ( 'NONE', ( #112681 ), #57927, .T. ) ;
#223713 = CARTESIAN_POINT ( 'NONE',  ( 23.15000000000000213, 85.60000000001230092, -160.1291383618718385 ) ) ;
#223714 = DIRECTION ( 'NONE',  ( -3.265361837132813093E-16, -1.000000000000000000, -6.982962677686266711E-15 ) ) ;
#223715 = ORIENTED_EDGE ( 'NONE', *, *, #174407, .F. ) ;
#223716 = ORIENTED_EDGE ( 'NONE', *, *, #112274, .T. ) ;
#223717 = VERTEX_POINT ( 'NONE', #154412 ) ;
#223718 = DIRECTION ( 'NONE',  ( 3.469446951953728416E-14, 0.8660254037844343777, -0.5000000000000074385 ) ) ;
#223719 = CARTESIAN_POINT ( 'NONE',  ( -23.25000000000000000, 87.48912529308852015, -173.1231074845242688 ) ) ;
#223720 = CIRCLE ( 'NONE', #86328, 2.000000000000003553 ) ;
#223721 = ORIENTED_EDGE ( 'NONE', *, *, #240335, .T. ) ;
#223722 = CARTESIAN_POINT ( 'NONE',  ( 20.94999999999999929, 85.00000000001149658, -45.41707660717670336 ) ) ;
#223723 = ORIENTED_EDGE ( 'NONE', *, *, #180288, .T. ) ;
#223725 = CARTESIAN_POINT ( 'NONE',  ( 20.94999999999999574, 1.835341550235567887, -45.05515129256298223 ) ) ;
#223724 = AXIS2_PLACEMENT_3D ( 'NONE', #77822, #122107, #199072 ) ;
#223726 = ORIENTED_EDGE ( 'NONE', *, *, #252999, .F. ) ;
#223727 = CARTESIAN_POINT ( 'NONE',  ( 12.30626653967341255, 9.356790025057035720, -151.2048265086139054 ) ) ;
#223728 = EDGE_CURVE ( 'NONE', #7914, #18470, #196073, .T. ) ;
#223729 = CIRCLE ( 'NONE', #257023, 0.09999999999998898659 ) ;
#223730 = EDGE_LOOP ( 'NONE', ( #23067, #249103, #80938, #92074, #45660 ) ) ;
#223731 = ORIENTED_EDGE ( 'NONE', *, *, #198397, .T. ) ;
#223732 = CIRCLE ( 'NONE', #252967, 7.791421356237338003 ) ;
#223733 = ORIENTED_EDGE ( 'NONE', *, *, #187979, .F. ) ;
#223735 = DIRECTION ( 'NONE',  ( 0.000000000000000000, 0.000000000000000000, 1.000000000000000000 ) ) ;
#223734 = AXIS2_PLACEMENT_3D ( 'NONE', #175944, #157682, #118532 ) ;
#223736 = CARTESIAN_POINT ( 'NONE',  ( 16.87683809663749557, 9.950000000011131718, -154.8500000000000227 ) ) ;
#223737 = CARTESIAN_POINT ( 'NONE',  ( 15.07585980824113214, 27.57398452308367709, -234.0009067267211833 ) ) ;
#223738 = DIRECTION ( 'NONE',  ( 0.000000000000000000, 0.2617529984165030132, 0.9651348961777157509 ) ) ;
#223739 = AXIS2_PLACEMENT_3D ( 'NONE', #221657, #40517, #99140 ) ;
#223740 = LINE ( 'NONE', #122100, #34507 ) ;
#223741 =( BOUNDED_SURFACE ( )  B_SPLINE_SURFACE ( 3, 2, ( 
 ( #138114, #78146, #57293 ),
 ( #117295, #97695, #256746 ),
 ( #141978, #19485, #37777 ),
 ( #196815, #40363, #201970 ) ),
 .UNSPECIFIED., .F., .F., .F. ) 
 B_SPLINE_SURFACE_WITH_KNOTS ( ( 4, 4 ),
 ( 3, 3 ),
 ( 4.712388980384689674, 5.765869716888459173 ),
 ( 0.000000000000000000, 1.000000000000000000 ),
 .UNSPECIFIED. ) 
 GEOMETRIC_REPRESENTATION_ITEM ( )  RATIONAL_B_SPLINE_SURFACE ( (
 ( 1.000000000000000000, 0.7071067811865359154, 1.000000000000000000),
 ( 1.000000000000000000, 0.7953136715913566857, 1.000000000000000000),
 ( 1.000000000000000000, 0.8646876308615015772, 1.000000000000000000),
 ( 1.000000000000000000, 0.8984936768950380070, 1.000000000000000000) ) ) 
 REPRESENTATION_ITEM ( '' )  SURFACE ( )  );
#223742 = CARTESIAN_POINT ( 'NONE',  ( -20.54999999999999716, 9.350000000011156942, -54.65000000000000568 ) ) ;
#223743 = CARTESIAN_POINT ( 'NONE',  ( -20.64999999999999858, 85.50000000001149658, -45.91707660717669626 ) ) ;
#223745 = ORIENTED_EDGE ( 'NONE', *, *, #197483, .F. ) ;
#223744 = CARTESIAN_POINT ( 'NONE',  ( -20.94788355080264353, 10.30207779525983192, -139.4895520716782755 ) ) ;
#223747 = CARTESIAN_POINT ( 'NONE',  ( 21.08078803292165659, 69.66698703557483441, -103.1022934716821311 ) ) ;
#223746 = DIRECTION ( 'NONE',  ( 0.000000000000000000, 0.000000000000000000, -1.000000000000000000 ) ) ;
#223748 = AXIS2_PLACEMENT_3D ( 'NONE', #28678, #129022, #186431 ) ;
#223749 = LINE ( 'NONE', #184635, #248879 ) ;
#223750 = EDGE_LOOP ( 'NONE', ( #217261, #38769, #218756, #204690 ) ) ;
#223751 = CARTESIAN_POINT ( 'NONE',  ( -18.50000000000000000, 22.33586458086958615, -231.4986017528744071 ) ) ;
#223752 = DIRECTION ( 'NONE',  ( -0.7070776581708965169, -0.7071359030027827286, -0.000000000000000000 ) ) ;
#223753 = FACE_OUTER_BOUND ( 'NONE', #187462, .T. ) ;
#223754 = ORIENTED_EDGE ( 'NONE', *, *, #118417, .T. ) ;
#223755 = CARTESIAN_POINT ( 'NONE',  ( 20.94999999999999929, 18.18127959618848877, -237.5711165786817389 ) ) ;
#223756 = TOROIDAL_SURFACE ( 'NONE', #15515, 0.6000000000000017542, 0.1000000000000000056 ) ;
#223757 = CARTESIAN_POINT ( 'NONE',  ( 20.73486653747088937, 7.750000000011182166, -54.35000000000000142 ) ) ;
#223758 = FACE_OUTER_BOUND ( 'NONE', #126299, .T. ) ;
#223759 = AXIS2_PLACEMENT_3D ( 'NONE', #96786, #77244, #135928 ) ;
#223761 = VERTEX_POINT ( 'NONE', #35735 ) ;
#223760 = AXIS2_PLACEMENT_3D ( 'NONE', #6318, #148422, #244937 ) ;
#223762 = VERTEX_POINT ( 'NONE', #231356 ) ;
#223763 = DIRECTION ( 'NONE',  ( -1.000000000000000000, 0.000000000000000000, -0.000000000000000000 ) ) ;
#223764 = ORIENTED_EDGE ( 'NONE', *, *, #69148, .F. ) ;
#223765 = DIRECTION ( 'NONE',  ( -4.801466763864313332E-15, -0.04908394489122119841, -0.9987946567507836049 ) ) ;
#223766 = FACE_OUTER_BOUND ( 'NONE', #189364, .T. ) ;
#223767 = DIRECTION ( 'NONE',  ( 0.000000000000000000, 0.000000000000000000, 1.000000000000000000 ) ) ;
#223768 = DIRECTION ( 'NONE',  ( 0.000000000000000000, 7.147358527629759053E-15, -1.000000000000000000 ) ) ;
#223769 = ORIENTED_EDGE ( 'NONE', *, *, #61159, .T. ) ;
#223770 = ADVANCED_FACE ( 'NONE', ( #38280 ), #94382, .F. ) ;
#223771 = CARTESIAN_POINT ( 'NONE',  ( -12.68215100488889924, 9.396630376328870327, -118.4070573928183023 ) ) ;
#223772 = CIRCLE ( 'NONE', #103533, 4.100000000000008527 ) ;
#223773 = DIRECTION ( 'NONE',  ( 1.000000000000000000, 0.000000000000000000, 0.000000000000000000 ) ) ;
#223774 = ADVANCED_FACE ( 'NONE', ( #55233 ), #137355, .T. ) ;
#223775 = CIRCLE ( 'NONE', #7304, 0.1000000000000002970 ) ;
#223776 = CARTESIAN_POINT ( 'NONE',  ( 18.49999999999999289, 10.49142135624846439, -192.3499999999999659 ) ) ;
#223777 = CYLINDRICAL_SURFACE ( 'NONE', #115897, 0.1000000000000028644 ) ;
#223778 = VERTEX_POINT ( 'NONE', #57815 ) ;
#223779 = CIRCLE ( 'NONE', #140997, 0.09999999999999939493 ) ;
#223780 = ADVANCED_FACE ( 'NONE', ( #117805 ), #52686, .F. ) ;
#223782 = VERTEX_POINT ( 'NONE', #95668 ) ;
#223781 = DIRECTION ( 'NONE',  ( -1.000000000000000000, -0.000000000000000000, 0.000000000000000000 ) ) ;
#223783 = DIRECTION ( 'NONE',  ( 0.000000000000000000, 6.982962677686266711E-15, -1.000000000000000000 ) ) ;
#223784 = CARTESIAN_POINT ( 'NONE',  ( 18.39999999999999858, 78.24072131640578220, -231.5548844243369331 ) ) ;
#223785 = DIRECTION ( 'NONE',  ( -1.000000000000000000, 0.000000000000000000, 0.000000000000000000 ) ) ;
#223786 = EDGE_CURVE ( 'NONE', #89589, #83182, #18708, .T. ) ;
#223787 = DIRECTION ( 'NONE',  ( 0.000000000000000000, 6.982962677686266711E-15, -1.000000000000000000 ) ) ;
#223788 = CIRCLE ( 'NONE', #136286, 0.1000000000000028644 ) ;
#223789 = DIRECTION ( 'NONE',  ( -1.000000000000000000, 0.000000000000000000, -0.000000000000000000 ) ) ;
#223790 = DIRECTION ( 'NONE',  ( -1.000000000000000000, -2.952720810173289112E-16, 0.000000000000000000 ) ) ;
#223792 = VERTEX_POINT ( 'NONE', #172700 ) ;
#223791 = AXIS2_PLACEMENT_3D ( 'NONE', #159229, #244828, #165303 ) ;
#223793 = DIRECTION ( 'NONE',  ( 0.000000000000000000, 1.000000000000000000, -1.224646799147353207E-16 ) ) ;
#223794 = FACE_OUTER_BOUND ( 'NONE', #45142, .T. ) ;
#223795 = AXIS2_PLACEMENT_3D ( 'NONE', #239816, #61164, #143263 ) ;
#223796 = AXIS2_PLACEMENT_3D ( 'NONE', #116958, #136494, #97353 ) ;
#223797 = DIRECTION ( 'NONE',  ( 1.000000000000000000, 0.000000000000000000, 0.000000000000000000 ) ) ;
#223798 = EDGE_CURVE ( 'NONE', #122206, #225681, #199446, .T. ) ;
#223799 = CIRCLE ( 'NONE', #19826, 0.09999999999998898659 ) ;
#223800 = DIRECTION ( 'NONE',  ( 0.000000000000000000, 0.000000000000000000, 1.000000000000000000 ) ) ;
#223801 = CARTESIAN_POINT ( 'NONE',  ( 23.40000000000005187, 64.35000000001120668, -51.02310748452479316 ) ) ;
#223802 = AXIS2_PLACEMENT_3D ( 'NONE', #230429, #208321, #28422 ) ;
#223803 = ORIENTED_EDGE ( 'NONE', *, *, #68165, .T. ) ;
#223804 = VERTEX_POINT ( 'NONE', #237756 ) ;
#223805 = CARTESIAN_POINT ( 'NONE',  ( 20.99780126800918723, 11.60538868788781031, -194.0873525717054804 ) ) ;
#223806 = CARTESIAN_POINT ( 'NONE',  ( 20.94999999999999574, 77.85102823015347440, -191.8691942151018566 ) ) ;
#223807 = FACE_OUTER_BOUND ( 'NONE', #63658, .T. ) ;
#223808 = DIRECTION ( 'NONE',  ( 1.000000000000000000, -0.000000000000000000, -0.000000000000000000 ) ) ;
#223809 = EDGE_CURVE ( 'NONE', #245204, #7237, #192521, .T. ) ;
#223810 = DIRECTION ( 'NONE',  ( 0.000000000000000000, 0.9126074666063632712, 0.4088369013363589710 ) ) ;
#223811 = CARTESIAN_POINT ( 'NONE',  ( -18.79999999999999716, 11.49641995933507665, 1.885425182446133663 ) ) ;
#223812 = VECTOR ( 'NONE', #185706, 1000.000000000000000 ) ;
#223813 = DIRECTION ( 'NONE',  ( 0.000000000000000000, -1.000000000000000000, 0.000000000000000000 ) ) ;
#223814 = CARTESIAN_POINT ( 'NONE',  ( -16.92925196614875816, 9.972331796410120575, -12.61674484771679694 ) ) ;
#223815 = ORIENTED_EDGE ( 'NONE', *, *, #251024, .T. ) ;
#223816 = CARTESIAN_POINT ( 'NONE',  ( -20.94999999999999929, -11.64999999998884483, -97.60000000000005116 ) ) ;
#223817 = VERTEX_POINT ( 'NONE', #43412 ) ;
#223818 = CARTESIAN_POINT ( 'NONE',  ( -21.04999999999999716, 76.01465611852449911, -76.01979407029223523 ) ) ;
#223819 = CYLINDRICAL_SURFACE ( 'NONE', #91496, 0.09999999999999945044 ) ;
#223820 = DIRECTION ( 'NONE',  ( -0.000000000000000000, 1.000000000000000000, -0.000000000000000000 ) ) ;
#223821 = CARTESIAN_POINT ( 'NONE',  ( 21.00000000000000000, 14.02742277431099538, -219.5907614236512870 ) ) ;
#223822 = DIRECTION ( 'NONE',  ( -1.000000000000000000, 0.000000000000000000, 0.000000000000000000 ) ) ;
#223823 = CARTESIAN_POINT ( 'NONE',  ( -18.54159361262949091, -9.463132135493086849, -7.049122216292921905 ) ) ;
#223824 = DIRECTION ( 'NONE',  ( 0.000000000000000000, -0.2128009952263604232, 0.9770955615653316162 ) ) ;
#223825 = DIRECTION ( 'NONE',  ( -3.469446951953660258E-14, 0.5000000000000209832, 0.8660254037844264952 ) ) ;
#223826 = DIRECTION ( 'NONE',  ( 0.000000000000000000, -1.000000000000000000, 0.000000000000000000 ) ) ;
#223827 = DIRECTION ( 'NONE',  ( 0.000000000000000000, -6.982962677686266711E-15, 1.000000000000000000 ) ) ;
#223828 = DIRECTION ( 'NONE',  ( -1.000000000000000000, -2.952720810173289112E-16, 0.000000000000000000 ) ) ;
#223829 = AXIS2_PLACEMENT_3D ( 'NONE', #57325, #62495, #142013 ) ;
#223830 = VECTOR ( 'NONE', #214794, 1000.000000000000000 ) ;
#223831 = AXIS2_PLACEMENT_3D ( 'NONE', #27224, #127577, #207121 ) ;
#223832 = CARTESIAN_POINT ( 'NONE',  ( 23.14999999999999858, 76.00000000001213607, -136.5231074845243313 ) ) ;
#223833 = CARTESIAN_POINT ( 'NONE',  ( 21.04999999999999716, 8.872080675388932747, -176.0210474188342005 ) ) ;
#223834 = ADVANCED_FACE ( 'NONE', ( #239044 ), #257265, .F. ) ;
#223835 = ORIENTED_EDGE ( 'NONE', *, *, #119745, .T. ) ;
#223836 =( BOUNDED_CURVE ( )  B_SPLINE_CURVE ( 3, ( #189599, #33127, #232594, #73522 ),
 .UNSPECIFIED., .F., .F. ) 
 B_SPLINE_CURVE_WITH_KNOTS ( ( 4, 4 ),
 ( 3.141592653589793116, 4.712388980384689674 ),
 .UNSPECIFIED. ) 
 CURVE ( )  GEOMETRIC_REPRESENTATION_ITEM ( )  RATIONAL_B_SPLINE_CURVE ( ( 1.000000000000000000, 0.8047378541243649375, 0.8047378541243649375, 1.000000000000000000 ) ) 
 REPRESENTATION_ITEM ( '' )  );
#223837 = CARTESIAN_POINT ( 'NONE',  ( 19.97071067811864609, 11.72071067812981404, -158.7500000000000284 ) ) ;
#223838 = LINE ( 'NONE', #2225, #245862 ) ;
#223839 = EDGE_CURVE ( 'NONE', #247315, #98792, #24668, .T. ) ;
#223840 = ORIENTED_EDGE ( 'NONE', *, *, #145146, .T. ) ;
#223841 = CARTESIAN_POINT ( 'NONE',  ( -21.05000000000000071, -1.162701749926853712, -108.6000000000000227 ) ) ;
#223842 = DIRECTION ( 'NONE',  ( 1.000000000000000000, 0.000000000000000000, 0.000000000000000000 ) ) ;
#223843 = CARTESIAN_POINT ( 'NONE',  ( -20.64999999999999858, -9.000000000000001776, -23.60603087734756045 ) ) ;
#223844 = EDGE_CURVE ( 'NONE', #39976, #143381, #220288, .T. ) ;
#223845 = VERTEX_POINT ( 'NONE', #59077 ) ;
#223846 = AXIS2_PLACEMENT_3D ( 'NONE', #205631, #163964, #243485 ) ;
#223848 = EDGE_CURVE ( 'NONE', #34155, #235411, #245228, .T. ) ;
#223847 = CARTESIAN_POINT ( 'NONE',  ( 18.39999999999999858, -9.499999999988844479, -174.4221498493304239 ) ) ;
#223849 = DIRECTION ( 'NONE',  ( -1.000000000000000000, 0.000000000000000000, 0.000000000000000000 ) ) ;
#223850 = TOROIDAL_SURFACE ( 'NONE', #44808, 14.20833333333334103, 0.1000000000000000056 ) ;
#223851 = VERTEX_POINT ( 'NONE', #62971 ) ;
#223852 = AXIS2_PLACEMENT_3D ( 'NONE', #222265, #43670, #256212 ) ;
#223853 = CARTESIAN_POINT ( 'NONE',  ( -23.25000000000000000, 87.65000000001238334, -170.0231074845242745 ) ) ;
#223854 = ORIENTED_EDGE ( 'NONE', *, *, #9379, .F. ) ;
#223855 = EDGE_CURVE ( 'NONE', #47133, #192971, #203526, .T. ) ;
#223856 = DIRECTION ( 'NONE',  ( 0.000000000000000000, 0.000000000000000000, -1.000000000000000000 ) ) ;
#223857 = DIRECTION ( 'NONE',  ( 1.000000000000000000, 0.000000000000000000, 0.000000000000000000 ) ) ;
#223858 = CARTESIAN_POINT ( 'NONE',  ( 23.14999999999999503, 11.65000000001116298, -146.2500000000000284 ) ) ;
#223859 = CYLINDRICAL_SURFACE ( 'NONE', #7725, 0.09999999999999939493 ) ;
#223860 = ADVANCED_FACE ( 'NONE', ( #203767 ), #181649, .F. ) ;
#223861 = CARTESIAN_POINT ( 'NONE',  ( -23.15000000000000213, 42.98415524044398950, -233.9519173640447889 ) ) ;
#223862 = CARTESIAN_POINT ( 'NONE',  ( -16.87683809663752754, 66.13411015068081156, -156.7556806774549045 ) ) ;
#223863 = CARTESIAN_POINT ( 'NONE',  ( -23.15000000000000213, 1.115600667400684642E-11, -167.5000000000000284 ) ) ;
#223864 = DIRECTION ( 'NONE',  ( -0.000000000000000000, -0.000000000000000000, 1.000000000000000000 ) ) ;
#223865 = DIRECTION ( 'NONE',  ( -0.000000000000000000, -1.000000000000000000, 0.000000000000000000 ) ) ;
#223867 = EDGE_LOOP ( 'NONE', ( #168216, #75813, #122335, #244406 ) ) ;
#223866 = DIRECTION ( 'NONE',  ( -1.000000000000000000, -2.952720810173289112E-16, 0.000000000000000000 ) ) ;
#223868 = ORIENTED_EDGE ( 'NONE', *, *, #15905, .F. ) ;
#223870 = DIRECTION ( 'NONE',  ( 0.000000000000000000, 6.982962677686267499E-15, -1.000000000000000000 ) ) ;
#223869 = DIRECTION ( 'NONE',  ( 0.000000000000000000, 0.000000000000000000, 1.000000000000000000 ) ) ;
#223872 = ORIENTED_EDGE ( 'NONE', *, *, #193578, .T. ) ;
#223871 = PLANE ( 'NONE',  #130252 ) ;
#223873 = CIRCLE ( 'NONE', #123952, 11.74999999999999645 ) ;
#223874 = ORIENTED_EDGE ( 'NONE', *, *, #106181, .F. ) ;
#223875 = CARTESIAN_POINT ( 'NONE',  ( 18.59999999999999432, 2.953700692300310848, -208.6327728934509764 ) ) ;
#223877 = CARTESIAN_POINT ( 'NONE',  ( 20.19326291200817280, 10.15606098791077017, -175.2618618076036228 ) ) ;
#223876 = CIRCLE ( 'NONE', #115555, 11.65000000000000036 ) ;
#223879 = EDGE_CURVE ( 'NONE', #200983, #101872, #253567, .T. ) ;
#223878 = LINE ( 'NONE', #101329, #154863 ) ;
#223880 = DIRECTION ( 'NONE',  ( 0.000000000000000000, 0.000000000000000000, 1.000000000000000000 ) ) ;
#223881 = ADVANCED_FACE ( 'NONE', ( #40874 ), #413, .F. ) ;
#223882 = EDGE_CURVE ( 'NONE', #211413, #200161, #103360, .T. ) ;
#223883 = CARTESIAN_POINT ( 'NONE',  ( -18.39999999999999858, 20.72457956333081341, -227.9937486218739480 ) ) ;
#223884 = CARTESIAN_POINT ( 'NONE',  ( -20.65000000000000568, 7.249999999999983125, -12.65000000000000213 ) ) ;
#223886 = VECTOR ( 'NONE', #136954, 1000.000000000000000 ) ;
#223885 = DIRECTION ( 'NONE',  ( 0.000000000000000000, -1.000000000000000000, 6.308085367188393199E-16 ) ) ;
#223887 = EDGE_LOOP ( 'NONE', ( #80270, #77396, #48860, #52528 ) ) ;
#223888 = ORIENTED_EDGE ( 'NONE', *, *, #32590, .T. ) ;
#223889 = CYLINDRICAL_SURFACE ( 'NONE', #2401, 0.09999999999999939493 ) ;
#223890 = CIRCLE ( 'NONE', #144786, 7.900000000000007461 ) ;
#223891 = TOROIDAL_SURFACE ( 'NONE', #119902, 7.791421356237335338, 0.1000000000000000056 ) ;
#223892 = ORIENTED_EDGE ( 'NONE', *, *, #154390, .F. ) ;
#223893 = CARTESIAN_POINT ( 'NONE',  ( -21.05000000000000071, 79.13126459505528487, -235.8705213229730191 ) ) ;
#223894 = EDGE_LOOP ( 'NONE', ( #226787, #39268, #198011, #251069 ) ) ;
#223896 = CARTESIAN_POINT ( 'NONE',  ( -16.83794479845801106, 9.926357419362647150, -154.6964447042223014 ) ) ;
#223895 = AXIS2_PLACEMENT_3D ( 'NONE', #86910, #28284, #109055 ) ;
#223897 = DIRECTION ( 'NONE',  ( 1.000000000000000000, 0.000000000000000000, 0.000000000000000000 ) ) ;
#223898 = AXIS2_PLACEMENT_3D ( 'NONE', #103488, #225988, #183062 ) ;
#223899 = CARTESIAN_POINT ( 'NONE',  ( -20.85000000000000142, 71.99422445362657186, -246.4870034924427671 ) ) ;
#223900 = DIRECTION ( 'NONE',  ( 1.000000000000000000, -0.000000000000000000, -0.000000000000000000 ) ) ;
#223901 = VERTEX_POINT ( 'NONE', #199936 ) ;
#223902 = SPHERICAL_SURFACE ( 'NONE', #42204, 0.1000000000000000056 ) ;
#223903 = ORIENTED_EDGE ( 'NONE', *, *, #223024, .T. ) ;
#223904 = CARTESIAN_POINT ( 'NONE',  ( -16.84419801905645997, 66.05000000001155058, -48.69259733074643037 ) ) ;
#223905 = CARTESIAN_POINT ( 'NONE',  ( -20.64999999999999858, 76.00000000001142553, -36.02310748452432421 ) ) ;
#223906 = EDGE_CURVE ( 'NONE', #253143, #199368, #99500, .T. ) ;
#223907 = FACE_OUTER_BOUND ( 'NONE', #86787, .T. ) ;
#223908 = DIRECTION ( 'NONE',  ( -1.000000000000000000, -0.000000000000000000, -0.000000000000000000 ) ) ;
#223909 = ORIENTED_EDGE ( 'NONE', *, *, #11040, .T. ) ;
#223910 = LINE ( 'NONE', #183527, #210778 ) ;
#223911 = VERTEX_POINT ( 'NONE', #82503 ) ;
#223913 = ORIENTED_EDGE ( 'NONE', *, *, #62770, .T. ) ;
#223912 = CARTESIAN_POINT ( 'NONE',  ( -23.25000000000000000, 1.115600667400684642E-11, -74.90000000000000568 ) ) ;
#223914 = DIRECTION ( 'NONE',  ( -0.000000000000000000, 1.000000000000000000, 6.982962677686266711E-15 ) ) ;
#223915 = AXIS2_PLACEMENT_3D ( 'NONE', #174983, #173702, #191961 ) ;
#223916 = ORIENTED_EDGE ( 'NONE', *, *, #120066, .T. ) ;
#223917 = AXIS2_PLACEMENT_3D ( 'NONE', #50492, #51781, #93489 ) ;
#223918 = DIRECTION ( 'NONE',  ( -7.304098846218201720E-16, 1.000000000000000000, 0.000000000000000000 ) ) ;
#223919 = EDGE_LOOP ( 'NONE', ( #197397, #142282, #148498, #250981 ) ) ;
#223921 = AXIS2_PLACEMENT_3D ( 'NONE', #179118, #78675, #199948 ) ;
#223920 = CARTESIAN_POINT ( 'NONE',  ( -18.39999999999999858, 64.52683809664983983, -160.6971614177164724 ) ) ;
#223922 = VECTOR ( 'NONE', #48474, 1000.000000000000000 ) ;
#223923 = EDGE_CURVE ( 'NONE', #134939, #182341, #141167, .T. ) ;
#223924 = DIRECTION ( 'NONE',  ( 1.000000000000000000, 3.469446951953704435E-14, -2.003086131649669752E-14 ) ) ;
#223925 = VECTOR ( 'NONE', #80226, 1000.000000000000000 ) ;
#223926 = DIRECTION ( 'NONE',  ( -1.836970198721029934E-16, 0.9770955615653316162, 0.2128009952263604232 ) ) ;
#223927 = CARTESIAN_POINT ( 'NONE',  ( 0.000000000000000000, -11.25000000000000000, 0.000000000000000000 ) ) ;
#223928 = EDGE_CURVE ( 'NONE', #15616, #3891, #141228, .T. ) ;
#223929 = DIRECTION ( 'NONE',  ( 0.000000000000000000, -0.1350103645451945777, 0.9908441862701590219 ) ) ;
#223930 = ORIENTED_EDGE ( 'NONE', *, *, #174241, .F. ) ;
#223931 = EDGE_CURVE ( 'NONE', #154967, #181023, #201197, .T. ) ;
#223932 = LINE ( 'NONE', #203100, #156658 ) ;
#223933 = SURFACE_STYLE_FILL_AREA ( #244784 ) ;
#223934 = CARTESIAN_POINT ( 'NONE',  ( -18.33981767444297972, -9.569575789792892806, -140.8191618437252259 ) ) ;
#223935 = CIRCLE ( 'NONE', #194763, 0.09999999999999939493 ) ;
#223936 = VERTEX_POINT ( 'NONE', #42144 ) ;
#223937 = DIRECTION ( 'NONE',  ( 1.000000000000000000, 0.000000000000000000, 0.000000000000000000 ) ) ;
#223939 = EDGE_LOOP ( 'NONE', ( #17959, #142883, #127004, #132117, #196037 ) ) ;
#223938 = AXIS2_PLACEMENT_3D ( 'NONE', #64937, #162781, #63655 ) ;
#223941 = VECTOR ( 'NONE', #32027, 1000.000000000000227 ) ;
#223940 = CARTESIAN_POINT ( 'NONE',  ( -20.65000000000000568, 5.650000000011139001, -176.7499999999999716 ) ) ;
#223942 = ADVANCED_FACE ( 'NONE', ( #219460 ), #241610, .T. ) ;
#223943 = CLOSED_SHELL ( 'NONE', ( #9645, #196690, #132798, #135225, #252168, #47332, #190203, #65019, #175176, #216816, #194308, #198202, #229337, #28729, #143139, #124558, #228692, #130696, #54008, #232475, #214690, #188788, #221689, #220956, #109176, #28279, #45564, #10067, #7628, #98478, #120223, #160650, #19321, #132150, #196919, #65907, #10550, #152488, #151254, #232142, #132266, #9955, #91459, #235125, #156871, #112942, #226248, #212314, #179252, #4652, #160747, #236014, #184553, #71098, #129398, #133517, #240437, #130427, #129608, #45195, #152171, #32324, #52262, #109452, #80782, #6090, #195295, #124768, #179572, #93836, #68801, #109664, #77124, #145902, #91069, #232276, #85002, #121528, #43777, #255958, #141717, #132196, #212265, #203390, #201607, #231328, #240832, #88283, #104455, #116326, #199617, #194098, #66340, #239013, #99549, #167758, #56138, #204292, #104738, #136543, #33532, #210684, #220674, #113402, #216784, #217609, #135435, #94379, #134428, #248065, #136136, #15593, #135419, #117715, #45625, #37083, #247289, #165447, #57944, #28324, #165542, #24917, #224281, #102655, #82220, #244567, #102608, #210847, #167436, #53957, #78205, #201262, #3515, #240692, #156286, #191584, #110752, #62298, #129075, #223650, #8479, #185941, #106836, #29794, #154109, #141388, #208417, #152391, #28927, #178556, #222000, #124219, #177766, #62015, #100026, #160801, #100893, #229260, #113037, #33840, #17375, #77354, #249489, #143892, #162976, #31097, #256948, #27479, #243266, #243032, #52603, #130362, #147571, #146876, #189907, #189313, #34895, #182831, #71542, #57545, #212579, #55415, #21042, #111152, #174206, #180356, #30551, #172047, #170852, #99262, #90666, #104288, #49066, #119744, #185156, #215433, #127307, #72381, #137441, #21731, #62240, #83786, #128132, #2311, #41047, #85275, #166505, #132594, #242244, #173653, #221243, #34640, #43330, #100215, #159027, #90849, #25807, #126017, #230337, #87865, #216587, #84866, #9907, #60435, #38277, #246243, #228100, #88901, #21458, #91790, #148511, #82651, #59833, #114928, #70312, #226697, #48815, #178650, #119259, #173122, #67107, #36504, #93718, #142226, #252542, #160775, #247594, #203509, #60533, #37881, #80093, #200613, #94387, #194249, #219584, #52257, #141452, #12305, #226837, #235682, #100342, #91265, #12889, #37584, #9638, #47262, #164786, #252635, #157675, #141885, #257001, #251580, #19993, #78995, #1899, #223628, #83978, #140796, #121531, #118637, #42621, #192136, #155248, #239215, #147927, #33317, #31459, #210244, #133056, #220947, #146589, #31998, #172382, #240354, #44007, #138016, #200675, #178747, #164527, #245209, #224492, #249949, #211900, #209748, #74373, #21229, #52043, #26933, #8615, #88188, #6680, #251791, #15524, #243970, #19739, #1987, #241648, #220352, #181050, #37299, #193956, #44163, #90618, #140951, #142120, #135850, #36113, #162941, #151153, #48406, #171152, #37014, #163065, #235008, #194530, #227909, #39660, #68438, #232067, #152330, #254549, #28402, #109442, #184533, #256687, #201494, #118236, #120840, #136740, #216578, #103821, #109146, #166353, #206445, #257071, #211146, #65856, #106744, #4894, #31267, #16018, #24365, #182916, #229948, #32993, #208209, #256626, #63607, #36230, #245852, #257260, #176624, #87903, #42955, #84791, #236310, #117683, #96668, #228241, #90339, #102597, #17079, #100168, #203024, #89362, #53129, #182413, #124213, #236109, #101744, #178902, #92329, #65232, #45896, #231173, #30800, #160469, #254553, #64615, #182604, #27673, #4729, #16343, #183966, #140341, #110326, #118619, #171043, #244814, #104415, #68827, #241244, #16411, #122119, #211318, #159309, #150375, #109802, #29255, #39317, #121642, #162351, #45869, #106116, #258008, #145015, #21580, #140763, #185053, #166361, #210948, #20049, #94103, #107637, #77547, #159425, #18997, #52409, #179271, #37785, #34142, #120535, #16142, #5768, #46056, #119061, #70590, #257075, #233347, #150977, #144249, #22598, #126001, #248441, #135692, #127064, #39135, #231170, #59028, #14361, #60720, #55973, #170295, #149835, #78462, #115162, #203707, #251820, #164830, #42116, #39085, #27662, #99346, #53870, #213555, #197231, #187507, #207452 ) ) ;
#223944 = EDGE_CURVE ( 'NONE', #247736, #130315, #62054, .T. ) ;
#223945 = CARTESIAN_POINT ( 'NONE',  ( 21.05000000000000071, 87.29603075034764004, -166.9752083248604038 ) ) ;
#223946 = CYLINDRICAL_SURFACE ( 'NONE', #205873, 0.09999999999999817368 ) ;
#223948 = ORIENTED_EDGE ( 'NONE', *, *, #198970, .T. ) ;
#223947 = CARTESIAN_POINT ( 'NONE',  ( -16.93658623642901873, 9.980381671668284937, -146.6119027291292127 ) ) ;
#223949 = CARTESIAN_POINT ( 'NONE',  ( 20.95512820512820440, 12.01161663143393632, -206.2285874551107554 ) ) ;
#223950 = DIRECTION ( 'NONE',  ( -3.265361837132813093E-16, 1.000000000000000000, 0.000000000000000000 ) ) ;
#223951 = DIRECTION ( 'NONE',  ( 0.000000000000000000, 0.000000000000000000, 1.000000000000000000 ) ) ;
#223952 = CIRCLE ( 'NONE', #124038, 11.65000000000000746 ) ;
#223953 = EDGE_LOOP ( 'NONE', ( #181870, #146994 ) ) ;
#223954 = CARTESIAN_POINT ( 'NONE',  ( 21.13461538461538325, 8.885417037974459475, -12.35000000000000320 ) ) ;
#223955 = CARTESIAN_POINT ( 'NONE',  ( -17.11825945287481332, 10.05000000001113847, -154.8500000000000227 ) ) ;
#223956 = ORIENTED_EDGE ( 'NONE', *, *, #29132, .T. ) ;
#223957 = CARTESIAN_POINT ( 'NONE',  ( 18.54999999999999716, 66.05000000001152216, -48.67310748452433700 ) ) ;
#223958 = ADVANCED_FACE ( 'NONE', ( #186791 ), #228483, .F. ) ;
#223959 = ADVANCED_FACE ( 'NONE', ( #10709 ), #207835, .T. ) ;
#223960 = ORIENTED_EDGE ( 'NONE', *, *, #41457, .T. ) ;
#223961 = CIRCLE ( 'NONE', #211338, 0.1000000000000056677 ) ;
#223962 = DIRECTION ( 'NONE',  ( -0.000000000000000000, 1.000000000000000000, -0.000000000000000000 ) ) ;
#223964 = ORIENTED_EDGE ( 'NONE', *, *, #242505, .T. ) ;
#223963 = DIRECTION ( 'NONE',  ( 0.000000000000000000, 0.000000000000000000, 1.000000000000000000 ) ) ;
#223965 = ADVANCED_FACE ( 'NONE', ( #87655 ), #219156, .T. ) ;
#223966 = AXIS2_PLACEMENT_3D ( 'NONE', #164976, #65872, #201529 ) ;
#223969 = ORIENTED_EDGE ( 'NONE', *, *, #58089, .T. ) ;
#223968 = ORIENTED_EDGE ( 'NONE', *, *, #186855, .F. ) ;
#223967 = DIRECTION ( 'NONE',  ( 0.000000000000000000, 0.5000000000000014433, -0.8660254037844378194 ) ) ;
#223970 = DIRECTION ( 'NONE',  ( 1.000000000000000000, 0.000000000000000000, 0.000000000000000000 ) ) ;
#223971 = VECTOR ( 'NONE', #230516, 1000.000000000000000 ) ;
#223972 = DIRECTION ( 'NONE',  ( -0.000000000000000000, 0.9910465087640860649, -0.1335171055202901413 ) ) ;
#223973 = CIRCLE ( 'NONE', #199053, 0.6000000000000015321 ) ;
#223974 = ADVANCED_FACE ( 'NONE', ( #25156 ), #184188, .T. ) ;
#223975 = DIRECTION ( 'NONE',  ( -0.000000000000000000, 1.000000000000000000, 2.891205793294679805E-16 ) ) ;
#223976 = CIRCLE ( 'NONE', #219892, 11.75000000000001066 ) ;
#223978 = CARTESIAN_POINT ( 'NONE',  ( -12.25000000000000178, 66.65000000001155911, -52.77310748452439526 ) ) ;
#223977 = CARTESIAN_POINT ( 'NONE',  ( 18.39999999999999503, 5.650000000011139001, -46.15000000000000568 ) ) ;
#223979 = DIRECTION ( 'NONE',  ( 0.000000000000000000, -1.000000000000000000, -6.982962677686265922E-15 ) ) ;
#223980 = EDGE_CURVE ( 'NONE', #75871, #126699, #105922, .T. ) ;
#223981 = FACE_OUTER_BOUND ( 'NONE', #145172, .T. ) ;
#223982 = CIRCLE ( 'NONE', #194803, 0.09999999999999568956 ) ;
#223983 = CARTESIAN_POINT ( 'NONE',  ( -21.05000000000000071, 87.48912529308822172, -139.6231074845242688 ) ) ;
#223984 = DIRECTION ( 'NONE',  ( 0.000000000000000000, 0.8700118002898321601, -0.4930308989875230585 ) ) ;
#223985 = ORIENTED_EDGE ( 'NONE', *, *, #51942, .T. ) ;
#223986 = EDGE_LOOP ( 'NONE', ( #202198, #158587, #62162, #178595 ) ) ;
#223987 = EDGE_CURVE ( 'NONE', #61689, #23723, #145065, .T. ) ;
#223988 = DIRECTION ( 'NONE',  ( 1.186688945009010077E-16, 0.9651348961777157509, -0.2617529984165031243 ) ) ;
#223990 = ORIENTED_EDGE ( 'NONE', *, *, #106759, .T. ) ;
#223989 = DIRECTION ( 'NONE',  ( -1.000000000000000000, -0.000000000000000000, -0.000000000000000000 ) ) ;
#223991 = VERTEX_POINT ( 'NONE', #45973 ) ;
#223992 = EDGE_LOOP ( 'NONE', ( #145668, #106002, #186687, #81805, #237229, #92746, #243422, #33755, #33196, #246792, #48767, #28140 ) ) ;
#223993 = DIRECTION ( 'NONE',  ( 0.000000000000000000, -1.000000000000000000, 0.000000000000000000 ) ) ;
#223994 = EDGE_CURVE ( 'NONE', #164531, #249043, #178605, .T. ) ;
#223995 = B_SPLINE_CURVE_WITH_KNOTS ( 'NONE', 3,
 ( #181543, #114157, #2866, #160712, #60279, #219355, #75069, #306, #159408, #122848, #82388, #161987, #241500, #221903 ),
 .UNSPECIFIED., .F., .F.,
 ( 4, 2, 2, 2, 2, 2, 4 ),
 ( 1.398578778534940505E-17, 0.0003823333598417389258, 0.0005735000397626219141, 0.0006690833797230837099, 0.0007168750497033132526, 0.0007407708846934279697, 0.0007646667196835427952 ),
 .UNSPECIFIED. ) ;
#223996 = VECTOR ( 'NONE', #15074, 1000.000000000000000 ) ;
#223997 = ORIENTED_EDGE ( 'NONE', *, *, #92571, .F. ) ;
#223998 = DIRECTION ( 'NONE',  ( 1.000000000000000000, -0.000000000000000000, -0.000000000000000000 ) ) ;
#223999 = DIRECTION ( 'NONE',  ( 0.000000000000000000, -1.000000000000000000, -2.891205793294679805E-16 ) ) ;
#224000 = AXIS2_PLACEMENT_3D ( 'NONE', #236065, #79540, #142095 ) ;
#224002 = VERTEX_POINT ( 'NONE', #26430 ) ;
#224001 = ORIENTED_EDGE ( 'NONE', *, *, #157741, .F. ) ;
#224003 = ORIENTED_EDGE ( 'NONE', *, *, #126834, .T. ) ;
#224004 = FACE_OUTER_BOUND ( 'NONE', #205440, .T. ) ;
#224005 = EDGE_LOOP ( 'NONE', ( #53995, #121877, #224507, #90411 ) ) ;
#224006 = ORIENTED_EDGE ( 'NONE', *, *, #230723, .T. ) ;
#224007 = FACE_OUTER_BOUND ( 'NONE', #11196, .T. ) ;
#224008 = CARTESIAN_POINT ( 'NONE',  ( 23.24999999999999645, 78.10000000001190301, -103.0231074845242887 ) ) ;
#224010 = VERTEX_POINT ( 'NONE', #86352 ) ;
#224009 = CARTESIAN_POINT ( 'NONE',  ( -22.39999999999999858, 0.000000000000000000, 7.790779598373403836 ) ) ;
#224011 = FACE_OUTER_BOUND ( 'NONE', #242617, .T. ) ;
#224012 = CARTESIAN_POINT ( 'NONE',  ( 20.94999999999999574, 1.835341550224413698, -11.55515129256298046 ) ) ;
#224014 = ORIENTED_EDGE ( 'NONE', *, *, #165745, .F. ) ;
#224013 = DIRECTION ( 'NONE',  ( 0.000000000000000000, 0.000000000000000000, -1.000000000000000000 ) ) ;
#224015 = CARTESIAN_POINT ( 'NONE',  ( -18.44085059012131822, 11.51401249349495437, -176.7596946808784253 ) ) ;
#224016 = ORIENTED_EDGE ( 'NONE', *, *, #75807, .T. ) ;
#224017 = DIRECTION ( 'NONE',  ( 0.000000000000000000, 1.000000000000000000, 0.000000000000000000 ) ) ;
#224018 = VERTEX_POINT ( 'NONE', #165952 ) ;
#224019 = DIRECTION ( 'NONE',  ( 0.000000000000000000, 0.000000000000000000, -1.000000000000000000 ) ) ;
#224020 = DIRECTION ( 'NONE',  ( 0.000000000000000000, -0.008583690987162452199, -0.9999631594459053030 ) ) ;
#224021 = VERTEX_POINT ( 'NONE', #188062 ) ;
#224022 = VECTOR ( 'NONE', #75353, 1000.000000000000000 ) ;
#224023 = AXIS2_PLACEMENT_3D ( 'NONE', #21449, #203905, #181784 ) ;
#224025 = CARTESIAN_POINT ( 'NONE',  ( 23.24999999999999289, 64.35000000001156195, -57.37310748452439668 ) ) ;
#224024 = CARTESIAN_POINT ( 'NONE',  ( 21.04116576186320131, 10.62466307876251115, -45.82858176862794863 ) ) ;
#224026 = VECTOR ( 'NONE', #8601, 1000.000000000000000 ) ;
#224027 = DIRECTION ( 'NONE',  ( 0.000000000000000000, 0.000000000000000000, -1.000000000000000000 ) ) ;
#224028 = ORIENTED_EDGE ( 'NONE', *, *, #6841, .F. ) ;
#224029 = EDGE_LOOP ( 'NONE', ( #237087, #128118, #21823 ) ) ;
#224030 = CYLINDRICAL_SURFACE ( 'NONE', #9551, 0.5000000000000004441 ) ;
#224031 = EDGE_CURVE ( 'NONE', #38016, #66775, #66138, .T. ) ;
#224032 = CARTESIAN_POINT ( 'NONE',  ( 20.04999999999999716, 8.750000000011173285, -87.85000000000003695 ) ) ;
#224033 = ORIENTED_EDGE ( 'NONE', *, *, #111501, .T. ) ;
#224034 = CARTESIAN_POINT ( 'NONE',  ( 22.88900146558018989, 19.39258630652192394, -230.4280346437470826 ) ) ;
#224035 = EDGE_LOOP ( 'NONE', ( #238590, #29826, #177698, #80132 ) ) ;
#224036 = DIRECTION ( 'NONE',  ( 0.000000000000000000, -0.9126074666063769270, -0.4088369013363280513 ) ) ;
#224037 =( NAMED_UNIT ( * ) PLANE_ANGLE_UNIT ( ) SI_UNIT ( $, .RADIAN. ) );
#224038 = FACE_OUTER_BOUND ( 'NONE', #149331, .T. ) ;
#224039 = FACE_OUTER_BOUND ( 'NONE', #235758, .T. ) ;
#224040 = VECTOR ( 'NONE', #191563, 1000.000000000000000 ) ;
#224041 = VERTEX_POINT ( 'NONE', #167243 ) ;
#224042 = VECTOR ( 'NONE', #83672, 1000.000000000000114 ) ;
#224043 = CARTESIAN_POINT ( 'NONE',  ( 18.43630871534867666, -9.679800874791856913, -207.6606320679839541 ) ) ;
#224044 = EDGE_CURVE ( 'NONE', #249596, #160190, #20370, .T. ) ;
#224045 = VERTEX_POINT ( 'NONE', #48540 ) ;
#224046 = VECTOR ( 'NONE', #80640, 1000.000000000000000 ) ;
#224047 = EDGE_LOOP ( 'NONE', ( #150077, #236227, #12826 ) ) ;
#224048 = ORIENTED_EDGE ( 'NONE', *, *, #240549, .F. ) ;
#224049 = B_SPLINE_CURVE_WITH_KNOTS ( 'NONE', 3,
 ( #40770, #103248, #39490, #137260, #120317, #199833, #119003 ),
 .UNSPECIFIED., .F., .F.,
 ( 4, 3, 4 ),
 ( 0.000000000000000000, 3.357501770815288591E-05, 5.199112466349617109E-05 ),
 .UNSPECIFIED. ) ;
#224050 = DIRECTION ( 'NONE',  ( 1.000000000000000000, 1.541880601228652843E-16, 2.878400969107353907E-16 ) ) ;
#224051 = CARTESIAN_POINT ( 'NONE',  ( 18.59999999999999076, 11.65000000001115943, -192.3499999999999659 ) ) ;
#224052 = DIRECTION ( 'NONE',  ( 1.000000000000000000, -0.000000000000000000, -0.000000000000000000 ) ) ;
#224053 = DIRECTION ( 'NONE',  ( 1.000000000000000000, 0.000000000000000000, 0.000000000000000000 ) ) ;
#224054 = FACE_OUTER_BOUND ( 'NONE', #35980, .T. ) ;
#224056 = CARTESIAN_POINT ( 'NONE',  ( -18.69999999999999929, -11.65000000000000036, 32.89999999999999858 ) ) ;
#224055 = LINE ( 'NONE', #246206, #170562 ) ;
#224058 = ORIENTED_EDGE ( 'NONE', *, *, #13314, .F. ) ;
#224057 = CARTESIAN_POINT ( 'NONE',  ( 18.44208962362600701, 77.38084206055300740, -241.7753309371236980 ) ) ;
#224059 = DIRECTION ( 'NONE',  ( 1.000000000000000000, -0.000000000000000000, -0.000000000000000000 ) ) ;
#224060 = ORIENTED_EDGE ( 'NONE', *, *, #205775, .T. ) ;
#224061 = SPHERICAL_SURFACE ( 'NONE', #92503, 0.1000000000000000056 ) ;
#224062 = ORIENTED_EDGE ( 'NONE', *, *, #137577, .F. ) ;
#224063 = ORIENTED_EDGE ( 'NONE', *, *, #14971, .T. ) ;
#224064 = DIRECTION ( 'NONE',  ( 1.000000000000000000, 0.000000000000000000, 0.000000000000000000 ) ) ;
#224065 = CARTESIAN_POINT ( 'NONE',  ( -21.55000000000000071, 68.85000000001222986, -148.7731074845244166 ) ) ;
#224066 = FACE_OUTER_BOUND ( 'NONE', #79703, .T. ) ;
#224067 = CARTESIAN_POINT ( 'NONE',  ( 14.11444803880196552, 9.457431528860066550, -81.99991693789971237 ) ) ;
#224068 = AXIS2_PLACEMENT_3D ( 'NONE', #234329, #54414, #36156 ) ;
#224069 = AXIS2_PLACEMENT_3D ( 'NONE', #23880, #103362, #143784 ) ;
#224070 = CIRCLE ( 'NONE', #169965, 0.09999999999999939493 ) ;
#224071 = DIRECTION ( 'NONE',  ( 1.000000000000000000, 2.952720810173289112E-16, -0.000000000000000000 ) ) ;
#224072 = ORIENTED_EDGE ( 'NONE', *, *, #142115, .T. ) ;
#224073 = VERTEX_POINT ( 'NONE', #168546 ) ;
#224074 = DIRECTION ( 'NONE',  ( 1.000000000000000000, 0.000000000000000000, 0.000000000000000000 ) ) ;
#224075 = VERTEX_POINT ( 'NONE', #248020 ) ;
#224076 = DIRECTION ( 'NONE',  ( -1.000000000000000000, 0.000000000000000000, 0.000000000000000000 ) ) ;
#224077 = FACE_OUTER_BOUND ( 'NONE', #178823, .T. ) ;
#224079 = LINE ( 'NONE', #126265, #194665 ) ;
#224078 = CIRCLE ( 'NONE', #257337, 0.09999999999998898659 ) ;
#224080 = DIRECTION ( 'NONE',  ( 0.000000000000000000, -6.547589603894034005E-15, 1.000000000000000000 ) ) ;
#224081 = DIRECTION ( 'NONE',  ( 0.000000000000000000, -6.308085367188388072E-15, 1.000000000000000000 ) ) ;
#224082 = CARTESIAN_POINT ( 'NONE',  ( 21.05000000000000071, 71.00000000001260503, -191.1178414656112921 ) ) ;
#224083 = ORIENTED_EDGE ( 'NONE', *, *, #228535, .F. ) ;
#224084 = CARTESIAN_POINT ( 'NONE',  ( 20.85000000000000142, -1.835859311432481045, -212.6044391687984785 ) ) ;
#224085 = CARTESIAN_POINT ( 'NONE',  ( 21.00000000000000000, -11.75000000000000178, 11.89999999999999680 ) ) ;
#224087 = EDGE_CURVE ( 'NONE', #101407, #34727, #203701, .T. ) ;
#224086 = DIRECTION ( 'NONE',  ( -1.073024830501117923E-15, 0.9126074666063771490, 0.4088369013363281623 ) ) ;
#224088 = CARTESIAN_POINT ( 'NONE',  ( 18.53691006697079757, 65.69784844286159853, -178.8209087672253474 ) ) ;
#224089 = FACE_OUTER_BOUND ( 'NONE', #105094, .T. ) ;
#224090 = ADVANCED_FACE ( 'NONE', ( #14582 ), #176215, .T. ) ;
#224091 = AXIS2_PLACEMENT_3D ( 'NONE', #158225, #162053, #220726 ) ;
#224092 = CARTESIAN_POINT ( 'NONE',  ( 18.47688499308725696, 77.21655692720625552, -241.7530664668917098 ) ) ;
#224093 = VECTOR ( 'NONE', #1493, 1000.000000000000000 ) ;
#224094 = VECTOR ( 'NONE', #66450, 1000.000000000000114 ) ;
#224095 = VERTEX_POINT ( 'NONE', #253156 ) ;
#224096 = AXIS2_PLACEMENT_3D ( 'NONE', #207485, #147496, #229605 ) ;
#224097 = ADVANCED_FACE ( 'NONE', ( #91528 ), #52377, .F. ) ;
#224098 = LINE ( 'NONE', #130133, #53829 ) ;
#224099 = ORIENTED_EDGE ( 'NONE', *, *, #24165, .T. ) ;
#224100 =( REPRESENTATION_RELATIONSHIP ('NONE','NONE', #36900, #151872 ) REPRESENTATION_RELATIONSHIP_WITH_TRANSFORMATION ( #104172 )SHAPE_REPRESENTATION_RELATIONSHIP( ) );
#224101 = CARTESIAN_POINT ( 'NONE',  ( 18.49999999999999645, -1.835859311443640340, -45.00443916879852679 ) ) ;
#224102 = ADVANCED_FACE ( 'NONE', ( #92791 ), #128883, .F. ) ;
#224103 = CARTESIAN_POINT ( 'NONE',  ( -20.94999999999999929, -11.29603075032412995, -137.0478991596638991 ) ) ;
#224104 = DIRECTION ( 'NONE',  ( -1.000000000000000000, -0.000000000000000000, -0.000000000000000000 ) ) ;
#224105 = ORIENTED_EDGE ( 'NONE', *, *, #48174, .T. ) ;
#224106 = PLANE ( 'NONE',  #142435 ) ;
#224107 = CARTESIAN_POINT ( 'NONE',  ( 20.94999999999999929, 1.115649653272650466E-11, -196.9999999999999432 ) ) ;
#224108 = DIRECTION ( 'NONE',  ( -1.000000000000000000, 1.335000415235278971E-16, -2.979993593738921214E-16 ) ) ;
#224109 = LINE ( 'NONE', #200710, #242106 ) ;
#224111 = EDGE_CURVE ( 'NONE', #3356, #78303, #78770, .T. ) ;
#224110 = CIRCLE ( 'NONE', #128272, 0.2000000000000000944 ) ;
#224112 = DIRECTION ( 'NONE',  ( 0.000000000000000000, 0.000000000000000000, -1.000000000000000000 ) ) ;
#224113 = AXIS2_PLACEMENT_3D ( 'NONE', #146062, #45687, #204748 ) ;
#224114 = CARTESIAN_POINT ( 'NONE',  ( -18.59999999999999787, 1.115600667400684642E-11, -134.0000000000000000 ) ) ;
#224115 = AXIS2_PLACEMENT_3D ( 'NONE', #34838, #156071, #118196 ) ;
#224116 = EDGE_LOOP ( 'NONE', ( #152877, #76440, #113644, #8087 ) ) ;
#224117 = CARTESIAN_POINT ( 'NONE',  ( -23.25000000000000000, 77.83585931145600512, -158.5186683157258187 ) ) ;
#224119 = ORIENTED_EDGE ( 'NONE', *, *, #255759, .T. ) ;
#224118 = LINE ( 'NONE', #45491, #109389 ) ;
#224120 = DIRECTION ( 'NONE',  ( 0.000000000000000000, 0.9126074666063769270, 0.4088369013363282733 ) ) ;
#224121 = AXIS2_PLACEMENT_3D ( 'NONE', #184542, #244520, #65892 ) ;
#224122 = EDGE_CURVE ( 'NONE', #251542, #64025, #49756, .T. ) ;
#224123 = ORIENTED_EDGE ( 'NONE', *, *, #159213, .T. ) ;
#224124 = DIRECTION ( 'NONE',  ( 0.7071067811865456854, -0.7071067811865493491, -0.000000000000000000 ) ) ;
#224125 = APPLICATION_PROTOCOL_DEFINITION ( 'draft international standard', 'automotive_design', 1998, #130817 ) ;
#224126 = DIRECTION ( 'NONE',  ( 1.000000000000000000, 0.000000000000000000, 0.000000000000000000 ) ) ;
#224127 = ORIENTED_EDGE ( 'NONE', *, *, #245504, .T. ) ;
#224128 = CARTESIAN_POINT ( 'NONE',  ( -20.54999999999999716, 6.300962096140152013, -220.8843452229073705 ) ) ;
#224129 = CARTESIAN_POINT ( 'NONE',  ( 14.88075390448864610, 9.431689550535256927, -185.7792900322359912 ) ) ;
#224130 = PRODUCT_DEFINITION_SHAPE ( 'NONE', 'NONE',  #94639 ) ;
#224131 = TOROIDAL_SURFACE ( 'NONE', #257395, 0.6000000000000009770, 0.1000000000000000056 ) ;
#224132 = VECTOR ( 'NONE', #249472, 1000.000000000000227 ) ;
#224133 = CLOSED_SHELL ( 'NONE', ( #93897, #47892, #33653, #170708, #97719, #139357, #64147, #80802, #7186, #51314, #182074, #120636, #213007, #179478, #100553, #2770, #17306, #181923, #191589, #169559, #44640, #9334, #66194, #198188, #48023, #94882, #121358, #108761, #19307, #258021, #193846, #211537, #11068, #11001, #241014, #208471, #4014, #86740, #197326, #164529, #44662, #183888, #186011, #205671, #119718, #13122, #224532, #171339, #163535, #70517, #190255, #154595, #115889, #118161, #191048, #179096, #122679, #258020, #94552, #163372, #61318, #94738, #139505, #57481, #69428, #89839, #99120, #2628, #92925, #86458, #206268, #233916, #103919, #185211, #1940, #100690, #68652, #56422, #65402, #81514, #59692, #42662, #188399, #222418, #149592, #137074, #67560, #94021, #19654, #138162, #32751, #242608, #159916, #231090, #174871, #37111, #18072, #49478, #113408, #138811, #101697, #153954, #189282, #22296, #172687, #182188, #37556, #71753, #189242, #27508, #120858, #15639, #42922, #71572, #137581, #54086, #51408, #90143, #191102, #64823, #81975, #76630, #127970, #192267, #182708, #140081, #204178, #162066, #119834, #186235, #139084, #50499, #153976, #33444, #217904, #212193, #58763, #148720, #123805, #97289, #118623, #204649, #236510, #12695, #159095, #98391, #237860, #139395, #7836, #46428, #242785, #17858, #140897, #147112, #70115, #61441, #214578, #96858, #91979, #227760, #65331, #45270, #37992, #92245, #207098, #232717, #35664, #48202, #227511, #246503, #69526, #131837, #17048, #154468, #29554, #156589, #7195, #25598, #62841, #188049, #167470, #95644, #175490, #186716, #159322, #100201, #251266, #31939, #80523, #47469, #33054, #56734, #147879, #152926, #57846, #62765, #253991, #99107, #241167, #29631, #125646, #54997, #204100, #11762, #176744, #141176, #88574, #176264, #74765, #179137, #131958, #89495, #165784, #150158, #78273, #203018, #70292, #71787, #101958, #128554, #257949, #191055, #57699, #158952, #244493, #97946, #248633, #117888, #38320, #62649, #127439, #70202, #186045, #167916, #159473, #112352, #257709, #255235, #101123, #169155, #159750, #218227, #225111, #230087, #147758, #101059, #125203, #198506, #230127, #206439, #121734, #114503, #71374, #108850, #80934, #59645, #18701, #190458, #7990, #237126, #98754, #94791, #145853, #184515, #194053, #169381, #19869, #81736, #102231, #126012, #167876, #87145, #51905, #228676, #89373, #113604, #244780, #60641, #51797, #100852, #241339, #147934, #70066, #179579, #39348, #178031, #150587 ) ) ;
#224134 = CARTESIAN_POINT ( 'NONE',  ( -20.94999999999999929, 67.23127455305835554, -235.8551265064784559 ) ) ;
#224135 = ORIENTED_EDGE ( 'NONE', *, *, #227888, .T. ) ;
#224136 = ORIENTED_EDGE ( 'NONE', *, *, #235329, .F. ) ;
#224137 = CARTESIAN_POINT ( 'NONE',  ( 21.05000000000000071, 10.62872031401550288, -74.66491356908764487 ) ) ;
#224138 = CARTESIAN_POINT ( 'NONE',  ( -22.48660254037843487, 64.35000000001166143, -69.57310748452438531 ) ) ;
#224139 = CARTESIAN_POINT ( 'NONE',  ( -18.59999999999999787, -1.164121893230052995, -208.9148480855715775 ) ) ;
#224140 = ADVANCED_FACE ( 'NONE', ( #77089 ), #132988, .T. ) ;
#224141 = CARTESIAN_POINT ( 'NONE',  ( 23.14999999999999858, 1.115625160336667635E-11, -132.0000000000000284 ) ) ;
#224143 = AXIS2_PLACEMENT_3D ( 'NONE', #174097, #171516, #193617 ) ;
#224142 = LINE ( 'NONE', #6384, #236122 ) ;
#224144 = AXIS2_PLACEMENT_3D ( 'NONE', #87307, #144713, #166899 ) ;
#224146 = CARTESIAN_POINT ( 'NONE',  ( -18.50000000000000355, -9.419203418015493767, -74.24778581042869519 ) ) ;
#224145 = CARTESIAN_POINT ( 'NONE',  ( 21.07954640115312728, -1.282382883101060633, -194.8016345785744647 ) ) ;
#224147 = DIRECTION ( 'NONE',  ( -1.000000000000000000, 0.000000000000000000, 0.000000000000000000 ) ) ;
#224148 = VECTOR ( 'NONE', #48394, 1000.000000000000227 ) ;
#224149 = FACE_OUTER_BOUND ( 'NONE', #224175, .T. ) ;
#224150 = DIRECTION ( 'NONE',  ( 1.000000000000000000, 0.000000000000000000, -0.000000000000000000 ) ) ;
#224151 = LINE ( 'NONE', #143334, #153182 ) ;
#224152 = ORIENTED_EDGE ( 'NONE', *, *, #145802, .F. ) ;
#224153 = EDGE_LOOP ( 'NONE', ( #171097, #65405, #47423 ) ) ;
#224154 = LINE ( 'NONE', #102909, #202592 ) ;
#224155 = CYLINDRICAL_SURFACE ( 'NONE', #99426, 0.9000000000000014655 ) ;
#224157 = CARTESIAN_POINT ( 'NONE',  ( -15.75000000000000355, 12.70026017068886937, -215.3766613508543628 ) ) ;
#224156 = CARTESIAN_POINT ( 'NONE',  ( 20.94999999999999929, 7.128833340093095217, -233.7327013124392749 ) ) ;
#224158 = AXIS2_PLACEMENT_3D ( 'NONE', #165700, #200946, #203521 ) ;
#224159 = EDGE_CURVE ( 'NONE', #161458, #211904, #33066, .T. ) ;
#224160 = CARTESIAN_POINT ( 'NONE',  ( 20.95462737510932882, 39.25131534400754418, -236.8220897444442414 ) ) ;
#224161 = DIRECTION ( 'NONE',  ( 0.000000000000000000, -6.982962677686266711E-15, 1.000000000000000000 ) ) ;
#224162 = DIRECTION ( 'NONE',  ( 0.000000000000000000, -1.000000000000000000, -6.982962677686266711E-15 ) ) ;
#224163 = AXIS2_PLACEMENT_3D ( 'NONE', #90282, #9475, #227238 ) ;
#224164 = DIRECTION ( 'NONE',  ( 0.000000000000000000, 0.8814952561688442767, -0.4721928772777324035 ) ) ;
#224165 = EDGE_CURVE ( 'NONE', #128905, #247, #216348, .T. ) ;
#224166 = ORIENTED_EDGE ( 'NONE', *, *, #191910, .F. ) ;
#224167 = AXIS2_PLACEMENT_3D ( 'NONE', #42275, #142628, #117946 ) ;
#224168 = AXIS2_PLACEMENT_3D ( 'NONE', #150345, #79753, #255803 ) ;
#224169 = CARTESIAN_POINT ( 'NONE',  ( -23.25000000000000000, 74.00000000001229239, -156.7984855617622770 ) ) ;
#224170 = AXIS2_PLACEMENT_3D ( 'NONE', #228784, #65834, #187098 ) ;
#224171 = ORIENTED_EDGE ( 'NONE', *, *, #33761, .F. ) ;
#224172 = EDGE_CURVE ( 'NONE', #166383, #151298, #149085, .T. ) ;
#224173 = CARTESIAN_POINT ( 'NONE',  ( -18.59999999999999787, -9.523954320741633950, -73.88201705682730847 ) ) ;
#224174 = LINE ( 'NONE', #204607, #88000 ) ;
#224175 = EDGE_LOOP ( 'NONE', ( #135719, #126782, #168236, #154705 ) ) ;
#224176 = CARTESIAN_POINT ( 'NONE',  ( -18.50000000000000000, 18.34711819382569686, -236.8747682978092541 ) ) ;
#224177 = EDGE_CURVE ( 'NONE', #1798, #99053, #251870, .T. ) ;
#224178 = ORIENTED_EDGE ( 'NONE', *, *, #248413, .F. ) ;
#224179 = DIRECTION ( 'NONE',  ( 1.000000000000000000, -3.265361837132813093E-16, -2.280189983783949500E-30 ) ) ;
#224180 = CARTESIAN_POINT ( 'NONE',  ( 21.05000000000000071, -11.74999999998883560, -97.60000000000005116 ) ) ;
#224181 = DIRECTION ( 'NONE',  ( 0.000000000000000000, -0.9915357197604971473, 0.1298341882519111479 ) ) ;
#224182 = ADVANCED_FACE ( 'NONE', ( #54938 ), #194500, .T. ) ;
#224183 = LINE ( 'NONE', #246328, #29264 ) ;
#224184 = EDGE_CURVE ( 'NONE', #147639, #56206, #171112, .T. ) ;
#224185 = CARTESIAN_POINT ( 'NONE',  ( 23.14999999999999503, 17.01923898301590654, -224.3994341343041867 ) ) ;
#224186 = FACE_OUTER_BOUND ( 'NONE', #179999, .T. ) ;
#224187 = CARTESIAN_POINT ( 'NONE',  ( -21.14999999999999858, 57.65152438469984730, -226.2879053819737010 ) ) ;
#224188 = DIRECTION ( 'NONE',  ( 0.7071359030028113724, 0.000000000000000000, 0.7070776581708677622 ) ) ;
#224190 = ORIENTED_EDGE ( 'NONE', *, *, #72040, .T. ) ;
#224189 = CARTESIAN_POINT ( 'NONE',  ( 21.07189867249812210, 65.27501972991944967, -191.3106560422477003 ) ) ;
#224192 = CARTESIAN_POINT ( 'NONE',  ( 21.56666275994540172, 76.00000000001242029, -176.9804758914176830 ) ) ;
#224191 = CARTESIAN_POINT ( 'NONE',  ( 18.59999999999999432, 2.859758780633683273, -208.6670499591424459 ) ) ;
#224193 = ORIENTED_EDGE ( 'NONE', *, *, #69453, .F. ) ;
#224195 = VERTEX_POINT ( 'NONE', #94078 ) ;
#224194 = DIRECTION ( 'NONE',  ( -1.000000000000000000, 0.000000000000000000, 0.000000000000000000 ) ) ;
#224196 = ORIENTED_EDGE ( 'NONE', *, *, #209290, .F. ) ;
#224197 = CARTESIAN_POINT ( 'NONE',  ( 18.52130828395272744, 85.48139550263741171, -62.49860076064062753 ) ) ;
#224198 = CARTESIAN_POINT ( 'NONE',  ( 21.00000000000000000, 9.750000000011153745, -45.85000000000000142 ) ) ;
#224199 = EDGE_CURVE ( 'NONE', #218111, #187553, #58100, .T. ) ;
#224200 = CARTESIAN_POINT ( 'NONE',  ( 21.04999999999999361, -0.01759718699768685404, -127.5592291063394725 ) ) ;
#224201 = DIRECTION ( 'NONE',  ( -1.000000000000000000, 0.000000000000000000, -0.000000000000000000 ) ) ;
#224202 = LINE ( 'NONE', #45581, #106468 ) ;
#224203 = EDGE_CURVE ( 'NONE', #234881, #182918, #62230, .T. ) ;
#224204 = EDGE_CURVE ( 'NONE', #75721, #68978, #60085, .T. ) ;
#224205 = CARTESIAN_POINT ( 'NONE',  ( 18.49999999999999645, 1.728086936805617757, -53.88443500516780915 ) ) ;
#224206 = CARTESIAN_POINT ( 'NONE',  ( 23.24999999999999645, 1.148907358139439339E-11, -201.0000000000015064 ) ) ;
#224207 = DIRECTION ( 'NONE',  ( 1.000000000000000000, 0.000000000000000000, 0.000000000000000000 ) ) ;
#224208 = CIRCLE ( 'NONE', #111799, 0.09999999999999939493 ) ;
#224209 = ORIENTED_EDGE ( 'NONE', *, *, #187171, .T. ) ;
#224210 = EDGE_LOOP ( 'NONE', ( #214569, #46670, #154836, #235399 ) ) ;
#224211 = AXIS2_PLACEMENT_3D ( 'NONE', #248380, #69761, #90573 ) ;
#224212 = LINE ( 'NONE', #20919, #210355 ) ;
#224213 = CIRCLE ( 'NONE', #249179, 0.1000000000000124678 ) ;
#224214 = ORIENTED_EDGE ( 'NONE', *, *, #85522, .F. ) ;
#224215 = DIRECTION ( 'NONE',  ( 1.000000000000000000, 0.000000000000000000, 0.000000000000000000 ) ) ;
#224216 = ORIENTED_EDGE ( 'NONE', *, *, #216413, .T. ) ;
#224217 = DIRECTION ( 'NONE',  ( 4.336808689942128965E-15, -0.8660254037844367092, 0.5000000000000037748 ) ) ;
#224218 = EDGE_CURVE ( 'NONE', #256147, #18136, #23585, .T. ) ;
#224219 = CARTESIAN_POINT ( 'NONE',  ( 20.04142135391667168, 11.75000000000000711, -24.70250686562997089 ) ) ;
#224220 = CARTESIAN_POINT ( 'NONE',  ( -5.999999999999938716, 64.65000000001120384, -22.02310748452479316 ) ) ;
#224221 = EDGE_CURVE ( 'NONE', #56815, #4098, #157957, .T. ) ;
#224222 = CARTESIAN_POINT ( 'NONE',  ( -20.85000000000000142, -1.736705739456431807, -212.5174225876236846 ) ) ;
#224223 = CARTESIAN_POINT ( 'NONE',  ( 21.05000000000000071, 7.128833340093095217, -233.7327013124392749 ) ) ;
#224224 = VERTEX_POINT ( 'NONE', #198320 ) ;
#224225 = CARTESIAN_POINT ( 'NONE',  ( 23.14999999999998437, 71.95000000001213891, -136.5231074845243029 ) ) ;
#224226 = AXIS2_PLACEMENT_3D ( 'NONE', #231211, #115096, #194666 ) ;
#224227 = EDGE_CURVE ( 'NONE', #83831, #196062, #117508, .T. ) ;
#224229 = AXIS2_PLACEMENT_3D ( 'NONE', #96526, #176116, #255572 ) ;
#224228 = DIRECTION ( 'NONE',  ( 1.000000000000000000, 0.000000000000000000, 0.000000000000000000 ) ) ;
#224230 = CARTESIAN_POINT ( 'NONE',  ( 18.40000000000000213, 85.50000000001161027, -62.52374538734413534 ) ) ;
#224231 = DIRECTION ( 'NONE',  ( 1.000000000000000000, 0.000000000000000000, 0.000000000000000000 ) ) ;
#224232 = ORIENTED_EDGE ( 'NONE', *, *, #54167, .T. ) ;
#224234 = LINE ( 'NONE', #222947, #206328 ) ;
#224233 = CARTESIAN_POINT ( 'NONE',  ( -22.47071067811865319, 7.720074744509219933, -133.9009075452974002 ) ) ;
#224235 = VERTEX_POINT ( 'NONE', #163077 ) ;
#224238 = ORIENTED_EDGE ( 'NONE', *, *, #36832, .T. ) ;
#224237 = CYLINDRICAL_SURFACE ( 'NONE', #175358, 0.09999999999998898659 ) ;
#224236 = DIRECTION ( 'NONE',  ( 0.000000000000000000, 0.000000000000000000, -1.000000000000000000 ) ) ;
#224239 = ORIENTED_EDGE ( 'NONE', *, *, #205213, .F. ) ;
#224240 = AXIS2_PLACEMENT_3D ( 'NONE', #236849, #154784, #76488 ) ;
#224241 = CARTESIAN_POINT ( 'NONE',  ( 18.59999999999999076, 69.55000000001230376, -160.0060803140843859 ) ) ;
#224242 = DIRECTION ( 'NONE',  ( -1.000000000000000000, -0.000000000000000000, -0.000000000000000000 ) ) ;
#224243 = SPHERICAL_SURFACE ( 'NONE', #95919, 0.1000000000000000056 ) ;
#224244 = ORIENTED_EDGE ( 'NONE', *, *, #170019, .F. ) ;
#224245 = DIRECTION ( 'NONE',  ( 1.000000000000000000, 0.000000000000000000, 0.000000000000000000 ) ) ;
#224246 = DIRECTION ( 'NONE',  ( -1.000000000000000000, 0.000000000000000000, 0.000000000000000000 ) ) ;
#224248 = LINE ( 'NONE', #83433, #30120 ) ;
#224247 = CARTESIAN_POINT ( 'NONE',  ( -20.85000000000000142, -1.164121893241208960, -41.41484808557160591 ) ) ;
#224250 = EDGE_LOOP ( 'NONE', ( #104413, #6535, #178409, #180336, #111880 ) ) ;
#224249 = LINE ( 'NONE', #120060, #126638 ) ;
#224251 = EDGE_CURVE ( 'NONE', #209230, #52463, #137246, .T. ) ;
#224252 = ORIENTED_EDGE ( 'NONE', *, *, #144468, .T. ) ;
#224253 = EDGE_CURVE ( 'NONE', #125106, #73834, #183045, .T. ) ;
#224254 = AXIS2_PLACEMENT_3D ( 'NONE', #219908, #144202, #165071 ) ;
#224255 = CARTESIAN_POINT ( 'NONE',  ( 19.80993210785464242, 64.25000000001178080, -78.25598973563708682 ) ) ;
#224256 = DIRECTION ( 'NONE',  ( 0.000000000000000000, 0.000000000000000000, -1.000000000000000000 ) ) ;
#224257 = AXIS2_PLACEMENT_3D ( 'NONE', #79642, #103056, #21004 ) ;
#224258 = AXIS2_PLACEMENT_3D ( 'NONE', #226377, #47748, #187298 ) ;
#224259 = CARTESIAN_POINT ( 'NONE',  ( -20.94999999999999929, 11.60000000001115517, -160.5717967697245285 ) ) ;
#224260 = VERTEX_POINT ( 'NONE', #19704 ) ;
#224261 = DIRECTION ( 'NONE',  ( 0.000000000000000000, 0.000000000000000000, -1.000000000000000000 ) ) ;
#224262 = ORIENTED_EDGE ( 'NONE', *, *, #133954, .T. ) ;
#224263 = DIRECTION ( 'NONE',  ( 1.000000000000000000, 0.000000000000000000, -0.000000000000000000 ) ) ;
#224264 = EDGE_CURVE ( 'NONE', #90934, #114385, #66336, .T. ) ;
#224265 = DIRECTION ( 'NONE',  ( -1.000000000000000000, -0.000000000000000000, -0.000000000000000000 ) ) ;
#224266 = FACE_OUTER_BOUND ( 'NONE', #356, .T. ) ;
#224267 = CIRCLE ( 'NONE', #216069, 0.09999999999999939493 ) ;
#224268 = VERTEX_POINT ( 'NONE', #120113 ) ;
#224269 = DIRECTION ( 'NONE',  ( 0.000000000000000000, -0.01562499999996560217, -0.9998779222360102414 ) ) ;
#224270 = EDGE_CURVE ( 'NONE', #61130, #186768, #80926, .T. ) ;
#224271 = ADVANCED_FACE ( 'NONE', ( #180056 ), #207991, .T. ) ;
#224272 = AXIS2_PLACEMENT_3D ( 'NONE', #196363, #215911, #78957 ) ;
#224273 = CIRCLE ( 'NONE', #37053, 0.3999999999999975797 ) ;
#224274 = CARTESIAN_POINT ( 'NONE',  ( -18.34374000495059676, 64.52683809664929981, -78.77310748452438816 ) ) ;
#224275 = CIRCLE ( 'NONE', #111874, 0.09999999999999939493 ) ;
#224276 = EDGE_CURVE ( 'NONE', #22349, #52627, #100478, .T. ) ;
#224277 = ORIENTED_EDGE ( 'NONE', *, *, #128764, .T. ) ;
#224278 = EDGE_LOOP ( 'NONE', ( #32511, #12620, #37457, #4649 ) ) ;
#224281 = ADVANCED_FACE ( 'NONE', ( #177519 ), #121400, .T. ) ;
#224280 = EDGE_CURVE ( 'NONE', #80961, #222419, #99607, .T. ) ;
#224279 = VECTOR ( 'NONE', #109323, 1000.000000000000000 ) ;
#224282 = VERTEX_POINT ( 'NONE', #157965 ) ;
#224283 = DIRECTION ( 'NONE',  ( -1.000000000000000000, 0.000000000000000000, -0.000000000000000000 ) ) ;
#224284 = ORIENTED_EDGE ( 'NONE', *, *, #44094, .F. ) ;
#224286 = ORIENTED_EDGE ( 'NONE', *, *, #44275, .F. ) ;
#224285 = CARTESIAN_POINT ( 'NONE',  ( 12.68104795156995301, 66.60346600605868161, -185.6171677053511928 ) ) ;
#224287 = ORIENTED_EDGE ( 'NONE', *, *, #12259, .F. ) ;
#224288 = CIRCLE ( 'NONE', #36904, 0.09999999999999939493 ) ;
#224290 = ORIENTED_EDGE ( 'NONE', *, *, #47048, .T. ) ;
#224289 = EDGE_LOOP ( 'NONE', ( #169809, #179495, #84077 ) ) ;
#224291 = CARTESIAN_POINT ( 'NONE',  ( -18.41809261886924176, -9.682403314745313239, -107.1568435500914092 ) ) ;
#224293 = ORIENTED_EDGE ( 'NONE', *, *, #225405, .F. ) ;
#224292 = VECTOR ( 'NONE', #82084, 1000.000000000000000 ) ;
#224294 = DIRECTION ( 'NONE',  ( 0.000000000000000000, 0.000000000000000000, -1.000000000000000000 ) ) ;
#224295 = EDGE_CURVE ( 'NONE', #106745, #71546, #138325, .T. ) ;
#224296 = ADVANCED_FACE ( 'NONE', ( #178805 ), #159222, .T. ) ;
#224297 = FACE_OUTER_BOUND ( 'NONE', #86270, .T. ) ;
#224298 = CARTESIAN_POINT ( 'NONE',  ( -18.43634282235120025, 87.08574601666215642, -199.6283932421960685 ) ) ;
#224299 = AXIS2_PLACEMENT_3D ( 'NONE', #131779, #168397, #211326 ) ;
#224300 = VECTOR ( 'NONE', #9172, 1000.000000000000000 ) ;
#224301 = VERTEX_POINT ( 'NONE', #111 ) ;
#224302 = AXIS2_PLACEMENT_3D ( 'NONE', #114969, #75846, #36756 ) ;
#224303 = EDGE_CURVE ( 'NONE', #180800, #31307, #41400, .T. ) ;
#224304 = CARTESIAN_POINT ( 'NONE',  ( 21.10000000000000142, -11.65000000000000036, 11.89999999999999680 ) ) ;
#224306 = VERTEX_POINT ( 'NONE', #241319 ) ;
#224305 = CARTESIAN_POINT ( 'NONE',  ( 18.50000000000002132, 63.58402440245807696, -209.2218768284338637 ) ) ;
#224307 = CARTESIAN_POINT ( 'NONE',  ( -13.40000000000000036, -11.75000000000000000, 12.30000000000000426 ) ) ;
#224309 = ORIENTED_EDGE ( 'NONE', *, *, #173343, .F. ) ;
#224308 = FACE_OUTER_BOUND ( 'NONE', #245881, .T. ) ;
#224310 = VECTOR ( 'NONE', #76152, 1000.000000000000000 ) ;
#224311 = ORIENTED_EDGE ( 'NONE', *, *, #250258, .T. ) ;
#224312 = EDGE_CURVE ( 'NONE', #38886, #22668, #199628, .T. ) ;
#224313 = CARTESIAN_POINT ( 'NONE',  ( 20.94999999999999929, 71.00000000001223555, -148.5283735034374786 ) ) ;
#224314 = EDGE_CURVE ( 'NONE', #58261, #174523, #249674, .T. ) ;
#224315 = ORIENTED_EDGE ( 'NONE', *, *, #79129, .T. ) ;
#224316 = ORIENTED_EDGE ( 'NONE', *, *, #68477, .T. ) ;
#224317 = CARTESIAN_POINT ( 'NONE',  ( -18.50000000000000000, 85.40000000001241176, -163.1410656363516125 ) ) ;
#224318 = DIRECTION ( 'NONE',  ( -2.952720810173289112E-16, -1.000000000000000000, -6.982962677686266711E-15 ) ) ;
#224319 = AXIS2_PLACEMENT_3D ( 'NONE', #56830, #191273, #13898 ) ;
#224321 = ORIENTED_EDGE ( 'NONE', *, *, #206211, .F. ) ;
#224320 = ORIENTED_EDGE ( 'NONE', *, *, #171225, .F. ) ;
#224323 = ORIENTED_EDGE ( 'NONE', *, *, #173023, .T. ) ;
#224322 = CIRCLE ( 'NONE', #145204, 11.90000000000000391 ) ;
#224324 = CARTESIAN_POINT ( 'NONE',  ( -22.50047199488095728, 64.11232401186653362, -247.1837530084900436 ) ) ;
#224325 = EDGE_LOOP ( 'NONE', ( #163811, #7803, #85844 ) ) ;
#224326 = VERTEX_POINT ( 'NONE', #123939 ) ;
#224327 = CARTESIAN_POINT ( 'NONE',  ( -22.39999999999999858, 0.2612980822699374484, -230.0539506776466681 ) ) ;
#224329 = ORIENTED_EDGE ( 'NONE', *, *, #155334, .F. ) ;
#224328 = DIRECTION ( 'NONE',  ( 1.186688945009009831E-16, 0.4088369013363281068, -0.9126074666063770380 ) ) ;
#224330 = ADVANCED_FACE ( 'NONE', ( #109480 ), #5229, .F. ) ;
#224331 = CARTESIAN_POINT ( 'NONE',  ( -20.64999999999999858, 74.00000000001229239, -156.7984855617622770 ) ) ;
#224333 = CARTESIAN_POINT ( 'NONE',  ( 18.54147908293623459, -9.463261657916778091, -107.5489488967560305 ) ) ;
#224332 = DIRECTION ( 'NONE',  ( 0.000000000000000000, 0.000000000000000000, -1.000000000000000000 ) ) ;
#224334 = CARTESIAN_POINT ( 'NONE',  ( 18.40000000000000213, 85.51932773110506503, -196.5501311079649724 ) ) ;
#224335 = EDGE_LOOP ( 'NONE', ( #3088, #124646, #182241, #244736 ) ) ;
#224336 = ORIENTED_EDGE ( 'NONE', *, *, #219239, .F. ) ;
#224337 = EDGE_CURVE ( 'NONE', #106564, #224045, #46932, .T. ) ;
#224338 = DIRECTION ( 'NONE',  ( -1.000000000000000000, 0.000000000000000000, -0.000000000000000000 ) ) ;
#224339 = LINE ( 'NONE', #204765, #186922 ) ;
#224340 = AXIS2_PLACEMENT_3D ( 'NONE', #37853, #54807, #20860 ) ;
#224341 = ORIENTED_EDGE ( 'NONE', *, *, #177141, .T. ) ;
#224342 = AXIS2_PLACEMENT_3D ( 'NONE', #200316, #24265, #179489 ) ;
#224343 = DIRECTION ( 'NONE',  ( 0.000000000000000000, -0.8814952561688423893, 0.4721928772777359007 ) ) ;
#224344 = VERTEX_POINT ( 'NONE', #108220 ) ;
#224345 = ORIENTED_EDGE ( 'NONE', *, *, #5801, .T. ) ;
#224346 = CARTESIAN_POINT ( 'NONE',  ( 23.25000000000000000, 28.50120599808395028, -258.2149742250584268 ) ) ;
#224347 = EDGE_CURVE ( 'NONE', #206635, #181531, #104334, .T. ) ;
#224348 = ORIENTED_EDGE ( 'NONE', *, *, #82167, .T. ) ;
#224349 = CARTESIAN_POINT ( 'NONE',  ( -21.05000000000000426, 11.75000000001115374, -107.2838656629781866 ) ) ;
#224350 = CARTESIAN_POINT ( 'NONE',  ( -22.39999999999999858, 68.20922040163927136, -203.5231074845243882 ) ) ;
#224351 = ORIENTED_EDGE ( 'NONE', *, *, #203394, .F. ) ;
#224352 = CARTESIAN_POINT ( 'NONE',  ( 20.04142135623731136, 64.25000000001220712, -145.3731074845244109 ) ) ;
#224353 = DIRECTION ( 'NONE',  ( -1.000000000000000000, 0.000000000000000000, 0.000000000000000000 ) ) ;
#224355 = CARTESIAN_POINT ( 'NONE',  ( 20.94999999999999929, 70.10000000001177511, -79.74220724918072278 ) ) ;
#224354 = CARTESIAN_POINT ( 'NONE',  ( 21.10000000000000142, 6.322468214605804882, 12.11686199900910310 ) ) ;
#224356 = DIRECTION ( 'NONE',  ( 0.000000000000000000, 0.000000000000000000, 1.000000000000000000 ) ) ;
#224358 = AXIS2_PLACEMENT_3D ( 'NONE', #65675, #6985, #69552 ) ;
#224357 = DIRECTION ( 'NONE',  ( 1.000000000000000000, 0.000000000000000000, 0.000000000000000000 ) ) ;
#224359 = CIRCLE ( 'NONE', #82672, 0.09999999999999939493 ) ;
#224360 = CARTESIAN_POINT ( 'NONE',  ( -20.94999999999999929, -1.164121893230052995, -175.4148480855716059 ) ) ;
#224361 = CARTESIAN_POINT ( 'NONE',  ( -20.64999999999999858, 76.00000000001192291, -104.9231074845242944 ) ) ;
#224362 = VECTOR ( 'NONE', #182939, 1000.000000000000000 ) ;
#224363 = ORIENTED_EDGE ( 'NONE', *, *, #72564, .T. ) ;
#224364 = ADVANCED_FACE ( 'NONE', ( #24857 ), #74753, .T. ) ;
#224366 = ORIENTED_EDGE ( 'NONE', *, *, #7693, .T. ) ;
#224365 = ORIENTED_EDGE ( 'NONE', *, *, #210536, .T. ) ;
#224367 = ORIENTED_EDGE ( 'NONE', *, *, #194805, .T. ) ;
#224368 = DIRECTION ( 'NONE',  ( 1.000000000000000000, -7.304098846218134667E-16, -4.217023435051625732E-16 ) ) ;
#224369 = CARTESIAN_POINT ( 'NONE',  ( -16.86733706339143524, 66.03400947037214053, -82.11999218252567800 ) ) ;
#224371 = CARTESIAN_POINT ( 'NONE',  ( -15.15766958671843412, 9.410538608528867144, -15.43268799714089035 ) ) ;
#224370 = FACE_OUTER_BOUND ( 'NONE', #42770, .T. ) ;
#224372 = DIRECTION ( 'NONE',  ( 0.000000000000000000, 0.000000000000000000, -1.000000000000000000 ) ) ;
#224373 = ORIENTED_EDGE ( 'NONE', *, *, #183603, .T. ) ;
#224374 = VECTOR ( 'NONE', #80476, 1000.000000000000000 ) ;
#224375 = DIRECTION ( 'NONE',  ( 1.000000000000000000, 0.000000000000000000, 0.000000000000000000 ) ) ;
#224376 = CARTESIAN_POINT ( 'NONE',  ( 20.94999999999999929, 67.23127455305835554, -235.8551265064784559 ) ) ;
#224377 = CARTESIAN_POINT ( 'NONE',  ( 20.85000000000000142, 80.78317333349157536, -192.9003134612048882 ) ) ;
#224378 = VERTEX_POINT ( 'NONE', #69104 ) ;
#224379 = CARTESIAN_POINT ( 'NONE',  ( 18.49505832270840955, -9.438028062782890970, -7.198473174893858406 ) ) ;
#224380 = DIRECTION ( 'NONE',  ( 0.000000000000000000, 0.2128009952263604232, -0.9770955615653316162 ) ) ;
#224381 = ORIENTED_EDGE ( 'NONE', *, *, #256300, .T. ) ;
#224382 = ORIENTED_EDGE ( 'NONE', *, *, #222051, .F. ) ;
#224383 = CARTESIAN_POINT ( 'NONE',  ( -16.88560720703333473, 66.04943515626187889, -56.87499556366067566 ) ) ;
#224384 = CARTESIAN_POINT ( 'NONE',  ( -21.05000000000000071, 46.45388641681647357, -243.1520440498138385 ) ) ;
#224385 = CARTESIAN_POINT ( 'NONE',  ( -20.54999999999999716, 2.000000000011154189, -80.22462192276213955 ) ) ;
#224386 = CARTESIAN_POINT ( 'NONE',  ( 20.95159278453404283, 67.09210366206254150, -61.03838729941513463 ) ) ;
#224387 = DIRECTION ( 'NONE',  ( 1.000000000000000000, -2.952720810173289112E-16, -2.061873921506763405E-30 ) ) ;
#224388 = ORIENTED_EDGE ( 'NONE', *, *, #211764, .F. ) ;
#224389 = CARTESIAN_POINT ( 'NONE',  ( 18.49999999999999645, 74.36282728704190959, -158.4409541190523498 ) ) ;
#224390 = FACE_OUTER_BOUND ( 'NONE', #155712, .T. ) ;
#224391 = CARTESIAN_POINT ( 'NONE',  ( -21.14999999999999858, 1.115526128501326264E-11, -60.45934304829881256 ) ) ;
#224393 = CARTESIAN_POINT ( 'NONE',  ( 26.01805557925458956, 8.624264858734573380, 33.00000000000000000 ) ) ;
#224392 = DIRECTION ( 'NONE',  ( 0.000000000000000000, 0.000000000000000000, 1.000000000000000000 ) ) ;
#224395 = EDGE_CURVE ( 'NONE', #248044, #191668, #108032, .T. ) ;
#224394 = DIRECTION ( 'NONE',  ( 1.000000000000000000, 0.000000000000000000, 0.000000000000000000 ) ) ;
#224396 = DIRECTION ( 'NONE',  ( -0.000000000000000000, 0.000000000000000000, 1.000000000000000000 ) ) ;
#224397 = AXIS2_PLACEMENT_3D ( 'NONE', #100341, #143341, #179926 ) ;
#224398 = AXIS2_PLACEMENT_3D ( 'NONE', #80976, #117550, #103104 ) ;
#224399 = LINE ( 'NONE', #7945, #164425 ) ;
#224400 = CARTESIAN_POINT ( 'NONE',  ( 22.39999999999999503, 64.25000000001165290, -69.62310748452439668 ) ) ;
#224401 = VECTOR ( 'NONE', #124395, 1000.000000000000000 ) ;
#224402 = CIRCLE ( 'NONE', #111994, 0.1000000000000008937 ) ;
#224404 = EDGE_LOOP ( 'NONE', ( #38736, #109997, #118792, #34331 ) ) ;
#224403 = CARTESIAN_POINT ( 'NONE',  ( -18.40000000000000213, 23.69729366125098480, -229.5924034189314966 ) ) ;
#224405 = AXIS2_PLACEMENT_3D ( 'NONE', #51202, #130768, #250712 ) ;
#224406 = ADVANCED_FACE ( 'NONE', ( #84756 ), #44402, .F. ) ;
#224407 = DIRECTION ( 'NONE',  ( 0.000000000000000000, 1.000000000000000000, 0.000000000000000000 ) ) ;
#224408 = ADVANCED_FACE ( 'NONE', ( #166941 ), #147335, .F. ) ;
#224409 = AXIS2_PLACEMENT_3D ( 'NONE', #125522, #145071, #5549 ) ;
#224410 = AXIS2_PLACEMENT_3D ( 'NONE', #6606, #167012, #86114 ) ;
#224412 = CIRCLE ( 'NONE', #149435, 0.1000000000000028644 ) ;
#224411 = CARTESIAN_POINT ( 'NONE',  ( -23.15000000000000213, 11.15983666280819975, -246.1019239270423213 ) ) ;
#224413 = FACE_OUTER_BOUND ( 'NONE', #190974, .T. ) ;
#224414 = EDGE_CURVE ( 'NONE', #135192, #3158, #112313, .T. ) ;
#224415 = EDGE_LOOP ( 'NONE', ( #242009, #5307, #101083, #171114 ) ) ;
#224416 = AXIS2_PLACEMENT_3D ( 'NONE', #12392, #129745, #188429 ) ;
#224417 = CARTESIAN_POINT ( 'NONE',  ( -20.54999999999999716, 4.350000000011156054, -184.2499999999999716 ) ) ;
#224418 = DIRECTION ( 'NONE',  ( 0.000000000000000000, 0.9910465087640866200, -0.1335171055202867274 ) ) ;
#224419 = CARTESIAN_POINT ( 'NONE',  ( -20.54999999999999716, 4.350000000011156054, -188.6499999999999488 ) ) ;
#224420 = EDGE_CURVE ( 'NONE', #217322, #145739, #208172, .T. ) ;
#224422 = ORIENTED_EDGE ( 'NONE', *, *, #49569, .F. ) ;
#224421 = EDGE_CURVE ( 'NONE', #48432, #255690, #204048, .T. ) ;
#224423 = PLANE ( 'NONE',  #141206 ) ;
#224425 = ORIENTED_EDGE ( 'NONE', *, *, #135832, .T. ) ;
#224424 = CARTESIAN_POINT ( 'NONE',  ( -16.80891096016325292, 9.950000000011137047, -188.3676628072681183 ) ) ;
#224427 = CARTESIAN_POINT ( 'NONE',  ( 18.49999999999999645, 74.16465844978819177, -191.9679561919613775 ) ) ;
#224426 = CARTESIAN_POINT ( 'NONE',  ( -20.85000000000000142, 1.115600667400684642E-11, -100.5000000000000426 ) ) ;
#224428 = EDGE_CURVE ( 'NONE', #127391, #159618, #183900, .T. ) ;
#224429 = FACE_OUTER_BOUND ( 'NONE', #24549, .T. ) ;
#224430 = VERTEX_POINT ( 'NONE', #89919 ) ;
#224431 = DIRECTION ( 'NONE',  ( -6.938893903907222856E-15, -1.000000000000000000, -7.272083257015735086E-15 ) ) ;
#224432 = DIRECTION ( 'NONE',  ( 0.000000000000000000, 0.000000000000000000, 1.000000000000000000 ) ) ;
#224433 = DIRECTION ( 'NONE',  ( 1.000000000000000000, -0.000000000000000000, -0.000000000000000000 ) ) ;
#224434 = CARTESIAN_POINT ( 'NONE',  ( 21.04999999999999716, 67.12872031401643369, -127.9644784893834100 ) ) ;
#224436 = EDGE_CURVE ( 'NONE', #139087, #201117, #166491, .T. ) ;
#224435 = DIRECTION ( 'NONE',  ( 1.734723475976817507E-14, -6.982962677686266711E-15, 1.000000000000000000 ) ) ;
#224437 = VERTEX_POINT ( 'NONE', #148640 ) ;
#224438 = CARTESIAN_POINT ( 'NONE',  ( 23.14999999999999858, 5.000000000011153745, -88.09473398108696074 ) ) ;
#224439 = AXIS2_PLACEMENT_3D ( 'NONE', #81884, #101434, #139306 ) ;
#224440 = CIRCLE ( 'NONE', #82941, 0.1999999999999987899 ) ;
#224441 = CARTESIAN_POINT ( 'NONE',  ( -23.39999999999994529, 74.14873292176677921, -47.62635315998165453 ) ) ;
#224442 = DIRECTION ( 'NONE',  ( -1.000000000000000000, -0.000000000000000000, -0.000000000000000000 ) ) ;
#224443 = VERTEX_POINT ( 'NONE', #129066 ) ;
#224444 = AXIS2_PLACEMENT_3D ( 'NONE', #185558, #201260, #4337 ) ;
#224445 = ORIENTED_EDGE ( 'NONE', *, *, #229048, .T. ) ;
#224446 = DIRECTION ( 'NONE',  ( 0.000000000000000000, 0.000000000000000000, -1.000000000000000000 ) ) ;
#224447 = EDGE_CURVE ( 'NONE', #193670, #61689, #208615, .T. ) ;
#224448 = CARTESIAN_POINT ( 'NONE',  ( -23.15000000000000213, 71.65000000001253966, -182.3731074845244109 ) ) ;
#224449 = CARTESIAN_POINT ( 'NONE',  ( -20.94999999999999929, 74.14897176987119565, -124.8691942151018139 ) ) ;
#224450 = CARTESIAN_POINT ( 'NONE',  ( 21.05000000000000071, 10.72371710471868056, -141.6649135690876449 ) ) ;
#224451 = DIRECTION ( 'NONE',  ( 0.000000000000000000, -0.4721928772777813088, -0.8814952561688180754 ) ) ;
#224453 = CARTESIAN_POINT ( 'NONE',  ( -23.39999999999994529, 64.35000000001120668, -51.02310748452479316 ) ) ;
#224452 = CARTESIAN_POINT ( 'NONE',  ( -20.94999999999999929, 5.850000000011105428, -77.13249722427802624 ) ) ;
#224454 = TOROIDAL_SURFACE ( 'NONE', #136371, 11.70000000000000462, 0.1000000000000000056 ) ;
#224456 = CARTESIAN_POINT ( 'NONE',  ( 23.14999999999999858, 76.00000000001213607, -136.5231074845243313 ) ) ;
#224455 = CIRCLE ( 'NONE', #228577, 0.1000000000000002554 ) ;
#224457 = DIRECTION ( 'NONE',  ( -0.000000000000000000, 0.000000000000000000, 1.000000000000000000 ) ) ;
#224458 = FACE_OUTER_BOUND ( 'NONE', #31594, .T. ) ;
#224459 = CARTESIAN_POINT ( 'NONE',  ( -20.54999999999999716, -8.999999999988844479, -57.10603087734755690 ) ) ;
#224461 = ORIENTED_EDGE ( 'NONE', *, *, #105016, .F. ) ;
#224460 = CARTESIAN_POINT ( 'NONE',  ( 20.94999999999999929, 14.05000000001115623, -128.4863049292391395 ) ) ;
#224462 = DIRECTION ( 'NONE',  ( 0.7071067811865486830, 0.1850873201762206766, 0.6824534298470361637 ) ) ;
#224464 = DIRECTION ( 'NONE',  ( 1.000000000000000000, -0.000000000000000000, -0.000000000000000000 ) ) ;
#224463 = CARTESIAN_POINT ( 'NONE',  ( 22.47007471830798053, 76.00000000001200817, -110.7438181364507699 ) ) ;
#224465 = EDGE_CURVE ( 'NONE', #85043, #61130, #133150, .T. ) ;
#224466 = EDGE_LOOP ( 'NONE', ( #241562, #22903, #77066, #140978 ) ) ;
#224467 = DIRECTION ( 'NONE',  ( 1.000000000000000000, 0.000000000000000000, -0.000000000000000000 ) ) ;
#224468 = CARTESIAN_POINT ( 'NONE',  ( -21.44999999999999929, 7.350000000011155166, -155.2500000000000284 ) ) ;
#224469 = CARTESIAN_POINT ( 'NONE',  ( 20.99999999999997868, 67.23127455305841238, -235.8551265064783991 ) ) ;
#224470 = CARTESIAN_POINT ( 'NONE',  ( -20.64999999999999858, 74.00000000001180922, -82.24772940728641402 ) ) ;
#224471 = CARTESIAN_POINT ( 'NONE',  ( -23.25000000000000000, 1.115600667400684642E-11, -200.9999999999999432 ) ) ;
#224472 = ORIENTED_EDGE ( 'NONE', *, *, #51733, .T. ) ;
#224473 = TOROIDAL_SURFACE ( 'NONE', #157894, 0.2000000000000000111, 0.1000000000000000056 ) ;
#224474 = AXIS2_PLACEMENT_3D ( 'NONE', #255213, #110624, #12833 ) ;
#224475 = VERTEX_POINT ( 'NONE', #65226 ) ;
#224476 = DIRECTION ( 'NONE',  ( 0.000000000000000000, -6.982962677686266711E-15, 1.000000000000000000 ) ) ;
#224477 = AXIS2_PLACEMENT_3D ( 'NONE', #119660, #81762, #180908 ) ;
#224478 = ORIENTED_EDGE ( 'NONE', *, *, #236536, .F. ) ;
#224479 = DIRECTION ( 'NONE',  ( 0.000000000000000000, 0.2128009952263601456, -0.9770955615653316162 ) ) ;
#224480 = ORIENTED_EDGE ( 'NONE', *, *, #186029, .F. ) ;
#224481 = ADVANCED_FACE ( 'NONE', ( #144749 ), #154046, .T. ) ;
#224482 = AXIS2_PLACEMENT_3D ( 'NONE', #135530, #18168, #80686 ) ;
#224483 = CARTESIAN_POINT ( 'NONE',  ( 19.97071067811864609, 11.72071067811865674, -24.75000000000000000 ) ) ;
#224484 = CIRCLE ( 'NONE', #87099, 0.09999999999999134581 ) ;
#224486 = VECTOR ( 'NONE', #192951, 1000.000000000000000 ) ;
#224485 = DIRECTION ( 'NONE',  ( 1.000000000000000000, 0.000000000000000000, 0.000000000000000000 ) ) ;
#224487 = CIRCLE ( 'NONE', #20312, 0.1000000000000017958 ) ;
#224488 =( BOUNDED_SURFACE ( )  B_SPLINE_SURFACE ( 3, 2, ( 
 ( #27451, #69118, #249037 ),
 ( #251585, #72984, #228181 ),
 ( #230758, #190350, #109494 ),
 ( #189049, #70422, #229464 ) ),
 .UNSPECIFIED., .F., .F., .F. ) 
 B_SPLINE_SURFACE_WITH_KNOTS ( ( 4, 4 ),
 ( 3, 3 ),
 ( 0.0008258556059633768206, 0.0009616864997632988948 ),
 ( 0.000000000000000000, 1.000000000000000000 ),
 .UNSPECIFIED. ) 
 GEOMETRIC_REPRESENTATION_ITEM ( )  RATIONAL_B_SPLINE_SURFACE ( (
 ( 1.000000000000000000, 0.9152888060719485130, 1.000000000000000000),
 ( 1.000000000000000000, 0.9327727094137853170, 1.000000000000000000),
 ( 1.000000000000000000, 0.9369023509258459503, 1.000000000000000000),
 ( 1.000000000000000000, 0.9246339933864583527, 1.000000000000000000) ) ) 
 REPRESENTATION_ITEM ( '' )  SURFACE ( )  );
#224489 = CARTESIAN_POINT ( 'NONE',  ( -18.50000000000000000, 9.250000000011157297, -155.2500000000000284 ) ) ;
#224490 = VERTEX_POINT ( 'NONE', #211166 ) ;
#224491 = CIRCLE ( 'NONE', #7850, 0.8750000000000007772 ) ;
#224492 = ADVANCED_FACE ( 'NONE', ( #75527 ), #50780, .T. ) ;
#224493 = CARTESIAN_POINT ( 'NONE',  ( -20.94999999999999929, 42.96960653111219131, -254.4772109693542745 ) ) ;
#224494 = CARTESIAN_POINT ( 'NONE',  ( 21.95218792049437795, 68.79849243876547860, -136.6221359243242546 ) ) ;
#224495 = CARTESIAN_POINT ( 'NONE',  ( 20.94560253601876809, 11.75000000001115907, -160.5100835125150809 ) ) ;
#224496 = ADVANCED_FACE ( 'NONE', ( #149930 ), #132926, .T. ) ;
#224497 = CARTESIAN_POINT ( 'NONE',  ( -16.80939487329394666, 30.20632856012771583, -234.8070450048004716 ) ) ;
#224498 = EDGE_CURVE ( 'NONE', #74752, #158778, #71676, .T. ) ;
#224499 = CYLINDRICAL_SURFACE ( 'NONE', #68614, 0.09999999999998898659 ) ;
#224500 = DIRECTION ( 'NONE',  ( 0.000000000000000000, -0.008583690987135041833, 0.9999631594459055250 ) ) ;
#224501 = CARTESIAN_POINT ( 'NONE',  ( 21.11747605621531321, 11.18329185709994888, -211.0959905261389338 ) ) ;
#224502 = EDGE_LOOP ( 'NONE', ( #200088, #195666, #147355, #225553 ) ) ;
#224505 = EDGE_CURVE ( 'NONE', #197295, #255597, #12365, .T. ) ;
#224504 = DIRECTION ( 'NONE',  ( 1.000000000000000000, 0.000000000000000000, 0.000000000000000000 ) ) ;
#224503 = CARTESIAN_POINT ( 'NONE',  ( -20.64999999999999858, 85.40000000001158753, -59.62913836187181715 ) ) ;
#224506 = AXIS2_PLACEMENT_3D ( 'NONE', #57999, #81400, #176705 ) ;
#224507 = ORIENTED_EDGE ( 'NONE', *, *, #11192, .F. ) ;
#224509 = VERTEX_POINT ( 'NONE', #112084 ) ;
#224508 = DIRECTION ( 'NONE',  ( 1.000000000000000000, 0.000000000000000000, 0.000000000000000000 ) ) ;
#224510 = EDGE_LOOP ( 'NONE', ( #246230, #255025, #230957 ) ) ;
#224511 = DIRECTION ( 'NONE',  ( 0.000000000000000000, 0.000000000000000000, -1.000000000000000000 ) ) ;
#224512 = CARTESIAN_POINT ( 'NONE',  ( 18.49999999999999289, 10.29270135741298731, -72.45736188715193293 ) ) ;
#224513 = CARTESIAN_POINT ( 'NONE',  ( -23.15000000000000213, 76.00000000001213607, -136.5231074845242745 ) ) ;
#224514 = EDGE_CURVE ( 'NONE', #167246, #201908, #99788, .T. ) ;
#224515 = FACE_OUTER_BOUND ( 'NONE', #72572, .T. ) ;
#224516 = ORIENTED_EDGE ( 'NONE', *, *, #94170, .T. ) ;
#224517 = PLANE ( 'NONE',  #138817 ) ;
#224518 = CARTESIAN_POINT ( 'NONE',  ( 22.50000000000000000, 7.790779598384538929, -66.90000000000004832 ) ) ;
#224519 = CIRCLE ( 'NONE', #57898, 11.69999999999998863 ) ;
#224520 = ORIENTED_EDGE ( 'NONE', *, *, #210203, .T. ) ;
#224521 = CIRCLE ( 'NONE', #216319, 0.1000000000000052097 ) ;
#224522 = FACE_OUTER_BOUND ( 'NONE', #19123, .T. ) ;
#224523 = AXIS2_PLACEMENT_3D ( 'NONE', #238269, #157503, #76635 ) ;
#224524 = DIRECTION ( 'NONE',  ( 0.000000000000000000, -0.4930308989875165082, -0.8700118002898358238 ) ) ;
#224525 = ORIENTED_EDGE ( 'NONE', *, *, #242309, .F. ) ;
#224526 = CARTESIAN_POINT ( 'NONE',  ( -16.77180007708460252, 9.950000000011137047, -146.6356141189548339 ) ) ;
#224527 = AXIS2_PLACEMENT_3D ( 'NONE', #222107, #124329, #246828 ) ;
#224528 = ADVANCED_FACE ( 'NONE', ( #152508 ), #194191, .F. ) ;
#224529 = ORIENTED_EDGE ( 'NONE', *, *, #179176, .F. ) ;
#224530 = VERTEX_POINT ( 'NONE', #212465 ) ;
#224531 = DIRECTION ( 'NONE',  ( 1.000000000000000000, 0.000000000000000000, 0.000000000000000000 ) ) ;
#224532 = ADVANCED_FACE ( 'NONE', ( #16834 ), #254125, .F. ) ;
#224533 = CYLINDRICAL_SURFACE ( 'NONE', #206470, 4.049999999999998934 ) ;
#224534 = DIRECTION ( 'NONE',  ( 1.000000000000000000, -1.207181226542539700E-16, 2.694675058168174199E-16 ) ) ;
#224535 = EDGE_CURVE ( 'NONE', #85650, #155390, #249027, .T. ) ;
#224536 = LINE ( 'NONE', #125453, #249298 ) ;
#224537 = VECTOR ( 'NONE', #151526, 1000.000000000000000 ) ;
#224538 = DIRECTION ( 'NONE',  ( -1.000000000000000000, -0.000000000000000000, -0.000000000000000000 ) ) ;
#224539 = FACE_OUTER_BOUND ( 'NONE', #132464, .T. ) ;
#224541 = DIRECTION ( 'NONE',  ( 0.000000000000000000, 0.2617529984165031243, 0.9651348961777157509 ) ) ;
#224540 = AXIS2_PLACEMENT_3D ( 'NONE', #138565, #61635, #198567 ) ;
#224542 = ORIENTED_EDGE ( 'NONE', *, *, #39688, .F. ) ;
#224544 = DIRECTION ( 'NONE',  ( 0.000000000000000000, 0.8660254037844309360, -0.5000000000000134337 ) ) ;
#224543 = DIRECTION ( 'NONE',  ( 0.000000000000000000, -0.2606175937107792495, 0.9654421110809303652 ) ) ;
#224545 = DIRECTION ( 'NONE',  ( 0.000000000000000000, 0.2617529984164915779, 0.9651348961777189706 ) ) ;
#224546 = SPHERICAL_SURFACE ( 'NONE', #222643, 0.1000000000000000056 ) ;
#224547 = CARTESIAN_POINT ( 'NONE',  ( -23.25000000000000000, 11.65000000001115588, -134.0000000000000000 ) ) ;
#224548 = ORIENTED_EDGE ( 'NONE', *, *, #100641, .F. ) ;
#224550 = ORIENTED_EDGE ( 'NONE', *, *, #34144, .F. ) ;
#224549 = DIRECTION ( 'NONE',  ( -2.952720810173289112E-16, -0.9651348961777157509, 0.2617529984165031243 ) ) ;
#224551 = LINE ( 'NONE', #244113, #18773 ) ;
#224553 = LINE ( 'NONE', #6798, #200644 ) ;
#224552 =( BOUNDED_CURVE ( )  B_SPLINE_CURVE ( 3, ( #28318, #149537, #107813, #170413 ),
 .UNSPECIFIED., .F., .F. ) 
 B_SPLINE_CURVE_WITH_KNOTS ( ( 4, 4 ),
 ( 4.712388980384689674, 6.231880751915386263 ),
 .UNSPECIFIED. ) 
 CURVE ( )  GEOMETRIC_REPRESENTATION_ITEM ( )  RATIONAL_B_SPLINE_CURVE ( ( 1.000000000000000000, 0.8166740347213228279, 0.8166740347213228279, 1.000000000000000000 ) ) 
 REPRESENTATION_ITEM ( '' )  );
#224554 = LINE ( 'NONE', #30231, #213650 ) ;
#224557 = EDGE_CURVE ( 'NONE', #218583, #59445, #174662, .T. ) ;
#224556 = ORIENTED_EDGE ( 'NONE', *, *, #163805, .T. ) ;
#224555 = CARTESIAN_POINT ( 'NONE',  ( 21.06277459767450111, 67.12713756174402135, -157.8191082921680675 ) ) ;
#224558 = AXIS2_PLACEMENT_3D ( 'NONE', #247613, #43004, #102946 ) ;
#224559 = CYLINDRICAL_SURFACE ( 'NONE', #155877, 0.1000000000000064587 ) ;
#224560 = DIRECTION ( 'NONE',  ( 1.186688945009010077E-16, -1.000000000000000000, -0.000000000000000000 ) ) ;
#224561 = ORIENTED_EDGE ( 'NONE', *, *, #192727, .F. ) ;
#224562 = ORIENTED_EDGE ( 'NONE', *, *, #250120, .F. ) ;
#224563 = CARTESIAN_POINT ( 'NONE',  ( 20.99999999999999645, 66.25000000001230660, -157.3731074845244393 ) ) ;
#224564 = CARTESIAN_POINT ( 'NONE',  ( -20.54999999999999716, -8.999999999988844479, -191.1060308773475356 ) ) ;
#224565 = ORIENTED_EDGE ( 'NONE', *, *, #256324, .T. ) ;
#224566 = DIRECTION ( 'NONE',  ( 0.000000000000000000, 1.000000000000000000, 6.982962677686266711E-15 ) ) ;
#224567 = ADVANCED_FACE ( 'NONE', ( #229450 ), #72972, .F. ) ;
#224568 = DIRECTION ( 'NONE',  ( 0.000000000000000000, -1.000000000000000000, 0.000000000000000000 ) ) ;
#224569 = CIRCLE ( 'NONE', #257845, 0.09999999999999939493 ) ;
#224570 = AXIS2_PLACEMENT_3D ( 'NONE', #123989, #164394, #144802 ) ;
#224571 = ADVANCED_FACE ( 'NONE', ( #192895 ), #220644, .F. ) ;
#224572 = EDGE_LOOP ( 'NONE', ( #164526, #49328, #57454, #49837, #147917, #90200, #245917, #3177, #118506, #138917, #2056 ) ) ;
#224573 = VECTOR ( 'NONE', #202977, 1000.000000000000000 ) ;
#224574 = CIRCLE ( 'NONE', #112194, 0.09999999999998712696 ) ;
#224575 = CARTESIAN_POINT ( 'NONE',  ( -16.88328101497759448, 66.04964716579266337, -48.67192796959511725 ) ) ;
#224576 =( BOUNDED_CURVE ( )  B_SPLINE_CURVE ( 3, ( #91524, #8138, #90209, #171104 ),
 .UNSPECIFIED., .F., .F. ) 
 B_SPLINE_CURVE_WITH_KNOTS ( ( 4, 4 ),
 ( 3.432212674861198742, 3.693332928900582957 ),
 .UNSPECIFIED. ) 
 CURVE ( )  GEOMETRIC_REPRESENTATION_ITEM ( )  RATIONAL_B_SPLINE_CURVE ( ( 1.000000000000000000, 0.9943260843901261525, 0.9943260843901261525, 1.000000000000000000 ) ) 
 REPRESENTATION_ITEM ( '' )  );
#224577 = ADVANCED_FACE ( 'NONE', ( #153816 ), #233137, .F. ) ;
#224578 = ORIENTED_EDGE ( 'NONE', *, *, #28237, .T. ) ;
#224579 = AXIS2_PLACEMENT_3D ( 'NONE', #33010, #246855, #112508 ) ;
#224580 = VERTEX_POINT ( 'NONE', #70411 ) ;
#224582 = EDGE_CURVE ( 'NONE', #141490, #177470, #185986, .T. ) ;
#224581 = CARTESIAN_POINT ( 'NONE',  ( -21.09107601085561257, 61.07898507579771064, -234.2272990812096225 ) ) ;
#224583 = VERTEX_POINT ( 'NONE', #250291 ) ;
#224584 = CARTESIAN_POINT ( 'NONE',  ( 20.85000000000000142, 77.83585931145526615, -58.01866831572577610 ) ) ;
#224585 = ORIENTED_EDGE ( 'NONE', *, *, #163858, .T. ) ;
#224587 = ORIENTED_EDGE ( 'NONE', *, *, #98664, .T. ) ;
#224586 = CARTESIAN_POINT ( 'NONE',  ( -18.39999999999999858, 40.47920047438133651, -235.2678785906695396 ) ) ;
#224588 = CARTESIAN_POINT ( 'NONE',  ( -21.14999999999999858, 1.363275264940686293, -230.6442496871288483 ) ) ;
#224589 = VERTEX_POINT ( 'NONE', #200584 ) ;
#224590 = DIRECTION ( 'NONE',  ( 0.000000000000000000, -6.467318590049456648E-15, 1.000000000000000000 ) ) ;
#224591 = VECTOR ( 'NONE', #182308, 1000.000000000000000 ) ;
#224592 = AXIS2_PLACEMENT_3D ( 'NONE', #98984, #100277, #140710 ) ;
#224593 = ORIENTED_EDGE ( 'NONE', *, *, #150151, .F. ) ;
#224595 = ORIENTED_EDGE ( 'NONE', *, *, #225628, .T. ) ;
#224594 = VERTEX_POINT ( 'NONE', #139304 ) ;
#224597 = DIRECTION ( 'NONE',  ( -1.000000000000000000, 0.000000000000000000, 0.000000000000000000 ) ) ;
#224596 = AXIS2_PLACEMENT_3D ( 'NONE', #61951, #64515, #205290 ) ;
#224598 = FACE_OUTER_BOUND ( 'NONE', #207416, .T. ) ;
#224599 = VERTEX_POINT ( 'NONE', #21964 ) ;
#224601 = EDGE_CURVE ( 'NONE', #253988, #53312, #20742, .T. ) ;
#224600 = CIRCLE ( 'NONE', #178865, 0.09999999999998802902 ) ;
#224602 = EDGE_CURVE ( 'NONE', #258063, #74293, #237212, .T. ) ;
#224603 = ORIENTED_EDGE ( 'NONE', *, *, #67104, .F. ) ;
#224604 = DIRECTION ( 'NONE',  ( 0.000000000000000000, 0.000000000000000000, 1.000000000000000000 ) ) ;
#224605 = DIRECTION ( 'NONE',  ( 0.000000000000000000, 0.000000000000000000, -1.000000000000000000 ) ) ;
#224607 = VERTEX_POINT ( 'NONE', #201869 ) ;
#224606 = CARTESIAN_POINT ( 'NONE',  ( -23.15000000000000213, 25.94586868676353575, -241.5435999122864530 ) ) ;
#224608 = CARTESIAN_POINT ( 'NONE',  ( -18.50000000000000000, 7.021664781900089913, -37.33356540189728889 ) ) ;
#224609 = ORIENTED_EDGE ( 'NONE', *, *, #64441, .T. ) ;
#224610 = DIRECTION ( 'NONE',  ( 0.000000000000000000, -0.2617529984165152257, -0.9651348961777124202 ) ) ;
#224611 = CARTESIAN_POINT ( 'NONE',  ( 18.49999999999999289, 65.74999999739293344, -111.8359355348920872 ) ) ;
#224612 = ORIENTED_EDGE ( 'NONE', *, *, #97318, .F. ) ;
#224614 = ADVANCED_FACE ( 'NONE', ( #41541 ), #76781, .F. ) ;
#224613 = DIRECTION ( 'NONE',  ( 3.616040088954497272E-32, -1.224646799147352961E-16, 1.000000000000000000 ) ) ;
#224615 = CARTESIAN_POINT ( 'NONE',  ( -20.94999999999999929, 1.115600667400684642E-11, -167.5000000000000284 ) ) ;
#224616 = ORIENTED_EDGE ( 'NONE', *, *, #177503, .F. ) ;
#224617 = EDGE_CURVE ( 'NONE', #151638, #27482, #19389, .T. ) ;
#224618 = DIRECTION ( 'NONE',  ( 1.000000000000000000, 0.000000000000000000, 0.000000000000000000 ) ) ;
#224619 = VERTEX_POINT ( 'NONE', #255366 ) ;
#224620 = TOROIDAL_SURFACE ( 'NONE', #137314, 0.2000000000000000111, 0.1000000000000000056 ) ;
#224622 = VERTEX_POINT ( 'NONE', #179752 ) ;
#224621 = VERTEX_POINT ( 'NONE', #23264 ) ;
#224623 = VERTEX_POINT ( 'NONE', #38962 ) ;
#224624 = CARTESIAN_POINT ( 'NONE',  ( -18.39999999999999858, -9.599999999988845900, -107.2001893912220964 ) ) ;
#224625 = ORIENTED_EDGE ( 'NONE', *, *, #254006, .F. ) ;
#224626 = CARTESIAN_POINT ( 'NONE',  ( -16.93388492042257454, 66.01145817749561218, -48.62256236133821830 ) ) ;
#224627 = AXIS2_PLACEMENT_3D ( 'NONE', #84836, #64029, #45746 ) ;
#224629 = EDGE_LOOP ( 'NONE', ( #153646, #219741, #242776, #46397 ) ) ;
#224628 = B_SPLINE_CURVE_WITH_KNOTS ( 'NONE', 3,
 ( #99211, #56237, #41855, #116249, #157973, #240040, #256971, #61392 ),
 .UNSPECIFIED., .F., .F.,
 ( 4, 2, 2, 4 ),
 ( 0.000000000000000000, 0.0002114466876442291910, 0.0003171700314663174268, 0.0004228933752884056355 ),
 .UNSPECIFIED. ) ;
#224630 = EDGE_CURVE ( 'NONE', #91491, #45068, #58294, .T. ) ;
#224631 = CARTESIAN_POINT ( 'NONE',  ( -16.94107738177414291, 65.98576071487489969, -48.57310748452439952 ) ) ;
#224632 = VERTEX_POINT ( 'NONE', #20689 ) ;
#224633 = ORIENTED_EDGE ( 'NONE', *, *, #150054, .T. ) ;
#224634 = EDGE_CURVE ( 'NONE', #19725, #116714, #162379, .T. ) ;
#224636 = ORIENTED_EDGE ( 'NONE', *, *, #103472, .F. ) ;
#224635 = AXIS2_PLACEMENT_3D ( 'NONE', #31453, #133089, #110952 ) ;
#224637 = TOROIDAL_SURFACE ( 'NONE', #245507, 11.65000000000000036, 0.1000000000000000056 ) ;
#224638 = CARTESIAN_POINT ( 'NONE',  ( -18.52139480978221542, 85.48135884507900073, -129.4985509174051685 ) ) ;
#224639 = EDGE_LOOP ( 'NONE', ( #198886, #63448, #240952, #80540 ) ) ;
#224640 = DIRECTION ( 'NONE',  ( 0.000000000000000000, 1.000000000000000000, 0.000000000000000000 ) ) ;
#224641 = EDGE_CURVE ( 'NONE', #113334, #257983, #249850, .T. ) ;
#224643 = VERTEX_POINT ( 'NONE', #235850 ) ;
#224642 = CARTESIAN_POINT ( 'NONE',  ( -18.50000000000000000, 9.250000000011157297, -88.25000000000005684 ) ) ;
#224644 = LINE ( 'NONE', #125554, #192771 ) ;
#224645 = CARTESIAN_POINT ( 'NONE',  ( -22.39999999999999858, 0.1000000000111554016, -92.70922040162662370 ) ) ;
#224646 = CIRCLE ( 'NONE', #233063, 0.09999999999999963085 ) ;
#224648 = AXIS2_PLACEMENT_3D ( 'NONE', #8648, #186002, #86872 ) ;
#224647 = CARTESIAN_POINT ( 'NONE',  ( 20.90000000000000213, -1.885425182446133885, -11.49641995933507843 ) ) ;
#224649 = DIRECTION ( 'NONE',  ( 0.000000000000000000, -6.982962677686266711E-15, 1.000000000000000000 ) ) ;
#224650 = DIRECTION ( 'NONE',  ( 0.000000000000000000, 0.000000000000000000, -1.000000000000000000 ) ) ;
#224652 = CARTESIAN_POINT ( 'NONE',  ( 21.05000000000000071, 33.98486250090727623, -243.5821103306120108 ) ) ;
#224651 = CARTESIAN_POINT ( 'NONE',  ( 21.15000000000005542, 83.80000000001119531, -51.02310748452479316 ) ) ;
#224653 = DIRECTION ( 'NONE',  ( -0.000000000000000000, 0.4791956752371485107, 0.8777080977375185666 ) ) ;
#224654 = CARTESIAN_POINT ( 'NONE',  ( 21.14999999999999503, 67.23127455305841238, -235.8551265064783991 ) ) ;
#224655 = CARTESIAN_POINT ( 'NONE',  ( -23.15000000000000213, 70.60814576644823148, -215.7631455941064189 ) ) ;
#224656 = CARTESIAN_POINT ( 'NONE',  ( -23.24999999999999645, 85.60000000001210196, -129.9229180933022576 ) ) ;
#224657 = ORIENTED_EDGE ( 'NONE', *, *, #246469, .F. ) ;
#224658 = CIRCLE ( 'NONE', #195660, 0.1000000000000008937 ) ;
#224659 = AXIS2_PLACEMENT_3D ( 'NONE', #194041, #57038, #257782 ) ;
#224660 = TOROIDAL_SURFACE ( 'NONE', #141283, 3.899999999999999467, 0.1000000000000000056 ) ;
#224661 = VECTOR ( 'NONE', #1107, 1000.000000000000000 ) ;
#224663 = ORIENTED_EDGE ( 'NONE', *, *, #193849, .T. ) ;
#224662 = DIRECTION ( 'NONE',  ( -0.000000000000000000, 6.982962677686266711E-15, -1.000000000000000000 ) ) ;
#224664 = VERTEX_POINT ( 'NONE', #121086 ) ;
#224665 = VECTOR ( 'NONE', #53729, 1000.000000000000000 ) ;
#224666 = CARTESIAN_POINT ( 'NONE',  ( 18.50000000000000000, -0.5913595841389442942, -242.4574432119242999 ) ) ;
#224667 = CARTESIAN_POINT ( 'NONE',  ( 20.77526135991795186, 8.932009016637321608, -142.4685685427219539 ) ) ;
#224668 = CARTESIAN_POINT ( 'NONE',  ( 21.00000000000000000, 66.25000000001206502, -124.2731074845243597 ) ) ;
#224669 = ORIENTED_EDGE ( 'NONE', *, *, #187651, .F. ) ;
#224670 = DIRECTION ( 'NONE',  ( 0.000000000000000000, 0.000000000000000000, -1.000000000000000000 ) ) ;
#224671 = CARTESIAN_POINT ( 'NONE',  ( 20.99999999999999645, 66.25000000001182343, -82.17310748452439384 ) ) ;
#224672 = CIRCLE ( 'NONE', #257954, 11.74999999999999645 ) ;
#224673 = ORIENTED_EDGE ( 'NONE', *, *, #64855, .T. ) ;
#224674 = DIRECTION ( 'NONE',  ( 0.000000000000000000, 0.000000000000000000, 1.000000000000000000 ) ) ;
#224675 = CARTESIAN_POINT ( 'NONE',  ( 23.15000000000000213, 85.00000000001179501, -79.41707660717668205 ) ) ;
#224676 = PLANE ( 'NONE',  #180290 ) ;
#224677 = CARTESIAN_POINT ( 'NONE',  ( 20.95263205890648095, 40.76960636093260604, -237.9620195468288557 ) ) ;
#224679 = VERTEX_POINT ( 'NONE', #237153 ) ;
#224678 = CARTESIAN_POINT ( 'NONE',  ( -20.90000000000000213, 7.800000000000000711, -1.212568896937008089 ) ) ;
#224680 = DIRECTION ( 'NONE',  ( 1.000000000000000000, 6.828358547165751995E-15, 1.501968970420579709E-14 ) ) ;
#224681 = CARTESIAN_POINT ( 'NONE',  ( -20.00857864376270001, 52.27009174976920747, -232.4217594817395138 ) ) ;
#224682 = CARTESIAN_POINT ( 'NONE',  ( 20.94999999999999929, 11.36448785225375424, -246.7787679937655980 ) ) ;
#224683 = CARTESIAN_POINT ( 'NONE',  ( -18.59999999999999787, 11.74999999999999645, 11.75000000000000000 ) ) ;
#224684 = ORIENTED_EDGE ( 'NONE', *, *, #73807, .F. ) ;
#224685 = CARTESIAN_POINT ( 'NONE',  ( -16.94037747912386394, 65.98646061752597802, -157.4719765265489286 ) ) ;
#224686 = CIRCLE ( 'NONE', #45649, 0.09999999999999939493 ) ;
#224687 = DIRECTION ( 'NONE',  ( 0.000000000000000000, 0.000000000000000000, -1.000000000000000000 ) ) ;
#224689 = DIRECTION ( 'NONE',  ( -1.000000000000000000, -0.000000000000000000, -0.000000000000000000 ) ) ;
#224688 = CARTESIAN_POINT ( 'NONE',  ( -17.78241384940471193, 65.14442424718357927, -79.77214515698624098 ) ) ;
#224691 = EDGE_CURVE ( 'NONE', #199100, #82771, #117203, .T. ) ;
#224690 = DIRECTION ( 'NONE',  ( 0.000000000000000000, 0.8814952561688438326, -0.4721928772777334582 ) ) ;
#224692 = CIRCLE ( 'NONE', #62215, 0.1000000000000028644 ) ;
#224693 = CARTESIAN_POINT ( 'NONE',  ( -16.87683809663752399, 9.950000000011137047, -53.59763598180367694 ) ) ;
#224694 = FILL_AREA_STYLE_COLOUR ( '', #170566 ) ;
#224695 = CARTESIAN_POINT ( 'NONE',  ( -20.85000000000000142, -1.736705739456431807, -112.0174225876237699 ) ) ;
#224696 = CARTESIAN_POINT ( 'NONE',  ( -23.25000000000000355, 70.35000000001190301, -93.77310748452434552 ) ) ;
#224697 = CARTESIAN_POINT ( 'NONE',  ( -23.15000000000000213, 69.15921093109223250, -247.4965637597669854 ) ) ;
#224699 = ORIENTED_EDGE ( 'NONE', *, *, #34622, .F. ) ;
#224698 = VECTOR ( 'NONE', #35536, 1000.000000000000000 ) ;
#224700 = CARTESIAN_POINT ( 'NONE',  ( -20.85000000000000142, 68.97833521811179480, -99.18954208262705663 ) ) ;
#224701 = ORIENTED_EDGE ( 'NONE', *, *, #253966, .T. ) ;
#224702 = ORIENTED_EDGE ( 'NONE', *, *, #41362, .T. ) ;
#224703 = FACE_OUTER_BOUND ( 'NONE', #189482, .T. ) ;
#224704 = LINE ( 'NONE', #202588, #231804 ) ;
#224705 = ORIENTED_EDGE ( 'NONE', *, *, #8325, .T. ) ;
#224707 = EDGE_CURVE ( 'NONE', #228258, #80890, #61066, .T. ) ;
#224706 = VECTOR ( 'NONE', #81398, 1000.000000000000000 ) ;
#224708 = ORIENTED_EDGE ( 'NONE', *, *, #189705, .T. ) ;
#224709 = CIRCLE ( 'NONE', #33229, 0.2000000000000057288 ) ;
#224710 = ORIENTED_EDGE ( 'NONE', *, *, #198383, .F. ) ;
#224711 = DIRECTION ( 'NONE',  ( 0.000000000000000000, -6.982962677686266711E-15, 1.000000000000000000 ) ) ;
#224712 = ORIENTED_EDGE ( 'NONE', *, *, #94759, .F. ) ;
#224713 = DIRECTION ( 'NONE',  ( 1.000000000000000000, 0.000000000000000000, 0.000000000000000000 ) ) ;
#224714 = DIRECTION ( 'NONE',  ( 0.000000000000000000, 0.4088369013363276072, -0.9126074666063773710 ) ) ;
#224715 = CARTESIAN_POINT ( 'NONE',  ( -23.25000000000000000, 69.01799029515524353, -65.82695536626808064 ) ) ;
#224716 = CARTESIAN_POINT ( 'NONE',  ( -20.54999999999999716, 73.60000000001204512, -123.2984855617622202 ) ) ;
#224717 = CARTESIAN_POINT ( 'NONE',  ( -21.07928932188134041, 1.596973512272247042, -230.6572452218044020 ) ) ;
#224718 = ADVANCED_FACE ( 'NONE', ( #138024 ), #83229, .T. ) ;
#224719 = LINE ( 'NONE', #125634, #37620 ) ;
#224720 = EDGE_CURVE ( 'NONE', #122419, #119288, #4148, .T. ) ;
#224721 = LINE ( 'NONE', #164770, #203571 ) ;
#224723 = ORIENTED_EDGE ( 'NONE', *, *, #36075, .T. ) ;
#224722 = CARTESIAN_POINT ( 'NONE',  ( 21.14999999999999858, 44.24607648097409651, -236.5241869975821771 ) ) ;
#224725 = DIRECTION ( 'NONE',  ( 0.000000000000000000, 0.000000000000000000, 1.000000000000000000 ) ) ;
#224724 = CARTESIAN_POINT ( 'NONE',  ( 20.99749315643149217, 11.75000000000000355, -26.48519423124078997 ) ) ;
#224726 = LINE ( 'NONE', #46094, #28325 ) ;
#224727 = ORIENTED_EDGE ( 'NONE', *, *, #72986, .F. ) ;
#224728 = FACE_OUTER_BOUND ( 'NONE', #2608, .T. ) ;
#224730 = EDGE_CURVE ( 'NONE', #247235, #10361, #149918, .T. ) ;
#224729 = DIRECTION ( 'NONE',  ( -1.000000000000000000, 0.000000000000000000, -0.000000000000000000 ) ) ;
#224731 = FILL_AREA_STYLE_COLOUR ( '', #224831 ) ;
#224732 = ORIENTED_EDGE ( 'NONE', *, *, #10904, .T. ) ;
#224733 = CARTESIAN_POINT ( 'NONE',  ( 22.39999999999999503, 76.00000000001170974, -77.31388708289769340 ) ) ;
#224734 = AXIS2_PLACEMENT_3D ( 'NONE', #81163, #202414, #75112 ) ;
#224735 = AXIS2_PLACEMENT_3D ( 'NONE', #91475, #52318, #172341 ) ;
#224736 = DIRECTION ( 'NONE',  ( 1.000000000000000000, 0.000000000000000000, 0.000000000000000000 ) ) ;
#224737 = ORIENTED_EDGE ( 'NONE', *, *, #57799, .T. ) ;
#224738 = DIRECTION ( 'NONE',  ( -0.000000000000000000, -0.9770955615653310611, -0.2128009952263620608 ) ) ;
#224739 = EDGE_CURVE ( 'NONE', #81995, #67087, #37488, .T. ) ;
#224740 = DIRECTION ( 'NONE',  ( 0.000000000000000000, 0.000000000000000000, 1.000000000000000000 ) ) ;
#224741 = PLANE ( 'NONE',  #203299 ) ;
#224742 = VERTEX_POINT ( 'NONE', #81883 ) ;
#224743 = ORIENTED_EDGE ( 'NONE', *, *, #113241, .T. ) ;
#224744 = EDGE_CURVE ( 'NONE', #4036, #25616, #170797, .T. ) ;
#224745 = CARTESIAN_POINT ( 'NONE',  ( 23.14999999999999503, 14.10000000001115694, -61.39970238886063925 ) ) ;
#224746 = DIRECTION ( 'NONE',  ( 1.000000000000000000, 0.000000000000000000, 0.000000000000000000 ) ) ;
#224747 = AXIS2_PLACEMENT_3D ( 'NONE', #98402, #196262, #76302 ) ;
#224748 = LINE ( 'NONE', #207800, #220130 ) ;
#224750 = CARTESIAN_POINT ( 'NONE',  ( 18.39999999999999503, 11.47316190337363828, -91.25000000000005684 ) ) ;
#224749 = AXIS2_PLACEMENT_3D ( 'NONE', #132316, #63683, #33261 ) ;
#224751 = AXIS2_PLACEMENT_3D ( 'NONE', #55126, #232544, #53883 ) ;
#224752 = AXIS2_PLACEMENT_3D ( 'NONE', #83249, #124984, #221484 ) ;
#224753 = CARTESIAN_POINT ( 'NONE',  ( 20.94999999999999929, 67.23127455305835554, -235.8551265064784559 ) ) ;
#224754 = DIRECTION ( 'NONE',  ( 0.000000000000000000, 0.000000000000000000, -1.000000000000000000 ) ) ;
#224755 = VERTEX_POINT ( 'NONE', #42800 ) ;
#224756 = DIRECTION ( 'NONE',  ( -0.000000000000000000, 1.000000000000000000, -0.000000000000000000 ) ) ;
#224758 = ORIENTED_EDGE ( 'NONE', *, *, #17210, .T. ) ;
#224757 = CARTESIAN_POINT ( 'NONE',  ( 21.11747605621531321, 8.778708005504054057, -179.7445631697897568 ) ) ;
#224759 = AXIS2_PLACEMENT_3D ( 'NONE', #230877, #13106, #52199 ) ;
#224760 = CARTESIAN_POINT ( 'NONE',  ( 23.15000000000000213, -8.999999999988844479, -43.39396912265245021 ) ) ;
#224761 = CARTESIAN_POINT ( 'NONE',  ( -16.82055514392384055, 66.05000000001189164, -90.34630940998262361 ) ) ;
#224762 = CARTESIAN_POINT ( 'NONE',  ( -21.11927991906891577, 75.99091632053783485, -75.97160060301582973 ) ) ;
#224763 = CARTESIAN_POINT ( 'NONE',  ( -23.15000000000000213, 85.60000000001221565, -148.2731074845242176 ) ) ;
#224764 = LINE ( 'NONE', #223479, #163072 ) ;
#224766 = ORIENTED_EDGE ( 'NONE', *, *, #161719, .T. ) ;
#224765 = DIRECTION ( 'NONE',  ( -0.000000000000000000, -0.9770955615653313941, -0.2128009952263603677 ) ) ;
#224767 = DIRECTION ( 'NONE',  ( 1.000000000000000000, 0.000000000000000000, 0.000000000000000000 ) ) ;
#224768 = CARTESIAN_POINT ( 'NONE',  ( -18.59117750673697245, 65.66751761918722252, -164.4282609406112670 ) ) ;
#224769 = DIRECTION ( 'NONE',  ( 0.000000000000000000, 0.1575844902526835067, 0.9875055080513738259 ) ) ;
#224770 = DIRECTION ( 'NONE',  ( 1.000000000000000000, 0.000000000000000000, 0.000000000000000000 ) ) ;
#224771 = ORIENTED_EDGE ( 'NONE', *, *, #195131, .T. ) ;
#224772 = CARTESIAN_POINT ( 'NONE',  ( -21.05000000000000071, 46.91436717984746707, -255.3877622108296634 ) ) ;
#224773 = DIRECTION ( 'NONE',  ( 1.000000000000000000, 0.000000000000000000, 0.000000000000000000 ) ) ;
#224774 = CIRCLE ( 'NONE', #112371, 0.09999999999998898659 ) ;
#224775 = DIRECTION ( 'NONE',  ( 0.000000000000000000, 0.000000000000000000, 1.000000000000000000 ) ) ;
#224776 = CARTESIAN_POINT ( 'NONE',  ( -20.64999999999999858, 1.999999999999998224, -12.72462192276209869 ) ) ;
#224777 = ORIENTED_EDGE ( 'NONE', *, *, #120984, .F. ) ;
#224778 = CARTESIAN_POINT ( 'NONE',  ( -16.92280123533709357, 9.950000000011137047, -87.64936768591496730 ) ) ;
#224779 = EDGE_LOOP ( 'NONE', ( #165376, #28525, #217598, #160502 ) ) ;
#224780 = EDGE_CURVE ( 'NONE', #138314, #238428, #124965, .T. ) ;
#224781 = LINE ( 'NONE', #160987, #130808 ) ;
#224783 = EDGE_CURVE ( 'NONE', #166275, #102030, #256651, .T. ) ;
#224782 = DIRECTION ( 'NONE',  ( -0.000000000000000000, 0.5474227397873200340, -0.8368562265788217491 ) ) ;
#224784 = DIRECTION ( 'NONE',  ( 1.000000000000000000, 0.000000000000000000, 0.000000000000000000 ) ) ;
#224785 = CARTESIAN_POINT ( 'NONE',  ( -23.15000000000000213, 0.000000000000000000, -33.50000000000000000 ) ) ;
#224786 = VERTEX_POINT ( 'NONE', #64914 ) ;
#224787 = EDGE_CURVE ( 'NONE', #34288, #160017, #224709, .T. ) ;
#224788 = ADVANCED_FACE ( 'NONE', ( #27119 ), #154227, .T. ) ;
#224789 = CARTESIAN_POINT ( 'NONE',  ( 20.94999999999999929, 76.00000000001142553, -36.02310748452432421 ) ) ;
#224790 = ADVANCED_FACE ( 'NONE', ( #106595 ), #184866, .T. ) ;
#224791 = LINE ( 'NONE', #26633, #158187 ) ;
#224792 = CARTESIAN_POINT ( 'NONE',  ( -20.94999999999999929, 1.115600667400684642E-11, -155.8000000000000398 ) ) ;
#224794 = DIRECTION ( 'NONE',  ( 6.484947573744954877E-15, 0.9274965247785529332, -0.3738317757009255171 ) ) ;
#224793 = CIRCLE ( 'NONE', #37574, 0.1000000000000054040 ) ;
#224795 = ADVANCED_FACE ( 'NONE', ( #102740 ), #84438, .F. ) ;
#224798 = EDGE_CURVE ( 'NONE', #246752, #250586, #107899, .T. ) ;
#224797 = EDGE_CURVE ( 'NONE', #27216, #24894, #105296, .T. ) ;
#224796 = FACE_OUTER_BOUND ( 'NONE', #228878, .T. ) ;
#224799 = ORIENTED_EDGE ( 'NONE', *, *, #175835, .T. ) ;
#224801 = ORIENTED_EDGE ( 'NONE', *, *, #206129, .T. ) ;
#224800 = CARTESIAN_POINT ( 'NONE',  ( -20.64999999999999858, 68.75000000001260503, -191.1731074845243938 ) ) ;
#224802 = ORIENTED_EDGE ( 'NONE', *, *, #144665, .T. ) ;
#224803 = LINE ( 'NONE', #227381, #252863 ) ;
#224804 = VERTEX_POINT ( 'NONE', #45362 ) ;
#224805 = CARTESIAN_POINT ( 'NONE',  ( 21.05000000000001492, 61.10422374072478391, -234.2088091958333678 ) ) ;
#224806 = CARTESIAN_POINT ( 'NONE',  ( -20.54999999999999716, 7.150000000011155876, -45.85000000000000142 ) ) ;
#224807 = DIRECTION ( 'NONE',  ( 0.000000000000000000, -0.5000000000000209832, -0.8660254037844264952 ) ) ;
#224808 = CIRCLE ( 'NONE', #162471, 0.09999999999998898659 ) ;
#224809 = ORIENTED_EDGE ( 'NONE', *, *, #5446, .T. ) ;
#224811 = VECTOR ( 'NONE', #106493, 1000.000000000000000 ) ;
#224810 = CARTESIAN_POINT ( 'NONE',  ( -16.92570016628985385, 66.04121104227171202, -56.90245681448540438 ) ) ;
#224812 = CARTESIAN_POINT ( 'NONE',  ( -23.25000000000000000, 64.25000000001203659, -114.7731074845243882 ) ) ;
#224813 = CARTESIAN_POINT ( 'NONE',  ( 20.97438252431638972, 8.925423506087151182, -41.97237068901081614 ) ) ;
#224814 = VERTEX_POINT ( 'NONE', #203150 ) ;
#224815 = DIRECTION ( 'NONE',  ( 1.000000000000000000, 0.000000000000000000, 0.000000000000000000 ) ) ;
#224816 = EDGE_CURVE ( 'NONE', #223292, #191184, #191626, .T. ) ;
#224818 = ORIENTED_EDGE ( 'NONE', *, *, #247256, .T. ) ;
#224817 = FACE_OUTER_BOUND ( 'NONE', #199279, .T. ) ;
#224819 = CARTESIAN_POINT ( 'NONE',  ( -23.25000000000000355, 9.950000000011138823, -42.75000000000000000 ) ) ;
#224820 = DIRECTION ( 'NONE',  ( 0.000000000000000000, 0.000000000000000000, -1.000000000000000000 ) ) ;
#224821 = EDGE_CURVE ( 'NONE', #92784, #135478, #58466, .T. ) ;
#224822 = EDGE_CURVE ( 'NONE', #21472, #2690, #245756, .T. ) ;
#224823 = AXIS2_PLACEMENT_3D ( 'NONE', #7707, #67662, #202045 ) ;
#224824 = TOROIDAL_SURFACE ( 'NONE', #216636, 11.65000000000000036, 0.1000000000000000056 ) ;
#224825 = ORIENTED_EDGE ( 'NONE', *, *, #106163, .F. ) ;
#224827 = ADVANCED_FACE ( 'NONE', ( #145733 ), #29557, .T. ) ;
#224826 = CARTESIAN_POINT ( 'NONE',  ( 21.08750232978087524, 10.72486338602132250, -79.22885817299962241 ) ) ;
#224828 = CARTESIAN_POINT ( 'NONE',  ( 23.24999999999999645, 8.822561741677553471, -46.15000000000001279 ) ) ;
#224829 = VERTEX_POINT ( 'NONE', #187460 ) ;
#224830 = DIRECTION ( 'NONE',  ( 0.000000000000000000, 0.8814952561688444987, -0.4721928772777320149 ) ) ;
#224831 = COLOUR_RGB ( '', 0.31764706, 0.68627451, 0.89019608) ;
#224832 = CARTESIAN_POINT ( 'NONE',  ( -20.85000000000000142, 79.24821784679178904, -196.3217825494968736 ) ) ;
#224833 = EDGE_CURVE ( 'NONE', #244974, #153506, #45848, .T. ) ;
#224834 = AXIS2_PLACEMENT_3D ( 'NONE', #257392, #176657, #80061 ) ;
#224835 = CIRCLE ( 'NONE', #20873, 4.099999999999992539 ) ;
#224836 = ORIENTED_EDGE ( 'NONE', *, *, #177769, .T. ) ;
#224837 = AXIS2_PLACEMENT_3D ( 'NONE', #183056, #205151, #106044 ) ;
#224838 = AXIS2_PLACEMENT_3D ( 'NONE', #127017, #187013, #15763 ) ;
#224839 = AXIS2_PLACEMENT_3D ( 'NONE', #167333, #13378, #231158 ) ;
#224840 = ORIENTED_EDGE ( 'NONE', *, *, #105959, .T. ) ;
#224842 = CARTESIAN_POINT ( 'NONE',  ( 21.11344571971183015, 65.38212097649690691, -191.2770865921224015 ) ) ;
#224841 = AXIS2_PLACEMENT_3D ( 'NONE', #211879, #52767, #216974 ) ;
#224843 = AXIS2_PLACEMENT_3D ( 'NONE', #7403, #201758, #126061 ) ;
#224844 = ORIENTED_EDGE ( 'NONE', *, *, #232940, .F. ) ;
#224845 = CARTESIAN_POINT ( 'NONE',  ( 18.59999999999999787, 77.26327546522934142, -128.6212428177779543 ) ) ;
#224846 = CARTESIAN_POINT ( 'NONE',  ( -16.93710578446435377, 66.05000000001255955, -182.9419114683242640 ) ) ;
#224848 = VERTEX_POINT ( 'NONE', #63638 ) ;
#224847 = DIRECTION ( 'NONE',  ( 1.000000000000000000, 0.000000000000000000, 0.000000000000000000 ) ) ;
#224849 = CARTESIAN_POINT ( 'NONE',  ( 20.96428641294275863, 11.75000000001150013, -127.1748931779422946 ) ) ;
#224850 = DIRECTION ( 'NONE',  ( 1.000000000000000000, -0.000000000000000000, -0.000000000000000000 ) ) ;
#224851 = FILL_AREA_STYLE ('',( #205282 ) ) ;
#224852 = CARTESIAN_POINT ( 'NONE',  ( 23.14999999999998437, 1.115650265596050101E-11, -129.9500000000000171 ) ) ;
#224853 = DIRECTION ( 'NONE',  ( -1.000000000000000000, -0.000000000000000000, -0.000000000000000000 ) ) ;
#224854 = DIRECTION ( 'NONE',  ( 2.952720810173289112E-16, -0.9770955615653301729, -0.2128009952263660853 ) ) ;
#224855 = FACE_OUTER_BOUND ( 'NONE', #94838, .T. ) ;
#224857 = ORIENTED_EDGE ( 'NONE', *, *, #171534, .T. ) ;
#224856 = PLANE ( 'NONE',  #56854 ) ;
#224858 = CARTESIAN_POINT ( 'NONE',  ( -20.94999999999999929, 7.128833340094563376, -233.7327013124401276 ) ) ;
#224859 = EDGE_LOOP ( 'NONE', ( #67937, #179696, #32629, #129368 ) ) ;
#224860 = LINE ( 'NONE', #46228, #160015 ) ;
#224861 = DIRECTION ( 'NONE',  ( 0.000000000000000000, 0.9651348961777163060, -0.2617529984165013479 ) ) ;
#224862 = DIRECTION ( 'NONE',  ( -0.000000000000000000, 1.000000000000000000, -0.000000000000000000 ) ) ;
#224863 = CARTESIAN_POINT ( 'NONE',  ( 20.44999100639871514, 65.56028929680083195, -195.7640317585554044 ) ) ;
#224864 = CARTESIAN_POINT ( 'NONE',  ( -20.54999999999999716, 4.590145742703442444, -213.0289728181953706 ) ) ;
#224865 = ORIENTED_EDGE ( 'NONE', *, *, #53836, .T. ) ;
#224866 = DIRECTION ( 'NONE',  ( 0.000000000000000000, 0.9651348961777156399, -0.2617529984165037349 ) ) ;
#224867 = ADVANCED_FACE ( 'NONE', ( #149623 ), #15238, .F. ) ;
#224868 = DIRECTION ( 'NONE',  ( 1.186688945009009831E-16, 1.000000000000000000, 6.982962677686266711E-15 ) ) ;
#224869 = CIRCLE ( 'NONE', #112482, 0.09999999999999520384 ) ;
#224870 = EDGE_CURVE ( 'NONE', #84512, #164185, #79143, .T. ) ;
#224871 = ORIENTED_EDGE ( 'NONE', *, *, #162211, .T. ) ;
#224872 = DIRECTION ( 'NONE',  ( -1.000000000000000000, -0.000000000000000000, -0.000000000000000000 ) ) ;
#224873 = CARTESIAN_POINT ( 'NONE',  ( -18.44448725179913495, 86.89435926455711012, -199.6093239235941894 ) ) ;
#224874 = EDGE_CURVE ( 'NONE', #130245, #212130, #33553, .T. ) ;
#224875 = ORIENTED_EDGE ( 'NONE', *, *, #147284, .F. ) ;
#224877 = EDGE_CURVE ( 'NONE', #149698, #75395, #224883, .T. ) ;
#224876 = CARTESIAN_POINT ( 'NONE',  ( 20.27550659511089037, 66.78395627750316521, -115.6731074845243654 ) ) ;
#224878 = VERTEX_POINT ( 'NONE', #32243 ) ;
#224879 = CARTESIAN_POINT ( 'NONE',  ( -23.39999999999994529, 87.50449464844290048, -37.85861909827351468 ) ) ;
#224880 = EDGE_LOOP ( 'NONE', ( #29997, #212097, #238078, #241860 ) ) ;
#224881 = AXIS2_PLACEMENT_3D ( 'NONE', #175153, #76002, #172589 ) ;
#224882 = DIRECTION ( 'NONE',  ( -3.265361837132813093E-16, 1.000000000000000000, 0.000000000000000000 ) ) ;
#224883 = CIRCLE ( 'NONE', #150109, 0.1000000000000028644 ) ;
#224884 = CARTESIAN_POINT ( 'NONE',  ( 12.93225390519045703, 9.417651958852161442, -182.8587873924404050 ) ) ;
#224885 = ORIENTED_EDGE ( 'NONE', *, *, #173239, .T. ) ;
#224886 = DIRECTION ( 'NONE',  ( 2.952720810173289112E-16, 0.9651348961777191926, -0.2617529984164898571 ) ) ;
#224888 = ORIENTED_EDGE ( 'NONE', *, *, #38185, .F. ) ;
#224887 = CARTESIAN_POINT ( 'NONE',  ( 13.22261339317536688, 9.436552840015581367, -48.67795547276031698 ) ) ;
#224889 = CARTESIAN_POINT ( 'NONE',  ( 23.14999999999999858, 7.525330762710603416, -212.0571253909869256 ) ) ;
#224890 = AXIS2_PLACEMENT_3D ( 'NONE', #232416, #116313, #255763 ) ;
#224891 = EDGE_LOOP ( 'NONE', ( #178603, #218577 ) ) ;
#224892 =( BOUNDED_SURFACE ( )  B_SPLINE_SURFACE ( 3, 2, ( 
 ( #243673, #85845, #188832 ),
 ( #246246, #91016, #66327 ),
 ( #205829, #244951, #31085 ),
 ( #6333, #145843, #10214 ) ),
 .UNSPECIFIED., .F., .F., .T. ) 
 B_SPLINE_SURFACE_WITH_KNOTS ( ( 4, 4 ),
 ( 3, 3 ),
 ( 0.04058434257139457990, 0.04256401539001584966 ),
 ( 0.000000000000000000, 1.000000000000000000 ),
 .UNSPECIFIED. ) 
 GEOMETRIC_REPRESENTATION_ITEM ( )  RATIONAL_B_SPLINE_SURFACE ( (
 ( 1.000000000000000000, 0.7103081912007894738, 1.000000000000000000),
 ( 1.000000000000000000, 0.7104998333556562518, 1.000000000000000000),
 ( 1.000000000000000000, 0.7107238315754180746, 1.000000000000000000),
 ( 1.000000000000000000, 0.7110073749539692622, 1.000000000000000000) ) ) 
 REPRESENTATION_ITEM ( '' )  SURFACE ( )  );
#224893 = EDGE_CURVE ( 'NONE', #92153, #33930, #75094, .T. ) ;
#224894 = TOROIDAL_SURFACE ( 'NONE', #241666, 7.800000000000000711, 0.1000000000000000056 ) ;
#224895 = EDGE_CURVE ( 'NONE', #86684, #127278, #192004, .T. ) ;
#224896 = ORIENTED_EDGE ( 'NONE', *, *, #51951, .T. ) ;
#224897 = CARTESIAN_POINT ( 'NONE',  ( 18.59999999999999787, 18.37021030142088662, -237.6367305148568221 ) ) ;
#224898 = DIRECTION ( 'NONE',  ( 0.000000000000000000, 0.01283462868040404978, 0.9999176327611370985 ) ) ;
#224899 = CYLINDRICAL_SURFACE ( 'NONE', #257161, 2.600000000000001421 ) ;
#224900 = CARTESIAN_POINT ( 'NONE',  ( -23.15000000000000213, 87.65000000001238334, -170.0231074845242745 ) ) ;
#224901 = CARTESIAN_POINT ( 'NONE',  ( -13.88555196119804691, 66.54256847116366202, -188.5231905466247611 ) ) ;
#224902 = DIRECTION ( 'NONE',  ( 0.000000000000000000, 0.000000000000000000, -1.000000000000000000 ) ) ;
#224903 = VERTEX_POINT ( 'NONE', #191327 ) ;
#224904 = CARTESIAN_POINT ( 'NONE',  ( -18.59999999999999787, 11.75000000001115552, -200.9999999999999432 ) ) ;
#224906 = ADVANCED_FACE ( 'NONE', ( #11376 ), #92182, .F. ) ;
#224905 = DIRECTION ( 'NONE',  ( -0.000000000000000000, -6.982962677686266711E-15, 1.000000000000000000 ) ) ;
#224907 = LINE ( 'NONE', #207956, #32835 ) ;
#224908 = VECTOR ( 'NONE', #60766, 1000.000000000000000 ) ;
#224909 = CARTESIAN_POINT ( 'NONE',  ( 21.14999999999999858, 8.786607556611267356, -79.35000000000005116 ) ) ;
#224910 = AXIS2_PLACEMENT_3D ( 'NONE', #103005, #181297, #205972 ) ;
#224911 = VERTEX_POINT ( 'NONE', #75224 ) ;
#224912 = EDGE_CURVE ( 'NONE', #220667, #91403, #188720, .T. ) ;
#224913 = CARTESIAN_POINT ( 'NONE',  ( -21.04999999999999005, 75.90156250001201954, -109.3223383946111653 ) ) ;
#224914 = ORIENTED_EDGE ( 'NONE', *, *, #160758, .T. ) ;
#224915 = CARTESIAN_POINT ( 'NONE',  ( 14.87567385445977308, 9.430764995433477793, -115.7305373947504989 ) ) ;
#224916 = ORIENTED_EDGE ( 'NONE', *, *, #60826, .T. ) ;
#224917 = DIRECTION ( 'NONE',  ( 0.000000000000000000, 0.000000000000000000, 1.000000000000000000 ) ) ;
#224918 = ORIENTED_EDGE ( 'NONE', *, *, #220109, .T. ) ;
#224919 = ORIENTED_EDGE ( 'NONE', *, *, #228165, .T. ) ;
#224921 = VERTEX_POINT ( 'NONE', #54336 ) ;
#224920 = CARTESIAN_POINT ( 'NONE',  ( -23.25000000000000000, 0.000000000000000000, -33.50000000000000000 ) ) ;
#224922 = CARTESIAN_POINT ( 'NONE',  ( 23.15000000000000213, 87.48912529308822172, -139.6231074845242688 ) ) ;
#224923 = VERTEX_POINT ( 'NONE', #94749 ) ;
#224924 = EDGE_CURVE ( 'NONE', #11015, #229726, #158307, .T. ) ;
#224925 = DIRECTION ( 'NONE',  ( 0.000000000000000000, -1.000000000000000000, -6.982962677686265922E-15 ) ) ;
#224926 = CARTESIAN_POINT ( 'NONE',  ( -18.59999999999999787, 77.83585931145600512, -158.5186683157258187 ) ) ;
#224927 = ADVANCED_FACE ( 'NONE', ( #72652 ), #230419, .F. ) ;
#224928 = ORIENTED_EDGE ( 'NONE', *, *, #239965, .T. ) ;
#224929 = AXIS2_PLACEMENT_3D ( 'NONE', #16082, #95581, #175173 ) ;
#224930 = CARTESIAN_POINT ( 'NONE',  ( -18.59999999999999787, 77.83585931145498193, -24.51866831572578320 ) ) ;
#224931 = VECTOR ( 'NONE', #235567, 1000.000000000000000 ) ;
#224933 = DIRECTION ( 'NONE',  ( -0.000000000000000000, -6.982962677686266711E-15, 1.000000000000000000 ) ) ;
#224932 = CIRCLE ( 'NONE', #112537, 0.1000000000000000472 ) ;
#224934 = EDGE_CURVE ( 'NONE', #144062, #160208, #71367, .T. ) ;
#224935 = VERTEX_POINT ( 'NONE', #152195 ) ;
#224936 = AXIS2_PLACEMENT_3D ( 'NONE', #147151, #165454, #244971 ) ;
#224937 = DIRECTION ( 'NONE',  ( -1.000000000000000000, -0.000000000000000000, -0.000000000000000000 ) ) ;
#224938 = EDGE_CURVE ( 'NONE', #74560, #67154, #133880, .T. ) ;
#224939 = SHAPE_REPRESENTATION ( 'Snap Open Cable Crossbars ', ( #2425 ), #247943 ) ;
#224941 = VERTEX_POINT ( 'NONE', #29682 ) ;
#224940 = CARTESIAN_POINT ( 'NONE',  ( 20.94999999999999929, -8.999999999988842703, -124.1060308773475924 ) ) ;
#224942 = DIRECTION ( 'NONE',  ( -1.000000000000000000, 0.000000000000000000, -1.020425574104004196E-15 ) ) ;
#224943 = CIRCLE ( 'NONE', #253995, 0.09999999999999939493 ) ;
#224944 = CARTESIAN_POINT ( 'NONE',  ( 18.59999999999999432, 68.22930980752001062, -227.7331931781284879 ) ) ;
#224945 = AXIS2_PLACEMENT_3D ( 'NONE', #175622, #196441, #17797 ) ;
#224946 = ADVANCED_FACE ( 'NONE', ( #192579 ), #248702, .T. ) ;
#224948 = CARTESIAN_POINT ( 'NONE',  ( -21.55000000000000426, 29.43195280696657790, -236.8879924315548351 ) ) ;
#224947 = FACE_OUTER_BOUND ( 'NONE', #154821, .T. ) ;
#224949 = CARTESIAN_POINT ( 'NONE',  ( -20.64999999999999858, 74.07476635515205032, -90.29286395139820343 ) ) ;
#224950 = DIRECTION ( 'NONE',  ( 1.000000000000000000, 0.000000000000000000, 0.000000000000000000 ) ) ;
#224951 = LINE ( 'NONE', #247086, #130160 ) ;
#224952 = VERTEX_POINT ( 'NONE', #233011 ) ;
#224953 = EDGE_LOOP ( 'NONE', ( #161500, #232645, #188200, #5037 ) ) ;
#224954 = CARTESIAN_POINT ( 'NONE',  ( 20.94999999999999929, 76.00000000001126921, -203.5231074845248997 ) ) ;
#224955 = ORIENTED_EDGE ( 'NONE', *, *, #201825, .F. ) ;
#224956 = CARTESIAN_POINT ( 'NONE',  ( -21.05315837477650120, 64.25000000001220712, -143.3647514783579595 ) ) ;
#224957 = ORIENTED_EDGE ( 'NONE', *, *, #148020, .T. ) ;
#224958 = PRESENTATION_STYLE_ASSIGNMENT (( #145432 ) ) ;
#224959 = DIRECTION ( 'NONE',  ( 1.000000000000000000, -0.000000000000000000, -0.000000000000000000 ) ) ;
#224960 = CARTESIAN_POINT ( 'NONE',  ( -20.54999999999999716, 7.150000000000000355, -12.25000000000000000 ) ) ;
#224961 = AXIS2_PLACEMENT_3D ( 'NONE', #115189, #55171, #134727 ) ;
#224962 = ORIENTED_EDGE ( 'NONE', *, *, #225667, .T. ) ;
#224963 = CARTESIAN_POINT ( 'NONE',  ( -21.05000000000000071, 61.95000000001162022, -64.00941241376342816 ) ) ;
#224964 = EDGE_LOOP ( 'NONE', ( #235848, #105394, #233614, #114294 ) ) ;
#224965 = EDGE_LOOP ( 'NONE', ( #194914, #191414, #149250, #254804, #177074 ) ) ;
#224966 = FACE_OUTER_BOUND ( 'NONE', #1623, .T. ) ;
#224968 = ORIENTED_EDGE ( 'NONE', *, *, #11494, .T. ) ;
#224967 = DIRECTION ( 'NONE',  ( -0.000000000000000000, 0.9910827722268050755, 0.1332476588733589318 ) ) ;
#224969 = TOROIDAL_SURFACE ( 'NONE', #50191, 0.2000000000000000111, 0.1000000000000000056 ) ;
#224970 = CARTESIAN_POINT ( 'NONE',  ( 20.04142135391667168, 11.75000000001116263, -158.7025068656295446 ) ) ;
#224972 = ORIENTED_EDGE ( 'NONE', *, *, #219747, .T. ) ;
#224971 = DIRECTION ( 'NONE',  ( 0.000000000000000000, 0.4088369013363287729, -0.9126074666063767049 ) ) ;
#224973 = DIRECTION ( 'NONE',  ( 4.377807931758638789E-15, 0.2605042016806672911, 0.9654727137038716656 ) ) ;
#224974 = CARTESIAN_POINT ( 'NONE',  ( -22.59999999999999787, 0.1008583691098682150, -122.2504328765106294 ) ) ;
#224976 = EDGE_LOOP ( 'NONE', ( #216970, #26666, #42520, #132229 ) ) ;
#224975 = DIRECTION ( 'NONE',  ( 1.000000000000000000, 0.000000000000000000, 0.000000000000000000 ) ) ;
#224977 = LINE ( 'NONE', #46351, #176492 ) ;
#224978 = FACE_OUTER_BOUND ( 'NONE', #50160, .T. ) ;
#224979 = DIRECTION ( 'NONE',  ( -0.7071067811865474617, -0.7071067811865474617, -2.044391222244499837E-16 ) ) ;
#224981 = CARTESIAN_POINT ( 'NONE',  ( -17.78043020864321022, 10.85359211200569085, -23.16304916572022066 ) ) ;
#224980 = DIRECTION ( 'NONE',  ( -1.000000000000000000, 0.000000000000000000, -0.000000000000000000 ) ) ;
#224982 = CARTESIAN_POINT ( 'NONE',  ( 21.05000000000000071, -10.38870553492056104, -206.3818953267866902 ) ) ;
#224983 = AXIS2_PLACEMENT_3D ( 'NONE', #22145, #221577, #3844 ) ;
#224984 = FACE_OUTER_BOUND ( 'NONE', #57318, .T. ) ;
#224985 = CARTESIAN_POINT ( 'NONE',  ( 21.14999999999999858, 1.363275264940683407, -230.6442496871288483 ) ) ;
#224986 = DIRECTION ( 'NONE',  ( -1.000000000000000000, -1.394253735153569469E-16, -2.602809386958778209E-16 ) ) ;
#224987 = ORIENTED_EDGE ( 'NONE', *, *, #72461, .F. ) ;
#224988 = ORIENTED_EDGE ( 'NONE', *, *, #68420, .F. ) ;
#224989 = ORIENTED_EDGE ( 'NONE', *, *, #102886, .F. ) ;
#224990 = DIRECTION ( 'NONE',  ( 1.000000000000000000, 0.000000000000000000, 0.000000000000000000 ) ) ;
#224991 = ORIENTED_EDGE ( 'NONE', *, *, #135873, .F. ) ;
#224993 = CARTESIAN_POINT ( 'NONE',  ( 21.05000000000000071, 85.40000000001148805, -45.91707660717669626 ) ) ;
#224992 = AXIS2_PLACEMENT_3D ( 'NONE', #107043, #105743, #148769 ) ;
#224994 = ORIENTED_EDGE ( 'NONE', *, *, #160495, .F. ) ;
#224995 = FACE_OUTER_BOUND ( 'NONE', #106033, .T. ) ;
#224996 = EDGE_CURVE ( 'NONE', #202617, #99286, #145787, .T. ) ;
#224997 = CARTESIAN_POINT ( 'NONE',  ( 18.43565242384934066, -9.519327731081281385, -40.47297637655933755 ) ) ;
#224998 = AXIS2_PLACEMENT_3D ( 'NONE', #171248, #212896, #107360 ) ;
#224999 = AXIS2_PLACEMENT_3D ( 'NONE', #94938, #174547, #113226 ) ;
#225000 = EDGE_CURVE ( 'NONE', #184932, #7699, #87524, .T. ) ;
#225001 = EDGE_CURVE ( 'NONE', #220739, #170250, #233307, .T. ) ;
#225002 = VERTEX_POINT ( 'NONE', #37371 ) ;
#225003 = CARTESIAN_POINT ( 'NONE',  ( -21.05000000000000071, 76.00000000001170974, -69.52310748452431710 ) ) ;
#225004 = SHAPE_REPRESENTATION_RELATIONSHIP ( 'NONE' , 'NONE' ,  #215063, #42038 ) ;
#225006 = EDGE_LOOP ( 'NONE', ( #44983, #192909, #36869, #69152 ) ) ;
#225005 = AXIS2_PLACEMENT_3D ( 'NONE', #130137, #209687, #31089 ) ;
#225007 = EDGE_LOOP ( 'NONE', ( #94025, #50398, #167277 ) ) ;
#225008 = AXIS2_PLACEMENT_3D ( 'NONE', #126594, #7942, #226978 ) ;
#225009 = ORIENTED_EDGE ( 'NONE', *, *, #45998, .F. ) ;
#225010 = CIRCLE ( 'NONE', #204172, 0.09999999999999939493 ) ;
#225011 = CIRCLE ( 'NONE', #173, 0.1000000000000124678 ) ;
#225012 = FACE_OUTER_BOUND ( 'NONE', #184920, .T. ) ;
#225013 = DIRECTION ( 'NONE',  ( 0.000000000000000000, -0.4721928772777383987, -0.8814952561688410571 ) ) ;
#225014 = DIRECTION ( 'NONE',  ( -1.000000000000000000, 0.000000000000000000, -0.000000000000000000 ) ) ;
#225015 = LINE ( 'NONE', #125923, #194103 ) ;
#225016 = DIRECTION ( 'NONE',  ( 1.000000000000000000, 0.000000000000000000, 0.000000000000000000 ) ) ;
#225017 = ADVANCED_FACE ( 'NONE', ( #25192 ), #158482, .T. ) ;
#225019 = DIRECTION ( 'NONE',  ( -0.000000000000000000, -6.982962677686266711E-15, 1.000000000000000000 ) ) ;
#225018 = DIRECTION ( 'NONE',  ( 0.000000000000000000, -0.6728388485993177515, 0.7397890806274072251 ) ) ;
#225020 = SPHERICAL_SURFACE ( 'NONE', #70704, 0.1000000000000000056 ) ;
#225022 = ORIENTED_EDGE ( 'NONE', *, *, #250068, .F. ) ;
#225021 = DIRECTION ( 'NONE',  ( 0.000000000000000000, 0.000000000000000000, -1.000000000000000000 ) ) ;
#225024 = DIRECTION ( 'NONE',  ( 0.000000000000000000, -6.938893903907222067E-15, 1.000000000000000000 ) ) ;
#225023 = CARTESIAN_POINT ( 'NONE',  ( 20.11144452914042091, 9.933610851134151432, -74.89029345395306336 ) ) ;
#225025 = LINE ( 'NONE', #88074, #40624 ) ;
#225026 = ORIENTED_EDGE ( 'NONE', *, *, #125274, .T. ) ;
#225027 = CARTESIAN_POINT ( 'NONE',  ( 20.95539060131842746, 10.62386215766680131, -74.65373381365624539 ) ) ;
#225028 = DIRECTION ( 'NONE',  ( 0.000000000000000000, -0.9394191166662618775, -0.3427706569150580362 ) ) ;
#225029 = DIRECTION ( 'NONE',  ( 1.000000000000000000, 0.000000000000000000, 0.000000000000000000 ) ) ;
#225030 = ORIENTED_EDGE ( 'NONE', *, *, #126646, .F. ) ;
#225031 = AXIS2_PLACEMENT_3D ( 'NONE', #98228, #175279, #216919 ) ;
#225032 = CARTESIAN_POINT ( 'NONE',  ( -16.91776028072577631, 30.23471468080184721, -234.8070487828878470 ) ) ;
#225033 = DIRECTION ( 'NONE',  ( 1.000000000000000000, 0.000000000000000000, 0.000000000000000000 ) ) ;
#225034 = CARTESIAN_POINT ( 'NONE',  ( -18.59999999999999787, -1.162701749926853712, -175.5999999999999659 ) ) ;
#225035 = VERTEX_POINT ( 'NONE', #4305 ) ;
#225036 = VERTEX_POINT ( 'NONE', #3017 ) ;
#225037 = CARTESIAN_POINT ( 'NONE',  ( -18.40000000000000213, 64.58541674041208580, -90.37310748452436826 ) ) ;
#225039 = EDGE_LOOP ( 'NONE', ( #146617, #26241, #136523, #240983 ) ) ;
#225038 = EDGE_CURVE ( 'NONE', #98224, #2617, #38639, .T. ) ;
#225040 = CARTESIAN_POINT ( 'NONE',  ( 19.95447128016623140, 5.488301201494659942, 16.50000000000000000 ) ) ;
#225041 = ADVANCED_FACE ( 'NONE', ( #242924 ), #141695, .T. ) ;
#225042 = CARTESIAN_POINT ( 'NONE',  ( -18.36527282682077100, -9.500000599987968641, -174.4221489645001952 ) ) ;
#225043 = FACE_OUTER_BOUND ( 'NONE', #2163, .T. ) ;
#225044 = CARTESIAN_POINT ( 'NONE',  ( -21.52071067811865746, 7.779289321881349473, -12.34999999999999964 ) ) ;
#225045 = ORIENTED_EDGE ( 'NONE', *, *, #52022, .F. ) ;
#225046 = AXIS2_PLACEMENT_3D ( 'NONE', #44375, #225530, #143452 ) ;
#225047 = CARTESIAN_POINT ( 'NONE',  ( -15.06720934482788188, 9.417690691074263043, -118.6416006967646695 ) ) ;
#225048 = DIRECTION ( 'NONE',  ( 2.952720810173289112E-16, 1.000000000000000000, 7.006261805886911631E-15 ) ) ;
#225049 = AXIS2_PLACEMENT_3D ( 'NONE', #62344, #102717, #41513 ) ;
#225050 = ADVANCED_FACE ( 'NONE', ( #182976 ), #199977, .F. ) ;
#225051 = DIRECTION ( 'NONE',  ( 1.000000000000000000, 0.000000000000000000, 0.000000000000000000 ) ) ;
#225052 = CARTESIAN_POINT ( 'NONE',  ( 21.05000000000000071, 8.815452279208702890, -41.92039255261426689 ) ) ;
#225053 = CIRCLE ( 'NONE', #175067, 0.09999999999998898659 ) ;
#225054 = ORIENTED_EDGE ( 'NONE', *, *, #129954, .T. ) ;
#225055 = DIRECTION ( 'NONE',  ( 0.000000000000000000, 0.000000000000000000, -1.000000000000000000 ) ) ;
#225056 = CIRCLE ( 'NONE', #54391, 0.09999999999999939493 ) ;
#225058 = ORIENTED_EDGE ( 'NONE', *, *, #59055, .T. ) ;
#225057 = CARTESIAN_POINT ( 'NONE',  ( 18.59999999999999076, 65.79142135624910281, -81.67310748452439384 ) ) ;
#225059 = DIRECTION ( 'NONE',  ( 0.000000000000000000, 1.000000000000000000, 0.000000000000000000 ) ) ;
#225060 = FACE_OUTER_BOUND ( 'NONE', #87120, .T. ) ;
#225061 = CARTESIAN_POINT ( 'NONE',  ( -16.92778301347296122, 10.00094491684659381, -87.92851810796820189 ) ) ;
#225062 = DIRECTION ( 'NONE',  ( 0.000000000000000000, 0.000000000000000000, -1.000000000000000000 ) ) ;
#225063 = CARTESIAN_POINT ( 'NONE',  ( 18.59999999999999432, 7.661991824395936845, -241.5144583139544636 ) ) ;
#225064 = DIRECTION ( 'NONE',  ( 0.000000000000000000, -0.2617529984165031243, -0.9651348961777157509 ) ) ;
#225065 = ORIENTED_EDGE ( 'NONE', *, *, #158787, .F. ) ;
#225066 = EDGE_CURVE ( 'NONE', #14833, #254925, #62605, .T. ) ;
#225067 = CARTESIAN_POINT ( 'NONE',  ( -20.93284271247462058, 11.74999999999999645, -26.48519422934604961 ) ) ;
#225068 = VECTOR ( 'NONE', #27772, 1000.000000000000000 ) ;
#225069 = PLANE ( 'NONE',  #102337 ) ;
#225070 = DIRECTION ( 'NONE',  ( -0.000000000000000000, -0.9126074666063771490, -0.4088369013363281623 ) ) ;
#225071 = VECTOR ( 'NONE', #105688, 1000.000000000000114 ) ;
#225072 = FACE_OUTER_BOUND ( 'NONE', #44181, .T. ) ;
#225073 = VECTOR ( 'NONE', #60802, 1000.000000000000000 ) ;
#225074 = ORIENTED_EDGE ( 'NONE', *, *, #205978, .F. ) ;
#225075 = EDGE_LOOP ( 'NONE', ( #103761, #15977, #71020, #26359 ) ) ;
#225076 = CARTESIAN_POINT ( 'NONE',  ( -21.05000000000000071, 47.95459712139159336, -246.5019368548292675 ) ) ;
#225077 = EDGE_CURVE ( 'NONE', #68027, #239535, #8431, .T. ) ;
#225078 = CARTESIAN_POINT ( 'NONE',  ( -20.54999999999999716, -8.999999999988844479, -91.00603087734759811 ) ) ;
#225080 = EDGE_CURVE ( 'NONE', #213808, #71516, #41776, .T. ) ;
#225079 = DIRECTION ( 'NONE',  ( 0.000000000000000000, -0.5000000000000144329, -0.8660254037844302699 ) ) ;
#225081 = FACE_OUTER_BOUND ( 'NONE', #208594, .T. ) ;
#225082 = EDGE_CURVE ( 'NONE', #1731, #247713, #254112, .T. ) ;
#225083 = EDGE_CURVE ( 'NONE', #183267, #14291, #85101, .T. ) ;
#225084 = CARTESIAN_POINT ( 'NONE',  ( -22.47071067811865319, 0.09909245471376171288, -92.77992525550196490 ) ) ;
#225085 = CARTESIAN_POINT ( 'NONE',  ( -23.25000000000000000, 64.25000000001195133, -103.0231074845244024 ) ) ;
#225086 = AXIS2_PLACEMENT_3D ( 'NONE', #192843, #252785, #254073 ) ;
#225087 = CARTESIAN_POINT ( 'NONE',  ( -20.99780126800909841, 16.99738886486947465, -224.5087459288188256 ) ) ;
#225088 = EDGE_CURVE ( 'NONE', #59827, #255696, #76474, .T. ) ;
#225089 = EDGE_CURVE ( 'NONE', #92784, #132009, #182267, .T. ) ;
#225090 = ORIENTED_EDGE ( 'NONE', *, *, #186855, .T. ) ;
#225091 = DIRECTION ( 'NONE',  ( 0.000000000000000000, 0.000000000000000000, -1.000000000000000000 ) ) ;
#225092 = ORIENTED_EDGE ( 'NONE', *, *, #9843, .F. ) ;
#225093 = DIRECTION ( 'NONE',  ( 0.000000000000000000, 0.4930308989875230585, 0.8700118002898322711 ) ) ;
#225094 = DIRECTION ( 'NONE',  ( 0.000000000000000000, -0.4999999999999088507, 0.8660254037844913322 ) ) ;
#225096 = EDGE_CURVE ( 'NONE', #250042, #126428, #241655, .T. ) ;
#225095 = DIRECTION ( 'NONE',  ( 1.000000000000000000, 0.000000000000000000, 0.000000000000000000 ) ) ;
#225097 = LINE ( 'NONE', #10911, #240677 ) ;
#225098 = CARTESIAN_POINT ( 'NONE',  ( -16.77828822508139694, 9.946229374931901290, -46.16262825137395254 ) ) ;
#225099 = CARTESIAN_POINT ( 'NONE',  ( -5.999999999999938716, 64.25000000001119815, -22.12310748452479103 ) ) ;
#225100 = CARTESIAN_POINT ( 'NONE',  ( -23.49999999999994316, 87.75000000001119815, -3.123107484524795474 ) ) ;
#225101 = FACE_OUTER_BOUND ( 'NONE', #157053, .T. ) ;
#225102 = CARTESIAN_POINT ( 'NONE',  ( 22.47071067811864964, 0.09909245471376176839, -92.77992525550199332 ) ) ;
#225103 = AXIS2_PLACEMENT_3D ( 'NONE', #76991, #174869, #78267 ) ;
#225104 = EDGE_CURVE ( 'NONE', #204482, #195703, #228914, .T. ) ;
#225105 = DIRECTION ( 'NONE',  ( 0.000000000000000000, 0.9525900758537791946, -0.3042567129660269099 ) ) ;
#225106 = AXIS2_PLACEMENT_3D ( 'NONE', #186576, #65320, #109574 ) ;
#225107 = LINE ( 'NONE', #202993, #144018 ) ;
#225108 = PLANE ( 'NONE',  #152161 ) ;
#225109 = CIRCLE ( 'NONE', #133553, 0.09999999999999939493 ) ;
#225110 = ADVANCED_FACE ( 'NONE', ( #142534 ), #43451, .F. ) ;
#225111 = ADVANCED_FACE ( 'NONE', ( #168587 ), #162573, .T. ) ;
#225112 = DIRECTION ( 'NONE',  ( 0.000000000000000000, 2.891205793294679805E-16, -1.000000000000000000 ) ) ;
#225113 = CARTESIAN_POINT ( 'NONE',  ( 20.99142135623731065, 64.40000000001248281, -176.9513107147999449 ) ) ;
#225114 = TOROIDAL_SURFACE ( 'NONE', #4369, 11.70000000000000107, 0.1000000000000000056 ) ;
#225115 = ORIENTED_EDGE ( 'NONE', *, *, #130866, .T. ) ;
#225116 = CARTESIAN_POINT ( 'NONE',  ( -18.50000000000000000, 11.65000000000000036, -33.50000000000000000 ) ) ;
#225118 = ADVANCED_FACE ( 'NONE', ( #185530 ), #245512, .T. ) ;
#225117 = DIRECTION ( 'NONE',  ( 0.000000000000000000, 1.000000000000000000, 6.982962677686266711E-15 ) ) ;
#225119 = ORIENTED_EDGE ( 'NONE', *, *, #96506, .T. ) ;
#225120 = CARTESIAN_POINT ( 'NONE',  ( -23.25000000000000000, 7.021664781911246322, -70.83356540189728889 ) ) ;
#225121 = CARTESIAN_POINT ( 'NONE',  ( -20.85000000000000142, 45.93315328338058379, -256.6017782078560003 ) ) ;
#225122 = ADVANCED_FACE ( 'NONE', ( #108561 ), #171149, .F. ) ;
#225123 = TOROIDAL_SURFACE ( 'NONE', #183463, 0.2000000000000000111, 0.1000000000000000056 ) ;
#225124 = ADVANCED_FACE ( 'NONE', ( #26468 ), #70996, .F. ) ;
#225125 = DIRECTION ( 'NONE',  ( 0.000000000000000000, 0.000000000000000000, 1.000000000000000000 ) ) ;
#225126 = ORIENTED_EDGE ( 'NONE', *, *, #166144, .F. ) ;
#225127 = CARTESIAN_POINT ( 'NONE',  ( 20.73486653747088226, 7.250000000011182166, -180.1499999999999773 ) ) ;
#225128 = DIRECTION ( 'NONE',  ( 0.000000000000000000, 0.000000000000000000, 1.000000000000000000 ) ) ;
#225129 = ADVANCED_FACE ( 'NONE', ( #150269 ), #96076, .T. ) ;
#225130 = ORIENTED_EDGE ( 'NONE', *, *, #117481, .T. ) ;
#225131 = DIRECTION ( 'NONE',  ( -1.000000000000000000, -0.000000000000000000, 0.000000000000000000 ) ) ;
#225132 = ORIENTED_EDGE ( 'NONE', *, *, #212284, .T. ) ;
#225133 = EDGE_CURVE ( 'NONE', #95988, #213361, #58004, .T. ) ;
#225134 = CARTESIAN_POINT ( 'NONE',  ( -22.39999999999999858, 68.20922040163824818, -69.52310748452437394 ) ) ;
#225135 = AXIS2_PLACEMENT_3D ( 'NONE', #244649, #208123, #30775 ) ;
#225136 = DIRECTION ( 'NONE',  ( -1.000000000000000000, 0.000000000000000000, 0.000000000000000000 ) ) ;
#225137 = FACE_OUTER_BOUND ( 'NONE', #189055, .T. ) ;
#225139 = DIRECTION ( 'NONE',  ( 0.000000000000000000, 0.9910827722268055195, 0.1332476588733540468 ) ) ;
#225138 = UNCERTAINTY_MEASURE_WITH_UNIT (LENGTH_MEASURE( 1.000000000000000082E-05 ), #185556, 'distance_accuracy_value', 'NONE');
#225140 = CYLINDRICAL_SURFACE ( 'NONE', #221094, 0.1000000000000028644 ) ;
#225141 = FACE_OUTER_BOUND ( 'NONE', #103384, .T. ) ;
#225142 = AXIS2_PLACEMENT_3D ( 'NONE', #225057, #46432, #26912 ) ;
#225143 = LINE ( 'NONE', #126050, #122090 ) ;
#225144 = DIRECTION ( 'NONE',  ( 1.296989514748957922E-15, 0.9887567792719351711, -0.1495327102803594987 ) ) ;
#225146 = ORIENTED_EDGE ( 'NONE', *, *, #62932, .T. ) ;
#225145 = CARTESIAN_POINT ( 'NONE',  ( 23.24999999999999645, 1.115600667400684642E-11, -134.0000000000000284 ) ) ;
#225147 = ORIENTED_EDGE ( 'NONE', *, *, #141465, .F. ) ;
#225149 = SPHERICAL_SURFACE ( 'NONE', #202052, 0.1000000000000000056 ) ;
#225148 = CARTESIAN_POINT ( 'NONE',  ( 18.57071067811864040, 10.17928932188134539, -21.25000000000000000 ) ) ;
#225151 = ORIENTED_EDGE ( 'NONE', *, *, #189997, .T. ) ;
#225150 = CARTESIAN_POINT ( 'NONE',  ( 20.95346350065193519, 8.887177249185651107, -109.0117319470354289 ) ) ;
#225152 = AXIS2_PLACEMENT_3D ( 'NONE', #216207, #59689, #199240 ) ;
#225153 = ORIENTED_EDGE ( 'NONE', *, *, #208280, .T. ) ;
#225154 = CARTESIAN_POINT ( 'NONE',  ( 19.95857864376268864, 5.488301202077012775, 16.50000000000000000 ) ) ;
#225155 = CARTESIAN_POINT ( 'NONE',  ( 23.14999999999999858, 67.23127455305835554, -235.8551265064784559 ) ) ;
#225156 = CARTESIAN_POINT ( 'NONE',  ( -23.15000000000000213, -8.999999999988844479, -124.1060308773475924 ) ) ;
#225157 = CIRCLE ( 'NONE', #246039, 0.1000000000000008937 ) ;
#225158 = LINE ( 'NONE', #47808, #198452 ) ;
#225159 = CARTESIAN_POINT ( 'NONE',  ( -18.53317502108577131, 67.49276774653023381, -195.4544018784149841 ) ) ;
#225160 = FACE_OUTER_BOUND ( 'NONE', #231744, .T. ) ;
#225161 = CARTESIAN_POINT ( 'NONE',  ( 18.59999999999999787, 1.115600667400684642E-11, -100.5000000000000284 ) ) ;
#225163 = ORIENTED_EDGE ( 'NONE', *, *, #47264, .F. ) ;
#225162 = EDGE_CURVE ( 'NONE', #150112, #87393, #91565, .T. ) ;
#225164 = VERTEX_POINT ( 'NONE', #169867 ) ;
#225165 = LINE ( 'NONE', #244737, #77236 ) ;
#225166 = TOROIDAL_SURFACE ( 'NONE', #112771, 1.900000000000002576, 0.1000000000000000056 ) ;
#225167 = ADVANCED_FACE ( 'NONE', ( #167280 ), #250622, .T. ) ;
#225168 = ORIENTED_EDGE ( 'NONE', *, *, #211559, .F. ) ;
#225169 = CARTESIAN_POINT ( 'NONE',  ( -21.05000000000000071, 1.360870587192041681, -8.072997927090961312 ) ) ;
#225171 = ORIENTED_EDGE ( 'NONE', *, *, #244882, .F. ) ;
#225170 = AXIS2_PLACEMENT_3D ( 'NONE', #86611, #166214, #47492 ) ;
#225172 = CIRCLE ( 'NONE', #112778, 4.050000000000002487 ) ;
#225173 = CIRCLE ( 'NONE', #79619, 4.300000000000025580 ) ;
#225174 = DIRECTION ( 'NONE',  ( 0.000000000000000000, 0.000000000000000000, -1.000000000000000000 ) ) ;
#225175 = ADVANCED_FACE ( 'NONE', ( #88975 ), #6883, .F. ) ;
#225177 = ADVANCED_FACE ( 'NONE', ( #228520 ), #70746, .F. ) ;
#225176 = CARTESIAN_POINT ( 'NONE',  ( 21.00000000000000000, 66.25000000001260503, -191.2731074845244166 ) ) ;
#225178 = CARTESIAN_POINT ( 'NONE',  ( 21.87500000000000355, 51.97441255244040548, -232.0063394385699667 ) ) ;
#225179 = ORIENTED_EDGE ( 'NONE', *, *, #113555, .T. ) ;
#225180 = AXIS2_PLACEMENT_3D ( 'NONE', #47907, #247391, #11366 ) ;
#225182 = CIRCLE ( 'NONE', #112787, 0.09999999999999939493 ) ;
#225181 = CARTESIAN_POINT ( 'NONE',  ( -21.00219873199058540, 11.60538868787663702, -6.912647428294775409 ) ) ;
#225183 = ORIENTED_EDGE ( 'NONE', *, *, #148924, .T. ) ;
#225184 = DIRECTION ( 'NONE',  ( 0.000000000000000000, 1.000000000000000000, 0.000000000000000000 ) ) ;
#225185 = CARTESIAN_POINT ( 'NONE',  ( -23.25000000000000000, 78.57213941646344324, -232.7862224702232652 ) ) ;
#225186 = DIRECTION ( 'NONE',  ( -1.020425574104004196E-15, 6.982962677686266711E-15, -1.000000000000000000 ) ) ;
#225187 = DIRECTION ( 'NONE',  ( 0.000000000000000000, 0.000000000000000000, -1.000000000000000000 ) ) ;
#225188 = ORIENTED_EDGE ( 'NONE', *, *, #171140, .T. ) ;
#225189 = CARTESIAN_POINT ( 'NONE',  ( -20.94999999999999929, 62.93978069479755533, -206.9800818407681220 ) ) ;
#225190 = ORIENTED_EDGE ( 'NONE', *, *, #204204, .F. ) ;
#225193 = VERTEX_POINT ( 'NONE', #68149 ) ;
#225192 = CARTESIAN_POINT ( 'NONE',  ( 23.40000000000005542, 74.26359666348515987, -47.54092689884382850 ) ) ;
#225191 = LINE ( 'NONE', #109105, #115997 ) ;
#225194 = CARTESIAN_POINT ( 'NONE',  ( 22.39999999999999503, 11.75000000001116263, -167.3999999999999773 ) ) ;
#225196 = EDGE_LOOP ( 'NONE', ( #198851, #231591, #35823, #190871 ) ) ;
#225195 = AXIS2_PLACEMENT_3D ( 'NONE', #96121, #152293, #54439 ) ;
#225197 = AXIS2_PLACEMENT_3D ( 'NONE', #91610, #37767, #57279 ) ;
#225198 = AXIS2_PLACEMENT_3D ( 'NONE', #110565, #248810, #188819 ) ;
#225199 = DIRECTION ( 'NONE',  ( 1.000000000000000000, 2.952720810173289112E-16, -0.000000000000000000 ) ) ;
#225200 = ORIENTED_EDGE ( 'NONE', *, *, #5967, .F. ) ;
#225201 = LINE ( 'NONE', #46569, #22342 ) ;
#225202 = DIRECTION ( 'NONE',  ( 0.000000000000000000, -1.000000000000000000, -6.982962677686265922E-15 ) ) ;
#225203 = DIRECTION ( 'NONE',  ( 1.000000000000000000, 0.000000000000000000, 0.000000000000000000 ) ) ;
#225204 = CARTESIAN_POINT ( 'NONE',  ( -17.80356949363931918, 53.39653902550993081, -230.1346155703532759 ) ) ;
#225205 = CARTESIAN_POINT ( 'NONE',  ( -16.87487986503753845, 9.950007555085599975, -12.64997473968673347 ) ) ;
#225206 = AXIS2_PLACEMENT_3D ( 'NONE', #218855, #178492, #101439 ) ;
#225207 = VERTEX_POINT ( 'NONE', #229786 ) ;
#225208 = FACE_OUTER_BOUND ( 'NONE', #89340, .T. ) ;
#225209 = CARTESIAN_POINT ( 'NONE',  ( -14.87779219673431363, 66.56936653093950440, -154.7913416897003742 ) ) ;
#225210 = ORIENTED_EDGE ( 'NONE', *, *, #82912, .T. ) ;
#225211 = ADVANCED_FACE ( 'NONE', ( #125551 ), #205068, .F. ) ;
#225212 = DIRECTION ( 'NONE',  ( 0.000000000000000000, 0.000000000000000000, 1.000000000000000000 ) ) ;
#225213 = ORIENTED_EDGE ( 'NONE', *, *, #140857, .T. ) ;
#225214 = CARTESIAN_POINT ( 'NONE',  ( 21.13614978966382552, 30.72779294459459720, -252.2082365290035284 ) ) ;
#225215 = DIRECTION ( 'NONE',  ( -0.000000000000000000, 1.000000000000000000, 6.982962677686266711E-15 ) ) ;
#225216 = DIRECTION ( 'NONE',  ( 0.000000000000000000, 0.000000000000000000, -1.000000000000000000 ) ) ;
#225218 = ORIENTED_EDGE ( 'NONE', *, *, #180931, .T. ) ;
#225217 = CARTESIAN_POINT ( 'NONE',  ( -16.87683809663752399, 44.86297841676467613, -235.0825981793917379 ) ) ;
#225219 = LINE ( 'NONE', #23227, #241993 ) ;
#225220 = EDGE_CURVE ( 'NONE', #180952, #116556, #54398, .T. ) ;
#225221 = AXIS2_PLACEMENT_3D ( 'NONE', #114600, #35104, #113311 ) ;
#225222 = LINE ( 'NONE', #188684, #94227 ) ;
#225223 = DIRECTION ( 'NONE',  ( 0.000000000000000000, 0.000000000000000000, -1.000000000000000000 ) ) ;
#225224 = EDGE_CURVE ( 'NONE', #132493, #135164, #41954, .T. ) ;
#225225 = ORIENTED_EDGE ( 'NONE', *, *, #76402, .F. ) ;
#225226 = SPHERICAL_SURFACE ( 'NONE', #72651, 0.1000000000000000056 ) ;
#225227 = CARTESIAN_POINT ( 'NONE',  ( 21.14999999999999858, 6.649999999999999467, -12.15000000000000036 ) ) ;
#225228 = EDGE_LOOP ( 'NONE', ( #151597, #156803, #73722, #44390 ) ) ;
#225229 = CARTESIAN_POINT ( 'NONE',  ( 22.48660254037844197, 64.35000000001237197, -170.0731074845244564 ) ) ;
#225230 = TOROIDAL_SURFACE ( 'NONE', #146151, 0.2000000000000000111, 0.1000000000000000056 ) ;
#225231 = ORIENTED_EDGE ( 'NONE', *, *, #141080, .T. ) ;
#225232 = EDGE_CURVE ( 'NONE', #31046, #34062, #79318, .T. ) ;
#225234 = CARTESIAN_POINT ( 'NONE',  ( -16.85939591225058010, 44.43675737074195098, -235.2130249156476793 ) ) ;
#225233 = AXIS2_PLACEMENT_3D ( 'NONE', #105041, #107652, #184622 ) ;
#225236 = ORIENTED_EDGE ( 'NONE', *, *, #218691, .T. ) ;
#225235 = DIRECTION ( 'NONE',  ( -0.000000000000000000, -0.8700118002898321601, 0.4930308989875230030 ) ) ;
#225237 = ADVANCED_FACE ( 'NONE', ( #95414 ), #75279, .F. ) ;
#225238 = EDGE_CURVE ( 'NONE', #177774, #63643, #46016, .T. ) ;
#225241 = EDGE_LOOP ( 'NONE', ( #131704, #257256, #44101, #47605, #240978 ) ) ;
#225240 = ORIENTED_EDGE ( 'NONE', *, *, #102032, .T. ) ;
#225239 = CARTESIAN_POINT ( 'NONE',  ( -21.14999999999999858, 76.10085836911045476, -81.27267460801371612 ) ) ;
#225242 = CARTESIAN_POINT ( 'NONE',  ( 21.14999999999999858, 31.98723526783714988, -238.8784020251475511 ) ) ;
#225243 = CARTESIAN_POINT ( 'NONE',  ( -23.25000000000000000, 21.13195309841794867, -243.6318585593224100 ) ) ;
#225244 = DIRECTION ( 'NONE',  ( 0.000000000000000000, 0.2617529984165152257, 0.9651348961777124202 ) ) ;
#225245 = ADVANCED_FACE ( 'NONE', ( #57553 ), #255727, .F. ) ;
#225247 = DIRECTION ( 'NONE',  ( -0.000000000000000000, 0.9274965247785350586, 0.3738317757009704811 ) ) ;
#225246 = CARTESIAN_POINT ( 'NONE',  ( -17.11825945287481332, 62.98921886345645760, -213.1014462870871569 ) ) ;
#225248 = LINE ( 'NONE', #186150, #132035 ) ;
#225249 = DIRECTION ( 'NONE',  ( 1.000000000000000000, 0.000000000000000000, 0.000000000000000000 ) ) ;
#225250 = VECTOR ( 'NONE', #20456, 1000.000000000000000 ) ;
#225251 = CARTESIAN_POINT ( 'NONE',  ( -23.25000000000000000, 64.25000000001196554, -110.0379132551783243 ) ) ;
#225252 = CIRCLE ( 'NONE', #112858, 11.70000000000000817 ) ;
#225253 = DIRECTION ( 'NONE',  ( 1.000000000000000000, 0.000000000000000000, 0.000000000000000000 ) ) ;
#225254 = CARTESIAN_POINT ( 'NONE',  ( -22.60000000000094289, 75.89914163091371790, -148.2726746080137161 ) ) ;
#225255 = ORIENTED_EDGE ( 'NONE', *, *, #1956, .T. ) ;
#225256 = ORIENTED_EDGE ( 'NONE', *, *, #175466, .F. ) ;
#225257 = CARTESIAN_POINT ( 'NONE',  ( -20.99551997958379701, 64.25000000001176659, -76.37144834683515171 ) ) ;
#225259 = EDGE_LOOP ( 'NONE', ( #13161, #81719, #254849, #202078 ) ) ;
#225258 = DIRECTION ( 'NONE',  ( 1.000000000000000000, -0.000000000000000000, 0.000000000000000000 ) ) ;
#225260 = ORIENTED_EDGE ( 'NONE', *, *, #67051, .F. ) ;
#225261 = EDGE_CURVE ( 'NONE', #41443, #6405, #50285, .T. ) ;
#225262 = CARTESIAN_POINT ( 'NONE',  ( 21.00023020733438273, 6.390869245278871347, -100.5000000000000426 ) ) ;
#225263 =( BOUNDED_CURVE ( )  B_SPLINE_CURVE ( 3, ( #57282, #19475, #74342, #55993 ),
 .UNSPECIFIED., .F., .F. ) 
 B_SPLINE_CURVE_WITH_KNOTS ( ( 4, 4 ),
 ( 0.06456096931748307732, 3.077031684272310219 ),
 .UNSPECIFIED. ) 
 CURVE ( )  GEOMETRIC_REPRESENTATION_ITEM ( )  RATIONAL_B_SPLINE_CURVE ( ( 1.000000000000000000, 0.3763440860215093164, 0.3763440860215093164, 1.000000000000000000 ) ) 
 REPRESENTATION_ITEM ( '' )  );
#225264 = EDGE_LOOP ( 'NONE', ( #155100, #192661, #139039, #248325, #1471, #72092, #45299, #96756, #100741 ) ) ;
#225265 = CARTESIAN_POINT ( 'NONE',  ( 23.24999999999999645, 2.100000000011158274, -100.5000000000000426 ) ) ;
#225266 = ORIENTED_EDGE ( 'NONE', *, *, #47322, .F. ) ;
#225267 = AXIS2_PLACEMENT_3D ( 'NONE', #78001, #19322, #134118 ) ;
#225268 = DIRECTION ( 'NONE',  ( -1.000000000000000000, 0.000000000000000000, -0.000000000000000000 ) ) ;
#225269 = CARTESIAN_POINT ( 'NONE',  ( -20.64999999999999858, 7.249999999999999112, -12.25000000000000000 ) ) ;
#225271 = ORIENTED_EDGE ( 'NONE', *, *, #56179, .F. ) ;
#225270 = VERTEX_POINT ( 'NONE', #236203 ) ;
#225272 = ORIENTED_EDGE ( 'NONE', *, *, #30549, .T. ) ;
#225273 = FACE_OUTER_BOUND ( 'NONE', #230110, .T. ) ;
#225274 = VERTEX_POINT ( 'NONE', #116280 ) ;
#225275 = ORIENTED_EDGE ( 'NONE', *, *, #250943, .T. ) ;
#225276 = CARTESIAN_POINT ( 'NONE',  ( -21.05000000000000071, 87.48912529308769592, -66.42310748452423752 ) ) ;
#225277 = FACE_OUTER_BOUND ( 'NONE', #21039, .T. ) ;
#225279 = EDGE_LOOP ( 'NONE', ( #61648, #104737, #175895, #123386 ) ) ;
#225278 = LINE ( 'NONE', #124931, #255840 ) ;
#225280 = DIRECTION ( 'NONE',  ( 1.000000000000000000, 0.000000000000000000, 0.000000000000000000 ) ) ;
#225281 = DIRECTION ( 'NONE',  ( 0.000000000000000000, -1.000000000000000000, -8.717686153663073805E-15 ) ) ;
#225283 = ORIENTED_EDGE ( 'NONE', *, *, #157293, .T. ) ;
#225282 = CARTESIAN_POINT ( 'NONE',  ( 20.94999999999999929, 85.00000000001222134, -146.4170766071767389 ) ) ;
#225284 = FACE_OUTER_BOUND ( 'NONE', #230134, .T. ) ;
#225285 = ORIENTED_EDGE ( 'NONE', *, *, #218611, .F. ) ;
#225286 = DIRECTION ( 'NONE',  ( -0.7071067811865214825, -0.7071067811865735520, 0.000000000000000000 ) ) ;
#225287 = EDGE_LOOP ( 'NONE', ( #8884, #9816, #52286, #233057 ) ) ;
#225288 = DIRECTION ( 'NONE',  ( 1.000000000000000000, 0.000000000000000000, 0.000000000000000000 ) ) ;
#225289 = DIRECTION ( 'NONE',  ( 0.000000000000000000, 0.000000000000000000, -1.000000000000000000 ) ) ;
#225290 = AXIS2_PLACEMENT_3D ( 'NONE', #9714, #110103, #189652 ) ;
#225291 = TOROIDAL_SURFACE ( 'NONE', #158887, 4.149999999999999467, 0.1000000000000000056 ) ;
#225292 = AXIS2_PLACEMENT_3D ( 'NONE', #255811, #194634, #236290 ) ;
#225293 = ORIENTED_EDGE ( 'NONE', *, *, #163938, .T. ) ;
#225295 = DIRECTION ( 'NONE',  ( 1.000000000000000000, 1.836970198721029934E-16, 0.000000000000000000 ) ) ;
#225294 = CARTESIAN_POINT ( 'NONE',  ( 21.07928932188134397, 0.09889514566555242248, -27.17148334360669537 ) ) ;
#225296 = EDGE_CURVE ( 'NONE', #185475, #203922, #114978, .T. ) ;
#225297 = CARTESIAN_POINT ( 'NONE',  ( -17.11825945287482753, 9.949999999999983302, -12.75000000000000178 ) ) ;
#225298 = AXIS2_PLACEMENT_3D ( 'NONE', #17572, #119272, #219628 ) ;
#225299 = CARTESIAN_POINT ( 'NONE',  ( -18.34374000495060386, 20.70020979027691155, -227.9869476361872103 ) ) ;
#225300 = ORIENTED_EDGE ( 'NONE', *, *, #144550, .F. ) ;
#225301 = ORIENTED_EDGE ( 'NONE', *, *, #249325, .T. ) ;
#225302 = CARTESIAN_POINT ( 'NONE',  ( 23.25000000000000000, -11.48912529306489994, -63.89999999999999858 ) ) ;
#225303 = CARTESIAN_POINT ( 'NONE',  ( -20.94999999999999929, 79.07891399537199106, -236.0635483022085452 ) ) ;
#225304 = ORIENTED_EDGE ( 'NONE', *, *, #149141, .T. ) ;
#225305 = FACE_OUTER_BOUND ( 'NONE', #238333, .T. ) ;
#225306 = ORIENTED_EDGE ( 'NONE', *, *, #219762, .F. ) ;
#225307 = LINE ( 'NONE', #165367, #114972 ) ;
#225308 = ADVANCED_FACE ( 'NONE', ( #56269 ), #72015, .F. ) ;
#225309 = EDGE_LOOP ( 'NONE', ( #225375, #219367, #46442, #44618 ) ) ;
#225310 = DIRECTION ( 'NONE',  ( -0.000000000000000000, -0.000000000000000000, 1.000000000000000000 ) ) ;
#225311 = AXIS2_PLACEMENT_3D ( 'NONE', #53515, #250426, #152649 ) ;
#225312 = DIRECTION ( 'NONE',  ( -0.000000000000000000, 0.8660254037844411501, 0.4999999999999956146 ) ) ;
#225313 = DIRECTION ( 'NONE',  ( 0.000000000000000000, 0.000000000000000000, 1.000000000000000000 ) ) ;
#225314 = EDGE_CURVE ( 'NONE', #165490, #61312, #91994, .T. ) ;
#225315 = EDGE_CURVE ( 'NONE', #46937, #143803, #97953, .T. ) ;
#225316 = ORIENTED_EDGE ( 'NONE', *, *, #67095, .F. ) ;
#225317 = CARTESIAN_POINT ( 'NONE',  ( 18.47135592147651195, -9.471088613254559974, -207.6835949398434309 ) ) ;
#225318 =( NAMED_UNIT ( * ) PLANE_ANGLE_UNIT ( ) SI_UNIT ( $, .RADIAN. ) );
#225319 = ORIENTED_EDGE ( 'NONE', *, *, #200583, .T. ) ;
#225320 = ORIENTED_EDGE ( 'NONE', *, *, #198290, .F. ) ;
#225321 = VERTEX_POINT ( 'NONE', #133261 ) ;
#225322 = DIRECTION ( 'NONE',  ( 0.000000000000000000, 0.000000000000000000, -1.000000000000000000 ) ) ;
#225323 = CARTESIAN_POINT ( 'NONE',  ( 20.94999999999999929, 5.000000000011153745, -155.0947339810869323 ) ) ;
#225324 = DIRECTION ( 'NONE',  ( -1.000000000000000000, 0.000000000000000000, 0.000000000000000000 ) ) ;
#225325 = CARTESIAN_POINT ( 'NONE',  ( -22.39999999999999858, 64.35000000001268461, -203.5231074845244166 ) ) ;
#225326 = CARTESIAN_POINT ( 'NONE',  ( 21.05000000000000071, -8.663551401869158397, -9.524101118067305194 ) ) ;
#225327 = ADVANCED_FACE ( 'NONE', ( #13318 ), #96660, .T. ) ;
#225328 = AXIS2_PLACEMENT_3D ( 'NONE', #211022, #28586, #188889 ) ;
#225330 = DIRECTION ( 'NONE',  ( 1.000000000000000000, 0.000000000000000000, 0.000000000000000000 ) ) ;
#225329 = CARTESIAN_POINT ( 'NONE',  ( 18.59999999999999432, 77.29973367124323147, -179.9949779616549392 ) ) ;
#225332 = VERTEX_POINT ( 'NONE', #253195 ) ;
#225331 = DIRECTION ( 'NONE',  ( 0.000000000000000000, 0.2617529984165152257, 0.9651348961777124202 ) ) ;
#225333 = CARTESIAN_POINT ( 'NONE',  ( -23.25000000000000000, 1.115600667400684642E-11, -134.0000000000000000 ) ) ;
#225334 = EDGE_LOOP ( 'NONE', ( #26057, #167914, #129779, #244872 ) ) ;
#225335 = ADVANCED_FACE ( 'NONE', ( #52419 ), #131971, .T. ) ;
#225336 = LINE ( 'NONE', #84513, #109256 ) ;
#225337 = ORIENTED_EDGE ( 'NONE', *, *, #105775, .F. ) ;
#225338 = VERTEX_POINT ( 'NONE', #172430 ) ;
#225339 = DIRECTION ( 'NONE',  ( 0.000000000000000000, -0.05616704890741856110, 0.9984213852963245150 ) ) ;
#225340 = AXIS2_PLACEMENT_3D ( 'NONE', #142645, #222174, #66982 ) ;
#225341 = CARTESIAN_POINT ( 'NONE',  ( -16.94180778212363236, 9.992443055743304825, -46.10418357053324456 ) ) ;
#225342 = FACE_OUTER_BOUND ( 'NONE', #67227, .T. ) ;
#225343 = FACE_OUTER_BOUND ( 'NONE', #109250, .T. ) ;
#225344 = PRODUCT_RELATED_PRODUCT_CATEGORY ( 'part', '', ( #203297 ) ) ;
#225345 = VECTOR ( 'NONE', #186084, 1000.000000000000000 ) ;
#225346 = DIRECTION ( 'NONE',  ( 1.000000000000000000, -0.000000000000000000, -0.000000000000000000 ) ) ;
#225347 = AXIS2_PLACEMENT_3D ( 'NONE', #225986, #27859, #47366 ) ;
#225348 = VERTEX_POINT ( 'NONE', #251916 ) ;
#225349 = VERTEX_POINT ( 'NONE', #212808 ) ;
#225350 = EDGE_CURVE ( 'NONE', #53100, #221732, #129414, .T. ) ;
#225351 = AXIS2_PLACEMENT_3D ( 'NONE', #30101, #112208, #108335 ) ;
#225352 = CARTESIAN_POINT ( 'NONE',  ( -18.59999999999999787, -1.835859311443637010, -45.00443916879852679 ) ) ;
#225354 = EDGE_LOOP ( 'NONE', ( #143992, #241348, #145745, #59351 ) ) ;
#225353 = EDGE_CURVE ( 'NONE', #250736, #163271, #53717, .T. ) ;
#225355 = DIRECTION ( 'NONE',  ( 0.000000000000000000, 0.2617529984163859957, 0.9651348961777475033 ) ) ;
#225356 = CARTESIAN_POINT ( 'NONE',  ( -20.54999999999999716, 62.08591502004791352, -248.5699171172615820 ) ) ;
#225357 = EDGE_CURVE ( 'NONE', #156950, #29429, #173724, .T. ) ;
#225358 = DIRECTION ( 'NONE',  ( 0.000000000000000000, 0.8741572761215371523, -0.4856429311786332748 ) ) ;
#225359 = DIRECTION ( 'NONE',  ( 1.000000000000000000, 3.265361837132813093E-16, -0.000000000000000000 ) ) ;
#225360 = CARTESIAN_POINT ( 'NONE',  ( -16.93388492042258164, 66.01145817749616640, -123.9236526077105509 ) ) ;
#225361 = CARTESIAN_POINT ( 'NONE',  ( -20.64999999999999858, 76.00000000001215028, -138.5231074845243313 ) ) ;
#225362 = VERTEX_POINT ( 'NONE', #15910 ) ;
#225363 = CARTESIAN_POINT ( 'NONE',  ( -23.49999999999994316, 64.35000000001120668, -21.92310748452479174 ) ) ;
#225365 = CARTESIAN_POINT ( 'NONE',  ( -21.05000000000000071, 11.62071067812980907, -140.8684166523410681 ) ) ;
#225364 = AXIS2_PLACEMENT_3D ( 'NONE', #60765, #85440, #165017 ) ;
#225366 = CARTESIAN_POINT ( 'NONE',  ( -18.40000000000000213, 53.37686160793744961, -235.8706811220569932 ) ) ;
#225367 = DIRECTION ( 'NONE',  ( 0.000000000000000000, -6.982962677686266711E-15, 1.000000000000000000 ) ) ;
#225368 = DIRECTION ( 'NONE',  ( -0.000000000000000000, 0.8814952561688430555, -0.4721928772777346239 ) ) ;
#225369 = AXIS2_PLACEMENT_3D ( 'NONE', #29542, #109030, #30819 ) ;
#225370 = CARTESIAN_POINT ( 'NONE',  ( -21.05000000000000071, 76.00000000001270450, -207.8231074845243143 ) ) ;
#225371 = VERTEX_POINT ( 'NONE', #41888 ) ;
#225373 =( BOUNDED_CURVE ( )  B_SPLINE_CURVE ( 3, ( #111686, #191253, #188654, #226475 ),
 .UNSPECIFIED., .F., .T. ) 
 B_SPLINE_CURVE_WITH_KNOTS ( ( 4, 4 ),
 ( 0.3000847527772389500, 0.5517402753107891744 ),
 .UNSPECIFIED. ) 
 CURVE ( )  GEOMETRIC_REPRESENTATION_ITEM ( )  RATIONAL_B_SPLINE_CURVE ( ( 1.000000000000000000, 0.9947294176030464508, 0.9947294176030464508, 1.000000000000000000 ) ) 
 REPRESENTATION_ITEM ( '' )  );
#225372 = AXIS2_PLACEMENT_3D ( 'NONE', #136230, #193678, #157135 ) ;
#225374 = CARTESIAN_POINT ( 'NONE',  ( -17.11825945287482753, 66.05000000001231797, -157.2731074845244166 ) ) ;
#225375 = ORIENTED_EDGE ( 'NONE', *, *, #106100, .T. ) ;
#225376 = AXIS2_PLACEMENT_3D ( 'NONE', #138568, #219407, #18659 ) ;
#225377 = DIRECTION ( 'NONE',  ( 0.000000000000000000, -1.000000000000000000, 0.000000000000000000 ) ) ;
#225378 = DIRECTION ( 'NONE',  ( 1.000000000000000000, 0.000000000000000000, -0.000000000000000000 ) ) ;
#225379 = CARTESIAN_POINT ( 'NONE',  ( 20.95512828230154767, 61.85861388774331715, -221.7547760186666892 ) ) ;
#225380 = EDGE_LOOP ( 'NONE', ( #138113, #213413, #45130, #3011 ) ) ;
#225381 = EDGE_CURVE ( 'NONE', #193487, #45997, #62716, .T. ) ;
#225382 = DIRECTION ( 'NONE',  ( 2.952720810173289112E-16, 1.000000000000000000, 6.982962677686266711E-15 ) ) ;
#225383 = LINE ( 'NONE', #247538, #152299 ) ;
#225384 = DIRECTION ( 'NONE',  ( -1.000000000000000000, 0.000000000000000000, -0.000000000000000000 ) ) ;
#225385 = DIRECTION ( 'NONE',  ( 1.000000000000000000, 0.000000000000000000, 0.000000000000000000 ) ) ;
#225386 = AXIS2_PLACEMENT_3D ( 'NONE', #59235, #38437, #214498 ) ;
#225387 = CARTESIAN_POINT ( 'NONE',  ( -20.85000000000000142, 7.021664781911246322, -204.8335654018972605 ) ) ;
#225388 = DIRECTION ( 'NONE',  ( 0.000000000000000000, -0.8660254037844412611, -0.4999999999999956701 ) ) ;
#225389 = VECTOR ( 'NONE', #166269, 1000.000000000000114 ) ;
#225390 = VERTEX_POINT ( 'NONE', #79683 ) ;
#225391 = ORIENTED_EDGE ( 'NONE', *, *, #239344, .T. ) ;
#225392 = DIRECTION ( 'NONE',  ( 0.000000000000000000, 0.000000000000000000, -1.000000000000000000 ) ) ;
#225394 = VERTEX_POINT ( 'NONE', #80969 ) ;
#225393 = CARTESIAN_POINT ( 'NONE',  ( 21.05000000000000071, 70.15000000001148805, -46.15560470880229360 ) ) ;
#225395 = DIRECTION ( 'NONE',  ( 0.000000000000000000, -0.9126074666063771490, -0.4088369013363281623 ) ) ;
#225396 = EDGE_CURVE ( 'NONE', #4584, #54157, #142240, .T. ) ;
#225397 = ORIENTED_EDGE ( 'NONE', *, *, #217062, .F. ) ;
#225398 = CARTESIAN_POINT ( 'NONE',  ( 20.94999999999999929, 1.115600667400684642E-11, -104.5000000000000568 ) ) ;
#225399 = EDGE_CURVE ( 'NONE', #55107, #26254, #116946, .T. ) ;
#225401 = B_SPLINE_CURVE_WITH_KNOTS ( 'NONE', 3,
 ( #20751, #97672, #179825, #222765, #58553, #161547, #177272, #160273, #3730, #258003 ),
 .UNSPECIFIED., .F., .F.,
 ( 4, 2, 2, 2, 4 ),
 ( 0.000000000000000000, 3.990160268012413235E-05, 7.980320536024826470E-05, 0.0001596064107204978033, 0.0003192128214410639114 ),
 .UNSPECIFIED. ) ;
#225400 = APPLICATION_PROTOCOL_DEFINITION ( 'draft international standard', 'automotive_design', 1998, #162437 ) ;
#225402 = CARTESIAN_POINT ( 'NONE',  ( 20.94999999999999929, 8.776282895292474961, -21.25000000000000000 ) ) ;
#225403 = ORIENTED_EDGE ( 'NONE', *, *, #78590, .F. ) ;
#225405 = EDGE_CURVE ( 'NONE', #208323, #25427, #139651, .T. ) ;
#225404 = DIRECTION ( 'NONE',  ( 0.000000000000000000, 0.1350103645451835865, 0.9908441862701605762 ) ) ;
#225406 = ADVANCED_FACE ( 'NONE', ( #199678 ), #21041, .T. ) ;
#225407 = ADVANCED_FACE ( 'NONE', ( #24895 ), #221752, .T. ) ;
#225408 = ORIENTED_EDGE ( 'NONE', *, *, #99625, .T. ) ;
#225409 = ORIENTED_EDGE ( 'NONE', *, *, #136292, .T. ) ;
#225410 = CARTESIAN_POINT ( 'NONE',  ( -21.64999999999999858, 68.65000000001187175, -90.77310748452435973 ) ) ;
#225411 = DIRECTION ( 'NONE',  ( -0.000000000000000000, 0.000000000000000000, 1.000000000000000000 ) ) ;
#225412 = CARTESIAN_POINT ( 'NONE',  ( -20.54999999999999716, 66.65000000001259650, -191.2731074845244166 ) ) ;
#225413 = AXIS2_PLACEMENT_3D ( 'NONE', #52713, #31909, #8473 ) ;
#225414 = DIRECTION ( 'NONE',  ( 0.000000000000000000, 1.734723475976757554E-14, -1.000000000000000000 ) ) ;
#225415 = DIRECTION ( 'NONE',  ( -0.000000000000000000, 6.982962677686266711E-15, -1.000000000000000000 ) ) ;
#225416 = CARTESIAN_POINT ( 'NONE',  ( 22.59999999999999787, 55.96169194136206215, -232.9023299069559130 ) ) ;
#225417 = CARTESIAN_POINT ( 'NONE',  ( -18.39999999999999858, 87.08727414655710675, -199.6327537731849873 ) ) ;
#225419 = DIRECTION ( 'NONE',  ( -1.000000000000000000, 0.000000000000000000, 0.000000000000000000 ) ) ;
#225418 = DIRECTION ( 'NONE',  ( 1.186688945009009831E-16, 1.000000000000000000, 6.982962677686266711E-15 ) ) ;
#225420 = FACE_OUTER_BOUND ( 'NONE', #219759, .T. ) ;
#225421 = CYLINDRICAL_SURFACE ( 'NONE', #38113, 14.30833333333333890 ) ;
#225422 = CARTESIAN_POINT ( 'NONE',  ( 20.94999999999999929, 11.65000000001115943, -200.9999999999999432 ) ) ;
#225423 = ORIENTED_EDGE ( 'NONE', *, *, #1783, .F. ) ;
#225424 = EDGE_CURVE ( 'NONE', #48432, #156856, #158668, .T. ) ;
#225425 = ORIENTED_EDGE ( 'NONE', *, *, #226399, .T. ) ;
#225426 = LINE ( 'NONE', #165491, #240017 ) ;
#225427 = EDGE_CURVE ( 'NONE', #222832, #148718, #101803, .T. ) ;
#225428 = DIRECTION ( 'NONE',  ( 0.000000000000000000, 0.8814952561688436106, -0.4721928772777336247 ) ) ;
#225430 = CARTESIAN_POINT ( 'NONE',  ( -14.22969084473442081, 13.17382239637292862, -217.0529139566851597 ) ) ;
#225429 = DIRECTION ( 'NONE',  ( -0.000000000000000000, 0.000000000000000000, 1.000000000000000000 ) ) ;
#225431 = AXIS2_PLACEMENT_3D ( 'NONE', #213168, #55342, #214445 ) ;
#225432 = CARTESIAN_POINT ( 'NONE',  ( 20.95561247346651967, 39.25743729385360581, -236.7774612551371547 ) ) ;
#225434 = EDGE_CURVE ( 'NONE', #223504, #150828, #166870, .T. ) ;
#225433 = DIRECTION ( 'NONE',  ( 0.000000000000000000, -0.9908441862701782288, 0.1350103645450542456 ) ) ;
#225435 = CARTESIAN_POINT ( 'NONE',  ( -21.70464131381649509, 6.932842828061964724, -199.4901007520778080 ) ) ;
#225436 = ORIENTED_EDGE ( 'NONE', *, *, #227096, .F. ) ;
#225437 = ORIENTED_EDGE ( 'NONE', *, *, #179661, .T. ) ;
#225438 = EDGE_CURVE ( 'NONE', #176002, #54306, #62782, .T. ) ;
#225439 = DIRECTION ( 'NONE',  ( 0.000000000000000000, 7.026728003956683390E-15, -1.000000000000000000 ) ) ;
#225440 = ORIENTED_EDGE ( 'NONE', *, *, #178207, .T. ) ;
#225441 = DIRECTION ( 'NONE',  ( 0.000000000000000000, 0.000000000000000000, -1.000000000000000000 ) ) ;
#225442 = EDGE_CURVE ( 'NONE', #40042, #181952, #17009, .T. ) ;
#225443 = AXIS2_PLACEMENT_3D ( 'NONE', #168917, #187172, #248409 ) ;
#225444 = DIRECTION ( 'NONE',  ( 0.000000000000000000, -0.9770955615653313941, -0.2128009952263603677 ) ) ;
#225445 = CIRCLE ( 'NONE', #113039, 0.1000000000000000472 ) ;
#225446 = ORIENTED_EDGE ( 'NONE', *, *, #128898, .T. ) ;
#225447 = CARTESIAN_POINT ( 'NONE',  ( -18.59117750673696889, 18.41524492703433324, -237.0006385043383546 ) ) ;
#225448 = VERTEX_POINT ( 'NONE', #23624 ) ;
#225449 = EDGE_CURVE ( 'NONE', #13509, #82665, #162747, .T. ) ;
#225450 = CARTESIAN_POINT ( 'NONE',  ( -20.94999999999999929, 1.115600667400684642E-11, -134.0000000000000284 ) ) ;
#225451 = ADVANCED_FACE ( 'NONE', ( #22327 ), #180104, .F. ) ;
#225452 = FACE_OUTER_BOUND ( 'NONE', #46704, .T. ) ;
#225453 = CARTESIAN_POINT ( 'NONE',  ( -20.94999999999999929, -1.835341550213257733, -145.5551512925629822 ) ) ;
#225454 = CARTESIAN_POINT ( 'NONE',  ( 23.24999999999999645, 5.000000000011153745, -179.9052660189130677 ) ) ;
#225455 = DIRECTION ( 'NONE',  ( 0.000000000000000000, 0.000000000000000000, -1.000000000000000000 ) ) ;
#225456 = CARTESIAN_POINT ( 'NONE',  ( -16.92989507731676468, 66.05000000001254534, -182.9056085539142487 ) ) ;
#225457 = AXIS2_PLACEMENT_3D ( 'NONE', #240317, #61668, #158240 ) ;
#225458 = DIRECTION ( 'NONE',  ( 1.000000000000000000, 0.000000000000000000, 0.000000000000000000 ) ) ;
#225459 = DIRECTION ( 'NONE',  ( 0.000000000000000000, -0.4721928772777346239, -0.8814952561688430555 ) ) ;
#225461 = ORIENTED_EDGE ( 'NONE', *, *, #179362, .T. ) ;
#225460 = DIRECTION ( 'NONE',  ( 1.000000000000000000, 0.000000000000000000, 0.000000000000000000 ) ) ;
#225463 = LINE ( 'NONE', #248913, #143597 ) ;
#225462 = CARTESIAN_POINT ( 'NONE',  ( -18.46902351632711969, 85.50947011869349978, -196.5366535502670047 ) ) ;
#225464 = ORIENTED_EDGE ( 'NONE', *, *, #108225, .F. ) ;
#225466 = VERTEX_POINT ( 'NONE', #19750 ) ;
#225465 = CARTESIAN_POINT ( 'NONE',  ( 20.94999999999999929, 24.12844930803501242, -253.0488546976795021 ) ) ;
#225467 = ORIENTED_EDGE ( 'NONE', *, *, #244269, .F. ) ;
#225468 = DIRECTION ( 'NONE',  ( 1.000000000000000000, 0.000000000000000000, 0.000000000000000000 ) ) ;
#225469 = CARTESIAN_POINT ( 'NONE',  ( 18.49999999999999645, 77.13501884592155022, -28.30613060109199353 ) ) ;
#225470 = CARTESIAN_POINT ( 'NONE',  ( -16.97683809663752186, 9.850000000011137402, -113.9023640181965220 ) ) ;
#225471 = CARTESIAN_POINT ( 'NONE',  ( 20.94999999999999929, -11.64999999998883595, -97.50000000000004263 ) ) ;
#225472 = DIRECTION ( 'NONE',  ( -1.000000000000000000, -0.000000000000000000, -0.000000000000000000 ) ) ;
#225473 = CARTESIAN_POINT ( 'NONE',  ( -23.25000000000000000, -11.74999999998884448, -197.8999999999999773 ) ) ;
#225474 = CYLINDRICAL_SURFACE ( 'NONE', #140074, 0.1000000000000028644 ) ;
#225475 = CIRCLE ( 'NONE', #225290, 0.09999999999998898659 ) ;
#225476 = AXIS2_PLACEMENT_3D ( 'NONE', #251108, #253684, #72512 ) ;
#225477 = CARTESIAN_POINT ( 'NONE',  ( 21.08376601933332495, 69.65805272873649301, -136.5868834954543445 ) ) ;
#225478 = ORIENTED_EDGE ( 'NONE', *, *, #30824, .T. ) ;
#225479 = ORIENTED_EDGE ( 'NONE', *, *, #23563, .T. ) ;
#225480 = DIRECTION ( 'NONE',  ( 1.000000000000000000, 0.000000000000000000, 0.000000000000000000 ) ) ;
#225481 = ADVANCED_FACE ( 'NONE', ( #203510 ), #250220, .F. ) ;
#225482 = EDGE_LOOP ( 'NONE', ( #18513, #188257, #148660, #137481 ) ) ;
#225483 = DIRECTION ( 'NONE',  ( 0.000000000000000000, -7.026728003956683390E-15, 1.000000000000000000 ) ) ;
#225484 = ORIENTED_EDGE ( 'NONE', *, *, #46044, .F. ) ;
#225485 = DIRECTION ( 'NONE',  ( 2.557131231893036985E-16, -0.8660254037844383745, 0.5000000000000003331 ) ) ;
#225486 = DIRECTION ( 'NONE',  ( 1.000000000000000000, -0.000000000000000000, -0.000000000000000000 ) ) ;
#225487 = CARTESIAN_POINT ( 'NONE',  ( -22.49917693094574389, -2.395810317367125020, -189.5988992245846134 ) ) ;
#225488 = DIRECTION ( 'NONE',  ( 0.000000000000000000, 0.000000000000000000, 1.000000000000000000 ) ) ;
#225489 = CARTESIAN_POINT ( 'NONE',  ( 21.12400247839510925, 10.72148804404153921, -179.7500000000000000 ) ) ;
#225490 = ORIENTED_EDGE ( 'NONE', *, *, #155726, .F. ) ;
#225491 = AXIS2_PLACEMENT_3D ( 'NONE', #195312, #16661, #2193 ) ;
#225492 = LINE ( 'NONE', #216844, #182793 ) ;
#225493 = LINE ( 'NONE', #7770, #167163 ) ;
#225494 = CARTESIAN_POINT ( 'NONE',  ( 18.40000000000000213, 85.51932773110404185, -62.55013110796493692 ) ) ;
#225496 = EDGE_CURVE ( 'NONE', #254433, #237868, #100155, .T. ) ;
#225495 = CARTESIAN_POINT ( 'NONE',  ( -21.64999999999999858, 9.350000000011133849, -42.75000000000000000 ) ) ;
#225497 = ORIENTED_EDGE ( 'NONE', *, *, #188443, .F. ) ;
#225499 = DIRECTION ( 'NONE',  ( 0.000000000000000000, 0.9651348961777157509, -0.2617529984165031243 ) ) ;
#225498 = CARTESIAN_POINT ( 'NONE',  ( 20.95512820512820440, 8.876151316299271343, -88.25000000000005684 ) ) ;
#225500 = VERTEX_POINT ( 'NONE', #120157 ) ;
#225503 = EDGE_LOOP ( 'NONE', ( #10396, #99871, #108001, #230421 ) ) ;
#225502 = DIRECTION ( 'NONE',  ( 0.000000000000000000, -6.982962677686266711E-15, 1.000000000000000000 ) ) ;
#225501 = CARTESIAN_POINT ( 'NONE',  ( -21.14999999999999858, 76.00000000001237765, -170.0231074845243597 ) ) ;
#225504 = EDGE_LOOP ( 'NONE', ( #45814, #105, #66379, #185451 ) ) ;
#225505 = CARTESIAN_POINT ( 'NONE',  ( 21.05000000000000071, 10.40540721059935159, -207.3515911714149809 ) ) ;
#225506 = CARTESIAN_POINT ( 'NONE',  ( -21.05000000000000071, 34.05153573962405034, -243.7669379519762174 ) ) ;
#225507 = CARTESIAN_POINT ( 'NONE',  ( 21.05000000000000071, 47.74710514101221293, -244.5837943500090716 ) ) ;
#225508 = ORIENTED_EDGE ( 'NONE', *, *, #98431, .T. ) ;
#225509 = CARTESIAN_POINT ( 'NONE',  ( -5.900000000000002132, -11.65000000000000036, 14.10000000000000142 ) ) ;
#225510 = CARTESIAN_POINT ( 'NONE',  ( 20.94999999999999929, 67.23127455305835554, -235.8551265064784559 ) ) ;
#225512 = DIRECTION ( 'NONE',  ( 0.000000000000000000, 1.265107689135680095E-16, -1.000000000000000000 ) ) ;
#225511 = LINE ( 'NONE', #149881, #242866 ) ;
#225514 = EDGE_LOOP ( 'NONE', ( #179538, #220640, #230391, #245464 ) ) ;
#225513 = CARTESIAN_POINT ( 'NONE',  ( -18.54118089899629851, 46.96055236759813312, -255.3059391806394274 ) ) ;
#225515 = AXIS2_PLACEMENT_3D ( 'NONE', #165736, #109577, #84851 ) ;
#225516 = ORIENTED_EDGE ( 'NONE', *, *, #72087, .F. ) ;
#225517 = VECTOR ( 'NONE', #108793, 1000.000000000000000 ) ;
#225518 = CARTESIAN_POINT ( 'NONE',  ( 19.87657994472052181, 64.25000000001176659, -78.25731935989793442 ) ) ;
#225519 = CARTESIAN_POINT ( 'NONE',  ( -18.59999999999999787, 69.06610602788578035, -132.7374616501508342 ) ) ;
#225520 = DIRECTION ( 'NONE',  ( 0.000000000000000000, 0.000000000000000000, -1.000000000000000000 ) ) ;
#225522 = EDGE_LOOP ( 'NONE', ( #93201, #74425, #223348, #76035 ) ) ;
#225521 = AXIS2_PLACEMENT_3D ( 'NONE', #247851, #90048, #45796 ) ;
#225523 = FACE_OUTER_BOUND ( 'NONE', #27250, .T. ) ;
#225524 = EDGE_LOOP ( 'NONE', ( #186095, #87082, #82461 ) ) ;
#225525 = DIRECTION ( 'NONE',  ( 1.000000000000000000, 0.000000000000000000, 0.000000000000000000 ) ) ;
#225526 = AXIS2_PLACEMENT_3D ( 'NONE', #97408, #197820, #193999 ) ;
#225527 = CARTESIAN_POINT ( 'NONE',  ( 20.99999999999999645, 9.750000000011137757, -188.3499999999999659 ) ) ;
#225528 = CARTESIAN_POINT ( 'NONE',  ( 20.94999999999999929, -6.488386256076840830, -212.2361678873109554 ) ) ;
#225529 = EDGE_LOOP ( 'NONE', ( #32565, #227382, #175276, #216644 ) ) ;
#225530 = DIRECTION ( 'NONE',  ( 1.000000000000000000, -7.304098846218133681E-16, 0.000000000000000000 ) ) ;
#225531 = CIRCLE ( 'NONE', #133974, 0.09999999999999484301 ) ;
#225532 = EDGE_CURVE ( 'NONE', #207975, #241304, #137769, .T. ) ;
#225533 = ORIENTED_EDGE ( 'NONE', *, *, #82509, .F. ) ;
#225534 = AXIS2_PLACEMENT_3D ( 'NONE', #159134, #199541, #20907 ) ;
#225535 = DIRECTION ( 'NONE',  ( -0.000000000000000000, -0.000000000000000000, 1.000000000000000000 ) ) ;
#225536 = DIRECTION ( 'NONE',  ( 1.000000000000000000, 0.000000000000000000, 0.000000000000000000 ) ) ;
#225537 = CIRCLE ( 'NONE', #204887, 0.09999999999999990841 ) ;
#225538 = VERTEX_POINT ( 'NONE', #84803 ) ;
#225539 = VERTEX_POINT ( 'NONE', #129110 ) ;
#225540 = VECTOR ( 'NONE', #109821, 999.9999999999998863 ) ;
#225541 = EDGE_CURVE ( 'NONE', #250767, #243771, #133505, .T. ) ;
#225542 = LINE ( 'NONE', #149907, #58280 ) ;
#225543 = ORIENTED_EDGE ( 'NONE', *, *, #228316, .T. ) ;
#225545 = VERTEX_POINT ( 'NONE', #10450 ) ;
#225544 = CARTESIAN_POINT ( 'NONE',  ( 12.60873083341399514, 66.61042836546617707, -185.7054667721552903 ) ) ;
#225546 = AXIS2_PLACEMENT_3D ( 'NONE', #155640, #235143, #136012 ) ;
#225547 = EDGE_CURVE ( 'NONE', #88879, #163406, #138423, .T. ) ;
#225548 = VERTEX_POINT ( 'NONE', #105662 ) ;
#225551 = ORIENTED_EDGE ( 'NONE', *, *, #191005, .F. ) ;
#225550 = ORIENTED_EDGE ( 'NONE', *, *, #112736, .F. ) ;
#225549 = B_SPLINE_CURVE_WITH_KNOTS ( 'NONE', 3,
 ( #172869, #231523, #252340, #114118, #15047, #94554, #154575 ),
 .UNSPECIFIED., .F., .F.,
 ( 4, 3, 4 ),
 ( 0.000000000000000000, 4.520325912680724513E-05, 5.794988040901477241E-05 ),
 .UNSPECIFIED. ) ;
#225552 = CARTESIAN_POINT ( 'NONE',  ( -18.40000000000000213, 45.89348038176515843, -239.2231437130149061 ) ) ;
#225554 = ADVANCED_FACE ( 'NONE', ( #144796 ), #148684, .F. ) ;
#225553 = ORIENTED_EDGE ( 'NONE', *, *, #145019, .F. ) ;
#225555 = DIRECTION ( 'NONE',  ( -4.801466763864313332E-15, 0.5041370733442360752, 0.8636236514129915776 ) ) ;
#225556 = DIRECTION ( 'NONE',  ( 1.000000000000000000, 0.000000000000000000, 0.000000000000000000 ) ) ;
#225557 = AXIS2_PLACEMENT_3D ( 'NONE', #166814, #122532, #34669 ) ;
#225558 = AXIS2_PLACEMENT_3D ( 'NONE', #167075, #52211, #150068 ) ;
#225559 = DIRECTION ( 'NONE',  ( 0.000000000000000000, 0.000000000000000000, 1.000000000000000000 ) ) ;
#225560 = VECTOR ( 'NONE', #19229, 1000.000000000000227 ) ;
#225562 = CARTESIAN_POINT ( 'NONE',  ( -18.47130263965444286, 86.89034400014838866, -199.5518236931774823 ) ) ;
#225561 = VECTOR ( 'NONE', #217638, 1000.000000000000000 ) ;
#225563 = EDGE_LOOP ( 'NONE', ( #135078, #68941, #152669 ) ) ;
#225564 = VERTEX_POINT ( 'NONE', #224346 ) ;
#225565 = CARTESIAN_POINT ( 'NONE',  ( -16.97683809663752186, 9.850000000011140955, -46.15000000000000568 ) ) ;
#225567 = ORIENTED_EDGE ( 'NONE', *, *, #223060, .F. ) ;
#225566 = DIRECTION ( 'NONE',  ( 0.000000000000000000, 0.000000000000000000, 1.000000000000000000 ) ) ;
#225568 = CARTESIAN_POINT ( 'NONE',  ( -16.87036670365548474, 14.22508806334145959, -219.3732768077300932 ) ) ;
#225570 = ORIENTED_EDGE ( 'NONE', *, *, #4293, .T. ) ;
#225569 = CARTESIAN_POINT ( 'NONE',  ( 21.05000000000000071, 1.148907358139439339E-11, -201.0000000000015064 ) ) ;
#225571 = EDGE_CURVE ( 'NONE', #16721, #191564, #221629, .T. ) ;
#225572 = ORIENTED_EDGE ( 'NONE', *, *, #203008, .T. ) ;
#225573 = DIRECTION ( 'NONE',  ( 0.000000000000000000, -0.9126074666063770380, -0.4088369013363281068 ) ) ;
#225574 = ORIENTED_EDGE ( 'NONE', *, *, #119219, .T. ) ;
#225575 = ORIENTED_EDGE ( 'NONE', *, *, #11389, .T. ) ;
#225576 = FACE_OUTER_BOUND ( 'NONE', #80756, .T. ) ;
#225577 = DIRECTION ( 'NONE',  ( 0.000000000000000000, 1.224646799142015331E-16, 1.000000000000000000 ) ) ;
#225578 = CIRCLE ( 'NONE', #34116, 4.049999999999987388 ) ;
#225580 = ORIENTED_EDGE ( 'NONE', *, *, #84751, .F. ) ;
#225579 = VERTEX_POINT ( 'NONE', #7892 ) ;
#225581 = ORIENTED_EDGE ( 'NONE', *, *, #43038, .T. ) ;
#225582 = CARTESIAN_POINT ( 'NONE',  ( -16.89021194854739960, 9.950000000011135270, -54.24256813160434376 ) ) ;
#225583 = ORIENTED_EDGE ( 'NONE', *, *, #155124, .F. ) ;
#225584 = ORIENTED_EDGE ( 'NONE', *, *, #178298, .T. ) ;
#225585 = DIRECTION ( 'NONE',  ( 0.000000000000000000, 1.000000000000000000, 1.626303258728238113E-15 ) ) ;
#225587 = ORIENTED_EDGE ( 'NONE', *, *, #16409, .T. ) ;
#225586 = DIRECTION ( 'NONE',  ( 0.000000000000000000, 0.1350103645451946055, -0.9908441862701591329 ) ) ;
#225588 = DIRECTION ( 'NONE',  ( 1.000000000000000000, 0.000000000000000000, 0.000000000000000000 ) ) ;
#225590 = CARTESIAN_POINT ( 'NONE',  ( 21.14999999999999858, 23.42819724844704155, -229.2476443247244902 ) ) ;
#225589 = CARTESIAN_POINT ( 'NONE',  ( 23.14999999999999503, 23.34004772283015683, -229.2004250369967338 ) ) ;
#225591 = DIRECTION ( 'NONE',  ( 0.000000000000000000, -4.562560375171877784E-14, 1.000000000000000000 ) ) ;
#225592 = DIRECTION ( 'NONE',  ( 1.186688945009010077E-16, -0.9770955615653316162, -0.2128009952263604232 ) ) ;
#225593 = ORIENTED_EDGE ( 'NONE', *, *, #148829, .T. ) ;
#225594 = EDGE_LOOP ( 'NONE', ( #222067, #227609, #175499, #91485 ) ) ;
#225595 = CYLINDRICAL_SURFACE ( 'NONE', #248493, 0.1000000000000028644 ) ;
#225596 = CARTESIAN_POINT ( 'NONE',  ( 20.94999999999999929, 7.872214528623318053, -209.6555322433423783 ) ) ;
#225597 = ORIENTED_EDGE ( 'NONE', *, *, #9330, .T. ) ;
#225598 = EDGE_CURVE ( 'NONE', #162629, #157579, #166987, .T. ) ;
#225599 = AXIS2_PLACEMENT_3D ( 'NONE', #153952, #191778, #78200 ) ;
#225600 = CARTESIAN_POINT ( 'NONE',  ( 21.05000000000000071, 65.27628289530507288, -191.3731074845244393 ) ) ;
#225601 = VERTEX_POINT ( 'NONE', #45712 ) ;
#225602 = ORIENTED_EDGE ( 'NONE', *, *, #221528, .T. ) ;
#225603 = CARTESIAN_POINT ( 'NONE',  ( -21.00219873199078435, 64.39461131213606393, -196.6104600562298401 ) ) ;
#225604 = DIRECTION ( 'NONE',  ( 1.000000000000000000, 0.000000000000000000, 0.000000000000000000 ) ) ;
#225605 = ORIENTED_EDGE ( 'NONE', *, *, #232779, .T. ) ;
#225606 = CARTESIAN_POINT ( 'NONE',  ( -22.59999999999999787, 11.64957080754479968, 0.09999999999999592548 ) ) ;
#225607 = DIRECTION ( 'NONE',  ( 0.000000000000000000, 0.000000000000000000, 1.000000000000000000 ) ) ;
#225609 = EDGE_LOOP ( 'NONE', ( #82442, #243077, #135648, #238452 ) ) ;
#225608 = APPLICATION_CONTEXT ( 'automotive_design' ) ;
#225610 = CYLINDRICAL_SURFACE ( 'NONE', #85525, 0.1000000000000028644 ) ;
#225612 = ADVANCED_FACE ( 'NONE', ( #245212 ), #76004, .T. ) ;
#225611 = DIRECTION ( 'NONE',  ( 1.000000000000000000, 0.000000000000000000, 0.000000000000000000 ) ) ;
#225614 = CARTESIAN_POINT ( 'NONE',  ( 23.15000000000000213, -11.64999999998883595, -63.89999999999999858 ) ) ;
#225613 = DIRECTION ( 'NONE',  ( 1.000000000000000000, 0.000000000000000000, 0.000000000000000000 ) ) ;
#225615 = CARTESIAN_POINT ( 'NONE',  ( -2.995603634470891112E-16, 87.75000000001151079, -48.27310748452424605 ) ) ;
#225616 = DIRECTION ( 'NONE',  ( 0.000000000000000000, 1.000000000000000000, 6.982962677686266711E-15 ) ) ;
#225617 = CARTESIAN_POINT ( 'NONE',  ( 22.39999999999999858, 0.09999999999999939493, 7.790779598373383408 ) ) ;
#225618 = DIRECTION ( 'NONE',  ( -1.000000000000000000, -0.000000000000000000, -0.000000000000000000 ) ) ;
#225619 = EDGE_CURVE ( 'NONE', #14256, #11996, #48279, .T. ) ;
#225620 = ORIENTED_EDGE ( 'NONE', *, *, #10188, .F. ) ;
#225621 = VECTOR ( 'NONE', #230124, 1000.000000000000000 ) ;
#225622 = CIRCLE ( 'NONE', #196599, 0.09999999999998898659 ) ;
#225623 = ADVANCED_BREP_SHAPE_REPRESENTATION ( '', ( #197191, #2425 ), #193986 ) ;
#225625 = VERTEX_POINT ( 'NONE', #106958 ) ;
#225624 = ORIENTED_EDGE ( 'NONE', *, *, #45027, .T. ) ;
#225626 = ORIENTED_EDGE ( 'NONE', *, *, #27449, .F. ) ;
#225627 = FACE_OUTER_BOUND ( 'NONE', #190406, .T. ) ;
#225628 = EDGE_CURVE ( 'NONE', #63952, #224878, #249072, .T. ) ;
#225629 = DIRECTION ( 'NONE',  ( -3.265361837132813586E-16, 1.000000000000000000, 0.000000000000000000 ) ) ;
#225631 = CARTESIAN_POINT ( 'NONE',  ( -16.97092634996681682, 10.00088896635984881, -146.6301427662976096 ) ) ;
#225630 = DIRECTION ( 'NONE',  ( 1.000000000000000000, 0.000000000000000000, 0.000000000000000000 ) ) ;
#225632 = DIRECTION ( 'NONE',  ( 0.000000000000000000, -0.6728971962617102953, -0.7397360091702507301 ) ) ;
#225633 = ORIENTED_EDGE ( 'NONE', *, *, #161599, .F. ) ;
#225634 = EDGE_CURVE ( 'NONE', #195188, #68571, #86089, .T. ) ;
#225635 = CARTESIAN_POINT ( 'NONE',  ( -21.05000000000000071, 44.52640028187936849, -247.3006740988509193 ) ) ;
#225636 = ADVANCED_FACE ( 'NONE', ( #206077 ), #49568, .T. ) ;
#225637 = DIRECTION ( 'NONE',  ( -0.000000000000000000, 1.000000000000000000, 6.982962677686267499E-15 ) ) ;
#225639 = VECTOR ( 'NONE', #5066, 1000.000000000000000 ) ;
#225638 = CARTESIAN_POINT ( 'NONE',  ( -18.59999999999999787, 44.52640028187936849, -247.3006740988509193 ) ) ;
#225640 = LINE ( 'NONE', #199714, #91738 ) ;
#225641 = EDGE_LOOP ( 'NONE', ( #101133, #236384, #66214, #93477, #161927 ) ) ;
#225642 = EDGE_CURVE ( 'NONE', #53312, #131589, #109524, .T. ) ;
#225643 = DIRECTION ( 'NONE',  ( -1.000000000000000000, -0.000000000000000000, 0.000000000000000000 ) ) ;
#225644 = ORIENTED_EDGE ( 'NONE', *, *, #34747, .T. ) ;
#225645 = ORIENTED_EDGE ( 'NONE', *, *, #215837, .T. ) ;
#225646 = DIRECTION ( 'NONE',  ( -1.000000000000000000, 0.000000000000000000, 0.000000000000000000 ) ) ;
#225647 = CARTESIAN_POINT ( 'NONE',  ( 20.94999999999999929, -1.349153571964892606, -208.7874973355898476 ) ) ;
#225648 = CARTESIAN_POINT ( 'NONE',  ( 21.05000000000000071, 74.16465844978819177, -191.9679561919613775 ) ) ;
#225649 = ADVANCED_FACE ( 'NONE', ( #209943 ), #192618, .T. ) ;
#225650 = DIRECTION ( 'NONE',  ( 0.000000000000000000, 1.000000000000000000, 0.000000000000000000 ) ) ;
#225651 = DIRECTION ( 'NONE',  ( -1.000000000000000000, -0.000000000000000000, -0.000000000000000000 ) ) ;
#225652 = EDGE_CURVE ( 'NONE', #200730, #228810, #155047, .T. ) ;
#225653 = VERTEX_POINT ( 'NONE', #151251 ) ;
#225654 = CARTESIAN_POINT ( 'NONE',  ( -20.94999999999999929, 76.00000000001213607, -136.5231074845242745 ) ) ;
#225655 = DIRECTION ( 'NONE',  ( -0.7070776581709312669, -0.6453375049857505985, -0.2891032514073097470 ) ) ;
#225658 = CARTESIAN_POINT ( 'NONE',  ( 20.85000000000000142, 0.1610488207298751417, -167.2158101556397867 ) ) ;
#225657 = AXIS2_PLACEMENT_3D ( 'NONE', #220690, #204951, #203693 ) ;
#225656 = CARTESIAN_POINT ( 'NONE',  ( 18.49999999999999289, 30.78873405139468034, -234.7786928665882442 ) ) ;
#225660 = CARTESIAN_POINT ( 'NONE',  ( -20.54999999999999716, 4.350000000011156054, -188.7499999999999716 ) ) ;
#225659 = AXIS2_PLACEMENT_3D ( 'NONE', #127283, #64735, #144250 ) ;
#225661 = CIRCLE ( 'NONE', #179915, 4.099999999999992539 ) ;
#225662 = DIRECTION ( 'NONE',  ( 0.000000000000000000, -6.982962677686266711E-15, 1.000000000000000000 ) ) ;
#225663 = FACE_OUTER_BOUND ( 'NONE', #34643, .T. ) ;
#225664 = DIRECTION ( 'NONE',  ( 2.978066053179067751E-16, -1.000000000000000000, 0.000000000000000000 ) ) ;
#225666 = VERTEX_POINT ( 'NONE', #96374 ) ;
#225665 = CARTESIAN_POINT ( 'NONE',  ( 21.93340585899775164, 29.97485316283794532, -252.5455442746994947 ) ) ;
#225667 = EDGE_CURVE ( 'NONE', #194728, #52702, #205059, .T. ) ;
#225668 = EDGE_CURVE ( 'NONE', #100977, #128703, #96725, .T. ) ;
#225669 = VECTOR ( 'NONE', #137548, 1000.000000000000000 ) ;
#225670 = CARTESIAN_POINT ( 'NONE',  ( 21.76363531954645936, 7.012936547882880234, -100.4009981257005819 ) ) ;
#225671 = EDGE_CURVE ( 'NONE', #28056, #172722, #213452, .T. ) ;
#225672 = DIRECTION ( 'NONE',  ( 0.000000000000000000, 0.000000000000000000, 1.000000000000000000 ) ) ;
#225673 = CARTESIAN_POINT ( 'NONE',  ( 14.45204356427542258, 9.450668889178682974, -149.0555464902073481 ) ) ;
#225674 = ORIENTED_EDGE ( 'NONE', *, *, #231410, .T. ) ;
#225675 = DIRECTION ( 'NONE',  ( 0.000000000000000000, -0.9994937237965558774, -0.03181660087586650476 ) ) ;
#225676 = CARTESIAN_POINT ( 'NONE',  ( 20.95512820512821150, 65.37615131629968346, -57.32294546509999122 ) ) ;
#225677 = FACE_OUTER_BOUND ( 'NONE', #248757, .T. ) ;
#225678 = ORIENTED_EDGE ( 'NONE', *, *, #110243, .T. ) ;
#225679 = CARTESIAN_POINT ( 'NONE',  ( -17.01764560440442864, 66.05000000001159322, -56.77310748530980788 ) ) ;
#225681 = VERTEX_POINT ( 'NONE', #135503 ) ;
#225680 = DIRECTION ( 'NONE',  ( 0.000000000000000000, 6.467318590049456648E-15, -1.000000000000000000 ) ) ;
#225683 = LINE ( 'NONE', #74060, #241877 ) ;
#225682 = DIRECTION ( 'NONE',  ( 0.000000000000000000, 0.000000000000000000, -1.000000000000000000 ) ) ;
#225684 = CIRCLE ( 'NONE', #238171, 0.2000000000000057288 ) ;
#225685 = CARTESIAN_POINT ( 'NONE',  ( 23.14999999999999503, 11.75000000000000711, -21.35000000000000142 ) ) ;
#225686 = EDGE_LOOP ( 'NONE', ( #54418, #170590, #64453, #242209 ) ) ;
#225687 = DIRECTION ( 'NONE',  ( 0.000000000000000000, -0.9651348961777066471, 0.2617529984165365975 ) ) ;
#225688 = VECTOR ( 'NONE', #251350, 1000.000000000000000 ) ;
#225689 = EDGE_CURVE ( 'NONE', #170174, #163726, #252896, .T. ) ;
#225690 = DIRECTION ( 'NONE',  ( 0.000000000000000000, 0.000000000000000000, 1.000000000000000000 ) ) ;
#225691 = CARTESIAN_POINT ( 'NONE',  ( 20.94999999999999574, -11.39257802169451672, -137.0739495798319467 ) ) ;
#225692 = LINE ( 'NONE', #88762, #81545 ) ;
#225694 = CIRCLE ( 'NONE', #213237, 0.09999999999999810429 ) ;
#225693 = FACE_OUTER_BOUND ( 'NONE', #58221, .T. ) ;
#225695 = ORIENTED_EDGE ( 'NONE', *, *, #158026, .T. ) ;
#225696 = CIRCLE ( 'NONE', #88317, 4.000000000000002665 ) ;
#225698 = EDGE_CURVE ( 'NONE', #19024, #143115, #52118, .T. ) ;
#225697 = CARTESIAN_POINT ( 'NONE',  ( -18.50000000000000000, 68.97833521811131163, -32.38954208262708079 ) ) ;
#225699 = DIRECTION ( 'NONE',  ( 0.000000000000000000, -1.000000000000000000, -2.891205793294679805E-16 ) ) ;
#225700 = VECTOR ( 'NONE', #90240, 999.9999999999998863 ) ;
#225701 = FACE_OUTER_BOUND ( 'NONE', #40599, .T. ) ;
#225702 = VECTOR ( 'NONE', #36545, 999.9999999999998863 ) ;
#225703 = B_SPLINE_CURVE_WITH_KNOTS ( 'NONE', 3,
 ( #106510, #103941, #68701, #183511 ),
 .UNSPECIFIED., .F., .F.,
 ( 4, 4 ),
 ( 0.000000000000000000, 0.001767853679387133359 ),
 .UNSPECIFIED. ) ;
#225704 = EDGE_CURVE ( 'NONE', #245998, #98647, #134330, .T. ) ;
#225705 = EDGE_CURVE ( 'NONE', #13877, #111909, #67714, .T. ) ;
#225706 = CARTESIAN_POINT ( 'NONE',  ( -23.15000000000000213, 74.00000000001199396, -116.2477294072864140 ) ) ;
#225707 = ORIENTED_EDGE ( 'NONE', *, *, #170241, .F. ) ;
#225708 = ORIENTED_EDGE ( 'NONE', *, *, #251922, .T. ) ;
#225709 = EDGE_CURVE ( 'NONE', #220166, #133447, #80144, .T. ) ;
#225710 = B_SPLINE_CURVE_WITH_KNOTS ( 'NONE', 3,
 ( #248594, #69981, #189908, #109072, #34707, #114219, #167805, #13841, #11274, #251139 ),
 .UNSPECIFIED., .F., .F.,
 ( 4, 3, 3, 4 ),
 ( -2.000561356218653466E-06, 0.000000000000000000, 1.787822682428266431E-05, 4.206475347089651067E-05 ),
 .UNSPECIFIED. ) ;
#225712 = AXIS2_PLACEMENT_3D ( 'NONE', #24614, #207078, #23331 ) ;
#225711 = FACE_OUTER_BOUND ( 'NONE', #127869, .T. ) ;
#225714 = AXIS2_PLACEMENT_3D ( 'NONE', #235303, #213174, #172821 ) ;
#225713 = FACE_OUTER_BOUND ( 'NONE', #158702, .T. ) ;
#225715 = DIRECTION ( 'NONE',  ( 0.000000000000000000, 0.000000000000000000, 1.000000000000000000 ) ) ;
#225716 = CARTESIAN_POINT ( 'NONE',  ( 21.07189867249812210, 13.07815244086534712, -210.6504456248233623 ) ) ;
#225717 = CARTESIAN_POINT ( 'NONE',  ( 21.13461538461538680, 8.885417037985613220, -146.2500000000000568 ) ) ;
#225719 = DIRECTION ( 'NONE',  ( -1.000000000000000000, 0.000000000000000000, 0.000000000000000000 ) ) ;
#225718 = FACE_OUTER_BOUND ( 'NONE', #65296, .T. ) ;
#225720 = AXIS2_PLACEMENT_3D ( 'NONE', #209465, #51649, #92086 ) ;
#225721 = LINE ( 'NONE', #84917, #227445 ) ;
#225722 = CARTESIAN_POINT ( 'NONE',  ( 20.04142135623730070, 8.882751598337870647, -187.0399955572217721 ) ) ;
#225724 = CARTESIAN_POINT ( 'NONE',  ( 21.05000000000000071, 76.00000000001205080, -124.3731074845242972 ) ) ;
#225723 = AXIS2_PLACEMENT_3D ( 'NONE', #233769, #69561, #92953 ) ;
#225725 = FACE_OUTER_BOUND ( 'NONE', #61634, .T. ) ;
#225726 = EDGE_CURVE ( 'NONE', #180772, #246470, #32614, .T. ) ;
#225728 = VERTEX_POINT ( 'NONE', #13036 ) ;
#225727 = CARTESIAN_POINT ( 'NONE',  ( 15.66039659514494709, 62.72902952540357546, -216.6940264888114882 ) ) ;
#225729 = CARTESIAN_POINT ( 'NONE',  ( 21.09316766718127667, 69.62984668753796313, -170.0623708868390906 ) ) ;
#225730 = EDGE_CURVE ( 'NONE', #95420, #164666, #17627, .T. ) ;
#225731 = DIRECTION ( 'NONE',  ( 0.000000000000000000, -0.2617529984165030132, -0.9651348961777157509 ) ) ;
#225733 = CARTESIAN_POINT ( 'NONE',  ( 11.60000000000006004, 67.75000000001118394, -25.06452884076210097 ) ) ;
#225732 = CARTESIAN_POINT ( 'NONE',  ( -17.04761207306817994, 14.23370139713091120, -219.2388037341914071 ) ) ;
#225734 = VECTOR ( 'NONE', #179565, 1000.000000000000000 ) ;
#225735 = ORIENTED_EDGE ( 'NONE', *, *, #241252, .F. ) ;
#225736 = DIRECTION ( 'NONE',  ( 0.000000000000000000, -0.9691069652679039637, 0.2466408114429434750 ) ) ;
#225738 = ADVANCED_FACE ( 'NONE', ( #75579 ), #92531, .F. ) ;
#225737 = CARTESIAN_POINT ( 'NONE',  ( -20.64999999999999858, 1.115600667400684642E-11, -180.3749999999999716 ) ) ;
#225739 = CARTESIAN_POINT ( 'NONE',  ( 23.15000000000000213, -4.356730526971939632, -226.1082375506050539 ) ) ;
#225740 = CARTESIAN_POINT ( 'NONE',  ( 20.04999999999999716, 62.09751964147213954, -221.3558313336858703 ) ) ;
#225742 = DIRECTION ( 'NONE',  ( 0.000000000000000000, 0.2128009952263666682, -0.9770955615653300619 ) ) ;
#225741 = CIRCLE ( 'NONE', #217361, 0.09999999999999939493 ) ;
#225743 = ORIENTED_EDGE ( 'NONE', *, *, #207433, .F. ) ;
#225744 = ORIENTED_EDGE ( 'NONE', *, *, #157689, .T. ) ;
#225745 = CARTESIAN_POINT ( 'NONE',  ( 20.94999999999999574, 13.59055429284667404, -238.6121134008722038 ) ) ;
#225746 = ORIENTED_EDGE ( 'NONE', *, *, #46503, .F. ) ;
#225748 = CARTESIAN_POINT ( 'NONE',  ( -21.05000000000000071, 12.82677665681128332, -205.1493534351658354 ) ) ;
#225747 = VECTOR ( 'NONE', #157192, 1000.000000000000000 ) ;
#225749 = ADVANCED_FACE ( 'NONE', ( #155125 ), #190385, .T. ) ;
#225750 = ADVANCED_FACE ( 'NONE', ( #16878 ), #254169, .F. ) ;
#225751 = VECTOR ( 'NONE', #8946, 1000.000000000000000 ) ;
#225752 = ORIENTED_EDGE ( 'NONE', *, *, #157215, .F. ) ;
#225753 = VECTOR ( 'NONE', #243102, 1000.000000000000000 ) ;
#225754 = DIRECTION ( 'NONE',  ( 1.000000000000000000, 0.000000000000000000, 0.000000000000000000 ) ) ;
#225755 = AXIS2_PLACEMENT_3D ( 'NONE', #145818, #205802, #144533 ) ;
#225756 = CARTESIAN_POINT ( 'NONE',  ( 18.59999999999999076, 8.433899723187009201, -209.4150263691077782 ) ) ;
#225757 = ADVANCED_FACE ( 'NONE', ( #93822 ), #38499, .T. ) ;
#225758 = CARTESIAN_POINT ( 'NONE',  ( 23.04999999999999716, 67.17743825834548943, -93.77310748452437394 ) ) ;
#225759 = VERTEX_POINT ( 'NONE', #113397 ) ;
#225760 = ADVANCED_FACE ( 'NONE', ( #234622 ), #167698, .T. ) ;
#225761 = DIRECTION ( 'NONE',  ( 0.000000000000000000, -1.000000000000000000, 0.000000000000000000 ) ) ;
#225762 = LINE ( 'NONE', #165834, #125369 ) ;
#225763 = EDGE_CURVE ( 'NONE', #20940, #116282, #230021, .T. ) ;
#225764 = CARTESIAN_POINT ( 'NONE',  ( 21.04386569057559697, 11.75000000001105427, -160.6428373517805710 ) ) ;
#225765 = FACE_OUTER_BOUND ( 'NONE', #174733, .T. ) ;
#225766 = DIRECTION ( 'NONE',  ( 0.000000000000000000, -0.8814952561688707000, 0.4721928772776828875 ) ) ;
#225767 = DIRECTION ( 'NONE',  ( 0.000000000000000000, 0.2128009952263604232, -0.9770955615653316162 ) ) ;
#225768 = DIRECTION ( 'NONE',  ( 0.000000000000000000, 0.000000000000000000, -1.000000000000000000 ) ) ;
#225769 = EDGE_LOOP ( 'NONE', ( #6710, #167116 ) ) ;
#225770 = AXIS2_PLACEMENT_3D ( 'NONE', #119868, #40348, #184948 ) ;
#225771 = LINE ( 'NONE', #244062, #253264 ) ;
#225772 = ORIENTED_EDGE ( 'NONE', *, *, #213079, .T. ) ;
#225774 = EDGE_LOOP ( 'NONE', ( #211427, #180070, #255383, #250964 ) ) ;
#225773 = CARTESIAN_POINT ( 'NONE',  ( 23.15000000000000213, -9.599999999988845900, -76.89396912265249284 ) ) ;
#225775 = ORIENTED_EDGE ( 'NONE', *, *, #21938, .F. ) ;
#225776 = CARTESIAN_POINT ( 'NONE',  ( 21.14999999999999858, 76.10000000001238618, -170.0231074845243313 ) ) ;
#225777 = DIRECTION ( 'NONE',  ( 0.000000000000000000, 0.8103668758649523740, -0.5859227990963290500 ) ) ;
#225778 = PLANE ( 'NONE',  #201259 ) ;
#225779 = LINE ( 'NONE', #47139, #46057 ) ;
#225780 = ORIENTED_EDGE ( 'NONE', *, *, #61619, .T. ) ;
#225781 = EDGE_CURVE ( 'NONE', #11381, #198367, #125964, .T. ) ;
#225782 = CARTESIAN_POINT ( 'NONE',  ( -18.38639463286148867, 40.40701426736398361, -235.2925055146703528 ) ) ;
#225783 = LINE ( 'NONE', #70618, #222839 ) ;
#225784 = ORIENTED_EDGE ( 'NONE', *, *, #1029, .T. ) ;
#225785 = CARTESIAN_POINT ( 'NONE',  ( -16.90987985657661952, 9.957807518190888274, -154.8692870888836808 ) ) ;
#225786 = ADVANCED_FACE ( 'NONE', ( #178531 ), #37734, .F. ) ;
#225787 = B_SPLINE_CURVE_WITH_KNOTS ( 'NONE', 3,
 ( #183121, #100943, #1874, #160988, #25342, #123141, #237937, #64450 ),
 .UNSPECIFIED., .F., .F.,
 ( 4, 2, 2, 4 ),
 ( 0.000000000000000000, 6.534141206309673484E-05, 0.0001306828241261934697, 0.0002613656482524646225 ),
 .UNSPECIFIED. ) ;
#225788 = ORIENTED_EDGE ( 'NONE', *, *, #91435, .T. ) ;
#225789 = CARTESIAN_POINT ( 'NONE',  ( 21.14999999999999858, 67.21339244341194785, -124.2731074845243597 ) ) ;
#225790 = CIRCLE ( 'NONE', #167576, 0.5000000000000013323 ) ;
#225791 = VERTEX_POINT ( 'NONE', #79380 ) ;
#225792 = CARTESIAN_POINT ( 'NONE',  ( -20.94999999999999929, 88.41227409416185878, -139.5231074845242745 ) ) ;
#225793 = ORIENTED_EDGE ( 'NONE', *, *, #190134, .T. ) ;
#225794 = CARTESIAN_POINT ( 'NONE',  ( 22.19999999999999929, -11.65000000000000036, 12.09999999999999787 ) ) ;
#225795 = EDGE_CURVE ( 'NONE', #127472, #251836, #98930, .T. ) ;
#225796 = CARTESIAN_POINT ( 'NONE',  ( 23.40000000000005187, 74.16448838626247664, -47.52760213295649550 ) ) ;
#225797 = DIRECTION ( 'NONE',  ( 0.000000000000000000, 0.000000000000000000, 1.000000000000000000 ) ) ;
#225798 = DIRECTION ( 'NONE',  ( 0.000000000000000000, -0.3738317757009718689, 0.9274965247785342815 ) ) ;
#225799 = AXIS2_PLACEMENT_3D ( 'NONE', #84238, #118300, #40071 ) ;
#225800 = DIRECTION ( 'NONE',  ( 0.000000000000000000, 0.000000000000000000, 1.000000000000000000 ) ) ;
#225802 = EDGE_CURVE ( 'NONE', #35026, #59716, #188328, .T. ) ;
#225801 = DIRECTION ( 'NONE',  ( 1.000000000000000000, -0.000000000000000000, -0.000000000000000000 ) ) ;
#225803 = CARTESIAN_POINT ( 'NONE',  ( 20.93302460841142931, 10.31565961587945424, -72.53641941191781939 ) ) ;
#225805 = EDGE_LOOP ( 'NONE', ( #166868, #46801, #207396, #211010 ) ) ;
#225804 = AXIS2_PLACEMENT_3D ( 'NONE', #71879, #230963, #148847 ) ;
#225807 = FACE_OUTER_BOUND ( 'NONE', #152829, .T. ) ;
#225806 = DIRECTION ( 'NONE',  ( -2.952720810173289112E-16, 1.000000000000000000, 0.000000000000000000 ) ) ;
#225808 = ORIENTED_EDGE ( 'NONE', *, *, #112233, .F. ) ;
#225809 = CARTESIAN_POINT ( 'NONE',  ( 23.14999999999999147, 76.00000000001165290, -69.52310748452431710 ) ) ;
#225811 = DIRECTION ( 'NONE',  ( 0.000000000000000000, 6.982962677686266711E-15, -1.000000000000000000 ) ) ;
#225810 = VECTOR ( 'NONE', #258005, 1000.000000000000000 ) ;
#225812 = CARTESIAN_POINT ( 'NONE',  ( -21.45000000000000284, 68.29142135624930177, -115.3731074845243540 ) ) ;
#225814 = ORIENTED_EDGE ( 'NONE', *, *, #3038, .F. ) ;
#225813 = CARTESIAN_POINT ( 'NONE',  ( -18.54260524012575928, -9.624219390062513924, -207.7407730457709079 ) ) ;
#225816 = EDGE_LOOP ( 'NONE', ( #207345, #207057, #29574, #137950 ) ) ;
#225815 = CYLINDRICAL_SURFACE ( 'NONE', #182880, 0.1000000000000000472 ) ;
#225817 = LINE ( 'NONE', #4217, #196343 ) ;
#225819 = VERTEX_POINT ( 'NONE', #242316 ) ;
#225818 = LINE ( 'NONE', #47187, #161331 ) ;
#225820 = AXIS2_PLACEMENT_3D ( 'NONE', #42751, #105246, #240957 ) ;
#225821 = FACE_OUTER_BOUND ( 'NONE', #114328, .T. ) ;
#225822 = CARTESIAN_POINT ( 'NONE',  ( -20.94999999999999929, 76.00000000001213607, -136.5231074845243313 ) ) ;
#225823 = EDGE_LOOP ( 'NONE', ( #194005, #82424, #39854, #30503 ) ) ;
#225824 = DIRECTION ( 'NONE',  ( -1.000000000000000000, 1.207181226542539700E-16, -2.694675058168174199E-16 ) ) ;
#225825 = VERTEX_POINT ( 'NONE', #143209 ) ;
#225826 = DIRECTION ( 'NONE',  ( 0.000000000000000000, 0.000000000000000000, 1.000000000000000000 ) ) ;
#225827 = CARTESIAN_POINT ( 'NONE',  ( 19.75857864376269291, 34.44688795055758845, -235.1500552906961730 ) ) ;
#225828 = ORIENTED_EDGE ( 'NONE', *, *, #69293, .T. ) ;
#225829 = CARTESIAN_POINT ( 'NONE',  ( -21.05000000000000071, 36.65892442174472876, -249.5511627012454596 ) ) ;
#225830 = AXIS2_PLACEMENT_3D ( 'NONE', #139539, #178721, #40496 ) ;
#225831 = EDGE_CURVE ( 'NONE', #243619, #178254, #5139, .T. ) ;
#225832 = DIRECTION ( 'NONE',  ( -0.000000000000000000, 0.8660254037844383745, -0.5000000000000003331 ) ) ;
#225833 = CIRCLE ( 'NONE', #234228, 4.050000000000000711 ) ;
#225834 = VERTEX_POINT ( 'NONE', #23307 ) ;
#225835 = CARTESIAN_POINT ( 'NONE',  ( 23.14999999999999858, 70.50000000001253397, -182.4283735034374843 ) ) ;
#225836 = ORIENTED_EDGE ( 'NONE', *, *, #26671, .T. ) ;
#225837 = ORIENTED_EDGE ( 'NONE', *, *, #134187, .F. ) ;
#225838 = CARTESIAN_POINT ( 'NONE',  ( -18.44204374631831200, -9.491036389587213407, -73.62620127022113081 ) ) ;
#225839 = ORIENTED_EDGE ( 'NONE', *, *, #113359, .T. ) ;
#225840 = EDGE_CURVE ( 'NONE', #195640, #134466, #237198, .T. ) ;
#225841 = DIRECTION ( 'NONE',  ( 0.000000000000000000, -0.9908441862701791170, 0.1350103645450472789 ) ) ;
#225842 = ORIENTED_EDGE ( 'NONE', *, *, #243426, .T. ) ;
#225844 = ORIENTED_EDGE ( 'NONE', *, *, #156421, .F. ) ;
#225843 = DIRECTION ( 'NONE',  ( 0.000000000000000000, -0.9160831752668552319, -0.4009882990724247809 ) ) ;
#225846 = EDGE_CURVE ( 'NONE', #19404, #163287, #196766, .T. ) ;
#225845 = CARTESIAN_POINT ( 'NONE',  ( 21.05000000000000071, 62.04503132991427350, -248.4786563706009588 ) ) ;
#225847 = EDGE_LOOP ( 'NONE', ( #45978, #198836, #113001, #72672, #117616 ) ) ;
#225848 = CYLINDRICAL_SURFACE ( 'NONE', #89110, 0.09999999999999939493 ) ;
#225849 = ORIENTED_EDGE ( 'NONE', *, *, #117024, .F. ) ;
#225851 = ORIENTED_EDGE ( 'NONE', *, *, #89929, .T. ) ;
#225850 = VERTEX_POINT ( 'NONE', #239765 ) ;
#225852 = CARTESIAN_POINT ( 'NONE',  ( 20.85000000000000142, -11.64999999999999147, -33.50000000000000000 ) ) ;
#225854 = CARTESIAN_POINT ( 'NONE',  ( 18.39999999999997371, 64.25000000001264766, -194.2731074845244450 ) ) ;
#225853 = CIRCLE ( 'NONE', #121853, 0.1000000000000028644 ) ;
#225856 = EDGE_CURVE ( 'NONE', #114049, #243012, #180163, .T. ) ;
#225855 = ORIENTED_EDGE ( 'NONE', *, *, #34449, .F. ) ;
#225857 = AXIS2_PLACEMENT_3D ( 'NONE', #250329, #139347, #255412 ) ;
#225858 = EDGE_CURVE ( 'NONE', #28028, #233325, #141932, .T. ) ;
#225859 = EDGE_CURVE ( 'NONE', #107947, #198131, #218894, .T. ) ;
#225860 = ORIENTED_EDGE ( 'NONE', *, *, #133818, .T. ) ;
#225861 = CARTESIAN_POINT ( 'NONE',  ( -21.05000000000000071, 69.74115727647347285, -203.5551211777124934 ) ) ;
#225863 = DIRECTION ( 'NONE',  ( 1.000000000000000000, -0.000000000000000000, -0.000000000000000000 ) ) ;
#225862 = VECTOR ( 'NONE', #250922, 1000.000000000000000 ) ;
#225865 = ORIENTED_EDGE ( 'NONE', *, *, #58797, .F. ) ;
#225864 = DIRECTION ( 'NONE',  ( 0.000000000000000000, 0.000000000000000000, 1.000000000000000000 ) ) ;
#225866 = FACE_OUTER_BOUND ( 'NONE', #117860, .T. ) ;
#225867 = ORIENTED_EDGE ( 'NONE', *, *, #199886, .F. ) ;
#225868 = EDGE_CURVE ( 'NONE', #252063, #221674, #241058, .T. ) ;
#225869 = DIRECTION ( 'NONE',  ( 0.000000000000000000, 0.000000000000000000, -1.000000000000000000 ) ) ;
#225870 = CARTESIAN_POINT ( 'NONE',  ( 18.49999999999999289, 65.50857864377465489, -111.7731074845243597 ) ) ;
#225871 = CIRCLE ( 'NONE', #171770, 11.65000000000000746 ) ;
#225872 = ORIENTED_EDGE ( 'NONE', *, *, #157064, .F. ) ;
#225873 = DIRECTION ( 'NONE',  ( 0.000000000000000000, 0.000000000000000000, 1.000000000000000000 ) ) ;
#225875 = EDGE_CURVE ( 'NONE', #162811, #204755, #59295, .T. ) ;
#225874 = AXIS2_PLACEMENT_3D ( 'NONE', #166892, #207285, #246396 ) ;
#225876 = AXIS2_PLACEMENT_3D ( 'NONE', #79486, #39120, #118657 ) ;
#225878 = ORIENTED_EDGE ( 'NONE', *, *, #88227, .F. ) ;
#225877 = CIRCLE ( 'NONE', #9422, 0.09999999999999983902 ) ;
#225879 = CARTESIAN_POINT ( 'NONE',  ( 19.96984138294275368, 54.41891991186830779, -228.7197075361649183 ) ) ;
#225880 = AXIS2_PLACEMENT_3D ( 'NONE', #57012, #160021, #256456 ) ;
#225881 = AXIS2_PLACEMENT_3D ( 'NONE', #167826, #46544, #145649 ) ;
#225883 = ORIENTED_EDGE ( 'NONE', *, *, #252259, .T. ) ;
#225882 = ORIENTED_EDGE ( 'NONE', *, *, #53113, .F. ) ;
#225884 = ORIENTED_EDGE ( 'NONE', *, *, #227484, .T. ) ;
#225885 = CARTESIAN_POINT ( 'NONE',  ( -17.11825945287481332, 65.95000000001255103, -182.6731074845244223 ) ) ;
#225886 = ORIENTED_EDGE ( 'NONE', *, *, #238838, .T. ) ;
#225887 = FACE_OUTER_BOUND ( 'NONE', #126830, .T. ) ;
#225888 = ORIENTED_EDGE ( 'NONE', *, *, #185717, .T. ) ;
#225889 = CIRCLE ( 'NONE', #171795, 7.800000000000001599 ) ;
#225890 = PLANE ( 'NONE',  #119122 ) ;
#225891 = EDGE_CURVE ( 'NONE', #225448, #169411, #171802, .T. ) ;
#225893 = VERTEX_POINT ( 'NONE', #199364 ) ;
#225892 = VECTOR ( 'NONE', #215441, 1000.000000000000000 ) ;
#225894 = ORIENTED_EDGE ( 'NONE', *, *, #38022, .T. ) ;
#225895 = VECTOR ( 'NONE', #50821, 1000.000000000000000 ) ;
#225896 = ORIENTED_EDGE ( 'NONE', *, *, #124201, .T. ) ;
#225897 = TOROIDAL_SURFACE ( 'NONE', #13560, 0.2000000000000000111, 0.1000000000000000056 ) ;
#225898 = VECTOR ( 'NONE', #146818, 1000.000000000000000 ) ;
#225899 = ADVANCED_FACE ( 'NONE', ( #61114 ), #3705, .T. ) ;
#225900 = DIRECTION ( 'NONE',  ( 0.000000000000000000, 0.2617529984165031243, 0.9651348961777157509 ) ) ;
#225901 = EDGE_LOOP ( 'NONE', ( #104380, #106341, #227450, #136048 ) ) ;
#225902 = VECTOR ( 'NONE', #162468, 1000.000000000000000 ) ;
#225904 = ORIENTED_EDGE ( 'NONE', *, *, #236912, .T. ) ;
#225903 = CARTESIAN_POINT ( 'NONE',  ( 23.14999999999999858, 69.35000000001186038, -90.67310748452435121 ) ) ;
#225905 = DIRECTION ( 'NONE',  ( 0.000000000000000000, 0.6728971962616783209, 0.7397360091702797069 ) ) ;
#225906 = FACE_OUTER_BOUND ( 'NONE', #198995, .T. ) ;
#225907 = CARTESIAN_POINT ( 'NONE',  ( 20.85000000000000142, 43.08613539620618837, -254.3146655184800409 ) ) ;
#225908 = CARTESIAN_POINT ( 'NONE',  ( 21.04999999999999716, -0.03753606327451243507, -127.6677277260643564 ) ) ;
#225909 = DIRECTION ( 'NONE',  ( -1.000000000000000000, -7.304098846218135653E-16, 4.607487905232624742E-31 ) ) ;
#225911 = DIRECTION ( 'NONE',  ( 0.000000000000000000, 0.000000000000000000, -1.000000000000000000 ) ) ;
#225910 = FACE_OUTER_BOUND ( 'NONE', #71683, .T. ) ;
#225912 = DIRECTION ( 'NONE',  ( 1.000000000000000000, -0.000000000000000000, 0.000000000000000000 ) ) ;
#225913 = DIRECTION ( 'NONE',  ( 1.000000000000000000, 0.000000000000000000, 0.000000000000000000 ) ) ;
#225914 = EDGE_CURVE ( 'NONE', #24822, #98560, #17922, .T. ) ;
#225915 = VECTOR ( 'NONE', #183426, 1000.000000000000000 ) ;
#225917 = VERTEX_POINT ( 'NONE', #122382 ) ;
#225916 = VECTOR ( 'NONE', #9002, 1000.000000000000000 ) ;
#225918 = EDGE_CURVE ( 'NONE', #82535, #135547, #147104, .T. ) ;
#225919 = ORIENTED_EDGE ( 'NONE', *, *, #92026, .F. ) ;
#225921 = ORIENTED_EDGE ( 'NONE', *, *, #85576, .T. ) ;
#225920 = CARTESIAN_POINT ( 'NONE',  ( 21.05000000000000071, 67.22371710472012296, -191.3731074845244109 ) ) ;
#225922 = ORIENTED_EDGE ( 'NONE', *, *, #146143, .T. ) ;
#225923 = CARTESIAN_POINT ( 'NONE',  ( -20.65000000000000568, 70.35000000001230092, -157.3731074845244109 ) ) ;
#225924 = EDGE_CURVE ( 'NONE', #99917, #174669, #126260, .T. ) ;
#225925 = CARTESIAN_POINT ( 'NONE',  ( 20.12481660106788084, 9.526343992285099205, -142.2261416690962506 ) ) ;
#225927 = CARTESIAN_POINT ( 'NONE',  ( 18.39999999999999503, 11.75000000001113953, -121.3500000000000369 ) ) ;
#225926 = CARTESIAN_POINT ( 'NONE',  ( 20.74897398619109978, 39.33521109263118376, -236.7418682356311876 ) ) ;
#225928 = ORIENTED_EDGE ( 'NONE', *, *, #249137, .F. ) ;
#225929 = ADVANCED_FACE ( 'NONE', ( #165360 ), #105339, .T. ) ;
#225930 = SURFACE_STYLE_USAGE ( .BOTH. , #87719 ) ;
#225931 = EDGE_CURVE ( 'NONE', #39964, #205600, #6263, .T. ) ;
#225932 = CARTESIAN_POINT ( 'NONE',  ( 21.03675099975491136, 67.12481996722674182, -57.19756534774633394 ) ) ;
#225933 = CARTESIAN_POINT ( 'NONE',  ( 18.54999999999999716, 66.05000000001254534, -182.6731074845243654 ) ) ;
#225934 = VECTOR ( 'NONE', #124639, 1000.000000000000000 ) ;
#225935 = ORIENTED_EDGE ( 'NONE', *, *, #255971, .T. ) ;
#225936 = PLANE ( 'NONE',  #96447 ) ;
#225937 = LINE ( 'NONE', #228557, #46470 ) ;
#225938 = DIRECTION ( 'NONE',  ( -1.000000000000000000, 0.000000000000000000, 0.000000000000000000 ) ) ;
#225939 = EDGE_CURVE ( 'NONE', #200951, #52766, #184512, .T. ) ;
#225940 = AXIS2_PLACEMENT_3D ( 'NONE', #87511, #31448, #109648 ) ;
#225941 = DIRECTION ( 'NONE',  ( -1.000000000000000000, 0.000000000000000000, 0.000000000000000000 ) ) ;
#225943 = EDGE_LOOP ( 'NONE', ( #15933, #149054, #76012, #95471, #78271, #14029, #79874, #76706 ) ) ;
#225942 = LINE ( 'NONE', #85142, #197782 ) ;
#225944 = DIRECTION ( 'NONE',  ( 2.952720810173289112E-16, -1.000000000000000000, 0.000000000000000000 ) ) ;
#225945 = CARTESIAN_POINT ( 'NONE',  ( 23.14999999999999858, 19.82851818057134707, -235.1178474969725016 ) ) ;
#225946 = FACE_OUTER_BOUND ( 'NONE', #237570, .T. ) ;
#225947 = CARTESIAN_POINT ( 'NONE',  ( -18.50000000000000000, 70.65875701002110532, -213.3297576910124178 ) ) ;
#225948 = ORIENTED_EDGE ( 'NONE', *, *, #178003, .T. ) ;
#225949 = CARTESIAN_POINT ( 'NONE',  ( 23.50000000000004263, 74.73834681386826162, -44.00978271863746016 ) ) ;
#225950 = DIRECTION ( 'NONE',  ( 0.000000000000000000, -1.000000000000000000, -2.891205793294679805E-16 ) ) ;
#225952 = DIRECTION ( 'NONE',  ( 0.000000000000000000, 0.000000000000000000, -1.000000000000000000 ) ) ;
#225951 = CARTESIAN_POINT ( 'NONE',  ( 21.05000000000000071, 76.00000000001190870, -103.0231074845243029 ) ) ;
#225953 = DIRECTION ( 'NONE',  ( 0.000000000000000000, 1.734723475976807292E-15, -1.000000000000000000 ) ) ;
#225954 = CARTESIAN_POINT ( 'NONE',  ( 17.74533788810830615, 65.18150020854078264, -59.20948480957681426 ) ) ;
#225955 = DIRECTION ( 'NONE',  ( 0.000000000000000000, 1.000000000000000000, 0.000000000000000000 ) ) ;
#225956 = CARTESIAN_POINT ( 'NONE',  ( -23.25000000000000000, 87.75000000001173817, -72.62310748452422615 ) ) ;
#225957 = CARTESIAN_POINT ( 'NONE',  ( 20.94999999999999929, -9.000000000000001776, -9.893969122652443104 ) ) ;
#225958 = ORIENTED_EDGE ( 'NONE', *, *, #80214, .F. ) ;
#225960 = CIRCLE ( 'NONE', #51181, 0.09999999999999939493 ) ;
#225959 = DIRECTION ( 'NONE',  ( 1.000000000000000000, 0.000000000000000000, 0.000000000000000000 ) ) ;
#225961 = VERTEX_POINT ( 'NONE', #126218 ) ;
#225962 = ORIENTED_EDGE ( 'NONE', *, *, #118369, .T. ) ;
#225963 = CARTESIAN_POINT ( 'NONE',  ( 20.74897398619119215, 65.40430697834545981, -95.34379602826817290 ) ) ;
#225964 = CARTESIAN_POINT ( 'NONE',  ( 23.14999999999999503, 29.08883969319483498, -237.9520757887960940 ) ) ;
#225965 = EDGE_CURVE ( 'NONE', #77430, #163271, #128809, .T. ) ;
#225966 = ORIENTED_EDGE ( 'NONE', *, *, #134222, .F. ) ;
#225967 = EDGE_CURVE ( 'NONE', #224903, #74036, #251143, .T. ) ;
#225968 = EDGE_LOOP ( 'NONE', ( #29455, #59088, #161010, #214776 ) ) ;
#225969 = AXIS2_PLACEMENT_3D ( 'NONE', #152006, #174152, #196227 ) ;
#225970 = B_SPLINE_CURVE_WITH_KNOTS ( 'NONE', 3,
 ( #111518, #128515, #91946, #189768, #90653, #228900, #210613 ),
 .UNSPECIFIED., .F., .F.,
 ( 4, 3, 4 ),
 ( 0.000000000000000000, 3.882884552234471334E-05, 5.798605692158493495E-05 ),
 .UNSPECIFIED. ) ;
#225971 = VERTEX_POINT ( 'NONE', #10137 ) ;
#225972 = DIRECTION ( 'NONE',  ( 1.000000000000000000, 0.000000000000000000, -0.000000000000000000 ) ) ;
#225973 = ORIENTED_EDGE ( 'NONE', *, *, #67837, .F. ) ;
#225974 = AXIS2_PLACEMENT_3D ( 'NONE', #71579, #230640, #247623 ) ;
#225975 = DIRECTION ( 'NONE',  ( 0.000000000000000000, 0.2128009952263403282, -0.9770955615653358350 ) ) ;
#225976 = CARTESIAN_POINT ( 'NONE',  ( 21.05000000000000071, 3.338403738567039980, -231.7022719401450104 ) ) ;
#225977 = CARTESIAN_POINT ( 'NONE',  ( -16.93294127766158752, 30.30192492100473700, -234.7978104885644370 ) ) ;
#225978 = CARTESIAN_POINT ( 'NONE',  ( -22.39999999999999858, 10.71943444926882449, -226.8179467668883547 ) ) ;
#225979 = FACE_OUTER_BOUND ( 'NONE', #183173, .T. ) ;
#225980 = AXIS2_PLACEMENT_3D ( 'NONE', #137175, #81031, #138435 ) ;
#225981 =( BOUNDED_SURFACE ( )  B_SPLINE_SURFACE ( 3, 2, ( 
 ( #192529, #133827, #34763 ),
 ( #70033, #8756, #229090 ),
 ( #230360, #227789, #50418 ),
 ( #209515, #10032, #90843 ) ),
 .UNSPECIFIED., .F., .F., .F. ) 
 B_SPLINE_SURFACE_WITH_KNOTS ( ( 4, 4 ),
 ( 3, 3 ),
 ( 0.0008258556059633882047, 0.0009616864997632823065 ),
 ( 0.000000000000000000, 1.000000000000000000 ),
 .UNSPECIFIED. ) 
 GEOMETRIC_REPRESENTATION_ITEM ( )  RATIONAL_B_SPLINE_SURFACE ( (
 ( 1.000000000000000000, 0.9152888060719445162, 1.000000000000000000),
 ( 1.000000000000000000, 0.9327727094138145159, 1.000000000000000000),
 ( 1.000000000000000000, 0.9369023509258376237, 1.000000000000000000),
 ( 1.000000000000000000, 0.9246339933864682337, 1.000000000000000000) ) ) 
 REPRESENTATION_ITEM ( '' )  SURFACE ( )  );
#225982 = DIRECTION ( 'NONE',  ( 0.000000000000000000, -6.982962677686266711E-15, 1.000000000000000000 ) ) ;
#225983 = CARTESIAN_POINT ( 'NONE',  ( 21.00000000000000000, 9.750000000011153745, -45.85000000000000142 ) ) ;
#225985 = ORIENTED_EDGE ( 'NONE', *, *, #164436, .T. ) ;
#225984 = FACE_OUTER_BOUND ( 'NONE', #65567, .T. ) ;
#225987 = LINE ( 'NONE', #47367, #200196 ) ;
#225986 = CARTESIAN_POINT ( 'NONE',  ( -23.15000000000000213, 64.35000000001173248, -81.27310748452440237 ) ) ;
#225988 = DIRECTION ( 'NONE',  ( 0.000000000000000000, -0.000000000000000000, 1.000000000000000000 ) ) ;
#225989 = ORIENTED_EDGE ( 'NONE', *, *, #285, .T. ) ;
#225990 = CARTESIAN_POINT ( 'NONE',  ( -20.64999999999999858, 84.66355140188136374, -146.0472086025916099 ) ) ;
#225991 = CARTESIAN_POINT ( 'NONE',  ( -21.05000000000000071, 74.16465844978787914, -158.3679561919613832 ) ) ;
#225992 = CARTESIAN_POINT ( 'NONE',  ( 21.04999999999999716, 0.06570161033324389832, -60.74168394266798998 ) ) ;
#225993 = EDGE_LOOP ( 'NONE', ( #17276, #84365, #252243, #151677 ) ) ;
#225994 = CIRCLE ( 'NONE', #126049, 7.720710678118663850 ) ;
#225996 = CARTESIAN_POINT ( 'NONE',  ( -16.93658211146644987, 66.00589133767080341, -115.6188124145686942 ) ) ;
#225995 = AXIS2_PLACEMENT_3D ( 'NONE', #173015, #107853, #131268 ) ;
#225997 = EDGE_CURVE ( 'NONE', #167959, #44364, #55304, .T. ) ;
#225998 = CARTESIAN_POINT ( 'NONE',  ( -16.77308656112214535, 66.05000000001183480, -82.17330067622667400 ) ) ;
#225999 = ORIENTED_EDGE ( 'NONE', *, *, #113844, .F. ) ;
#226000 = CARTESIAN_POINT ( 'NONE',  ( 20.94999999999999574, 1.115600667400684642E-11, -67.00000000000004263 ) ) ;
#226001 = PLANE ( 'NONE',  #57924 ) ;
#226002 = VECTOR ( 'NONE', #71899, 1000.000000000000000 ) ;
#226003 = DIRECTION ( 'NONE',  ( 0.000000000000000000, 0.000000000000000000, -1.000000000000000000 ) ) ;
#226004 = ADVANCED_FACE ( 'NONE', ( #27166 ), #167955, .F. ) ;
#226005 = DIRECTION ( 'NONE',  ( 0.000000000000000000, 0.9915357197604892647, -0.1298341882519715440 ) ) ;
#226006 = VERTEX_POINT ( 'NONE', #106638 ) ;
#226007 = EDGE_LOOP ( 'NONE', ( #243087, #80340, #100233, #185494 ) ) ;
#226008 = CIRCLE ( 'NONE', #59407, 1.900000000000004574 ) ;
#226009 = EDGE_CURVE ( 'NONE', #182849, #27184, #142802, .T. ) ;
#226010 = AXIS2_PLACEMENT_3D ( 'NONE', #244741, #102650, #161389 ) ;
#226011 = VECTOR ( 'NONE', #61568, 1000.000000000000000 ) ;
#226012 = LINE ( 'NONE', #227328, #39958 ) ;
#226013 = DIRECTION ( 'NONE',  ( 1.000000000000000000, 0.000000000000000000, 0.000000000000000000 ) ) ;
#226014 = SPHERICAL_SURFACE ( 'NONE', #206938, 0.1000000000000000056 ) ;
#226015 = EDGE_CURVE ( 'NONE', #78170, #156714, #186210, .T. ) ;
#226016 = DIRECTION ( 'NONE',  ( 1.000000000000000000, 0.000000000000000000, 0.000000000000000000 ) ) ;
#226017 = DIRECTION ( 'NONE',  ( 0.000000000000000000, 0.000000000000000000, -1.000000000000000000 ) ) ;
#226018 = VERTEX_POINT ( 'NONE', #203193 ) ;
#226019 = FACE_OUTER_BOUND ( 'NONE', #133855, .T. ) ;
#226020 = EDGE_CURVE ( 'NONE', #198338, #201217, #121988, .T. ) ;
#226022 = VERTEX_POINT ( 'NONE', #225302 ) ;
#226021 = CARTESIAN_POINT ( 'NONE',  ( -20.54999999999999716, 70.60814576644823148, -215.7631455941064189 ) ) ;
#226023 = DIRECTION ( 'NONE',  ( -1.000000000000000000, 0.000000000000000000, -0.000000000000000000 ) ) ;
#226025 = ADVANCED_FACE ( 'NONE', ( #144483 ), #147058, .T. ) ;
#226024 = ADVANCED_FACE ( 'NONE', ( #67534 ), #226594, .T. ) ;
#226026 = CARTESIAN_POINT ( 'NONE',  ( -20.85000000000000142, 7.021664781911246322, -204.8335654018972605 ) ) ;
#226027 = CARTESIAN_POINT ( 'NONE',  ( 21.05000000000000071, 85.00000000001222134, -146.4170766071767389 ) ) ;
#226028 = CARTESIAN_POINT ( 'NONE',  ( -23.15000000000000213, -11.48912529306489994, -63.89999999999999858 ) ) ;
#226030 = ORIENTED_EDGE ( 'NONE', *, *, #110953, .F. ) ;
#226029 = CARTESIAN_POINT ( 'NONE',  ( -23.25000000000000000, 76.00000000001213607, -136.5231074845243313 ) ) ;
#226031 = DIRECTION ( 'NONE',  ( -6.938893903907222067E-15, -1.000000000000000000, -6.982962677686266711E-15 ) ) ;
#226032 = CARTESIAN_POINT ( 'NONE',  ( -18.50211644919735576, 65.69792220476374212, -164.5335554128461979 ) ) ;
#226033 = CARTESIAN_POINT ( 'NONE',  ( -18.59999999999999787, -9.321008403350132809, -40.73593824907788274 ) ) ;
#226034 = CARTESIAN_POINT ( 'NONE',  ( 20.94999999999999929, 70.50000000001185185, -90.61784146561124942 ) ) ;
#226035 = ORIENTED_EDGE ( 'NONE', *, *, #61688, .T. ) ;
#226036 = CARTESIAN_POINT ( 'NONE',  ( 18.50000000000001066, -7.567701079425766864, -210.0537230116848377 ) ) ;
#226037 = DIRECTION ( 'NONE',  ( 0.000000000000000000, -0.9915357197604971473, 0.1298341882519111479 ) ) ;
#226038 = CARTESIAN_POINT ( 'NONE',  ( -18.52328366898030865, 87.06376465862938119, -199.5663074770583592 ) ) ;
#226039 = CIRCLE ( 'NONE', #47165, 0.09999999999998898659 ) ;
#226040 = DIRECTION ( 'NONE',  ( -1.000000000000000000, 7.304098846218133681E-16, -4.217023435051677994E-16 ) ) ;
#226041 = ORIENTED_EDGE ( 'NONE', *, *, #50554, .F. ) ;
#226042 = DIRECTION ( 'NONE',  ( -0.000000000000000000, 1.000000000000000000, -0.000000000000000000 ) ) ;
#226043 = ADVANCED_FACE ( 'NONE', ( #248752 ), #47964, .F. ) ;
#226044 = ADVANCED_FACE ( 'NONE', ( #127517 ), #224030, .F. ) ;
#226045 = ORIENTED_EDGE ( 'NONE', *, *, #190900, .F. ) ;
#226046 = CARTESIAN_POINT ( 'NONE',  ( -22.48660254037843487, 11.65000000001115588, -167.4499999999999886 ) ) ;
#226047 = FACE_OUTER_BOUND ( 'NONE', #47859, .T. ) ;
#226048 = AXIS2_PLACEMENT_3D ( 'NONE', #12637, #214655, #13907 ) ;
#226049 = ADVANCED_FACE ( 'NONE', ( #90947 ), #131359, .T. ) ;
#226050 = AXIS2_PLACEMENT_3D ( 'NONE', #206384, #68152, #147693 ) ;
#226051 = CARTESIAN_POINT ( 'NONE',  ( 23.24999999999999289, 6.650000000011155876, -121.8500000000000369 ) ) ;
#226052 = FACE_OUTER_BOUND ( 'NONE', #223554, .T. ) ;
#226053 = ORIENTED_EDGE ( 'NONE', *, *, #213937, .T. ) ;
#226054 =( BOUNDED_SURFACE ( )  B_SPLINE_SURFACE ( 3, 2, ( 
 ( #88952, #207655, #180697 ),
 ( #181978, #81553, #42454 ),
 ( #122003, #102397, #3309 ),
 ( #82832, #63297, #142817 ) ),
 .UNSPECIFIED., .F., .F., .F. ) 
 B_SPLINE_SURFACE_WITH_KNOTS ( ( 4, 4 ),
 ( 3, 3 ),
 ( 0.0008258556059633687975, 0.0009616864997632754760 ),
 ( 0.000000000000000000, 1.000000000000000000 ),
 .UNSPECIFIED. ) 
 GEOMETRIC_REPRESENTATION_ITEM ( )  RATIONAL_B_SPLINE_SURFACE ( (
 ( 1.000000000000000000, 0.9152888060719464036, 1.000000000000000000),
 ( 1.000000000000000000, 0.9327727094138169583, 1.000000000000000000),
 ( 1.000000000000000000, 0.9369023509258193050, 1.000000000000000000),
 ( 1.000000000000000000, 0.9246339933864469174, 1.000000000000000000) ) ) 
 REPRESENTATION_ITEM ( '' )  SURFACE ( )  );
#226055 = AXIS2_PLACEMENT_3D ( 'NONE', #20153, #44532, #219608 ) ;
#226056 = CYLINDRICAL_SURFACE ( 'NONE', #221390, 0.09999999999999939493 ) ;
#226057 = EDGE_CURVE ( 'NONE', #80064, #101254, #152242, .T. ) ;
#226058 = CARTESIAN_POINT ( 'NONE',  ( -18.59999999999999787, 13.96869538424787649, -210.3925794786331949 ) ) ;
#226059 = CIRCLE ( 'NONE', #13707, 0.09999999999999939493 ) ;
#226060 = VECTOR ( 'NONE', #156067, 999.9999999999998863 ) ;
#226061 = ADVANCED_FACE ( 'NONE', ( #92225 ), #39480, .F. ) ;
#226062 = CARTESIAN_POINT ( 'NONE',  ( 15.69410316191958898, 9.356746017078247490, -17.20335972136419755 ) ) ;
#226063 = FACE_OUTER_BOUND ( 'NONE', #257913, .T. ) ;
#226064 = CYLINDRICAL_SURFACE ( 'NONE', #99133, 0.09999999999999939493 ) ;
#226065 = VERTEX_POINT ( 'NONE', #50515 ) ;
#226067 = ORIENTED_EDGE ( 'NONE', *, *, #186253, .F. ) ;
#226066 = CARTESIAN_POINT ( 'NONE',  ( 20.92356734117541706, 10.31973158071402175, -106.0505334713354841 ) ) ;
#226068 = VECTOR ( 'NONE', #88226, 1000.000000000000000 ) ;
#226069 = VERTEX_POINT ( 'NONE', #171814 ) ;
#226070 = LINE ( 'NONE', #245667, #40539 ) ;
#226071 = ORIENTED_EDGE ( 'NONE', *, *, #218294, .T. ) ;
#226072 = DIRECTION ( 'NONE',  ( 0.000000000000000000, -0.6728971962616697722, -0.7397360091702875895 ) ) ;
#226073 = CARTESIAN_POINT ( 'NONE',  ( -16.97683809663752186, 9.950000000011138823, -46.90236401819648648 ) ) ;
#226074 = DIRECTION ( 'NONE',  ( 0.000000000000000000, -0.8660254037844419273, 0.4999999999999942824 ) ) ;
#226075 = ORIENTED_EDGE ( 'NONE', *, *, #192546, .T. ) ;
#226076 = EDGE_CURVE ( 'NONE', #86390, #196737, #242788, .T. ) ;
#226077 = CARTESIAN_POINT ( 'NONE',  ( -23.15000000000000213, 12.67709964810647882, -223.3751320524553705 ) ) ;
#226078 = DIRECTION ( 'NONE',  ( 0.000000000000000000, 0.9908441862701791170, -0.1350103645450472789 ) ) ;
#226080 = CARTESIAN_POINT ( 'NONE',  ( 20.30531438145591139, 10.09690106110208596, -41.29601780727334415 ) ) ;
#226079 = AXIS2_PLACEMENT_3D ( 'NONE', #71122, #13687, #151948 ) ;
#226081 = EDGE_LOOP ( 'NONE', ( #235278, #14135 ) ) ;
#226082 = DIRECTION ( 'NONE',  ( -0.7071067811865463515, 0.7071067811865487940, -0.000000000000000000 ) ) ;
#226083 = AXIS2_PLACEMENT_3D ( 'NONE', #66346, #63766, #123755 ) ;
#226085 = VERTEX_POINT ( 'NONE', #11433 ) ;
#226084 = CARTESIAN_POINT ( 'NONE',  ( -21.14999999999999858, 1.148907358139439339E-11, -201.0000000000015064 ) ) ;
#226086 = CARTESIAN_POINT ( 'NONE',  ( -20.94999999999999929, -11.48912529306489994, -97.50000000000004263 ) ) ;
#226087 = FACE_OUTER_BOUND ( 'NONE', #217293, .T. ) ;
#226088 = EDGE_CURVE ( 'NONE', #79663, #235074, #149667, .T. ) ;
#226089 = AXIS2_PLACEMENT_3D ( 'NONE', #107851, #187407, #88262 ) ;
#226090 = CIRCLE ( 'NONE', #251042, 0.1000000000000124678 ) ;
#226091 = VERTEX_POINT ( 'NONE', #214746 ) ;
#226093 =( BOUNDED_CURVE ( )  B_SPLINE_CURVE ( 3, ( #148372, #227907, #85786, #204476 ),
 .UNSPECIFIED., .F., .T. ) 
 B_SPLINE_CURVE_WITH_KNOTS ( ( 4, 4 ),
 ( 1.570796326794977382, 3.141592653589781570 ),
 .UNSPECIFIED. ) 
 CURVE ( )  GEOMETRIC_REPRESENTATION_ITEM ( )  RATIONAL_B_SPLINE_CURVE ( ( 1.000000000000000000, 0.8047378541243868089, 0.8047378541243868089, 1.000000000000000000 ) ) 
 REPRESENTATION_ITEM ( '' )  );
#226092 = VECTOR ( 'NONE', #216771, 1000.000000000000000 ) ;
#226094 = CIRCLE ( 'NONE', #242685, 0.09999999999998898659 ) ;
#226095 = LINE ( 'NONE', #102283, #122701 ) ;
#226096 = DIRECTION ( 'NONE',  ( -0.4999999999999800160, 0.7903412497644920487, 0.3540631425617770112 ) ) ;
#226097 = CIRCLE ( 'NONE', #138598, 0.1000000000000028644 ) ;
#226098 = CARTESIAN_POINT ( 'NONE',  ( -23.25000000000000355, 64.25000000001188027, -90.37310748452439668 ) ) ;
#226099 = ORIENTED_EDGE ( 'NONE', *, *, #210323, .F. ) ;
#226100 = EDGE_CURVE ( 'NONE', #86723, #146761, #134441, .T. ) ;
#226101 = CARTESIAN_POINT ( 'NONE',  ( -18.59999999999999787, -1.687074390080403941, -154.6854270334582964 ) ) ;
#226102 = EDGE_LOOP ( 'NONE', ( #174540, #11660, #109809 ) ) ;
#226103 = CIRCLE ( 'NONE', #51137, 0.09999999999998898659 ) ;
#226104 = AXIS2_PLACEMENT_3D ( 'NONE', #203028, #24430, #243443 ) ;
#226105 = AXIS2_PLACEMENT_3D ( 'NONE', #162686, #184801, #124844 ) ;
#226106 = AXIS2_PLACEMENT_3D ( 'NONE', #116662, #119248, #138753 ) ;
#226107 = ORIENTED_EDGE ( 'NONE', *, *, #66396, .T. ) ;
#226108 = DIRECTION ( 'NONE',  ( 0.000000000000000000, 1.000000000000000000, 6.938893903907222067E-15 ) ) ;
#226109 = EDGE_LOOP ( 'NONE', ( #147599, #181817, #106188, #118266 ) ) ;
#226110 = CARTESIAN_POINT ( 'NONE',  ( 18.49999999999998934, 10.29288807858825905, -38.95800201601215917 ) ) ;
#226111 = DIRECTION ( 'NONE',  ( 0.000000000000000000, 0.9915357197604862671, -0.1298341882519953583 ) ) ;
#226113 = EDGE_LOOP ( 'NONE', ( #47521, #166150, #183022, #67604 ) ) ;
#226112 = DIRECTION ( 'NONE',  ( 0.000000000000000000, 0.000000000000000000, 1.000000000000000000 ) ) ;
#226114 = CYLINDRICAL_SURFACE ( 'NONE', #115967, 5.000000000000000888 ) ;
#226115 = CARTESIAN_POINT ( 'NONE',  ( 21.03670563405602678, 10.62482368933940258, -112.8255468862091817 ) ) ;
#226116 = FACE_OUTER_BOUND ( 'NONE', #131959, .T. ) ;
#226117 = CARTESIAN_POINT ( 'NONE',  ( -21.14999999999999858, -11.64999999998884483, -134.0000000000000000 ) ) ;
#226118 = DIRECTION ( 'NONE',  ( -1.000000000000000000, 0.000000000000000000, -1.020425574104004196E-15 ) ) ;
#226119 = LINE ( 'NONE', #230986, #158586 ) ;
#226120 = CYLINDRICAL_SURFACE ( 'NONE', #59886, 0.09999999999999939493 ) ;
#226121 = DIRECTION ( 'NONE',  ( 1.000000000000000000, 0.000000000000000000, 0.000000000000000000 ) ) ;
#226123 = ORIENTED_EDGE ( 'NONE', *, *, #145870, .F. ) ;
#226122 = LINE ( 'NONE', #21545, #177739 ) ;
#226124 = DIRECTION ( 'NONE',  ( 0.000000000000000000, 0.000000000000000000, -1.000000000000000000 ) ) ;
#226125 = VERTEX_POINT ( 'NONE', #193919 ) ;
#226126 = FACE_OUTER_BOUND ( 'NONE', #194059, .T. ) ;
#226127 = AXIS2_PLACEMENT_3D ( 'NONE', #73491, #34363, #8360 ) ;
#226128 = CARTESIAN_POINT ( 'NONE',  ( 20.30531438145591139, 65.90309893892256810, -195.7270896772506035 ) ) ;
#226129 = CARTESIAN_POINT ( 'NONE',  ( 21.05000000000000071, 1.115600667400684642E-11, -167.4999999999999716 ) ) ;
#226130 = ORIENTED_EDGE ( 'NONE', *, *, #147574, .F. ) ;
#226131 = DIRECTION ( 'NONE',  ( 1.000000000000000000, 0.000000000000000000, 0.000000000000000000 ) ) ;
#226132 = EDGE_CURVE ( 'NONE', #152864, #75024, #54390, .T. ) ;
#226133 = DIRECTION ( 'NONE',  ( 0.000000000000000000, 0.9651348961777118651, -0.2617529984165174461 ) ) ;
#226134 = ORIENTED_EDGE ( 'NONE', *, *, #169255, .F. ) ;
#226135 = CARTESIAN_POINT ( 'NONE',  ( 21.09107601085585770, 75.96069283529571692, -209.8869854598850679 ) ) ;
#226136 = AXIS2_PLACEMENT_3D ( 'NONE', #138200, #173555, #253031 ) ;
#226137 = CARTESIAN_POINT ( 'NONE',  ( 22.50497660315937054, -0.07871793021434789206, -21.75020449510456189 ) ) ;
#226138 = ORIENTED_EDGE ( 'NONE', *, *, #166921, .F. ) ;
#226139 = CARTESIAN_POINT ( 'NONE',  ( -21.05000000000000071, 6.300179817925684489, -66.94851711811826078 ) ) ;
#226140 = VERTEX_POINT ( 'NONE', #229193 ) ;
#226141 = ORIENTED_EDGE ( 'NONE', *, *, #173235, .F. ) ;
#226142 = EDGE_CURVE ( 'NONE', #73461, #117400, #72118, .T. ) ;
#226144 = EDGE_CURVE ( 'NONE', #21468, #239334, #53102, .T. ) ;
#226143 = CARTESIAN_POINT ( 'NONE',  ( -21.05000000000000071, 5.850000000011156942, -56.86750277572208034 ) ) ;
#226145 = LINE ( 'NONE', #90514, #226455 ) ;
#226146 = VERTEX_POINT ( 'NONE', #230468 ) ;
#226147 = VERTEX_POINT ( 'NONE', #55637 ) ;
#226149 = DIRECTION ( 'NONE',  ( 2.952720810173289112E-16, 1.000000000000000000, 6.467318590049456648E-15 ) ) ;
#226148 = AXIS2_PLACEMENT_3D ( 'NONE', #57691, #120292, #201069 ) ;
#226150 = VERTEX_POINT ( 'NONE', #175640 ) ;
#226151 = CARTESIAN_POINT ( 'NONE',  ( -23.15000000000000213, 36.02918351690956200, -236.0543695120161374 ) ) ;
#226152 = ORIENTED_EDGE ( 'NONE', *, *, #176869, .F. ) ;
#226153 = VECTOR ( 'NONE', #189909, 1000.000000000000000 ) ;
#226154 = CIRCLE ( 'NONE', #197152, 0.09999999999999939493 ) ;
#226155 = EDGE_CURVE ( 'NONE', #160843, #211107, #51802, .T. ) ;
#226156 = ADVANCED_FACE ( 'NONE', ( #93512 ), #164349, .T. ) ;
#226157 = ORIENTED_EDGE ( 'NONE', *, *, #212801, .F. ) ;
#226158 = DIRECTION ( 'NONE',  ( 0.7071067811865487940, -4.937700262164522799E-15, 0.7071067811865463515 ) ) ;
#226159 = CARTESIAN_POINT ( 'NONE',  ( 21.05000000000000071, 87.65000000001214175, -136.5231074845242176 ) ) ;
#226160 = LINE ( 'NONE', #26742, #157879 ) ;
#226161 = EDGE_CURVE ( 'NONE', #124945, #58661, #217295, .T. ) ;
#226162 = LINE ( 'NONE', #89249, #125543 ) ;
#226163 = LINE ( 'NONE', #228790, #131272 ) ;
#226164 = CARTESIAN_POINT ( 'NONE',  ( -23.15000000000000213, -8.999999999988844479, -191.1060308773475356 ) ) ;
#226165 = ORIENTED_EDGE ( 'NONE', *, *, #80788, .F. ) ;
#226166 = AXIS2_PLACEMENT_3D ( 'NONE', #244486, #205347, #80242 ) ;
#226167 = CARTESIAN_POINT ( 'NONE',  ( -22.50000000000000000, 11.65000000001115588, -134.0000000000000284 ) ) ;
#226168 = CARTESIAN_POINT ( 'NONE',  ( 21.05000000000000071, 10.41478453976545460, -207.3430624819218622 ) ) ;
#226169 = CARTESIAN_POINT ( 'NONE',  ( 20.95392731769792150, 67.11693852082331091, -128.0008795049530761 ) ) ;
#226170 = VECTOR ( 'NONE', #20211, 1000.000000000000000 ) ;
#226171 = EDGE_CURVE ( 'NONE', #245888, #77303, #59592, .T. ) ;
#226172 = DIRECTION ( 'NONE',  ( 0.000000000000000000, 0.000000000000000000, 1.000000000000000000 ) ) ;
#226173 = EDGE_LOOP ( 'NONE', ( #230300, #146360, #89345, #154512 ) ) ;
#226174 = CARTESIAN_POINT ( 'NONE',  ( 18.57399277249656322, 10.33112638556969820, -106.0901228926975080 ) ) ;
#226175 = VERTEX_POINT ( 'NONE', #141627 ) ;
#226176 = LINE ( 'NONE', #46279, #69097 ) ;
#226177 = ORIENTED_EDGE ( 'NONE', *, *, #216710, .F. ) ;
#226178 = EDGE_CURVE ( 'NONE', #125839, #198947, #92938, .T. ) ;
#226179 = CARTESIAN_POINT ( 'NONE',  ( -23.15000000000000213, -8.596261682231835621, -109.9501275171503210 ) ) ;
#226180 = DIRECTION ( 'NONE',  ( 0.000000000000000000, 0.000000000000000000, -1.000000000000000000 ) ) ;
#226182 = EDGE_LOOP ( 'NONE', ( #144, #12843, #184170, #230338, #88639, #184104, #73521 ) ) ;
#226181 = CIRCLE ( 'NONE', #159588, 4.099999999999992539 ) ;
#226183 = EDGE_LOOP ( 'NONE', ( #247344, #211810, #231426, #201850 ) ) ;
#226185 = ORIENTED_EDGE ( 'NONE', *, *, #131507, .F. ) ;
#226184 = DIRECTION ( 'NONE',  ( -3.890533409366484652E-14, -0.1298341882520124002, -0.9915357197604841577 ) ) ;
#226186 = DIRECTION ( 'NONE',  ( 0.000000000000000000, 0.000000000000000000, -1.000000000000000000 ) ) ;
#226187 = ORIENTED_EDGE ( 'NONE', *, *, #153991, .F. ) ;
#226188 = CARTESIAN_POINT ( 'NONE',  ( -23.15000000000000213, 18.47808476326695626, -239.8121846073901224 ) ) ;
#226189 = CIRCLE ( 'NONE', #55312, 0.1000000000000013933 ) ;
#226190 = CIRCLE ( 'NONE', #13850, 0.1000000000000000472 ) ;
#226191 = AXIS2_PLACEMENT_3D ( 'NONE', #48103, #8980, #49400 ) ;
#226192 = CARTESIAN_POINT ( 'NONE',  ( 18.49999999999999645, 1.115600667400684642E-11, -100.5000000000000426 ) ) ;
#226193 = EDGE_CURVE ( 'NONE', #98150, #246378, #137762, .T. ) ;
#226194 = AXIS2_PLACEMENT_3D ( 'NONE', #98360, #257420, #194965 ) ;
#226195 = EDGE_LOOP ( 'NONE', ( #145779, #148455, #159209, #192503 ) ) ;
#226196 = LINE ( 'NONE', #64579, #243497 ) ;
#226197 = DIRECTION ( 'NONE',  ( 0.000000000000000000, -6.982962677686266711E-15, 1.000000000000000000 ) ) ;
#226198 = ORIENTED_EDGE ( 'NONE', *, *, #71480, .T. ) ;
#226199 = DIRECTION ( 'NONE',  ( 0.000000000000000000, 0.000000000000000000, 1.000000000000000000 ) ) ;
#226200 = FACE_OUTER_BOUND ( 'NONE', #104068, .T. ) ;
#226201 = DIRECTION ( 'NONE',  ( 1.000000000000000000, 0.000000000000000000, 0.000000000000000000 ) ) ;
#226203 = ORIENTED_EDGE ( 'NONE', *, *, #138949, .F. ) ;
#226202 = CARTESIAN_POINT ( 'NONE',  ( -20.64999999999999858, 2.000000000011154189, -120.7753780772379315 ) ) ;
#226204 = DIRECTION ( 'NONE',  ( 0.000000000000000000, 0.000000000000000000, -1.000000000000000000 ) ) ;
#226205 = DIRECTION ( 'NONE',  ( 1.000000000000000000, -7.304098846218133681E-16, 4.607487905232622991E-31 ) ) ;
#226206 = CARTESIAN_POINT ( 'NONE',  ( 18.59999999999999432, 1.162701749949165642, -175.5999999999999659 ) ) ;
#226207 = CIRCLE ( 'NONE', #109714, 0.1000000000000028644 ) ;
#226209 = CARTESIAN_POINT ( 'NONE',  ( -16.91256925476570316, 60.87407910423024049, -221.1459158692213407 ) ) ;
#226208 = DIRECTION ( 'NONE',  ( -1.000000000000000000, 0.000000000000000000, 0.000000000000000000 ) ) ;
#226210 = CARTESIAN_POINT ( 'NONE',  ( -20.85000000000000142, -1.835859311443637010, -45.10443916879852821 ) ) ;
#226211 = DIRECTION ( 'NONE',  ( 0.000000000000000000, -0.1350103645451876666, -0.9908441862701600211 ) ) ;
#226212 = CIRCLE ( 'NONE', #30465, 0.09999999999999939493 ) ;
#226213 = CARTESIAN_POINT ( 'NONE',  ( 23.14999999999999503, 56.06656052939784729, -228.0911609752645290 ) ) ;
#226214 = DIRECTION ( 'NONE',  ( 1.000000000000000000, 1.836970198721029934E-16, 3.186635328391151676E-31 ) ) ;
#226215 = VERTEX_POINT ( 'NONE', #235585 ) ;
#226216 = EDGE_CURVE ( 'NONE', #61591, #114424, #118222, .T. ) ;
#226217 = EDGE_CURVE ( 'NONE', #199798, #232547, #197751, .T. ) ;
#226218 = AXIS2_PLACEMENT_3D ( 'NONE', #159538, #156983, #56539 ) ;
#226219 = VERTEX_POINT ( 'NONE', #56924 ) ;
#226221 = FACE_OUTER_BOUND ( 'NONE', #193831, .T. ) ;
#226220 = AXIS2_PLACEMENT_3D ( 'NONE', #217907, #79686, #23627 ) ;
#226222 = EDGE_LOOP ( 'NONE', ( #101201, #226652, #90256, #96568, #106165, #29475, #1681, #26886, #126232, #18157, #3945, #44152 ) ) ;
#226223 = EDGE_CURVE ( 'NONE', #25429, #16283, #130350, .T. ) ;
#226224 = EDGE_CURVE ( 'NONE', #187394, #87663, #105385, .T. ) ;
#226225 = DIRECTION ( 'NONE',  ( -0.000000000000000000, 0.6922311945860614157, 0.7216758089626911232 ) ) ;
#226226 = VECTOR ( 'NONE', #224124, 1000.000000000000000 ) ;
#226227 = ORIENTED_EDGE ( 'NONE', *, *, #9236, .T. ) ;
#226228 = AXIS2_PLACEMENT_3D ( 'NONE', #18709, #39597, #121686 ) ;
#226229 = EDGE_CURVE ( 'NONE', #13877, #257956, #66080, .T. ) ;
#226231 = AXIS2_PLACEMENT_3D ( 'NONE', #216934, #16208, #57853 ) ;
#226230 = SHAPE_REPRESENTATION_RELATIONSHIP ( 'NONE' , 'NONE' ,  #233377, #191218 ) ;
#226232 = CARTESIAN_POINT ( 'NONE',  ( 20.94999999999999929, 6.277629359189122127, -229.8243190661787878 ) ) ;
#226233 = AXIS2_PLACEMENT_3D ( 'NONE', #117197, #132919, #151197 ) ;
#226234 = CARTESIAN_POINT ( 'NONE',  ( 23.24999999999999289, 6.450000000011156587, -79.35000000000005116 ) ) ;
#226235 = AXIS2_PLACEMENT_3D ( 'NONE', #170184, #209254, #206695 ) ;
#226236 = PRODUCT_DEFINITION_SHAPE ( 'NONE', 'NONE',  #190348 ) ;
#226237 = EDGE_CURVE ( 'NONE', #203708, #41142, #196990, .T. ) ;
#226238 = ORIENTED_EDGE ( 'NONE', *, *, #137648, .F. ) ;
#226239 = PLANE ( 'NONE',  #192228 ) ;
#226240 = EDGE_LOOP ( 'NONE', ( #166330, #244187, #16832, #171179 ) ) ;
#226241 = EDGE_CURVE ( 'NONE', #203718, #82204, #230310, .T. ) ;
#226242 = ORIENTED_EDGE ( 'NONE', *, *, #255479, .F. ) ;
#226243 = AXIS2_PLACEMENT_3D ( 'NONE', #247687, #69071, #148601 ) ;
#226244 = CARTESIAN_POINT ( 'NONE',  ( 20.04142135623730070, 54.35086488289006468, -228.7501953506800305 ) ) ;
#226245 = LINE ( 'NONE', #187173, #213469 ) ;
#226247 = EDGE_LOOP ( 'NONE', ( #240687, #93187, #214067, #11351 ) ) ;
#226246 = CARTESIAN_POINT ( 'NONE',  ( -18.59999999999999787, -1.362429037182155023, -175.3888812479212334 ) ) ;
#226248 = ADVANCED_FACE ( 'NONE', ( #102468 ), #101171, .F. ) ;
#226249 = DIRECTION ( 'NONE',  ( -7.304098846218201720E-16, 1.000000000000000000, 0.000000000000000000 ) ) ;
#226251 = ORIENTED_EDGE ( 'NONE', *, *, #141863, .F. ) ;
#226250 = CARTESIAN_POINT ( 'NONE',  ( 18.59999999999999787, -6.937571600298356067, -224.3614019333310807 ) ) ;
#226252 = CARTESIAN_POINT ( 'NONE',  ( 23.14999999999999858, 1.115600667400684642E-11, -204.9999999999999716 ) ) ;
#226253 = CARTESIAN_POINT ( 'NONE',  ( -16.89146115310546037, 9.951443245667611848, -121.3548224189542424 ) ) ;
#226254 = AXIS2_PLACEMENT_3D ( 'NONE', #150344, #69531, #189466 ) ;
#226256 = VERTEX_POINT ( 'NONE', #17819 ) ;
#226255 = CARTESIAN_POINT ( 'NONE',  ( -20.94999999999999929, 74.83729825007388570, -95.02310748452431710 ) ) ;
#226257 = CIRCLE ( 'NONE', #113871, 0.9750000000000036415 ) ;
#226258 = FACE_OUTER_BOUND ( 'NONE', #37207, .T. ) ;
#226259 = EDGE_CURVE ( 'NONE', #120435, #15704, #122076, .T. ) ;
#226260 = DIRECTION ( 'NONE',  ( 1.000000000000000000, 0.000000000000000000, 0.000000000000000000 ) ) ;
#226261 = VECTOR ( 'NONE', #17143, 1000.000000000000000 ) ;
#226263 = DIRECTION ( 'NONE',  ( 0.000000000000000000, -0.4999999999999689138, -0.8660254037844565822 ) ) ;
#226262 = DIRECTION ( 'NONE',  ( 0.000000000000000000, 0.6728971962616412394, -0.7397360091703134577 ) ) ;
#226264 = CARTESIAN_POINT ( 'NONE',  ( 18.49999999999999289, 10.34378108836433263, -91.82844527787746358 ) ) ;
#226265 = EDGE_CURVE ( 'NONE', #220406, #142529, #77789, .T. ) ;
#226266 = DIRECTION ( 'NONE',  ( 1.000000000000000000, 0.000000000000000000, 0.000000000000000000 ) ) ;
#226267 = CARTESIAN_POINT ( 'NONE',  ( 23.14999999999999858, 11.65000000001116298, -126.9851942293460922 ) ) ;
#226268 = CARTESIAN_POINT ( 'NONE',  ( -17.11825945287483108, 44.09459801588531036, -235.2076708599468020 ) ) ;
#226270 = VERTEX_POINT ( 'NONE', #59491 ) ;
#226269 = AXIS2_PLACEMENT_3D ( 'NONE', #252826, #75511, #155057 ) ;
#226271 = EDGE_LOOP ( 'NONE', ( #5880, #130845, #217966, #121807 ) ) ;
#226272 = VECTOR ( 'NONE', #256487, 1000.000000000000000 ) ;
#226274 = ORIENTED_EDGE ( 'NONE', *, *, #212335, .T. ) ;
#226273 = VECTOR ( 'NONE', #108798, 1000.000000000000000 ) ;
#226275 = EDGE_CURVE ( 'NONE', #129128, #51208, #226181, .T. ) ;
#226276 = FACE_OUTER_BOUND ( 'NONE', #241383, .T. ) ;
#226277 = AXIS2_PLACEMENT_3D ( 'NONE', #19850, #41982, #99340 ) ;
#226278 = ORIENTED_EDGE ( 'NONE', *, *, #63806, .F. ) ;
#226279 = CARTESIAN_POINT ( 'NONE',  ( -18.59999999999999787, -1.261786168553869603, -108.5864989635455089 ) ) ;
#226280 = ORIENTED_EDGE ( 'NONE', *, *, #134268, .F. ) ;
#226281 = CARTESIAN_POINT ( 'NONE',  ( 23.14999999999999147, -4.054946580484636520, -201.8831241301909074 ) ) ;
#226282 = CARTESIAN_POINT ( 'NONE',  ( 20.94999999999999929, 7.021664781900089913, -37.33356540189728889 ) ) ;
#226283 = EDGE_CURVE ( 'NONE', #77477, #212886, #47138, .T. ) ;
#226284 = ADVANCED_FACE ( 'NONE', ( #68523 ), #103757, .T. ) ;
#226285 = VERTEX_POINT ( 'NONE', #29425 ) ;
#226286 = DIRECTION ( 'NONE',  ( 1.000000000000000000, -0.000000000000000000, -0.000000000000000000 ) ) ;
#226287 = SURFACE_STYLE_FILL_AREA ( #184614 ) ;
#226288 = CIRCLE ( 'NONE', #38895, 0.1999999999999987899 ) ;
#226289 = AXIS2_PLACEMENT_3D ( 'NONE', #223562, #239297, #84016 ) ;
#226290 = VERTEX_POINT ( 'NONE', #223719 ) ;
#226291 = VECTOR ( 'NONE', #84057, 1000.000000000000000 ) ;
#226293 = ORIENTED_EDGE ( 'NONE', *, *, #163360, .F. ) ;
#226292 = AXIS2_PLACEMENT_3D ( 'NONE', #169177, #248685, #249968 ) ;
#226294 = ORIENTED_EDGE ( 'NONE', *, *, #147720, .T. ) ;
#226295 = CARTESIAN_POINT ( 'NONE',  ( -21.14999999999999858, 11.75000000000000000, -0.1000000000000028644 ) ) ;
#226296 = CARTESIAN_POINT ( 'NONE',  ( -20.94999999999999929, 14.83511725869332132, -235.8887435844146978 ) ) ;
#226297 = CARTESIAN_POINT ( 'NONE',  ( -18.59999999999999787, 1.250000000011155299, -175.4999999999999716 ) ) ;
#226298 = DIRECTION ( 'NONE',  ( 0.000000000000000000, 0.000000000000000000, -1.000000000000000000 ) ) ;
#226299 = DIRECTION ( 'NONE',  ( -1.000000000000000000, -0.000000000000000000, -0.000000000000000000 ) ) ;
#226301 = CARTESIAN_POINT ( 'NONE',  ( 18.46921299892754931, 85.50937817783642458, -196.5365287751538403 ) ) ;
#226300 = CARTESIAN_POINT ( 'NONE',  ( 20.27550659511088682, 66.78395627750323627, -127.2731074845243597 ) ) ;
#226302 = CARTESIAN_POINT ( 'NONE',  ( -16.87036670365548474, 9.989418819312801290, -54.47956011730205006 ) ) ;
#226304 = ORIENTED_EDGE ( 'NONE', *, *, #57268, .T. ) ;
#226303 = CARTESIAN_POINT ( 'NONE',  ( -18.40000000000000213, 64.52683809664981140, -157.4731074845244621 ) ) ;
#226306 = FACE_OUTER_BOUND ( 'NONE', #128083, .T. ) ;
#226305 = CARTESIAN_POINT ( 'NONE',  ( 20.97565083910961548, 10.47461740128996510, -74.57794317658860450 ) ) ;
#226307 = CARTESIAN_POINT ( 'NONE',  ( 21.13461538461538325, 8.885417037985616773, -146.3500000000000227 ) ) ;
#226308 = VERTEX_POINT ( 'NONE', #183334 ) ;
#226309 = CARTESIAN_POINT ( 'NONE',  ( 20.95265033839679347, 10.51225083247831371, -74.56576375603000884 ) ) ;
#226310 = CARTESIAN_POINT ( 'NONE',  ( 22.39999999999999503, 7.790779598373379855, 0.09999999999999939493 ) ) ;
#226311 = DIRECTION ( 'NONE',  ( -1.000000000000000000, -0.000000000000000000, -0.000000000000000000 ) ) ;
#226312 = VERTEX_POINT ( 'NONE', #227581 ) ;
#226313 = PLANE ( 'NONE',  #24577 ) ;
#226314 = CARTESIAN_POINT ( 'NONE',  ( 21.05000000000000071, 1.115600667400684642E-11, -96.20000000000000284 ) ) ;
#226315 = DIRECTION ( 'NONE',  ( 0.000000000000000000, 1.776356839400277286E-15, -1.000000000000000000 ) ) ;
#226316 = VERTEX_POINT ( 'NONE', #108914 ) ;
#226317 = ORIENTED_EDGE ( 'NONE', *, *, #119205, .T. ) ;
#226318 = TOROIDAL_SURFACE ( 'NONE', #209789, 12.77500000000000036, 0.1000000000000000056 ) ;
#226319 = CARTESIAN_POINT ( 'NONE',  ( -23.25000000000000000, 78.57213941646344324, -232.7862224702232652 ) ) ;
#226320 = ORIENTED_EDGE ( 'NONE', *, *, #235983, .T. ) ;
#226321 = CARTESIAN_POINT ( 'NONE',  ( -0.8999999999999437339, 64.25000000001119815, -12.72310748452478890 ) ) ;
#226322 = DIRECTION ( 'NONE',  ( 1.000000000000000000, 0.000000000000000000, 0.000000000000000000 ) ) ;
#226323 = CARTESIAN_POINT ( 'NONE',  ( 18.47688499308725341, 85.46485595029577098, -62.82175973138684810 ) ) ;
#226324 = LINE ( 'NONE', #222474, #134308 ) ;
#226325 = ORIENTED_EDGE ( 'NONE', *, *, #198119, .T. ) ;
#226326 = CARTESIAN_POINT ( 'NONE',  ( -15.66061380678752535, 9.360723793997191677, -117.8139271946067481 ) ) ;
#226327 = ADVANCED_FACE ( 'NONE', ( #45100 ), #185889, .F. ) ;
#226328 = DIRECTION ( 'NONE',  ( 0.000000000000000000, -1.000000000000000000, 0.000000000000000000 ) ) ;
#226329 = CARTESIAN_POINT ( 'NONE',  ( 20.94999999999999574, 77.83534155023700407, -191.8679561919613832 ) ) ;
#226330 = CARTESIAN_POINT ( 'NONE',  ( 21.14999999999999858, 9.125777775466493935, -211.6520035670780544 ) ) ;
#226331 = ADVANCED_FACE ( 'NONE', ( #226276 ), #201267, .T. ) ;
#226332 = AXIS2_PLACEMENT_3D ( 'NONE', #204988, #163330, #221975 ) ;
#226334 = ORIENTED_EDGE ( 'NONE', *, *, #34671, .T. ) ;
#226333 = CIRCLE ( 'NONE', #209802, 0.1000000000000028644 ) ;
#226335 = DIRECTION ( 'NONE',  ( 1.000000000000000000, 1.836970198721029934E-16, -0.000000000000000000 ) ) ;
#226336 = CIRCLE ( 'NONE', #64058, 0.09999999999998898659 ) ;
#226337 = EDGE_CURVE ( 'NONE', #94509, #10056, #34911, .T. ) ;
#226339 = ORIENTED_EDGE ( 'NONE', *, *, #136931, .F. ) ;
#226338 = CARTESIAN_POINT ( 'NONE',  ( -23.25000000000000355, 65.95000000001181206, -82.27310748452437394 ) ) ;
#226340 = EDGE_CURVE ( 'NONE', #148316, #91171, #105574, .T. ) ;
#226341 = DIRECTION ( 'NONE',  ( -1.000000000000000000, -1.875376730785737719E-16, -0.000000000000000000 ) ) ;
#226342 = DIRECTION ( 'NONE',  ( 0.000000000000000000, 1.000000000000000000, 0.000000000000000000 ) ) ;
#226343 = FACE_OUTER_BOUND ( 'NONE', #86922, .T. ) ;
#226344 = DIRECTION ( 'NONE',  ( 1.000000000000000000, 0.000000000000000000, -0.000000000000000000 ) ) ;
#226345 = DIRECTION ( 'NONE',  ( 0.000000000000000000, 0.000000000000000000, -1.000000000000000000 ) ) ;
#226346 = CARTESIAN_POINT ( 'NONE',  ( -18.50000000000000355, 79.28756800457986742, -196.2274082906208434 ) ) ;
#226347 = DIRECTION ( 'NONE',  ( 1.000000000000000000, 0.000000000000000000, 0.000000000000000000 ) ) ;
#226348 = ORIENTED_EDGE ( 'NONE', *, *, #50756, .T. ) ;
#226349 = DIRECTION ( 'NONE',  ( 1.000000000000000000, 0.000000000000000000, 0.000000000000000000 ) ) ;
#226350 = LINE ( 'NONE', #9889, #223349 ) ;
#226351 = CARTESIAN_POINT ( 'NONE',  ( -23.25000000000000000, -9.599999999988838795, -90.60603087734760663 ) ) ;
#226352 = CIRCLE ( 'NONE', #39148, 0.1000000000000033362 ) ;
#226353 = CARTESIAN_POINT ( 'NONE',  ( -18.59999999999999787, 14.90151243843701856, -203.3975529985363551 ) ) ;
#226355 = DIRECTION ( 'NONE',  ( -7.304098846217948299E-16, -1.000000000000000000, 0.000000000000000000 ) ) ;
#226354 = AXIS2_PLACEMENT_3D ( 'NONE', #148884, #70653, #151459 ) ;
#226356 = EDGE_CURVE ( 'NONE', #89456, #245959, #24274, .T. ) ;
#226358 = ORIENTED_EDGE ( 'NONE', *, *, #188036, .F. ) ;
#226357 = TOROIDAL_SURFACE ( 'NONE', #93676, 0.6000000000000004219, 0.1000000000000000056 ) ;
#226359 = EDGE_LOOP ( 'NONE', ( #176755, #10943, #205388, #226957 ) ) ;
#226361 = CYLINDRICAL_SURFACE ( 'NONE', #59269, 0.09999999999999986677 ) ;
#226360 = AXIS2_PLACEMENT_3D ( 'NONE', #165612, #146020, #126465 ) ;
#226362 = DIRECTION ( 'NONE',  ( 1.000000000000000000, 0.000000000000000000, 0.000000000000000000 ) ) ;
#226363 = LINE ( 'NONE', #205530, #42789 ) ;
#226364 = CIRCLE ( 'NONE', #43065, 6.329289321881370611 ) ;
#226365 = AXIS2_PLACEMENT_3D ( 'NONE', #126163, #102735, #81879 ) ;
#226366 = FACE_OUTER_BOUND ( 'NONE', #119740, .T. ) ;
#226367 = EDGE_CURVE ( 'NONE', #9346, #63115, #206740, .T. ) ;
#226368 = CIRCLE ( 'NONE', #113962, 0.09999999999999939493 ) ;
#226369 = CARTESIAN_POINT ( 'NONE',  ( -20.99551997958315042, 17.15237243733772132, -224.5408061578804961 ) ) ;
#226370 = EDGE_CURVE ( 'NONE', #38453, #241591, #67225, .T. ) ;
#226371 = ORIENTED_EDGE ( 'NONE', *, *, #27309, .F. ) ;
#226372 = CARTESIAN_POINT ( 'NONE',  ( -23.25000000000000000, 76.00000000001165290, -69.52310748452431710 ) ) ;
#226373 = AXIS2_PLACEMENT_3D ( 'NONE', #188455, #90627, #55328 ) ;
#226374 = ORIENTED_EDGE ( 'NONE', *, *, #34571, .F. ) ;
#226375 = DIRECTION ( 'NONE',  ( 0.000000000000000000, -0.8700118002898321601, 0.4930308989875230030 ) ) ;
#226376 = DIRECTION ( 'NONE',  ( 1.000000000000000000, 0.000000000000000000, 0.000000000000000000 ) ) ;
#226377 = CARTESIAN_POINT ( 'NONE',  ( -18.50000000000000000, -1.835341550213255957, -179.0551512925629538 ) ) ;
#226378 = EDGE_CURVE ( 'NONE', #229015, #165380, #193107, .T. ) ;
#226380 = AXIS2_PLACEMENT_3D ( 'NONE', #50938, #251735, #212621 ) ;
#226379 = CARTESIAN_POINT ( 'NONE',  ( -16.77779411503079032, 9.946101446935278645, -46.16305741761983228 ) ) ;
#226381 = CARTESIAN_POINT ( 'NONE',  ( 21.14999999999999503, 55.89093952297024970, -232.7795287750844579 ) ) ;
#226383 = DIRECTION ( 'NONE',  ( 0.000000000000000000, -0.9999631594459056361, -0.008583690987124413183 ) ) ;
#226382 = VECTOR ( 'NONE', #86006, 1000.000000000000000 ) ;
#226384 = VECTOR ( 'NONE', #20554, 1000.000000000000000 ) ;
#226385 = CARTESIAN_POINT ( 'NONE',  ( -17.11825945287481687, 65.95000000001181206, -82.17310748452439384 ) ) ;
#226386 = ADVANCED_FACE ( 'NONE', ( #243285 ), #218006, .F. ) ;
#226387 = ORIENTED_EDGE ( 'NONE', *, *, #66350, .T. ) ;
#226389 = CARTESIAN_POINT ( 'NONE',  ( 18.59999999999999076, 14.83511725869332132, -235.8887435844146978 ) ) ;
#226388 = AXIS2_PLACEMENT_3D ( 'NONE', #166131, #198162, #76928 ) ;
#226390 = DIRECTION ( 'NONE',  ( -0.7071067811865474617, -0.7071067811865474617, -0.000000000000000000 ) ) ;
#226391 = DIRECTION ( 'NONE',  ( 1.000000000000000000, -0.000000000000000000, -0.000000000000000000 ) ) ;
#226392 = DIRECTION ( 'NONE',  ( 0.000000000000000000, -6.982962677686266711E-15, 1.000000000000000000 ) ) ;
#226393 = EDGE_CURVE ( 'NONE', #54689, #76475, #247136, .T. ) ;
#226394 = CARTESIAN_POINT ( 'NONE',  ( -17.78043020864321022, 10.85359211201684460, -157.1630491657202526 ) ) ;
#226395 = CARTESIAN_POINT ( 'NONE',  ( 21.05000000000000071, 1.115600667400684642E-11, -79.97500000000005116 ) ) ;
#226396 = ORIENTED_EDGE ( 'NONE', *, *, #18720, .T. ) ;
#226397 = DIRECTION ( 'NONE',  ( 0.000000000000000000, 0.9651348961777157509, -0.2617529984165028467 ) ) ;
#226398 = DIRECTION ( 'NONE',  ( 0.000000000000000000, 0.4999999999999689138, 0.8660254037844565822 ) ) ;
#226399 = EDGE_CURVE ( 'NONE', #80932, #215192, #142887, .T. ) ;
#226400 = EDGE_LOOP ( 'NONE', ( #166486, #146967, #136299, #111582 ) ) ;
#226401 = CARTESIAN_POINT ( 'NONE',  ( -16.89268316805465986, 51.62340874627276577, -231.9425458505251072 ) ) ;
#226402 = CARTESIAN_POINT ( 'NONE',  ( 21.13461538461538325, 11.28871374199622046, -211.0785950404945766 ) ) ;
#226403 = CARTESIAN_POINT ( 'NONE',  ( 20.12500000000000000, 59.94448977088796937, -225.4740812377367263 ) ) ;
#226404 = EDGE_CURVE ( 'NONE', #205485, #21653, #18116, .T. ) ;
#226405 = VECTOR ( 'NONE', #95890, 1000.000000000000000 ) ;
#226406 = ORIENTED_EDGE ( 'NONE', *, *, #202464, .T. ) ;
#226407 = DIRECTION ( 'NONE',  ( 0.000000000000000000, -0.1686199900910312910, 0.9856811345164826488 ) ) ;
#226408 = DIRECTION ( 'NONE',  ( 0.000000000000000000, 1.000000000000000000, 6.982962677686266711E-15 ) ) ;
#226409 = AXIS2_PLACEMENT_3D ( 'NONE', #198407, #216684, #220546 ) ;
#226411 = ORIENTED_EDGE ( 'NONE', *, *, #4222, .T. ) ;
#226410 = AXIS2_PLACEMENT_3D ( 'NONE', #49412, #165521, #190214 ) ;
#226412 =( BOUNDED_CURVE ( )  B_SPLINE_CURVE ( 3, ( #251967, #73367, #94168, #154207 ),
 .UNSPECIFIED., .F., .T. ) 
 B_SPLINE_CURVE_WITH_KNOTS ( ( 4, 4 ),
 ( 1.570796326794885012, 3.141592653589794448 ),
 .UNSPECIFIED. ) 
 CURVE ( )  GEOMETRIC_REPRESENTATION_ITEM ( )  RATIONAL_B_SPLINE_CURVE ( ( 1.000000000000000000, 0.8047378541243619399, 0.8047378541243619399, 1.000000000000000000 ) ) 
 REPRESENTATION_ITEM ( '' )  );
#226414 = SPHERICAL_SURFACE ( 'NONE', #247795, 0.1000000000000000056 ) ;
#226413 = VECTOR ( 'NONE', #250519, 1000.000000000000000 ) ;
#226415 = CIRCLE ( 'NONE', #151652, 3.900000000000000799 ) ;
#226416 = EDGE_LOOP ( 'NONE', ( #30532, #115337, #238788, #176383 ) ) ;
#226417 = CYLINDRICAL_SURFACE ( 'NONE', #212856, 0.1000000000000012546 ) ;
#226418 = DIRECTION ( 'NONE',  ( -1.000000000000000000, 0.000000000000000000, 0.000000000000000000 ) ) ;
#226419 = CARTESIAN_POINT ( 'NONE',  ( -20.64999999999999858, 8.751106741858205140, -220.7398867978736234 ) ) ;
#226421 = AXIS2_PLACEMENT_3D ( 'NONE', #116713, #41057, #140108 ) ;
#226420 = DIRECTION ( 'NONE',  ( 0.000000000000000000, -1.509041004344873323E-14, 1.000000000000000000 ) ) ;
#226422 = LINE ( 'NONE', #107782, #204346 ) ;
#226423 = CARTESIAN_POINT ( 'NONE',  ( -16.80891096016298647, 66.05000000001230376, -157.3907702917945812 ) ) ;
#226424 = CARTESIAN_POINT ( 'NONE',  ( -16.77828822508139694, 66.05377062509185748, -190.8604792331504711 ) ) ;
#226425 = CARTESIAN_POINT ( 'NONE',  ( -23.25000000000000000, 10.33248238083634440, -206.5948465439131496 ) ) ;
#226426 = AXIS2_PLACEMENT_3D ( 'NONE', #139468, #119955, #168080 ) ;
#226428 = ORIENTED_EDGE ( 'NONE', *, *, #117039, .T. ) ;
#226427 = DIRECTION ( 'NONE',  ( 0.000000000000000000, 0.2128009952263485993, -0.9770955615653341697 ) ) ;
#226429 = ORIENTED_EDGE ( 'NONE', *, *, #251071, .F. ) ;
#226431 = CARTESIAN_POINT ( 'NONE',  ( -20.64999999999999858, 85.00000000001149658, -45.51707660717670478 ) ) ;
#226430 = DIRECTION ( 'NONE',  ( -1.000000000000000000, 0.000000000000000000, -0.000000000000000000 ) ) ;
#226432 = VECTOR ( 'NONE', #199982, 1000.000000000000000 ) ;
#226434 = ORIENTED_EDGE ( 'NONE', *, *, #21741, .F. ) ;
#226433 = CARTESIAN_POINT ( 'NONE',  ( -20.05000000000000426, 66.75000000001179501, -81.77310748452437394 ) ) ;
#226435 = ORIENTED_EDGE ( 'NONE', *, *, #243675, .F. ) ;
#226436 = CARTESIAN_POINT ( 'NONE',  ( 20.95000000000005613, 65.15000000001120384, -4.423107484524790856 ) ) ;
#226437 = CARTESIAN_POINT ( 'NONE',  ( 20.94999999999999929, 67.22371710471941242, -94.46447848938342418 ) ) ;
#226438 = AXIS2_PLACEMENT_3D ( 'NONE', #36368, #254087, #170771 ) ;
#226439 = DIRECTION ( 'NONE',  ( -0.000000000000000000, -0.000000000000000000, 1.000000000000000000 ) ) ;
#226440 = CARTESIAN_POINT ( 'NONE',  ( 20.94999999999999929, 68.87972903831452243, -132.8635444426850825 ) ) ;
#226441 = DIRECTION ( 'NONE',  ( 0.000000000000000000, -6.982962677686266711E-15, 1.000000000000000000 ) ) ;
#226442 = AXIS2_PLACEMENT_3D ( 'NONE', #143298, #44217, #200713 ) ;
#226443 = PLANE ( 'NONE',  #94724 ) ;
#226444 = DIRECTION ( 'NONE',  ( 1.000000000000000000, -2.849773892568378313E-16, 7.728835255496647986E-17 ) ) ;
#226445 = AXIS2_PLACEMENT_3D ( 'NONE', #119785, #20678, #234566 ) ;
#226446 = ORIENTED_EDGE ( 'NONE', *, *, #3250, .T. ) ;
#226447 = VERTEX_POINT ( 'NONE', #205442 ) ;
#226448 = EDGE_CURVE ( 'NONE', #158981, #90057, #107632, .T. ) ;
#226449 = DIRECTION ( 'NONE',  ( 0.000000000000000000, 1.000000000000000000, 0.000000000000000000 ) ) ;
#226450 = ORIENTED_EDGE ( 'NONE', *, *, #60961, .T. ) ;
#226451 = CARTESIAN_POINT ( 'NONE',  ( 20.94999999999999574, -1.736257131586239844, -112.0686523290175245 ) ) ;
#226452 = EDGE_LOOP ( 'NONE', ( #160413, #253216, #219867, #170484 ) ) ;
#226454 = VECTOR ( 'NONE', #67167, 1000.000000000000000 ) ;
#226453 = CARTESIAN_POINT ( 'NONE',  ( 22.10000000000000142, -11.65000000000000036, 32.89999999999999858 ) ) ;
#226455 = VECTOR ( 'NONE', #248317, 1000.000000000000000 ) ;
#226456 = CIRCLE ( 'NONE', #118353, 4.149999999999999467 ) ;
#226457 = CARTESIAN_POINT ( 'NONE',  ( -23.15000000000000213, -8.999999999988846255, -110.3939691226524786 ) ) ;
#226458 = EDGE_CURVE ( 'NONE', #194584, #180208, #242010, .T. ) ;
#226459 = DIRECTION ( 'NONE',  ( -2.952720810173289605E-16, -1.000000000000000000, -7.086529944415894657E-15 ) ) ;
#226460 = CARTESIAN_POINT ( 'NONE',  ( 23.14999999999999503, 11.65000000001116298, -55.25000000000004974 ) ) ;
#226461 = ORIENTED_EDGE ( 'NONE', *, *, #121385, .F. ) ;
#226463 = FACE_OUTER_BOUND ( 'NONE', #13520, .T. ) ;
#226462 =( BOUNDED_CURVE ( )  B_SPLINE_CURVE ( 3, ( #187931, #25022, #104501, #87516 ),
 .UNSPECIFIED., .F., .F. ) 
 B_SPLINE_CURVE_WITH_KNOTS ( ( 4, 4 ),
 ( 5.731445031868799056, 5.983100554402348337 ),
 .UNSPECIFIED. ) 
 CURVE ( )  GEOMETRIC_REPRESENTATION_ITEM ( )  RATIONAL_B_SPLINE_CURVE ( ( 1.000000000000000000, 0.9947294176030464508, 0.9947294176030464508, 1.000000000000000000 ) ) 
 REPRESENTATION_ITEM ( '' )  );
#226464 = ORIENTED_EDGE ( 'NONE', *, *, #84400, .F. ) ;
#226465 = EDGE_CURVE ( 'NONE', #68804, #166946, #168006, .T. ) ;
#226466 = DIRECTION ( 'NONE',  ( 0.000000000000000000, 0.000000000000000000, -1.000000000000000000 ) ) ;
#226467 = EDGE_CURVE ( 'NONE', #205134, #218074, #38983, .T. ) ;
#226468 = CARTESIAN_POINT ( 'NONE',  ( -20.85000000000000142, 6.933893972137497030, -171.2856458343736108 ) ) ;
#226469 = DIRECTION ( 'NONE',  ( -1.000000000000000000, 0.000000000000000000, -0.000000000000000000 ) ) ;
#226470 = DIRECTION ( 'NONE',  ( 0.000000000000000000, 0.000000000000000000, -1.000000000000000000 ) ) ;
#226471 = ORIENTED_EDGE ( 'NONE', *, *, #193431, .T. ) ;
#226472 = CARTESIAN_POINT ( 'NONE',  ( -20.94999999999999929, 65.70729864261026876, -131.0657455973724836 ) ) ;
#226473 = ORIENTED_EDGE ( 'NONE', *, *, #249459, .F. ) ;
#226476 = ORIENTED_EDGE ( 'NONE', *, *, #3514, .T. ) ;
#226475 = CARTESIAN_POINT ( 'NONE',  ( -18.34374000495059676, 11.47316190336247388, -24.25000000000001066 ) ) ;
#226474 = LINE ( 'NONE', #28339, #28550 ) ;
#226477 = AXIS2_PLACEMENT_3D ( 'NONE', #31837, #168801, #248286 ) ;
#226478 = CIRCLE ( 'NONE', #114058, 2.000000000000000444 ) ;
#226479 = DIRECTION ( 'NONE',  ( -0.7071067811865388020, 0.7071067811865561215, 0.000000000000000000 ) ) ;
#226480 = AXIS2_PLACEMENT_3D ( 'NONE', #17464, #95707, #193550 ) ;
#226481 = ORIENTED_EDGE ( 'NONE', *, *, #72913, .T. ) ;
#226482 = CARTESIAN_POINT ( 'NONE',  ( -21.05000000000000071, 36.65892442174935439, -249.5511627012433848 ) ) ;
#226483 = EDGE_LOOP ( 'NONE', ( #166058, #232630, #152999, #160236 ) ) ;
#226484 = ADVANCED_FACE ( 'NONE', ( #74962 ), #9820, .T. ) ;
#226485 = DIRECTION ( 'NONE',  ( -0.7071067811865462405, -0.6824534298470383842, 0.1850873201762212872 ) ) ;
#226486 = DIRECTION ( 'NONE',  ( 0.000000000000000000, -0.8741572761215384846, 0.4856429311786307212 ) ) ;
#226487 = FACE_OUTER_BOUND ( 'NONE', #122403, .T. ) ;
#226488 = FACE_OUTER_BOUND ( 'NONE', #210912, .T. ) ;
#226489 = VERTEX_POINT ( 'NONE', #174079 ) ;
#226490 = CARTESIAN_POINT ( 'NONE',  ( -17.22361732159832215, 14.81732475420846207, -220.4208988007774224 ) ) ;
#226491 = CARTESIAN_POINT ( 'NONE',  ( -20.94999999999999929, 69.25640205380744874, -247.7135141964517402 ) ) ;
#226492 = CARTESIAN_POINT ( 'NONE',  ( -12.60206096961793598, 66.61031399435663047, -154.3502639781731318 ) ) ;
#226493 = ORIENTED_EDGE ( 'NONE', *, *, #59914, .F. ) ;
#226494 = CARTESIAN_POINT ( 'NONE',  ( -21.05000000000000071, 1.115650877919449575E-11, -71.09999999999999432 ) ) ;
#226495 = EDGE_LOOP ( 'NONE', ( #252913, #87445, #242985, #65640, #26166 ) ) ;
#226496 = CARTESIAN_POINT ( 'NONE',  ( 21.10257677756356642, 30.80951268217205907, -252.1442870260762845 ) ) ;
#226497 = TOROIDAL_SURFACE ( 'NONE', #159904, 0.2000000000000000111, 0.1000000000000000056 ) ;
#226498 = EDGE_CURVE ( 'NONE', #80255, #100189, #80633, .T. ) ;
#226499 = LINE ( 'NONE', #186117, #76615 ) ;
#226500 = CARTESIAN_POINT ( 'NONE',  ( 23.14999999999999858, 9.863005973831429074, -220.4411654715779321 ) ) ;
#226501 = ADVANCED_FACE ( 'NONE', ( #231456 ), #71100, .T. ) ;
#226503 = EDGE_LOOP ( 'NONE', ( #229402, #178087, #72245, #178815 ) ) ;
#226502 = DIRECTION ( 'NONE',  ( 0.000000000000000000, 0.2128009952263601456, -0.9770955615653315052 ) ) ;
#226504 = CARTESIAN_POINT ( 'NONE',  ( -20.64999999999999858, 4.350000000011156054, -146.3500000000000227 ) ) ;
#226505 = CARTESIAN_POINT ( 'NONE',  ( -13.11924609551135568, 62.91308081279556319, -215.7443727990306002 ) ) ;
#226506 = DIRECTION ( 'NONE',  ( 0.000000000000000000, 0.08413937888704771384, -0.9964539953858891908 ) ) ;
#226508 = ADVANCED_FACE ( 'NONE', ( #72385 ), #192317, .T. ) ;
#226507 = ORIENTED_EDGE ( 'NONE', *, *, #12603, .F. ) ;
#226509 = PLANE ( 'NONE',  #139239 ) ;
#226510 = CARTESIAN_POINT ( 'NONE',  ( 18.60000000000000497, 85.36423601037908782, -162.8428530837996675 ) ) ;
#226511 = ORIENTED_EDGE ( 'NONE', *, *, #217623, .T. ) ;
#226513 = DIRECTION ( 'NONE',  ( 0.000000000000000000, 2.664535259100315349E-15, 1.000000000000000000 ) ) ;
#226512 = VECTOR ( 'NONE', #256930, 1000.000000000000114 ) ;
#226514 = AXIS2_PLACEMENT_3D ( 'NONE', #183468, #100039, #59625 ) ;
#226515 = VERTEX_POINT ( 'NONE', #134873 ) ;
#226516 = VECTOR ( 'NONE', #207409, 999.9999999999998863 ) ;
#226517 = DIRECTION ( 'NONE',  ( 1.000000000000000000, 0.000000000000000000, 0.000000000000000000 ) ) ;
#226519 = ORIENTED_EDGE ( 'NONE', *, *, #223309, .F. ) ;
#226518 = DIRECTION ( 'NONE',  ( -0.7071067811865127117, -0.7071067811865821007, 0.000000000000000000 ) ) ;
#226522 = EDGE_LOOP ( 'NONE', ( #27764, #224777, #24097, #254359 ) ) ;
#226521 = EDGE_LOOP ( 'NONE', ( #103471, #246911, #174003, #155144 ) ) ;
#226520 = DIRECTION ( 'NONE',  ( 0.7071067811865456854, -0.6909108974501254608, -0.1504730267678059674 ) ) ;
#226523 = CARTESIAN_POINT ( 'NONE',  ( 21.05000000000000071, 1.115600667400684642E-11, -67.00000000000004263 ) ) ;
#226524 = DIRECTION ( 'NONE',  ( 0.000000000000000000, 0.000000000000000000, 1.000000000000000000 ) ) ;
#226525 = DIRECTION ( 'NONE',  ( 1.734723475976817507E-14, 0.000000000000000000, -1.000000000000000000 ) ) ;
#226526 = CIRCLE ( 'NONE', #30957, 2.599999999999998312 ) ;
#226528 = CARTESIAN_POINT ( 'NONE',  ( -16.89797118371577156, 9.976380722644002219, -20.93729336755886905 ) ) ;
#226527 = DIRECTION ( 'NONE',  ( 0.000000000000000000, 0.000000000000000000, 1.000000000000000000 ) ) ;
#226529 = DIRECTION ( 'NONE',  ( 0.000000000000000000, -1.000000000000000000, -7.272083257015735086E-15 ) ) ;
#226530 = DIRECTION ( 'NONE',  ( -1.000000000000000000, 0.000000000000000000, 0.000000000000000000 ) ) ;
#226531 = DIRECTION ( 'NONE',  ( 2.710505431213777355E-16, -1.000000000000000000, 0.000000000000000000 ) ) ;
#226532 = AXIS2_PLACEMENT_3D ( 'NONE', #119821, #19423, #40300 ) ;
#226533 = DIRECTION ( 'NONE',  ( 3.265361837132813093E-16, -1.000000000000000000, -0.000000000000000000 ) ) ;
#226534 = VECTOR ( 'NONE', #97514, 1000.000000000000000 ) ;
#226535 = ORIENTED_EDGE ( 'NONE', *, *, #49124, .F. ) ;
#226536 = ORIENTED_EDGE ( 'NONE', *, *, #187402, .T. ) ;
#226537 = AXIS2_PLACEMENT_3D ( 'NONE', #197980, #221380, #42768 ) ;
#226538 = EDGE_CURVE ( 'NONE', #87244, #59994, #184698, .T. ) ;
#226539 = ADVANCED_FACE ( 'NONE', ( #249721 ), #168944, .F. ) ;
#226541 = ORIENTED_EDGE ( 'NONE', *, *, #133333, .F. ) ;
#226540 = LINE ( 'NONE', #49210, #37032 ) ;
#226542 = ORIENTED_EDGE ( 'NONE', *, *, #141265, .T. ) ;
#226543 = CARTESIAN_POINT ( 'NONE',  ( 21.14999999999999858, 17.83900070254454562, -239.4698447713637677 ) ) ;
#226544 = ORIENTED_EDGE ( 'NONE', *, *, #30559, .T. ) ;
#226545 = CARTESIAN_POINT ( 'NONE',  ( -23.25000000000000000, 21.17283678855157802, -243.7231193059830332 ) ) ;
#226546 = EDGE_CURVE ( 'NONE', #163056, #120584, #69818, .T. ) ;
#226547 = EDGE_CURVE ( 'NONE', #68121, #146093, #170237, .T. ) ;
#226548 = VECTOR ( 'NONE', #243277, 1000.000000000000114 ) ;
#226549 = AXIS2_PLACEMENT_3D ( 'NONE', #39158, #22160, #156549 ) ;
#226550 = ORIENTED_EDGE ( 'NONE', *, *, #215424, .F. ) ;
#226551 = ADVANCED_FACE ( 'NONE', ( #30700 ), #92739, .T. ) ;
#226552 = DIRECTION ( 'NONE',  ( 0.000000000000000000, 0.000000000000000000, -1.000000000000000000 ) ) ;
#226553 = CARTESIAN_POINT ( 'NONE',  ( 23.15000000000000213, 87.65000000001144542, -39.12310748452424747 ) ) ;
#226554 = AXIS2_PLACEMENT_3D ( 'NONE', #113913, #39553, #35697 ) ;
#226555 = ADVANCED_FACE ( 'NONE', ( #132331 ), #211894, .T. ) ;
#226557 = ORIENTED_EDGE ( 'NONE', *, *, #124433, .F. ) ;
#226556 = EDGE_LOOP ( 'NONE', ( #89625, #57000, #166414, #52668, #244917 ) ) ;
#226558 = ORIENTED_EDGE ( 'NONE', *, *, #237277, .T. ) ;
#226561 = ADVANCED_FACE ( 'NONE', ( #16271 ), #18801, .F. ) ;
#226560 = ADVANCED_FACE ( 'NONE', ( #34544 ), #252268, .F. ) ;
#226559 = DIRECTION ( 'NONE',  ( 0.000000000000000000, 0.000000000000000000, 1.000000000000000000 ) ) ;
#226562 = ORIENTED_EDGE ( 'NONE', *, *, #178086, .T. ) ;
#226563 = ORIENTED_EDGE ( 'NONE', *, *, #15321, .F. ) ;
#226565 = CARTESIAN_POINT ( 'NONE',  ( 23.14999999999999503, 14.06640494040442135, -210.3712993791105532 ) ) ;
#226564 = CIRCLE ( 'NONE', #18307, 0.09999999999999036049 ) ;
#226566 = DIRECTION ( 'NONE',  ( 1.000000000000000000, 0.000000000000000000, 0.000000000000000000 ) ) ;
#226567 = CARTESIAN_POINT ( 'NONE',  ( -22.50000000000000000, 1.115600667400684642E-11, -33.50000000000000000 ) ) ;
#226569 = ORIENTED_EDGE ( 'NONE', *, *, #256427, .F. ) ;
#226568 = DIRECTION ( 'NONE',  ( 0.000000000000000000, 0.000000000000000000, 1.000000000000000000 ) ) ;
#226570 = EDGE_CURVE ( 'NONE', #36408, #2508, #172298, .T. ) ;
#226571 = CARTESIAN_POINT ( 'NONE',  ( -20.85000000000000142, 42.15997144203495139, -239.2817429668763793 ) ) ;
#226572 = DIRECTION ( 'NONE',  ( 0.000000000000000000, 0.000000000000000000, -1.000000000000000000 ) ) ;
#226574 = ORIENTED_EDGE ( 'NONE', *, *, #146392, .F. ) ;
#226573 = CARTESIAN_POINT ( 'NONE',  ( 20.94999999999999929, 3.047642603966940200, -208.5984958277594785 ) ) ;
#226575 = FACE_OUTER_BOUND ( 'NONE', #112151, .T. ) ;
#226576 = ORIENTED_EDGE ( 'NONE', *, *, #182661, .F. ) ;
#226577 = TOROIDAL_SURFACE ( 'NONE', #14239, 0.2000000000000000111, 0.1000000000000000056 ) ;
#226578 = CARTESIAN_POINT ( 'NONE',  ( -21.14999999999999858, 57.76315019072730905, -226.2583585926041110 ) ) ;
#226579 = AXIS2_PLACEMENT_3D ( 'NONE', #90131, #133136, #131845 ) ;
#226580 = ORIENTED_EDGE ( 'NONE', *, *, #118019, .F. ) ;
#226581 = AXIS2_PLACEMENT_3D ( 'NONE', #205538, #141724, #7354 ) ;
#226582 = CARTESIAN_POINT ( 'NONE',  ( -21.00448002041633444, 18.71387963086063166, -226.6088698288088779 ) ) ;
#226583 = ADVANCED_FACE ( 'NONE', ( #95756 ), #155784, .F. ) ;
#226584 = ORIENTED_EDGE ( 'NONE', *, *, #102335, .F. ) ;
#226586 = CARTESIAN_POINT ( 'NONE',  ( -20.54999999999999716, 74.00000000001180922, -82.74772940728641402 ) ) ;
#226585 = DIRECTION ( 'NONE',  ( 0.000000000000000000, 0.000000000000000000, 1.000000000000000000 ) ) ;
#226587 = ADVANCED_FACE ( 'NONE', ( #240430 ), #256071, .F. ) ;
#226588 = EDGE_CURVE ( 'NONE', #107664, #165453, #234594, .T. ) ;
#226589 = FACE_OUTER_BOUND ( 'NONE', #218802, .T. ) ;
#226590 = DIRECTION ( 'NONE',  ( 0.000000000000000000, -1.000000000000000000, -6.982962677686266711E-15 ) ) ;
#226591 = ORIENTED_EDGE ( 'NONE', *, *, #137301, .T. ) ;
#226592 = ORIENTED_EDGE ( 'NONE', *, *, #25918, .T. ) ;
#226593 = ADVANCED_FACE ( 'NONE', ( #175345 ), #100863, .F. ) ;
#226594 = CYLINDRICAL_SURFACE ( 'NONE', #209467, 0.09999999999998898659 ) ;
#226595 = SPHERICAL_SURFACE ( 'NONE', #140028, 0.1000000000000000056 ) ;
#226596 = ORIENTED_EDGE ( 'NONE', *, *, #55339, .F. ) ;
#226597 = FACE_OUTER_BOUND ( 'NONE', #250465, .T. ) ;
#226598 = ORIENTED_EDGE ( 'NONE', *, *, #51259, .F. ) ;
#226599 = DIRECTION ( 'NONE',  ( -1.000000000000000000, 0.000000000000000000, 0.000000000000000000 ) ) ;
#226600 = VERTEX_POINT ( 'NONE', #257354 ) ;
#226601 = EDGE_CURVE ( 'NONE', #206496, #18090, #76361, .T. ) ;
#226602 = CYLINDRICAL_SURFACE ( 'NONE', #61656, 0.9000000000000014655 ) ;
#226603 = CARTESIAN_POINT ( 'NONE',  ( -15.75000000000000355, 26.54497872210690090, -232.9592037335782209 ) ) ;
#226604 = CIRCLE ( 'NONE', #247465, 0.1000000000000000472 ) ;
#226605 = EDGE_CURVE ( 'NONE', #85650, #240913, #109692, .T. ) ;
#226606 = AXIS2_PLACEMENT_3D ( 'NONE', #229698, #64518, #241864 ) ;
#226607 = ORIENTED_EDGE ( 'NONE', *, *, #217692, .T. ) ;
#226608 = CARTESIAN_POINT ( 'NONE',  ( 18.44208962362927551, -9.552340496896620792, -207.8421730554641442 ) ) ;
#226609 = B_SPLINE_CURVE_WITH_KNOTS ( 'NONE', 3,
 ( #56171, #138273, #97850, #118751, #96575, #176163, #215267, #36662, #116185, #195731, #255622, #77028, #236110, #137010, #216545, #170615, #191440, #192695, #51869, #151002, #173177, #131423, #96132, #50588, #195280, #248823 ),
 .UNSPECIFIED., .F., .F.,
 ( 4, 2, 2, 2, 2, 2, 2, 2, 2, 2, 2, 2, 4 ),
 ( 0.005476422646581303143, 0.006160811967703536639, 0.006845201288825770135, 0.007187395949386886883, 0.007529590609948002763, 0.007871785270509119511, 0.008213979931070236259, 0.008556174591631353007, 0.008898369252192471490, 0.009240563912753588238, 0.009582758573314703252, 0.01026714789443687430, 0.01095153721555904534 ),
 .UNSPECIFIED. ) ;
#226610 = EDGE_LOOP ( 'NONE', ( #172375, #134282, #181975, #13699, #27742, #157427 ) ) ;
#226611 = ORIENTED_EDGE ( 'NONE', *, *, #28596, .F. ) ;
#226612 = EDGE_LOOP ( 'NONE', ( #219542, #61163, #240925, #97894, #82984 ) ) ;
#226613 = CIRCLE ( 'NONE', #105800, 0.09999999999998898659 ) ;
#226614 = CARTESIAN_POINT ( 'NONE',  ( 22.59999985501178799, 64.25013020700916400, -136.5887061543241998 ) ) ;
#226615 = DIRECTION ( 'NONE',  ( 0.000000000000000000, 0.000000000000000000, -1.000000000000000000 ) ) ;
#226616 = VECTOR ( 'NONE', #99906, 1000.000000000000000 ) ;
#226617 = LINE ( 'NONE', #187532, #67518 ) ;
#226618 = CARTESIAN_POINT ( 'NONE',  ( 20.94999999999999929, -6.688413578037176066, -212.5825622730469036 ) ) ;
#226619 = CARTESIAN_POINT ( 'NONE',  ( -17.71734398241073905, 32.72136639016480331, -235.1419597067196889 ) ) ;
#226620 = ADVANCED_FACE ( 'NONE', ( #136154 ), #77467, .F. ) ;
#226622 = DIRECTION ( 'NONE',  ( 0.000000000000000000, 0.5859227990963212784, 0.8103668758649578141 ) ) ;
#226621 = DIRECTION ( 'NONE',  ( 0.000000000000000000, -0.05616704890745314455, 0.9984213852963225166 ) ) ;
#226624 = EDGE_LOOP ( 'NONE', ( #222991, #217368, #201176, #124874 ) ) ;
#226623 = CARTESIAN_POINT ( 'NONE',  ( -23.25000000000000000, 84.59626168225550202, -179.4732350016745954 ) ) ;
#226625 = FACE_OUTER_BOUND ( 'NONE', #24846, .T. ) ;
#226626 = ORIENTED_EDGE ( 'NONE', *, *, #184275, .T. ) ;
#226627 = VECTOR ( 'NONE', #238933, 1000.000000000000000 ) ;
#226628 = CARTESIAN_POINT ( 'NONE',  ( -23.25000000000000000, 61.47936603916258491, -212.1738987416902376 ) ) ;
#226629 = ORIENTED_EDGE ( 'NONE', *, *, #72590, .F. ) ;
#226630 = VERTEX_POINT ( 'NONE', #157055 ) ;
#226631 = DIRECTION ( 'NONE',  ( -1.020425574104004196E-15, -6.982962677686266711E-15, 1.000000000000000000 ) ) ;
#226632 = AXIS2_PLACEMENT_3D ( 'NONE', #51463, #131028, #94461 ) ;
#226633 = CARTESIAN_POINT ( 'NONE',  ( 20.94999999999999929, 69.45000000001205365, -124.2731074845243597 ) ) ;
#226634 = CARTESIAN_POINT ( 'NONE',  ( -16.80891096016330266, 66.05000000001153637, -48.65544467725587197 ) ) ;
#226635 = AXIS2_PLACEMENT_3D ( 'NONE', #180253, #241504, #165837 ) ;
#226636 = DIRECTION ( 'NONE',  ( -0.7071067811865475727, -0.7071067811865475727, 0.000000000000000000 ) ) ;
#226637 = VECTOR ( 'NONE', #36125, 1000.000000000000000 ) ;
#226638 = CONICAL_SURFACE ( 'NONE', #167848, 7.750000000000034639, 0.7853981633974531640 ) ;
#226639 = DIRECTION ( 'NONE',  ( 0.000000000000000000, 0.8855159391400395652, -0.4646089985449416981 ) ) ;
#226640 = ORIENTED_EDGE ( 'NONE', *, *, #158928, .F. ) ;
#226641 = EDGE_LOOP ( 'NONE', ( #135110, #239147, #39773, #127720 ) ) ;
#226642 = CARTESIAN_POINT ( 'NONE',  ( -23.15000000000000213, 2.000000000011154189, -154.8753780772379116 ) ) ;
#226643 = ORIENTED_EDGE ( 'NONE', *, *, #125498, .T. ) ;
#226644 = DIRECTION ( 'NONE',  ( 0.000000000000000000, 0.2617529984165152257, 0.9651348961777124202 ) ) ;
#226645 = DIRECTION ( 'NONE',  ( -0.000000000000000000, 0.000000000000000000, 1.000000000000000000 ) ) ;
#226646 = ORIENTED_EDGE ( 'NONE', *, *, #132202, .T. ) ;
#226647 = DIRECTION ( 'NONE',  ( -0.1538461538461510236, 0.9880948137434718559, 0.000000000000000000 ) ) ;
#226649 = AXIS2_PLACEMENT_3D ( 'NONE', #225387, #153286, #232807 ) ;
#226648 = DIRECTION ( 'NONE',  ( 1.000000000000000000, -0.000000000000000000, -0.000000000000000000 ) ) ;
#226650 = DIRECTION ( 'NONE',  ( -1.000000000000000000, 0.000000000000000000, -0.000000000000000000 ) ) ;
#226651 = LINE ( 'NONE', #127568, #225688 ) ;
#226652 = ORIENTED_EDGE ( 'NONE', *, *, #121235, .F. ) ;
#226653 = CARTESIAN_POINT ( 'NONE',  ( -20.94999999999999929, 36.73178316696986911, -249.7991537124309218 ) ) ;
#226654 = CARTESIAN_POINT ( 'NONE',  ( -21.44999999999999929, 7.350000000011155166, -88.25000000000005684 ) ) ;
#226655 = DIRECTION ( 'NONE',  ( 1.000000000000000000, -0.000000000000000000, -0.000000000000000000 ) ) ;
#226656 = CIRCLE ( 'NONE', #114230, 0.1000000000000000472 ) ;
#226657 = ADVANCED_FACE ( 'NONE', ( #76199 ), #111031, .T. ) ;
#226658 = LINE ( 'NONE', #207119, #58158 ) ;
#226659 = CARTESIAN_POINT ( 'NONE',  ( -18.50000000000000000, 77.86671491006917734, -91.27043223824227880 ) ) ;
#226660 = EDGE_CURVE ( 'NONE', #37771, #204044, #59782, .T. ) ;
#226661 = CIRCLE ( 'NONE', #43339, 0.1000000000000024342 ) ;
#226662 = AXIS2_PLACEMENT_3D ( 'NONE', #155082, #117209, #136752 ) ;
#226663 = ORIENTED_EDGE ( 'NONE', *, *, #247474, .T. ) ;
#226664 = VECTOR ( 'NONE', #133413, 1000.000000000000000 ) ;
#226665 = EDGE_CURVE ( 'NONE', #64951, #254689, #14044, .T. ) ;
#226666 = DIRECTION ( 'NONE',  ( -6.938893903907222067E-15, -1.000000000000000000, -7.272083257015735086E-15 ) ) ;
#226667 = ADVANCED_FACE ( 'NONE', ( #123056 ), #64094, .F. ) ;
#226668 = ORIENTED_EDGE ( 'NONE', *, *, #211818, .F. ) ;
#226669 = CARTESIAN_POINT ( 'NONE',  ( -18.59999999999999787, -9.499999999988842703, -179.6499999999999773 ) ) ;
#226670 = DIRECTION ( 'NONE',  ( 1.000000000000000000, -0.000000000000000000, 0.000000000000000000 ) ) ;
#226672 = EDGE_CURVE ( 'NONE', #133625, #161032, #84899, .T. ) ;
#226671 = CYLINDRICAL_SURFACE ( 'NONE', #256224, 3.999999999999996447 ) ;
#226673 = DIRECTION ( 'NONE',  ( 0.000000000000000000, 0.9770955615653313941, 0.2128009952263603677 ) ) ;
#226674 = ORIENTED_EDGE ( 'NONE', *, *, #247000, .F. ) ;
#226675 = FACE_OUTER_BOUND ( 'NONE', #257871, .T. ) ;
#226676 = DIRECTION ( 'NONE',  ( 0.000000000000000000, 0.000000000000000000, -1.000000000000000000 ) ) ;
#226677 =( LENGTH_UNIT ( ) NAMED_UNIT ( * ) SI_UNIT ( .MILLI., .METRE. ) );
#226678 = DIRECTION ( 'NONE',  ( 1.000000000000000000, 0.000000000000000000, 0.000000000000000000 ) ) ;
#226680 = DIRECTION ( 'NONE',  ( 0.000000000000000000, 0.3848449534832868446, 0.9229812358755982160 ) ) ;
#226679 = VECTOR ( 'NONE', #23918, 1000.000000000000000 ) ;
#226681 = CARTESIAN_POINT ( 'NONE',  ( 22.46250603428203618, 75.97885582387365844, -181.6729705818644334 ) ) ;
#226682 = EDGE_CURVE ( 'NONE', #247600, #175543, #145159, .T. ) ;
#226683 = EDGE_LOOP ( 'NONE', ( #188679, #194732, #109973 ) ) ;
#226684 = ORIENTED_EDGE ( 'NONE', *, *, #66062, .T. ) ;
#226685 = DIRECTION ( 'NONE',  ( 1.000000000000000000, -7.304098846218134667E-16, -4.217023435051626718E-16 ) ) ;
#226686 = DIRECTION ( 'NONE',  ( 0.000000000000000000, 0.5000000000000078826, 0.8660254037844340447 ) ) ;
#226687 = DIRECTION ( 'NONE',  ( 0.000000000000000000, 0.000000000000000000, 1.000000000000000000 ) ) ;
#226688 = DIRECTION ( 'NONE',  ( 0.000000000000000000, -0.9770955615653313941, -0.2128009952263603677 ) ) ;
#226689 = VECTOR ( 'NONE', #210984, 1000.000000000000000 ) ;
#226690 = CARTESIAN_POINT ( 'NONE',  ( 20.94999999999999574, 14.81796439977981272, -236.5325475414793743 ) ) ;
#226691 = EDGE_LOOP ( 'NONE', ( #222300, #151008, #254657, #165617 ) ) ;
#226692 = CARTESIAN_POINT ( 'NONE',  ( -18.39999999999999858, -9.499999999988849808, -174.1001893912220737 ) ) ;
#226693 = CONTEXT_DEPENDENT_SHAPE_REPRESENTATION ( #109094, #236982 ) ;
#226694 = CARTESIAN_POINT ( 'NONE',  ( -18.59999999999999787, 64.35000000001222986, -148.6731074845244507 ) ) ;
#226695 = VERTEX_POINT ( 'NONE', #121781 ) ;
#226696 = DIRECTION ( 'NONE',  ( 1.000000000000000000, 0.000000000000000000, -0.000000000000000000 ) ) ;
#226697 = ADVANCED_FACE ( 'NONE', ( #3077 ), #59980, .T. ) ;
#226698 = AXIS2_PLACEMENT_3D ( 'NONE', #133472, #34397, #213002 ) ;
#226699 = ORIENTED_EDGE ( 'NONE', *, *, #238282, .T. ) ;
#226700 = VERTEX_POINT ( 'NONE', #183035 ) ;
#226701 = EDGE_LOOP ( 'NONE', ( #139, #166172, #220327 ) ) ;
#226702 = DIRECTION ( 'NONE',  ( 4.408576920032447355E-17, -0.1350103645451876666, 0.9908441862701600211 ) ) ;
#226703 = DIRECTION ( 'NONE',  ( 0.000000000000000000, -0.9893560106964500722, 0.1455152366551550613 ) ) ;
#226704 = EDGE_CURVE ( 'NONE', #250549, #183793, #155706, .T. ) ;
#226705 = CARTESIAN_POINT ( 'NONE',  ( 20.73486653747088582, 68.75000000001257661, -190.8731074845244109 ) ) ;
#226706 = DIRECTION ( 'NONE',  ( -1.000000000000000000, 0.000000000000000000, 0.000000000000000000 ) ) ;
#226707 = LINE ( 'NONE', #29837, #186907 ) ;
#226708 = DIRECTION ( 'NONE',  ( 1.000000000000000000, 0.000000000000000000, 0.000000000000000000 ) ) ;
#226709 = ADVANCED_FACE ( 'NONE', ( #6945 ), #65634, .F. ) ;
#226710 = B_SPLINE_CURVE_WITH_KNOTS ( 'NONE', 3,
 ( #256403, #94824, #16603, #97360, #156122, #192660, #213488, #77819, #157414, #217323 ),
 .UNSPECIFIED., .F., .F.,
 ( 4, 3, 3, 4 ),
 ( 0.000000000000000000, 4.874959354401679605E-05, 9.785140065120178569E-05, 0.0001360444631935948218 ),
 .UNSPECIFIED. ) ;
#226712 = DIRECTION ( 'NONE',  ( 0.000000000000000000, 0.000000000000000000, -1.000000000000000000 ) ) ;
#226711 = CARTESIAN_POINT ( 'NONE',  ( -20.94999999999999929, 70.15000000001266756, -193.3906102602464330 ) ) ;
#226713 = CARTESIAN_POINT ( 'NONE',  ( -20.85000000000000142, 36.65892442174935439, -249.5511627012433848 ) ) ;
#226714 = DIRECTION ( 'NONE',  ( 1.000000000000000000, 7.136802563874200093E-16, 1.554319503706925554E-16 ) ) ;
#226715 = DIRECTION ( 'NONE',  ( -1.000000000000000000, 0.000000000000000000, 0.000000000000000000 ) ) ;
#226717 = CARTESIAN_POINT ( 'NONE',  ( 20.94999999999999574, 69.45000000001260787, -193.6792853948412869 ) ) ;
#226716 = CIRCLE ( 'NONE', #143515, 0.1000000000000028644 ) ;
#226718 = ORIENTED_EDGE ( 'NONE', *, *, #223125, .T. ) ;
#226719 = TOROIDAL_SURFACE ( 'NONE', #47817, 11.65000000000000036, 0.1000000000000000056 ) ;
#226720 = EDGE_LOOP ( 'NONE', ( #49208, #245496, #239083, #27355 ) ) ;
#226721 = CARTESIAN_POINT ( 'NONE',  ( -18.39999999999999858, 46.91436717984746707, -255.3877622108296634 ) ) ;
#226722 = CYLINDRICAL_SURFACE ( 'NONE', #249481, 0.09999999999999939493 ) ;
#226725 = DIRECTION ( 'NONE',  ( 0.000000000000000000, 0.2128009952263603677, -0.9770955615653313941 ) ) ;
#226724 = CARTESIAN_POINT ( 'NONE',  ( -22.20000000000000284, 11.75000000000000000, -15.00000000000000000 ) ) ;
#226723 = AXIS2_PLACEMENT_3D ( 'NONE', #11468, #210939, #251330 ) ;
#226726 = AXIS2_PLACEMENT_3D ( 'NONE', #71409, #233051, #213458 ) ;
#226727 = ADVANCED_FACE ( 'NONE', ( #184293 ), #124339, .F. ) ;
#226728 = DIRECTION ( 'NONE',  ( 1.000000000000000000, 0.000000000000000000, 0.000000000000000000 ) ) ;
#226729 = DIRECTION ( 'NONE',  ( 1.000000000000000000, 0.000000000000000000, 0.000000000000000000 ) ) ;
#226730 = DIRECTION ( 'NONE',  ( 1.000000000000000000, 0.000000000000000000, 0.000000000000000000 ) ) ;
#226731 = EDGE_CURVE ( 'NONE', #194529, #34168, #201294, .T. ) ;
#226732 = ADVANCED_FACE ( 'NONE', ( #4368 ), #243153, .F. ) ;
#226733 = EDGE_LOOP ( 'NONE', ( #138990, #10016, #158471, #219521 ) ) ;
#226734 = ORIENTED_EDGE ( 'NONE', *, *, #12970, .F. ) ;
#226736 = AXIS2_PLACEMENT_3D ( 'NONE', #117125, #136664, #58395 ) ;
#226735 = FACE_OUTER_BOUND ( 'NONE', #118724, .T. ) ;
#226737 = EDGE_CURVE ( 'NONE', #3158, #250243, #209855, .T. ) ;
#226738 = ORIENTED_EDGE ( 'NONE', *, *, #192733, .F. ) ;
#226739 = CARTESIAN_POINT ( 'NONE',  ( 20.94999999999999929, 85.40000000001178648, -79.41707660717668205 ) ) ;
#226740 = AXIS2_PLACEMENT_3D ( 'NONE', #62397, #38998, #221438 ) ;
#226742 = DIRECTION ( 'NONE',  ( 0.000000000000000000, -1.000000000000000000, -6.982962677686265922E-15 ) ) ;
#226741 = CIRCLE ( 'NONE', #230871, 0.09999999999999939493 ) ;
#226743 = AXIS2_PLACEMENT_3D ( 'NONE', #97922, #236177, #121 ) ;
#226744 = AXIS2_PLACEMENT_3D ( 'NONE', #23745, #203631, #118974 ) ;
#226745 = ORIENTED_EDGE ( 'NONE', *, *, #114632, .T. ) ;
#226746 = CARTESIAN_POINT ( 'NONE',  ( -20.94999999999999929, 16.44800918141279666, -240.8068063186265135 ) ) ;
#226747 = EDGE_CURVE ( 'NONE', #111708, #99517, #101659, .T. ) ;
#226748 = ORIENTED_EDGE ( 'NONE', *, *, #196470, .T. ) ;
#226749 = LINE ( 'NONE', #68992, #12271 ) ;
#226750 = FACE_OUTER_BOUND ( 'NONE', #17283, .T. ) ;
#226752 = CIRCLE ( 'NONE', #177301, 0.1000000000000028644 ) ;
#226751 = DIRECTION ( 'NONE',  ( 0.000000000000000000, 1.000000000000000000, 6.982962677686266711E-15 ) ) ;
#226753 = TOROIDAL_SURFACE ( 'NONE', #68556, 0.2000000000000000111, 0.1000000000000000056 ) ;
#226755 = CARTESIAN_POINT ( 'NONE',  ( -21.65000000000000213, 23.06621698515930419, -230.9822826988504119 ) ) ;
#226754 = CIRCLE ( 'NONE', #76916, 0.09999999999999711897 ) ;
#226756 = CARTESIAN_POINT ( 'NONE',  ( 13.99999999999999822, 62.10905854918434699, -217.1108499610991203 ) ) ;
#226758 = CIRCLE ( 'NONE', #22784, 11.70000000000000639 ) ;
#226757 = DIRECTION ( 'NONE',  ( 1.000000000000000000, -0.000000000000000000, -0.000000000000000000 ) ) ;
#226759 = CARTESIAN_POINT ( 'NONE',  ( 21.14999999999999858, 6.540656951701244282, 0.000000000000000000 ) ) ;
#226761 = ORIENTED_EDGE ( 'NONE', *, *, #106220, .F. ) ;
#226760 = CARTESIAN_POINT ( 'NONE',  ( 18.31572054635827840, -0.7431314789941730892, -242.4582880902354702 ) ) ;
#226763 = FACE_OUTER_BOUND ( 'NONE', #33999, .T. ) ;
#226762 = CARTESIAN_POINT ( 'NONE',  ( 20.94999999999999929, 67.92720994251783395, -214.1870976236629929 ) ) ;
#226764 = CIRCLE ( 'NONE', #168565, 0.09999999999998898659 ) ;
#226765 = EDGE_LOOP ( 'NONE', ( #60395, #468, #163349, #145592 ) ) ;
#226767 = EDGE_LOOP ( 'NONE', ( #165978, #37384, #2613, #14250 ) ) ;
#226766 = CARTESIAN_POINT ( 'NONE',  ( -18.59999999999999787, 80.69087520990402140, -192.8618289658565743 ) ) ;
#226768 = VERTEX_POINT ( 'NONE', #43520 ) ;
#226769 = DIRECTION ( 'NONE',  ( -1.000000000000000000, -7.304098846218134667E-16, 4.217023435051678980E-16 ) ) ;
#226770 = CARTESIAN_POINT ( 'NONE',  ( 21.05000000000000071, 1.115600667400684642E-11, -71.09999999999999432 ) ) ;
#226771 = CIRCLE ( 'NONE', #189186, 0.09999999999998898659 ) ;
#226772 = CARTESIAN_POINT ( 'NONE',  ( -21.14999999999999858, 1.363275264940686293, -230.6442496871288483 ) ) ;
#226773 = DIRECTION ( 'NONE',  ( -1.000000000000000000, -0.000000000000000000, -0.000000000000000000 ) ) ;
#226774 = DIRECTION ( 'NONE',  ( 1.000000000000000000, 7.049440681616510987E-16, -1.911869773728121864E-16 ) ) ;
#226775 = AXIS2_PLACEMENT_3D ( 'NONE', #38909, #121029, #4865 ) ;
#226776 = LINE ( 'NONE', #48139, #218433 ) ;
#226777 = VECTOR ( 'NONE', #70313, 1000.000000000000000 ) ;
#226778 = CARTESIAN_POINT ( 'NONE',  ( -17.78241384942234049, 12.78794030309596330, -208.7042118961428514 ) ) ;
#226779 = CARTESIAN_POINT ( 'NONE',  ( -16.80939487329394666, 51.61886293219204447, -231.9464690156492281 ) ) ;
#226780 = CARTESIAN_POINT ( 'NONE',  ( 21.14999999999999858, 69.35000000001205933, -124.3731074845243540 ) ) ;
#226781 = ORIENTED_EDGE ( 'NONE', *, *, #157878, .T. ) ;
#226782 = ORIENTED_EDGE ( 'NONE', *, *, #154379, .F. ) ;
#226783 = CARTESIAN_POINT ( 'NONE',  ( -20.94999999999999929, 74.63912941282003999, -128.4501095574333647 ) ) ;
#226784 = EDGE_CURVE ( 'NONE', #36158, #133767, #39183, .T. ) ;
#226785 = VERTEX_POINT ( 'NONE', #23970 ) ;
#226786 = DIRECTION ( 'NONE',  ( 1.000000000000000000, 0.000000000000000000, 0.000000000000000000 ) ) ;
#226787 = ORIENTED_EDGE ( 'NONE', *, *, #224822, .T. ) ;
#226788 = CARTESIAN_POINT ( 'NONE',  ( 18.55857864376268296, 65.63284271248610935, -44.77310748452438816 ) ) ;
#226789 = DIRECTION ( 'NONE',  ( 0.000000000000000000, -7.272083257015735086E-15, 1.000000000000000000 ) ) ;
#226790 = DIRECTION ( 'NONE',  ( 0.000000000000000000, 0.000000000000000000, -1.000000000000000000 ) ) ;
#226791 = EDGE_CURVE ( 'NONE', #152685, #110735, #47505, .T. ) ;
#226792 = CARTESIAN_POINT ( 'NONE',  ( -23.15000000000000213, 64.35000000001195986, -110.0379132551783243 ) ) ;
#226793 = CARTESIAN_POINT ( 'NONE',  ( -18.79999999999999716, -11.75000000000000000, 5.900000000000001243 ) ) ;
#226794 = ORIENTED_EDGE ( 'NONE', *, *, #188275, .F. ) ;
#226795 = DIRECTION ( 'NONE',  ( 1.000000000000000000, 0.000000000000000000, -0.000000000000000000 ) ) ;
#226796 = AXIS2_PLACEMENT_3D ( 'NONE', #165528, #82094, #44296 ) ;
#226797 = EDGE_CURVE ( 'NONE', #27421, #216194, #189002, .T. ) ;
#226798 = EDGE_CURVE ( 'NONE', #38549, #29044, #58753, .T. ) ;
#226799 = CIRCLE ( 'NONE', #55898, 7.800000000000001599 ) ;
#226800 = CARTESIAN_POINT ( 'NONE',  ( -20.64999999999999858, 7.150000000011155876, -121.6500000000000341 ) ) ;
#226801 = CARTESIAN_POINT ( 'NONE',  ( -23.25000000000000000, 70.22889768795992893, -198.1282601183952750 ) ) ;
#226802 = DIRECTION ( 'NONE',  ( 0.000000000000000000, 0.000000000000000000, 1.000000000000000000 ) ) ;
#226803 = AXIS2_PLACEMENT_3D ( 'NONE', #101009, #18945, #198874 ) ;
#226804 = ORIENTED_EDGE ( 'NONE', *, *, #118850, .T. ) ;
#226806 = DIRECTION ( 'NONE',  ( 0.000000000000000000, -0.1575844902526579161, -0.9875055080513779338 ) ) ;
#226805 = CARTESIAN_POINT ( 'NONE',  ( 21.08078803292165659, 61.09833557356314060, -234.2738665335206463 ) ) ;
#226807 = ORIENTED_EDGE ( 'NONE', *, *, #139690, .F. ) ;
#226810 = VERTEX_POINT ( 'NONE', #216568 ) ;
#226809 = CARTESIAN_POINT ( 'NONE',  ( -16.80100914604136975, 51.59158805982346507, -231.9661947804042370 ) ) ;
#226808 = CARTESIAN_POINT ( 'NONE',  ( 21.14999999999999503, -0.09999999998884338825, -21.85042919245520210 ) ) ;
#226811 = ORIENTED_EDGE ( 'NONE', *, *, #105244, .F. ) ;
#226812 = CARTESIAN_POINT ( 'NONE',  ( -16.97092634996651483, 10.00088896635950420, -113.1301427662976948 ) ) ;
#226813 = AXIS2_PLACEMENT_3D ( 'NONE', #36001, #127719, #115512 ) ;
#226814 = DIRECTION ( 'NONE',  ( 0.000000000000000000, -0.8814952561688320642, 0.4721928772777551075 ) ) ;
#226815 = DIRECTION ( 'NONE',  ( 1.000000000000000000, 0.000000000000000000, 0.000000000000000000 ) ) ;
#226816 = CIRCLE ( 'NONE', #206155, 0.1000000000000028644 ) ;
#226817 = VERTEX_POINT ( 'NONE', #239997 ) ;
#226818 = CARTESIAN_POINT ( 'NONE',  ( -18.59999999999999787, 18.81339837015603322, -226.7756228984618190 ) ) ;
#226819 = ADVANCED_FACE ( 'NONE', ( #37958 ), #100442, .T. ) ;
#226821 = CARTESIAN_POINT ( 'NONE',  ( 20.94999999999999929, -1.362429037182151470, -141.8888812479212334 ) ) ;
#226820 =( BOUNDED_CURVE ( )  B_SPLINE_CURVE ( 3, ( #139017, #159931, #197746, #81615 ),
 .UNSPECIFIED., .F., .F. ) 
 B_SPLINE_CURVE_WITH_KNOTS ( ( 4, 4 ),
 ( 3.141592653589793116, 4.712388980384689674 ),
 .UNSPECIFIED. ) 
 CURVE ( )  GEOMETRIC_REPRESENTATION_ITEM ( )  RATIONAL_B_SPLINE_CURVE ( ( 1.000000000000000000, 0.8047378541243649375, 0.8047378541243649375, 1.000000000000000000 ) ) 
 REPRESENTATION_ITEM ( '' )  );
#226823 = CARTESIAN_POINT ( 'NONE',  ( -18.40000000000000213, 11.48667500175766953, -9.250000000000001776 ) ) ;
#226822 = CARTESIAN_POINT ( 'NONE',  ( 21.30000000000002558, -0.8618440306552703767, -197.0427629756619297 ) ) ;
#226825 = EDGE_LOOP ( 'NONE', ( #113070, #165506, #35812, #56410, #38830 ) ) ;
#226824 = CARTESIAN_POINT ( 'NONE',  ( 20.99780126800942526, 11.60538868788779610, -93.58735257170532407 ) ) ;
#226826 = AXIS2_PLACEMENT_3D ( 'NONE', #73656, #35806, #194879 ) ;
#226827 = AXIS2_PLACEMENT_3D ( 'NONE', #90108, #131818, #206228 ) ;
#226828 = CIRCLE ( 'NONE', #155939, 0.1000000000000028644 ) ;
#226829 = VERTEX_POINT ( 'NONE', #19667 ) ;
#226830 = LINE ( 'NONE', #48188, #257409 ) ;
#226831 = B_SPLINE_CURVE_WITH_KNOTS ( 'NONE', 3,
 ( #164484, #257407, #65368, #158405, #237902, #59220 ),
 .UNSPECIFIED., .F., .F.,
 ( 4, 2, 4 ),
 ( 0.000000000000000000, 0.0001496588209255837190, 0.0002993176418511674379 ),
 .UNSPECIFIED. ) ;
#226832 = DIRECTION ( 'NONE',  ( -1.000000000000000000, 0.000000000000000000, -0.000000000000000000 ) ) ;
#226833 = CARTESIAN_POINT ( 'NONE',  ( -23.15000000000000213, 64.35000000001275566, -215.2731074845244450 ) ) ;
#226834 = ORIENTED_EDGE ( 'NONE', *, *, #177148, .T. ) ;
#226835 = LINE ( 'NONE', #5192, #189346 ) ;
#226837 = ADVANCED_FACE ( 'NONE', ( #238699 ), #201452, .T. ) ;
#226836 = CARTESIAN_POINT ( 'NONE',  ( 21.00000000000000000, 66.25000000001158185, -57.27310748452438816 ) ) ;
#226838 = ADVANCED_FACE ( 'NONE', ( #161759 ), #39246, .F. ) ;
#226839 = AXIS2_PLACEMENT_3D ( 'NONE', #38151, #117667, #177678 ) ;
#226840 = VERTEX_POINT ( 'NONE', #117479 ) ;
#226841 = FACE_OUTER_BOUND ( 'NONE', #245229, .T. ) ;
#226842 = AXIS2_PLACEMENT_3D ( 'NONE', #46020, #79988, #145113 ) ;
#226844 = ADVANCED_FACE ( 'NONE', ( #82162 ), #198286, .F. ) ;
#226843 = EDGE_LOOP ( 'NONE', ( #34140, #209969, #1600 ) ) ;
#226845 = CARTESIAN_POINT ( 'NONE',  ( 21.05000000000000071, -11.48912529306489994, -97.40000000000004832 ) ) ;
#226846 = CARTESIAN_POINT ( 'NONE',  ( -18.36973785203555920, 64.52449679952756867, -78.77310748452438816 ) ) ;
#226847 = AXIS2_PLACEMENT_3D ( 'NONE', #107922, #170524, #30993 ) ;
#226848 = AXIS2_PLACEMENT_3D ( 'NONE', #191331, #131317, #231723 ) ;
#226849 = EDGE_LOOP ( 'NONE', ( #31, #243464, #137169, #22850 ) ) ;
#226850 = CIRCLE ( 'NONE', #114432, 0.2000000000000057288 ) ;
#226851 = ORIENTED_EDGE ( 'NONE', *, *, #26440, .T. ) ;
#226852 = CARTESIAN_POINT ( 'NONE',  ( 23.30000000000000426, 3.332938107839120701, -347.0000000000001137 ) ) ;
#226853 = EDGE_LOOP ( 'NONE', ( #64629, #186348, #190687, #80594 ) ) ;
#226855 = VERTEX_POINT ( 'NONE', #96593 ) ;
#226854 = CARTESIAN_POINT ( 'NONE',  ( -21.07928932188134041, 6.328516656393293083, 0.09889514565439641580 ) ) ;
#226856 = VERTEX_POINT ( 'NONE', #178770 ) ;
#226859 = EDGE_CURVE ( 'NONE', #228856, #245204, #77, .T. ) ;
#226858 = EDGE_LOOP ( 'NONE', ( #174361, #135284, #38519, #164059 ) ) ;
#226857 = ORIENTED_EDGE ( 'NONE', *, *, #76556, .F. ) ;
#226860 = CARTESIAN_POINT ( 'NONE',  ( -18.59999999999999787, -9.480686695267820596, -107.4411151687578894 ) ) ;
#226861 = ORIENTED_EDGE ( 'NONE', *, *, #166078, .F. ) ;
#226862 = CARTESIAN_POINT ( 'NONE',  ( 20.97239005616515328, 22.11792297137228758, -231.6940034657905301 ) ) ;
#226863 = DIRECTION ( 'NONE',  ( -1.000000000000000000, 0.000000000000000000, 0.000000000000000000 ) ) ;
#226864 = AXIS2_PLACEMENT_3D ( 'NONE', #226922, #48284, #34845 ) ;
#226865 = DIRECTION ( 'NONE',  ( 1.000000000000000000, -0.000000000000000000, -0.000000000000000000 ) ) ;
#226866 = DIRECTION ( 'NONE',  ( -1.000000000000000000, 0.000000000000000000, 0.000000000000000000 ) ) ;
#226867 = VERTEX_POINT ( 'NONE', #2645 ) ;
#226868 = ORIENTED_EDGE ( 'NONE', *, *, #237263, .T. ) ;
#226869 = EDGE_CURVE ( 'NONE', #224430, #88161, #130724, .T. ) ;
#226870 = CARTESIAN_POINT ( 'NONE',  ( 22.39999999999999503, 75.90000000001242597, -176.2731074845243597 ) ) ;
#226871 = CIRCLE ( 'NONE', #35389, 0.09999999999999939493 ) ;
#226873 = EDGE_LOOP ( 'NONE', ( #137859, #48539, #83965, #36953 ) ) ;
#226872 = DIRECTION ( 'NONE',  ( 0.000000000000000000, -0.4721928772777332917, -0.8814952561688437216 ) ) ;
#226874 = CARTESIAN_POINT ( 'NONE',  ( -16.79814274880124358, 9.949272542688458287, -180.1524330370479845 ) ) ;
#226876 = ORIENTED_EDGE ( 'NONE', *, *, #205184, .F. ) ;
#226875 = FACE_OUTER_BOUND ( 'NONE', #111276, .T. ) ;
#226877 = ORIENTED_EDGE ( 'NONE', *, *, #255199, .F. ) ;
#226878 = CARTESIAN_POINT ( 'NONE',  ( -21.05000000000000071, 1.115600667400684642E-11, -167.4999999999999716 ) ) ;
#226879 = EDGE_CURVE ( 'NONE', #209722, #218497, #226564, .T. ) ;
#226880 = EDGE_CURVE ( 'NONE', #133463, #77132, #164055, .T. ) ;
#226881 = ORIENTED_EDGE ( 'NONE', *, *, #163174, .F. ) ;
#226882 = CARTESIAN_POINT ( 'NONE',  ( -16.82055514392353501, 9.950000000011076651, -180.1767980745427167 ) ) ;
#226883 = CARTESIAN_POINT ( 'NONE',  ( 18.49999999999999645, 68.50594083727658301, -224.0235912779512830 ) ) ;
#226884 = EDGE_CURVE ( 'NONE', #194066, #75197, #51579, .T. ) ;
#226887 = ORIENTED_EDGE ( 'NONE', *, *, #111377, .T. ) ;
#226886 = VERTEX_POINT ( 'NONE', #120072 ) ;
#226885 = VECTOR ( 'NONE', #7482, 1000.000000000000000 ) ;
#226888 = AXIS2_PLACEMENT_3D ( 'NONE', #196027, #177759, #38234 ) ;
#226889 = ORIENTED_EDGE ( 'NONE', *, *, #177474, .F. ) ;
#226891 = EDGE_CURVE ( 'NONE', #52329, #233201, #35099, .T. ) ;
#226890 = DIRECTION ( 'NONE',  ( 0.000000000000000000, -1.000000000000000000, 0.000000000000000000 ) ) ;
#226892 = ORIENTED_EDGE ( 'NONE', *, *, #95373, .F. ) ;
#226893 = ORIENTED_EDGE ( 'NONE', *, *, #197054, .T. ) ;
#226894 = DIRECTION ( 'NONE',  ( 0.000000000000000000, 0.8096735173027139743, -0.5868805631290339164 ) ) ;
#226896 = ORIENTED_EDGE ( 'NONE', *, *, #198190, .T. ) ;
#226895 = DIRECTION ( 'NONE',  ( 0.000000000000000000, 0.9998779222360096863, -0.01562500000001061998 ) ) ;
#226897 = DIRECTION ( 'NONE',  ( -3.265361837132813093E-16, -1.000000000000000000, -6.982962677686266711E-15 ) ) ;
#226899 = LINE ( 'NONE', #131653, #227434 ) ;
#226898 = DIRECTION ( 'NONE',  ( 0.000000000000000000, -0.9126074666063660468, -0.4088369013363524762 ) ) ;
#226900 = CARTESIAN_POINT ( 'NONE',  ( -23.25000000000000000, 76.00000000001195133, -103.0231074845243171 ) ) ;
#226901 = CARTESIAN_POINT ( 'NONE',  ( -20.90000000000000213, 0.000000000000000000, 0.000000000000000000 ) ) ;
#226902 = ORIENTED_EDGE ( 'NONE', *, *, #30056, .T. ) ;
#226903 = ORIENTED_EDGE ( 'NONE', *, *, #133915, .T. ) ;
#226904 = CARTESIAN_POINT ( 'NONE',  ( 20.94999999999999574, 0.6869237119019839799, -212.7787591058053067 ) ) ;
#226906 = EDGE_CURVE ( 'NONE', #55121, #164375, #109865, .T. ) ;
#226905 = CARTESIAN_POINT ( 'NONE',  ( -23.25000000000000000, -9.599999999988838795, -157.6060308773475924 ) ) ;
#226907 = ORIENTED_EDGE ( 'NONE', *, *, #122388, .F. ) ;
#226908 = CIRCLE ( 'NONE', #172967, 0.09999999999999326095 ) ;
#226909 = ADVANCED_FACE ( 'NONE', ( #121365 ), #160479, .T. ) ;
#226910 = ADVANCED_FACE ( 'NONE', ( #196989 ), #18370, .F. ) ;
#226911 = AXIS2_PLACEMENT_3D ( 'NONE', #155811, #239174, #181772 ) ;
#226912 = AXIS2_PLACEMENT_3D ( 'NONE', #136279, #83989, #166187 ) ;
#226913 = DIRECTION ( 'NONE',  ( -0.000000000000000000, 1.000000000000000000, -0.000000000000000000 ) ) ;
#226914 = ORIENTED_EDGE ( 'NONE', *, *, #248266, .T. ) ;
#226915 = VERTEX_POINT ( 'NONE', #182599 ) ;
#226916 =( BOUNDED_SURFACE ( )  B_SPLINE_SURFACE ( 3, 2, ( 
 ( #146683, #171454, #151882 ),
 ( #128437, #29379, #248385 ),
 ( #210545, #69765, #231401 ),
 ( #52738, #226209, #47595 ) ),
 .UNSPECIFIED., .F., .F., .T. ) 
 B_SPLINE_SURFACE_WITH_KNOTS ( ( 4, 4 ),
 ( 3, 3 ),
 ( 5.727910411845712702, 5.983100554402350113 ),
 ( 0.000000000000000000, 1.000000000000000000 ),
 .UNSPECIFIED. ) 
 GEOMETRIC_REPRESENTATION_ITEM ( )  RATIONAL_B_SPLINE_SURFACE ( (
 ( 1.000000000000000000, 0.8946697475932056109, 1.000000000000000000),
 ( 1.000000000000000000, 0.9035312726220235957, 1.000000000000000000),
 ( 1.000000000000000000, 0.9104333467450250739, 1.000000000000000000),
 ( 1.000000000000000000, 0.9152888060719243102, 1.000000000000000000) ) ) 
 REPRESENTATION_ITEM ( '' )  SURFACE ( )  );
#226917 = ADVANCED_FACE ( 'NONE', ( #231662 ), #83446, .F. ) ;
#226918 = CARTESIAN_POINT ( 'NONE',  ( -20.94999999999999929, 64.25000000001264766, -196.6815067946272961 ) ) ;
#226919 = CARTESIAN_POINT ( 'NONE',  ( -20.54999999999999716, 68.56901367119438362, -214.3038979092079046 ) ) ;
#226920 = ORIENTED_EDGE ( 'NONE', *, *, #197737, .T. ) ;
#226921 = DIRECTION ( 'NONE',  ( -1.000000000000000000, 0.000000000000000000, 0.000000000000000000 ) ) ;
#226922 = CARTESIAN_POINT ( 'NONE',  ( -20.64999999999999858, 1.115600667400684642E-11, -167.4999999999999716 ) ) ;
#226923 = ORIENTED_EDGE ( 'NONE', *, *, #23592, .T. ) ;
#226924 = DIRECTION ( 'NONE',  ( 0.000000000000000000, 0.9910827722268050755, 0.1332476588733589318 ) ) ;
#226925 = CARTESIAN_POINT ( 'NONE',  ( 24.30000000000000071, -12.79999999999999716, -347.0000000000001137 ) ) ;
#226927 = DIRECTION ( 'NONE',  ( 1.000000000000000000, 0.000000000000000000, 0.000000000000000000 ) ) ;
#226926 = CARTESIAN_POINT ( 'NONE',  ( -33.72168855820452649, 13.17878477875124688, -207.5966336730521391 ) ) ;
#226928 = CARTESIAN_POINT ( 'NONE',  ( 19.86930884467567182, 11.68691006698220392, -91.73922263893891227 ) ) ;
#226929 = ADVANCED_FACE ( 'NONE', ( #12621 ), #137649, .F. ) ;
#226930 = LINE ( 'NONE', #10461, #149358 ) ;
#226932 = ADVANCED_FACE ( 'NONE', ( #92131 ), #247423, .T. ) ;
#226931 = DIRECTION ( 'NONE',  ( 0.000000000000000000, -0.9999176327611369874, 0.01283462868041987913 ) ) ;
#226933 = DIRECTION ( 'NONE',  ( -1.000000000000000000, -0.000000000000000000, -0.000000000000000000 ) ) ;
#226934 = ADVANCED_FACE ( 'NONE', ( #144721 ), #123902, .T. ) ;
#226935 = ORIENTED_EDGE ( 'NONE', *, *, #117747, .F. ) ;
#226936 = TOROIDAL_SURFACE ( 'NONE', #2052, 2.100000000000002309, 0.1000000000000000056 ) ;
#226937 = AXIS2_PLACEMENT_3D ( 'NONE', #19401, #173384, #195494 ) ;
#226939 = EDGE_LOOP ( 'NONE', ( #126939, #51577, #33089, #65231 ) ) ;
#226938 = ORIENTED_EDGE ( 'NONE', *, *, #76503, .T. ) ;
#226940 = ORIENTED_EDGE ( 'NONE', *, *, #129444, .F. ) ;
#226941 = CIRCLE ( 'NONE', #131068, 0.1000000000000028644 ) ;
#226942 = CARTESIAN_POINT ( 'NONE',  ( -22.94999999999999929, -1.901609089591594692, -11.59510167572422112 ) ) ;
#226943 = DIRECTION ( 'NONE',  ( -1.000000000000000000, 0.000000000000000000, 0.000000000000000000 ) ) ;
#226944 = EDGE_CURVE ( 'NONE', #9432, #30065, #172476, .T. ) ;
#226946 = CARTESIAN_POINT ( 'NONE',  ( 23.15000000000000213, -11.74999999998883560, -97.40000000000004832 ) ) ;
#226945 = DIRECTION ( 'NONE',  ( 0.000000000000000000, 0.000000000000000000, -1.000000000000000000 ) ) ;
#226947 = EDGE_CURVE ( 'NONE', #176243, #25637, #150822, .T. ) ;
#226948 = DIRECTION ( 'NONE',  ( 0.000000000000000000, -6.982962677686266711E-15, 1.000000000000000000 ) ) ;
#226949 = ORIENTED_EDGE ( 'NONE', *, *, #67365, .F. ) ;
#226950 = AXIS2_PLACEMENT_3D ( 'NONE', #211707, #246947, #30502 ) ;
#226951 = CARTESIAN_POINT ( 'NONE',  ( 18.59999999999999076, 1.115600667400684642E-11, -67.00000000000000000 ) ) ;
#226952 = CIRCLE ( 'NONE', #214463, 11.74999999999999822 ) ;
#226954 = AXIS2_PLACEMENT_3D ( 'NONE', #172644, #8390, #30533 ) ;
#226953 = CARTESIAN_POINT ( 'NONE',  ( -18.59999999999999787, 85.40000000001154490, -62.22584772486096938 ) ) ;
#226955 = CARTESIAN_POINT ( 'NONE',  ( -16.84421487269769813, 66.05000000001187743, -90.35360536207943483 ) ) ;
#226956 = CARTESIAN_POINT ( 'NONE',  ( 22.39999999999999858, 0.1000000000111554016, -59.20922040162665922 ) ) ;
#226957 = ORIENTED_EDGE ( 'NONE', *, *, #29813, .F. ) ;
#226958 = CARTESIAN_POINT ( 'NONE',  ( -23.25000000000000000, 4.349999999999999645, -12.35000000000000142 ) ) ;
#226959 = AXIS2_PLACEMENT_3D ( 'NONE', #204372, #242216, #45313 ) ;
#226960 = DIRECTION ( 'NONE',  ( 0.000000000000000000, -0.1350103645451807555, -0.9908441862701610203 ) ) ;
#226961 = ORIENTED_EDGE ( 'NONE', *, *, #227726, .T. ) ;
#226962 = ORIENTED_EDGE ( 'NONE', *, *, #126776, .T. ) ;
#226963 = DIRECTION ( 'NONE',  ( -0.000000000000000000, -0.1350103645451876666, -0.9908441862701600211 ) ) ;
#226964 = AXIS2_PLACEMENT_3D ( 'NONE', #182159, #124751, #7358 ) ;
#226965 = DIRECTION ( 'NONE',  ( -0.000000000000000000, -0.000000000000000000, 1.000000000000000000 ) ) ;
#226966 = FACE_OUTER_BOUND ( 'NONE', #4417, .T. ) ;
#226967 = CARTESIAN_POINT ( 'NONE',  ( 20.95346350065193519, 67.11282275083711113, -61.01137553748900189 ) ) ;
#226968 = FACE_OUTER_BOUND ( 'NONE', #246939, .T. ) ;
#226969 = AXIS2_PLACEMENT_3D ( 'NONE', #147632, #172384, #128076 ) ;
#226970 = CARTESIAN_POINT ( 'NONE',  ( 20.94999999999999929, -8.730841121484166578, -124.4019252810156928 ) ) ;
#226972 = ORIENTED_EDGE ( 'NONE', *, *, #52609, .T. ) ;
#226971 = AXIS2_PLACEMENT_3D ( 'NONE', #234475, #76683, #237053 ) ;
#226973 = DIRECTION ( 'NONE',  ( 1.000000000000000000, 0.000000000000000000, 0.000000000000000000 ) ) ;
#226974 = CARTESIAN_POINT ( 'NONE',  ( 21.05000000000000071, 11.83124523798471905, -206.0547899340221818 ) ) ;
#226976 = FACE_OUTER_BOUND ( 'NONE', #190128, .T. ) ;
#226975 = CARTESIAN_POINT ( 'NONE',  ( -16.94132844910801694, 9.992436755191498321, -87.89620175598236074 ) ) ;
#226977 = DIRECTION ( 'NONE',  ( 0.000000000000000000, -1.000000000000000000, 0.000000000000000000 ) ) ;
#226978 = DIRECTION ( 'NONE',  ( 0.000000000000000000, 0.2617529984164915779, 0.9651348961777189706 ) ) ;
#226979 = ADVANCED_FACE ( 'NONE', ( #202148 ), #143447, .F. ) ;
#226980 = CARTESIAN_POINT ( 'NONE',  ( -23.15000000000000213, 61.88149656937975607, -248.1136133839584090 ) ) ;
#226981 = CARTESIAN_POINT ( 'NONE',  ( 20.94999999999999929, 74.16465844978715438, -57.96795619196134908 ) ) ;
#226983 = EDGE_LOOP ( 'NONE', ( #235638, #209183, #221165, #134059 ) ) ;
#226982 = DIRECTION ( 'NONE',  ( 0.000000000000000000, 0.6728388485993012091, -0.7397890806274222131 ) ) ;
#226984 = EDGE_CURVE ( 'NONE', #4874, #108089, #32187, .T. ) ;
#226985 = AXIS2_PLACEMENT_3D ( 'NONE', #28296, #110356, #107791 ) ;
#226986 = AXIS2_PLACEMENT_3D ( 'NONE', #209830, #50716, #195420 ) ;
#226987 = DIRECTION ( 'NONE',  ( -1.000000000000000000, 0.000000000000000000, 0.000000000000000000 ) ) ;
#226988 = EDGE_CURVE ( 'NONE', #66961, #203823, #24823, .T. ) ;
#226989 = VECTOR ( 'NONE', #182243, 1000.000000000000114 ) ;
#226990 = CARTESIAN_POINT ( 'NONE',  ( -23.25000000000000000, -1.835859311443637010, -45.10443916879852821 ) ) ;
#226991 = ORIENTED_EDGE ( 'NONE', *, *, #99081, .F. ) ;
#226992 = CARTESIAN_POINT ( 'NONE',  ( -18.59999999999999787, 77.16412189325258453, -28.10825939895270764 ) ) ;
#226993 = FACE_OUTER_BOUND ( 'NONE', #106981, .T. ) ;
#226994 = CARTESIAN_POINT ( 'NONE',  ( -18.50000000000000000, 25.52560498759422103, -248.6860249505299407 ) ) ;
#226995 = CIRCLE ( 'NONE', #168789, 0.09999999999999939493 ) ;
#226996 = ORIENTED_EDGE ( 'NONE', *, *, #37178, .F. ) ;
#226997 = CARTESIAN_POINT ( 'NONE',  ( -16.86379686415369861, 12.42092813644865501, -211.1560426965246791 ) ) ;
#226999 = ORIENTED_EDGE ( 'NONE', *, *, #237805, .F. ) ;
#226998 = CARTESIAN_POINT ( 'NONE',  ( -16.87401514999227814, 9.950000000011137047, -188.2800179925320663 ) ) ;
#227000 = DIRECTION ( 'NONE',  ( 0.000000000000000000, -0.008583690987162452199, 0.9999631594459053030 ) ) ;
#227001 = DIRECTION ( 'NONE',  ( 1.000000000000000000, 0.000000000000000000, 0.000000000000000000 ) ) ;
#227002 = ORIENTED_EDGE ( 'NONE', *, *, #61072, .F. ) ;
#227003 = DIRECTION ( 'NONE',  ( 0.000000000000000000, -6.982962677686266711E-15, 1.000000000000000000 ) ) ;
#227004 = AXIS2_PLACEMENT_3D ( 'NONE', #29110, #47317, #186872 ) ;
#227005 = CARTESIAN_POINT ( 'NONE',  ( 0.000000000000000000, 0.000000000000000000, 0.000000000000000000 ) ) ;
#227006 = DIRECTION ( 'NONE',  ( 0.000000000000000000, 1.000000000000000000, -6.308085367188393199E-16 ) ) ;
#227007 = CIRCLE ( 'NONE', #114588, 0.09999999999999939493 ) ;
#227008 = ORIENTED_EDGE ( 'NONE', *, *, #148607, .F. ) ;
#227009 = DIRECTION ( 'NONE',  ( -1.000000000000000000, -0.000000000000000000, -0.000000000000000000 ) ) ;
#227010 = PLANE ( 'NONE',  #150797 ) ;
#227011 = DIRECTION ( 'NONE',  ( 0.000000000000000000, 0.9654727137038715545, 0.2605042016806676242 ) ) ;
#227012 = FACE_OUTER_BOUND ( 'NONE', #108190, .T. ) ;
#227013 = ORIENTED_EDGE ( 'NONE', *, *, #165874, .F. ) ;
#227014 = VECTOR ( 'NONE', #91835, 1000.000000000000000 ) ;
#227015 = ORIENTED_EDGE ( 'NONE', *, *, #177803, .F. ) ;
#227016 = DIRECTION ( 'NONE',  ( 0.000000000000000000, 1.000000000000000000, 0.000000000000000000 ) ) ;
#227017 = EDGE_CURVE ( 'NONE', #164049, #187774, #22422, .T. ) ;
#227018 = CARTESIAN_POINT ( 'NONE',  ( 18.49505816908824229, 85.43787255322298790, -96.24545028285334070 ) ) ;
#227019 = DIRECTION ( 'NONE',  ( 0.000000000000000000, 0.4999999999999608646, -0.8660254037844612451 ) ) ;
#227020 = DIRECTION ( 'NONE',  ( 0.000000000000000000, -6.938893903907270030E-14, 1.000000000000000000 ) ) ;
#227021 = CARTESIAN_POINT ( 'NONE',  ( -21.05000000000000071, 0.2561057920922211739, 0.03489644167229202787 ) ) ;
#227022 = EDGE_CURVE ( 'NONE', #174346, #18466, #234790, .T. ) ;
#227024 = DIRECTION ( 'NONE',  ( 0.000000000000000000, -0.8814952561688629284, 0.4721928772776973204 ) ) ;
#227023 = DIRECTION ( 'NONE',  ( 0.000000000000000000, 0.2617529984165042345, 0.9651348961777153068 ) ) ;
#227025 = CARTESIAN_POINT ( 'NONE',  ( 23.24999999999999645, 31.05627573922685158, -233.2203535436961488 ) ) ;
#227026 = B_SPLINE_CURVE_WITH_KNOTS ( 'NONE', 3,
 ( #165261, #205656, #105243, #25754, #81833, #6176, #85684, #225209, #46578, #143112, #103976, #62315, #161435, #183551, #33498, #51702, #8761, #229093, #146964, #68736, #170451, #226492, #129964, #128713, #86978, #247356 ),
 .UNSPECIFIED., .F., .F.,
 ( 4, 2, 2, 2, 2, 2, 2, 2, 2, 2, 2, 2, 4 ),
 ( 0.005476422646581329164, 0.006160811967703599956, 0.006845201288825871616, 0.007187395949386978823, 0.007529590609948086030, 0.007871785270509192370, 0.008213979931070300444, 0.008556174591631406784, 0.008898369252192513124, 0.009240563912753619463, 0.009582758573314727538, 0.01026714789443688644, 0.01095153721555904361 ),
 .UNSPECIFIED. ) ;
#227027 = CARTESIAN_POINT ( 'NONE',  ( 20.84999999999999432, 77.16412189325305349, -95.10825939895268277 ) ) ;
#227028 = CARTESIAN_POINT ( 'NONE',  ( -18.40000000000000213, 46.96039402156215914, -255.3459641718773128 ) ) ;
#227029 = DIRECTION ( 'NONE',  ( -1.000000000000000000, -0.000000000000000000, -0.000000000000000000 ) ) ;
#227030 = TOROIDAL_SURFACE ( 'NONE', #23054, 12.97499999999999609, 0.1000000000000000056 ) ;
#227032 = ORIENTED_EDGE ( 'NONE', *, *, #92768, .T. ) ;
#227031 = DIRECTION ( 'NONE',  ( 0.000000000000000000, 0.000000000000000000, -1.000000000000000000 ) ) ;
#227033 = CYLINDRICAL_SURFACE ( 'NONE', #256005, 0.09999999999998898659 ) ;
#227034 = FACE_OUTER_BOUND ( 'NONE', #215423, .T. ) ;
#227036 = DIRECTION ( 'NONE',  ( 1.000000000000000000, 3.190570557967288949E-16, 6.948722487160392945E-17 ) ) ;
#227035 = LINE ( 'NONE', #30148, #71882 ) ;
#227037 = EDGE_CURVE ( 'NONE', #173670, #69817, #23548, .T. ) ;
#227038 = ORIENTED_EDGE ( 'NONE', *, *, #254506, .T. ) ;
#227039 = DIRECTION ( 'NONE',  ( 1.000000000000000000, 0.000000000000000000, -0.000000000000000000 ) ) ;
#227040 = DIRECTION ( 'NONE',  ( 0.000000000000000000, 0.9651348961777157509, -0.2617529984165031243 ) ) ;
#227041 = CARTESIAN_POINT ( 'NONE',  ( -20.54999999999999716, 9.350000000011156942, -54.75000000000000000 ) ) ;
#227042 = DIRECTION ( 'NONE',  ( 1.000000000000000000, -0.000000000000000000, -0.000000000000000000 ) ) ;
#227043 = CARTESIAN_POINT ( 'NONE',  ( 22.49999999999999645, 12.54152817314150070, -223.4164406214577241 ) ) ;
#227044 = EDGE_CURVE ( 'NONE', #32735, #233386, #152133, .T. ) ;
#227045 = ORIENTED_EDGE ( 'NONE', *, *, #107595, .T. ) ;
#227046 = ORIENTED_EDGE ( 'NONE', *, *, #251062, .F. ) ;
#227047 = CARTESIAN_POINT ( 'NONE',  ( 21.05000000000000071, 6.540656951712400691, -100.6000000000000369 ) ) ;
#227048 = EDGE_CURVE ( 'NONE', #166855, #81393, #170442, .T. ) ;
#227049 = ORIENTED_EDGE ( 'NONE', *, *, #180474, .F. ) ;
#227050 = CARTESIAN_POINT ( 'NONE',  ( 21.05000000000000071, 65.57661458509899433, -95.53105556065429482 ) ) ;
#227051 = AXIS2_PLACEMENT_3D ( 'NONE', #215687, #179181, #157036 ) ;
#227052 = ORIENTED_EDGE ( 'NONE', *, *, #89318, .T. ) ;
#227053 = SPHERICAL_SURFACE ( 'NONE', #102543, 0.1000000000000000056 ) ;
#227054 = AXIS2_PLACEMENT_3D ( 'NONE', #67651, #164198, #125071 ) ;
#227055 = CARTESIAN_POINT ( 'NONE',  ( -21.10000000000000142, 6.223900101154156594, 12.00000000000000000 ) ) ;
#227056 = ORIENTED_EDGE ( 'NONE', *, *, #66477, .T. ) ;
#227057 = EDGE_CURVE ( 'NONE', #146076, #184932, #111698, .T. ) ;
#227058 = DIRECTION ( 'NONE',  ( 0.000000000000000000, -6.982962677686266711E-15, 1.000000000000000000 ) ) ;
#227059 = CARTESIAN_POINT ( 'NONE',  ( -21.05000000000000426, -0.02103547652896323866, -161.1955441780523586 ) ) ;
#227060 = CARTESIAN_POINT ( 'NONE',  ( 21.05000000000000071, 76.00000000001145395, -40.12310748452431852 ) ) ;
#227061 = LINE ( 'NONE', #210094, #222125 ) ;
#227062 = CARTESIAN_POINT ( 'NONE',  ( 23.24999999999999645, 65.72352950616313194, -223.1694128933794730 ) ) ;
#227063 = PLANE ( 'NONE',  #123971 ) ;
#227064 = ORIENTED_EDGE ( 'NONE', *, *, #250429, .T. ) ;
#227066 = CARTESIAN_POINT ( 'NONE',  ( 23.14999999999999858, 69.35000000001156195, -57.17310748452436542 ) ) ;
#227065 = CARTESIAN_POINT ( 'NONE',  ( -16.97048326478264713, 66.05000000001207638, -123.3820006043972057 ) ) ;
#227067 = VERTEX_POINT ( 'NONE', #98499 ) ;
#227069 = EDGE_LOOP ( 'NONE', ( #227963, #175289, #49492, #240321 ) ) ;
#227068 = DIRECTION ( 'NONE',  ( 1.000000000000000000, 0.000000000000000000, 0.000000000000000000 ) ) ;
#227070 = CIRCLE ( 'NONE', #56366, 0.09999999999998898659 ) ;
#227071 = VERTEX_POINT ( 'NONE', #158549 ) ;
#227072 = AXIS2_PLACEMENT_3D ( 'NONE', #182438, #205835, #123741 ) ;
#227073 = CARTESIAN_POINT ( 'NONE',  ( -20.64999999999999858, 68.85000000001205933, -124.1731074845243370 ) ) ;
#227074 = CARTESIAN_POINT ( 'NONE',  ( -18.39999999999999858, 11.47867410001042998, -176.7746932163406086 ) ) ;
#227075 = DIRECTION ( 'NONE',  ( -0.000000000000000000, -1.000000000000000000, -0.000000000000000000 ) ) ;
#227076 = DIRECTION ( 'NONE',  ( -4.391705002472924160E-16, -0.4088369013363268301, 0.9126074666063775931 ) ) ;
#227077 = ORIENTED_EDGE ( 'NONE', *, *, #124760, .T. ) ;
#227078 = DIRECTION ( 'NONE',  ( -2.602085213965225788E-14, 0.8814952561688430555, -0.4721928772777346239 ) ) ;
#227079 = CARTESIAN_POINT ( 'NONE',  ( 18.49999999999999289, 10.20857864377384416, -158.6500000000000057 ) ) ;
#227080 = ORIENTED_EDGE ( 'NONE', *, *, #201513, .F. ) ;
#227081 = CARTESIAN_POINT ( 'NONE',  ( 18.46947024752506294, -9.509297157144905199, -174.4866894486979447 ) ) ;
#227083 = AXIS2_PLACEMENT_3D ( 'NONE', #147340, #44406, #3977 ) ;
#227082 = CARTESIAN_POINT ( 'NONE',  ( 21.13498764882293557, 6.495618143473869566, 0.001656394731334435771 ) ) ;
#227084 = ORIENTED_EDGE ( 'NONE', *, *, #140428, .F. ) ;
#227086 = DIRECTION ( 'NONE',  ( 0.7071359030027680737, 0.7070776581709111719, 0.000000000000000000 ) ) ;
#227085 = AXIS2_PLACEMENT_3D ( 'NONE', #125138, #80840, #23493 ) ;
#227087 = CIRCLE ( 'NONE', #239575, 0.1000000000000028644 ) ;
#227088 = AXIS2_PLACEMENT_3D ( 'NONE', #33951, #170899, #74349 ) ;
#227089 = EDGE_CURVE ( 'NONE', #177719, #64371, #13886, .T. ) ;
#227090 = ORIENTED_EDGE ( 'NONE', *, *, #218653, .T. ) ;
#227091 = DIRECTION ( 'NONE',  ( 0.5932847527679310229, 0.8049926720990042694, 6.257843056355992909E-15 ) ) ;
#227092 = ORIENTED_EDGE ( 'NONE', *, *, #131840, .F. ) ;
#227093 = FACE_OUTER_BOUND ( 'NONE', #61085, .T. ) ;
#227094 = CARTESIAN_POINT ( 'NONE',  ( -18.39999999999999858, 8.841736820195469804, -245.4273993276876240 ) ) ;
#227095 = DIRECTION ( 'NONE',  ( 0.000000000000000000, 0.9126074666063772600, 0.4088369013363276627 ) ) ;
#227096 = EDGE_CURVE ( 'NONE', #131327, #239872, #35284, .T. ) ;
#227097 = EDGE_CURVE ( 'NONE', #250193, #122594, #101848, .T. ) ;
#227098 = EDGE_CURVE ( 'NONE', #141186, #196430, #56058, .T. ) ;
#227099 = CARTESIAN_POINT ( 'NONE',  ( -20.54999999999999716, 1.115600667400684642E-11, -134.0000000000000284 ) ) ;
#227100 = DIRECTION ( 'NONE',  ( 1.000000000000000000, 0.000000000000000000, 0.000000000000000000 ) ) ;
#227101 = ORIENTED_EDGE ( 'NONE', *, *, #26090, .F. ) ;
#227102 = CARTESIAN_POINT ( 'NONE',  ( 21.14999999999999858, 31.94635157770351341, -238.7871412784868710 ) ) ;
#227103 = AXIS2_PLACEMENT_3D ( 'NONE', #222654, #10041, #84390 ) ;
#227104 = VERTEX_POINT ( 'NONE', #174292 ) ;
#227106 = CARTESIAN_POINT ( 'NONE',  ( 23.25000000000000355, 98.45632476063525473, -163.2292090367925823 ) ) ;
#227105 = DIRECTION ( 'NONE',  ( -1.000000000000000000, -0.000000000000000000, -0.000000000000000000 ) ) ;
#227107 = AXIS2_PLACEMENT_3D ( 'NONE', #106928, #186488, #7858 ) ;
#227108 = ORIENTED_EDGE ( 'NONE', *, *, #159185, .T. ) ;
#227109 = VECTOR ( 'NONE', #213267, 1000.000000000000000 ) ;
#227110 = CYLINDRICAL_SURFACE ( 'NONE', #205325, 0.09999999999999939493 ) ;
#227111 = CARTESIAN_POINT ( 'NONE',  ( -20.94999999999999929, -1.835341550224413698, -11.55515129256298223 ) ) ;
#227112 = DIRECTION ( 'NONE',  ( 1.000000000000000000, 0.000000000000000000, 0.000000000000000000 ) ) ;
#227113 = VERTEX_POINT ( 'NONE', #115539 ) ;
#227115 = ORIENTED_EDGE ( 'NONE', *, *, #74173, .F. ) ;
#227114 = CARTESIAN_POINT ( 'NONE',  ( 23.24999999999999289, 38.35559756229049100, -253.3384836876619204 ) ) ;
#227116 = EDGE_CURVE ( 'NONE', #51183, #69524, #154706, .T. ) ;
#227117 = FACE_OUTER_BOUND ( 'NONE', #106126, .T. ) ;
#227118 = AXIS2_PLACEMENT_3D ( 'NONE', #25069, #207544, #28941 ) ;
#227119 = ADVANCED_FACE ( 'NONE', ( #195113, #238051, #112988 ), #93406, .T. ) ;
#227120 = SPHERICAL_SURFACE ( 'NONE', #217730, 0.1000000000000000056 ) ;
#227121 = VECTOR ( 'NONE', #257194, 1000.000000000000000 ) ;
#227122 = AXIS2_PLACEMENT_3D ( 'NONE', #177839, #100795, #21334 ) ;
#227124 = VERTEX_POINT ( 'NONE', #192524 ) ;
#227123 = CARTESIAN_POINT ( 'NONE',  ( 20.95000000000005258, 64.35000000001120668, -30.02310748452479316 ) ) ;
#227125 = B_SPLINE_CURVE_WITH_KNOTS ( 'NONE', 3,
 ( #128345, #188297, #50074, #33132, #209143, #189604, #132186, #149202, #111343, #89195, #53931, #231302, #249578, #90477, #91776, #171362 ),
 .UNSPECIFIED., .F., .F.,
 ( 4, 3, 3, 3, 3, 4 ),
 ( 0.000000000000000000, 3.357088238233650135E-05, 6.714213034887348832E-05, 0.0001007408646120970340, 0.0001343627955914237268, 0.0001573956632895990877 ),
 .UNSPECIFIED. ) ;
#227126 = VERTEX_POINT ( 'NONE', #19002 ) ;
#227127 = FACE_OUTER_BOUND ( 'NONE', #218189, .T. ) ;
#227128 = CIRCLE ( 'NONE', #189558, 0.1000000000000028644 ) ;
#227129 = FACE_OUTER_BOUND ( 'NONE', #74322, .T. ) ;
#227130 = ORIENTED_EDGE ( 'NONE', *, *, #136219, .F. ) ;
#227131 = CARTESIAN_POINT ( 'NONE',  ( 18.59999999999997655, 0.000000000000000000, -33.50000000000000000 ) ) ;
#227132 = EDGE_LOOP ( 'NONE', ( #217972, #106670 ) ) ;
#227133 = TOROIDAL_SURFACE ( 'NONE', #85443, 0.9750000000000019762, 0.1000000000000000056 ) ;
#227134 = ADVANCED_FACE ( 'NONE', ( #234194 ), #55532, .F. ) ;
#227136 = EDGE_CURVE ( 'NONE', #72480, #96293, #143386, .T. ) ;
#227135 = DIRECTION ( 'NONE',  ( -1.000000000000000000, -0.000000000000000000, -0.000000000000000000 ) ) ;
#227137 = DIRECTION ( 'NONE',  ( 1.000000000000000000, 0.000000000000000000, 0.000000000000000000 ) ) ;
#227138 = EDGE_CURVE ( 'NONE', #177565, #143659, #118460, .T. ) ;
#227139 = CIRCLE ( 'NONE', #223044, 0.2000000000000031197 ) ;
#227141 = ORIENTED_EDGE ( 'NONE', *, *, #16442, .F. ) ;
#227140 = CIRCLE ( 'NONE', #243715, 11.80000000000000426 ) ;
#227142 = DIRECTION ( 'NONE',  ( 0.000000000000000000, 0.000000000000000000, 1.000000000000000000 ) ) ;
#227143 = DIRECTION ( 'NONE',  ( 0.000000000000000000, 0.000000000000000000, -1.000000000000000000 ) ) ;
#227144 = EDGE_LOOP ( 'NONE', ( #91915, #7057, #204667, #147314 ) ) ;
#227145 = B_SPLINE_CURVE_WITH_KNOTS ( 'NONE', 3,
 ( #47664, #144199, #142909, #63381, #162523, #127227, #45119 ),
 .UNSPECIFIED., .F., .F.,
 ( 4, 3, 4 ),
 ( 0.000000000000000000, 4.520325912680593053E-05, 5.794988040901352558E-05 ),
 .UNSPECIFIED. ) ;
#227146 = B_SPLINE_CURVE_WITH_KNOTS ( 'NONE', 3,
 ( #82584, #256060, #78752, #219549, #220839, #138702, #39675, #120498, #240418, #119191, #99586, #17503, #181729, #80016, #140005, #102150, #60473, #40960, #61775, #42223, #121773, #201281, #22676, #3064, #162185, #241696 ),
 .UNSPECIFIED., .F., .F.,
 ( 4, 2, 2, 2, 2, 2, 2, 2, 2, 2, 2, 2, 4 ),
 ( 0.005476422646581349113, 0.006160811967703574803, 0.006845201288825800492, 0.007187395949386913771, 0.007529590609948027050, 0.007871785270509140328, 0.008213979931070251872, 0.008556174591631365151, 0.008898369252192478429, 0.009240563912753591708, 0.009582758573314704986, 0.01026714789443687256, 0.01095153721555903840 ),
 .UNSPECIFIED. ) ;
#227147 = CYLINDRICAL_SURFACE ( 'NONE', #31404, 0.1000000000000098310 ) ;
#227148 = EDGE_LOOP ( 'NONE', ( #39629, #33857, #131631, #36220 ) ) ;
#227149 = ORIENTED_EDGE ( 'NONE', *, *, #206958, .F. ) ;
#227150 = CARTESIAN_POINT ( 'NONE',  ( -18.46919391072058403, -9.670724388266654259, -73.67380353179945018 ) ) ;
#227151 = EDGE_CURVE ( 'NONE', #33602, #97347, #155881, .T. ) ;
#227152 = ORIENTED_EDGE ( 'NONE', *, *, #46523, .T. ) ;
#227153 = EDGE_CURVE ( 'NONE', #43410, #134789, #76401, .T. ) ;
#227154 = CARTESIAN_POINT ( 'NONE',  ( -23.15000000000000213, 14.06640494040442135, -210.3712993791105532 ) ) ;
#227155 = ORIENTED_EDGE ( 'NONE', *, *, #77830, .T. ) ;
#227157 = EDGE_LOOP ( 'NONE', ( #204080, #23170, #73193, #40559 ) ) ;
#227156 = CARTESIAN_POINT ( 'NONE',  ( 20.94999999999999929, 71.14953271029261828, -148.5573748935260880 ) ) ;
#227158 = CARTESIAN_POINT ( 'NONE',  ( -21.04999999999999361, 11.75000000001115374, -73.78386566297821503 ) ) ;
#227159 = VERTEX_POINT ( 'NONE', #235481 ) ;
#227160 = DIRECTION ( 'NONE',  ( 0.000000000000000000, -0.9609271840673806464, 0.2768012769485257429 ) ) ;
#227161 = ORIENTED_EDGE ( 'NONE', *, *, #239546, .T. ) ;
#227162 = CIRCLE ( 'NONE', #177130, 0.09999999999998898659 ) ;
#227166 = ADVANCED_FACE ( 'NONE', ( #54277 ), #133821, .T. ) ;
#227165 = VERTEX_POINT ( 'NONE', #77680 ) ;
#227164 = ORIENTED_EDGE ( 'NONE', *, *, #194776, .T. ) ;
#227163 = CARTESIAN_POINT ( 'NONE',  ( -16.93302609847409457, 66.00331747920836278, -56.93671898916184659 ) ) ;
#227167 = DIRECTION ( 'NONE',  ( 1.000000000000000000, 0.000000000000000000, 0.000000000000000000 ) ) ;
#227168 = AXIS2_PLACEMENT_3D ( 'NONE', #163650, #102348, #43699 ) ;
#227169 = DIRECTION ( 'NONE',  ( 0.000000000000000000, 0.000000000000000000, -1.000000000000000000 ) ) ;
#227170 = ORIENTED_EDGE ( 'NONE', *, *, #197750, .T. ) ;
#227171 = AXIS2_PLACEMENT_3D ( 'NONE', #142173, #46906, #5202 ) ;
#227172 = ORIENTED_EDGE ( 'NONE', *, *, #250632, .T. ) ;
#227173 = DIRECTION ( 'NONE',  ( 0.000000000000000000, 0.000000000000000000, -1.000000000000000000 ) ) ;
#227174 = CYLINDRICAL_SURFACE ( 'NONE', #88888, 0.1000000000000028644 ) ;
#227176 = ORIENTED_EDGE ( 'NONE', *, *, #14964, .F. ) ;
#227175 = DIRECTION ( 'NONE',  ( 0.000000000000000000, -0.6728971962617388280, -0.7397360091702248619 ) ) ;
#227177 = CARTESIAN_POINT ( 'NONE',  ( 19.99999999999998934, 11.75000000001115552, -155.3500000000000227 ) ) ;
#227178 = ORIENTED_EDGE ( 'NONE', *, *, #99711, .T. ) ;
#227180 = VECTOR ( 'NONE', #163413, 1000.000000000000227 ) ;
#227179 = CARTESIAN_POINT ( 'NONE',  ( -20.94999999999999929, 76.00000000001190870, -103.0231074845243029 ) ) ;
#227181 = CARTESIAN_POINT ( 'NONE',  ( -20.94999999999999929, 87.65000000001245439, -170.0231074845242745 ) ) ;
#227182 = CIRCLE ( 'NONE', #156312, 0.1000000000000028644 ) ;
#227184 = VERTEX_POINT ( 'NONE', #215908 ) ;
#227183 = EDGE_CURVE ( 'NONE', #148274, #42457, #22793, .T. ) ;
#227185 = CYLINDRICAL_SURFACE ( 'NONE', #190317, 0.5000000000000004441 ) ;
#227186 = DIRECTION ( 'NONE',  ( 0.000000000000000000, 0.000000000000000000, 1.000000000000000000 ) ) ;
#227187 = AXIS2_PLACEMENT_3D ( 'NONE', #111884, #209689, #109283 ) ;
#227188 = ADVANCED_FACE ( 'NONE', ( #37313 ), #213348, .F. ) ;
#227189 = ORIENTED_EDGE ( 'NONE', *, *, #157839, .T. ) ;
#227191 = ORIENTED_EDGE ( 'NONE', *, *, #243430, .T. ) ;
#227190 = DIRECTION ( 'NONE',  ( 0.000000000000000000, 0.9908441862701605762, 0.1350103645451835310 ) ) ;
#227192 = DIRECTION ( 'NONE',  ( 1.000000000000000000, 0.000000000000000000, 0.000000000000000000 ) ) ;
#227193 = EDGE_CURVE ( 'NONE', #128029, #244617, #226771, .T. ) ;
#227195 = ORIENTED_EDGE ( 'NONE', *, *, #55953, .F. ) ;
#227194 = ORIENTED_EDGE ( 'NONE', *, *, #64832, .F. ) ;
#227196 = ORIENTED_EDGE ( 'NONE', *, *, #55615, .F. ) ;
#227198 = EDGE_CURVE ( 'NONE', #5270, #12040, #64277, .T. ) ;
#227197 = FACE_OUTER_BOUND ( 'NONE', #175741, .T. ) ;
#227199 = ORIENTED_EDGE ( 'NONE', *, *, #187125, .F. ) ;
#227200 = DIRECTION ( 'NONE',  ( 0.000000000000000000, 0.000000000000000000, -1.000000000000000000 ) ) ;
#227201 = CIRCLE ( 'NONE', #2328, 0.09999999999999939493 ) ;
#227202 = ORIENTED_EDGE ( 'NONE', *, *, #92749, .T. ) ;
#227203 = CARTESIAN_POINT ( 'NONE',  ( 23.24999999999999289, 80.15000000001194280, -103.0231074845242887 ) ) ;
#227204 = ADVANCED_FACE ( 'NONE', ( #158868 ), #136698, .F. ) ;
#227205 = DIRECTION ( 'NONE',  ( 0.000000000000000000, 0.000000000000000000, -1.000000000000000000 ) ) ;
#227206 = ORIENTED_EDGE ( 'NONE', *, *, #227825, .F. ) ;
#227207 = EDGE_LOOP ( 'NONE', ( #206541, #39172, #202500, #207300 ) ) ;
#227208 = ORIENTED_EDGE ( 'NONE', *, *, #96609, .T. ) ;
#227209 = CIRCLE ( 'NONE', #114794, 7.800000000000001599 ) ;
#227210 = AXIS2_PLACEMENT_3D ( 'NONE', #75584, #19440, #199370 ) ;
#227211 = EDGE_CURVE ( 'NONE', #212622, #210192, #137974, .T. ) ;
#227212 = EDGE_CURVE ( 'NONE', #146046, #171481, #97562, .T. ) ;
#227213 = CARTESIAN_POINT ( 'NONE',  ( -21.14999999999999858, -3.140208063160686791, -228.2318569537739847 ) ) ;
#227214 = ORIENTED_EDGE ( 'NONE', *, *, #171698, .T. ) ;
#227215 = EDGE_CURVE ( 'NONE', #189211, #226915, #37633, .T. ) ;
#227216 = CARTESIAN_POINT ( 'NONE',  ( -23.25000000000000000, -11.74999999998884448, -122.2500000000000284 ) ) ;
#227218 = VERTEX_POINT ( 'NONE', #255320 ) ;
#227217 = DIRECTION ( 'NONE',  ( 0.000000000000000000, -0.8660254037844411501, -0.4999999999999956701 ) ) ;
#227219 = FACE_OUTER_BOUND ( 'NONE', #19846, .T. ) ;
#227220 = DIRECTION ( 'NONE',  ( -0.000000000000000000, 1.000000000000000000, -0.000000000000000000 ) ) ;
#227221 = CARTESIAN_POINT ( 'NONE',  ( -17.05016517655962360, 12.41886358333906948, -211.2650670624473435 ) ) ;
#227222 = FACE_OUTER_BOUND ( 'NONE', #144739, .T. ) ;
#227223 = FACE_OUTER_BOUND ( 'NONE', #104000, .T. ) ;
#227225 = DIRECTION ( 'NONE',  ( 1.000000000000000000, 0.000000000000000000, 0.000000000000000000 ) ) ;
#227224 = CYLINDRICAL_SURFACE ( 'NONE', #202876, 0.09999999999999939493 ) ;
#227226 = DIRECTION ( 'NONE',  ( 1.000000000000000000, 0.000000000000000000, 0.000000000000000000 ) ) ;
#227227 = CARTESIAN_POINT ( 'NONE',  ( 18.36493879433257348, 38.27493291353503935, -261.1939576383761050 ) ) ;
#227228 = CARTESIAN_POINT ( 'NONE',  ( 18.59999999999999432, 68.13014604066189861, -227.7202878558733516 ) ) ;
#227229 = EDGE_CURVE ( 'NONE', #247770, #29779, #39367, .T. ) ;
#227230 = AXIS2_PLACEMENT_3D ( 'NONE', #72061, #211564, #92881 ) ;
#227231 = EDGE_LOOP ( 'NONE', ( #214616, #229374, #229819 ) ) ;
#227232 = EDGE_CURVE ( 'NONE', #118333, #104609, #98828, .T. ) ;
#227233 = ORIENTED_EDGE ( 'NONE', *, *, #118604, .F. ) ;
#227234 = TOROIDAL_SURFACE ( 'NONE', #198007, 11.70000000000000639, 0.1000000000000000056 ) ;
#227236 = VERTEX_POINT ( 'NONE', #115873 ) ;
#227235 = DIRECTION ( 'NONE',  ( 0.000000000000000000, -0.4721928772777366778, -0.8814952561688420563 ) ) ;
#227237 = ORIENTED_EDGE ( 'NONE', *, *, #108866, .F. ) ;
#227238 = DIRECTION ( 'NONE',  ( 0.000000000000000000, 1.000000000000000000, 0.000000000000000000 ) ) ;
#227239 = FACE_OUTER_BOUND ( 'NONE', #175615, .T. ) ;
#227241 = CARTESIAN_POINT ( 'NONE',  ( 21.05000000000000071, 6.257814610476124528, 0.09779029130879343668 ) ) ;
#227240 = FACE_OUTER_BOUND ( 'NONE', #120749, .T. ) ;
#227242 = ADVANCED_FACE ( 'NONE', ( #196672 ), #239249, .F. ) ;
#227243 = ORIENTED_EDGE ( 'NONE', *, *, #157449, .F. ) ;
#227244 = DIRECTION ( 'NONE',  ( 0.000000000000000000, 0.000000000000000000, 1.000000000000000000 ) ) ;
#227245 = LINE ( 'NONE', #128161, #4059 ) ;
#227246 = ORIENTED_EDGE ( 'NONE', *, *, #176592, .F. ) ;
#227248 = DIRECTION ( 'NONE',  ( -0.000000000000000000, 1.000000000000000000, 6.352154140967427193E-15 ) ) ;
#227247 = VECTOR ( 'NONE', #120446, 1000.000000000000000 ) ;
#227249 = AXIS2_PLACEMENT_3D ( 'NONE', #69566, #109949, #242080 ) ;
#227250 = DIRECTION ( 'NONE',  ( 0.000000000000000000, 0.000000000000000000, 1.000000000000000000 ) ) ;
#227251 = CARTESIAN_POINT ( 'NONE',  ( 23.25000000000000000, 64.25000000001199396, -115.1731074845243796 ) ) ;
#227252 = CARTESIAN_POINT ( 'NONE',  ( 21.05000000000000071, 65.57661458509871011, -62.03105556065429482 ) ) ;
#227253 = EDGE_CURVE ( 'NONE', #86736, #121418, #251717, .T. ) ;
#227254 = CARTESIAN_POINT ( 'NONE',  ( -18.60000000000001208, 78.14848145811066615, -231.3763360729035412 ) ) ;
#227256 = ORIENTED_EDGE ( 'NONE', *, *, #89724, .T. ) ;
#227255 = DIRECTION ( 'NONE',  ( 1.000000000000000000, -0.000000000000000000, -0.000000000000000000 ) ) ;
#227257 = LINE ( 'NONE', #108599, #48646 ) ;
#227258 = LINE ( 'NONE', #190742, #56518 ) ;
#227259 = LINE ( 'NONE', #224682, #166815 ) ;
#227260 = LINE ( 'NONE', #69503, #125189 ) ;
#227261 = ORIENTED_EDGE ( 'NONE', *, *, #184746, .F. ) ;
#227262 = CARTESIAN_POINT ( 'NONE',  ( 15.39170923737819763, 66.61047060254509233, -85.20599957163069860 ) ) ;
#227263 = CARTESIAN_POINT ( 'NONE',  ( -18.40000000000000213, 13.76412598303084778, -210.9488531877278206 ) ) ;
#227265 = CARTESIAN_POINT ( 'NONE',  ( -16.98495255085918032, 65.99443563401730728, -123.8884902783038768 ) ) ;
#227264 = DIRECTION ( 'NONE',  ( 0.000000000000000000, 1.000000000000000000, 0.000000000000000000 ) ) ;
#227266 = DIRECTION ( 'NONE',  ( 6.938893903907222067E-15, -1.000000000000000000, -0.000000000000000000 ) ) ;
#227267 = CYLINDRICAL_SURFACE ( 'NONE', #186758, 12.87499999999999822 ) ;
#227268 = AXIS2_PLACEMENT_3D ( 'NONE', #133740, #109036, #9949 ) ;
#227269 = CARTESIAN_POINT ( 'NONE',  ( 20.04142135623730070, 64.35000000001254250, -182.1731074845244507 ) ) ;
#227270 = DIRECTION ( 'NONE',  ( 1.000000000000000000, -0.000000000000000000, -0.000000000000000000 ) ) ;
#227271 = DIRECTION ( 'NONE',  ( 1.000000000000000000, 0.000000000000000000, 0.000000000000000000 ) ) ;
#227272 = CIRCLE ( 'NONE', #48206, 0.09999999999999939493 ) ;
#227273 = CARTESIAN_POINT ( 'NONE',  ( -21.05000000000000071, 74.73821383144657204, -61.43660852097884373 ) ) ;
#227274 = CIRCLE ( 'NONE', #214802, 0.09999999999998708533 ) ;
#227275 = ORIENTED_EDGE ( 'NONE', *, *, #94, .T. ) ;
#227276 = TOROIDAL_SURFACE ( 'NONE', #114857, 11.70000000000000462, 0.1000000000000000056 ) ;
#227277 = ORIENTED_EDGE ( 'NONE', *, *, #206951, .F. ) ;
#227279 = EDGE_LOOP ( 'NONE', ( #178419, #243845, #134758, #792 ) ) ;
#227278 =( GEOMETRIC_REPRESENTATION_CONTEXT ( 3 ) GLOBAL_UNCERTAINTY_ASSIGNED_CONTEXT ( ( #120957 ) ) GLOBAL_UNIT_ASSIGNED_CONTEXT ( ( #180467, #39698, #241720 ) ) REPRESENTATION_CONTEXT ( 'NONE', 'WORKASPACE' ) );
#227280 = EDGE_CURVE ( 'NONE', #41259, #209479, #130912, .T. ) ;
#227281 = CARTESIAN_POINT ( 'NONE',  ( -22.39999999999999858, 1.115600667400684642E-11, -159.7092204016265384 ) ) ;
#227282 = FACE_OUTER_BOUND ( 'NONE', #199529, .T. ) ;
#227283 = ORIENTED_EDGE ( 'NONE', *, *, #152182, .F. ) ;
#227284 = ORIENTED_EDGE ( 'NONE', *, *, #165647, .T. ) ;
#227285 = SURFACE_STYLE_FILL_AREA ( #164756 ) ;
#227286 = EDGE_CURVE ( 'NONE', #60211, #48905, #155022, .T. ) ;
#227287 = ORIENTED_EDGE ( 'NONE', *, *, #138933, .F. ) ;
#227288 = CARTESIAN_POINT ( 'NONE',  ( -20.54999999999999716, 21.35054858842500281, -233.1262234518673893 ) ) ;
#227289 = AXIS2_PLACEMENT_3D ( 'NONE', #230371, #169153, #210813 ) ;
#227290 = VERTEX_POINT ( 'NONE', #139250 ) ;
#227291 =( GEOMETRIC_REPRESENTATION_CONTEXT ( 3 ) GLOBAL_UNCERTAINTY_ASSIGNED_CONTEXT ( ( #66086 ) ) GLOBAL_UNIT_ASSIGNED_CONTEXT ( ( #179460, #84129, #43781 ) ) REPRESENTATION_CONTEXT ( 'NONE', 'WORKASPACE' ) );
#227292 = DIRECTION ( 'NONE',  ( -1.000000000000000000, 0.000000000000000000, 0.000000000000000000 ) ) ;
#227293 = CARTESIAN_POINT ( 'NONE',  ( -16.93415306273742260, 30.28081097614087369, -234.7951876594369764 ) ) ;
#227294 = AXIS2_PLACEMENT_3D ( 'NONE', #14199, #93704, #74183 ) ;
#227295 = DIRECTION ( 'NONE',  ( 0.000000000000000000, 1.000000000000000000, 0.000000000000000000 ) ) ;
#227296 = CARTESIAN_POINT ( 'NONE',  ( -21.10320863425827298, 1.498834514567453757, -230.6884789221961398 ) ) ;
#227297 = CARTESIAN_POINT ( 'NONE',  ( -16.97683809663752186, 29.54312324717475136, -234.4517840742877013 ) ) ;
#227298 = DIRECTION ( 'NONE',  ( 1.000000000000000000, -2.952720810173289112E-16, -2.061873921506763405E-30 ) ) ;
#227300 = VERTEX_POINT ( 'NONE', #197959 ) ;
#227299 = FACE_OUTER_BOUND ( 'NONE', #138626, .T. ) ;
#227302 = DIRECTION ( 'NONE',  ( -1.000000000000000000, 0.000000000000000000, 0.000000000000000000 ) ) ;
#227301 = CARTESIAN_POINT ( 'NONE',  ( 21.05000000000000071, 11.75000000000000355, -26.48519422934606027 ) ) ;
#227303 = DIRECTION ( 'NONE',  ( -0.000000000000000000, 0.9126074666063770380, 0.4088369013363281068 ) ) ;
#227304 = ORIENTED_EDGE ( 'NONE', *, *, #142740, .T. ) ;
#227305 = CARTESIAN_POINT ( 'NONE',  ( 14.87567385445976598, 66.56923500458972853, -121.2925700897739176 ) ) ;
#227306 = AXIS2_PLACEMENT_3D ( 'NONE', #145948, #204633, #126393 ) ;
#227307 = DIRECTION ( 'NONE',  ( 0.000000000000000000, 0.000000000000000000, -1.000000000000000000 ) ) ;
#227308 = CARTESIAN_POINT ( 'NONE',  ( 23.14999999999999503, 35.97645343225767789, -235.9694016464868298 ) ) ;
#227309 = VECTOR ( 'NONE', #49752, 1000.000000000000000 ) ;
#227311 = ORIENTED_EDGE ( 'NONE', *, *, #61107, .T. ) ;
#227310 = AXIS2_PLACEMENT_3D ( 'NONE', #194526, #116262, #78391 ) ;
#227312 = CARTESIAN_POINT ( 'NONE',  ( -18.59999999999999787, 9.150000000011157653, -45.85000000000000142 ) ) ;
#227313 = DIRECTION ( 'NONE',  ( 0.000000000000000000, 1.000000000000000000, 6.982962677686266711E-15 ) ) ;
#227314 = ORIENTED_EDGE ( 'NONE', *, *, #119766, .T. ) ;
#227315 = B_SPLINE_CURVE_WITH_KNOTS ( 'NONE', 3,
 ( #21056, #77141, #254468, #257018, #100526, #195839, #58839, #57565, #238798, #156721 ),
 .UNSPECIFIED., .F., .F.,
 ( 4, 2, 2, 2, 4 ),
 ( 5.201972647453647240E-16, 9.930191194500248098E-05, 0.0001986038238894847617, 0.0003972076477784387523, 0.0007944152955563468961 ),
 .UNSPECIFIED. ) ;
#227316 = TOROIDAL_SURFACE ( 'NONE', #148209, 0.6000000000000009770, 0.1000000000000000056 ) ;
#227317 = LINE ( 'NONE', #52522, #184424 ) ;
#227318 = CARTESIAN_POINT ( 'NONE',  ( -22.94999999999999929, 7.900000000000000355, -1.300000000000000044 ) ) ;
#227319 = AXIS2_PLACEMENT_3D ( 'NONE', #193372, #14746, #233775 ) ;
#227320 = DIRECTION ( 'NONE',  ( 0.000000000000000000, 0.000000000000000000, 1.000000000000000000 ) ) ;
#227321 = DIRECTION ( 'NONE',  ( 0.7071067811865475727, 0.7071067811865475727, 4.937700262164531476E-15 ) ) ;
#227322 = ORIENTED_EDGE ( 'NONE', *, *, #221774, .F. ) ;
#227323 = AXIS2_PLACEMENT_3D ( 'NONE', #101617, #181215, #82062 ) ;
#227324 = AXIS2_PLACEMENT_3D ( 'NONE', #41976, #250, #121522 ) ;
#227325 = ORIENTED_EDGE ( 'NONE', *, *, #107891, .T. ) ;
#227326 = EDGE_CURVE ( 'NONE', #50255, #12967, #195428, .T. ) ;
#227327 = DIRECTION ( 'NONE',  ( 1.000000000000000000, 0.000000000000000000, 0.000000000000000000 ) ) ;
#227328 = CARTESIAN_POINT ( 'NONE',  ( -21.44999999999999929, 65.79629777212066699, -213.4483007241822747 ) ) ;
#227329 = DIRECTION ( 'NONE',  ( 0.000000000000000000, -6.467318590049456648E-15, 1.000000000000000000 ) ) ;
#227330 = DIRECTION ( 'NONE',  ( 1.000000000000000000, 0.000000000000000000, 0.000000000000000000 ) ) ;
#227331 = CARTESIAN_POINT ( 'NONE',  ( 18.39999999999999503, 53.98582189624753624, -228.9137301112145622 ) ) ;
#227332 = DIRECTION ( 'NONE',  ( -0.000000000000000000, 0.9126074666063772600, 0.4088369013363276072 ) ) ;
#227333 = DIRECTION ( 'NONE',  ( 0.000000000000000000, -0.4088369013363281068, 0.9126074666063770380 ) ) ;
#227334 = ORIENTED_EDGE ( 'NONE', *, *, #217958, .F. ) ;
#227335 = DIRECTION ( 'NONE',  ( 1.000000000000000000, -0.000000000000000000, -0.000000000000000000 ) ) ;
#227337 = VERTEX_POINT ( 'NONE', #100121 ) ;
#227336 = DIRECTION ( 'NONE',  ( -1.000000000000000000, 0.000000000000000000, 0.000000000000000000 ) ) ;
#227338 = DIRECTION ( 'NONE',  ( 1.000000000000000000, 0.000000000000000000, -0.000000000000000000 ) ) ;
#227339 = PLANE ( 'NONE',  #190689 ) ;
#227340 = CARTESIAN_POINT ( 'NONE',  ( 20.09999999999999787, 66.25000000001156764, -56.87310748452438958 ) ) ;
#227341 = CYLINDRICAL_SURFACE ( 'NONE', #51413, 0.5000000000000004441 ) ;
#227342 = ADVANCED_FACE ( 'NONE', ( #121031 ), #1011, .T. ) ;
#227344 = VERTEX_POINT ( 'NONE', #239669 ) ;
#227343 = DIRECTION ( 'NONE',  ( 0.000000000000000000, 0.000000000000000000, 1.000000000000000000 ) ) ;
#227345 = DIRECTION ( 'NONE',  ( 0.000000000000000000, 0.2617529984165152257, 0.9651348961777124202 ) ) ;
#227346 = CARTESIAN_POINT ( 'NONE',  ( -18.55807992284872299, 65.67101464000555211, -164.4404391622479977 ) ) ;
#227347 = CARTESIAN_POINT ( 'NONE',  ( -20.94999999999999929, 43.51422117117169108, -240.0698702536254530 ) ) ;
#227348 = EDGE_CURVE ( 'NONE', #140623, #121176, #80555, .T. ) ;
#227349 = EDGE_LOOP ( 'NONE', ( #86840, #242624, #69123, #53968 ) ) ;
#227350 = LINE ( 'NONE', #224772, #59565 ) ;
#227351 = AXIS2_PLACEMENT_3D ( 'NONE', #247660, #113283, #170747 ) ;
#227352 = CARTESIAN_POINT ( 'NONE',  ( -16.77180007708460963, 66.05000000001201954, -115.6587216034791936 ) ) ;
#227353 = VERTEX_POINT ( 'NONE', #78010 ) ;
#227355 = AXIS2_PLACEMENT_3D ( 'NONE', #68102, #112378, #69405 ) ;
#227354 = CARTESIAN_POINT ( 'NONE',  ( 20.94999999999999929, 1.115600667400684642E-11, -200.9999999999999432 ) ) ;
#227356 = CIRCLE ( 'NONE', #239843, 11.80000000000000426 ) ;
#227357 = AXIS2_PLACEMENT_3D ( 'NONE', #235178, #56508, #77365 ) ;
#227358 = CARTESIAN_POINT ( 'NONE',  ( 23.25000000000000355, -22.45632476061176774, -73.79389844773164953 ) ) ;
#227359 = ADVANCED_FACE ( 'NONE', ( #75486 ), #214962, .F. ) ;
#227360 = ORIENTED_EDGE ( 'NONE', *, *, #130813, .F. ) ;
#227361 = CARTESIAN_POINT ( 'NONE',  ( -20.85000000000000142, 80.78317333349157536, -192.9003134612049166 ) ) ;
#227362 = VERTEX_POINT ( 'NONE', #240951 ) ;
#227363 = AXIS2_PLACEMENT_3D ( 'NONE', #225227, #144403, #81852 ) ;
#227364 = DIRECTION ( 'NONE',  ( 1.000000000000000000, -0.000000000000000000, -0.000000000000000000 ) ) ;
#227365 = CARTESIAN_POINT ( 'NONE',  ( -21.44999999999999929, 7.350000000011155166, -79.35000000000005116 ) ) ;
#227366 = DIRECTION ( 'NONE',  ( 0.000000000000000000, 0.000000000000000000, 1.000000000000000000 ) ) ;
#227367 = VERTEX_POINT ( 'NONE', #3608 ) ;
#227368 = EDGE_CURVE ( 'NONE', #256883, #101237, #221356, .T. ) ;
#227369 = CIRCLE ( 'NONE', #106540, 4.000000000000003553 ) ;
#227370 = DIRECTION ( 'NONE',  ( 0.000000000000000000, 0.000000000000000000, -1.000000000000000000 ) ) ;
#227371 = ADVANCED_FACE ( 'NONE', ( #226488 ), #127418, .T. ) ;
#227372 = TOROIDAL_SURFACE ( 'NONE', #60757, 0.2000000000000000111, 0.1000000000000000056 ) ;
#227373 = CARTESIAN_POINT ( 'NONE',  ( 21.05000012384925512, 12.97676112483788735, -210.6372453404386533 ) ) ;
#227374 = CARTESIAN_POINT ( 'NONE',  ( -22.10000000000000497, 6.223900101154157483, 12.09999999999999964 ) ) ;
#227375 = SPHERICAL_SURFACE ( 'NONE', #161192, 0.1000000000000000056 ) ;
#227376 = CARTESIAN_POINT ( 'NONE',  ( 21.14999999999999858, -0.09999999998884338825, -93.95934304829877703 ) ) ;
#227377 = ORIENTED_EDGE ( 'NONE', *, *, #251041, .F. ) ;
#227379 = ORIENTED_EDGE ( 'NONE', *, *, #111327, .F. ) ;
#227378 = DIRECTION ( 'NONE',  ( 1.000000000000000000, -0.000000000000000000, -0.000000000000000000 ) ) ;
#227380 = ORIENTED_EDGE ( 'NONE', *, *, #3641, .T. ) ;
#227381 = CARTESIAN_POINT ( 'NONE',  ( -23.25000000000000000, 69.06610602788553877, -99.23746165015076315 ) ) ;
#227382 = ORIENTED_EDGE ( 'NONE', *, *, #63070, .F. ) ;
#227383 = CYLINDRICAL_SURFACE ( 'NONE', #5045, 0.09999999999999939493 ) ;
#227384 = CARTESIAN_POINT ( 'NONE',  ( 21.05000000000000071, 11.65000000000000391, -0.1000000000000028644 ) ) ;
#227385 = DIRECTION ( 'NONE',  ( 0.000000000000000000, 0.000000000000000000, -1.000000000000000000 ) ) ;
#227387 = ORIENTED_EDGE ( 'NONE', *, *, #223928, .F. ) ;
#227386 = AXIS2_PLACEMENT_3D ( 'NONE', #218837, #100158, #237138 ) ;
#227388 = DIRECTION ( 'NONE',  ( 0.000000000000000000, -0.2617529984165031243, -0.9651348961777157509 ) ) ;
#227389 = CARTESIAN_POINT ( 'NONE',  ( -16.86420534634261514, 66.02938455441979215, -48.60477093528701431 ) ) ;
#227390 = CARTESIAN_POINT ( 'NONE',  ( -20.94999999999999929, 77.83534155023627932, -91.36795619196131213 ) ) ;
#227391 = ORIENTED_EDGE ( 'NONE', *, *, #109360, .F. ) ;
#227392 = ADVANCED_FACE ( 'NONE', ( #161431 ), #60169, .F. ) ;
#227393 = DIRECTION ( 'NONE',  ( -1.000000000000000000, 0.000000000000000000, 0.000000000000000000 ) ) ;
#227395 = ORIENTED_EDGE ( 'NONE', *, *, #215686, .F. ) ;
#227394 = PLANE ( 'NONE',  #188356 ) ;
#227396 = DIRECTION ( 'NONE',  ( 0.000000000000000000, 0.4999999999999956701, -0.8660254037844411501 ) ) ;
#227397 = DIRECTION ( 'NONE',  ( 0.000000000000000000, -0.2617529984165031243, -0.9651348961777157509 ) ) ;
#227398 = VECTOR ( 'NONE', #29738, 1000.000000000000000 ) ;
#227399 = CIRCLE ( 'NONE', #194106, 11.64999999999999325 ) ;
#227400 = EDGE_LOOP ( 'NONE', ( #254383, #186423, #190044, #137055 ) ) ;
#227401 = CARTESIAN_POINT ( 'NONE',  ( -23.25000000000000000, 75.49601185175265528, -250.2710592679604531 ) ) ;
#227403 = EDGE_CURVE ( 'NONE', #29869, #128626, #93483, .T. ) ;
#227402 = CARTESIAN_POINT ( 'NONE',  ( -14.56556274378147720, 66.55344247693948034, -121.4331655301784281 ) ) ;
#227404 = CARTESIAN_POINT ( 'NONE',  ( 21.05000000000000071, 39.26973050389061370, -236.6309188891183055 ) ) ;
#227405 = ORIENTED_EDGE ( 'NONE', *, *, #155753, .F. ) ;
#227406 = DIRECTION ( 'NONE',  ( 0.000000000000000000, -1.000000000000000000, 0.000000000000000000 ) ) ;
#227407 = CARTESIAN_POINT ( 'NONE',  ( -22.59999970745345976, -2.509662979759784029, -189.5206167450800478 ) ) ;
#227408 = EDGE_CURVE ( 'NONE', #218249, #233645, #62310, .T. ) ;
#227409 = ORIENTED_EDGE ( 'NONE', *, *, #129472, .T. ) ;
#227410 = CIRCLE ( 'NONE', #135825, 2.000000000000001776 ) ;
#227411 = EDGE_CURVE ( 'NONE', #226215, #47766, #141322, .T. ) ;
#227412 = VECTOR ( 'NONE', #181440, 1000.000000000000000 ) ;
#227413 = EDGE_CURVE ( 'NONE', #24511, #100761, #114343, .T. ) ;
#227414 = ORIENTED_EDGE ( 'NONE', *, *, #216363, .T. ) ;
#227415 = CARTESIAN_POINT ( 'NONE',  ( -23.39999999999994529, 76.00000000001119815, -36.02310748452479316 ) ) ;
#227416 = VECTOR ( 'NONE', #87863, 1000.000000000000000 ) ;
#227417 = ORIENTED_EDGE ( 'NONE', *, *, #117301, .T. ) ;
#227418 = CARTESIAN_POINT ( 'NONE',  ( -16.97092634996667471, 10.00088896635978308, -188.3698572337024757 ) ) ;
#227419 = CARTESIAN_POINT ( 'NONE',  ( -16.83558968593874994, 66.05000000001255955, -182.6854126721411262 ) ) ;
#227422 = EDGE_CURVE ( 'NONE', #47325, #182399, #1892, .T. ) ;
#227421 = ORIENTED_EDGE ( 'NONE', *, *, #127815, .F. ) ;
#227420 = CARTESIAN_POINT ( 'NONE',  ( 20.85000000000000142, 1.115600667400684642E-11, -67.00000000000000000 ) ) ;
#227423 = CARTESIAN_POINT ( 'NONE',  ( -20.94999999999999929, -10.56629024491939894, -206.4738935375009703 ) ) ;
#227424 = CARTESIAN_POINT ( 'NONE',  ( -16.87683809663752399, 66.05000000001230376, -157.3731074845244393 ) ) ;
#227425 = DIRECTION ( 'NONE',  ( 1.000000000000000000, -0.000000000000000000, 0.000000000000000000 ) ) ;
#227426 = DIRECTION ( 'NONE',  ( 0.000000000000000000, 0.000000000000000000, -1.000000000000000000 ) ) ;
#227427 = CARTESIAN_POINT ( 'NONE',  ( 23.25000000000000000, -11.74999999998883560, -88.75000000000004263 ) ) ;
#227428 = EDGE_CURVE ( 'NONE', #22692, #59070, #122748, .T. ) ;
#227429 = CARTESIAN_POINT ( 'NONE',  ( 18.49999999999999289, 10.20857864376269575, -21.35000000000000142 ) ) ;
#227430 = ADVANCED_FACE ( 'NONE', ( #123568 ), #182266, .F. ) ;
#227431 = CARTESIAN_POINT ( 'NONE',  ( -18.52186455168981993, -9.481018481431380707, -107.5250164779145194 ) ) ;
#227433 = VERTEX_POINT ( 'NONE', #203098 ) ;
#227432 = CARTESIAN_POINT ( 'NONE',  ( 20.94999999999999574, 59.10678033798691189, -225.7992625810339575 ) ) ;
#227434 = VECTOR ( 'NONE', #127814, 1000.000000000000114 ) ;
#227436 = EDGE_CURVE ( 'NONE', #235860, #194536, #31190, .T. ) ;
#227435 = CARTESIAN_POINT ( 'NONE',  ( -23.25000000000000000, 7.128833340093095217, -233.7327013124392749 ) ) ;
#227437 = DIRECTION ( 'NONE',  ( -1.000000000000000000, 0.000000000000000000, 0.000000000000000000 ) ) ;
#227439 = EDGE_CURVE ( 'NONE', #31578, #211434, #168753, .T. ) ;
#227438 = FACE_OUTER_BOUND ( 'NONE', #110353, .T. ) ;
#227440 = CARTESIAN_POINT ( 'NONE',  ( 18.59999999999999787, 43.02787096365918984, -254.3959382439171577 ) ) ;
#227441 = ADVANCED_FACE ( 'NONE', ( #124854 ), #151974, .T. ) ;
#227442 = EDGE_LOOP ( 'NONE', ( #95388, #186496, #157907 ) ) ;
#227443 = CARTESIAN_POINT ( 'NONE',  ( -21.07928932188134041, 1.148907358139439339E-11, -201.0000000000015064 ) ) ;
#227444 = DIRECTION ( 'NONE',  ( 1.441126678808781001E-14, 0.9876197685951252359, 0.1568667991644863424 ) ) ;
#227445 = VECTOR ( 'NONE', #144909, 1000.000000000000000 ) ;
#227446 = EDGE_LOOP ( 'NONE', ( #165152, #210335, #35160, #155835 ) ) ;
#227447 = CIRCLE ( 'NONE', #106633, 1.900000000000012790 ) ;
#227448 = CARTESIAN_POINT ( 'NONE',  ( 21.05000000000000071, 76.10000000001272724, -210.0637644362255969 ) ) ;
#227449 = CARTESIAN_POINT ( 'NONE',  ( -18.45140287520616695, 86.89352149375004331, -199.5971161776188580 ) ) ;
#227450 = ORIENTED_EDGE ( 'NONE', *, *, #193392, .F. ) ;
#227451 = CARTESIAN_POINT ( 'NONE',  ( -21.14999999999999858, 6.540656951712399803, -67.00000000000004263 ) ) ;
#227452 = EDGE_CURVE ( 'NONE', #148820, #191859, #10317, .T. ) ;
#227453 = ORIENTED_EDGE ( 'NONE', *, *, #24882, .F. ) ;
#227454 = EDGE_CURVE ( 'NONE', #150237, #211426, #85272, .T. ) ;
#227455 = DIRECTION ( 'NONE',  ( 0.000000000000000000, 6.505213034913742890E-15, -1.000000000000000000 ) ) ;
#227456 = ORIENTED_EDGE ( 'NONE', *, *, #188039, .T. ) ;
#227457 = DIRECTION ( 'NONE',  ( -0.000000000000000000, -0.000000000000000000, -1.000000000000000000 ) ) ;
#227458 = CARTESIAN_POINT ( 'NONE',  ( 18.39999999999999503, 43.39957528361355799, -233.6562381667159798 ) ) ;
#227459 = ORIENTED_EDGE ( 'NONE', *, *, #25997, .T. ) ;
#227461 = EDGE_CURVE ( 'NONE', #44321, #165812, #102028, .T. ) ;
#227460 = ORIENTED_EDGE ( 'NONE', *, *, #168457, .F. ) ;
#227463 = EDGE_LOOP ( 'NONE', ( #45640, #164019, #193573, #195925, #88100, #252173, #256653 ) ) ;
#227462 = CARTESIAN_POINT ( 'NONE',  ( 12.29592348164039350, 9.355806591641286474, -49.79110253154616572 ) ) ;
#227464 = DIRECTION ( 'NONE',  ( 0.000000000000000000, -0.2128009952263602289, 0.9770955615653315052 ) ) ;
#227466 = ORIENTED_EDGE ( 'NONE', *, *, #181224, .T. ) ;
#227465 = AXIS2_PLACEMENT_3D ( 'NONE', #248349, #51397, #130973 ) ;
#227467 = AXIS2_PLACEMENT_3D ( 'NONE', #112965, #231637, #154683 ) ;
#227468 = ORIENTED_EDGE ( 'NONE', *, *, #33803, .T. ) ;
#227469 = VECTOR ( 'NONE', #245053, 1000.000000000000000 ) ;
#227470 = CARTESIAN_POINT ( 'NONE',  ( -18.40000000000000213, 11.33174054712516110, -12.65000000000000213 ) ) ;
#227471 = DIRECTION ( 'NONE',  ( -0.000000000000000000, -0.2128009952263604232, 0.9770955615653316162 ) ) ;
#227472 = DIRECTION ( 'NONE',  ( -0.000000000000000000, 1.000000000000000000, -0.000000000000000000 ) ) ;
#227473 = CIRCLE ( 'NONE', #181707, 11.74999999999999645 ) ;
#227474 = DIRECTION ( 'NONE',  ( -1.000000000000000000, -2.952720810173289112E-16, 0.000000000000000000 ) ) ;
#227475 = CIRCLE ( 'NONE', #248166, 0.1000000000000028644 ) ;
#227476 = CARTESIAN_POINT ( 'NONE',  ( 21.04999999999999716, 65.37127968600721317, -57.37310748452440379 ) ) ;
#227477 = CARTESIAN_POINT ( 'NONE',  ( 20.94999999999999574, 87.48912529308817909, -133.5231074845242176 ) ) ;
#227479 = ORIENTED_EDGE ( 'NONE', *, *, #109038, .F. ) ;
#227478 = ADVANCED_FACE ( 'NONE', ( #148260 ), #187403, .F. ) ;
#227480 = DIRECTION ( 'NONE',  ( 7.304098846218134667E-16, 1.000000000000000000, 6.982962677686266711E-15 ) ) ;
#227481 = CARTESIAN_POINT ( 'NONE',  ( 23.15000000000000213, 87.65000000001172964, -72.52310748452423184 ) ) ;
#227482 = CARTESIAN_POINT ( 'NONE',  ( 20.73486653747090003, 68.75000000001222134, -149.1731074845244223 ) ) ;
#227483 = DIRECTION ( 'NONE',  ( 1.000000000000000000, 0.000000000000000000, 0.000000000000000000 ) ) ;
#227484 = EDGE_CURVE ( 'NONE', #127120, #255180, #72874, .T. ) ;
#227485 = VERTEX_POINT ( 'NONE', #149570 ) ;
#227486 = CARTESIAN_POINT ( 'NONE',  ( 22.45463910399148233, 1.026727559903907920E-11, -55.35042918981653060 ) ) ;
#227487 = ORIENTED_EDGE ( 'NONE', *, *, #224303, .T. ) ;
#227488 = CARTESIAN_POINT ( 'NONE',  ( 14.77516762759922031, 9.436674251854007878, -115.6768619309992516 ) ) ;
#227489 = ORIENTED_EDGE ( 'NONE', *, *, #134124, .F. ) ;
#227490 = AXIS2_PLACEMENT_3D ( 'NONE', #50163, #172743, #110147 ) ;
#227491 = AXIS2_PLACEMENT_3D ( 'NONE', #93621, #158757, #253961 ) ;
#227492 = CARTESIAN_POINT ( 'NONE',  ( -14.77738660682464378, 24.96400212477831460, -232.5813472152648842 ) ) ;
#227493 = DIRECTION ( 'NONE',  ( 0.000000000000000000, -7.272083257015735086E-15, 1.000000000000000000 ) ) ;
#227494 = EDGE_LOOP ( 'NONE', ( #173063, #252362, #148019, #14652 ) ) ;
#227495 = VERTEX_POINT ( 'NONE', #170445 ) ;
#227498 = ORIENTED_EDGE ( 'NONE', *, *, #174325, .T. ) ;
#227497 = EDGE_CURVE ( 'NONE', #123645, #97414, #22969, .T. ) ;
#227496 = FACE_OUTER_BOUND ( 'NONE', #144842, .T. ) ;
#227499 = DIRECTION ( 'NONE',  ( 3.469446951953646374E-14, -0.7899159663865635839, -0.6132151058540398214 ) ) ;
#227500 = VERTEX_POINT ( 'NONE', #249932 ) ;
#227501 = CIRCLE ( 'NONE', #198291, 0.1000000000000028644 ) ;
#227502 = CARTESIAN_POINT ( 'NONE',  ( -22.46246831459151494, 0.02191216695058596786, -21.85013543879003350 ) ) ;
#227503 = ADVANCED_FACE ( 'NONE', ( #73894 ), #225981, .T. ) ;
#227504 = DIRECTION ( 'NONE',  ( -2.978066053179067751E-16, 1.000000000000000000, 0.000000000000000000 ) ) ;
#227505 = ORIENTED_EDGE ( 'NONE', *, *, #237160, .F. ) ;
#227506 = DIRECTION ( 'NONE',  ( 1.000000000000000000, 0.000000000000000000, 0.000000000000000000 ) ) ;
#227507 = EDGE_CURVE ( 'NONE', #119088, #200872, #64467, .T. ) ;
#227508 = CIRCLE ( 'NONE', #252636, 0.1000000000000055844 ) ;
#227509 = CARTESIAN_POINT ( 'NONE',  ( 20.94999999999999929, 68.03098227380377239, -227.7073825336181869 ) ) ;
#227510 = ORIENTED_EDGE ( 'NONE', *, *, #128612, .T. ) ;
#227511 = ADVANCED_FACE ( 'NONE', ( #51697 ), #43618, .T. ) ;
#227514 = EDGE_CURVE ( 'NONE', #8126, #143848, #11321, .T. ) ;
#227513 = EDGE_CURVE ( 'NONE', #147926, #146255, #252480, .T. ) ;
#227512 = DIRECTION ( 'NONE',  ( -0.000000000000000000, 0.8660254037844502539, 0.4999999999999799050 ) ) ;
#227515 = DIRECTION ( 'NONE',  ( -3.265361837132813093E-16, 1.000000000000000000, 0.000000000000000000 ) ) ;
#227516 = CARTESIAN_POINT ( 'NONE',  ( -18.40000000000000213, 11.47316190337364183, -54.45000000000000284 ) ) ;
#227518 = ORIENTED_EDGE ( 'NONE', *, *, #13962, .T. ) ;
#227517 = CARTESIAN_POINT ( 'NONE',  ( 18.39999999999999503, 5.650000000011139001, -91.25000000000005684 ) ) ;
#227519 = CIRCLE ( 'NONE', #194254, 0.6000000000000015321 ) ;
#227520 = DIRECTION ( 'NONE',  ( 0.000000000000000000, 0.000000000000000000, -1.000000000000000000 ) ) ;
#227521 = CARTESIAN_POINT ( 'NONE',  ( -22.59066674512257933, 12.65021040783261697, -223.3607282225494544 ) ) ;
#227522 = AXIS2_PLACEMENT_3D ( 'NONE', #246095, #44034, #67437 ) ;
#227523 = DIRECTION ( 'NONE',  ( 0.000000000000000000, -0.9908441862701782288, -0.1350103645450542456 ) ) ;
#227525 = CARTESIAN_POINT ( 'NONE',  ( -20.94999999999999929, 87.65000000001144542, -38.92310748452424463 ) ) ;
#227524 = DIRECTION ( 'NONE',  ( 0.000000000000000000, -0.000000000000000000, 1.000000000000000000 ) ) ;
#227527 = AXIS2_PLACEMENT_3D ( 'NONE', #248753, #167956, #250028 ) ;
#227526 = DIRECTION ( 'NONE',  ( -1.000000000000000000, 0.000000000000000000, 0.000000000000000000 ) ) ;
#227528 = AXIS2_PLACEMENT_3D ( 'NONE', #21295, #142481, #4250 ) ;
#227529 = FACE_OUTER_BOUND ( 'NONE', #13867, .T. ) ;
#227530 = CARTESIAN_POINT ( 'NONE',  ( 20.85000000000000142, 64.75617845954087670, -200.4736850529726269 ) ) ;
#227531 = CARTESIAN_POINT ( 'NONE',  ( -20.94999999999999929, 1.115600667400684642E-11, -200.9999999999999432 ) ) ;
#227532 = EDGE_CURVE ( 'NONE', #10427, #72750, #218547, .T. ) ;
#227533 = EDGE_CURVE ( 'NONE', #20990, #253186, #72598, .T. ) ;
#227535 = EDGE_LOOP ( 'NONE', ( #222958, #202678, #98654, #204050 ) ) ;
#227534 = AXIS2_PLACEMENT_3D ( 'NONE', #29043, #219802, #179420 ) ;
#227536 = ORIENTED_EDGE ( 'NONE', *, *, #226057, .F. ) ;
#227537 = EDGE_CURVE ( 'NONE', #201330, #16880, #172843, .T. ) ;
#227538 =( BOUNDED_CURVE ( )  B_SPLINE_CURVE ( 3, ( #253213, #211533, #113709, #97970 ),
 .UNSPECIFIED., .F., .F. ) 
 B_SPLINE_CURVE_WITH_KNOTS ( ( 4, 4 ),
 ( 1.570796326794901443, 3.141592653589853956 ),
 .UNSPECIFIED. ) 
 CURVE ( )  GEOMETRIC_REPRESENTATION_ITEM ( )  RATIONAL_B_SPLINE_CURVE ( ( 1.000000000000000000, 0.8047378541243517258, 0.8047378541243517258, 1.000000000000000000 ) ) 
 REPRESENTATION_ITEM ( '' )  );
#227539 = ORIENTED_EDGE ( 'NONE', *, *, #1364, .F. ) ;
#227540 = CIRCLE ( 'NONE', #115134, 0.2000000000000057288 ) ;
#227541 = ADVANCED_FACE ( 'NONE', ( #30918 ), #32190, .F. ) ;
#227542 = LINE ( 'NONE', #25511, #48603 ) ;
#227543 = AXIS2_PLACEMENT_3D ( 'NONE', #55396, #95820, #254855 ) ;
#227544 = CARTESIAN_POINT ( 'NONE',  ( 18.69999999999999929, 6.726092018229619995, 9.512212474619552438 ) ) ;
#227545 = EDGE_CURVE ( 'NONE', #146292, #169064, #201826, .T. ) ;
#227546 = ORIENTED_EDGE ( 'NONE', *, *, #561, .T. ) ;
#227547 = VECTOR ( 'NONE', #133375, 1000.000000000000000 ) ;
#227548 = CARTESIAN_POINT ( 'NONE',  ( 21.00000000000000000, 22.61918030723622408, -230.9697045991730988 ) ) ;
#227549 = CARTESIAN_POINT ( 'NONE',  ( -18.50000000000000000, 68.97833521811131163, -32.18954208262707795 ) ) ;
#227550 = CARTESIAN_POINT ( 'NONE',  ( -20.54999999999999716, 4.350000000011156054, -112.8500000000000369 ) ) ;
#227551 = VERTEX_POINT ( 'NONE', #213352 ) ;
#227552 = ORIENTED_EDGE ( 'NONE', *, *, #54532, .F. ) ;
#227553 = LINE ( 'NONE', #107606, #46374 ) ;
#227554 = CARTESIAN_POINT ( 'NONE',  ( -21.05000000000000071, 1.750000000011155743, -78.66951155790169992 ) ) ;
#227555 = ORIENTED_EDGE ( 'NONE', *, *, #85742, .T. ) ;
#227556 = TOROIDAL_SURFACE ( 'NONE', #115153, 3.899999999999999467, 0.1000000000000000056 ) ;
#227557 = ADVANCED_FACE ( 'NONE', ( #167854 ), #222655, .T. ) ;
#227558 = CARTESIAN_POINT ( 'NONE',  ( 21.78635804494511419, 0.09900506551883611617, -93.46433851484685817 ) ) ;
#227560 = ORIENTED_EDGE ( 'NONE', *, *, #114921, .F. ) ;
#227559 = LINE ( 'NONE', #232719, #230947 ) ;
#227561 = DIRECTION ( 'NONE',  ( 1.000000000000000000, 0.000000000000000000, 0.000000000000000000 ) ) ;
#227562 = DIRECTION ( 'NONE',  ( 0.000000000000000000, 0.000000000000000000, -1.000000000000000000 ) ) ;
#227564 = ORIENTED_EDGE ( 'NONE', *, *, #23594, .F. ) ;
#227563 = CYLINDRICAL_SURFACE ( 'NONE', #89664, 11.74999999999999645 ) ;
#227565 = CARTESIAN_POINT ( 'NONE',  ( -18.54148534481894472, 10.32532329027886497, -72.56993430183595706 ) ) ;
#227566 = CARTESIAN_POINT ( 'NONE',  ( -23.25000000000000000, 87.65000000001144542, -39.12310748452424747 ) ) ;
#227567 = DIRECTION ( 'NONE',  ( 0.000000000000000000, 0.000000000000000000, 1.000000000000000000 ) ) ;
#227568 = DIRECTION ( 'NONE',  ( -0.000000000000000000, 0.9876197685951241256, 0.1568667991644932258 ) ) ;
#227569 = EDGE_CURVE ( 'NONE', #190290, #65545, #135095, .T. ) ;
#227571 = FACE_OUTER_BOUND ( 'NONE', #101336, .T. ) ;
#227570 = DIRECTION ( 'NONE',  ( 0.000000000000000000, 0.1290532225515392817, 0.9916376685811520986 ) ) ;
#227572 = CARTESIAN_POINT ( 'NONE',  ( -20.07928932188135107, 44.15985985257265867, -236.0871375574735680 ) ) ;
#227573 = CIRCLE ( 'NONE', #189986, 0.09999999999999939493 ) ;
#227574 = AXIS2_PLACEMENT_3D ( 'NONE', #35827, #154509, #14979 ) ;
#227575 = FACE_OUTER_BOUND ( 'NONE', #87400, .T. ) ;
#227576 = AXIS2_PLACEMENT_3D ( 'NONE', #16418, #18950, #95914 ) ;
#227578 = CARTESIAN_POINT ( 'NONE',  ( 20.94999999999999929, 4.813084112160684214, -155.5584822434762202 ) ) ;
#227577 = VECTOR ( 'NONE', #60805, 999.9999999999998863 ) ;
#227579 = VERTEX_POINT ( 'NONE', #155988 ) ;
#227580 = ORIENTED_EDGE ( 'NONE', *, *, #89643, .F. ) ;
#227581 = CARTESIAN_POINT ( 'NONE',  ( 18.59999999999997655, 1.115600667400684642E-11, -141.9000000000000341 ) ) ;
#227582 = EDGE_LOOP ( 'NONE', ( #53351, #252040, #252269, #185019, #1771 ) ) ;
#227583 = DIRECTION ( 'NONE',  ( 0.000000000000000000, 0.1022405907414230264, 0.9947597004326447223 ) ) ;
#227584 = ORIENTED_EDGE ( 'NONE', *, *, #127522, .F. ) ;
#227585 = EDGE_CURVE ( 'NONE', #249408, #206366, #131093, .T. ) ;
#227586 = CARTESIAN_POINT ( 'NONE',  ( -20.54999999999999716, -4.259020970815408091, -226.0869574510824123 ) ) ;
#227587 = CARTESIAN_POINT ( 'NONE',  ( 21.05000000000000071, 70.60000000001180354, -81.92837350343744163 ) ) ;
#227588 = ORIENTED_EDGE ( 'NONE', *, *, #224436, .T. ) ;
#227589 = AXIS2_PLACEMENT_3D ( 'NONE', #90670, #71142, #227616 ) ;
#227590 = DIRECTION ( 'NONE',  ( 0.000000000000000000, 0.4088369013363281623, -0.9126074666063771490 ) ) ;
#227591 = AXIS2_PLACEMENT_3D ( 'NONE', #50563, #110557, #147108 ) ;
#227592 = CIRCLE ( 'NONE', #127656, 0.1999999999999987899 ) ;
#227593 = VERTEX_POINT ( 'NONE', #60693 ) ;
#227594 = ORIENTED_EDGE ( 'NONE', *, *, #141366, .F. ) ;
#227595 = ORIENTED_EDGE ( 'NONE', *, *, #222485, .T. ) ;
#227596 = DIRECTION ( 'NONE',  ( 0.000000000000000000, 0.8660254037844420383, -0.4999999999999943379 ) ) ;
#227597 = CIRCLE ( 'NONE', #248458, 7.720710678118682502 ) ;
#227598 = DIRECTION ( 'NONE',  ( 1.000000000000000000, 0.000000000000000000, 0.000000000000000000 ) ) ;
#227599 = CARTESIAN_POINT ( 'NONE',  ( 19.99999999999998934, 11.75000000001115907, -91.85000000000003695 ) ) ;
#227600 = CARTESIAN_POINT ( 'NONE',  ( -21.05000000000000071, 87.65000000001266756, -200.5231074845242745 ) ) ;
#227602 = CARTESIAN_POINT ( 'NONE',  ( 18.43565242384934422, 85.51932773110506503, -196.5501311079650009 ) ) ;
#227601 = FACE_OUTER_BOUND ( 'NONE', #94658, .T. ) ;
#227603 = CARTESIAN_POINT ( 'NONE',  ( 20.94999999999999574, -11.64999999999999147, -2.900000000000003464 ) ) ;
#227605 = ORIENTED_EDGE ( 'NONE', *, *, #218422, .F. ) ;
#227604 = LINE ( 'NONE', #248465, #206528 ) ;
#227607 = CARTESIAN_POINT ( 'NONE',  ( 20.90000000000000213, 8.000000000000000000, -1.212568896937008089 ) ) ;
#227606 = CARTESIAN_POINT ( 'NONE',  ( 20.41140022480507454, 10.41043084241319683, -74.61500130363459959 ) ) ;
#227608 = LINE ( 'NONE', #202917, #11564 ) ;
#227609 = ORIENTED_EDGE ( 'NONE', *, *, #49358, .F. ) ;
#227610 = CARTESIAN_POINT ( 'NONE',  ( 20.95017935633852346, 10.47548927963648246, -74.57743979739053941 ) ) ;
#227611 = CARTESIAN_POINT ( 'NONE',  ( 22.39999999999999503, 76.00000000001273293, -211.3138870828977360 ) ) ;
#227612 = CARTESIAN_POINT ( 'NONE',  ( 18.59999999999999076, 76.00000000001170974, -69.52310748452431710 ) ) ;
#227613 = ORIENTED_EDGE ( 'NONE', *, *, #12921, .T. ) ;
#227614 = CARTESIAN_POINT ( 'NONE',  ( -16.87372386987899375, 61.13702328834270361, -220.5780305565725996 ) ) ;
#227615 = AXIS2_PLACEMENT_3D ( 'NONE', #78083, #252876, #113377 ) ;
#227616 = DIRECTION ( 'NONE',  ( 0.000000000000000000, 0.9770955615653551529, 0.2128009952262517601 ) ) ;
#227617 = DIRECTION ( 'NONE',  ( 0.000000000000000000, -0.9394191166662628767, -0.3427706569150552052 ) ) ;
#227618 = ORIENTED_EDGE ( 'NONE', *, *, #175401, .F. ) ;
#227619 = EDGE_LOOP ( 'NONE', ( #106846, #186165, #240361, #207657 ) ) ;
#227620 = CARTESIAN_POINT ( 'NONE',  ( 18.59999999999999787, 1.866714910068465239, -78.75267524628205251 ) ) ;
#227621 = CARTESIAN_POINT ( 'NONE',  ( -18.57399277249657032, 10.33112638556969465, -173.0901228926974795 ) ) ;
#227622 = CARTESIAN_POINT ( 'NONE',  ( -16.27683809663751191, 9.350000000011133849, -176.7499999999999432 ) ) ;
#227623 = CARTESIAN_POINT ( 'NONE',  ( -20.93302460841142931, 10.31565961587945424, -206.5364194119177625 ) ) ;
#227624 = EDGE_LOOP ( 'NONE', ( #103930, #75897, #43360, #120091 ) ) ;
#227625 = AXIS2_PLACEMENT_3D ( 'NONE', #53178, #15357, #153618 ) ;
#227626 = CARTESIAN_POINT ( 'NONE',  ( -12.42749937872396337, 9.370689921613768902, -118.0264651266610656 ) ) ;
#227628 = ADVANCED_FACE ( 'NONE', ( #234200 ), #110241, .T. ) ;
#227627 = DIRECTION ( 'NONE',  ( 0.000000000000000000, 0.000000000000000000, 1.000000000000000000 ) ) ;
#227629 = CIRCLE ( 'NONE', #115209, 0.09999999999999939493 ) ;
#227630 = DIRECTION ( 'NONE',  ( 0.000000000000000000, -0.2128009952263604232, 0.9770955615653316162 ) ) ;
#227631 = DIRECTION ( 'NONE',  ( 1.000000000000000000, -1.207181226542539700E-16, 2.694675058168174199E-16 ) ) ;
#227632 = AXIS2_PLACEMENT_3D ( 'NONE', #182667, #4005, #6573 ) ;
#227633 = ORIENTED_EDGE ( 'NONE', *, *, #173156, .T. ) ;
#227634 = DIRECTION ( 'NONE',  ( 0.000000000000000000, 0.000000000000000000, -1.000000000000000000 ) ) ;
#227635 =( BOUNDED_SURFACE ( )  B_SPLINE_SURFACE ( 3, 2, ( 
 ( #149207, #207901, #68370 ),
 ( #171367, #147914, #89200 ),
 ( #87895, #29285, #110052 ),
 ( #245720, #250836, #9670 ) ),
 .UNSPECIFIED., .F., .F., .F. ) 
 B_SPLINE_SURFACE_WITH_KNOTS ( ( 4, 4 ),
 ( 3, 3 ),
 ( 4.712388980384689674, 5.765869716888459173 ),
 ( 0.000000000000000000, 1.000000000000000000 ),
 .UNSPECIFIED. ) 
 GEOMETRIC_REPRESENTATION_ITEM ( )  RATIONAL_B_SPLINE_SURFACE ( (
 ( 1.000000000000000000, 0.7071067811865475727, 1.000000000000000000),
 ( 1.000000000000000000, 0.7953136715913110555, 1.000000000000000000),
 ( 1.000000000000000000, 0.8646876308615464302, 1.000000000000000000),
 ( 1.000000000000000000, 0.8984936768950617658, 1.000000000000000000) ) ) 
 REPRESENTATION_ITEM ( '' )  SURFACE ( )  );
#227636 = AXIS2_PLACEMENT_3D ( 'NONE', #108356, #186617, #5363 ) ;
#227638 = ORIENTED_EDGE ( 'NONE', *, *, #139969, .T. ) ;
#227637 = DIRECTION ( 'NONE',  ( 0.000000000000000000, 0.000000000000000000, -1.000000000000000000 ) ) ;
#227639 = CARTESIAN_POINT ( 'NONE',  ( -16.94445028196807002, 9.992063609708893068, -121.3926698215815918 ) ) ;
#227640 = DIRECTION ( 'NONE',  ( 0.000000000000000000, 0.9126074666063771490, 0.4088369013363281623 ) ) ;
#227641 = DIRECTION ( 'NONE',  ( -0.8049926720990042694, 0.5932847527679310229, 4.142885285818786163E-15 ) ) ;
#227642 = EDGE_CURVE ( 'NONE', #183531, #174107, #176906, .T. ) ;
#227643 = CARTESIAN_POINT ( 'NONE',  ( -18.50000000000000000, 43.08613539620618837, -254.3146655184800409 ) ) ;
#227644 = CYLINDRICAL_SURFACE ( 'NONE', #196276, 0.09999999999999939493 ) ;
#227645 = DIRECTION ( 'NONE',  ( 1.000000000000000000, 0.000000000000000000, 0.000000000000000000 ) ) ;
#227646 = DIRECTION ( 'NONE',  ( -1.000000000000000000, 2.952720810173289112E-16, 2.061873921506763405E-30 ) ) ;
#227647 = EDGE_CURVE ( 'NONE', #206303, #148934, #210223, .T. ) ;
#227648 = ORIENTED_EDGE ( 'NONE', *, *, #120612, .F. ) ;
#227649 = CARTESIAN_POINT ( 'NONE',  ( -23.25000000000000000, 1.115600667400684642E-11, -136.1000000000000227 ) ) ;
#227650 = DIRECTION ( 'NONE',  ( -0.000000000000000000, 0.8660254037844502539, 0.4999999999999799605 ) ) ;
#227651 = DIRECTION ( 'NONE',  ( 0.000000000000000000, 0.000000000000000000, 1.000000000000000000 ) ) ;
#227652 = CARTESIAN_POINT ( 'NONE',  ( 18.50000000000000000, 8.860057415267860392, -245.3237695635339719 ) ) ;
#227653 = DIRECTION ( 'NONE',  ( 0.000000000000000000, 0.000000000000000000, 1.000000000000000000 ) ) ;
#227655 = ADVANCED_FACE ( 'NONE', ( #158555 ), #196365, .F. ) ;
#227654 = VECTOR ( 'NONE', #115088, 1000.000000000000227 ) ;
#227656 = VECTOR ( 'NONE', #177787, 1000.000000000000000 ) ;
#227657 = ORIENTED_EDGE ( 'NONE', *, *, #10570, .F. ) ;
#227658 = ORIENTED_EDGE ( 'NONE', *, *, #240487, .F. ) ;
#227659 = DIRECTION ( 'NONE',  ( 0.000000000000000000, 0.2128009952263602844, -0.9770955615653315052 ) ) ;
#227660 = EDGE_CURVE ( 'NONE', #128128, #55661, #59387, .T. ) ;
#227661 = AXIS2_PLACEMENT_3D ( 'NONE', #134861, #18785, #214417 ) ;
#227662 = CARTESIAN_POINT ( 'NONE',  ( -18.44362607810622023, -9.490496158073668198, -141.0579538668471855 ) ) ;
#227663 = FACE_OUTER_BOUND ( 'NONE', #180102, .T. ) ;
#227664 = EDGE_CURVE ( 'NONE', #192351, #254124, #6181, .T. ) ;
#227665 = CARTESIAN_POINT ( 'NONE',  ( -21.44999999999999929, 7.350000000011155166, -188.6499999999999488 ) ) ;
#227666 = AXIS2_PLACEMENT_3D ( 'NONE', #45264, #167809, #169103 ) ;
#227667 = EDGE_CURVE ( 'NONE', #196105, #107215, #68742, .T. ) ;
#227668 = CIRCLE ( 'NONE', #127741, 0.1000000000000028644 ) ;
#227669 = CARTESIAN_POINT ( 'NONE',  ( -20.54999999999999716, 4.350000000011156054, -155.1500000000000057 ) ) ;
#227670 = CARTESIAN_POINT ( 'NONE',  ( 23.24999999999999645, 78.10000000001141984, -36.02310748452431000 ) ) ;
#227671 = EDGE_CURVE ( 'NONE', #248044, #125649, #57239, .T. ) ;
#227672 = PLANE ( 'NONE',  #195391 ) ;
#227673 = ADVANCED_FACE ( 'NONE', ( #217198 ), #257566, .T. ) ;
#227674 = VERTEX_POINT ( 'NONE', #19011 ) ;
#227675 = DIRECTION ( 'NONE',  ( 1.000000000000000000, 3.448943450116723568E-16, 6.438528483529607644E-16 ) ) ;
#227676 = ORIENTED_EDGE ( 'NONE', *, *, #175827, .T. ) ;
#227677 = FACE_OUTER_BOUND ( 'NONE', #66924, .T. ) ;
#227679 = EDGE_CURVE ( 'NONE', #171936, #140343, #139455, .T. ) ;
#227678 = DIRECTION ( 'NONE',  ( 1.000000000000000000, 0.000000000000000000, 0.000000000000000000 ) ) ;
#227680 = DIRECTION ( 'NONE',  ( -0.000000000000000000, 0.2617529984165031243, 0.9651348961777157509 ) ) ;
#227681 = CARTESIAN_POINT ( 'NONE',  ( -22.49806830649814415, 11.64988965483908068, 0.07746431632550303259 ) ) ;
#227682 = CARTESIAN_POINT ( 'NONE',  ( 23.14999999999999503, 11.65000000001116298, -93.48519422934610645 ) ) ;
#227683 = DIRECTION ( 'NONE',  ( 0.000000000000000000, 0.9908441862701600211, -0.1350103645451876666 ) ) ;
#227684 = DIRECTION ( 'NONE',  ( 1.000000000000000000, 0.000000000000000000, 0.000000000000000000 ) ) ;
#227685 = ORIENTED_EDGE ( 'NONE', *, *, #161602, .F. ) ;
#227686 = EDGE_CURVE ( 'NONE', #90665, #126512, #93683, .T. ) ;
#227687 = DIRECTION ( 'NONE',  ( 0.000000000000000000, 0.9126074666063751506, 0.4088369013363318816 ) ) ;
#227688 = DIRECTION ( 'NONE',  ( 0.000000000000000000, 0.000000000000000000, -1.000000000000000000 ) ) ;
#227689 = DIRECTION ( 'NONE',  ( 0.7071067811865474617, 0.6909108974501236844, 0.1504730267678055788 ) ) ;
#227690 = AXIS2_PLACEMENT_3D ( 'NONE', #167292, #249381, #169880 ) ;
#227691 = CARTESIAN_POINT ( 'NONE',  ( 20.94999999999999574, -11.64999999998883595, -137.0000000000000000 ) ) ;
#227692 = CARTESIAN_POINT ( 'NONE',  ( -22.59999999999999787, 11.74956712350054566, -167.3991416309012550 ) ) ;
#227693 = EDGE_LOOP ( 'NONE', ( #23876, #136257, #45009, #68140 ) ) ;
#227694 = CARTESIAN_POINT ( 'NONE',  ( 18.47688499308725341, 85.46485595029625415, -129.8217597313868623 ) ) ;
#227696 = EDGE_CURVE ( 'NONE', #200406, #51015, #160352, .T. ) ;
#227695 = DIRECTION ( 'NONE',  ( -1.000000000000000000, 0.000000000000000000, 0.000000000000000000 ) ) ;
#227697 = EDGE_LOOP ( 'NONE', ( #230570, #168215, #62682, #36929 ) ) ;
#227698 = ORIENTED_EDGE ( 'NONE', *, *, #154407, .T. ) ;
#227699 = CARTESIAN_POINT ( 'NONE',  ( -16.97683809663752186, 61.23280479334029991, -220.3417702668378126 ) ) ;
#227700 = CIRCLE ( 'NONE', #2852, 1.899999999999996136 ) ;
#227701 = CARTESIAN_POINT ( 'NONE',  ( 23.14999999999999858, 4.775700934590591196, -55.15123189595403375 ) ) ;
#227702 = ORIENTED_EDGE ( 'NONE', *, *, #118833, .F. ) ;
#227704 = AXIS2_PLACEMENT_3D ( 'NONE', #64345, #86434, #225944 ) ;
#227703 = CARTESIAN_POINT ( 'NONE',  ( 21.05000000000000071, 64.25000000001146816, -43.03791325517834565 ) ) ;
#227705 = DIRECTION ( 'NONE',  ( 1.000000000000000000, 0.000000000000000000, 0.000000000000000000 ) ) ;
#227706 = AXIS2_PLACEMENT_3D ( 'NONE', #248777, #190080, #209640 ) ;
#227707 = EDGE_LOOP ( 'NONE', ( #65947, #197046, #249909, #196658 ) ) ;
#227708 = AXIS2_PLACEMENT_3D ( 'NONE', #48249, #187780, #62690 ) ;
#227709 = EDGE_CURVE ( 'NONE', #105564, #134169, #127001, .T. ) ;
#227710 = CARTESIAN_POINT ( 'NONE',  ( 18.47149038651510367, -9.671457157995551057, -174.1727863347384471 ) ) ;
#227711 = ORIENTED_EDGE ( 'NONE', *, *, #147414, .F. ) ;
#227712 = DIRECTION ( 'NONE',  ( 0.000000000000000000, -6.938893903907222067E-15, 1.000000000000000000 ) ) ;
#227713 = FACE_OUTER_BOUND ( 'NONE', #214341, .T. ) ;
#227717 = EDGE_CURVE ( 'NONE', #115921, #105026, #181187, .T. ) ;
#227716 = EDGE_LOOP ( 'NONE', ( #142720, #8553, #244103, #50842 ) ) ;
#227715 = VECTOR ( 'NONE', #225950, 1000.000000000000000 ) ;
#227714 = DIRECTION ( 'NONE',  ( 0.7071067811865463515, 0.7071067811865487940, 7.587431340288849180E-16 ) ) ;
#227718 = DIRECTION ( 'NONE',  ( 1.000000000000000000, 0.000000000000000000, 0.000000000000000000 ) ) ;
#227720 = UNCERTAINTY_MEASURE_WITH_UNIT (LENGTH_MEASURE( 1.000000000000000082E-05 ), #7090, 'distance_accuracy_value', 'NONE');
#227719 = CARTESIAN_POINT ( 'NONE',  ( -23.39999999999994529, 77.84910827723388138, -47.62873275725970501 ) ) ;
#227721 = DIRECTION ( 'NONE',  ( 0.000000000000000000, -0.2558827019433787542, 0.9667078373770204847 ) ) ;
#227722 = CIRCLE ( 'NONE', #240232, 0.09999999999998898659 ) ;
#227723 = DIRECTION ( 'NONE',  ( -0.000000000000000000, 1.000000000000000000, 6.982962677686267499E-15 ) ) ;
#227724 = DIRECTION ( 'NONE',  ( 1.000000000000000000, 0.000000000000000000, 0.000000000000000000 ) ) ;
#227725 = AXIS2_PLACEMENT_3D ( 'NONE', #35291, #172237, #90066 ) ;
#227726 = EDGE_CURVE ( 'NONE', #5518, #51370, #241904, .T. ) ;
#227727 = DIRECTION ( 'NONE',  ( 0.000000000000000000, 0.000000000000000000, -1.000000000000000000 ) ) ;
#227728 = CARTESIAN_POINT ( 'NONE',  ( -23.15000000000000213, 76.00000000001213607, -136.5231074845242745 ) ) ;
#227729 = EDGE_CURVE ( 'NONE', #190086, #169179, #106301, .T. ) ;
#227731 = ORIENTED_EDGE ( 'NONE', *, *, #46379, .T. ) ;
#227730 = CARTESIAN_POINT ( 'NONE',  ( 18.52326479938715309, 87.06379029406096492, -199.5663785907607348 ) ) ;
#227732 = ORIENTED_EDGE ( 'NONE', *, *, #150642, .F. ) ;
#227734 = DIRECTION ( 'NONE',  ( 0.000000000000000000, 0.000000000000000000, -1.000000000000000000 ) ) ;
#227733 = FACE_OUTER_BOUND ( 'NONE', #41839, .T. ) ;
#227736 = EDGE_LOOP ( 'NONE', ( #208534, #215544, #96109, #202593, #117908, #233518 ) ) ;
#227735 = LINE ( 'NONE', #209460, #43354 ) ;
#227737 = EDGE_CURVE ( 'NONE', #219709, #239082, #106233, .T. ) ;
#227738 = ORIENTED_EDGE ( 'NONE', *, *, #225689, .F. ) ;
#227739 = DIRECTION ( 'NONE',  ( -1.000000000000000000, 0.000000000000000000, 0.000000000000000000 ) ) ;
#227740 = ADVANCED_FACE ( 'NONE', ( #200226 ), #166268, .F. ) ;
#227741 = CARTESIAN_POINT ( 'NONE',  ( 21.03675099975491136, 67.12481996722705446, -90.69756534774630552 ) ) ;
#227742 = CIRCLE ( 'NONE', #36238, 12.77499999999999503 ) ;
#227744 = ADVANCED_FACE ( 'NONE', ( #3282 ), #164947, .F. ) ;
#227743 = DIRECTION ( 'NONE',  ( 1.000000000000000000, 0.000000000000000000, 0.000000000000000000 ) ) ;
#227745 = DIRECTION ( 'NONE',  ( 0.000000000000000000, -7.272083257015735086E-15, 1.000000000000000000 ) ) ;
#227746 = LINE ( 'NONE', #149525, #217892 ) ;
#227747 = LINE ( 'NONE', #129921, #77967 ) ;
#227748 = DIRECTION ( 'NONE',  ( 1.000000000000000000, 0.000000000000000000, 0.000000000000000000 ) ) ;
#227749 = EDGE_LOOP ( 'NONE', ( #86574, #37898, #14062, #29401 ) ) ;
#227750 = ORIENTED_EDGE ( 'NONE', *, *, #45535, .F. ) ;
#227751 = CARTESIAN_POINT ( 'NONE',  ( 23.14999999999999503, 15.90518444080776739, -219.2841490888777116 ) ) ;
#227752 = AXIS2_PLACEMENT_3D ( 'NONE', #190779, #151650, #231181 ) ;
#227753 = VECTOR ( 'NONE', #99601, 1000.000000000000000 ) ;
#227754 = EDGE_LOOP ( 'NONE', ( #223516, #228237, #12467, #150623 ) ) ;
#227755 = CIRCLE ( 'NONE', #136151, 0.09999999999998898659 ) ;
#227757 = DIRECTION ( 'NONE',  ( 0.000000000000000000, 0.2128009952263623661, -0.9770955615653309501 ) ) ;
#227756 = AXIS2_PLACEMENT_3D ( 'NONE', #249732, #210602, #211906 ) ;
#227758 = EDGE_LOOP ( 'NONE', ( #191780, #194014, #244884, #250408 ) ) ;
#227759 = CARTESIAN_POINT ( 'NONE',  ( -16.85939681242906474, 9.905225185936462395, -154.5399219551915451 ) ) ;
#227760 = ADVANCED_FACE ( 'NONE', ( #161110 ), #243189, .T. ) ;
#227761 = DIRECTION ( 'NONE',  ( 0.000000000000000000, 0.000000000000000000, -1.000000000000000000 ) ) ;
#227762 = DIRECTION ( 'NONE',  ( 1.734723475976817507E-14, -0.9770955615653316162, -0.2128009952263604232 ) ) ;
#227763 = ADVANCED_FACE ( 'NONE', ( #24170 ), #144078, .F. ) ;
#227764 = CARTESIAN_POINT ( 'NONE',  ( -23.25000000000000000, 76.00000000001195133, -103.0231074845243171 ) ) ;
#227765 = VERTEX_POINT ( 'NONE', #240632 ) ;
#227766 = EDGE_CURVE ( 'NONE', #178700, #110389, #63746, .T. ) ;
#227767 = DIRECTION ( 'NONE',  ( 1.000000000000000000, 0.000000000000000000, 0.000000000000000000 ) ) ;
#227768 = VERTEX_POINT ( 'NONE', #249636 ) ;
#227769 = CARTESIAN_POINT ( 'NONE',  ( 20.94999999999999929, 5.400000000011154988, -146.4052660189131245 ) ) ;
#227770 = CARTESIAN_POINT ( 'NONE',  ( -16.87331047859649757, 9.950000000011138823, -87.85000000000005116 ) ) ;
#227771 = CARTESIAN_POINT ( 'NONE',  ( 18.41789779300687258, 8.841737057899697660, -245.4273994550192697 ) ) ;
#227772 = VECTOR ( 'NONE', #121526, 1000.000000000000000 ) ;
#227773 = ORIENTED_EDGE ( 'NONE', *, *, #109130, .F. ) ;
#227774 = VECTOR ( 'NONE', #244294, 1000.000000000000114 ) ;
#227776 = DIRECTION ( 'NONE',  ( 2.952720810173289112E-16, 1.000000000000000000, 6.982962677686266711E-15 ) ) ;
#227775 = AXIS2_PLACEMENT_3D ( 'NONE', #249480, #27887, #147809 ) ;
#227777 = ORIENTED_EDGE ( 'NONE', *, *, #195029, .F. ) ;
#227780 = ORIENTED_EDGE ( 'NONE', *, *, #67402, .T. ) ;
#227779 = CARTESIAN_POINT ( 'NONE',  ( 18.52643265882457868, 46.42459709376392851, -243.0752906381742662 ) ) ;
#227778 = CARTESIAN_POINT ( 'NONE',  ( -16.87036670365549895, 9.989418819301647545, -12.52043988269794639 ) ) ;
#227781 = CARTESIAN_POINT ( 'NONE',  ( 21.05000000000000071, 1.115600667400684642E-11, -100.5000000000000284 ) ) ;
#227782 = ORIENTED_EDGE ( 'NONE', *, *, #165739, .T. ) ;
#227783 = CARTESIAN_POINT ( 'NONE',  ( -21.14999999999999858, 11.75000000001115552, -174.2261306360591675 ) ) ;
#227784 = CIRCLE ( 'NONE', #198560, 0.09999999999999820144 ) ;
#227785 = ORIENTED_EDGE ( 'NONE', *, *, #49668, .F. ) ;
#227786 = DIRECTION ( 'NONE',  ( 1.000000000000000000, 0.000000000000000000, 0.000000000000000000 ) ) ;
#227787 = DIRECTION ( 'NONE',  ( -0.000000000000000000, -0.000000000000000000, -1.000000000000000000 ) ) ;
#227788 = DIRECTION ( 'NONE',  ( 1.000000000000000000, 0.000000000000000000, 0.000000000000000000 ) ) ;
#227789 = CARTESIAN_POINT ( 'NONE',  ( -16.90202395485801290, 66.03405545546117139, -123.9261212057851083 ) ) ;
#227790 = EDGE_CURVE ( 'NONE', #189583, #975, #226163, .T. ) ;
#227791 = ORIENTED_EDGE ( 'NONE', *, *, #226057, .T. ) ;
#227792 = CARTESIAN_POINT ( 'NONE',  ( -16.93255653858138388, 44.05329019094499898, -235.2826611615568595 ) ) ;
#227793 = DIRECTION ( 'NONE',  ( 1.000000000000000000, 0.000000000000000000, 0.000000000000000000 ) ) ;
#227794 = DIRECTION ( 'NONE',  ( 0.000000000000000000, -0.4721928772777346239, -0.8814952561688430555 ) ) ;
#227795 = CIRCLE ( 'NONE', #177936, 0.1000000000000013933 ) ;
#227796 = ORIENTED_EDGE ( 'NONE', *, *, #152958, .T. ) ;
#227797 = DIRECTION ( 'NONE',  ( 1.000000000000000000, 0.000000000000000000, 0.000000000000000000 ) ) ;
#227798 = VERTEX_POINT ( 'NONE', #29331 ) ;
#227799 = CARTESIAN_POINT ( 'NONE',  ( -22.50000000000000000, 0.1000000000111554016, -21.85042919245520210 ) ) ;
#227800 = VERTEX_POINT ( 'NONE', #30597 ) ;
#227801 = DIRECTION ( 'NONE',  ( 0.000000000000000000, 0.8814952561688629284, -0.4721928772776973204 ) ) ;
#227802 = LINE ( 'NONE', #226500, #164568 ) ;
#227804 = ORIENTED_EDGE ( 'NONE', *, *, #17207, .F. ) ;
#227803 = CARTESIAN_POINT ( 'NONE',  ( -23.39999999999994529, 74.26359666348515987, -47.54092689884382850 ) ) ;
#227805 = DIRECTION ( 'NONE',  ( -0.000000000000000000, 1.000000000000000000, 6.982962677686266711E-15 ) ) ;
#227806 = CIRCLE ( 'NONE', #227625, 0.2000000000000048683 ) ;
#227807 = CARTESIAN_POINT ( 'NONE',  ( -14.22969084473441015, 62.94440715787349916, -215.5359628679901789 ) ) ;
#227808 = ADVANCED_FACE ( 'NONE', ( #206644 ), #218743, .F. ) ;
#227809 = CARTESIAN_POINT ( 'NONE',  ( -21.10000000000000142, -11.65000000000000036, 12.09999999999999609 ) ) ;
#227810 = ORIENTED_EDGE ( 'NONE', *, *, #58933, .T. ) ;
#227811 = VECTOR ( 'NONE', #252075, 1000.000000000000000 ) ;
#227812 = CARTESIAN_POINT ( 'NONE',  ( -18.59999999999999787, 11.65000000001115232, -54.85000000000000142 ) ) ;
#227814 = ADVANCED_FACE ( 'NONE', ( #110104 ), #8451, .F. ) ;
#227813 = CYLINDRICAL_SURFACE ( 'NONE', #231848, 0.1000000000000000472 ) ;
#227815 = VERTEX_POINT ( 'NONE', #170131 ) ;
#227816 = CARTESIAN_POINT ( 'NONE',  ( -16.93906926870270624, 10.01214687095770906, -146.5534523072268485 ) ) ;
#227817 = VECTOR ( 'NONE', #179659, 1000.000000000000000 ) ;
#227818 = AXIS2_PLACEMENT_3D ( 'NONE', #114670, #48585, #86401 ) ;
#227819 = ORIENTED_EDGE ( 'NONE', *, *, #96691, .T. ) ;
#227820 = DIRECTION ( 'NONE',  ( 1.000000000000000000, 0.000000000000000000, 0.000000000000000000 ) ) ;
#227821 = EDGE_CURVE ( 'NONE', #172403, #196915, #93863, .T. ) ;
#227822 = CARTESIAN_POINT ( 'NONE',  ( -16.81930730667009044, 44.21085617933544398, -235.2794117849574320 ) ) ;
#227825 = EDGE_CURVE ( 'NONE', #158664, #16270, #28037, .T. ) ;
#227824 = CARTESIAN_POINT ( 'NONE',  ( -18.59999999999999787, 7.250000000011155521, -121.8500000000000369 ) ) ;
#227823 = VECTOR ( 'NONE', #105310, 1000.000000000000000 ) ;
#227826 = TOROIDAL_SURFACE ( 'NONE', #223538, 4.900000000000000355, 0.1000000000000000056 ) ;
#227829 = ORIENTED_EDGE ( 'NONE', *, *, #90933, .F. ) ;
#227828 = ORIENTED_EDGE ( 'NONE', *, *, #94254, .F. ) ;
#227827 = FACE_OUTER_BOUND ( 'NONE', #52004, .T. ) ;
#227830 = DIRECTION ( 'NONE',  ( 0.000000000000000000, 2.664535259100339804E-15, -1.000000000000000000 ) ) ;
#227831 = DIRECTION ( 'NONE',  ( 1.186688945009009831E-16, -0.4721928772777346239, -0.8814952561688430555 ) ) ;
#227832 = DIRECTION ( 'NONE',  ( 1.000000000000000000, 0.000000000000000000, 0.000000000000000000 ) ) ;
#227834 = PLANE ( 'NONE',  #225180 ) ;
#227833 = FACE_OUTER_BOUND ( 'NONE', #47612, .T. ) ;
#227835 = DIRECTION ( 'NONE',  ( 0.7071067811865463515, -0.2890913453342142114, 0.6453109281988457235 ) ) ;
#227836 = CARTESIAN_POINT ( 'NONE',  ( -18.39999999999999858, -9.500000000000005329, -40.10018939122204529 ) ) ;
#227837 = AXIS2_PLACEMENT_3D ( 'NONE', #245313, #207480, #107067 ) ;
#227838 = CARTESIAN_POINT ( 'NONE',  ( 20.90000000000000213, 11.49641995933507843, -1.885425182446133885 ) ) ;
#227839 = CARTESIAN_POINT ( 'NONE',  ( 18.59999999999999076, 6.550000000000000711, -21.25000000000000000 ) ) ;
#227840 = ADVANCED_FACE ( 'NONE', ( #47544 ), #162831, .F. ) ;
#227842 = EDGE_CURVE ( 'NONE', #190980, #43551, #48068, .T. ) ;
#227841 = AXIS2_PLACEMENT_3D ( 'NONE', #36046, #173024, #137675 ) ;
#227843 = ORIENTED_EDGE ( 'NONE', *, *, #93179, .F. ) ;
#227844 = ORIENTED_EDGE ( 'NONE', *, *, #48872, .T. ) ;
#227846 = CARTESIAN_POINT ( 'NONE',  ( 18.49999999999999645, 76.00000000001237765, -170.0231074845243597 ) ) ;
#227845 = AXIS2_PLACEMENT_3D ( 'NONE', #176313, #173777, #137158 ) ;
#227848 = ORIENTED_EDGE ( 'NONE', *, *, #26493, .T. ) ;
#227847 = CYLINDRICAL_SURFACE ( 'NONE', #53756, 1.749999999999998002 ) ;
#227849 = AXIS2_PLACEMENT_3D ( 'NONE', #94320, #13521, #117744 ) ;
#227850 = VERTEX_POINT ( 'NONE', #171411 ) ;
#227851 = DIRECTION ( 'NONE',  ( -1.000000000000000000, -0.000000000000000000, -0.000000000000000000 ) ) ;
#227852 = EDGE_LOOP ( 'NONE', ( #115597, #104688, #147273, #64991 ) ) ;
#227853 = DIRECTION ( 'NONE',  ( 0.000000000000000000, 0.000000000000000000, -1.000000000000000000 ) ) ;
#227854 = AXIS2_PLACEMENT_3D ( 'NONE', #61336, #224246, #5177 ) ;
#227855 = AXIS2_PLACEMENT_3D ( 'NONE', #12078, #248087, #131997 ) ;
#227856 = EDGE_CURVE ( 'NONE', #180521, #116815, #127179, .T. ) ;
#227857 = ORIENTED_EDGE ( 'NONE', *, *, #132173, .F. ) ;
#227858 = CARTESIAN_POINT ( 'NONE',  ( -16.88593481969334320, 66.04943990992792635, -149.1712352275798992 ) ) ;
#227859 = CARTESIAN_POINT ( 'NONE',  ( 20.94999999999999574, -1.835341550213255957, -78.55515129256303908 ) ) ;
#227860 = ADVANCED_FACE ( 'NONE', ( #72283 ), #174288, .T. ) ;
#227863 = VERTEX_POINT ( 'NONE', #236475 ) ;
#227862 = ORIENTED_EDGE ( 'NONE', *, *, #65537, .T. ) ;
#227861 = VECTOR ( 'NONE', #163122, 1000.000000000000114 ) ;
#227864 = ORIENTED_EDGE ( 'NONE', *, *, #157850, .T. ) ;
#227865 = CYLINDRICAL_SURFACE ( 'NONE', #144616, 0.1000000000000028644 ) ;
#227866 = AXIS2_PLACEMENT_3D ( 'NONE', #164136, #29786, #166724 ) ;
#227868 = ORIENTED_EDGE ( 'NONE', *, *, #119837, .F. ) ;
#227867 = B_SPLINE_CURVE_WITH_KNOTS ( 'NONE', 3,
 ( #220904, #137512, #97081, #117971 ),
 .UNSPECIFIED., .F., .F.,
 ( 4, 4 ),
 ( 0.000000000000000000, 0.0002118541922231684618 ),
 .UNSPECIFIED. ) ;
#227869 = ORIENTED_EDGE ( 'NONE', *, *, #207576, .F. ) ;
#227870 = DIRECTION ( 'NONE',  ( 0.000000000000000000, -0.8700118002898359348, 0.4930308989875165082 ) ) ;
#227871 = DIRECTION ( 'NONE',  ( 1.000000000000000000, 0.000000000000000000, 0.000000000000000000 ) ) ;
#227872 = CARTESIAN_POINT ( 'NONE',  ( -15.51798037960204546, 9.376659938544687378, -185.1281925482172710 ) ) ;
#227874 = VERTEX_POINT ( 'NONE', #78671 ) ;
#227873 = CARTESIAN_POINT ( 'NONE',  ( -21.04999999999999716, 85.60000000001232934, -162.9910380878246201 ) ) ;
#227875 = DIRECTION ( 'NONE',  ( 0.000000000000000000, 0.4999999999999478195, 0.8660254037844686836 ) ) ;
#227876 = EDGE_CURVE ( 'NONE', #166946, #198535, #202197, .T. ) ;
#227877 = FACE_OUTER_BOUND ( 'NONE', #216590, .T. ) ;
#227879 = EDGE_LOOP ( 'NONE', ( #249195, #72483, #98356, #80394 ) ) ;
#227878 = DIRECTION ( 'NONE',  ( 0.000000000000000000, 1.000000000000000000, 0.000000000000000000 ) ) ;
#227880 = DIRECTION ( 'NONE',  ( 1.000000000000000000, 0.000000000000000000, 0.000000000000000000 ) ) ;
#227881 = VERTEX_POINT ( 'NONE', #216904 ) ;
#227882 = CARTESIAN_POINT ( 'NONE',  ( -20.94999999999999929, 68.97833521811203639, -132.8895420826271163 ) ) ;
#227883 = VERTEX_POINT ( 'NONE', #420 ) ;
#227884 = CIRCLE ( 'NONE', #19803, 0.6000000000000033085 ) ;
#227885 = CARTESIAN_POINT ( 'NONE',  ( 21.53551880898956838, 69.21520223859606347, -170.1220772190960702 ) ) ;
#227886 = CARTESIAN_POINT ( 'NONE',  ( -16.90202395485949793, 30.26058880429625830, -234.8180226659985408 ) ) ;
#227888 = EDGE_CURVE ( 'NONE', #10139, #5552, #31108, .T. ) ;
#227887 = ORIENTED_EDGE ( 'NONE', *, *, #252813, .T. ) ;
#227890 = DIRECTION ( 'NONE',  ( 1.000000000000000000, 0.000000000000000000, 0.000000000000000000 ) ) ;
#227889 = CARTESIAN_POINT ( 'NONE',  ( -22.00356870071802007, 75.99999999998983924, -210.7773498462519797 ) ) ;
#227891 = DIRECTION ( 'NONE',  ( -1.000000000000000000, 0.000000000000000000, 0.000000000000000000 ) ) ;
#227892 = PLANE ( 'NONE',  #101440 ) ;
#227893 = CARTESIAN_POINT ( 'NONE',  ( 23.14999999999999503, 11.65000000001116298, -93.48519422934610645 ) ) ;
#227894 = EDGE_LOOP ( 'NONE', ( #14812, #182037, #204672, #67880 ) ) ;
#227895 = ORIENTED_EDGE ( 'NONE', *, *, #190572, .F. ) ;
#227896 = AXIS2_PLACEMENT_3D ( 'NONE', #233003, #76458, #13940 ) ;
#227897 = DIRECTION ( 'NONE',  ( 0.000000000000000000, 1.000000000000000000, 0.000000000000000000 ) ) ;
#227898 = CARTESIAN_POINT ( 'NONE',  ( -20.00857864376270001, 9.250000000011157297, -188.6499999999999488 ) ) ;
#227899 = ORIENTED_EDGE ( 'NONE', *, *, #172412, .T. ) ;
#227900 = LINE ( 'NONE', #209622, #85121 ) ;
#227901 = EDGE_LOOP ( 'NONE', ( #246141, #107732, #35213, #138574 ) ) ;
#227902 = EDGE_CURVE ( 'NONE', #191690, #132561, #198633, .T. ) ;
#227903 = CARTESIAN_POINT ( 'NONE',  ( -22.45437739390952459, 1.115486826172573664E-11, -55.35042918840623116 ) ) ;
#227904 = ORIENTED_EDGE ( 'NONE', *, *, #195597, .F. ) ;
#227905 = CARTESIAN_POINT ( 'NONE',  ( 21.14999999999999503, -13.98128454229088469, -192.0195388455185821 ) ) ;
#227906 = AXIS2_PLACEMENT_3D ( 'NONE', #137998, #217534, #79306 ) ;
#227907 = CARTESIAN_POINT ( 'NONE',  ( 18.49999999999999289, 55.11567808474818975, -229.9682219939384140 ) ) ;
#227908 = AXIS2_PLACEMENT_3D ( 'NONE', #25166, #163377, #23888 ) ;
#227909 = ADVANCED_FACE ( 'NONE', ( #94391 ), #134785, .T. ) ;
#227910 = VECTOR ( 'NONE', #157753, 1000.000000000000000 ) ;
#227911 = AXIS2_PLACEMENT_3D ( 'NONE', #37439, #60815, #98629 ) ;
#227912 = VERTEX_POINT ( 'NONE', #138628 ) ;
#227913 = CARTESIAN_POINT ( 'NONE',  ( 18.41815437325347204, -9.498709853130270275, -207.6039458388019341 ) ) ;
#227914 = AXIS2_PLACEMENT_3D ( 'NONE', #2375, #3669, #147023 ) ;
#227915 = ORIENTED_EDGE ( 'NONE', *, *, #221537, .T. ) ;
#227916 = EDGE_LOOP ( 'NONE', ( #59160, #93416, #37996, #150556 ) ) ;
#227917 = ORIENTED_EDGE ( 'NONE', *, *, #157322, .T. ) ;
#227918 = DIRECTION ( 'NONE',  ( 0.000000000000000000, 0.000000000000000000, -1.000000000000000000 ) ) ;
#227919 = DIRECTION ( 'NONE',  ( 0.000000000000000000, 0.1495327102803586661, 0.9887567792719350601 ) ) ;
#227920 = CARTESIAN_POINT ( 'NONE',  ( -21.10320863425827298, 0.02502225123826237740, -127.5997226135408056 ) ) ;
#227921 = DIRECTION ( 'NONE',  ( 0.000000000000000000, 0.000000000000000000, 1.000000000000000000 ) ) ;
#227922 = DIRECTION ( 'NONE',  ( -1.000000000000000000, -0.000000000000000000, -0.000000000000000000 ) ) ;
#227924 = CARTESIAN_POINT ( 'NONE',  ( 21.05543885634738643, 8.775771046847536283, -12.18438447071468822 ) ) ;
#227923 = CARTESIAN_POINT ( 'NONE',  ( 22.49436431346199683, -3.108951784663558371, -228.1727023102511964 ) ) ;
#227926 = ORIENTED_EDGE ( 'NONE', *, *, #153176, .F. ) ;
#227925 = FACE_OUTER_BOUND ( 'NONE', #94984, .T. ) ;
#227927 = DIRECTION ( 'NONE',  ( 0.000000000000000000, -0.2128009952263603677, 0.9770955615653313941 ) ) ;
#227928 = VERTEX_POINT ( 'NONE', #55238 ) ;
#227929 = LINE ( 'NONE', #205791, #217395 ) ;
#227930 = CIRCLE ( 'NONE', #98702, 0.1000000000000102612 ) ;
#227931 = ORIENTED_EDGE ( 'NONE', *, *, #75155, .T. ) ;
#227932 = EDGE_LOOP ( 'NONE', ( #99671, #164094, #37406, #226674 ) ) ;
#227933 = DIRECTION ( 'NONE',  ( 0.7071067811865475727, 0.7071067811865475727, 0.000000000000000000 ) ) ;
#227934 = AXIS2_PLACEMENT_3D ( 'NONE', #160045, #98717, #257777 ) ;
#227935 = DIRECTION ( 'NONE',  ( -1.836970198721029934E-16, -1.000000000000000000, -6.982962677686266711E-15 ) ) ;
#227936 = CYLINDRICAL_SURFACE ( 'NONE', #104395, 0.09999999999998898659 ) ;
#227937 = DIRECTION ( 'NONE',  ( 0.000000000000000000, -1.000000000000000000, -6.982962677686266711E-15 ) ) ;
#227938 = AXIS2_PLACEMENT_3D ( 'NONE', #222222, #178005, #181845 ) ;
#227939 = DIRECTION ( 'NONE',  ( 0.000000000000000000, -0.8700118002898357128, 0.4930308989875170633 ) ) ;
#227940 = ORIENTED_EDGE ( 'NONE', *, *, #90879, .T. ) ;
#227941 = ORIENTED_EDGE ( 'NONE', *, *, #184909, .T. ) ;
#227942 = CARTESIAN_POINT ( 'NONE',  ( 23.14999999999999858, 6.649999999999999467, -12.35000000000000320 ) ) ;
#227943 = ORIENTED_EDGE ( 'NONE', *, *, #88591, .T. ) ;
#227944 = CARTESIAN_POINT ( 'NONE',  ( -22.37643362114956602, 0.09908137369253962323, -126.3742100060416220 ) ) ;
#227945 = DIRECTION ( 'NONE',  ( 0.000000000000000000, -0.9126074666063769270, -0.4088369013363281623 ) ) ;
#227946 = ORIENTED_EDGE ( 'NONE', *, *, #93600, .T. ) ;
#227947 = PLANE ( 'NONE',  #173838 ) ;
#227948 = CARTESIAN_POINT ( 'NONE',  ( -23.25000000000000000, 87.75000000001267608, -203.5231074845243029 ) ) ;
#227949 = DIRECTION ( 'NONE',  ( 0.000000000000000000, 1.000000000000000000, 0.000000000000000000 ) ) ;
#227950 = DIRECTION ( 'NONE',  ( 0.000000000000000000, -0.8660254037844383745, 0.5000000000000003331 ) ) ;
#227951 = VERTEX_POINT ( 'NONE', #215619 ) ;
#227952 = CARTESIAN_POINT ( 'NONE',  ( -22.57320508075687115, 64.25000000001215028, -136.5231074845243597 ) ) ;
#227953 = SPHERICAL_SURFACE ( 'NONE', #50057, 0.1000000000000000056 ) ;
#227954 = DIRECTION ( 'NONE',  ( 0.000000000000000000, 0.000000000000000000, -1.000000000000000000 ) ) ;
#227955 = DIRECTION ( 'NONE',  ( 0.000000000000000000, 0.000000000000000000, -1.000000000000000000 ) ) ;
#227957 = EDGE_CURVE ( 'NONE', #168984, #112163, #178782, .T. ) ;
#227956 = FACE_OUTER_BOUND ( 'NONE', #74074, .T. ) ;
#227958 = AXIS2_PLACEMENT_3D ( 'NONE', #191456, #91033, #33679 ) ;
#227960 = VECTOR ( 'NONE', #230522, 1000.000000000000000 ) ;
#227959 = DIRECTION ( 'NONE',  ( 0.000000000000000000, 0.2128009952263485993, -0.9770955615653341697 ) ) ;
#227961 = AXIS2_PLACEMENT_3D ( 'NONE', #11965, #31544, #91482 ) ;
#227962 = CIRCLE ( 'NONE', #65632, 6.258578643762710669 ) ;
#227963 = ORIENTED_EDGE ( 'NONE', *, *, #87049, .F. ) ;
#227964 = FACE_OUTER_BOUND ( 'NONE', #45935, .T. ) ;
#227965 = EDGE_CURVE ( 'NONE', #7452, #175979, #39729, .T. ) ;
#227966 = ORIENTED_EDGE ( 'NONE', *, *, #68832, .F. ) ;
#227967 = CARTESIAN_POINT ( 'NONE',  ( -18.40000000000000213, 11.47316190337364183, -121.4500000000000313 ) ) ;
#227968 = CARTESIAN_POINT ( 'NONE',  ( -18.79999999999999716, 7.986648289447971116, -1.311673547813416718 ) ) ;
#227969 = DIRECTION ( 'NONE',  ( 0.000000000000000000, 0.000000000000000000, -1.000000000000000000 ) ) ;
#227970 = CARTESIAN_POINT ( 'NONE',  ( 18.59999999999999787, -1.263275465206102233, -175.4018646667464338 ) ) ;
#227971 = EDGE_CURVE ( 'NONE', #73109, #21187, #231262, .T. ) ;
#227972 = ORIENTED_EDGE ( 'NONE', *, *, #152773, .T. ) ;
#227973 = DIRECTION ( 'NONE',  ( 0.000000000000000000, 0.000000000000000000, -1.000000000000000000 ) ) ;
#227974 = CARTESIAN_POINT ( 'NONE',  ( -20.64999999999999858, -8.999999999988844479, -124.1060308773475924 ) ) ;
#227975 = CARTESIAN_POINT ( 'NONE',  ( 18.59999999999999076, 74.16465844978819177, -191.9679561919613775 ) ) ;
#227976 = DIRECTION ( 'NONE',  ( 1.000000000000000000, 0.000000000000000000, -0.000000000000000000 ) ) ;
#227977 = AXIS2_PLACEMENT_3D ( 'NONE', #44252, #126341, #48086 ) ;
#227978 = CARTESIAN_POINT ( 'NONE',  ( 20.99142135623731065, 11.60000000001116049, -60.07179676972450721 ) ) ;
#227979 =( BOUNDED_SURFACE ( )  B_SPLINE_SURFACE ( 3, 2, ( 
 ( #161302, #40085, #239542 ),
 ( #141709, #140421, #184684 ),
 ( #23082, #103851, #120903 ),
 ( #202969, #6042, #204248 ),
 ( #85552, #2187, #221234 ),
 ( #42617, #82990, #122164 ) ),
 .UNSPECIFIED., .F., .F., .T. ) 
 B_SPLINE_SURFACE_WITH_KNOTS ( ( 4, 2, 4 ),
 ( 3, 3 ),
 ( -1.776356839400250465E-15, 0.7853981633974468357, 1.570796326794895448 ),
 ( 0.000000000000000000, 1.000000000000000000 ),
 .UNSPECIFIED. ) 
 GEOMETRIC_REPRESENTATION_ITEM ( )  RATIONAL_B_SPLINE_SURFACE ( (
 ( 1.000000000000000000, 0.5000000000000655032, 1.000000000000000000),
 ( 1.000000000000000000, 0.4993418825348334145, 1.000000000000000000),
 ( 1.000000000000000000, 0.5278258667039918972, 1.000000000000000000),
 ( 1.000000000000000000, 0.6092287576712909214, 1.000000000000000000),
 ( 1.000000000000000000, 0.6611148371766234488, 1.000000000000000000),
 ( 1.000000000000000000, 0.7071067811865806574, 1.000000000000000000) ) ) 
 REPRESENTATION_ITEM ( '' )  SURFACE ( )  );
#227980 = AXIS2_PLACEMENT_3D ( 'NONE', #167490, #129625, #204014 ) ;
#227981 = VERTEX_POINT ( 'NONE', #17428 ) ;
#227982 = VERTEX_POINT ( 'NONE', #96930 ) ;
#227983 = FACE_OUTER_BOUND ( 'NONE', #154168, .T. ) ;
#227984 = DIRECTION ( 'NONE',  ( 0.000000000000000000, 1.776356839400250465E-15, 1.000000000000000000 ) ) ;
#227985 = CYLINDRICAL_SURFACE ( 'NONE', #55019, 0.09999999999999939493 ) ;
#227987 = ADVANCED_FACE ( 'NONE', ( #156971 ), #95674, .T. ) ;
#227986 = LINE ( 'NONE', #32386, #101845 ) ;
#227988 = CARTESIAN_POINT ( 'NONE',  ( -16.87845715379269507, 44.10835929761906016, -235.3024714938296995 ) ) ;
#227989 = EDGE_CURVE ( 'NONE', #53100, #207854, #10490, .T. ) ;
#227990 = ORIENTED_EDGE ( 'NONE', *, *, #72051, .F. ) ;
#227991 = CARTESIAN_POINT ( 'NONE',  ( 22.59066674512243722, 11.75000000001115552, -33.46949587636930090 ) ) ;
#227992 = ADVANCED_FACE ( 'NONE', ( #158272 ), #160528, .T. ) ;
#227993 = ITEM_DEFINED_TRANSFORMATION ( 'NONE', 'NONE', #127708,  #2425 ) ;
#227994 = FACE_OUTER_BOUND ( 'NONE', #246045, .T. ) ;
#227995 = VERTEX_POINT ( 'NONE', #23886 ) ;
#227996 = DIRECTION ( 'NONE',  ( 0.000000000000000000, -0.2617529984165152257, -0.9651348961777124202 ) ) ;
#227997 = AXIS2_PLACEMENT_3D ( 'NONE', #207404, #113421, #148710 ) ;
#227998 = EDGE_CURVE ( 'NONE', #129928, #84058, #227128, .T. ) ;
#227999 = VERTEX_POINT ( 'NONE', #223321 ) ;
#228000 = EDGE_LOOP ( 'NONE', ( #208322, #120450, #143387, #114340, #53650, #128533, #134693 ) ) ;
#228001 = VERTEX_POINT ( 'NONE', #139928 ) ;
#228002 = DIRECTION ( 'NONE',  ( 0.000000000000000000, -0.9126074666063771490, -0.4088369013363281623 ) ) ;
#228003 = DIRECTION ( 'NONE',  ( 0.000000000000000000, 0.000000000000000000, -1.000000000000000000 ) ) ;
#228004 = DIRECTION ( 'NONE',  ( 1.000000000000000000, 0.000000000000000000, 0.000000000000000000 ) ) ;
#228005 = CARTESIAN_POINT ( 'NONE',  ( 18.44444291854882323, -9.490101180932068559, -140.6289039648909807 ) ) ;
#228006 = DIRECTION ( 'NONE',  ( 1.000000000000000000, 0.000000000000000000, 0.000000000000000000 ) ) ;
#228007 = FACE_OUTER_BOUND ( 'NONE', #112103, .T. ) ;
#228008 = CARTESIAN_POINT ( 'NONE',  ( 22.39999999999999503, 11.65000000001116298, -167.3999999999999773 ) ) ;
#228009 = EDGE_CURVE ( 'NONE', #105539, #45147, #159527, .T. ) ;
#228012 = DIRECTION ( 'NONE',  ( 0.000000000000000000, -2.428612866367797514E-13, 1.000000000000000000 ) ) ;
#228011 = AXIS2_PLACEMENT_3D ( 'NONE', #185380, #184091, #225768 ) ;
#228010 = DIRECTION ( 'NONE',  ( 0.000000000000000000, 0.8814952561688428334, -0.4721928772777350125 ) ) ;
#228013 = CARTESIAN_POINT ( 'NONE',  ( -16.87036670365549895, 10.08494996326643189, -113.0500000000000398 ) ) ;
#228014 = CARTESIAN_POINT ( 'NONE',  ( -16.89268316805466341, 9.951721813253341153, -113.1442475214544885 ) ) ;
#228015 = DIRECTION ( 'NONE',  ( 0.000000000000000000, 1.000000000000000000, 6.352154140967427193E-15 ) ) ;
#228016 = CYLINDRICAL_SURFACE ( 'NONE', #7381, 0.09999999999999939493 ) ;
#228017 = AXIS2_PLACEMENT_3D ( 'NONE', #113915, #154374, #31846 ) ;
#228018 = ORIENTED_EDGE ( 'NONE', *, *, #193493, .T. ) ;
#228019 = CIRCLE ( 'NONE', #252952, 0.09999999999999609201 ) ;
#228020 = ORIENTED_EDGE ( 'NONE', *, *, #243357, .T. ) ;
#228021 = CARTESIAN_POINT ( 'NONE',  ( -18.59999994787167310, -9.523637689761692116, -40.38244953477238397 ) ) ;
#228022 = CARTESIAN_POINT ( 'NONE',  ( 13.40000000000000036, -8.250000000000003553, 12.40000000000000391 ) ) ;
#228024 = CARTESIAN_POINT ( 'NONE',  ( -15.06720934482787300, 13.06253445771512922, -216.7219835687084810 ) ) ;
#228023 = CYLINDRICAL_SURFACE ( 'NONE', #196414, 0.09999999999999939493 ) ;
#228025 = CIRCLE ( 'NONE', #195086, 0.3999999999999885869 ) ;
#228026 = CARTESIAN_POINT ( 'NONE',  ( -21.14999999999999858, 76.00000000001200817, -109.5637644362255543 ) ) ;
#228027 = DIRECTION ( 'NONE',  ( 0.000000000000000000, -6.982962677686266711E-15, 1.000000000000000000 ) ) ;
#228028 = VECTOR ( 'NONE', #5000, 1000.000000000000000 ) ;
#228029 = CARTESIAN_POINT ( 'NONE',  ( -18.59999999999999787, 77.25000000001209344, -128.7226267301092548 ) ) ;
#228030 = ORIENTED_EDGE ( 'NONE', *, *, #1497, .F. ) ;
#228031 = ORIENTED_EDGE ( 'NONE', *, *, #77638, .T. ) ;
#228032 = CARTESIAN_POINT ( 'NONE',  ( -15.73854595235691889, 9.351413679101387544, -16.98034356754896734 ) ) ;
#228033 = VERTEX_POINT ( 'NONE', #184196 ) ;
#228034 = CARTESIAN_POINT ( 'NONE',  ( 23.15000000000000213, -8.999999999988844479, -110.3939691226524786 ) ) ;
#228035 = TOROIDAL_SURFACE ( 'NONE', #65522, 0.4000000000000009104, 0.1000000000000000056 ) ;
#228036 = CIRCLE ( 'NONE', #11371, 0.09999999999999939493 ) ;
#228037 = DIRECTION ( 'NONE',  ( 1.000000000000000000, 0.000000000000000000, 0.000000000000000000 ) ) ;
#228038 = ADVANCED_FACE ( 'NONE', ( #203774 ), #148027, .F. ) ;
#228039 = TOROIDAL_SURFACE ( 'NONE', #78000, 0.2000000000000000111, 0.1000000000000000056 ) ;
#228041 = EDGE_CURVE ( 'NONE', #254300, #17154, #42151, .T. ) ;
#228040 = AXIS2_PLACEMENT_3D ( 'NONE', #184201, #5554, #145076 ) ;
#228042 = EDGE_LOOP ( 'NONE', ( #66851, #81201, #129619, #254410, #234804 ) ) ;
#228043 = DIRECTION ( 'NONE',  ( -3.265361837132813093E-16, -1.000000000000000000, -7.026728003956683390E-15 ) ) ;
#228044 = ORIENTED_EDGE ( 'NONE', *, *, #229237, .T. ) ;
#228045 = VECTOR ( 'NONE', #41480, 1000.000000000000000 ) ;
#228046 = EDGE_CURVE ( 'NONE', #70064, #193535, #181371, .T. ) ;
#228048 = EDGE_CURVE ( 'NONE', #147289, #189211, #6372, .T. ) ;
#228047 = CARTESIAN_POINT ( 'NONE',  ( 18.59999999999999432, 5.699452464332755319, -20.95772604343016710 ) ) ;
#228049 = CARTESIAN_POINT ( 'NONE',  ( -23.15000000000000213, 26.22918441313017723, -241.0147027585851731 ) ) ;
#228050 = CARTESIAN_POINT ( 'NONE',  ( -18.34374000495060386, 64.52683809664912928, -60.27310748452440947 ) ) ;
#228051 = CARTESIAN_POINT ( 'NONE',  ( -20.64999999999999858, 2.000000000011154189, -146.7246219227621111 ) ) ;
#228052 = CARTESIAN_POINT ( 'NONE',  ( -18.39999999999999858, -0.8467571797981087167, -242.2246066262668194 ) ) ;
#228053 = CYLINDRICAL_SURFACE ( 'NONE', #166600, 7.899999999999990585 ) ;
#228054 = EDGE_CURVE ( 'NONE', #228089, #145413, #219470, .T. ) ;
#228055 = DIRECTION ( 'NONE',  ( 0.000000000000000000, -0.2558827019433787542, 0.9667078373770204847 ) ) ;
#228056 = CARTESIAN_POINT ( 'NONE',  ( -15.55912972643740488, 8.490870273573721150, -154.8500000000000227 ) ) ;
#228058 = ORIENTED_EDGE ( 'NONE', *, *, #138946, .F. ) ;
#228057 = CARTESIAN_POINT ( 'NONE',  ( 21.14999999999999858, 11.40444339177024169, -198.6185779617709670 ) ) ;
#228060 = DIRECTION ( 'NONE',  ( 0.000000000000000000, 0.000000000000000000, 1.000000000000000000 ) ) ;
#228059 = CARTESIAN_POINT ( 'NONE',  ( -18.60000000000000853, 85.36424052760351344, -196.3428589026835596 ) ) ;
#228061 = ORIENTED_EDGE ( 'NONE', *, *, #186895, .F. ) ;
#228063 = ORIENTED_EDGE ( 'NONE', *, *, #68785, .F. ) ;
#228062 = DIRECTION ( 'NONE',  ( -0.000000000000000000, 0.8496786552930076786, 0.5273008465188218086 ) ) ;
#228064 = EDGE_CURVE ( 'NONE', #46950, #25924, #68944, .T. ) ;
#228065 = CIRCLE ( 'NONE', #69858, 0.09999999999999939493 ) ;
#228066 = ORIENTED_EDGE ( 'NONE', *, *, #172551, .T. ) ;
#228067 = CARTESIAN_POINT ( 'NONE',  ( 18.46921299892755641, 85.50937817783538719, -62.53652877515382613 ) ) ;
#228070 = EDGE_CURVE ( 'NONE', #246837, #171007, #77107, .T. ) ;
#228069 = EDGE_CURVE ( 'NONE', #60110, #186782, #22586, .T. ) ;
#228068 = AXIS2_PLACEMENT_3D ( 'NONE', #161952, #25013, #245326 ) ;
#228071 = AXIS2_PLACEMENT_3D ( 'NONE', #193650, #211935, #251028 ) ;
#228072 = LINE ( 'NONE', #110680, #84496 ) ;
#228073 = CARTESIAN_POINT ( 'NONE',  ( 22.45301702632625762, 75.98478912030155641, -81.17289970878471195 ) ) ;
#228074 = CARTESIAN_POINT ( 'NONE',  ( -22.59080734064477625, 11.47432927991817309, -198.4695429027907494 ) ) ;
#228075 = CARTESIAN_POINT ( 'NONE',  ( -20.85000000000000142, 11.75000000001115197, -93.71613433702194129 ) ) ;
#228076 = CARTESIAN_POINT ( 'NONE',  ( -21.05000000000000071, 86.19075908668452257, -209.4719249499869136 ) ) ;
#228077 = CARTESIAN_POINT ( 'NONE',  ( -21.44999999999999929, 68.65000000001150227, -48.37310748452437537 ) ) ;
#228078 = CARTESIAN_POINT ( 'NONE',  ( -16.80117486205003630, 51.61795800203399409, -231.9472499653515740 ) ) ;
#228079 = AXIS2_PLACEMENT_3D ( 'NONE', #94816, #114388, #230490 ) ;
#228080 = EDGE_CURVE ( 'NONE', #56789, #62705, #4273, .T. ) ;
#228081 = AXIS2_PLACEMENT_3D ( 'NONE', #67853, #11764, #148697 ) ;
#228082 = DIRECTION ( 'NONE',  ( 1.000000000000000000, 0.000000000000000000, 0.000000000000000000 ) ) ;
#228083 = ORIENTED_EDGE ( 'NONE', *, *, #173420, .F. ) ;
#228084 = ORIENTED_EDGE ( 'NONE', *, *, #103318, .T. ) ;
#228085 = CARTESIAN_POINT ( 'NONE',  ( 23.14999999999999858, 45.21086124044690280, -238.4331873168094091 ) ) ;
#228086 = VECTOR ( 'NONE', #120565, 1000.000000000000000 ) ;
#228087 = EDGE_CURVE ( 'NONE', #220745, #105532, #45980, .T. ) ;
#228088 = ADVANCED_FACE ( 'NONE', ( #181656 ), #199944, .F. ) ;
#228089 = VERTEX_POINT ( 'NONE', #26436 ) ;
#228090 = CARTESIAN_POINT ( 'NONE',  ( -20.94999999999999929, 76.00000000001188027, -99.02310748452428868 ) ) ;
#228091 = ORIENTED_EDGE ( 'NONE', *, *, #56608, .F. ) ;
#228092 = PLANE ( 'NONE',  #238514 ) ;
#228093 = AXIS2_PLACEMENT_3D ( 'NONE', #115288, #194856, #16219 ) ;
#228094 = EDGE_CURVE ( 'NONE', #114115, #121586, #31367, .T. ) ;
#228095 = CARTESIAN_POINT ( 'NONE',  ( -17.04295772865469871, 10.02489942527109612, -180.1499999999999773 ) ) ;
#228096 = CYLINDRICAL_SURFACE ( 'NONE', #89349, 2.599999999999998312 ) ;
#228097 = CARTESIAN_POINT ( 'NONE',  ( -21.05000000000000426, 1.561552638127804205, -230.7743248509848399 ) ) ;
#228098 = DIRECTION ( 'NONE',  ( 0.000000000000000000, 0.000000000000000000, -1.000000000000000000 ) ) ;
#228099 = ORIENTED_EDGE ( 'NONE', *, *, #225831, .F. ) ;
#228100 = ADVANCED_FACE ( 'NONE', ( #160824 ), #56175, .T. ) ;
#228101 = VECTOR ( 'NONE', #253789, 1000.000000000000000 ) ;
#228102 = CARTESIAN_POINT ( 'NONE',  ( 20.94999999999999929, 76.00000000001136868, -28.22310748452431994 ) ) ;
#228103 = AXIS2_PLACEMENT_3D ( 'NONE', #62458, #105386, #101537 ) ;
#228104 = AXIS2_PLACEMENT_3D ( 'NONE', #78778, #59193, #25268 ) ;
#228105 = CYLINDRICAL_SURFACE ( 'NONE', #246242, 2.000000000000001776 ) ;
#228106 = AXIS2_PLACEMENT_3D ( 'NONE', #7088, #205280, #223556 ) ;
#228107 = CARTESIAN_POINT ( 'NONE',  ( 18.59999994388910238, 85.36356618708258281, -62.34199024772312470 ) ) ;
#228108 = DIRECTION ( 'NONE',  ( 1.000000000000000000, 0.000000000000000000, -0.000000000000000000 ) ) ;
#228109 = ORIENTED_EDGE ( 'NONE', *, *, #88278, .T. ) ;
#228111 = DIRECTION ( 'NONE',  ( -1.000000000000000000, -0.000000000000000000, -0.000000000000000000 ) ) ;
#228110 = CARTESIAN_POINT ( 'NONE',  ( 21.07971444708685738, 61.09918328174379099, -234.2830459128522307 ) ) ;
#228112 = ORIENTED_EDGE ( 'NONE', *, *, #105663, .T. ) ;
#228115 = VERTEX_POINT ( 'NONE', #168554 ) ;
#228114 = CARTESIAN_POINT ( 'NONE',  ( 21.15000000000005542, 79.78873604695631627, -7.297728304630792806 ) ) ;
#228113 = CARTESIAN_POINT ( 'NONE',  ( -20.54999999999999716, 85.00000000001222134, -146.0170766071767332 ) ) ;
#228116 = CIRCLE ( 'NONE', #132426, 2.000000000000001776 ) ;
#228117 = DIRECTION ( 'NONE',  ( 2.879366945564059217E-14, 0.9875055080513762684, -0.1575844902526679081 ) ) ;
#228118 = CARTESIAN_POINT ( 'NONE',  ( -21.05000000000000071, 34.11489510919708579, -243.6630126800748428 ) ) ;
#228119 = FACE_OUTER_BOUND ( 'NONE', #169588, .T. ) ;
#228120 = ORIENTED_EDGE ( 'NONE', *, *, #199748, .T. ) ;
#228121 = DIRECTION ( 'NONE',  ( 0.000000000000000000, -0.2617529984165031243, -0.9651348961777157509 ) ) ;
#228122 = DIRECTION ( 'NONE',  ( 0.000000000000000000, 0.000000000000000000, 1.000000000000000000 ) ) ;
#228124 = CARTESIAN_POINT ( 'NONE',  ( -23.15000000000000213, 11.65000000000000036, -26.48519422934605316 ) ) ;
#228123 = DIRECTION ( 'NONE',  ( 0.000000000000000000, -0.4088369013363280513, 0.9126074666063769270 ) ) ;
#228126 = ORIENTED_EDGE ( 'NONE', *, *, #184232, .T. ) ;
#228125 = PLANE ( 'NONE',  #197368 ) ;
#228127 = CIRCLE ( 'NONE', #53141, 0.09999999999999939493 ) ;
#228128 = ORIENTED_EDGE ( 'NONE', *, *, #111916, .T. ) ;
#228129 = DIRECTION ( 'NONE',  ( 0.000000000000000000, 1.000000000000000000, 0.000000000000000000 ) ) ;
#228130 = DIRECTION ( 'NONE',  ( 1.000000000000000000, 0.000000000000000000, 0.000000000000000000 ) ) ;
#228131 = AXIS2_PLACEMENT_3D ( 'NONE', #131830, #211380, #95274 ) ;
#228132 = FACE_OUTER_BOUND ( 'NONE', #48319, .T. ) ;
#228133 = VERTEX_POINT ( 'NONE', #227181 ) ;
#228134 = CARTESIAN_POINT ( 'NONE',  ( -16.81931177881023132, 9.936996059515061930, -188.2732178786172028 ) ) ;
#228135 = CARTESIAN_POINT ( 'NONE',  ( 18.39999999999999503, 5.649999999999983480, -24.25000000000001066 ) ) ;
#228136 = DIRECTION ( 'NONE',  ( 1.000000000000000000, 0.000000000000000000, 0.000000000000000000 ) ) ;
#228137 = ORIENTED_EDGE ( 'NONE', *, *, #106982, .T. ) ;
#228138 = DIRECTION ( 'NONE',  ( 1.000000000000000000, -0.000000000000000000, -0.000000000000000000 ) ) ;
#228139 = EDGE_CURVE ( 'NONE', #135650, #199385, #248029, .T. ) ;
#228140 = ORIENTED_EDGE ( 'NONE', *, *, #209889, .F. ) ;
#228141 = VECTOR ( 'NONE', #74072, 1000.000000000000000 ) ;
#228142 = VECTOR ( 'NONE', #25292, 999.9999999999998863 ) ;
#228143 = LINE ( 'NONE', #46905, #209832 ) ;
#228145 = ADVANCED_FACE ( 'NONE', ( #228490 ), #66836, .T. ) ;
#228144 = DIRECTION ( 'NONE',  ( 1.000000000000000000, 0.000000000000000000, 0.000000000000000000 ) ) ;
#228146 = AXIS2_PLACEMENT_3D ( 'NONE', #75331, #153606, #53167 ) ;
#228147 = VERTEX_POINT ( 'NONE', #31592 ) ;
#228148 = ORIENTED_EDGE ( 'NONE', *, *, #13775, .F. ) ;
#228149 = EDGE_CURVE ( 'NONE', #50987, #54519, #243706, .T. ) ;
#228150 = CARTESIAN_POINT ( 'NONE',  ( 21.05000000000000071, 1.115649653272650466E-11, -96.50000000000004263 ) ) ;
#228151 = EDGE_LOOP ( 'NONE', ( #198708, #165609, #141962, #93530 ) ) ;
#228153 = EDGE_CURVE ( 'NONE', #137732, #157238, #112388, .T. ) ;
#228152 = ORIENTED_EDGE ( 'NONE', *, *, #40329, .T. ) ;
#228154 = ORIENTED_EDGE ( 'NONE', *, *, #160954, .F. ) ;
#228157 = ORIENTED_EDGE ( 'NONE', *, *, #161221, .F. ) ;
#228156 = ORIENTED_EDGE ( 'NONE', *, *, #225066, .F. ) ;
#228155 = DIRECTION ( 'NONE',  ( 1.000000000000000000, 0.000000000000000000, 0.000000000000000000 ) ) ;
#228158 = AXIS2_PLACEMENT_3D ( 'NONE', #101357, #157588, #197937 ) ;
#228159 = CARTESIAN_POINT ( 'NONE',  ( -18.48408745364664085, -9.664322258651962372, -107.1830785333284126 ) ) ;
#228160 = CIRCLE ( 'NONE', #161537, 0.1000000000000061395 ) ;
#228161 = ORIENTED_EDGE ( 'NONE', *, *, #160111, .T. ) ;
#228162 = FACE_OUTER_BOUND ( 'NONE', #103063, .T. ) ;
#228163 = DIRECTION ( 'NONE',  ( 0.000000000000000000, 6.938893903907222067E-15, -1.000000000000000000 ) ) ;
#228164 = DIRECTION ( 'NONE',  ( 0.000000000000000000, 0.000000000000000000, 1.000000000000000000 ) ) ;
#228165 = EDGE_CURVE ( 'NONE', #28990, #14615, #12016, .T. ) ;
#228166 = AXIS2_PLACEMENT_3D ( 'NONE', #45696, #60429, #186505 ) ;
#228167 = CYLINDRICAL_SURFACE ( 'NONE', #109365, 12.87499999999999822 ) ;
#228168 = ADVANCED_FACE ( 'NONE', ( #48548 ), #87662, .T. ) ;
#228169 = ORIENTED_EDGE ( 'NONE', *, *, #92649, .F. ) ;
#228170 = VERTEX_POINT ( 'NONE', #128096 ) ;
#228171 = CARTESIAN_POINT ( 'NONE',  ( 21.72449340488910607, 12.01681723992382800, -207.8496978137663689 ) ) ;
#228173 = EDGE_LOOP ( 'NONE', ( #12632, #206356, #142397, #9624 ) ) ;
#228172 = CARTESIAN_POINT ( 'NONE',  ( 18.52928932188133970, 63.76258513157055319, -209.3739165141044793 ) ) ;
#228174 = DIRECTION ( 'NONE',  ( 1.000000000000000000, -0.000000000000000000, 0.000000000000000000 ) ) ;
#228176 = ORIENTED_EDGE ( 'NONE', *, *, #119899, .F. ) ;
#228175 = CARTESIAN_POINT ( 'NONE',  ( 18.47654891039378455, 78.23178726748734846, -231.4551625896290545 ) ) ;
#228177 = ORIENTED_EDGE ( 'NONE', *, *, #81118, .T. ) ;
#228178 = CARTESIAN_POINT ( 'NONE',  ( 18.54999999999999716, 62.09751964147213954, -221.3558313336858987 ) ) ;
#228179 = EDGE_CURVE ( 'NONE', #245547, #144086, #23350, .T. ) ;
#228180 = ORIENTED_EDGE ( 'NONE', *, *, #6892, .T. ) ;
#228181 = CARTESIAN_POINT ( 'NONE',  ( -16.92778301347287950, 65.99905508317688430, -149.0945893765574510 ) ) ;
#228182 = DIRECTION ( 'NONE',  ( 1.000000000000000000, 3.469446951953704435E-14, -2.003086131649669752E-14 ) ) ;
#228183 = AXIS2_PLACEMENT_3D ( 'NONE', #137786, #255128, #98633 ) ;
#228184 = EDGE_CURVE ( 'NONE', #256777, #90926, #114899, .T. ) ;
#228185 = VECTOR ( 'NONE', #95671, 999.9999999999998863 ) ;
#228186 = VECTOR ( 'NONE', #91960, 1000.000000000000000 ) ;
#228188 = ORIENTED_EDGE ( 'NONE', *, *, #25067, .F. ) ;
#228187 = ORIENTED_EDGE ( 'NONE', *, *, #151936, .T. ) ;
#228189 = ORIENTED_EDGE ( 'NONE', *, *, #128080, .T. ) ;
#228190 = CARTESIAN_POINT ( 'NONE',  ( 18.39999999999999503, 11.75000000001113953, -79.65000000000004832 ) ) ;
#228191 = ORIENTED_EDGE ( 'NONE', *, *, #70904, .F. ) ;
#228192 = ORIENTED_EDGE ( 'NONE', *, *, #208138, .F. ) ;
#228193 = CARTESIAN_POINT ( 'NONE',  ( 23.24999999999999289, 69.55000000001157900, -57.17310748452436542 ) ) ;
#228195 = ORIENTED_EDGE ( 'NONE', *, *, #77184, .T. ) ;
#228194 = CYLINDRICAL_SURFACE ( 'NONE', #209936, 0.1000000000000052097 ) ;
#228196 = DIRECTION ( 'NONE',  ( 0.000000000000000000, 0.000000000000000000, -1.000000000000000000 ) ) ;
#228198 = DIRECTION ( 'NONE',  ( 1.000000000000000000, 0.000000000000000000, 0.000000000000000000 ) ) ;
#228197 = CYLINDRICAL_SURFACE ( 'NONE', #36538, 0.5000000000000004441 ) ;
#228199 = EDGE_CURVE ( 'NONE', #34898, #196043, #250594, .T. ) ;
#228200 = CARTESIAN_POINT ( 'NONE',  ( -20.94999999999999929, -1.736257131586239844, -45.06865232901750318 ) ) ;
#228201 = CARTESIAN_POINT ( 'NONE',  ( -13.22483237240078680, 62.09620004573545771, -218.7373296619003042 ) ) ;
#228202 = ORIENTED_EDGE ( 'NONE', *, *, #157382, .T. ) ;
#228203 = EDGE_CURVE ( 'NONE', #213361, #194690, #171118, .T. ) ;
#228204 = ORIENTED_EDGE ( 'NONE', *, *, #180296, .T. ) ;
#228205 = CARTESIAN_POINT ( 'NONE',  ( -23.25000000000000000, 71.65000000001155911, -57.27310748452435263 ) ) ;
#228206 = DIRECTION ( 'NONE',  ( 1.000000000000000000, 0.000000000000000000, 0.000000000000000000 ) ) ;
#228208 = ADVANCED_FACE ( 'NONE', ( #29035 ), #31547, .T. ) ;
#228207 = ORIENTED_EDGE ( 'NONE', *, *, #136340, .T. ) ;
#228209 = AXIS2_PLACEMENT_3D ( 'NONE', #180448, #159604, #239133 ) ;
#228210 = CIRCLE ( 'NONE', #244743, 0.1000000000000002554 ) ;
#228211 = CARTESIAN_POINT ( 'NONE',  ( 21.05000000000000071, 43.16354019706792400, -239.5695141926698284 ) ) ;
#228212 = AXIS2_PLACEMENT_3D ( 'NONE', #51142, #188116, #168606 ) ;
#228213 = EDGE_LOOP ( 'NONE', ( #170421, #145006, #42966, #46883 ) ) ;
#228214 = VERTEX_POINT ( 'NONE', #249337 ) ;
#228215 = CARTESIAN_POINT ( 'NONE',  ( -21.05439746398122836, 64.25000000001264766, -196.5331909970394406 ) ) ;
#228216 = CARTESIAN_POINT ( 'NONE',  ( 12.25000000000000000, 66.65000000001258229, -186.7731074845244166 ) ) ;
#228217 = ORIENTED_EDGE ( 'NONE', *, *, #135693, .T. ) ;
#228218 = CYLINDRICAL_SURFACE ( 'NONE', #88876, 0.1000000000000036415 ) ;
#228219 = LINE ( 'NONE', #54372, #126918 ) ;
#228220 = ORIENTED_EDGE ( 'NONE', *, *, #240851, .T. ) ;
#228221 = ADVANCED_FACE ( 'NONE', ( #229755 ), #130651, .T. ) ;
#228222 = CARTESIAN_POINT ( 'NONE',  ( -21.05000000000000071, 6.257814610487270279, -100.4022097086912311 ) ) ;
#228223 = CARTESIAN_POINT ( 'NONE',  ( -20.54999999999999716, 2.400000000011155432, -120.7753780772379315 ) ) ;
#228225 = CYLINDRICAL_SURFACE ( 'NONE', #33200, 0.09999999999999939493 ) ;
#228224 = DIRECTION ( 'NONE',  ( 1.000000000000000000, 0.000000000000000000, 0.000000000000000000 ) ) ;
#228226 = CARTESIAN_POINT ( 'NONE',  ( 21.05000000000000071, 14.05000000001115623, -128.4863049292391395 ) ) ;
#228227 = LINE ( 'NONE', #112143, #203505 ) ;
#228228 = DIRECTION ( 'NONE',  ( -0.000000000000000000, 0.8814952561688428334, -0.4721928772777352346 ) ) ;
#228230 = ADVANCED_FACE ( 'NONE', ( #190657 ), #126805, .T. ) ;
#228229 = FACE_OUTER_BOUND ( 'NONE', #149960, .T. ) ;
#228231 = AXIS2_PLACEMENT_3D ( 'NONE', #118999, #159410, #173876 ) ;
#228232 = ORIENTED_EDGE ( 'NONE', *, *, #126226, .T. ) ;
#228233 = AXIS2_PLACEMENT_3D ( 'NONE', #52712, #215634, #76133 ) ;
#228236 = EDGE_LOOP ( 'NONE', ( #194338, #238378, #3853, #3550 ) ) ;
#228235 = ORIENTED_EDGE ( 'NONE', *, *, #12245, .F. ) ;
#228234 = AXIS2_PLACEMENT_3D ( 'NONE', #171788, #10115, #149645 ) ;
#228237 = ORIENTED_EDGE ( 'NONE', *, *, #3264, .F. ) ;
#228238 = AXIS2_PLACEMENT_3D ( 'NONE', #38141, #117659, #237616 ) ;
#228239 = AXIS2_PLACEMENT_3D ( 'NONE', #226808, #148568, #49463 ) ;
#228241 = ADVANCED_FACE ( 'NONE', ( #256636 ), #179740, .T. ) ;
#228240 = CARTESIAN_POINT ( 'NONE',  ( -21.05000000000000071, 77.16270174995064224, -195.5231074845243313 ) ) ;
#228242 = DIRECTION ( 'NONE',  ( 1.000000000000000000, 0.000000000000000000, -0.000000000000000000 ) ) ;
#228243 = AXIS2_PLACEMENT_3D ( 'NONE', #121965, #99798, #179387 ) ;
#228245 = DIRECTION ( 'NONE',  ( 0.000000000000000000, -1.000000000000000000, -6.982962677686266711E-15 ) ) ;
#228244 = DIRECTION ( 'NONE',  ( 1.000000000000000000, 0.000000000000000000, 0.000000000000000000 ) ) ;
#228246 = CARTESIAN_POINT ( 'NONE',  ( -18.39999999999999858, 20.83093076766827423, -227.7429161672744442 ) ) ;
#228247 = EDGE_LOOP ( 'NONE', ( #17439, #11169, #19920, #105474 ) ) ;
#228248 = LINE ( 'NONE', #208694, #150780 ) ;
#228249 = ORIENTED_EDGE ( 'NONE', *, *, #195351, .F. ) ;
#228250 = LINE ( 'NONE', #186555, #83590 ) ;
#228251 = CARTESIAN_POINT ( 'NONE',  ( 18.59999999999999787, -1.249999999988843369, -141.8004807544151333 ) ) ;
#228252 = CARTESIAN_POINT ( 'NONE',  ( -21.15000000000000213, 1.363275264940683629, -230.6442496871288483 ) ) ;
#228253 = EDGE_LOOP ( 'NONE', ( #105383, #51703, #7794, #49436 ) ) ;
#228254 = AXIS2_PLACEMENT_3D ( 'NONE', #2949, #45942, #201162 ) ;
#228255 = AXIS2_PLACEMENT_3D ( 'NONE', #172544, #229897, #132082 ) ;
#228256 = DIRECTION ( 'NONE',  ( -1.000000000000000000, 0.000000000000000000, 0.000000000000000000 ) ) ;
#228257 = CARTESIAN_POINT ( 'NONE',  ( -22.39999999999999858, 75.90000000001199965, -110.8138870828977218 ) ) ;
#228258 = VERTEX_POINT ( 'NONE', #157641 ) ;
#228259 = ORIENTED_EDGE ( 'NONE', *, *, #206210, .T. ) ;
#228260 = CYLINDRICAL_SURFACE ( 'NONE', #179042, 0.1000000000000001443 ) ;
#228261 = CARTESIAN_POINT ( 'NONE',  ( -21.30740335185486245, 1.395886663891752866, -230.5494838277682845 ) ) ;
#228262 = DIRECTION ( 'NONE',  ( -1.000000000000000000, 0.000000000000000000, 0.000000000000000000 ) ) ;
#228263 = DIRECTION ( 'NONE',  ( 0.000000000000000000, 0.2128009952263604510, -0.9770955615653315052 ) ) ;
#228264 = CARTESIAN_POINT ( 'NONE',  ( 18.69999999999999929, 11.75000000000000000, 5.900000000000002132 ) ) ;
#228265 = DIRECTION ( 'NONE',  ( -1.000000000000000000, 0.000000000000000000, 0.000000000000000000 ) ) ;
#228266 = ORIENTED_EDGE ( 'NONE', *, *, #112045, .F. ) ;
#228267 = FACE_OUTER_BOUND ( 'NONE', #170314, .T. ) ;
#228268 = DIRECTION ( 'NONE',  ( -1.000000000000000000, -0.000000000000000000, -0.000000000000000000 ) ) ;
#228269 = CIRCLE ( 'NONE', #136651, 0.1000000000000028644 ) ;
#228271 = CARTESIAN_POINT ( 'NONE',  ( -21.05000000000000071, 11.63687328911514030, -174.3217592133248957 ) ) ;
#228270 = CARTESIAN_POINT ( 'NONE',  ( -16.93658211146644987, 9.994108662352344297, -87.90429506995572240 ) ) ;
#228272 = CARTESIAN_POINT ( 'NONE',  ( 18.59999999999999432, 1.162701749938009677, -8.099999999999999645 ) ) ;
#228273 = VECTOR ( 'NONE', #59817, 1000.000000000000000 ) ;
#228274 = DIRECTION ( 'NONE',  ( 0.000000000000000000, 0.000000000000000000, -1.000000000000000000 ) ) ;
#228275 = DIRECTION ( 'NONE',  ( 1.000000000000000000, 0.000000000000000000, 0.000000000000000000 ) ) ;
#228277 = CARTESIAN_POINT ( 'NONE',  ( 20.94788355080264353, 10.30207779525983192, -139.4895520716782755 ) ) ;
#228276 = VECTOR ( 'NONE', #28893, 1000.000000000000000 ) ;
#228279 = ORIENTED_EDGE ( 'NONE', *, *, #39113, .F. ) ;
#228278 = DIRECTION ( 'NONE',  ( 0.000000000000000000, -1.000000000000000000, -6.982962677686266711E-15 ) ) ;
#228280 = VECTOR ( 'NONE', #249380, 1000.000000000000000 ) ;
#228281 = EDGE_CURVE ( 'NONE', #213807, #125917, #119136, .T. ) ;
#228282 = AXIS2_PLACEMENT_3D ( 'NONE', #203825, #22649, #102126 ) ;
#228283 = CARTESIAN_POINT ( 'NONE',  ( -18.35668295345803713, 54.09900352584866567, -229.1663746252470446 ) ) ;
#228284 = ADVANCED_FACE ( 'NONE', ( #191949 ), #1058, .T. ) ;
#228286 = EDGE_CURVE ( 'NONE', #117188, #4716, #19376, .T. ) ;
#228285 = VECTOR ( 'NONE', #222468, 1000.000000000000114 ) ;
#228287 = AXIS2_PLACEMENT_3D ( 'NONE', #165764, #245287, #104452 ) ;
#228288 = DIRECTION ( 'NONE',  ( 0.000000000000000000, 0.000000000000000000, -1.000000000000000000 ) ) ;
#228289 = TOROIDAL_SURFACE ( 'NONE', #115849, 0.9750000000000019762, 0.1000000000000000056 ) ;
#228290 = CARTESIAN_POINT ( 'NONE',  ( -20.85000000000000142, 10.33248238083634440, -206.5948465439131496 ) ) ;
#228291 = EDGE_LOOP ( 'NONE', ( #36722, #201598, #23324, #145810 ) ) ;
#228292 = CONICAL_SURFACE ( 'NONE', #120177, 7.750000000000028422, 0.7853981633974531640 ) ;
#228293 = DIRECTION ( 'NONE',  ( -1.000000000000000000, 1.476360405086655403E-16, 0.000000000000000000 ) ) ;
#228294 = CARTESIAN_POINT ( 'NONE',  ( -20.54999999999999716, 7.150000000000000355, -12.34999999999999964 ) ) ;
#228295 = FACE_OUTER_BOUND ( 'NONE', #62717, .T. ) ;
#228296 = EDGE_LOOP ( 'NONE', ( #102972, #149951, #95178, #195081 ) ) ;
#228297 = CARTESIAN_POINT ( 'NONE',  ( -16.87368910959167678, 12.41706751708832357, -211.2038420430882013 ) ) ;
#228299 = ORIENTED_EDGE ( 'NONE', *, *, #179730, .T. ) ;
#228298 = CARTESIAN_POINT ( 'NONE',  ( 20.94999999999999929, -9.399999999988846611, -143.8939691226524644 ) ) ;
#228300 = DIRECTION ( 'NONE',  ( 0.000000000000000000, -0.3042567129660163627, -0.9525900758537824142 ) ) ;
#228301 = ADVANCED_FACE ( 'NONE', ( #216273 ), #206476, .T. ) ;
#228302 = CARTESIAN_POINT ( 'NONE',  ( -23.25000000000000000, 4.250000000011156409, -121.6500000000000341 ) ) ;
#228303 = ORIENTED_EDGE ( 'NONE', *, *, #45182, .F. ) ;
#228304 = CARTESIAN_POINT ( 'NONE',  ( 18.49999999999999289, 42.15997144203495139, -239.2817429668763793 ) ) ;
#228305 = CIRCLE ( 'NONE', #182523, 0.1000000000000072220 ) ;
#228306 = PRODUCT_CONTEXT ( 'NONE', #225608, 'mechanical' ) ;
#228307 = DIRECTION ( 'NONE',  ( 0.000000000000000000, 0.000000000000000000, 1.000000000000000000 ) ) ;
#228308 = CARTESIAN_POINT ( 'NONE',  ( -20.54999999999999716, 7.150000000011155876, -179.7499999999999716 ) ) ;
#228309 = CARTESIAN_POINT ( 'NONE',  ( 21.05000000000000071, 67.70174932746996888, -211.7710791003628401 ) ) ;
#228310 = VERTEX_POINT ( 'NONE', #257924 ) ;
#228311 = DIRECTION ( 'NONE',  ( -0.000000000000000000, 0.1298341882520022694, 0.9915357197604853789 ) ) ;
#228312 = FACE_OUTER_BOUND ( 'NONE', #187042, .T. ) ;
#228313 = DIRECTION ( 'NONE',  ( 0.000000000000000000, 0.000000000000000000, -1.000000000000000000 ) ) ;
#228314 = EDGE_CURVE ( 'NONE', #97822, #99579, #91449, .T. ) ;
#228315 = VERTEX_POINT ( 'NONE', #239708 ) ;
#228316 = EDGE_CURVE ( 'NONE', #142551, #118009, #100157, .T. ) ;
#228317 = ORIENTED_EDGE ( 'NONE', *, *, #116149, .F. ) ;
#228318 = DIRECTION ( 'NONE',  ( 1.000000000000000000, 0.000000000000000000, 0.000000000000000000 ) ) ;
#228319 = CARTESIAN_POINT ( 'NONE',  ( -16.89268316805466341, 44.12952801035616801, -235.2997120924900969 ) ) ;
#228320 = DIRECTION ( 'NONE',  ( 0.000000000000000000, 1.000000000000000000, 0.000000000000000000 ) ) ;
#228321 = CARTESIAN_POINT ( 'NONE',  ( 21.06277459767432703, 8.872862438279403463, -146.2039991923570881 ) ) ;
#228322 = ADVANCED_FACE ( 'NONE', ( #140587 ), #101419, .F. ) ;
#228324 = CARTESIAN_POINT ( 'NONE',  ( -13.40000000000000036, -9.650000000000005684, 12.40000000000000391 ) ) ;
#228323 = CARTESIAN_POINT ( 'NONE',  ( -20.94999999999999929, 7.021664781911246322, -204.6335654018972434 ) ) ;
#228325 = AXIS2_PLACEMENT_3D ( 'NONE', #101930, #21174, #64121 ) ;
#228326 = AXIS2_PLACEMENT_3D ( 'NONE', #161932, #1537, #160660 ) ;
#228328 = CARTESIAN_POINT ( 'NONE',  ( -21.11927991906891222, 75.99091632053855960, -176.4716006030158724 ) ) ;
#228327 = VECTOR ( 'NONE', #4614, 1000.000000000000000 ) ;
#228329 = CARTESIAN_POINT ( 'NONE',  ( 20.94999999999999929, 6.846123162363745074, -70.73772626684986164 ) ) ;
#228330 = CIRCLE ( 'NONE', #103390, 0.09999999999999939493 ) ;
#228331 = CARTESIAN_POINT ( 'NONE',  ( -18.46093223321744858, 47.00039116560562036, -255.3068790871464557 ) ) ;
#228333 = ORIENTED_EDGE ( 'NONE', *, *, #86590, .T. ) ;
#228332 = CARTESIAN_POINT ( 'NONE',  ( -23.25000000000000000, 67.85125148167622910, -227.9794913823769491 ) ) ;
#228334 = CARTESIAN_POINT ( 'NONE',  ( 21.10320863425824811, 69.59972261355321166, -170.0481297357515302 ) ) ;
#228335 = CARTESIAN_POINT ( 'NONE',  ( -21.13498764882296399, -1.380655549589986375, -194.6528078599425839 ) ) ;
#228337 = DIRECTION ( 'NONE',  ( 0.000000000000000000, 0.000000000000000000, -1.000000000000000000 ) ) ;
#228336 = DIRECTION ( 'NONE',  ( -1.000000000000000000, 0.000000000000000000, 0.000000000000000000 ) ) ;
#228338 = VERTEX_POINT ( 'NONE', #164022 ) ;
#228339 = CARTESIAN_POINT ( 'NONE',  ( 21.14999999999999858, 61.16604239671103471, -234.3115055913011417 ) ) ;
#228340 = CARTESIAN_POINT ( 'NONE',  ( 19.75857864376269291, 64.25000000001196554, -111.6731074845243796 ) ) ;
#228341 = DIRECTION ( 'NONE',  ( 1.000000000000000000, 0.000000000000000000, 0.000000000000000000 ) ) ;
#228342 = CARTESIAN_POINT ( 'NONE',  ( -21.05000000000000071, 69.74115727647277652, -103.0551211777124507 ) ) ;
#228343 = DIRECTION ( 'NONE',  ( -1.000000000000000000, -0.000000000000000000, -0.000000000000000000 ) ) ;
#228344 = ORIENTED_EDGE ( 'NONE', *, *, #235623, .T. ) ;
#228345 = ORIENTED_EDGE ( 'NONE', *, *, #4183, .T. ) ;
#228346 = ADVANCED_FACE ( 'NONE', ( #25787 ), #148306, .F. ) ;
#228347 = AXIS2_PLACEMENT_3D ( 'NONE', #95526, #172555, #73432 ) ;
#228349 = AXIS2_PLACEMENT_3D ( 'NONE', #34051, #171008, #112282 ) ;
#228348 = CARTESIAN_POINT ( 'NONE',  ( 21.05000000000000071, 10.42338541492406279, -174.9920519238700649 ) ) ;
#228350 = ORIENTED_EDGE ( 'NONE', *, *, #246861, .T. ) ;
#228351 = CARTESIAN_POINT ( 'NONE',  ( 18.39999999999999858, -9.499999999988842703, -73.60018939122203108 ) ) ;
#228352 = ORIENTED_EDGE ( 'NONE', *, *, #163865, .T. ) ;
#228354 = CARTESIAN_POINT ( 'NONE',  ( -1.820710678118658388, 83.26658958281765877, -214.6635725678450797 ) ) ;
#228353 = CIRCLE ( 'NONE', #74255, 0.1000000000000000472 ) ;
#228355 = DIRECTION ( 'NONE',  ( -0.000000000000000000, 1.000000000000000000, 0.000000000000000000 ) ) ;
#228356 = ADVANCED_FACE ( 'NONE', ( #85716 ), #227316, .T. ) ;
#228357 = CARTESIAN_POINT ( 'NONE',  ( -21.55000000000000426, 7.708578643773852157, -79.35000000000005116 ) ) ;
#228358 = ORIENTED_EDGE ( 'NONE', *, *, #87636, .F. ) ;
#228359 =( BOUNDED_SURFACE ( )  B_SPLINE_SURFACE ( 3, 2, ( 
 ( #194882, #18780, #159593 ),
 ( #59159, #60468, #74943 ),
 ( #97000, #56596, #98286 ),
 ( #140000, #176603, #219543 ),
 ( #17498, #120491, #177882 ),
 ( #16252, #95738, #257338 ),
 ( #175329, #254781, #218252 ),
 ( #14958, #76181, #136137 ),
 ( #94464, #174059, #185569 ),
 ( #6929, #3059, #82579 ) ),
 .UNSPECIFIED., .F., .F., .F. ) 
 B_SPLINE_SURFACE_WITH_KNOTS ( ( 4, 2, 2, 2, 4 ),
 ( 3, 3 ),
 ( 0.0001836757140119223738, 0.0004000170051583654498, 0.0005081876507315870014, 0.0005622729735181977500, 0.0006163582963048084987 ),
 ( 0.000000000000000000, 1.000000000000000000 ),
 .UNSPECIFIED. ) 
 GEOMETRIC_REPRESENTATION_ITEM ( )  RATIONAL_B_SPLINE_SURFACE ( (
 ( 1.000000000000000000, 0.7071067811865475727, 1.000000000000000000),
 ( 1.000000000000000000, 0.6461995200004808648, 1.000000000000000000),
 ( 1.000000000000000000, 0.5776453529583049917, 1.000000000000000000),
 ( 1.000000000000000000, 0.4585233068334871875, 1.000000000000000000),
 ( 1.000000000000000000, 0.4154092989933438895, 1.000000000000000000),
 ( 1.000000000000000000, 0.3550093145839735009, 1.000000000000000000),
 ( 1.000000000000000000, 0.3354498651682673582, 1.000000000000000000),
 ( 1.000000000000000000, 0.3060347992259510042, 1.000000000000000000),
 ( 1.000000000000000000, 0.2963555829621785653, 1.000000000000000000),
 ( 1.000000000000000000, 0.2966190024561813354, 1.000000000000000000) ) ) 
 REPRESENTATION_ITEM ( '' )  SURFACE ( )  );
#228360 = ADVANCED_FACE ( 'NONE', ( #165297, #146999, #24528 ), #183583, .F. ) ;
#228362 = ADVANCED_FACE ( 'NONE', ( #47903, #162749 ), #205694, .T. ) ;
#228361 = LINE ( 'NONE', #182835, #211988 ) ;
#228363 = CARTESIAN_POINT ( 'NONE',  ( -18.50000000000000000, 68.00417547777209393, -224.2303273613012777 ) ) ;
#228364 = FACE_OUTER_BOUND ( 'NONE', #8541, .T. ) ;
#228365 = DIRECTION ( 'NONE',  ( -1.000000000000000000, -0.000000000000000000, -0.000000000000000000 ) ) ;
#228366 = CARTESIAN_POINT ( 'NONE',  ( 21.00000000000000000, 7.800000000000000711, 0.000000000000000000 ) ) ;
#228367 = CARTESIAN_POINT ( 'NONE',  ( 21.05000000000000071, 36.02367271998545561, -235.8812521208699309 ) ) ;
#228368 = AXIS2_PLACEMENT_3D ( 'NONE', #3411, #161232, #101198 ) ;
#228369 = VERTEX_POINT ( 'NONE', #184850 ) ;
#228371 = DIRECTION ( 'NONE',  ( -1.000000000000000000, 3.265361837132813093E-16, 2.280189983783949500E-30 ) ) ;
#228370 = CARTESIAN_POINT ( 'NONE',  ( -16.81744102076749314, 66.05000000001207638, -123.8731074845243683 ) ) ;
#228373 = ORIENTED_EDGE ( 'NONE', *, *, #111590, .F. ) ;
#228372 = AXIS2_PLACEMENT_3D ( 'NONE', #125215, #123940, #86045 ) ;
#228375 = VERTEX_POINT ( 'NONE', #106583 ) ;
#228374 = CARTESIAN_POINT ( 'NONE',  ( 19.75857864376268935, 11.65000000001115943, -58.35000000000000142 ) ) ;
#228376 = AXIS2_PLACEMENT_3D ( 'NONE', #203309, #3819, #145884 ) ;
#228377 = EDGE_CURVE ( 'NONE', #95061, #117567, #144419, .T. ) ;
#228378 = ORIENTED_EDGE ( 'NONE', *, *, #157854, .F. ) ;
#228379 = CYLINDRICAL_SURFACE ( 'NONE', #44772, 0.09999999999999939493 ) ;
#228380 = EDGE_CURVE ( 'NONE', #153937, #144828, #246125, .T. ) ;
#228381 = CARTESIAN_POINT ( 'NONE',  ( -18.40000000000000213, 11.48667500176882328, -176.7499999999999716 ) ) ;
#228382 = DIRECTION ( 'NONE',  ( 0.000000000000000000, 0.000000000000000000, 1.000000000000000000 ) ) ;
#228383 = CARTESIAN_POINT ( 'NONE',  ( -20.85000000000000142, 67.76783854423860021, -227.9206834886612114 ) ) ;
#228384 = ORIENTED_EDGE ( 'NONE', *, *, #207080, .F. ) ;
#228385 = DIRECTION ( 'NONE',  ( 1.000000000000000000, 0.000000000000000000, 0.000000000000000000 ) ) ;
#228386 = AXIS2_PLACEMENT_3D ( 'NONE', #201066, #58955, #216772 ) ;
#228388 = EDGE_CURVE ( 'NONE', #611, #177234, #143923, .T. ) ;
#228387 = CARTESIAN_POINT ( 'NONE',  ( 21.72449340488910252, 43.99894805634765760, -234.9941606142489832 ) ) ;
#228389 = ORIENTED_EDGE ( 'NONE', *, *, #199870, .T. ) ;
#228390 = CARTESIAN_POINT ( 'NONE',  ( -16.93301857435213620, 9.976309354746611291, -154.8857755711614459 ) ) ;
#228391 = ADVANCED_FACE ( 'NONE', ( #204409 ), #85629, .F. ) ;
#228392 = FACE_OUTER_BOUND ( 'NONE', #127424, .T. ) ;
#228393 = CIRCLE ( 'NONE', #66052, 11.65000000000000746 ) ;
#228394 = ORIENTED_EDGE ( 'NONE', *, *, #222018, .F. ) ;
#228395 = VECTOR ( 'NONE', #245563, 1000.000000000000114 ) ;
#228396 = DIRECTION ( 'NONE',  ( 0.000000000000000000, 0.000000000000000000, 1.000000000000000000 ) ) ;
#228397 = EDGE_CURVE ( 'NONE', #219738, #149939, #247387, .T. ) ;
#228398 = EDGE_CURVE ( 'NONE', #232467, #147343, #77288, .T. ) ;
#228399 = AXIS2_PLACEMENT_3D ( 'NONE', #167483, #164892, #26684 ) ;
#228400 = ORIENTED_EDGE ( 'NONE', *, *, #253681, .F. ) ;
#228401 = CARTESIAN_POINT ( 'NONE',  ( 18.57399277249656322, 65.66887361445331805, -97.43298459182690863 ) ) ;
#228403 = VERTEX_POINT ( 'NONE', #182310 ) ;
#228402 = AXIS2_PLACEMENT_3D ( 'NONE', #14432, #172240, #187917 ) ;
#228404 = CARTESIAN_POINT ( 'NONE',  ( 20.73486653747090003, 7.250000000011182166, -154.8500000000000227 ) ) ;
#228405 = EDGE_CURVE ( 'NONE', #225834, #19166, #64816, .T. ) ;
#228406 = CARTESIAN_POINT ( 'NONE',  ( 20.87155475150661132, 64.25000000001175238, -76.42752095536712886 ) ) ;
#228407 = DIRECTION ( 'NONE',  ( 0.000000000000000000, 0.1575844902526876978, 0.9875055080513731598 ) ) ;
#228408 = DIRECTION ( 'NONE',  ( 0.000000000000000000, 0.000000000000000000, -1.000000000000000000 ) ) ;
#228409 = EDGE_CURVE ( 'NONE', #85564, #97821, #19025, .T. ) ;
#228410 = B_SPLINE_CURVE_WITH_KNOTS ( 'NONE', 3,
 ( #132934, #192901, #114638, #50788 ),
 .UNSPECIFIED., .F., .F.,
 ( 4, 4 ),
 ( 0.000000000000000000, 7.713889350930586977E-05 ),
 .UNSPECIFIED. ) ;
#228411 = VECTOR ( 'NONE', #50930, 1000.000000000000114 ) ;
#228412 = EDGE_CURVE ( 'NONE', #154251, #87157, #124896, .T. ) ;
#228413 = EDGE_CURVE ( 'NONE', #48651, #63775, #203136, .T. ) ;
#228414 = AXIS2_PLACEMENT_3D ( 'NONE', #45862, #142392, #220659 ) ;
#228415 = DIRECTION ( 'NONE',  ( -0.000000000000000000, -0.000000000000000000, -1.000000000000000000 ) ) ;
#228416 = CARTESIAN_POINT ( 'NONE',  ( 23.24999999999999289, 30.38404434817536881, -239.4399867032565794 ) ) ;
#228417 = VERTEX_POINT ( 'NONE', #206995 ) ;
#228418 = DIRECTION ( 'NONE',  ( 1.000000000000000000, -0.000000000000000000, 0.000000000000000000 ) ) ;
#228419 = ORIENTED_EDGE ( 'NONE', *, *, #57050, .T. ) ;
#228420 = LINE ( 'NONE', #190584, #25336 ) ;
#228421 = VECTOR ( 'NONE', #130706, 1000.000000000000114 ) ;
#228422 = EDGE_LOOP ( 'NONE', ( #109822, #89784, #47645, #104396 ) ) ;
#228423 = VECTOR ( 'NONE', #74416, 1000.000000000000000 ) ;
#228424 = CIRCLE ( 'NONE', #195108, 11.65000000000000036 ) ;
#228425 = DIRECTION ( 'NONE',  ( -0.000000000000000000, -0.000000000000000000, 1.000000000000000000 ) ) ;
#228426 = AXIS2_PLACEMENT_3D ( 'NONE', #143093, #146943, #86960 ) ;
#228427 = FACE_OUTER_BOUND ( 'NONE', #92311, .T. ) ;
#228428 = FACE_OUTER_BOUND ( 'NONE', #61367, .T. ) ;
#228429 = EDGE_LOOP ( 'NONE', ( #40607, #99155, #50404, #119030 ) ) ;
#228431 = ORIENTED_EDGE ( 'NONE', *, *, #45031, .F. ) ;
#228430 = DIRECTION ( 'NONE',  ( -1.000000000000000000, -0.000000000000000000, -0.000000000000000000 ) ) ;
#228432 = ADVANCED_FACE ( 'NONE', ( #28394 ), #114305, .F. ) ;
#228433 = CIRCLE ( 'NONE', #174293, 12.77500000000000036 ) ;
#228434 = DIRECTION ( 'NONE',  ( 0.000000000000000000, 0.000000000000000000, -1.000000000000000000 ) ) ;
#228436 = PLANE ( 'NONE',  #113297 ) ;
#228435 = CARTESIAN_POINT ( 'NONE',  ( -18.59999999999999787, 74.98773774893902555, -233.8732236541320333 ) ) ;
#228438 = ORIENTED_EDGE ( 'NONE', *, *, #76527, .T. ) ;
#228437 = DIRECTION ( 'NONE',  ( 0.000000000000000000, 0.000000000000000000, 1.000000000000000000 ) ) ;
#228439 = PRODUCT ( 'Injection Molded Chain Links 2', 'Injection Molded Chain Links 2', '', ( #177348 ) ) ;
#228440 = ORIENTED_EDGE ( 'NONE', *, *, #215098, .T. ) ;
#228441 = VECTOR ( 'NONE', #225832, 1000.000000000000114 ) ;
#228442 = AXIS2_PLACEMENT_3D ( 'NONE', #144896, #23720, #161933 ) ;
#228443 = CARTESIAN_POINT ( 'NONE',  ( -21.05000000000000071, 0.6869237119019852011, -212.7787591058053067 ) ) ;
#228444 = CYLINDRICAL_SURFACE ( 'NONE', #242796, 0.1000000000000028644 ) ;
#228445 = ORIENTED_EDGE ( 'NONE', *, *, #106269, .F. ) ;
#228446 = SPHERICAL_SURFACE ( 'NONE', #205897, 0.1000000000000000056 ) ;
#228447 = VERTEX_POINT ( 'NONE', #193854 ) ;
#228448 = CARTESIAN_POINT ( 'NONE',  ( 21.07928932188134397, 67.23127455305841238, -235.8551265064783991 ) ) ;
#228449 = DIRECTION ( 'NONE',  ( -0.000000000000000000, -0.000000000000000000, -1.000000000000000000 ) ) ;
#228450 = ORIENTED_EDGE ( 'NONE', *, *, #196112, .F. ) ;
#228451 = CARTESIAN_POINT ( 'NONE',  ( 23.14999999999999503, 11.65000000001116298, -188.8499999999999659 ) ) ;
#228452 = VECTOR ( 'NONE', #253573, 1000.000000000000000 ) ;
#228453 = AXIS2_PLACEMENT_3D ( 'NONE', #13376, #92890, #172495 ) ;
#228454 = ADVANCED_FACE ( 'NONE', ( #209561 ), #54320, .T. ) ;
#228456 = EDGE_LOOP ( 'NONE', ( #125394, #233627, #206518 ) ) ;
#228455 = CIRCLE ( 'NONE', #7885, 0.09999999999999344136 ) ;
#228458 = EDGE_CURVE ( 'NONE', #115551, #170938, #39907, .T. ) ;
#228457 = DIRECTION ( 'NONE',  ( -1.000000000000000000, -0.000000000000000000, -0.000000000000000000 ) ) ;
#228459 = AXIS2_PLACEMENT_3D ( 'NONE', #132983, #71727, #31339 ) ;
#228460 = ORIENTED_EDGE ( 'NONE', *, *, #17066, .T. ) ;
#228461 = ORIENTED_EDGE ( 'NONE', *, *, #44673, .T. ) ;
#228462 = CARTESIAN_POINT ( 'NONE',  ( -18.50000000000000000, -9.421290279511815413, -73.82388217902615679 ) ) ;
#228463 = VERTEX_POINT ( 'NONE', #253802 ) ;
#228464 = CARTESIAN_POINT ( 'NONE',  ( 23.04999999999999716, 55.18266668263805030, -231.5853321237989633 ) ) ;
#228465 = ORIENTED_EDGE ( 'NONE', *, *, #238385, .F. ) ;
#228467 = ORIENTED_EDGE ( 'NONE', *, *, #115052, .T. ) ;
#228466 = DIRECTION ( 'NONE',  ( -1.836970198721029934E-16, -1.000000000000000000, -6.982962677686266711E-15 ) ) ;
#228468 = CIRCLE ( 'NONE', #65564, 0.1999999999999987899 ) ;
#228469 = CARTESIAN_POINT ( 'NONE',  ( -18.59999999999999787, 7.021664781900089913, -37.33356540189728889 ) ) ;
#228470 = EDGE_LOOP ( 'NONE', ( #19411, #214122, #121931, #171403 ) ) ;
#228471 = DIRECTION ( 'NONE',  ( 1.000000000000000000, 0.000000000000000000, 0.000000000000000000 ) ) ;
#228472 = VECTOR ( 'NONE', #68567, 1000.000000000000000 ) ;
#228473 = EDGE_LOOP ( 'NONE', ( #221923, #27097, #184820, #82630, #199511 ) ) ;
#228476 = VERTEX_POINT ( 'NONE', #231705 ) ;
#228475 = EDGE_LOOP ( 'NONE', ( #80989, #43530, #202748, #204627, #233342, #168632, #42603, #174318, #216566, #97717, #14815, #76355, #97988, #255689, #221661, #164453, #30022, #227237 ) ) ;
#228474 = CARTESIAN_POINT ( 'NONE',  ( -16.93230518875208190, 65.99924963859173488, -56.94732913642289418 ) ) ;
#228477 = CARTESIAN_POINT ( 'NONE',  ( 18.49999999999999645, -1.162701749926855266, -175.5999999999999659 ) ) ;
#228478 = AXIS2_PLACEMENT_3D ( 'NONE', #178599, #174768, #18215 ) ;
#228479 = ADVANCED_FACE ( 'NONE', ( #93446 ), #208291, .F. ) ;
#228480 = LINE ( 'NONE', #70702, #102410 ) ;
#228481 = ORIENTED_EDGE ( 'NONE', *, *, #40341, .F. ) ;
#228482 = EDGE_LOOP ( 'NONE', ( #251641, #148682, #38744, #102165 ) ) ;
#228483 = PLANE ( 'NONE',  #86954 ) ;
#228484 = CYLINDRICAL_SURFACE ( 'NONE', #151476, 7.899999999999990585 ) ;
#228486 = ORIENTED_EDGE ( 'NONE', *, *, #211791, .F. ) ;
#228485 = CARTESIAN_POINT ( 'NONE',  ( -18.59999999999999787, -11.65000000000000036, 30.09999999999999787 ) ) ;
#228487 = CARTESIAN_POINT ( 'NONE',  ( 21.14999999999999858, 22.16427325743960708, -231.8189304678590190 ) ) ;
#228488 = ORIENTED_EDGE ( 'NONE', *, *, #176655, .F. ) ;
#228489 = DIRECTION ( 'NONE',  ( -1.000000000000000000, 0.000000000000000000, 0.000000000000000000 ) ) ;
#228490 = FACE_OUTER_BOUND ( 'NONE', #170949, .T. ) ;
#228491 = AXIS2_PLACEMENT_3D ( 'NONE', #143038, #86911, #226420 ) ;
#228492 = ORIENTED_EDGE ( 'NONE', *, *, #173760, .T. ) ;
#228493 = DIRECTION ( 'NONE',  ( 1.000000000000000000, 0.000000000000000000, 0.000000000000000000 ) ) ;
#228494 = CARTESIAN_POINT ( 'NONE',  ( 18.59999999999999076, 6.450000000000001066, -10.01702717044002000 ) ) ;
#228495 = ORIENTED_EDGE ( 'NONE', *, *, #111469, .T. ) ;
#228497 = ORIENTED_EDGE ( 'NONE', *, *, #136276, .F. ) ;
#228496 = LINE ( 'NONE', #49836, #151599 ) ;
#228498 = FACE_OUTER_BOUND ( 'NONE', #6522, .T. ) ;
#228500 = ORIENTED_EDGE ( 'NONE', *, *, #255090, .T. ) ;
#228499 = VERTEX_POINT ( 'NONE', #94737 ) ;
#228501 = ORIENTED_EDGE ( 'NONE', *, *, #168203, .F. ) ;
#228502 = ORIENTED_EDGE ( 'NONE', *, *, #14011, .T. ) ;
#228503 = ORIENTED_EDGE ( 'NONE', *, *, #92015, .T. ) ;
#228504 = DIRECTION ( 'NONE',  ( -0.000000000000000000, 7.272083257015735086E-15, -1.000000000000000000 ) ) ;
#228505 = ORIENTED_EDGE ( 'NONE', *, *, #174502, .F. ) ;
#228506 = CYLINDRICAL_SURFACE ( 'NONE', #214642, 11.74999999999999289 ) ;
#228507 = CARTESIAN_POINT ( 'NONE',  ( -23.25000000000000000, 77.16412189325286874, -61.60825939895269698 ) ) ;
#228508 = EDGE_CURVE ( 'NONE', #68874, #220110, #243837, .T. ) ;
#228509 = VERTEX_POINT ( 'NONE', #154743 ) ;
#228510 = EDGE_CURVE ( 'NONE', #51418, #210814, #49196, .T. ) ;
#228511 = EDGE_LOOP ( 'NONE', ( #209784, #223260, #140999, #218656 ) ) ;
#228512 = VECTOR ( 'NONE', #74429, 1000.000000000000000 ) ;
#228513 = CARTESIAN_POINT ( 'NONE',  ( -20.94999999999999929, 1.116121084443477685E-11, -170.3999999999999488 ) ) ;
#228514 = VECTOR ( 'NONE', #203611, 1000.000000000000114 ) ;
#228515 = ORIENTED_EDGE ( 'NONE', *, *, #249904, .T. ) ;
#228516 = EDGE_CURVE ( 'NONE', #241603, #156110, #35799, .T. ) ;
#228517 = VECTOR ( 'NONE', #159634, 1000.000000000000000 ) ;
#228518 = DIRECTION ( 'NONE',  ( 1.000000000000000000, 0.000000000000000000, -0.000000000000000000 ) ) ;
#228519 = ORIENTED_EDGE ( 'NONE', *, *, #12578, .F. ) ;
#228520 = FACE_OUTER_BOUND ( 'NONE', #36971, .T. ) ;
#228523 = EDGE_CURVE ( 'NONE', #72835, #3545, #69121, .T. ) ;
#228522 = ORIENTED_EDGE ( 'NONE', *, *, #203732, .T. ) ;
#228521 = DIRECTION ( 'NONE',  ( -0.7071067811865882069, -0.3338907855510964140, -0.6233112732207032325 ) ) ;
#228524 = DIRECTION ( 'NONE',  ( -1.000000000000000000, -1.394253735153569469E-16, -2.602809386958778209E-16 ) ) ;
#228525 = DIRECTION ( 'NONE',  ( -0.7071067811865474617, -0.6909108974501236844, -0.1504730267678055788 ) ) ;
#228526 = EDGE_CURVE ( 'NONE', #93557, #105209, #169181, .T. ) ;
#228527 = CARTESIAN_POINT ( 'NONE',  ( -23.15000000000000213, 62.42906104934358069, -247.8683112431566258 ) ) ;
#228528 = DIRECTION ( 'NONE',  ( 0.000000000000000000, 0.000000000000000000, -1.000000000000000000 ) ) ;
#228529 = DIRECTION ( 'NONE',  ( 0.000000000000000000, -6.938893903907222067E-15, 1.000000000000000000 ) ) ;
#228531 = CARTESIAN_POINT ( 'NONE',  ( -20.94999999999999929, 68.92903212821327941, -132.7765432626560766 ) ) ;
#228530 = CIRCLE ( 'NONE', #120226, 0.09999999999999939493 ) ;
#228533 = CARTESIAN_POINT ( 'NONE',  ( 21.76363531954645936, 10.35302234425203949, -227.5040830337958937 ) ) ;
#228532 = AXIS2_PLACEMENT_3D ( 'NONE', #74330, #228242, #132997 ) ;
#228534 = AXIS2_PLACEMENT_3D ( 'NONE', #33753, #92382, #254020 ) ;
#228535 = EDGE_CURVE ( 'NONE', #155707, #193211, #248172, .T. ) ;
#228536 = DIRECTION ( 'NONE',  ( -0.7071067811865475727, 0.2890913453342130457, -0.6453109281988448354 ) ) ;
#228537 = EDGE_LOOP ( 'NONE', ( #177583, #255713, #14669, #177070 ) ) ;
#228538 = CIRCLE ( 'NONE', #57812, 0.09999999999999609201 ) ;
#228539 = EDGE_LOOP ( 'NONE', ( #55113, #16557, #204500, #12636 ) ) ;
#228541 = ORIENTED_EDGE ( 'NONE', *, *, #237402, .F. ) ;
#228540 = DIRECTION ( 'NONE',  ( -1.000000000000000000, -0.000000000000000000, -0.000000000000000000 ) ) ;
#228542 = ORIENTED_EDGE ( 'NONE', *, *, #130505, .F. ) ;
#228544 = EDGE_CURVE ( 'NONE', #239499, #67751, #156449, .T. ) ;
#228543 = DIRECTION ( 'NONE',  ( 1.000000000000000000, 0.000000000000000000, 0.000000000000000000 ) ) ;
#228545 = FACE_OUTER_BOUND ( 'NONE', #43805, .T. ) ;
#228547 = FACE_OUTER_BOUND ( 'NONE', #174666, .T. ) ;
#228546 = CARTESIAN_POINT ( 'NONE',  ( 20.11144452913953273, 39.79843846208498093, -237.2598321417979150 ) ) ;
#228548 = ORIENTED_EDGE ( 'NONE', *, *, #234307, .F. ) ;
#228549 = EDGE_LOOP ( 'NONE', ( #186752, #220239, #232012, #146942 ) ) ;
#228550 = LINE ( 'NONE', #129437, #129248 ) ;
#228551 = FACE_OUTER_BOUND ( 'NONE', #118787, .T. ) ;
#228552 = ORIENTED_EDGE ( 'NONE', *, *, #239821, .T. ) ;
#228553 = ORIENTED_EDGE ( 'NONE', *, *, #137639, .T. ) ;
#228554 = VECTOR ( 'NONE', #177208, 1000.000000000000000 ) ;
#228555 = AXIS2_PLACEMENT_3D ( 'NONE', #141726, #25643, #161317 ) ;
#228556 = CARTESIAN_POINT ( 'NONE',  ( -23.25000000000000000, 1.115600667400684642E-11, -204.8999999999999488 ) ) ;
#228557 = CARTESIAN_POINT ( 'NONE',  ( -23.25000000000000000, 1.115650265596050101E-11, -62.95000000000004547 ) ) ;
#228558 = DIRECTION ( 'NONE',  ( 0.000000000000000000, -1.265107689135680095E-16, 1.000000000000000000 ) ) ;
#228559 = CARTESIAN_POINT ( 'NONE',  ( 21.05000000000000071, 65.31570632562490175, -61.99643354588710054 ) ) ;
#228560 = CARTESIAN_POINT ( 'NONE',  ( -21.14999999999999503, 64.25000000001233502, -163.1039602385656337 ) ) ;
#228562 = ORIENTED_EDGE ( 'NONE', *, *, #122809, .F. ) ;
#228561 = CARTESIAN_POINT ( 'NONE',  ( 22.39999999999999858, 0.1000000000111554016, -126.2092204016266379 ) ) ;
#228563 = AXIS2_PLACEMENT_3D ( 'NONE', #66246, #205741, #28440 ) ;
#228564 = CARTESIAN_POINT ( 'NONE',  ( -23.15000000000000213, 74.00000000001229239, -156.7984855617622770 ) ) ;
#228565 = FACE_OUTER_BOUND ( 'NONE', #220648, .T. ) ;
#228566 = DIRECTION ( 'NONE',  ( 1.000000000000000000, 0.000000000000000000, -0.000000000000000000 ) ) ;
#228567 = CARTESIAN_POINT ( 'NONE',  ( 18.51997666896863137, 85.39233213153069357, -95.87970129704063993 ) ) ;
#228568 = VERTEX_POINT ( 'NONE', #129998 ) ;
#228569 = DIRECTION ( 'NONE',  ( 1.000000000000000000, 0.000000000000000000, 0.000000000000000000 ) ) ;
#228571 = CARTESIAN_POINT ( 'NONE',  ( -16.87036670365548474, 66.01058118071036063, -115.5435473672223168 ) ) ;
#228570 = CARTESIAN_POINT ( 'NONE',  ( 23.40000000000005187, 79.88763423575340994, -7.282924647898262549 ) ) ;
#228572 = CARTESIAN_POINT ( 'NONE',  ( -21.05000000000000071, 68.22930980752001062, -227.7331931781284879 ) ) ;
#228573 = CARTESIAN_POINT ( 'NONE',  ( 18.49999999999999645, 0.000000000000000000, -33.50000000000000000 ) ) ;
#228574 = CARTESIAN_POINT ( 'NONE',  ( -18.59999999999999787, 0.6869237119019839799, -212.7787591058053067 ) ) ;
#228575 = CARTESIAN_POINT ( 'NONE',  ( -21.05000000000000071, -1.835341550213255957, -145.5551512925629822 ) ) ;
#228576 = AXIS2_PLACEMENT_3D ( 'NONE', #192230, #154414, #250889 ) ;
#228577 = AXIS2_PLACEMENT_3D ( 'NONE', #7939, #224392, #165740 ) ;
#228578 = CARTESIAN_POINT ( 'NONE',  ( -21.05000000000000071, 0.000000000000000000, 0.000000000000000000 ) ) ;
#228579 = CARTESIAN_POINT ( 'NONE',  ( -21.12230431290520016, 69.54243334671915022, -136.5283173362133482 ) ) ;
#228580 = ORIENTED_EDGE ( 'NONE', *, *, #204204, .T. ) ;
#228581 = ADVANCED_FACE ( 'NONE', ( #30955 ), #164959, .T. ) ;
#228582 = AXIS2_PLACEMENT_3D ( 'NONE', #28580, #108067, #130176 ) ;
#228583 = ORIENTED_EDGE ( 'NONE', *, *, #80459, .F. ) ;
#228584 = VERTEX_POINT ( 'NONE', #71352 ) ;
#228585 = CARTESIAN_POINT ( 'NONE',  ( 20.22483756094572271, 66.49809532114012711, -94.88356835580994186 ) ) ;
#228586 = DIRECTION ( 'NONE',  ( 0.000000000000000000, -0.9770955615653551529, -0.2128009952262517601 ) ) ;
#228587 = ORIENTED_EDGE ( 'NONE', *, *, #202443, .T. ) ;
#228588 = EDGE_CURVE ( 'NONE', #114955, #203670, #131298, .T. ) ;
#228589 = VECTOR ( 'NONE', #104187, 1000.000000000000000 ) ;
#228590 = ORIENTED_EDGE ( 'NONE', *, *, #128741, .T. ) ;
#228591 = EDGE_CURVE ( 'NONE', #171099, #250586, #148408, .T. ) ;
#228592 = EDGE_CURVE ( 'NONE', #20544, #89909, #27638, .T. ) ;
#228593 = VECTOR ( 'NONE', #10297, 1000.000000000000000 ) ;
#228594 = ORIENTED_EDGE ( 'NONE', *, *, #186894, .T. ) ;
#228595 = DIRECTION ( 'NONE',  ( 0.000000000000000000, 0.000000000000000000, 1.000000000000000000 ) ) ;
#228596 = ORIENTED_EDGE ( 'NONE', *, *, #202095, .F. ) ;
#228597 = CIRCLE ( 'NONE', #203646, 0.1000000000000028227 ) ;
#228598 = CARTESIAN_POINT ( 'NONE',  ( 18.49999999999999645, 28.08990005499213538, -254.8141779806076670 ) ) ;
#228599 = AXIS2_PLACEMENT_3D ( 'NONE', #220318, #242426, #63802 ) ;
#228600 = CIRCLE ( 'NONE', #241081, 0.4999999999999892308 ) ;
#228601 = DIRECTION ( 'NONE',  ( -2.952720810173289112E-16, -0.4088369013363281068, 0.9126074666063770380 ) ) ;
#228602 = DIRECTION ( 'NONE',  ( -1.000000000000000000, 2.849773892568378313E-16, -7.728835255496647986E-17 ) ) ;
#228603 = CIRCLE ( 'NONE', #249451, 0.09999999999999632794 ) ;
#228604 = FACE_OUTER_BOUND ( 'NONE', #142200, .T. ) ;
#228605 = DIRECTION ( 'NONE',  ( -0.7071067811865475727, 0.7071067811865475727, 4.937700262164531476E-15 ) ) ;
#228607 = ORIENTED_EDGE ( 'NONE', *, *, #216633, .F. ) ;
#228606 = DIRECTION ( 'NONE',  ( 0.000000000000000000, -0.2128009952263604232, 0.9770955615653316162 ) ) ;
#228609 = DIRECTION ( 'NONE',  ( 0.000000000000000000, -6.982962677686266711E-15, 1.000000000000000000 ) ) ;
#228608 = CARTESIAN_POINT ( 'NONE',  ( -18.59999999999999787, 85.40000000001204228, -129.2258477248609552 ) ) ;
#228610 = EDGE_CURVE ( 'NONE', #25144, #218493, #115080, .T. ) ;
#228611 = CIRCLE ( 'NONE', #24618, 0.1000000000000106498 ) ;
#228612 = CARTESIAN_POINT ( 'NONE',  ( -16.87304349924914604, 9.961745077968330975, -154.8890666750452567 ) ) ;
#228613 = ORIENTED_EDGE ( 'NONE', *, *, #33126, .T. ) ;
#228614 = CARTESIAN_POINT ( 'NONE',  ( -18.59999999999999787, 0.6656436123793491033, -212.6810495496487476 ) ) ;
#228615 = DIRECTION ( 'NONE',  ( -1.000000000000000000, -0.000000000000000000, -0.000000000000000000 ) ) ;
#228617 = EDGE_CURVE ( 'NONE', #14186, #75721, #20367, .T. ) ;
#228616 = LINE ( 'NONE', #26566, #175001 ) ;
#228618 = ORIENTED_EDGE ( 'NONE', *, *, #215196, .T. ) ;
#228619 = FACE_OUTER_BOUND ( 'NONE', #224153, .T. ) ;
#228620 = PRODUCT_DEFINITION ( 'UNKNOWN', '', #186339, #214892 ) ;
#228621 = ADVANCED_BREP_SHAPE_REPRESENTATION ( '', ( #193366, #2425 ), #35604 ) ;
#228622 = FACE_OUTER_BOUND ( 'NONE', #209478, .T. ) ;
#228623 = AXIS2_PLACEMENT_3D ( 'NONE', #210807, #174300, #175554 ) ;
#228625 = ORIENTED_EDGE ( 'NONE', *, *, #113986, .T. ) ;
#228624 = AXIS2_PLACEMENT_3D ( 'NONE', #77557, #3165, #141406 ) ;
#228626 = DIRECTION ( 'NONE',  ( 0.000000000000000000, 0.000000000000000000, -1.000000000000000000 ) ) ;
#228627 = PLANE ( 'NONE',  #74375 ) ;
#228628 = ADVANCED_FACE ( 'NONE', ( #98547 ), #81562, .T. ) ;
#228629 = DIRECTION ( 'NONE',  ( 0.000000000000000000, -6.982962677686267499E-15, 1.000000000000000000 ) ) ;
#228630 = DIRECTION ( 'NONE',  ( 0.000000000000000000, 0.2128009952263608395, -0.9770955615653315052 ) ) ;
#228631 = ADVANCED_FACE ( 'NONE', ( #58159 ), #235863, .T. ) ;
#228632 = ORIENTED_EDGE ( 'NONE', *, *, #213544, .T. ) ;
#228633 = EDGE_CURVE ( 'NONE', #182341, #232170, #176874, .T. ) ;
#228634 = ORIENTED_EDGE ( 'NONE', *, *, #45645, .T. ) ;
#228635 = B_SPLINE_CURVE_WITH_KNOTS ( 'NONE', 3,
 ( #63181, #85297, #244392, #140145, #145287, #61916, #100984 ),
 .UNSPECIFIED., .F., .F.,
 ( 4, 3, 4 ),
 ( 0.000000000000000000, 3.882884552234470657E-05, 5.798605692158490785E-05 ),
 .UNSPECIFIED. ) ;
#228636 = CIRCLE ( 'NONE', #186948, 11.64999999999999325 ) ;
#228637 = AXIS2_PLACEMENT_3D ( 'NONE', #208834, #189279, #10638 ) ;
#228638 = CARTESIAN_POINT ( 'NONE',  ( -20.94999999999999929, 77.16270174995034381, -162.0231074845243313 ) ) ;
#228639 = FACE_OUTER_BOUND ( 'NONE', #131226, .T. ) ;
#228640 = CARTESIAN_POINT ( 'NONE',  ( -21.05000000000000071, 65.61575147395463148, -242.1939180743342774 ) ) ;
#228641 = CARTESIAN_POINT ( 'NONE',  ( -20.54999999999999716, 85.40000000001158753, -59.62913836187181715 ) ) ;
#228642 = VECTOR ( 'NONE', #51920, 1000.000000000000000 ) ;
#228644 = DIRECTION ( 'NONE',  ( 0.000000000000000000, -0.9126074666063780372, -0.4088369013363258309 ) ) ;
#228643 = DIRECTION ( 'NONE',  ( 0.000000000000000000, -1.000000000000000000, -6.982962677686266711E-15 ) ) ;
#228645 = CARTESIAN_POINT ( 'NONE',  ( 21.15000000000005542, 87.50449464844290048, -37.85861909827351468 ) ) ;
#228646 = DIRECTION ( 'NONE',  ( 1.000000000000000000, 0.000000000000000000, 0.000000000000000000 ) ) ;
#228647 = DIRECTION ( 'NONE',  ( -1.020425574104004196E-15, -6.982962677686266711E-15, 1.000000000000000000 ) ) ;
#228648 = ORIENTED_EDGE ( 'NONE', *, *, #99944, .F. ) ;
#228649 = CARTESIAN_POINT ( 'NONE',  ( -20.93302460841142931, 65.68434038414356735, -97.48668807260655456 ) ) ;
#228650 = CIRCLE ( 'NONE', #232739, 4.049999999999998046 ) ;
#228652 = ORIENTED_EDGE ( 'NONE', *, *, #235370, .T. ) ;
#228651 = DIRECTION ( 'NONE',  ( 0.000000000000000000, 6.982962677686266711E-15, -1.000000000000000000 ) ) ;
#228653 = CARTESIAN_POINT ( 'NONE',  ( 18.49999999999999289, 65.67426406872445455, -178.6731074845244223 ) ) ;
#228654 = DIRECTION ( 'NONE',  ( 1.000000000000000000, 0.000000000000000000, 0.000000000000000000 ) ) ;
#228655 = FACE_OUTER_BOUND ( 'NONE', #80495, .T. ) ;
#228656 = SPHERICAL_SURFACE ( 'NONE', #138884, 0.1000000000000000056 ) ;
#228657 = DIRECTION ( 'NONE',  ( 0.000000000000000000, 0.000000000000000000, 1.000000000000000000 ) ) ;
#228659 = EDGE_LOOP ( 'NONE', ( #244004, #2475, #82134 ) ) ;
#228658 = DIRECTION ( 'NONE',  ( -3.469446951953515108E-14, -1.000000000000000000, 0.000000000000000000 ) ) ;
#228660 = DIRECTION ( 'NONE',  ( 0.000000000000000000, 0.000000000000000000, -1.000000000000000000 ) ) ;
#228661 = CARTESIAN_POINT ( 'NONE',  ( -16.84419801905645997, 51.60107635300602169, -231.9544371839865562 ) ) ;
#228662 = DIRECTION ( 'NONE',  ( -0.000000000000000000, 1.000000000000000000, 1.626303258728266709E-15 ) ) ;
#228663 = DIRECTION ( 'NONE',  ( 0.000000000000000000, -0.9908441862701420355, -0.1350103645453197554 ) ) ;
#228664 = ORIENTED_EDGE ( 'NONE', *, *, #32032, .T. ) ;
#228666 = ORIENTED_EDGE ( 'NONE', *, *, #24891, .T. ) ;
#228665 = TOROIDAL_SURFACE ( 'NONE', #149550, 0.4000000000000012990, 0.1000000000000000056 ) ;
#228667 = EDGE_CURVE ( 'NONE', #140599, #119943, #17753, .T. ) ;
#228668 = AXIS2_PLACEMENT_3D ( 'NONE', #16170, #72277, #194807 ) ;
#228669 = DIRECTION ( 'NONE',  ( 0.000000000000000000, 1.000000000000000000, 0.000000000000000000 ) ) ;
#228670 = EDGE_LOOP ( 'NONE', ( #143206, #256365, #69349, #238693 ) ) ;
#228671 = DIRECTION ( 'NONE',  ( -1.000000000000000000, 0.000000000000000000, 0.000000000000000000 ) ) ;
#228672 = AXIS2_PLACEMENT_3D ( 'NONE', #165018, #243256, #223689 ) ;
#228673 = VERTEX_POINT ( 'NONE', #119457 ) ;
#228674 = DIRECTION ( 'NONE',  ( 0.000000000000000000, 0.000000000000000000, -1.000000000000000000 ) ) ;
#228675 = DIRECTION ( 'NONE',  ( -7.304098846218135653E-16, -0.9770955615653315052, -0.2128009952263603954 ) ) ;
#228676 = ADVANCED_FACE ( 'NONE', ( #197682 ), #79000, .F. ) ;
#228677 = CARTESIAN_POINT ( 'NONE',  ( -18.40000000000000213, 70.35000000001200249, -112.2731074845243313 ) ) ;
#228678 = ORIENTED_EDGE ( 'NONE', *, *, #28897, .F. ) ;
#228679 = EDGE_CURVE ( 'NONE', #157975, #53997, #99845, .T. ) ;
#228680 = CARTESIAN_POINT ( 'NONE',  ( -16.85722902420156544, 9.949999999999983302, -12.76554747377053545 ) ) ;
#228681 = DIRECTION ( 'NONE',  ( 0.000000000000000000, -1.776356839400250465E-15, -1.000000000000000000 ) ) ;
#228682 = ADVANCED_FACE ( 'NONE', ( #140265 ), #180713, .F. ) ;
#228683 = CARTESIAN_POINT ( 'NONE',  ( 12.60873083341396850, 9.389571634546411971, -17.81764071236915825 ) ) ;
#228684 = CARTESIAN_POINT ( 'NONE',  ( 21.05000000000000071, 1.115600667400684642E-11, -134.0000000000000000 ) ) ;
#228685 = DIRECTION ( 'NONE',  ( -1.000000000000000000, -0.000000000000000000, -0.000000000000000000 ) ) ;
#228686 = ORIENTED_EDGE ( 'NONE', *, *, #185193, .T. ) ;
#228688 = ORIENTED_EDGE ( 'NONE', *, *, #154561, .T. ) ;
#228687 = CYLINDRICAL_SURFACE ( 'NONE', #202367, 0.1000000000000028644 ) ;
#228689 = ADVANCED_FACE ( 'NONE', ( #55578 ), #35984, .T. ) ;
#228690 = ORIENTED_EDGE ( 'NONE', *, *, #43332, .T. ) ;
#228691 = DIRECTION ( 'NONE',  ( 0.000000000000000000, 0.9126074666064696306, 0.4088369013361213278 ) ) ;
#228692 = ADVANCED_FACE ( 'NONE', ( #59427 ), #185804, .T. ) ;
#228693 = ORIENTED_EDGE ( 'NONE', *, *, #63929, .T. ) ;
#228694 = DIRECTION ( 'NONE',  ( 0.000000000000000000, 0.9090645160164306793, 0.4166553800442435729 ) ) ;
#228695 = CARTESIAN_POINT ( 'NONE',  ( 21.53699400384778428, 1.434816042522701864E-11, -26.71228820676085647 ) ) ;
#228696 = LINE ( 'NONE', #70920, #216573 ) ;
#228697 = ORIENTED_EDGE ( 'NONE', *, *, #166110, .T. ) ;
#228698 = CARTESIAN_POINT ( 'NONE',  ( -23.15000000000000213, 76.33602373114293016, -220.7416935524190365 ) ) ;
#228699 = DIRECTION ( 'NONE',  ( -1.000000000000000000, -0.000000000000000000, -0.000000000000000000 ) ) ;
#228700 = DIRECTION ( 'NONE',  ( 1.000000000000000000, -0.000000000000000000, -0.000000000000000000 ) ) ;
#228701 = VERTEX_POINT ( 'NONE', #96012 ) ;
#228703 = VERTEX_POINT ( 'NONE', #215955 ) ;
#228702 = CARTESIAN_POINT ( 'NONE',  ( 23.14999999999999858, 19.92792862942048870, -235.1286901285539841 ) ) ;
#228704 = FACE_OUTER_BOUND ( 'NONE', #209221, .T. ) ;
#228705 = DIRECTION ( 'NONE',  ( 1.000000000000000000, 0.000000000000000000, 0.000000000000000000 ) ) ;
#228706 = CIRCLE ( 'NONE', #37162, 0.09999999999999939493 ) ;
#228707 = CIRCLE ( 'NONE', #62091, 12.97499999999999964 ) ;
#228708 = VECTOR ( 'NONE', #126002, 1000.000000000000000 ) ;
#228709 = AXIS2_PLACEMENT_3D ( 'NONE', #241391, #27512, #167015 ) ;
#228710 = ADVANCED_FACE ( 'NONE', ( #218515 ), #255031, .F. ) ;
#228711 = EDGE_CURVE ( 'NONE', #155422, #184016, #152523, .T. ) ;
#228712 = ORIENTED_EDGE ( 'NONE', *, *, #45558, .T. ) ;
#228713 = DIRECTION ( 'NONE',  ( 0.000000000000000000, 1.000000000000000000, -6.308085367188393199E-16 ) ) ;
#228714 = CARTESIAN_POINT ( 'NONE',  ( -17.22767730082796689, 42.79277586624079532, -235.4629708983620446 ) ) ;
#228715 = AXIS2_PLACEMENT_3D ( 'NONE', #201024, #22403, #144879 ) ;
#228716 = CARTESIAN_POINT ( 'NONE',  ( -20.88420186297724612, 18.41141989892752662, -236.9935361838138022 ) ) ;
#228717 = ORIENTED_EDGE ( 'NONE', *, *, #35771, .F. ) ;
#228718 = CYLINDRICAL_SURFACE ( 'NONE', #125797, 0.09999999999999867328 ) ;
#228719 = EDGE_CURVE ( 'NONE', #144504, #252694, #202827, .T. ) ;
#228720 = CARTESIAN_POINT ( 'NONE',  ( -18.59999999999999787, 46.55954744353147134, -243.3218549665227783 ) ) ;
#228721 = ORIENTED_EDGE ( 'NONE', *, *, #105194, .F. ) ;
#228722 = CIRCLE ( 'NONE', #78834, 0.09999999999999939493 ) ;
#228723 = AXIS2_PLACEMENT_3D ( 'NONE', #192999, #36510, #116035 ) ;
#228724 = EDGE_CURVE ( 'NONE', #165690, #165183, #28078, .T. ) ;
#228725 = VECTOR ( 'NONE', #231606, 1000.000000000000000 ) ;
#228726 = EDGE_CURVE ( 'NONE', #165845, #90093, #63231, .T. ) ;
#228727 = CIRCLE ( 'NONE', #187213, 0.09999999999998898659 ) ;
#228728 = VERTEX_POINT ( 'NONE', #125847 ) ;
#228729 = CARTESIAN_POINT ( 'NONE',  ( 18.59999999999999076, 64.35000000001214460, -136.5231074845244166 ) ) ;
#228730 = EDGE_CURVE ( 'NONE', #6455, #7639, #162443, .T. ) ;
#228731 = ORIENTED_EDGE ( 'NONE', *, *, #113828, .T. ) ;
#228732 = DIRECTION ( 'NONE',  ( 0.000000000000000000, 0.000000000000000000, -1.000000000000000000 ) ) ;
#228733 = CARTESIAN_POINT ( 'NONE',  ( 20.94999999999999574, 1.162701749949165642, -41.60000000000000142 ) ) ;
#228735 = ORIENTED_EDGE ( 'NONE', *, *, #243643, .F. ) ;
#228734 = DIRECTION ( 'NONE',  ( -0.000000000000000000, -0.000000000000000000, -1.000000000000000000 ) ) ;
#228736 = CARTESIAN_POINT ( 'NONE',  ( -20.64999999999999858, 85.40000000001262492, -193.6291383618718385 ) ) ;
#228737 = DIRECTION ( 'NONE',  ( 0.000000000000000000, -1.000000000000000000, 0.000000000000000000 ) ) ;
#228738 = DIRECTION ( 'NONE',  ( 0.000000000000000000, 0.000000000000000000, -1.000000000000000000 ) ) ;
#228739 = CARTESIAN_POINT ( 'NONE',  ( 21.05000000000000071, -12.41227409413852811, -164.5000000000000000 ) ) ;
#228740 = DIRECTION ( 'NONE',  ( -3.265361837132813093E-16, 1.000000000000000000, 0.000000000000000000 ) ) ;
#228741 = EDGE_CURVE ( 'NONE', #57244, #148222, #44362, .T. ) ;
#228742 = CARTESIAN_POINT ( 'NONE',  ( -23.15000000000000213, 0.04003676617161597284, -188.9658445640203297 ) ) ;
#228743 = CARTESIAN_POINT ( 'NONE',  ( 23.14999999999999858, 2.100000000011158274, -100.5000000000000426 ) ) ;
#228745 = EDGE_LOOP ( 'NONE', ( #75507, #144576, #98765, #14042 ) ) ;
#228744 = DIRECTION ( 'NONE',  ( 0.000000000000000000, -6.982962677686266711E-15, 1.000000000000000000 ) ) ;
#228746 = TOROIDAL_SURFACE ( 'NONE', #103617, 11.90000000000000213, 0.1000000000000000056 ) ;
#228747 = CARTESIAN_POINT ( 'NONE',  ( -20.85000000000000142, 62.98048128140160173, -207.0210305352945852 ) ) ;
#228748 = DIRECTION ( 'NONE',  ( 0.000000000000000000, 0.000000000000000000, 1.000000000000000000 ) ) ;
#228749 = AXIS2_PLACEMENT_3D ( 'NONE', #126874, #245545, #146408 ) ;
#228750 = LINE ( 'NONE', #48805, #257183 ) ;
#228751 = DIRECTION ( 'NONE',  ( -0.000000000000000000, 0.000000000000000000, 1.000000000000000000 ) ) ;
#228752 = ORIENTED_EDGE ( 'NONE', *, *, #122605, .F. ) ;
#228753 = DIRECTION ( 'NONE',  ( 0.000000000000000000, -6.982962677686266711E-15, 1.000000000000000000 ) ) ;
#228754 = CYLINDRICAL_SURFACE ( 'NONE', #151901, 0.09999999999998898659 ) ;
#228755 = DIRECTION ( 'NONE',  ( 0.000000000000000000, -0.4088369013363280513, 0.9126074666063769270 ) ) ;
#228756 = AXIS2_PLACEMENT_3D ( 'NONE', #239177, #217026, #549 ) ;
#228757 = ORIENTED_EDGE ( 'NONE', *, *, #103227, .T. ) ;
#228758 = AXIS2_PLACEMENT_3D ( 'NONE', #113821, #193386, #214220 ) ;
#228760 = ADVANCED_FACE ( 'NONE', ( #86707 ), #222359, .T. ) ;
#228759 = CARTESIAN_POINT ( 'NONE',  ( 21.05000000000000071, 76.02138556595068053, -209.8280685972093522 ) ) ;
#228761 = AXIS2_PLACEMENT_3D ( 'NONE', #229946, #212956, #51277 ) ;
#228762 = CYLINDRICAL_SURFACE ( 'NONE', #159654, 0.09999999999999939493 ) ;
#228763 = ORIENTED_EDGE ( 'NONE', *, *, #197404, .T. ) ;
#228764 = CARTESIAN_POINT ( 'NONE',  ( -21.05000000000000071, 76.00000000001193712, -107.1231074845243114 ) ) ;
#228765 = ORIENTED_EDGE ( 'NONE', *, *, #4449, .F. ) ;
#228766 = ORIENTED_EDGE ( 'NONE', *, *, #205198, .F. ) ;
#228767 = AXIS2_PLACEMENT_3D ( 'NONE', #124035, #99296, #101864 ) ;
#228768 = AXIS2_PLACEMENT_3D ( 'NONE', #221908, #84956, #242771 ) ;
#228769 = DIRECTION ( 'NONE',  ( 1.000000000000000000, -0.000000000000000000, -0.000000000000000000 ) ) ;
#228770 = CARTESIAN_POINT ( 'NONE',  ( 22.50000000000000000, 0.3085173699977246109, -229.9658011520297975 ) ) ;
#228771 = ORIENTED_EDGE ( 'NONE', *, *, #234927, .F. ) ;
#228772 = ORIENTED_EDGE ( 'NONE', *, *, #65496, .F. ) ;
#228773 = CARTESIAN_POINT ( 'NONE',  ( 18.50000000000000355, 85.42145614550719301, -129.2811254005048340 ) ) ;
#228775 = VERTEX_POINT ( 'NONE', #244515 ) ;
#228774 = DIRECTION ( 'NONE',  ( 0.000000000000000000, -6.982962677686266711E-15, 1.000000000000000000 ) ) ;
#228776 = EDGE_CURVE ( 'NONE', #133438, #200563, #248351, .T. ) ;
#228777 = CARTESIAN_POINT ( 'NONE',  ( 20.92356734117541706, 65.68026841930881687, -63.97257401318893955 ) ) ;
#228778 = VERTEX_POINT ( 'NONE', #206686 ) ;
#228779 = VECTOR ( 'NONE', #90971, 1000.000000000000000 ) ;
#228780 = TOROIDAL_SURFACE ( 'NONE', #116355, 1.900000000000002576, 0.1000000000000000056 ) ;
#228781 = CIRCLE ( 'NONE', #66463, 0.09999999999999939493 ) ;
#228782 = AXIS2_PLACEMENT_3D ( 'NONE', #239753, #220190, #183632 ) ;
#228783 = ORIENTED_EDGE ( 'NONE', *, *, #207874, .T. ) ;
#228785 = CIRCLE ( 'NONE', #116365, 0.09999999999999939493 ) ;
#228784 = CARTESIAN_POINT ( 'NONE',  ( 23.15000000000000213, 87.65000000001192859, -106.1231074845242262 ) ) ;
#228786 = FACE_OUTER_BOUND ( 'NONE', #215639, .T. ) ;
#228787 = DIRECTION ( 'NONE',  ( 0.000000000000000000, 6.982962677686266711E-15, -1.000000000000000000 ) ) ;
#228788 = ORIENTED_EDGE ( 'NONE', *, *, #77368, .T. ) ;
#228789 = CARTESIAN_POINT ( 'NONE',  ( 22.39999999999999503, 75.90000000001242597, -177.8138870828977360 ) ) ;
#228790 = CARTESIAN_POINT ( 'NONE',  ( -22.94999999999999929, -1.786320531569725478, -11.50977166988710820 ) ) ;
#228791 = DIRECTION ( 'NONE',  ( 0.000000000000000000, 1.000000000000000000, 6.982962677686267499E-15 ) ) ;
#228792 = ORIENTED_EDGE ( 'NONE', *, *, #218621, .T. ) ;
#228793 = SPHERICAL_SURFACE ( 'NONE', #220968, 0.1000000000000000056 ) ;
#228794 = CARTESIAN_POINT ( 'NONE',  ( 20.94999999999999574, 77.36087058720413268, -128.4501095574333362 ) ) ;
#228795 = DIRECTION ( 'NONE',  ( 1.000000000000000000, 0.000000000000000000, 0.000000000000000000 ) ) ;
#228796 = DIRECTION ( 'NONE',  ( 0.000000000000000000, 0.000000000000000000, -1.000000000000000000 ) ) ;
#228797 = ORIENTED_EDGE ( 'NONE', *, *, #226171, .T. ) ;
#228798 = CARTESIAN_POINT ( 'NONE',  ( 22.59999954896768770, -0.008828232233011105295, -55.24949132593204837 ) ) ;
#228799 = ORIENTED_EDGE ( 'NONE', *, *, #8767, .F. ) ;
#228801 = CIRCLE ( 'NONE', #212242, 0.09999999999999939493 ) ;
#228800 = CARTESIAN_POINT ( 'NONE',  ( -23.15000000000000213, 2.500000000011154633, -87.27537807723794572 ) ) ;
#228802 = EDGE_LOOP ( 'NONE', ( #78045, #41889, #115433, #59489, #61418, #73260, #196379, #48450, #195693, #74993, #49706 ) ) ;
#228803 = CARTESIAN_POINT ( 'NONE',  ( 18.49999999999999645, 7.128833340093095217, -233.7327013124392749 ) ) ;
#228804 = FACE_OUTER_BOUND ( 'NONE', #14423, .T. ) ;
#228805 = ORIENTED_EDGE ( 'NONE', *, *, #13943, .F. ) ;
#228806 = ORIENTED_EDGE ( 'NONE', *, *, #185052, .F. ) ;
#228808 = ORIENTED_EDGE ( 'NONE', *, *, #123545, .T. ) ;
#228807 = CYLINDRICAL_SURFACE ( 'NONE', #219645, 0.09999999999998898659 ) ;
#228809 = CARTESIAN_POINT ( 'NONE',  ( -21.05000000000000071, 77.83534155023700407, -191.9679561919613491 ) ) ;
#228810 = VERTEX_POINT ( 'NONE', #204104 ) ;
#228811 = LINE ( 'NONE', #129698, #60519 ) ;
#228812 = TOROIDAL_SURFACE ( 'NONE', #253720, 12.97499999999999787, 0.1000000000000000056 ) ;
#228813 = ORIENTED_EDGE ( 'NONE', *, *, #125109, .T. ) ;
#228814 = CARTESIAN_POINT ( 'NONE',  ( -20.94999999999999929, 1.116121084443477685E-11, -103.4000000000000199 ) ) ;
#228815 = CIRCLE ( 'NONE', #3947, 0.8750000000000007772 ) ;
#228816 = EDGE_CURVE ( 'NONE', #88113, #126189, #135903, .T. ) ;
#228817 = LINE ( 'NONE', #28064, #132590 ) ;
#228818 = VERTEX_POINT ( 'NONE', #123302 ) ;
#228819 = VECTOR ( 'NONE', #22378, 1000.000000000000000 ) ;
#228820 = PLANE ( 'NONE',  #180883 ) ;
#228821 = EDGE_CURVE ( 'NONE', #88893, #248473, #166313, .T. ) ;
#228822 = DIRECTION ( 'NONE',  ( 1.000000000000000000, 0.000000000000000000, 0.000000000000000000 ) ) ;
#228823 = EDGE_CURVE ( 'NONE', #217985, #165864, #215025, .T. ) ;
#228824 = CARTESIAN_POINT ( 'NONE',  ( -21.14999999999999858, 64.27847795353595473, -247.1247091181747066 ) ) ;
#228826 = ORIENTED_EDGE ( 'NONE', *, *, #160593, .F. ) ;
#228825 = DIRECTION ( 'NONE',  ( 0.000000000000000000, -0.000000000000000000, 1.000000000000000000 ) ) ;
#228827 = CARTESIAN_POINT ( 'NONE',  ( 18.39999999999999503, 5.649999999999983480, -12.65000000000000213 ) ) ;
#228828 = AXIS2_PLACEMENT_3D ( 'NONE', #132757, #106734, #246272 ) ;
#228829 = PLANE ( 'NONE',  #60895 ) ;
#228830 = DIRECTION ( 'NONE',  ( -0.000000000000000000, -0.000000000000000000, -1.000000000000000000 ) ) ;
#228832 = CYLINDRICAL_SURFACE ( 'NONE', #182640, 4.049999999999998046 ) ;
#228831 = LINE ( 'NONE', #232689, #202698 ) ;
#228833 = CYLINDRICAL_SURFACE ( 'NONE', #140578, 11.80000000000000426 ) ;
#228834 = EDGE_CURVE ( 'NONE', #251809, #29656, #85819, .T. ) ;
#228835 = CARTESIAN_POINT ( 'NONE',  ( -23.25000000000000000, 78.57744179526842743, -232.8011145694030972 ) ) ;
#228836 = B_SPLINE_CURVE_WITH_KNOTS ( 'NONE', 3,
 ( #186322, #148477, #248859, #130175, #66368, #88468, #165479, #149779, #151048, #128915, #10255, #244999, #126334, #105453, #89765, #85894, #125067, #110625, #71527 ),
 .UNSPECIFIED., .F., .F.,
 ( 4, 3, 3, 3, 3, 3, 4 ),
 ( 0.0001624081864585773726, 0.0001685232196531712882, 0.0001764526673566857657, 0.0001916878551483174834, 0.0002009890782182555721, 0.0002238845907555098180, 0.0002283406619926331546 ),
 .UNSPECIFIED. ) ;
#228837 = LINE ( 'NONE', #52744, #88448 ) ;
#228838 = AXIS2_PLACEMENT_3D ( 'NONE', #153192, #187167, #88014 ) ;
#228839 = ORIENTED_EDGE ( 'NONE', *, *, #71658, .T. ) ;
#228840 = ORIENTED_EDGE ( 'NONE', *, *, #56042, .F. ) ;
#228841 = ORIENTED_EDGE ( 'NONE', *, *, #60474, .T. ) ;
#228842 = ADVANCED_FACE ( 'NONE', ( #163712 ), #65003, .T. ) ;
#228843 = CARTESIAN_POINT ( 'NONE',  ( 21.05000000000000071, -11.29603075032412995, -36.54789915966387071 ) ) ;
#228844 = DIRECTION ( 'NONE',  ( 0.000000000000000000, 0.000000000000000000, -1.000000000000000000 ) ) ;
#228845 = EDGE_LOOP ( 'NONE', ( #256980, #197375, #196874, #1947 ) ) ;
#228846 = CYLINDRICAL_SURFACE ( 'NONE', #107285, 12.87499999999999822 ) ;
#228847 = CARTESIAN_POINT ( 'NONE',  ( -23.15000000000000213, 4.389020526555173163, -221.1525959572864792 ) ) ;
#228848 = DIRECTION ( 'NONE',  ( 0.000000000000000000, 0.8660254037844384856, -0.5000000000000003331 ) ) ;
#228849 = ORIENTED_EDGE ( 'NONE', *, *, #124760, .F. ) ;
#228850 = ORIENTED_EDGE ( 'NONE', *, *, #71235, .T. ) ;
#228851 = CARTESIAN_POINT ( 'NONE',  ( -16.87845715379269507, 9.957858113908168107, -46.12380065105890026 ) ) ;
#228852 = CARTESIAN_POINT ( 'NONE',  ( -21.55000000000000426, 68.29142135624991283, -191.1731074845243938 ) ) ;
#228853 = VERTEX_POINT ( 'NONE', #104971 ) ;
#228854 = CARTESIAN_POINT ( 'NONE',  ( -20.64999999999999858, 7.150000000011155876, -121.6500000000000341 ) ) ;
#228856 = VERTEX_POINT ( 'NONE', #46311 ) ;
#228855 = CARTESIAN_POINT ( 'NONE',  ( -18.59999999999999787, 11.64999999999999680, -7.014805770654001016 ) ) ;
#228857 = DIRECTION ( 'NONE',  ( 0.000000000000000000, -6.467318590049456648E-15, 1.000000000000000000 ) ) ;
#228860 = EDGE_CURVE ( 'NONE', #163993, #47050, #169287, .T. ) ;
#228859 = ORIENTED_EDGE ( 'NONE', *, *, #256294, .F. ) ;
#228858 = FACE_OUTER_BOUND ( 'NONE', #119523, .T. ) ;
#228861 = DIRECTION ( 'NONE',  ( 0.000000000000000000, 0.8814952561688136345, -0.4721928772777895800 ) ) ;
#228862 = CARTESIAN_POINT ( 'NONE',  ( -22.39999999999999858, 0.09999999999999939493, 7.790779598373403836 ) ) ;
#228863 = CARTESIAN_POINT ( 'NONE',  ( -21.37071067811865532, 8.070710678129811910, -112.7500000000000284 ) ) ;
#228864 = AXIS2_PLACEMENT_3D ( 'NONE', #180566, #77574, #140126 ) ;
#228867 = DIRECTION ( 'NONE',  ( 0.000000000000000000, 0.9126074666063757057, 0.4088369013363311044 ) ) ;
#228866 = TOROIDAL_SURFACE ( 'NONE', #124632, 1.900000000000002576, 0.1000000000000000056 ) ;
#228865 = DIRECTION ( 'NONE',  ( -0.000000000000000000, 6.982962677686266711E-15, -1.000000000000000000 ) ) ;
#228868 = CARTESIAN_POINT ( 'NONE',  ( 18.49999999999999289, 10.20857864609425825, -91.70250686562992826 ) ) ;
#228869 = CIRCLE ( 'NONE', #183088, 11.75000000000000000 ) ;
#228870 = CIRCLE ( 'NONE', #4009, 0.09999999999998898659 ) ;
#228871 = CARTESIAN_POINT ( 'NONE',  ( 23.24999999999999289, -4.149999999988843058, -100.5000000000000284 ) ) ;
#228872 = DIRECTION ( 'NONE',  ( 0.000000000000000000, 1.000000000000000000, 0.000000000000000000 ) ) ;
#228873 = VERTEX_POINT ( 'NONE', #133566 ) ;
#228874 = ORIENTED_EDGE ( 'NONE', *, *, #162707, .F. ) ;
#228875 = EDGE_CURVE ( 'NONE', #253862, #37772, #252572, .T. ) ;
#228876 = DIRECTION ( 'NONE',  ( 0.000000000000000000, -1.000000000000000000, 0.000000000000000000 ) ) ;
#228877 = AXIS2_PLACEMENT_3D ( 'NONE', #93905, #142017, #162900 ) ;
#228878 = EDGE_LOOP ( 'NONE', ( #100120, #248311, #104333, #132040 ) ) ;
#228879 = DIRECTION ( 'NONE',  ( 0.000000000000000000, 0.2128009952263604232, -0.9770955615653316162 ) ) ;
#228880 = ORIENTED_EDGE ( 'NONE', *, *, #179536, .T. ) ;
#228881 = SPHERICAL_SURFACE ( 'NONE', #169370, 0.1000000000000000056 ) ;
#228882 = CARTESIAN_POINT ( 'NONE',  ( -18.34374000495060386, 11.47316190337362585, -76.25000000000004263 ) ) ;
#228883 = EDGE_CURVE ( 'NONE', #89546, #232502, #190100, .T. ) ;
#228884 = AXIS2_PLACEMENT_3D ( 'NONE', #53164, #234360, #91008 ) ;
#228885 = EDGE_LOOP ( 'NONE', ( #133137, #200480, #119644, #213916 ) ) ;
#228886 = AXIS2_PLACEMENT_3D ( 'NONE', #256899, #159163, #40514 ) ;
#228887 = DIRECTION ( 'NONE',  ( 1.000000000000000000, 0.000000000000000000, 0.000000000000000000 ) ) ;
#228888 =( NAMED_UNIT ( * ) PLANE_ANGLE_UNIT ( ) SI_UNIT ( $, .RADIAN. ) );
#228889 = EDGE_CURVE ( 'NONE', #185054, #117327, #6747, .T. ) ;
#228890 = ORIENTED_EDGE ( 'NONE', *, *, #155334, .T. ) ;
#228891 = AXIS2_PLACEMENT_3D ( 'NONE', #208706, #110866, #31371 ) ;
#228892 = ORIENTED_EDGE ( 'NONE', *, *, #100074, .F. ) ;
#228893 = EDGE_LOOP ( 'NONE', ( #108928, #134999, #188248, #153329 ) ) ;
#228894 = DIRECTION ( 'NONE',  ( -0.7071067811865475727, 0.6824534298470373850, -0.1850873201762210096 ) ) ;
#228895 = DIRECTION ( 'NONE',  ( 1.000000000000000000, 0.000000000000000000, 0.000000000000000000 ) ) ;
#228896 = FACE_OUTER_BOUND ( 'NONE', #65031, .T. ) ;
#228897 = CARTESIAN_POINT ( 'NONE',  ( 20.85000000000000142, 1.115600667400684642E-11, -67.00000000000000000 ) ) ;
#228898 = ADVANCED_FACE ( 'NONE', ( #252216 ), #177475, .F. ) ;
#228900 = CARTESIAN_POINT ( 'NONE',  ( -18.39418127959864790, 11.48390560170929220, -57.75000000000000000 ) ) ;
#228899 = DIRECTION ( 'NONE',  ( -0.000000000000000000, -0.2128009952263604232, 0.9770955615653316162 ) ) ;
#228901 = CARTESIAN_POINT ( 'NONE',  ( -12.25000000000000000, 9.350000000011133849, -83.51856895740269238 ) ) ;
#228903 = EDGE_LOOP ( 'NONE', ( #130760, #182758, #82815, #111045 ) ) ;
#228902 = CARTESIAN_POINT ( 'NONE',  ( -20.94999999999999929, 10.29288807859936661, -139.4580020160122160 ) ) ;
#228905 = CARTESIAN_POINT ( 'NONE',  ( -18.59999999999999787, 66.65000000001150227, -48.37310748452438958 ) ) ;
#228904 = DIRECTION ( 'NONE',  ( -1.000000000000000000, 0.000000000000000000, 0.000000000000000000 ) ) ;
#228906 = CARTESIAN_POINT ( 'NONE',  ( 20.94999999999999574, -11.64999999998883595, -103.5000000000000426 ) ) ;
#228907 = EDGE_LOOP ( 'NONE', ( #223339, #195129, #65376, #251459 ) ) ;
#228908 = CARTESIAN_POINT ( 'NONE',  ( 20.95378194480896639, 10.53491199155394220, -74.56505414814790811 ) ) ;
#228909 = DIRECTION ( 'NONE',  ( -1.000000000000000000, -0.000000000000000000, -0.000000000000000000 ) ) ;
#228911 = EDGE_CURVE ( 'NONE', #110576, #71835, #87685, .T. ) ;
#228910 = CARTESIAN_POINT ( 'NONE',  ( 21.05000000000000071, 1.115600667400684642E-11, -134.0000000000000284 ) ) ;
#228913 = EDGE_CURVE ( 'NONE', #93478, #86414, #98275, .T. ) ;
#228912 = ORIENTED_EDGE ( 'NONE', *, *, #159458, .T. ) ;
#228914 = B_SPLINE_CURVE_WITH_KNOTS ( 'NONE', 3,
 ( #103395, #201229, #22625, #82539, #241649, #63003 ),
 .UNSPECIFIED., .F., .F.,
 ( 4, 2, 4 ),
 ( 0.000000000000000000, 0.0001497467027049116195, 0.0002994934054098232390 ),
 .UNSPECIFIED. ) ;
#228915 = DIRECTION ( 'NONE',  ( 0.000000000000000000, 0.2617529984165031243, 0.9651348961777157509 ) ) ;
#228916 = CIRCLE ( 'NONE', #116490, 0.1000000000000021289 ) ;
#228917 = LINE ( 'NONE', #50253, #152623 ) ;
#228918 = CARTESIAN_POINT ( 'NONE',  ( 20.27550659511088682, 66.78395627750346364, -160.7731074845244166 ) ) ;
#228919 = ORIENTED_EDGE ( 'NONE', *, *, #253648, .T. ) ;
#228920 = VERTEX_POINT ( 'NONE', #52733 ) ;
#228921 = EDGE_CURVE ( 'NONE', #103163, #239496, #15130, .T. ) ;
#228922 = DIRECTION ( 'NONE',  ( 1.000000000000000000, 0.000000000000000000, 0.000000000000000000 ) ) ;
#228923 = CARTESIAN_POINT ( 'NONE',  ( -20.94999999999999929, -10.76604040606817847, -206.3127087229280789 ) ) ;
#228924 = FACE_OUTER_BOUND ( 'NONE', #26503, .T. ) ;
#228926 = EDGE_CURVE ( 'NONE', #85846, #230417, #139988, .T. ) ;
#228925 = CARTESIAN_POINT ( 'NONE',  ( -18.50000000000000000, -1.835859311432484375, -179.0044391687985410 ) ) ;
#228927 = ORIENTED_EDGE ( 'NONE', *, *, #195070, .F. ) ;
#228928 = ADVANCED_FACE ( 'NONE', ( #69762, #33227 ), #228829, .F. ) ;
#228929 = CARTESIAN_POINT ( 'NONE',  ( -15.15564720441980739, 9.410708747058238899, -118.5692084058441793 ) ) ;
#228930 = CARTESIAN_POINT ( 'NONE',  ( -22.59999999999999787, 64.25043287652299284, -170.1239658536231616 ) ) ;
#228931 = CARTESIAN_POINT ( 'NONE',  ( -20.54999999999999716, -3.770473190032741062, -225.9805569534692324 ) ) ;
#228932 = DIRECTION ( 'NONE',  ( 0.000000000000000000, -0.9651348961777157509, 0.2617529984165031243 ) ) ;
#228933 = AXIS2_PLACEMENT_3D ( 'NONE', #224468, #66696, #165814 ) ;
#228934 = ORIENTED_EDGE ( 'NONE', *, *, #14755, .F. ) ;
#228936 = CARTESIAN_POINT ( 'NONE',  ( 20.93302460841142931, 10.31565961586829872, -39.03641941191782649 ) ) ;
#228935 = AXIS2_PLACEMENT_3D ( 'NONE', #50972, #69300, #190540 ) ;
#228938 = ORIENTED_EDGE ( 'NONE', *, *, #236277, .F. ) ;
#228937 = DIRECTION ( 'NONE',  ( -1.000000000000000000, -0.000000000000000000, 0.000000000000000000 ) ) ;
#228940 = EDGE_CURVE ( 'NONE', #100799, #84436, #206657, .T. ) ;
#228939 = CARTESIAN_POINT ( 'NONE',  ( 22.49999999999999645, 31.81502280147385164, -238.9558108736092095 ) ) ;
#228941 = CARTESIAN_POINT ( 'NONE',  ( 18.49999999999999289, 6.450000000011156587, -188.6499999999999488 ) ) ;
#228942 = AXIS2_PLACEMENT_3D ( 'NONE', #209332, #129800, #11146 ) ;
#228943 = DIRECTION ( 'NONE',  ( 1.000000000000000000, -0.000000000000000000, -0.000000000000000000 ) ) ;
#228944 = EDGE_CURVE ( 'NONE', #98192, #9830, #209245, .T. ) ;
#228945 = CARTESIAN_POINT ( 'NONE',  ( -23.15000000000000213, 11.65000000001115588, -146.1500000000000341 ) ) ;
#228946 = CARTESIAN_POINT ( 'NONE',  ( 23.14999999999999858, 76.00000000001170974, -69.52310748452431710 ) ) ;
#228947 = AXIS2_PLACEMENT_3D ( 'NONE', #159024, #201976, #143272 ) ;
#228948 = DIRECTION ( 'NONE',  ( 0.000000000000000000, 6.982962677686266711E-15, -1.000000000000000000 ) ) ;
#228949 = CARTESIAN_POINT ( 'NONE',  ( 21.05000000000000071, 69.35000000001259934, -191.3731074845244109 ) ) ;
#228950 = VERTEX_POINT ( 'NONE', #90574 ) ;
#228951 = CARTESIAN_POINT ( 'NONE',  ( 21.72449340488910252, 65.71604372252045323, -56.87310748452438958 ) ) ;
#228952 = CYLINDRICAL_SURFACE ( 'NONE', #15086, 0.09999999999999939493 ) ;
#228953 = CARTESIAN_POINT ( 'NONE',  ( 20.04142135623730070, 11.75000000001115907, -58.15000000000000568 ) ) ;
#228954 = CARTESIAN_POINT ( 'NONE',  ( 23.14999999999999858, 73.97321671803807419, -202.9734261878502366 ) ) ;
#228955 = ADVANCED_FACE ( 'NONE', ( #191000 ), #82791, .T. ) ;
#228956 = DIRECTION ( 'NONE',  ( 0.000000000000000000, 0.2128009952263485993, -0.9770955615653341697 ) ) ;
#228958 = CARTESIAN_POINT ( 'NONE',  ( 15.07585980824112148, 9.417632963117448242, -185.6489484657322180 ) ) ;
#228957 = CIRCLE ( 'NONE', #141453, 0.5000000000000004441 ) ;
#228959 = VECTOR ( 'NONE', #131159, 1000.000000000000000 ) ;
#228961 = ORIENTED_EDGE ( 'NONE', *, *, #68575, .T. ) ;
#228960 = AXIS2_PLACEMENT_3D ( 'NONE', #207735, #73374, #232439 ) ;
#228962 = ORIENTED_EDGE ( 'NONE', *, *, #17488, .F. ) ;
#228963 = AXIS2_PLACEMENT_3D ( 'NONE', #120798, #41266, #144162 ) ;
#228964 = AXIS2_PLACEMENT_3D ( 'NONE', #12891, #211068, #29889 ) ;
#228965 = CARTESIAN_POINT ( 'NONE',  ( -22.39999999999999858, 36.56766367508408422, -249.5920463913791139 ) ) ;
#228966 = CARTESIAN_POINT ( 'NONE',  ( -17.01473183483381391, 66.05000000001207638, -123.7731074845243597 ) ) ;
#228967 = CARTESIAN_POINT ( 'NONE',  ( -18.79999999999999716, 11.49641995933507843, -1.885425182446133885 ) ) ;
#228968 = AXIS2_PLACEMENT_3D ( 'NONE', #205429, #221144, #4656 ) ;
#228969 = CARTESIAN_POINT ( 'NONE',  ( -18.59999999999999787, 55.11435547888748232, -226.8560373590520101 ) ) ;
#228970 = DIRECTION ( 'NONE',  ( 0.000000000000000000, 0.9126074666063770380, 0.4088369013363281068 ) ) ;
#228971 = DIRECTION ( 'NONE',  ( -0.000000000000000000, -6.982962677686266711E-15, 1.000000000000000000 ) ) ;
#228972 = EDGE_CURVE ( 'NONE', #150106, #178795, #81713, .T. ) ;
#228973 = DIRECTION ( 'NONE',  ( -1.000000000000000000, 0.000000000000000000, 0.000000000000000000 ) ) ;
#228974 = DIRECTION ( 'NONE',  ( 0.000000000000000000, -0.4088369013363280513, 0.9126074666063769270 ) ) ;
#228975 = EDGE_CURVE ( 'NONE', #10427, #186771, #123639, .T. ) ;
#228976 = DIRECTION ( 'NONE',  ( 0.000000000000000000, 0.1618390714546044939, 0.9868171638914228216 ) ) ;
#228977 = ORIENTED_EDGE ( 'NONE', *, *, #189924, .T. ) ;
#228978 = DIRECTION ( 'NONE',  ( 0.000000000000000000, -6.688090509790097607E-15, 1.000000000000000000 ) ) ;
#228979 = ADVANCED_FACE ( 'NONE', ( #210541 ), #48610, .F. ) ;
#228980 = EDGE_LOOP ( 'NONE', ( #62829, #132885, #240311 ) ) ;
#228981 = CARTESIAN_POINT ( 'NONE',  ( 21.00000000000000000, 63.38346053167636995, -212.7939182281409956 ) ) ;
#228982 = CARTESIAN_POINT ( 'NONE',  ( 18.79999999999999716, 1.885425182446134107, -11.59641995933507808 ) ) ;
#228983 = CARTESIAN_POINT ( 'NONE',  ( 18.39999999999999503, 64.25000000001153921, -48.67310748452440805 ) ) ;
#228984 = DIRECTION ( 'NONE',  ( -0.8660254037844653530, 0.000000000000000000, 0.4999999999999539257 ) ) ;
#228986 = ADVANCED_FACE ( 'NONE', ( #40919 ), #190293, .T. ) ;
#228985 = DIRECTION ( 'NONE',  ( 1.000000000000000000, 0.000000000000000000, 0.000000000000000000 ) ) ;
#228987 = DIRECTION ( 'NONE',  ( -1.000000000000000000, -1.476360405086644309E-16, 0.000000000000000000 ) ) ;
#228988 = DIRECTION ( 'NONE',  ( -1.000000000000000000, -0.000000000000000000, -0.000000000000000000 ) ) ;
#228990 = VERTEX_POINT ( 'NONE', #74909 ) ;
#228989 = AXIS2_PLACEMENT_3D ( 'NONE', #80525, #58398, #156284 ) ;
#228991 = CARTESIAN_POINT ( 'NONE',  ( -16.93230518875208190, 22.93660538467060661, -230.8552802729159055 ) ) ;
#228992 = CARTESIAN_POINT ( 'NONE',  ( 23.24999999999999289, 64.35000000001204512, -124.3731074845243825 ) ) ;
#228993 = EDGE_CURVE ( 'NONE', #102889, #126, #81894, .T. ) ;
#228994 = AXIS2_PLACEMENT_3D ( 'NONE', #140910, #180039, #61362 ) ;
#228995 = DIRECTION ( 'NONE',  ( 0.000000000000000000, -0.4721928772777346239, -0.8814952561688430555 ) ) ;
#228996 = CARTESIAN_POINT ( 'NONE',  ( -17.01473183483381391, 66.05000000001230376, -157.2731074845244166 ) ) ;
#228997 = CARTESIAN_POINT ( 'NONE',  ( -20.00857864376270001, 61.63293978347611812, -221.5406706031726003 ) ) ;
#228998 = CIRCLE ( 'NONE', #54192, 0.09999999999999939493 ) ;
#228999 = EDGE_CURVE ( 'NONE', #240710, #97170, #215221, .T. ) ;
#229001 = EDGE_CURVE ( 'NONE', #28102, #248002, #52705, .T. ) ;
#229000 = EDGE_CURVE ( 'NONE', #54821, #243146, #110987, .T. ) ;
#229002 = ORIENTED_EDGE ( 'NONE', *, *, #53792, .F. ) ;
#229003 = DIRECTION ( 'NONE',  ( 0.000000000000000000, 0.000000000000000000, -1.000000000000000000 ) ) ;
#229004 = CARTESIAN_POINT ( 'NONE',  ( -18.40000000000000213, 11.33174054713633261, -154.8500000000000227 ) ) ;
#229005 = VERTEX_POINT ( 'NONE', #37068 ) ;
#229006 = ADVANCED_FACE ( 'NONE', ( #76149 ), #456, .T. ) ;
#229007 = VERTEX_POINT ( 'NONE', #14921 ) ;
#229008 = CARTESIAN_POINT ( 'NONE',  ( -16.94389599337535657, 51.64067334384618846, -231.8915550546001612 ) ) ;
#229009 = DIRECTION ( 'NONE',  ( -0.000000000000000000, 0.9770955615653316162, 0.2128009952263603122 ) ) ;
#229010 = AXIS2_PLACEMENT_3D ( 'NONE', #115419, #236649, #13763 ) ;
#229011 = VECTOR ( 'NONE', #251568, 1000.000000000000000 ) ;
#229012 = ORIENTED_EDGE ( 'NONE', *, *, #44778, .F. ) ;
#229013 = CARTESIAN_POINT ( 'NONE',  ( 22.50000000000000000, 75.90000000001242597, -177.8138870828977360 ) ) ;
#229014 = DIRECTION ( 'NONE',  ( 0.000000000000000000, 0.000000000000000000, 1.000000000000000000 ) ) ;
#229015 = VERTEX_POINT ( 'NONE', #79981 ) ;
#229016 = ADVANCED_FACE ( 'NONE', ( #134820 ), #215651, .T. ) ;
#229017 = EDGE_CURVE ( 'NONE', #91518, #215393, #152716, .T. ) ;
#229018 = FACE_OUTER_BOUND ( 'NONE', #138597, .T. ) ;
#229019 = EDGE_CURVE ( 'NONE', #6865, #106717, #60434, .T. ) ;
#229020 = EDGE_LOOP ( 'NONE', ( #198790, #68099, #220855, #248193, #157433 ) ) ;
#229021 = CARTESIAN_POINT ( 'NONE',  ( 21.09610168723073187, 75.96641049312069072, -142.9020631997490796 ) ) ;
#229022 = DIRECTION ( 'NONE',  ( 0.000000000000000000, -0.4930308989874718772, -0.8700118002898612479 ) ) ;
#229024 = ORIENTED_EDGE ( 'NONE', *, *, #114968, .F. ) ;
#229023 = DIRECTION ( 'NONE',  ( 1.040834085586131715E-13, -0.9651348961777379554, 0.2617529984164210233 ) ) ;
#229025 = EDGE_CURVE ( 'NONE', #107696, #137697, #148594, .T. ) ;
#229026 = PLANE ( 'NONE',  #78163 ) ;
#229027 = CARTESIAN_POINT ( 'NONE',  ( -18.50000000000000000, -1.362429037182155023, -141.8888812479212334 ) ) ;
#229028 = CARTESIAN_POINT ( 'NONE',  ( -20.64999999999999858, 1.940186915899009490, -79.82911921105336717 ) ) ;
#229029 = DIRECTION ( 'NONE',  ( 0.000000000000000000, 0.9126074666064696306, 0.4088369013361213278 ) ) ;
#229030 = EDGE_CURVE ( 'NONE', #239916, #158987, #56730, .T. ) ;
#229031 = CARTESIAN_POINT ( 'NONE',  ( -16.78569801330234057, 66.05206626689910365, -190.8661945791769199 ) ) ;
#229032 = CARTESIAN_POINT ( 'NONE',  ( 20.94999999999999929, 77.83534155023627932, -91.46795619196132066 ) ) ;
#229033 = CARTESIAN_POINT ( 'NONE',  ( -16.78569801330234057, 66.05206626689880522, -157.3661945791769199 ) ) ;
#229035 = ORIENTED_EDGE ( 'NONE', *, *, #229545, .F. ) ;
#229034 = CARTESIAN_POINT ( 'NONE',  ( -18.59999999999999787, 79.37986612816742138, -196.2658927859692142 ) ) ;
#229036 = ORIENTED_EDGE ( 'NONE', *, *, #29908, .F. ) ;
#229039 = FACE_OUTER_BOUND ( 'NONE', #133620, .T. ) ;
#229038 = DIRECTION ( 'NONE',  ( -0.000000000000000000, 0.4856429311786307212, 0.8741572761215384846 ) ) ;
#229037 = AXIS2_PLACEMENT_3D ( 'NONE', #62901, #56766, #154651 ) ;
#229040 = CIRCLE ( 'NONE', #87357, 0.1000000000000089567 ) ;
#229042 = ORIENTED_EDGE ( 'NONE', *, *, #21696, .T. ) ;
#229041 = DIRECTION ( 'NONE',  ( 0.000000000000000000, 0.3738317757009942399, -0.9274965247785252886 ) ) ;
#229043 = ORIENTED_EDGE ( 'NONE', *, *, #172287, .T. ) ;
#229044 = CARTESIAN_POINT ( 'NONE',  ( -21.46681500597906833, 1.083969783932762665, -230.4946333871049831 ) ) ;
#229045 = DIRECTION ( 'NONE',  ( 1.186688945009009831E-16, 1.000000000000000000, 6.982962677686266711E-15 ) ) ;
#229046 = FACE_OUTER_BOUND ( 'NONE', #168908, .T. ) ;
#229047 = CARTESIAN_POINT ( 'NONE',  ( -20.94999675878240808, 10.29307482169070731, -172.9586421466940465 ) ) ;
#229048 = EDGE_CURVE ( 'NONE', #40840, #8640, #139961, .T. ) ;
#229049 = CARTESIAN_POINT ( 'NONE',  ( -20.94999999999999929, -11.41227409413852989, -70.00000000000004263 ) ) ;
#229050 = DIRECTION ( 'NONE',  ( 1.000000000000000000, 0.000000000000000000, 0.000000000000000000 ) ) ;
#229051 = CARTESIAN_POINT ( 'NONE',  ( -21.05000000000000071, 76.00000000001207923, -128.6231074845242972 ) ) ;
#229052 = ADVANCED_FACE ( 'NONE', ( #20055 ), #77420, .T. ) ;
#229053 = AXIS2_PLACEMENT_3D ( 'NONE', #137270, #134692, #99417 ) ;
#229054 = ORIENTED_EDGE ( 'NONE', *, *, #24101, .F. ) ;
#229055 = ORIENTED_EDGE ( 'NONE', *, *, #229156, .T. ) ;
#229056 = VECTOR ( 'NONE', #103443, 1000.000000000000000 ) ;
#229057 = CYLINDRICAL_SURFACE ( 'NONE', #102159, 0.09999999999999939493 ) ;
#229058 = CIRCLE ( 'NONE', #108259, 0.09999999999999939493 ) ;
#229059 = VERTEX_POINT ( 'NONE', #120460 ) ;
#229060 = DIRECTION ( 'NONE',  ( 0.000000000000000000, 0.4721928772777344574, 0.8814952561688431665 ) ) ;
#229061 = ORIENTED_EDGE ( 'NONE', *, *, #219774, .F. ) ;
#229062 = CARTESIAN_POINT ( 'NONE',  ( 18.59999999999999787, 86.35479209693788505, -176.2665665014505407 ) ) ;
#229063 = AXIS2_PLACEMENT_3D ( 'NONE', #157466, #32384, #96148 ) ;
#229064 = DIRECTION ( 'NONE',  ( 0.000000000000000000, 0.000000000000000000, 1.000000000000000000 ) ) ;
#229065 = ADVANCED_FACE ( 'NONE', ( #78706 ), #46013, .F. ) ;
#229066 = CARTESIAN_POINT ( 'NONE',  ( 23.24999999999999645, -2.099999999988846344, -167.5000000000000284 ) ) ;
#229067 = ORIENTED_EDGE ( 'NONE', *, *, #213074, .F. ) ;
#229068 = APPLICATION_CONTEXT ( 'automotive_design' ) ;
#229069 = CARTESIAN_POINT ( 'NONE',  ( 22.10000000000000142, -1.467286812112899463, 28.00000000000000000 ) ) ;
#229070 = ORIENTED_EDGE ( 'NONE', *, *, #53023, .T. ) ;
#229071 = CIRCLE ( 'NONE', #137464, 11.74999999999999645 ) ;
#229072 = CARTESIAN_POINT ( 'NONE',  ( 18.59999999999999787, -10.74999999999999289, 31.50000000000000000 ) ) ;
#229074 = AXIS2_PLACEMENT_3D ( 'NONE', #114352, #214725, #13979 ) ;
#229073 = DIRECTION ( 'NONE',  ( 1.000000000000000000, 0.000000000000000000, 0.000000000000000000 ) ) ;
#229075 = ORIENTED_EDGE ( 'NONE', *, *, #17504, .F. ) ;
#229076 = FACE_OUTER_BOUND ( 'NONE', #103529, .T. ) ;
#229077 = VERTEX_POINT ( 'NONE', #59127 ) ;
#229080 = ORIENTED_EDGE ( 'NONE', *, *, #248014, .T. ) ;
#229079 = DIRECTION ( 'NONE',  ( 0.000000000000000000, -3.122502256758163408E-13, 1.000000000000000000 ) ) ;
#229078 = DIRECTION ( 'NONE',  ( 0.000000000000000000, 2.362176648138631684E-15, 1.000000000000000000 ) ) ;
#229081 = EDGE_CURVE ( 'NONE', #60562, #18074, #177654, .T. ) ;
#229082 = DIRECTION ( 'NONE',  ( 0.7071067811865475727, 0.7071067811865475727, -0.000000000000000000 ) ) ;
#229083 = EDGE_LOOP ( 'NONE', ( #191112, #112554, #108040, #54933 ) ) ;
#229084 = CARTESIAN_POINT ( 'NONE',  ( 23.14999999999999858, 76.00000000001170974, -69.52310748452431710 ) ) ;
#229085 = ORIENTED_EDGE ( 'NONE', *, *, #51871, .T. ) ;
#229087 = DIRECTION ( 'NONE',  ( 0.000000000000000000, 0.000000000000000000, 1.000000000000000000 ) ) ;
#229086 =( BOUNDED_SURFACE ( )  B_SPLINE_SURFACE ( 3, 2, ( 
 ( #67693, #110671, #71571 ),
 ( #190218, #11589, #106805 ),
 ( #168127, #170698, #247614 ),
 ( #69002, #26012, #245048 ),
 ( #87237, #226760, #148522 ),
 ( #250187, #27328, #131515 ),
 ( #186371, #48123, #127676 ),
 ( #185071, #6429, #85938 ),
 ( #165525, #58364, #251458 ),
 ( #154960, #173267, #234456 ) ),
 .UNSPECIFIED., .F., .F., .F. ) 
 B_SPLINE_SURFACE_WITH_KNOTS ( ( 4, 2, 2, 2, 4 ),
 ( 3, 3 ),
 ( 0.0001701955120502364872, 0.0002247052511886114259, 0.0002792149903269863375, 0.0003882344686037362148, 0.0006062734251572359694 ),
 ( 0.000000000000000000, 1.000000000000000000 ),
 .UNSPECIFIED. ) 
 GEOMETRIC_REPRESENTATION_ITEM ( )  RATIONAL_B_SPLINE_SURFACE ( (
 ( 1.000000000000000000, 0.2966190024559251515, 1.000000000000000000),
 ( 1.000000000000000000, 0.2964522492711451074, 1.000000000000000000),
 ( 1.000000000000000000, 0.3059923531882451364, 1.000000000000000000),
 ( 1.000000000000000000, 0.3355751146951128083, 1.000000000000000000),
 ( 1.000000000000000000, 0.3550672384973958540, 1.000000000000000000),
 ( 1.000000000000000000, 0.4157034672164037770, 1.000000000000000000),
 ( 1.000000000000000000, 0.4588031877646243650, 1.000000000000000000),
 ( 1.000000000000000000, 0.5771441759675220995, 1.000000000000000000),
 ( 1.000000000000000000, 0.6469377121762164284, 1.000000000000000000),
 ( 1.000000000000000000, 0.7071067811865596742, 1.000000000000000000) ) ) 
 REPRESENTATION_ITEM ( '' )  SURFACE ( )  );
#229088 = CARTESIAN_POINT ( 'NONE',  ( -23.25000000000000000, 87.75000000001246292, -181.7731074845242745 ) ) ;
#229089 = DIRECTION ( 'NONE',  ( -1.000000000000000000, 0.000000000000000000, 0.000000000000000000 ) ) ;
#229090 = CARTESIAN_POINT ( 'NONE',  ( -16.85718274719396703, 66.02385768539031119, -123.9597611523418976 ) ) ;
#229091 = ORIENTED_EDGE ( 'NONE', *, *, #185252, .F. ) ;
#229092 = FACE_OUTER_BOUND ( 'NONE', #208194, .T. ) ;
#229093 = CARTESIAN_POINT ( 'NONE',  ( -13.22483237240080278, 66.56332574816946135, -154.8462455535252786 ) ) ;
#229094 = AXIS2_PLACEMENT_3D ( 'NONE', #54214, #109053, #68663 ) ;
#229095 = ORIENTED_EDGE ( 'NONE', *, *, #244403, .F. ) ;
#229096 = CARTESIAN_POINT ( 'NONE',  ( 23.15000000000000213, -11.74999999998883737, -45.75000000000000711 ) ) ;
#229097 = ORIENTED_EDGE ( 'NONE', *, *, #212527, .F. ) ;
#229098 = CARTESIAN_POINT ( 'NONE',  ( -20.85000000000000142, 67.84340367245323478, -228.0791829662263410 ) ) ;
#229099 = VERTEX_POINT ( 'NONE', #244201 ) ;
#229100 = DIRECTION ( 'NONE',  ( 0.000000000000000000, 1.000000000000000000, 0.000000000000000000 ) ) ;
#229101 = DIRECTION ( 'NONE',  ( -0.000000000000000000, -0.1350103645451876666, 0.9908441862701600211 ) ) ;
#229103 = VERTEX_POINT ( 'NONE', #242930 ) ;
#229102 = DIRECTION ( 'NONE',  ( -1.000000000000000000, 0.000000000000000000, 0.000000000000000000 ) ) ;
#229104 = DIRECTION ( 'NONE',  ( 0.000000000000000000, -1.000000000000000000, -6.982962677686265922E-15 ) ) ;
#229105 = ORIENTED_EDGE ( 'NONE', *, *, #167003, .F. ) ;
#229106 = CARTESIAN_POINT ( 'NONE',  ( -21.64999999999999858, 65.95000000001158469, -56.77310748452439526 ) ) ;
#229107 = EDGE_CURVE ( 'NONE', #71159, #57422, #86397, .T. ) ;
#229108 = FACE_OUTER_BOUND ( 'NONE', #223867, .T. ) ;
#229109 = ORIENTED_EDGE ( 'NONE', *, *, #195982, .F. ) ;
#229110 = CARTESIAN_POINT ( 'NONE',  ( 21.93340585971889212, 68.67585297715770309, -203.5231074845244166 ) ) ;
#229111 = LINE ( 'NONE', #209544, #6600 ) ;
#229112 = VERTEX_POINT ( 'NONE', #25197 ) ;
#229113 = CARTESIAN_POINT ( 'NONE',  ( 15.74999999999999645, 9.849999999999981881, -16.74999999999999645 ) ) ;
#229114 = AXIS2_PLACEMENT_3D ( 'NONE', #237324, #215187, #36588 ) ;
#229115 = VERTEX_POINT ( 'NONE', #47280 ) ;
#229116 = CARTESIAN_POINT ( 'NONE',  ( 13.22461703343585171, 9.436662931810239741, -118.8230367322948950 ) ) ;
#229117 = CYLINDRICAL_SURFACE ( 'NONE', #159670, 11.80000000000000426 ) ;
#229118 = CIRCLE ( 'NONE', #120815, 0.09999999999999976963 ) ;
#229119 = EDGE_CURVE ( 'NONE', #5669, #89956, #65582, .T. ) ;
#229120 = CIRCLE ( 'NONE', #199918, 0.09999999999999993616 ) ;
#229121 = VECTOR ( 'NONE', #161678, 1000.000000000000000 ) ;
#229122 = EDGE_CURVE ( 'NONE', #183971, #176002, #123005, .T. ) ;
#229125 = VERTEX_POINT ( 'NONE', #143821 ) ;
#229124 = ORIENTED_EDGE ( 'NONE', *, *, #5388, .F. ) ;
#229123 = DIRECTION ( 'NONE',  ( -0.000000000000000000, 6.982962677686266711E-15, -1.000000000000000000 ) ) ;
#229126 = DIRECTION ( 'NONE',  ( 1.000000000000000000, 0.000000000000000000, 0.000000000000000000 ) ) ;
#229127 = CARTESIAN_POINT ( 'NONE',  ( -22.49510344025093644, 0.06712767820541533370, -155.8500298948856937 ) ) ;
#229128 = CARTESIAN_POINT ( 'NONE',  ( -23.15000000000000213, 71.65000000001155911, -57.37310748452435405 ) ) ;
#229130 = CARTESIAN_POINT ( 'NONE',  ( -15.75000000000001066, 66.65000000001157332, -52.65883987690830992 ) ) ;
#229129 = DIRECTION ( 'NONE',  ( 0.000000000000000000, 0.6728971962616697722, 0.7397360091702875895 ) ) ;
#229131 = CARTESIAN_POINT ( 'NONE',  ( -22.39999999999999858, 7.790779598384560245, -167.3999999999999773 ) ) ;
#229132 = DIRECTION ( 'NONE',  ( 1.000000000000000000, -0.000000000000000000, -0.000000000000000000 ) ) ;
#229133 = EDGE_CURVE ( 'NONE', #113603, #249928, #16140, .T. ) ;
#229134 = DIRECTION ( 'NONE',  ( 0.000000000000000000, 0.4088369013363345461, -0.9126074666063741514 ) ) ;
#229135 = VECTOR ( 'NONE', #258059, 1000.000000000000000 ) ;
#229136 = CARTESIAN_POINT ( 'NONE',  ( -14.00000000000000178, 9.850000000011133849, -117.2500000000000284 ) ) ;
#229137 = AXIS2_PLACEMENT_3D ( 'NONE', #13171, #92687, #232232 ) ;
#229138 = VECTOR ( 'NONE', #238530, 1000.000000000000000 ) ;
#229139 = ORIENTED_EDGE ( 'NONE', *, *, #166306, .F. ) ;
#229140 = TOROIDAL_SURFACE ( 'NONE', #70953, 0.9750000000000019762, 0.1000000000000000056 ) ;
#229142 = ORIENTED_EDGE ( 'NONE', *, *, #110832, .T. ) ;
#229141 = CIRCLE ( 'NONE', #120834, 7.899999999999990585 ) ;
#229143 = EDGE_CURVE ( 'NONE', #180924, #15255, #240378, .T. ) ;
#229144 = DIRECTION ( 'NONE',  ( 0.000000000000000000, 0.2617529984165152257, 0.9651348961777124202 ) ) ;
#229147 = ORIENTED_EDGE ( 'NONE', *, *, #142557, .F. ) ;
#229146 = EDGE_CURVE ( 'NONE', #83974, #143516, #102753, .T. ) ;
#229145 = CARTESIAN_POINT ( 'NONE',  ( 21.05000000000000426, 10.56275983746217761, -174.9568139579185981 ) ) ;
#229148 = ORIENTED_EDGE ( 'NONE', *, *, #123894, .F. ) ;
#229149 = CARTESIAN_POINT ( 'NONE',  ( -16.77902162784673479, 12.41308644798263217, -211.2553675282883319 ) ) ;
#229150 = ORIENTED_EDGE ( 'NONE', *, *, #235505, .T. ) ;
#229151 = CARTESIAN_POINT ( 'NONE',  ( 21.05000000000000071, 43.38680032004197784, -234.7865223221098745 ) ) ;
#229152 = EDGE_CURVE ( 'NONE', #12777, #140846, #36172, .T. ) ;
#229153 = B_SPLINE_CURVE_WITH_KNOTS ( 'NONE', 3,
 ( #164010, #4896, #243533, #28382, #64888, #232984, #150854, #189985, #54307, #169169, #153476, #32215, #51724, #131289, #173036, #227816, #109144, #133856, #187428 ),
 .UNSPECIFIED., .F., .F.,
 ( 4, 3, 3, 3, 3, 3, 4 ),
 ( 0.0001624081864585664764, 0.0001685232196531825368, 0.0001764526673566942224, 0.0001916878551483208173, 0.0002009890782182613455, 0.0002238845907555189795, 0.0002283406619926576847 ),
 .UNSPECIFIED. ) ;
#229154 = AXIS2_PLACEMENT_3D ( 'NONE', #208624, #239072, #60416 ) ;
#229155 = ORIENTED_EDGE ( 'NONE', *, *, #28558, .F. ) ;
#229156 = EDGE_CURVE ( 'NONE', #159228, #231733, #220802, .T. ) ;
#229157 = CARTESIAN_POINT ( 'NONE',  ( 20.94999999999999574, 77.83534155023598089, -57.96795619196132776 ) ) ;
#229158 = CARTESIAN_POINT ( 'NONE',  ( -23.25000000000000000, 80.69087520990402140, -192.8618289658565743 ) ) ;
#229160 = ORIENTED_EDGE ( 'NONE', *, *, #74829, .T. ) ;
#229159 = ORIENTED_EDGE ( 'NONE', *, *, #211398, .T. ) ;
#229161 = EDGE_LOOP ( 'NONE', ( #194441, #171796, #35427, #61370 ) ) ;
#229162 = ORIENTED_EDGE ( 'NONE', *, *, #30312, .F. ) ;
#229163 = ORIENTED_EDGE ( 'NONE', *, *, #51019, .F. ) ;
#229164 = DIRECTION ( 'NONE',  ( 0.000000000000000000, -6.853228547068871147E-15, 1.000000000000000000 ) ) ;
#229165 = CARTESIAN_POINT ( 'NONE',  ( 20.94999999999999929, 69.15387683765879956, -32.28538121767450519 ) ) ;
#229166 = DIRECTION ( 'NONE',  ( 1.000000000000000000, 0.000000000000000000, -0.000000000000000000 ) ) ;
#229168 = ORIENTED_EDGE ( 'NONE', *, *, #184548, .F. ) ;
#229167 = DIRECTION ( 'NONE',  ( 1.000000000000000000, 0.000000000000000000, 0.000000000000000000 ) ) ;
#229169 = DIRECTION ( 'NONE',  ( -0.000000000000000000, 1.000000000000000000, 6.982962677686267499E-15 ) ) ;
#229170 = DIRECTION ( 'NONE',  ( 0.000000000000000000, 0.9126074666063770380, 0.4088369013363281068 ) ) ;
#229172 = ORIENTED_EDGE ( 'NONE', *, *, #158672, .F. ) ;
#229171 = CARTESIAN_POINT ( 'NONE',  ( -21.64999999999999858, 51.57797924205760864, -231.8552082689889460 ) ) ;
#229173 = LINE ( 'NONE', #210882, #130177 ) ;
#229174 = ORIENTED_EDGE ( 'NONE', *, *, #171255, .T. ) ;
#229175 = DIRECTION ( 'NONE',  ( 1.000000000000000000, 3.265361837132813093E-16, -0.000000000000000000 ) ) ;
#229176 = AXIS2_PLACEMENT_3D ( 'NONE', #147608, #129331, #45941 ) ;
#229178 = EDGE_CURVE ( 'NONE', #54754, #239491, #248527, .T. ) ;
#229177 = ORIENTED_EDGE ( 'NONE', *, *, #228921, .F. ) ;
#229179 = CARTESIAN_POINT ( 'NONE',  ( -20.54999999999999716, 82.09643798151613225, -215.4278993322501208 ) ) ;
#229180 = DIRECTION ( 'NONE',  ( 1.000000000000000000, 0.000000000000000000, 0.000000000000000000 ) ) ;
#229181 = TOROIDAL_SURFACE ( 'NONE', #33586, 2.100000000000002309, 0.1000000000000000056 ) ;
#229182 = VERTEX_POINT ( 'NONE', #5582 ) ;
#229184 = DIRECTION ( 'NONE',  ( -7.304098846218134667E-16, 1.000000000000000000, -0.000000000000000000 ) ) ;
#229183 = CARTESIAN_POINT ( 'NONE',  ( -21.07016717457011268, 76.00000000001274714, -209.8440483226252411 ) ) ;
#229185 = DIRECTION ( 'NONE',  ( 0.000000000000000000, -0.1335171055202866441, -0.9910465087640865089 ) ) ;
#229186 = VECTOR ( 'NONE', #49311, 1000.000000000000000 ) ;
#229187 = CARTESIAN_POINT ( 'NONE',  ( -20.64999999999999858, 1.115600667400684642E-11, -100.5000000000000284 ) ) ;
#229188 = DIRECTION ( 'NONE',  ( 1.444674012291107001E-15, -0.1332476588733650935, -0.9910827722268042983 ) ) ;
#229189 = EDGE_LOOP ( 'NONE', ( #186184, #249615, #157268, #167607 ) ) ;
#229190 = ORIENTED_EDGE ( 'NONE', *, *, #76395, .T. ) ;
#229191 =( BOUNDED_SURFACE ( )  B_SPLINE_SURFACE ( 3, 2, ( 
 ( #101177, #26856, #163779 ),
 ( #105029, #45103, #64662 ),
 ( #124647, #205448, #122083 ),
 ( #5953, #46368, #244579 ) ),
 .UNSPECIFIED., .F., .F., .F. ) 
 B_SPLINE_SURFACE_WITH_KNOTS ( ( 4, 4 ),
 ( 3, 3 ),
 ( 0.04058434257139457990, 0.04256401539001585660 ),
 ( 0.000000000000000000, 1.000000000000000000 ),
 .UNSPECIFIED. ) 
 GEOMETRIC_REPRESENTATION_ITEM ( )  RATIONAL_B_SPLINE_SURFACE ( (
 ( 1.000000000000000000, 0.7103081912008297749, 1.000000000000000000),
 ( 1.000000000000000000, 0.7104998333555392342, 1.000000000000000000),
 ( 1.000000000000000000, 0.7107238315755070035, 1.000000000000000000),
 ( 1.000000000000000000, 0.7110073749539291832, 1.000000000000000000) ) ) 
 REPRESENTATION_ITEM ( '' )  SURFACE ( )  );
#229192 = ADVANCED_FACE ( 'NONE', ( #6890 ), #121728, .T. ) ;
#229193 = CARTESIAN_POINT ( 'NONE',  ( -20.64999999999999858, 7.250000000011155521, -146.3500000000000227 ) ) ;
#229194 = DIRECTION ( 'NONE',  ( 0.000000000000000000, -0.9987946567507778317, 0.04908394489133698774 ) ) ;
#229195 = ORIENTED_EDGE ( 'NONE', *, *, #78769, .T. ) ;
#229196 = DIRECTION ( 'NONE',  ( 0.000000000000000000, 0.2617529984165031243, 0.9651348961777157509 ) ) ;
#229197 = ORIENTED_EDGE ( 'NONE', *, *, #194663, .F. ) ;
#229198 = CARTESIAN_POINT ( 'NONE',  ( -22.39999999999999858, 7.591056067193246548, -199.2444047917219052 ) ) ;
#229199 = CARTESIAN_POINT ( 'NONE',  ( -20.94999999999999929, 87.48912529308769592, -66.42310748452423752 ) ) ;
#229200 = AXIS2_PLACEMENT_3D ( 'NONE', #16057, #133414, #233806 ) ;
#229201 = DIRECTION ( 'NONE',  ( -1.000000000000000000, 0.000000000000000000, 0.000000000000000000 ) ) ;
#229202 = AXIS2_PLACEMENT_3D ( 'NONE', #129405, #86391, #31624 ) ;
#229203 = VERTEX_POINT ( 'NONE', #83819 ) ;
#229204 = CARTESIAN_POINT ( 'NONE',  ( -23.25000000000000000, 71.65000000001187175, -90.77310748452434552 ) ) ;
#229205 = SURFACE_STYLE_USAGE ( .BOTH. , #47977 ) ;
#229206 = AXIS2_PLACEMENT_3D ( 'NONE', #61461, #159295, #22358 ) ;
#229207 = ADVANCED_FACE ( 'NONE', ( #245520 ), #136077, .T. ) ;
#229209 = EDGE_LOOP ( 'NONE', ( #110720, #130313, #46270, #9548 ) ) ;
#229208 = AXIS2_PLACEMENT_3D ( 'NONE', #153247, #132359, #201014 ) ;
#229210 = ORIENTED_EDGE ( 'NONE', *, *, #102169, .T. ) ;
#229211 = EDGE_LOOP ( 'NONE', ( #162783, #49931, #189111, #79108, #13495, #74448, #208404, #97582 ) ) ;
#229212 = CARTESIAN_POINT ( 'NONE',  ( -21.05000000000000071, 79.23417978893665747, -236.1056577391152587 ) ) ;
#229213 = LINE ( 'NONE', #111831, #105080 ) ;
#229214 = LINE ( 'NONE', #10162, #119599 ) ;
#229215 = DIRECTION ( 'NONE',  ( -1.000000000000000000, 0.000000000000000000, -0.000000000000000000 ) ) ;
#229216 = EDGE_CURVE ( 'NONE', #193635, #53973, #201233, .T. ) ;
#229218 = DIRECTION ( 'NONE',  ( 0.000000000000000000, 0.2605042016806672911, -0.9654727137038716656 ) ) ;
#229217 = DIRECTION ( 'NONE',  ( 1.000000000000000000, 0.000000000000000000, 0.000000000000000000 ) ) ;
#229220 = ORIENTED_EDGE ( 'NONE', *, *, #19455, .F. ) ;
#229219 = DIRECTION ( 'NONE',  ( -1.000000000000000000, -0.000000000000000000, -0.000000000000000000 ) ) ;
#229221 = DIRECTION ( 'NONE',  ( 0.000000000000000000, -0.8814952561688438326, 0.4721928772777334582 ) ) ;
#229222 = ORIENTED_EDGE ( 'NONE', *, *, #19664, .T. ) ;
#229223 = DIRECTION ( 'NONE',  ( 0.000000000000000000, 0.9651348961777158619, -0.2617529984165028467 ) ) ;
#229224 = ORIENTED_EDGE ( 'NONE', *, *, #238295, .T. ) ;
#229225 = ORIENTED_EDGE ( 'NONE', *, *, #133206, .T. ) ;
#229226 = CARTESIAN_POINT ( 'NONE',  ( 18.69999999999999929, -11.65000000000000036, 33.00000000000000000 ) ) ;
#229227 = CARTESIAN_POINT ( 'NONE',  ( -18.40000000000000213, 43.57057518228153015, -234.0379448663882442 ) ) ;
#229229 = EDGE_CURVE ( 'NONE', #20238, #199047, #244231, .T. ) ;
#229228 = CARTESIAN_POINT ( 'NONE',  ( -16.90987985657661596, 66.04219248183177626, -48.65382039564075001 ) ) ;
#229230 = EDGE_CURVE ( 'NONE', #90874, #164553, #63008, .T. ) ;
#229231 = DIRECTION ( 'NONE',  ( 1.000000000000000000, 0.000000000000000000, 0.000000000000000000 ) ) ;
#229232 = CIRCLE ( 'NONE', #187550, 0.09999999999999996392 ) ;
#229233 = AXIS2_PLACEMENT_3D ( 'NONE', #189294, #188008, #231001 ) ;
#229234 = DIRECTION ( 'NONE',  ( 0.000000000000000000, 1.224646799142185182E-16, 1.000000000000000000 ) ) ;
#229235 = ORIENTED_EDGE ( 'NONE', *, *, #64260, .F. ) ;
#229236 = VERTEX_POINT ( 'NONE', #30329 ) ;
#229237 = EDGE_CURVE ( 'NONE', #127923, #257588, #210251, .T. ) ;
#229238 = CARTESIAN_POINT ( 'NONE',  ( 23.15000000000000213, 85.00000000001179501, -79.41707660717668205 ) ) ;
#229239 = ORIENTED_EDGE ( 'NONE', *, *, #242423, .T. ) ;
#229240 = CARTESIAN_POINT ( 'NONE',  ( -20.94999999999999929, 69.28189128378591022, -247.5258150475912089 ) ) ;
#229241 = FACE_OUTER_BOUND ( 'NONE', #111280, .T. ) ;
#229242 = EDGE_LOOP ( 'NONE', ( #225851, #131639, #168207, #182860 ) ) ;
#229243 = DIRECTION ( 'NONE',  ( 0.000000000000000000, -6.769652589177795712E-15, 1.000000000000000000 ) ) ;
#229244 = CARTESIAN_POINT ( 'NONE',  ( -18.59999999999999787, -9.480686695267820596, -207.9411151687578183 ) ) ;
#229245 = DIRECTION ( 'NONE',  ( 3.265361837132813093E-16, -1.000000000000000000, -0.000000000000000000 ) ) ;
#229246 = ORIENTED_EDGE ( 'NONE', *, *, #186171, .T. ) ;
#229247 = CARTESIAN_POINT ( 'NONE',  ( -22.59080734064477625, 64.25000000001215028, -136.5538571926213933 ) ) ;
#229248 = FACE_OUTER_BOUND ( 'NONE', #78031, .T. ) ;
#229249 = DIRECTION ( 'NONE',  ( 0.000000000000000000, 0.9908441862701596881, 0.1350103645451904977 ) ) ;
#229250 = DIRECTION ( 'NONE',  ( 0.000000000000000000, 0.000000000000000000, -1.000000000000000000 ) ) ;
#229251 = AXIS2_PLACEMENT_3D ( 'NONE', #6095, #183473, #205578 ) ;
#229252 = VECTOR ( 'NONE', #193292, 1000.000000000000114 ) ;
#229253 = DIRECTION ( 'NONE',  ( 1.000000000000000000, 1.394253735153569469E-16, 2.602809386958778209E-16 ) ) ;
#229254 = AXIS2_PLACEMENT_3D ( 'NONE', #228905, #187228, #108941 ) ;
#229255 = CYLINDRICAL_SURFACE ( 'NONE', #86452, 0.09999999999999939493 ) ;
#229256 = ORIENTED_EDGE ( 'NONE', *, *, #124581, .F. ) ;
#229257 = AXIS2_PLACEMENT_3D ( 'NONE', #160019, #73444, #169994 ) ;
#229258 = DIRECTION ( 'NONE',  ( 1.000000000000000000, -2.952720810173289112E-16, -2.061873921506763405E-30 ) ) ;
#229259 = ORIENTED_EDGE ( 'NONE', *, *, #35793, .F. ) ;
#229260 = ADVANCED_FACE ( 'NONE', ( #251925 ), #231106, .F. ) ;
#229261 = LINE ( 'NONE', #135261, #184857 ) ;
#229262 = EDGE_CURVE ( 'NONE', #41250, #254925, #191984, .T. ) ;
#229263 = CARTESIAN_POINT ( 'NONE',  ( -16.93344882324368683, 14.21793519637126124, -219.3067405467496371 ) ) ;
#229264 = LINE ( 'NONE', #247533, #77162 ) ;
#229265 = DIRECTION ( 'NONE',  ( -1.000000000000000000, 0.000000000000000000, 0.000000000000000000 ) ) ;
#229266 = CARTESIAN_POINT ( 'NONE',  ( 20.84451136049622377, 65.37985808520402031, -162.5291829250029991 ) ) ;
#229267 = AXIS2_PLACEMENT_3D ( 'NONE', #130476, #190487, #169658 ) ;
#229268 = ORIENTED_EDGE ( 'NONE', *, *, #20235, .F. ) ;
#229269 = DIRECTION ( 'NONE',  ( -0.000000000000000000, 0.1298341882520022694, 0.9915357197604853789 ) ) ;
#229270 = DIRECTION ( 'NONE',  ( 1.020425574104004196E-15, 0.2617529984165031243, 0.9651348961777157509 ) ) ;
#229271 = FACE_OUTER_BOUND ( 'NONE', #143862, .T. ) ;
#229272 = ADVANCED_FACE ( 'NONE', ( #13328 ), #211525, .F. ) ;
#229273 = FACE_OUTER_BOUND ( 'NONE', #54468, .T. ) ;
#229274 = ORIENTED_EDGE ( 'NONE', *, *, #30473, .F. ) ;
#229275 = EDGE_LOOP ( 'NONE', ( #20829, #43091, #90205, #83202 ) ) ;
#229276 = DIRECTION ( 'NONE',  ( 0.000000000000000000, 0.2617529984165152257, 0.9651348961777124202 ) ) ;
#229277 = DIRECTION ( 'NONE',  ( 0.000000000000000000, -0.4930308989874653269, -0.8700118002898649117 ) ) ;
#229278 = CARTESIAN_POINT ( 'NONE',  ( 22.60000000000000142, -3.180729737797944434, -228.0957332317254895 ) ) ;
#229279 = CARTESIAN_POINT ( 'NONE',  ( -16.89268316805466341, 44.12952801035616801, -235.2997120924900969 ) ) ;
#229280 = AXIS2_PLACEMENT_3D ( 'NONE', #142961, #189827, #167719 ) ;
#229281 = ORIENTED_EDGE ( 'NONE', *, *, #331, .F. ) ;
#229282 = FACE_OUTER_BOUND ( 'NONE', #205346, .T. ) ;
#229283 = ITEM_DEFINED_TRANSFORMATION ( 'NONE', 'NONE', #11171,  #2425 ) ;
#229284 = CARTESIAN_POINT ( 'NONE',  ( -20.85000000000000142, 86.48473784507379492, -209.3714211149925575 ) ) ;
#229285 = VECTOR ( 'NONE', #20483, 1000.000000000000000 ) ;
#229286 = ORIENTED_EDGE ( 'NONE', *, *, #153026, .F. ) ;
#229287 = DIRECTION ( 'NONE',  ( -2.952720810173288619E-16, 1.000000000000000000, 0.000000000000000000 ) ) ;
#229288 = CIRCLE ( 'NONE', #95975, 0.1000000000000002554 ) ;
#229289 = ADVANCED_FACE ( 'NONE', ( #227222 ), #231802, .T. ) ;
#229290 = ORIENTED_EDGE ( 'NONE', *, *, #91168, .T. ) ;
#229291 = EDGE_LOOP ( 'NONE', ( #82415, #168153, #91243, #197558 ) ) ;
#229292 = AXIS2_PLACEMENT_3D ( 'NONE', #103470, #104739, #181754 ) ;
#229293 = ADVANCED_FACE ( 'NONE', ( #31631 ), #156981, .F. ) ;
#229294 = ORIENTED_EDGE ( 'NONE', *, *, #166920, .F. ) ;
#229295 = CARTESIAN_POINT ( 'NONE',  ( -16.90138253750126651, 9.950000000011137047, -154.7115627079046192 ) ) ;
#229296 = LINE ( 'NONE', #72810, #217257 ) ;
#229297 = CARTESIAN_POINT ( 'NONE',  ( 21.12400247839524070, 10.72148804404149836, -112.7500000000000284 ) ) ;
#229298 = CARTESIAN_POINT ( 'NONE',  ( -21.12230431290520016, 69.54243334671895127, -103.0283173362133624 ) ) ;
#229299 = FACE_OUTER_BOUND ( 'NONE', #66345, .T. ) ;
#229300 = EDGE_CURVE ( 'NONE', #159966, #170648, #73599, .T. ) ;
#229301 = CARTESIAN_POINT ( 'NONE',  ( -18.50000000000000000, 36.65892442174935439, -249.5511627012433848 ) ) ;
#229302 = DIRECTION ( 'NONE',  ( 0.000000000000000000, 0.2128009952263603399, -0.9770955615653315052 ) ) ;
#229304 = CARTESIAN_POINT ( 'NONE',  ( -23.15000000000000213, 64.35000000001249987, -177.0379132551784096 ) ) ;
#229303 = CARTESIAN_POINT ( 'NONE',  ( 23.24999999999999289, 34.96225128119897363, -245.7638417148289989 ) ) ;
#229305 = CYLINDRICAL_SURFACE ( 'NONE', #133815, 0.1000000000000028644 ) ;
#229306 = EDGE_CURVE ( 'NONE', #100003, #4224, #230909, .T. ) ;
#229307 = CARTESIAN_POINT ( 'NONE',  ( 23.15000000000000213, 62.08591502004790641, -248.5699171172615820 ) ) ;
#229308 = CARTESIAN_POINT ( 'NONE',  ( -20.94999999999999929, 36.65892442174472876, -249.5511627012454596 ) ) ;
#229309 = FACE_OUTER_BOUND ( 'NONE', #58397, .T. ) ;
#229310 = AXIS2_PLACEMENT_3D ( 'NONE', #158781, #235710, #255229 ) ;
#229311 = VERTEX_POINT ( 'NONE', #10755 ) ;
#229312 = ORIENTED_EDGE ( 'NONE', *, *, #114043, .F. ) ;
#229313 = CARTESIAN_POINT ( 'NONE',  ( -18.54260524012581612, -9.624219390073767144, -40.24077304577079417 ) ) ;
#229314 = TOROIDAL_SURFACE ( 'NONE', #220899, 11.65000000000000036, 0.1000000000000000056 ) ;
#229315 = DIRECTION ( 'NONE',  ( 0.000000000000000000, 0.000000000000000000, -1.000000000000000000 ) ) ;
#229316 = DIRECTION ( 'NONE',  ( 0.000000000000000000, -1.000000000000000000, 0.000000000000000000 ) ) ;
#229317 = EDGE_CURVE ( 'NONE', #196737, #258053, #4390, .T. ) ;
#229318 = EDGE_CURVE ( 'NONE', #114424, #71987, #69460, .T. ) ;
#229319 = AXIS2_PLACEMENT_3D ( 'NONE', #185314, #47065, #168365 ) ;
#229320 = DIRECTION ( 'NONE',  ( -0.000000000000000000, -0.000000000000000000, 1.000000000000000000 ) ) ;
#229321 = DIRECTION ( 'NONE',  ( 0.000000000000000000, 0.000000000000000000, 1.000000000000000000 ) ) ;
#229322 = SPHERICAL_SURFACE ( 'NONE', #256292, 0.1000000000000000056 ) ;
#229323 = B_SPLINE_CURVE_WITH_KNOTS ( 'NONE', 3,
 ( #94819, #136495, #98631, #233080, #252604, #54412, #37440, #139045, #176963, #216043, #218602, #119543, #135218, #256397, #16596, #14020, #77813, #96090, #93536, #76537, #173133, #74019, #133941, #153569, #213483, #34888, #114392, #15312, #156117, #123381 ),
 .UNSPECIFIED., .F., .F.,
 ( 4, 2, 2, 2, 2, 2, 2, 2, 2, 2, 2, 2, 2, 2, 4 ),
 ( 0.000000000000000000, 0.0003422764154113352953, 0.0006845528308226705907, 0.001026829246234005778, 0.001369105661645341181, 0.002053658492468005484, 0.002738211323290670220, 0.003080487738702004756, 0.003422764154113338859, 0.003765040569524673829, 0.004107316984936008365, 0.004449593400347343769, 0.004791869815758677438, 0.005134146231170012842, 0.005476422646581347378 ),
 .UNSPECIFIED. ) ;
#229324 = AXIS2_PLACEMENT_3D ( 'NONE', #38121, #118942, #197166 ) ;
#229325 = ORIENTED_EDGE ( 'NONE', *, *, #257807, .T. ) ;
#229326 = ORIENTED_EDGE ( 'NONE', *, *, #219864, .F. ) ;
#229327 = CARTESIAN_POINT ( 'NONE',  ( -15.57281606413133979, 9.370655051123479851, -17.52582325598087820 ) ) ;
#229328 = EDGE_LOOP ( 'NONE', ( #56146, #219133, #232404, #4859 ) ) ;
#229329 = CIRCLE ( 'NONE', #154353, 0.09999999999999939493 ) ;
#229330 = EDGE_CURVE ( 'NONE', #135971, #60723, #190704, .T. ) ;
#229332 = EDGE_CURVE ( 'NONE', #60099, #222619, #206837, .T. ) ;
#229331 = CIRCLE ( 'NONE', #129360, 0.09999999999999939493 ) ;
#229333 = CIRCLE ( 'NONE', #216833, 0.09999999999999939493 ) ;
#229334 = CIRCLE ( 'NONE', #237700, 0.1000000000000028644 ) ;
#229335 = ORIENTED_EDGE ( 'NONE', *, *, #191230, .F. ) ;
#229336 = LINE ( 'NONE', #154947, #255934 ) ;
#229337 = ADVANCED_FACE ( 'NONE', ( #126844 ), #77633, .F. ) ;
#229338 = ORIENTED_EDGE ( 'NONE', *, *, #152927, .F. ) ;
#229339 = DIRECTION ( 'NONE',  ( -1.000000000000000000, 0.000000000000000000, 0.000000000000000000 ) ) ;
#229340 = DIRECTION ( 'NONE',  ( -0.000000000000000000, -1.000000000000000000, -1.734723475976807292E-15 ) ) ;
#229341 = DIRECTION ( 'NONE',  ( -0.000000000000000000, -0.000000000000000000, -1.000000000000000000 ) ) ;
#229342 = CARTESIAN_POINT ( 'NONE',  ( 18.51565452909268217, -9.352859338823158453, -141.1949093212308810 ) ) ;
#229343 = DIRECTION ( 'NONE',  ( 0.000000000000000000, 0.000000000000000000, 1.000000000000000000 ) ) ;
#229344 = ADVANCED_FACE ( 'NONE', ( #87697 ), #57152, .F. ) ;
#229345 = AXIS2_PLACEMENT_3D ( 'NONE', #49536, #7853, #129074 ) ;
#229346 = DIRECTION ( 'NONE',  ( 0.000000000000000000, 0.8814952561688431665, -0.4721928772777345129 ) ) ;
#229347 = DIRECTION ( 'NONE',  ( 0.000000000000000000, 6.982962677686266711E-15, -1.000000000000000000 ) ) ;
#229348 = DIRECTION ( 'NONE',  ( 0.000000000000000000, -0.9651348961777156399, 0.2617529984165037349 ) ) ;
#229351 = ORIENTED_EDGE ( 'NONE', *, *, #60861, .T. ) ;
#229350 = ADVANCED_FACE ( 'NONE', ( #246779 ), #223756, .T. ) ;
#229349 = DIRECTION ( 'NONE',  ( 1.000000000000000000, -0.000000000000000000, 0.000000000000000000 ) ) ;
#229353 = CARTESIAN_POINT ( 'NONE',  ( 20.04142135623730070, 11.75000000001115907, -188.8499999999999659 ) ) ;
#229352 = PLANE ( 'NONE',  #136939 ) ;
#229354 = VERTEX_POINT ( 'NONE', #35485 ) ;
#229356 = VERTEX_POINT ( 'NONE', #237513 ) ;
#229355 = DIRECTION ( 'NONE',  ( -0.000000000000000000, -0.000000000000000000, -1.000000000000000000 ) ) ;
#229357 = ORIENTED_EDGE ( 'NONE', *, *, #84789, .F. ) ;
#229358 = FACE_OUTER_BOUND ( 'NONE', #61573, .T. ) ;
#229359 = CARTESIAN_POINT ( 'NONE',  ( -18.35663730107557257, 11.47390742652235573, -143.2500000000000284 ) ) ;
#229360 = FACE_OUTER_BOUND ( 'NONE', #29089, .T. ) ;
#229361 = DIRECTION ( 'NONE',  ( 1.000000000000000000, 0.000000000000000000, 0.000000000000000000 ) ) ;
#229362 = CARTESIAN_POINT ( 'NONE',  ( -21.05000000000000071, 6.300000000011169554, -167.5999999999999659 ) ) ;
#229363 = ADVANCED_FACE ( 'NONE', ( #95423 ), #178851, .T. ) ;
#229364 = DIRECTION ( 'NONE',  ( 0.000000000000000000, 0.000000000000000000, 1.000000000000000000 ) ) ;
#229365 = DIRECTION ( 'NONE',  ( -3.469446951953515108E-14, -1.000000000000000000, 0.000000000000000000 ) ) ;
#229366 = AXIS2_PLACEMENT_3D ( 'NONE', #247691, #69075, #164319 ) ;
#229367 = DIRECTION ( 'NONE',  ( 0.000000000000000000, -1.000000000000000000, 2.775557561562888827E-14 ) ) ;
#229368 = DIRECTION ( 'NONE',  ( 0.000000000000000000, 0.000000000000000000, -1.000000000000000000 ) ) ;
#229369 = EDGE_CURVE ( 'NONE', #18621, #80050, #15919, .T. ) ;
#229370 = VERTEX_POINT ( 'NONE', #57561 ) ;
#229371 = EDGE_LOOP ( 'NONE', ( #238752, #221332, #3962, #254140 ) ) ;
#229372 = CARTESIAN_POINT ( 'NONE',  ( -20.54999999999999716, 1.925233644870972816, -180.2302435331260995 ) ) ;
#229373 = AXIS2_PLACEMENT_3D ( 'NONE', #22201, #1315, #144680 ) ;
#229374 = ORIENTED_EDGE ( 'NONE', *, *, #95071, .T. ) ;
#229375 = CARTESIAN_POINT ( 'NONE',  ( -23.15000000000000213, 2.272311100394799332, -217.9150152700588592 ) ) ;
#229376 = ORIENTED_EDGE ( 'NONE', *, *, #248371, .F. ) ;
#229377 = CARTESIAN_POINT ( 'NONE',  ( 18.50000000000000355, -9.480686695278970788, -40.44111516875785384 ) ) ;
#229378 = CIRCLE ( 'NONE', #116937, 0.1000000000000004496 ) ;
#229379 = CARTESIAN_POINT ( 'NONE',  ( 21.14999999999999503, -0.09999999998884338825, -55.35042919245524473 ) ) ;
#229380 = DIRECTION ( 'NONE',  ( -1.000000000000000000, 0.000000000000000000, -0.000000000000000000 ) ) ;
#229381 = EDGE_CURVE ( 'NONE', #199664, #17643, #113702, .T. ) ;
#229382 = FACE_OUTER_BOUND ( 'NONE', #161456, .T. ) ;
#229383 = CARTESIAN_POINT ( 'NONE',  ( 20.94999999999999574, 0.6713328740235187109, -212.7808875799876205 ) ) ;
#229384 = ORIENTED_EDGE ( 'NONE', *, *, #24625, .F. ) ;
#229385 = DIRECTION ( 'NONE',  ( 2.694716079187273439E-16, 1.000000000000000000, 6.467318590049456648E-15 ) ) ;
#229386 = VECTOR ( 'NONE', #82235, 1000.000000000000000 ) ;
#229387 = CARTESIAN_POINT ( 'NONE',  ( 23.14999999999999858, 6.277629359189123903, -229.8243190661787878 ) ) ;
#229388 = CARTESIAN_POINT ( 'NONE',  ( 23.24999999999999289, 64.35000000001195986, -110.0379132551783243 ) ) ;
#229389 = CARTESIAN_POINT ( 'NONE',  ( -21.05000000000000782, 6.332272273946818686, -134.0375360632857280 ) ) ;
#229390 = LINE ( 'NONE', #188969, #110096 ) ;
#229391 = ORIENTED_EDGE ( 'NONE', *, *, #248772, .T. ) ;
#229394 = DIRECTION ( 'NONE',  ( 1.000000000000000000, 0.000000000000000000, 0.000000000000000000 ) ) ;
#229393 = CARTESIAN_POINT ( 'NONE',  ( 21.14250536705908345, 60.94035912585616188, -234.1489753949848023 ) ) ;
#229392 = VECTOR ( 'NONE', #241395, 999.9999999999998863 ) ;
#229395 = EDGE_LOOP ( 'NONE', ( #190289, #51510, #202589, #17848 ) ) ;
#229398 = ORIENTED_EDGE ( 'NONE', *, *, #18515, .F. ) ;
#229397 = CARTESIAN_POINT ( 'NONE',  ( 20.95392731769792150, 67.11693852082356671, -161.5008795049531329 ) ) ;
#229396 = CARTESIAN_POINT ( 'NONE',  ( -18.59999999999999787, 64.35000000001264198, -196.5083017138704236 ) ) ;
#229399 = CARTESIAN_POINT ( 'NONE',  ( 18.59999999999999787, -9.399999999988843058, -140.8820418481727188 ) ) ;
#229400 = CIRCLE ( 'NONE', #116954, 0.09999999999998898659 ) ;
#229401 = DIRECTION ( 'NONE',  ( 0.000000000000000000, -6.308085367188393199E-16, -1.000000000000000000 ) ) ;
#229402 = ORIENTED_EDGE ( 'NONE', *, *, #244689, .T. ) ;
#229403 = CARTESIAN_POINT ( 'NONE',  ( -21.44999999999999929, 63.53703427598990316, -222.1606900896233583 ) ) ;
#229404 = CARTESIAN_POINT ( 'NONE',  ( 23.15000000000000213, 85.50000000001149658, -45.91707660717669626 ) ) ;
#229406 = FACE_OUTER_BOUND ( 'NONE', #138816, .T. ) ;
#229405 = DIRECTION ( 'NONE',  ( 0.000000000000000000, 1.000000000000000000, 0.000000000000000000 ) ) ;
#229408 = VERTEX_POINT ( 'NONE', #253204 ) ;
#229407 = CARTESIAN_POINT ( 'NONE',  ( -18.46902351632716943, 46.92263674392135187, -255.3732559572131606 ) ) ;
#229409 = AXIS2_PLACEMENT_3D ( 'NONE', #211111, #170756, #50719 ) ;
#229410 = ORIENTED_EDGE ( 'NONE', *, *, #72956, .T. ) ;
#229411 = FACE_OUTER_BOUND ( 'NONE', #242253, .T. ) ;
#229412 = CARTESIAN_POINT ( 'NONE',  ( 21.05000000000000071, 69.05648948627111849, -235.0374527038057977 ) ) ;
#229413 = DIRECTION ( 'NONE',  ( 3.265361837132813093E-16, 1.000000000000000000, 6.982962677686266711E-15 ) ) ;
#229414 = VERTEX_POINT ( 'NONE', #58835 ) ;
#229415 = DIRECTION ( 'NONE',  ( 0.000000000000000000, -0.9126074666063622720, -0.4088369013363611360 ) ) ;
#229416 = DIRECTION ( 'NONE',  ( -0.000000000000000000, 6.982962677686266711E-15, -1.000000000000000000 ) ) ;
#229417 = CARTESIAN_POINT ( 'NONE',  ( -21.05000000000000071, 14.05000000001115623, -106.0136950707610310 ) ) ;
#229418 = ORIENTED_EDGE ( 'NONE', *, *, #115220, .T. ) ;
#229419 = PLANE ( 'NONE',  #237901 ) ;
#229420 = VECTOR ( 'NONE', #24645, 1000.000000000000000 ) ;
#229422 = EDGE_CURVE ( 'NONE', #245188, #128091, #17190, .T. ) ;
#229421 = VECTOR ( 'NONE', #109986, 1000.000000000000000 ) ;
#229423 = ORIENTED_EDGE ( 'NONE', *, *, #230660, .F. ) ;
#229424 = VECTOR ( 'NONE', #176345, 1000.000000000000000 ) ;
#229425 = DIRECTION ( 'NONE',  ( 0.000000000000000000, 0.000000000000000000, 1.000000000000000000 ) ) ;
#229426 = DIRECTION ( 'NONE',  ( -1.000000000000000000, -0.000000000000000000, -0.000000000000000000 ) ) ;
#229427 = ORIENTED_EDGE ( 'NONE', *, *, #5792, .T. ) ;
#229428 = VECTOR ( 'NONE', #34315, 1000.000000000000000 ) ;
#229429 = ORIENTED_EDGE ( 'NONE', *, *, #197404, .F. ) ;
#229430 = CARTESIAN_POINT ( 'NONE',  ( 19.99999999999998934, 64.25000000001253397, -182.1731074845244507 ) ) ;
#229431 = ORIENTED_EDGE ( 'NONE', *, *, #136219, .T. ) ;
#229433 = ORIENTED_EDGE ( 'NONE', *, *, #125056, .T. ) ;
#229432 = DIRECTION ( 'NONE',  ( 0.000000000000000000, 0.000000000000000000, -1.000000000000000000 ) ) ;
#229434 = EDGE_LOOP ( 'NONE', ( #222601, #205262, #53793 ) ) ;
#229436 = EDGE_CURVE ( 'NONE', #210699, #172995, #152896, .T. ) ;
#229435 = AXIS2_PLACEMENT_3D ( 'NONE', #41673, #101587, #102883 ) ;
#229439 = ORIENTED_EDGE ( 'NONE', *, *, #246905, .F. ) ;
#229438 = ORIENTED_EDGE ( 'NONE', *, *, #132732, .T. ) ;
#229437 = DIRECTION ( 'NONE',  ( 1.000000000000000000, 0.000000000000000000, 0.000000000000000000 ) ) ;
#229440 = DIRECTION ( 'NONE',  ( 0.000000000000000000, 0.9126074666063770380, 0.4088369013363281068 ) ) ;
#229441 = EDGE_LOOP ( 'NONE', ( #135209, #162825, #206380, #198062, #119491 ) ) ;
#229442 = CARTESIAN_POINT ( 'NONE',  ( 21.13461538461538325, 22.21093039075207898, -231.7318303787629930 ) ) ;
#229443 = CARTESIAN_POINT ( 'NONE',  ( -21.05000000000000071, -1.299020131538773271, -194.8773804188782606 ) ) ;
#229444 = DIRECTION ( 'NONE',  ( 1.000000000000000000, 2.952720810173289112E-16, -0.000000000000000000 ) ) ;
#229445 = CARTESIAN_POINT ( 'NONE',  ( 20.95000000000005969, 67.73741572762334329, -25.54575917482290848 ) ) ;
#229446 = ORIENTED_EDGE ( 'NONE', *, *, #195271, .T. ) ;
#229447 = ORIENTED_EDGE ( 'NONE', *, *, #33500, .T. ) ;
#229448 = ORIENTED_EDGE ( 'NONE', *, *, #257839, .T. ) ;
#229449 = ADVANCED_FACE ( 'NONE', ( #138376 ), #52887, .T. ) ;
#229450 = FACE_OUTER_BOUND ( 'NONE', #131606, .T. ) ;
#229453 = EDGE_LOOP ( 'NONE', ( #44955, #34218, #212900, #57534 ) ) ;
#229452 = EDGE_CURVE ( 'NONE', #104231, #18666, #177830, .T. ) ;
#229451 = CARTESIAN_POINT ( 'NONE',  ( -16.93344882324368683, 66.00341123272467314, -182.6100817897194872 ) ) ;
#229454 = DIRECTION ( 'NONE',  ( 0.000000000000000000, 0.8814952561688430555, -0.4721928772777346239 ) ) ;
#229456 = ORIENTED_EDGE ( 'NONE', *, *, #258025, .T. ) ;
#229455 = CARTESIAN_POINT ( 'NONE',  ( 18.45068634130097962, 78.23730655674349066, -231.5159231784034546 ) ) ;
#229457 = AXIS2_PLACEMENT_3D ( 'NONE', #256141, #133695, #234073 ) ;
#229458 = VERTEX_POINT ( 'NONE', #118857 ) ;
#229459 = FACE_OUTER_BOUND ( 'NONE', #129986, .T. ) ;
#229460 = EDGE_CURVE ( 'NONE', #250767, #216880, #256857, .T. ) ;
#229461 = VECTOR ( 'NONE', #162562, 1000.000000000000000 ) ;
#229462 = ORIENTED_EDGE ( 'NONE', *, *, #5748, .F. ) ;
#229463 = ADVANCED_FACE ( 'NONE', ( #137123 ), #74618, .T. ) ;
#229465 = VECTOR ( 'NONE', #121632, 1000.000000000000000 ) ;
#229464 = CARTESIAN_POINT ( 'NONE',  ( -16.94878442675510399, 66.00827089702124795, -149.1348879088865829 ) ) ;
#229466 = CARTESIAN_POINT ( 'NONE',  ( 20.73486653747088937, 7.750000000011182166, -87.85000000000003695 ) ) ;
#229468 = ORIENTED_EDGE ( 'NONE', *, *, #174552, .T. ) ;
#229467 = ORIENTED_EDGE ( 'NONE', *, *, #105792, .F. ) ;
#229469 = EDGE_LOOP ( 'NONE', ( #155859, #253561, #73883, #170830 ) ) ;
#229471 = DIRECTION ( 'NONE',  ( 1.000000000000000000, 0.000000000000000000, 0.000000000000000000 ) ) ;
#229470 = VECTOR ( 'NONE', #57639, 1000.000000000000000 ) ;
#229473 = ORIENTED_EDGE ( 'NONE', *, *, #182176, .F. ) ;
#229472 = EDGE_CURVE ( 'NONE', #53148, #20990, #114985, .T. ) ;
#229474 = ORIENTED_EDGE ( 'NONE', *, *, #193976, .F. ) ;
#229475 = DIRECTION ( 'NONE',  ( 1.000000000000000000, -0.000000000000000000, -0.000000000000000000 ) ) ;
#229476 = VECTOR ( 'NONE', #130762, 1000.000000000000000 ) ;
#229478 = ORIENTED_EDGE ( 'NONE', *, *, #98490, .F. ) ;
#229477 = DIRECTION ( 'NONE',  ( 0.000000000000000000, -0.1568667991644355497, -0.9876197685951332295 ) ) ;
#229479 = DIRECTION ( 'NONE',  ( 0.000000000000000000, 0.000000000000000000, -1.000000000000000000 ) ) ;
#229481 = FACE_OUTER_BOUND ( 'NONE', #249793, .T. ) ;
#229480 = FACE_OUTER_BOUND ( 'NONE', #31349, .T. ) ;
#229482 = CARTESIAN_POINT ( 'NONE',  ( 20.94999999999999929, -11.29603075032412640, -130.9521008403361861 ) ) ;
#229483 = FACE_OUTER_BOUND ( 'NONE', #204807, .T. ) ;
#229484 = ORIENTED_EDGE ( 'NONE', *, *, #158598, .T. ) ;
#229486 = ADVANCED_FACE ( 'NONE', ( #18455 ), #176273, .T. ) ;
#229485 = ORIENTED_EDGE ( 'NONE', *, *, #12355, .F. ) ;
#229487 = DIRECTION ( 'NONE',  ( -0.000000000000000000, 0.7397360091702694929, 0.6728971962616898672 ) ) ;
#229488 = DIRECTION ( 'NONE',  ( -3.787827842127535236E-15, -0.9165223833629844163, 0.3999834006488702243 ) ) ;
#229490 = VERTEX_POINT ( 'NONE', #156718 ) ;
#229489 = VECTOR ( 'NONE', #155291, 1000.000000000000000 ) ;
#229491 = CIRCLE ( 'NONE', #341, 0.1000000000000028644 ) ;
#229492 = AXIS2_PLACEMENT_3D ( 'NONE', #242809, #162020, #19939 ) ;
#229493 = DIRECTION ( 'NONE',  ( 0.000000000000000000, 0.8700118002898322711, -0.4930308989875231696 ) ) ;
#229494 = CARTESIAN_POINT ( 'NONE',  ( -23.25000000000000000, 2.272311100394799332, -217.9150152700588592 ) ) ;
#229495 = ORIENTED_EDGE ( 'NONE', *, *, #144550, .T. ) ;
#229496 = EDGE_LOOP ( 'NONE', ( #222925, #200894, #5217, #45287 ) ) ;
#229497 = AXIS2_PLACEMENT_3D ( 'NONE', #44226, #202007, #179891 ) ;
#229498 = CARTESIAN_POINT ( 'NONE',  ( -20.64999999999999858, 2.500000000011154633, -154.2753780772379173 ) ) ;
#229499 = CARTESIAN_POINT ( 'NONE',  ( 21.05000000000000071, -8.999999999988842703, -191.1060308773475072 ) ) ;
#229500 = VERTEX_POINT ( 'NONE', #216652 ) ;
#229501 = CARTESIAN_POINT ( 'NONE',  ( -20.65000000000000568, 7.250000000011138646, -180.1499999999999773 ) ) ;
#229502 = ORIENTED_EDGE ( 'NONE', *, *, #158862, .F. ) ;
#229503 = TOROIDAL_SURFACE ( 'NONE', #21241, 0.2000000000000000111, 0.1000000000000000056 ) ;
#229504 = CARTESIAN_POINT ( 'NONE',  ( -21.05000000000000071, 6.413759733821437159, -100.5856130608040360 ) ) ;
#229506 = CIRCLE ( 'NONE', #29606, 0.09999999999999975575 ) ;
#229505 = CARTESIAN_POINT ( 'NONE',  ( 21.14999999999999858, 1.115600667400684642E-11, -112.6500000000000341 ) ) ;
#229508 = DIRECTION ( 'NONE',  ( 0.000000000000000000, 1.000000000000000000, 6.982962677686266711E-15 ) ) ;
#229507 = DIRECTION ( 'NONE',  ( -0.000000000000000000, -0.2617529984165031243, -0.9651348961777157509 ) ) ;
#229509 = DIRECTION ( 'NONE',  ( -0.000000000000000000, 1.000000000000000000, 6.982962677686266711E-15 ) ) ;
#229510 = CYLINDRICAL_SURFACE ( 'NONE', #199230, 0.1000000000000028644 ) ;
#229511 = DIRECTION ( 'NONE',  ( 0.000000000000000000, 0.000000000000000000, -1.000000000000000000 ) ) ;
#229512 = DIRECTION ( 'NONE',  ( 0.000000000000000000, 0.000000000000000000, -1.000000000000000000 ) ) ;
#229514 = ORIENTED_EDGE ( 'NONE', *, *, #155463, .T. ) ;
#229513 = CYLINDRICAL_SURFACE ( 'NONE', #102462, 0.09999999999999939493 ) ;
#229515 = VECTOR ( 'NONE', #166431, 1000.000000000000114 ) ;
#229516 = CIRCLE ( 'NONE', #62906, 0.1000000000000013933 ) ;
#229517 = EDGE_CURVE ( 'NONE', #228315, #2789, #40477, .T. ) ;
#229519 = EDGE_LOOP ( 'NONE', ( #41358, #31409, #86461, #160354 ) ) ;
#229518 = ORIENTED_EDGE ( 'NONE', *, *, #93584, .F. ) ;
#229520 = ORIENTED_EDGE ( 'NONE', *, *, #87458, .F. ) ;
#229521 = EDGE_CURVE ( 'NONE', #211804, #173014, #136254, .T. ) ;
#229522 = CARTESIAN_POINT ( 'NONE',  ( -18.50000000000000711, 11.64999999999999680, -7.014805770653998351 ) ) ;
#229523 = CARTESIAN_POINT ( 'NONE',  ( -23.15000000000000213, 74.07476635515175190, -56.79286395139820343 ) ) ;
#229524 = EDGE_CURVE ( 'NONE', #220102, #3155, #240359, .T. ) ;
#229525 = EDGE_CURVE ( 'NONE', #53632, #176194, #212815, .T. ) ;
#229527 = DIRECTION ( 'NONE',  ( 1.000000000000000000, 0.000000000000000000, -0.000000000000000000 ) ) ;
#229526 = CARTESIAN_POINT ( 'NONE',  ( 20.09999999999999787, 9.750000000011137757, -180.1499999999999773 ) ) ;
#229528 = DIRECTION ( 'NONE',  ( 0.000000000000000000, -0.8660254037844411501, -0.4999999999999956701 ) ) ;
#229529 = ORIENTED_EDGE ( 'NONE', *, *, #160121, .F. ) ;
#229530 = CARTESIAN_POINT ( 'NONE',  ( -22.59066674512252249, 11.75000000001115552, -100.4694958763693791 ) ) ;
#229531 = ORIENTED_EDGE ( 'NONE', *, *, #10501, .F. ) ;
#229532 = CARTESIAN_POINT ( 'NONE',  ( -21.04999999999999716, 0.01485563489362509877, 6.344359042043403285 ) ) ;
#229533 = DIRECTION ( 'NONE',  ( 0.000000000000000000, 6.938893903907270030E-14, 1.000000000000000000 ) ) ;
#229534 = EDGE_CURVE ( 'NONE', #131951, #116019, #111167, .T. ) ;
#229535 = DIRECTION ( 'NONE',  ( 1.000000000000000000, 0.000000000000000000, 0.000000000000000000 ) ) ;
#229536 = ORIENTED_EDGE ( 'NONE', *, *, #35440, .F. ) ;
#229537 = EDGE_CURVE ( 'NONE', #14440, #133775, #105669, .T. ) ;
#229538 = EDGE_CURVE ( 'NONE', #18191, #39515, #23631, .T. ) ;
#229539 = DIRECTION ( 'NONE',  ( 0.000000000000000000, 0.2128009952263604232, -0.9770955615653316162 ) ) ;
#229540 = FACE_OUTER_BOUND ( 'NONE', #126449, .T. ) ;
#229541 = ORIENTED_EDGE ( 'NONE', *, *, #1416, .F. ) ;
#229542 = ORIENTED_EDGE ( 'NONE', *, *, #210732, .F. ) ;
#229543 = DIRECTION ( 'NONE',  ( 0.7071067811865475727, 0.7071067811865475727, 0.000000000000000000 ) ) ;
#229544 = CARTESIAN_POINT ( 'NONE',  ( -16.91256925476569606, 9.985731158139328656, -54.46764248900526439 ) ) ;
#229545 = EDGE_CURVE ( 'NONE', #108305, #34745, #36362, .T. ) ;
#229546 = LINE ( 'NONE', #169610, #61315 ) ;
#229547 = CARTESIAN_POINT ( 'NONE',  ( 18.59999999999999432, 7.783179459866045313, -245.3643104511423303 ) ) ;
#229548 = DIRECTION ( 'NONE',  ( 0.000000000000000000, 0.000000000000000000, -1.000000000000000000 ) ) ;
#229549 = CARTESIAN_POINT ( 'NONE',  ( -21.09107601085575112, 6.363877975359904404, 0.03930716471739981871 ) ) ;
#229550 = ORIENTED_EDGE ( 'NONE', *, *, #30098, .T. ) ;
#229551 = CARTESIAN_POINT ( 'NONE',  ( -23.15000000000000213, 64.35000000001228670, -157.8731074845244393 ) ) ;
#229552 = AXIS2_PLACEMENT_3D ( 'NONE', #243523, #166589, #144396 ) ;
#229553 = CARTESIAN_POINT ( 'NONE',  ( -22.47007471830799119, 7.720710651937631397, -33.50000000000001421 ) ) ;
#229554 = EDGE_CURVE ( 'NONE', #6055, #230164, #111351, .T. ) ;
#229556 = CARTESIAN_POINT ( 'NONE',  ( 20.94999999999999929, 1.115600667400684642E-11, -33.50000000000000000 ) ) ;
#229555 = FACE_OUTER_BOUND ( 'NONE', #5872, .T. ) ;
#229557 = DIRECTION ( 'NONE',  ( 2.952720810173289112E-16, -1.000000000000000000, 0.000000000000000000 ) ) ;
#229558 = DIRECTION ( 'NONE',  ( 0.000000000000000000, 0.000000000000000000, 1.000000000000000000 ) ) ;
#229559 = DIRECTION ( 'NONE',  ( 1.000000000000000000, 0.000000000000000000, 0.000000000000000000 ) ) ;
#229560 = CARTESIAN_POINT ( 'NONE',  ( 23.25000000000000355, 98.45632476063501315, -129.7292090367925255 ) ) ;
#229561 = ADVANCED_FACE ( 'NONE', ( #40631 ), #223067, .F. ) ;
#229562 = EDGE_CURVE ( 'NONE', #17420, #189223, #142249, .T. ) ;
#229564 = EDGE_LOOP ( 'NONE', ( #95112, #131269, #205154 ) ) ;
#229563 = CARTESIAN_POINT ( 'NONE',  ( -23.25000000000000000, 19.89303971870268839, -235.6353404070293038 ) ) ;
#229565 = EDGE_CURVE ( 'NONE', #231005, #40222, #199686, .T. ) ;
#229566 = AXIS2_PLACEMENT_3D ( 'NONE', #140351, #7259, #128508 ) ;
#229567 = EDGE_CURVE ( 'NONE', #51895, #36183, #123990, .T. ) ;
#229568 = EDGE_CURVE ( 'NONE', #214956, #70987, #43163, .T. ) ;
#229569 = CARTESIAN_POINT ( 'NONE',  ( -22.50014994444008565, 64.25028026811963855, -103.1061876412435936 ) ) ;
#229570 = FACE_OUTER_BOUND ( 'NONE', #225482, .T. ) ;
#229571 = LINE ( 'NONE', #210009, #54671 ) ;
#229572 = CIRCLE ( 'NONE', #100354, 0.09999999999999681366 ) ;
#229573 = ORIENTED_EDGE ( 'NONE', *, *, #191849, .T. ) ;
#229574 = CIRCLE ( 'NONE', #187884, 0.09999999999999939493 ) ;
#229575 = FACE_OUTER_BOUND ( 'NONE', #56819, .T. ) ;
#229576 = DIRECTION ( 'NONE',  ( 0.000000000000000000, 7.147358527629762208E-15, -1.000000000000000000 ) ) ;
#229578 = LINE ( 'NONE', #50898, #190560 ) ;
#229577 = AXIS2_PLACEMENT_3D ( 'NONE', #189386, #66867, #167282 ) ;
#229579 = ORIENTED_EDGE ( 'NONE', *, *, #114716, .F. ) ;
#229580 = CARTESIAN_POINT ( 'NONE',  ( -16.86757978335471719, 12.41826068153812024, -211.1887541124544327 ) ) ;
#229582 = ORIENTED_EDGE ( 'NONE', *, *, #234234, .T. ) ;
#229581 = FACE_OUTER_BOUND ( 'NONE', #196656, .T. ) ;
#229583 = LINE ( 'NONE', #92611, #42387 ) ;
#229584 = CARTESIAN_POINT ( 'NONE',  ( 18.59999999999999432, 74.83729825007388570, -94.92310748452432279 ) ) ;
#229585 = ORIENTED_EDGE ( 'NONE', *, *, #114546, .T. ) ;
#229586 = CARTESIAN_POINT ( 'NONE',  ( -18.59999999999999787, 64.25000000001246292, -181.7731074845244450 ) ) ;
#229587 = APPLICATION_PROTOCOL_DEFINITION ( 'draft international standard', 'automotive_design', 1998, #225608 ) ;
#229588 = CARTESIAN_POINT ( 'NONE',  ( 18.49999999999999645, 1.115600667400684642E-11, -167.5000000000000284 ) ) ;
#229589 = DIRECTION ( 'NONE',  ( 0.000000000000000000, 0.000000000000000000, 1.000000000000000000 ) ) ;
#229590 = DIRECTION ( 'NONE',  ( 0.000000000000000000, 5.956132106358139644E-15, -1.000000000000000000 ) ) ;
#229591 = VECTOR ( 'NONE', #26413, 999.9999999999998863 ) ;
#229592 = ORIENTED_EDGE ( 'NONE', *, *, #185598, .F. ) ;
#229593 = DIRECTION ( 'NONE',  ( 0.000000000000000000, -6.938893903907222067E-15, 1.000000000000000000 ) ) ;
#229594 = DIRECTION ( 'NONE',  ( 1.186688945009010077E-16, 0.4088369013363280513, -0.9126074666063769270 ) ) ;
#229595 = CARTESIAN_POINT ( 'NONE',  ( 20.95224633520496127, 8.900522166568386240, -175.9932764479212324 ) ) ;
#229596 = ORIENTED_EDGE ( 'NONE', *, *, #208596, .T. ) ;
#229597 = ORIENTED_EDGE ( 'NONE', *, *, #110386, .T. ) ;
#229598 = CARTESIAN_POINT ( 'NONE',  ( 23.04999999999999716, 67.17743825834511995, -48.67310748452439384 ) ) ;
#229599 = CARTESIAN_POINT ( 'NONE',  ( -20.54999999999999716, 1.115600667400684642E-11, -165.5000000000000284 ) ) ;
#229600 = DIRECTION ( 'NONE',  ( 0.000000000000000000, -0.4088369013363783999, 0.9126074666063545004 ) ) ;
#229601 = EDGE_CURVE ( 'NONE', #25862, #62, #182089, .T. ) ;
#229603 = DIRECTION ( 'NONE',  ( -0.000000000000000000, 1.000000000000000000, -0.000000000000000000 ) ) ;
#229602 = CIRCLE ( 'NONE', #62996, 0.09999999999999990841 ) ;
#229604 = AXIS2_PLACEMENT_3D ( 'NONE', #111625, #232878, #192448 ) ;
#229607 = DIRECTION ( 'NONE',  ( 0.000000000000000000, -6.982962677686266711E-15, 1.000000000000000000 ) ) ;
#229606 = AXIS2_PLACEMENT_3D ( 'NONE', #137829, #178288, #217364 ) ;
#229605 = DIRECTION ( 'NONE',  ( 0.000000000000000000, -6.982962677686266711E-15, 1.000000000000000000 ) ) ;
#229608 = DIRECTION ( 'NONE',  ( -1.000000000000000000, -1.836970198721029934E-16, -0.000000000000000000 ) ) ;
#229609 = ADVANCED_FACE ( 'NONE', ( #238794 ), #61284, .T. ) ;
#229610 = CARTESIAN_POINT ( 'NONE',  ( -22.39999999999999858, 7.591056067193246548, -199.2444047917219052 ) ) ;
#229611 = DIRECTION ( 'NONE',  ( 1.000000000000000000, 0.000000000000000000, 0.000000000000000000 ) ) ;
#229612 = VERTEX_POINT ( 'NONE', #143530 ) ;
#229614 = ORIENTED_EDGE ( 'NONE', *, *, #225162, .F. ) ;
#229613 = CARTESIAN_POINT ( 'NONE',  ( -16.87383368123029825, 12.41403342719998371, -211.2428889513006993 ) ) ;
#229615 = CARTESIAN_POINT ( 'NONE',  ( -16.77683809663752257, 66.05416425680790837, -123.8591584654201512 ) ) ;
#229616 = CARTESIAN_POINT ( 'NONE',  ( -21.07928932188134041, -1.250084634896336366, -194.7953894783290423 ) ) ;
#229618 = LINE ( 'NONE', #164518, #53344 ) ;
#229617 = CARTESIAN_POINT ( 'NONE',  ( -20.94999999999999929, 7.128833340094563376, -233.7327013124401276 ) ) ;
#229619 = EDGE_CURVE ( 'NONE', #162643, #53701, #207021, .T. ) ;
#229620 = EDGE_CURVE ( 'NONE', #127854, #91133, #24903, .T. ) ;
#229621 = ORIENTED_EDGE ( 'NONE', *, *, #219166, .T. ) ;
#229622 = CARTESIAN_POINT ( 'NONE',  ( -16.89268316805465986, 66.04827818676982076, -115.6673550059788340 ) ) ;
#229623 = CARTESIAN_POINT ( 'NONE',  ( 19.87657994472052536, 64.25000000001196554, -111.7573193598979628 ) ) ;
#229624 = FACE_OUTER_BOUND ( 'NONE', #40892, .T. ) ;
#229625 = CYLINDRICAL_SURFACE ( 'NONE', #23359, 11.75000000000001066 ) ;
#229626 = EDGE_LOOP ( 'NONE', ( #24252, #220925, #152250, #219926, #10918, #34922, #238498, #191244, #45304, #119376, #173359, #243252, #137498, #115370 ) ) ;
#229628 = ORIENTED_EDGE ( 'NONE', *, *, #53447, .T. ) ;
#229627 = VECTOR ( 'NONE', #178312, 1000.000000000000000 ) ;
#229629 = DIRECTION ( 'NONE',  ( 1.000000000000000000, 0.000000000000000000, -0.000000000000000000 ) ) ;
#229630 = ORIENTED_EDGE ( 'NONE', *, *, #101539, .F. ) ;
#229631 = CARTESIAN_POINT ( 'NONE',  ( -16.87683809663752399, 9.849999999999985434, -12.65000000000000213 ) ) ;
#229632 = CARTESIAN_POINT ( 'NONE',  ( 21.05000000000000071, 10.42338541492406279, -141.4920519238701218 ) ) ;
#229633 = EDGE_CURVE ( 'NONE', #214190, #67836, #160559, .T. ) ;
#229634 = CARTESIAN_POINT ( 'NONE',  ( -18.40000000000000213, 28.17589918783267322, -238.5974746063260739 ) ) ;
#229635 = CARTESIAN_POINT ( 'NONE',  ( -20.85000000000000142, 1.115600667400684642E-11, -67.00000000000000000 ) ) ;
#229636 = ORIENTED_EDGE ( 'NONE', *, *, #232700, .T. ) ;
#229637 = FACE_OUTER_BOUND ( 'NONE', #217140, .T. ) ;
#229638 = AXIS2_PLACEMENT_3D ( 'NONE', #67000, #106099, #146517 ) ;
#229639 = CARTESIAN_POINT ( 'NONE',  ( -21.05000000000000071, 86.55507603484990398, -209.4941099044519603 ) ) ;
#229640 = CARTESIAN_POINT ( 'NONE',  ( -18.59999999999999787, 7.070967871809997973, -104.2465642218683541 ) ) ;
#229641 = AXIS2_PLACEMENT_3D ( 'NONE', #128252, #207812, #104787 ) ;
#229642 = CARTESIAN_POINT ( 'NONE',  ( 23.14999999999999858, 11.60000000001116227, -127.0717967697245427 ) ) ;
#229643 = DIRECTION ( 'NONE',  ( 0.000000000000000000, 1.000000000000000000, 0.000000000000000000 ) ) ;
#229644 = EDGE_CURVE ( 'NONE', #223778, #122251, #146044, .T. ) ;
#229645 = DIRECTION ( 'NONE',  ( 0.000000000000000000, 0.000000000000000000, -1.000000000000000000 ) ) ;
#229647 = CARTESIAN_POINT ( 'NONE',  ( 18.54999999999999716, 67.25000000001178080, -82.17310748452437963 ) ) ;
#229646 = AXIS2_PLACEMENT_3D ( 'NONE', #97197, #95949, #158531 ) ;
#229649 = ORIENTED_EDGE ( 'NONE', *, *, #141602, .T. ) ;
#229648 = ADVANCED_FACE ( 'NONE', ( #61436 ), #140987, .F. ) ;
#229651 = DIRECTION ( 'NONE',  ( -1.000000000000000000, -0.000000000000000000, -0.000000000000000000 ) ) ;
#229650 = CARTESIAN_POINT ( 'NONE',  ( -16.89020380669786192, 66.05000000001207638, -123.7656963364138534 ) ) ;
#229652 = ORIENTED_EDGE ( 'NONE', *, *, #51400, .T. ) ;
#229653 = ORIENTED_EDGE ( 'NONE', *, *, #54134, .F. ) ;
#229654 = ORIENTED_EDGE ( 'NONE', *, *, #11440, .T. ) ;
#229655 = CARTESIAN_POINT ( 'NONE',  ( -23.15000000000000213, 75.49601185175265528, -250.2710592679604531 ) ) ;
#229656 = VECTOR ( 'NONE', #214455, 1000.000000000000000 ) ;
#229657 = CARTESIAN_POINT ( 'NONE',  ( 15.73863059295127798, 66.64859682587062650, -153.0435770476859147 ) ) ;
#229658 = DIRECTION ( 'NONE',  ( 0.000000000000000000, 1.000000000000000000, 6.982962677686266711E-15 ) ) ;
#229659 = CARTESIAN_POINT ( 'NONE',  ( -17.29158576265544056, 10.36474766602906783, -44.91724175520782580 ) ) ;
#229660 = VECTOR ( 'NONE', #142007, 1000.000000000000000 ) ;
#229661 = EDGE_LOOP ( 'NONE', ( #49589, #49542, #141977, #69542, #27295 ) ) ;
#229662 = DIRECTION ( 'NONE',  ( -0.7071067811865127117, -0.7071067811865821007, 0.000000000000000000 ) ) ;
#229663 = DIRECTION ( 'NONE',  ( -1.000000000000000000, 0.000000000000000000, 0.000000000000000000 ) ) ;
#229664 = ADVANCED_FACE ( 'NONE', ( #200943 ), #102955, .F. ) ;
#229665 = ORIENTED_EDGE ( 'NONE', *, *, #164491, .F. ) ;
#229666 = AXIS2_PLACEMENT_3D ( 'NONE', #102138, #222086, #8224 ) ;
#229667 = EDGE_CURVE ( 'NONE', #114049, #73021, #52126, .T. ) ;
#229669 = VERTEX_POINT ( 'NONE', #48289 ) ;
#229668 = CARTESIAN_POINT ( 'NONE',  ( -16.92563707711778065, 9.968990694407935393, -154.8807582995239898 ) ) ;
#229670 = DIRECTION ( 'NONE',  ( 0.2834754621636357830, -0.9414141221712113428, 0.1827049887871715350 ) ) ;
#229672 = ADVANCED_FACE ( 'NONE', ( #11759 ), #168288, .T. ) ;
#229671 = CIRCLE ( 'NONE', #79790, 0.1000000000000002554 ) ;
#229673 = ORIENTED_EDGE ( 'NONE', *, *, #50104, .F. ) ;
#229674 = DIRECTION ( 'NONE',  ( 0.7070776581709139474, -0.7071359030027652981, -2.453168425935592377E-14 ) ) ;
#229675 = VECTOR ( 'NONE', #89849, 1000.000000000000000 ) ;
#229676 = ORIENTED_EDGE ( 'NONE', *, *, #220773, .F. ) ;
#229677 = CARTESIAN_POINT ( 'NONE',  ( 18.59117750673696179, 65.66751761918668251, -97.42826094061121012 ) ) ;
#229678 = VERTEX_POINT ( 'NONE', #209951 ) ;
#229679 = DIRECTION ( 'NONE',  ( -0.000000000000000000, 1.000000000000000000, 0.000000000000000000 ) ) ;
#229680 = AXIS2_PLACEMENT_3D ( 'NONE', #210665, #89424, #32059 ) ;
#229681 = CARTESIAN_POINT ( 'NONE',  ( 20.94999999999999929, 64.36312671090729509, -76.34486669784918433 ) ) ;
#229682 = DIRECTION ( 'NONE',  ( 1.000000000000000000, 0.000000000000000000, 0.000000000000000000 ) ) ;
#229683 = EDGE_CURVE ( 'NONE', #6498, #78259, #146099, .T. ) ;
#229684 = TOROIDAL_SURFACE ( 'NONE', #13211, 12.97499999999999787, 0.1000000000000000056 ) ;
#229685 = CARTESIAN_POINT ( 'NONE',  ( 18.50000000000000000, 85.40000000001208491, -129.2258477248609267 ) ) ;
#229686 = ADVANCED_FACE ( 'NONE', ( #46983 ), #115429, .T. ) ;
#229687 = DIRECTION ( 'NONE',  ( -0.000000000000000000, 1.000000000000000000, -0.000000000000000000 ) ) ;
#229688 = DIRECTION ( 'NONE',  ( 0.000000000000000000, 0.000000000000000000, -1.000000000000000000 ) ) ;
#229689 = AXIS2_PLACEMENT_3D ( 'NONE', #24034, #103526, #243052 ) ;
#229690 = ORIENTED_EDGE ( 'NONE', *, *, #126595, .F. ) ;
#229691 = DIRECTION ( 'NONE',  ( 0.000000000000000000, 0.000000000000000000, -1.000000000000000000 ) ) ;
#229692 = CIRCLE ( 'NONE', #100656, 12.87500000000000000 ) ;
#229693 = ORIENTED_EDGE ( 'NONE', *, *, #157634, .F. ) ;
#229695 = CARTESIAN_POINT ( 'NONE',  ( 21.05000000000000071, 71.00000000001253397, -182.4283735034374843 ) ) ;
#229694 = LINE ( 'NONE', #49763, #223922 ) ;
#229696 = CIRCLE ( 'NONE', #67369, 3.999999999999996447 ) ;
#229697 = VERTEX_POINT ( 'NONE', #147392 ) ;
#229698 = CARTESIAN_POINT ( 'NONE',  ( -20.64999999999999858, 71.65000000001253966, -182.3731074845244109 ) ) ;
#229699 = TOROIDAL_SURFACE ( 'NONE', #9115, 0.2000000000000000111, 0.1000000000000000056 ) ;
#229700 = CARTESIAN_POINT ( 'NONE',  ( 18.39999999999999503, 43.51275691321468031, -233.9088826807484622 ) ) ;
#229701 = LINE ( 'NONE', #14527, #223495 ) ;
#229702 = DIRECTION ( 'NONE',  ( 0.000000000000000000, 1.387778780781406043E-13, 1.000000000000000000 ) ) ;
#229703 = ORIENTED_EDGE ( 'NONE', *, *, #46919, .T. ) ;
#229705 = VERTEX_POINT ( 'NONE', #189090 ) ;
#229704 = DIRECTION ( 'NONE',  ( 1.000000000000000000, 0.000000000000000000, 0.000000000000000000 ) ) ;
#229707 = LINE ( 'NONE', #51026, #155023 ) ;
#229706 = FACE_OUTER_BOUND ( 'NONE', #66740, .T. ) ;
#229709 = ORIENTED_EDGE ( 'NONE', *, *, #121254, .T. ) ;
#229708 = DIRECTION ( 'NONE',  ( -0.000000000000000000, 0.8660254037844411501, 0.4999999999999956146 ) ) ;
#229710 = ORIENTED_EDGE ( 'NONE', *, *, #6253, .T. ) ;
#229711 = AXIS2_PLACEMENT_3D ( 'NONE', #40658, #181428, #82269 ) ;
#229712 = CARTESIAN_POINT ( 'NONE',  ( 20.97224591636399538, 10.62515341617478271, -179.7499259046635416 ) ) ;
#229713 = CARTESIAN_POINT ( 'NONE',  ( 20.94999999999999929, 67.07338541492478612, -94.55142446530125255 ) ) ;
#229714 = ORIENTED_EDGE ( 'NONE', *, *, #222352, .T. ) ;
#229715 = CARTESIAN_POINT ( 'NONE',  ( 18.79999999999999716, -8.150000000000007461, 33.00000000000000000 ) ) ;
#229716 = ORIENTED_EDGE ( 'NONE', *, *, #57682, .F. ) ;
#229717 = DIRECTION ( 'NONE',  ( 1.000000000000000000, 0.000000000000000000, 0.000000000000000000 ) ) ;
#229718 = CARTESIAN_POINT ( 'NONE',  ( -18.39999999999999858, 85.50000000001233502, -162.9910380878246201 ) ) ;
#229719 = ORIENTED_EDGE ( 'NONE', *, *, #53034, .F. ) ;
#229720 = DIRECTION ( 'NONE',  ( -0.000000000000000000, 1.000000000000000000, 6.982962677686266711E-15 ) ) ;
#229721 = AXIS2_PLACEMENT_3D ( 'NONE', #147979, #149283, #112705 ) ;
#229722 = VERTEX_POINT ( 'NONE', #32622 ) ;
#229723 = CARTESIAN_POINT ( 'NONE',  ( -21.05000000000000071, 1.115600667400684642E-11, -189.2999999999999545 ) ) ;
#229725 = ORIENTED_EDGE ( 'NONE', *, *, #208667, .T. ) ;
#229724 = CIRCLE ( 'NONE', #217043, 0.1000000000000028644 ) ;
#229726 = VERTEX_POINT ( 'NONE', #148693 ) ;
#229727 = CARTESIAN_POINT ( 'NONE',  ( 18.46921299892753865, -9.509378177812608968, -107.4865787093704625 ) ) ;
#229728 = ORIENTED_EDGE ( 'NONE', *, *, #18121, .T. ) ;
#229729 = CARTESIAN_POINT ( 'NONE',  ( -23.25000000000000000, 1.115600667400684642E-11, -33.50000000000000000 ) ) ;
#229731 = EDGE_CURVE ( 'NONE', #144652, #167344, #191693, .T. ) ;
#229730 = ORIENTED_EDGE ( 'NONE', *, *, #92735, .T. ) ;
#229733 = ORIENTED_EDGE ( 'NONE', *, *, #13411, .T. ) ;
#229732 = DIRECTION ( 'NONE',  ( 0.000000000000000000, -0.4009882990724537022, 0.9160831752668424643 ) ) ;
#229734 = ORIENTED_EDGE ( 'NONE', *, *, #97199, .F. ) ;
#229735 = EDGE_CURVE ( 'NONE', #99142, #223586, #119561, .T. ) ;
#229736 = CARTESIAN_POINT ( 'NONE',  ( -20.94999999999999929, 67.23127455305835554, -235.8551265064784559 ) ) ;
#229737 = ADVANCED_FACE ( 'NONE', ( #206086 ), #27491, .F. ) ;
#229738 = ORIENTED_EDGE ( 'NONE', *, *, #1983, .F. ) ;
#229741 = ORIENTED_EDGE ( 'NONE', *, *, #248140, .F. ) ;
#229740 = ORIENTED_EDGE ( 'NONE', *, *, #227348, .F. ) ;
#229739 = DIRECTION ( 'NONE',  ( 0.000000000000000000, 0.000000000000000000, 1.000000000000000000 ) ) ;
#229742 = DIRECTION ( 'NONE',  ( -2.940209281316621509E-16, 1.000000000000000000, 0.000000000000000000 ) ) ;
#229743 = VECTOR ( 'NONE', #47047, 1000.000000000000114 ) ;
#229744 = ORIENTED_EDGE ( 'NONE', *, *, #16448, .F. ) ;
#229745 = AXIS2_PLACEMENT_3D ( 'NONE', #198079, #234644, #155146 ) ;
#229746 = AXIS2_PLACEMENT_3D ( 'NONE', #224156, #2537, #45532 ) ;
#229747 = ORIENTED_EDGE ( 'NONE', *, *, #51045, .T. ) ;
#229748 = EDGE_CURVE ( 'NONE', #179511, #150811, #166996, .T. ) ;
#229749 = CARTESIAN_POINT ( 'NONE',  ( -21.04999999999988347, 69.69982018209628905, -203.5745903664068521 ) ) ;
#229751 = ORIENTED_EDGE ( 'NONE', *, *, #131915, .F. ) ;
#229750 = DIRECTION ( 'NONE',  ( 0.000000000000000000, 0.000000000000000000, -1.000000000000000000 ) ) ;
#229752 = CARTESIAN_POINT ( 'NONE',  ( 21.05000000000000071, 41.42187432231295219, -260.1830396872097140 ) ) ;
#229753 = ORIENTED_EDGE ( 'NONE', *, *, #198005, .F. ) ;
#229754 = CARTESIAN_POINT ( 'NONE',  ( 22.88900146558018989, 61.25204754149966391, -224.6493555398289459 ) ) ;
#229755 = FACE_OUTER_BOUND ( 'NONE', #213392, .T. ) ;
#229756 = VERTEX_POINT ( 'NONE', #165698 ) ;
#229757 = CARTESIAN_POINT ( 'NONE',  ( -16.77683809663752257, 66.05416425680839154, -182.6870565036286393 ) ) ;
#229758 = CARTESIAN_POINT ( 'NONE',  ( 18.49999999999998934, 18.34743685832673421, -236.8753540304231251 ) ) ;
#229759 = CIRCLE ( 'NONE', #167255, 0.09999999999999938105 ) ;
#229760 = VERTEX_POINT ( 'NONE', #245220 ) ;
#229762 = ORIENTED_EDGE ( 'NONE', *, *, #168013, .F. ) ;
#229761 = CARTESIAN_POINT ( 'NONE',  ( -18.59999999999999787, -9.399999999988851940, -140.8820418481727188 ) ) ;
#229763 = DIRECTION ( 'NONE',  ( 0.000000000000000000, 0.6052030477779125617, 0.7960711469211315672 ) ) ;
#229765 = EDGE_LOOP ( 'NONE', ( #152558, #110120, #150000 ) ) ;
#229764 = ORIENTED_EDGE ( 'NONE', *, *, #234440, .F. ) ;
#229766 = VERTEX_POINT ( 'NONE', #10458 ) ;
#229767 = CARTESIAN_POINT ( 'NONE',  ( 21.05000000000000071, 6.650000000011155876, -144.0170271704400307 ) ) ;
#229769 = ORIENTED_EDGE ( 'NONE', *, *, #38779, .T. ) ;
#229768 = EDGE_CURVE ( 'NONE', #165955, #30570, #246487, .T. ) ;
#229770 = ORIENTED_EDGE ( 'NONE', *, *, #235169, .F. ) ;
#229771 = EDGE_CURVE ( 'NONE', #132227, #113334, #50831, .T. ) ;
#229772 = DIRECTION ( 'NONE',  ( -1.000000000000000000, -1.836970198721029934E-16, 0.000000000000000000 ) ) ;
#229773 = ORIENTED_EDGE ( 'NONE', *, *, #152515, .F. ) ;
#229774 = LINE ( 'NONE', #51106, #231417 ) ;
#229775 = DIRECTION ( 'NONE',  ( 0.000000000000000000, -1.000000000000000000, -0.000000000000000000 ) ) ;
#229776 = ORIENTED_EDGE ( 'NONE', *, *, #64589, .F. ) ;
#229777 = TOROIDAL_SURFACE ( 'NONE', #175629, 0.4000000000000003553, 0.1000000000000000056 ) ;
#229778 = VECTOR ( 'NONE', #86449, 1000.000000000000000 ) ;
#229780 = EDGE_CURVE ( 'NONE', #228701, #51021, #66581, .T. ) ;
#229779 = ORIENTED_EDGE ( 'NONE', *, *, #57861, .F. ) ;
#229781 = AXIS2_PLACEMENT_3D ( 'NONE', #239209, #224767, #200089 ) ;
#229782 = CARTESIAN_POINT ( 'NONE',  ( -20.64999999999999858, 76.00000000001126921, -203.5231074845248997 ) ) ;
#229783 = VERTEX_POINT ( 'NONE', #49577 ) ;
#229784 = CARTESIAN_POINT ( 'NONE',  ( -18.50000000000000000, 86.88220057837979482, -199.3100076076936205 ) ) ;
#229785 = EDGE_LOOP ( 'NONE', ( #117610, #254602, #90221, #204057 ) ) ;
#229786 = CARTESIAN_POINT ( 'NONE',  ( -20.94999999999999929, 77.73625713160970463, -158.4544551555068495 ) ) ;
#229788 = ORIENTED_EDGE ( 'NONE', *, *, #204805, .T. ) ;
#229787 = FACE_OUTER_BOUND ( 'NONE', #17881, .T. ) ;
#229789 = DIRECTION ( 'NONE',  ( -1.000000000000000000, -2.885090398161910739E-16, -6.283419270304611573E-17 ) ) ;
#229790 = CARTESIAN_POINT ( 'NONE',  ( -0.8999999999999437339, 66.35000000001119247, -7.423107484524793520 ) ) ;
#229791 = FACE_OUTER_BOUND ( 'NONE', #129139, .T. ) ;
#229792 = VECTOR ( 'NONE', #191146, 1000.000000000000227 ) ;
#229793 = DIRECTION ( 'NONE',  ( -1.073024830501118120E-15, 0.8814952561688430555, -0.4721928772777346239 ) ) ;
#229794 = CARTESIAN_POINT ( 'NONE',  ( -16.87331047859651179, 66.05000000001230376, -157.3731074845244393 ) ) ;
#229795 = FACE_OUTER_BOUND ( 'NONE', #249916, .T. ) ;
#229796 = CARTESIAN_POINT ( 'NONE',  ( 22.39999999999999503, 33.47376623175147614, -242.4412390690852988 ) ) ;
#229797 = CARTESIAN_POINT ( 'NONE',  ( -21.14999999999999858, 64.25000000001237765, -170.0231074845244166 ) ) ;
#229798 = DIRECTION ( 'NONE',  ( -0.7071067811865475727, -0.7071067811865475727, 0.000000000000000000 ) ) ;
#229799 = VERTEX_POINT ( 'NONE', #129117 ) ;
#229800 = EDGE_CURVE ( 'NONE', #86957, #112457, #252992, .T. ) ;
#229801 = ORIENTED_EDGE ( 'NONE', *, *, #118940, .T. ) ;
#229804 = ORIENTED_EDGE ( 'NONE', *, *, #36412, .T. ) ;
#229803 = EDGE_CURVE ( 'NONE', #170728, #1479, #236425, .T. ) ;
#229802 = CARTESIAN_POINT ( 'NONE',  ( -18.59999999999999787, 76.00000000001213607, -136.5231074845242745 ) ) ;
#229805 = ORIENTED_EDGE ( 'NONE', *, *, #39273, .F. ) ;
#229806 = LINE ( 'NONE', #26492, #24281 ) ;
#229807 = AXIS2_PLACEMENT_3D ( 'NONE', #138328, #114, #195791 ) ;
#229808 = DIRECTION ( 'NONE',  ( -1.000000000000000000, -7.125593699324843413E-30, 1.020425574104004196E-15 ) ) ;
#229809 = EDGE_CURVE ( 'NONE', #6683, #175441, #169571, .T. ) ;
#229810 = EDGE_CURVE ( 'NONE', #182212, #124526, #71724, .T. ) ;
#229812 = CYLINDRICAL_SURFACE ( 'NONE', #236179, 0.09999999999999939493 ) ;
#229811 = CARTESIAN_POINT ( 'NONE',  ( 23.14999999999999503, 11.65000000001116298, -54.85000000000000142 ) ) ;
#229813 = ORIENTED_EDGE ( 'NONE', *, *, #114556, .T. ) ;
#229814 = ORIENTED_EDGE ( 'NONE', *, *, #199964, .T. ) ;
#229815 = AXIS2_PLACEMENT_3D ( 'NONE', #83572, #1491, #99293 ) ;
#229816 = DIRECTION ( 'NONE',  ( -0.7071067811865456854, 0.7071067811865493491, 0.000000000000000000 ) ) ;
#229817 = AXIS2_PLACEMENT_3D ( 'NONE', #50925, #228318, #212608 ) ;
#229818 = FACE_OUTER_BOUND ( 'NONE', #165881, .T. ) ;
#229819 = ORIENTED_EDGE ( 'NONE', *, *, #51170, .F. ) ;
#229820 = ORIENTED_EDGE ( 'NONE', *, *, #203737, .T. ) ;
#229821 = EDGE_CURVE ( 'NONE', #67101, #187259, #90669, .T. ) ;
#229822 = DIRECTION ( 'NONE',  ( -1.000000000000000000, -0.000000000000000000, -0.000000000000000000 ) ) ;
#229825 = EDGE_CURVE ( 'NONE', #126637, #126709, #54707, .T. ) ;
#229824 = EDGE_CURVE ( 'NONE', #145089, #1286, #254177, .T. ) ;
#229823 = CIRCLE ( 'NONE', #221421, 0.09999999999999749367 ) ;
#229826 = DIRECTION ( 'NONE',  ( -1.000000000000000000, -0.000000000000000000, -0.000000000000000000 ) ) ;
#229827 = DIRECTION ( 'NONE',  ( 0.000000000000000000, 0.000000000000000000, 1.000000000000000000 ) ) ;
#229828 = CIRCLE ( 'NONE', #34061, 11.74999999999999645 ) ;
#229829 = CARTESIAN_POINT ( 'NONE',  ( 15.48841904831874849, 8.561580951692381092, -113.1500000000000341 ) ) ;
#229831 = EDGE_LOOP ( 'NONE', ( #177036, #41765, #25328, #50557 ) ) ;
#229830 = CARTESIAN_POINT ( 'NONE',  ( -23.15000000000000213, 15.90518444080776028, -219.2841490888777116 ) ) ;
#229832 = EDGE_CURVE ( 'NONE', #191992, #235775, #144836, .T. ) ;
#229833 = CARTESIAN_POINT ( 'NONE',  ( -20.64999999999999858, -9.399999999988846611, -157.6060308773475924 ) ) ;
#229834 = CARTESIAN_POINT ( 'NONE',  ( 22.59999999999999787, 64.35042919246716053, -103.1231074845243825 ) ) ;
#229835 = DIRECTION ( 'NONE',  ( -0.000000000000000000, 1.000000000000000000, -0.000000000000000000 ) ) ;
#229837 = CIRCLE ( 'NONE', #204876, 2.099999999999990763 ) ;
#229836 = DIRECTION ( 'NONE',  ( -0.000000000000000000, -0.8660254037844377084, -0.5000000000000016653 ) ) ;
#229838 = ORIENTED_EDGE ( 'NONE', *, *, #63809, .F. ) ;
#229839 = CARTESIAN_POINT ( 'NONE',  ( 13.54577453029515688, 66.54939790392327836, -84.57921152142770893 ) ) ;
#229840 = CARTESIAN_POINT ( 'NONE',  ( 18.69999999999999929, 0.000000000000000000, 0.000000000000000000 ) ) ;
#229841 = AXIS2_PLACEMENT_3D ( 'NONE', #162224, #98324, #256092 ) ;
#229842 = EDGE_CURVE ( 'NONE', #192936, #169719, #177259, .T. ) ;
#229843 = DIRECTION ( 'NONE',  ( 0.000000000000000000, -6.938893903907222067E-15, 1.000000000000000000 ) ) ;
#229844 = DIRECTION ( 'NONE',  ( -0.9880948137434723000, 0.07264505804272583522, 0.1356146547952018222 ) ) ;
#229845 = DIRECTION ( 'NONE',  ( -3.890533409366484652E-14, -0.1298341882520124002, -0.9915357197604841577 ) ) ;
#229847 = LINE ( 'NONE', #29127, #116532 ) ;
#229846 = CIRCLE ( 'NONE', #54857, 0.09999999999999939493 ) ;
#229848 = CYLINDRICAL_SURFACE ( 'NONE', #189421, 0.09999999999998898659 ) ;
#229849 = CARTESIAN_POINT ( 'NONE',  ( 18.59999999999999432, 1.637172712981537659, -145.5821533654720383 ) ) ;
#229850 = CARTESIAN_POINT ( 'NONE',  ( 20.12500000000000000, 9.750000000011153745, -155.2500000000000284 ) ) ;
#229851 = EDGE_CURVE ( 'NONE', #12214, #150828, #144655, .T. ) ;
#229853 = EDGE_CURVE ( 'NONE', #153129, #215339, #40663, .T. ) ;
#229852 = AXIS2_PLACEMENT_3D ( 'NONE', #218776, #160130, #196653 ) ;
#229854 = ORIENTED_EDGE ( 'NONE', *, *, #104104, .T. ) ;
#229855 = ORIENTED_EDGE ( 'NONE', *, *, #108829, .T. ) ;
#229856 = CIRCLE ( 'NONE', #250691, 12.97499999999998721 ) ;
#229857 = ORIENTED_EDGE ( 'NONE', *, *, #196561, .T. ) ;
#229858 = EDGE_CURVE ( 'NONE', #119088, #137736, #169839, .T. ) ;
#229859 = CARTESIAN_POINT ( 'NONE',  ( 20.53930447208010790, 67.02285131248687833, -94.58060034294609864 ) ) ;
#229860 = FACE_OUTER_BOUND ( 'NONE', #149375, .T. ) ;
#229861 = ORIENTED_EDGE ( 'NONE', *, *, #246088, .T. ) ;
#229862 = AXIS2_PLACEMENT_3D ( 'NONE', #58192, #217265, #115625 ) ;
#229863 = EDGE_CURVE ( 'NONE', #197589, #72909, #53068, .T. ) ;
#229864 = ORIENTED_EDGE ( 'NONE', *, *, #185888, .F. ) ;
#229865 =( NAMED_UNIT ( * ) PLANE_ANGLE_UNIT ( ) SI_UNIT ( $, .RADIAN. ) );
#229866 = ADVANCED_FACE ( 'NONE', ( #198065 ), #134231, .F. ) ;
#229868 = ORIENTED_EDGE ( 'NONE', *, *, #109231, .T. ) ;
#229867 = AXIS2_PLACEMENT_3D ( 'NONE', #65767, #227406, #10948 ) ;
#229869 = LINE ( 'NONE', #51192, #229476 ) ;
#229870 = AXIS2_PLACEMENT_3D ( 'NONE', #153645, #154901, #118322 ) ;
#229871 = ORIENTED_EDGE ( 'NONE', *, *, #79931, .T. ) ;
#229872 = CIRCLE ( 'NONE', #184079, 11.65000000000000036 ) ;
#229874 = CYLINDRICAL_SURFACE ( 'NONE', #80505, 0.1000000000000028644 ) ;
#229873 = CIRCLE ( 'NONE', #117458, 0.09999999999999939493 ) ;
#229875 = CARTESIAN_POINT ( 'NONE',  ( -19.89999999999999858, 5.488301202077012775, 16.50000000000000000 ) ) ;
#229876 = CARTESIAN_POINT ( 'NONE',  ( 21.14999999999999503, 76.00000000001267608, -203.5231074845243597 ) ) ;
#229877 = CARTESIAN_POINT ( 'NONE',  ( 23.14999999999999858, 11.60000000000000675, -26.57179676972450011 ) ) ;
#229878 = CARTESIAN_POINT ( 'NONE',  ( 23.14999999999998437, 1.115600667400684642E-11, -33.50000000000000000 ) ) ;
#229880 = ORIENTED_EDGE ( 'NONE', *, *, #146211, .T. ) ;
#229879 = CARTESIAN_POINT ( 'NONE',  ( -16.89155683852646561, 29.65330325090004138, -234.5108044860495511 ) ) ;
#229882 = CARTESIAN_POINT ( 'NONE',  ( 21.05000000000000071, 8.776282889879928106, -79.17621514106816960 ) ) ;
#229881 = CARTESIAN_POINT ( 'NONE',  ( 21.02374657821574644, 11.60000000082048643, -26.57179677019820829 ) ) ;
#229883 = EDGE_CURVE ( 'NONE', #237934, #26254, #232173, .T. ) ;
#229884 = CARTESIAN_POINT ( 'NONE',  ( -16.97092634996658944, 10.00088896634839664, -20.86985723370230872 ) ) ;
#229885 =( BOUNDED_SURFACE ( )  B_SPLINE_SURFACE ( 3, 2, ( 
 ( #244796, #123582, #225217 ),
 ( #57489, #203111, #103985 ),
 ( #255662, #183560, #46585 ),
 ( #4882, #126127, #28369 ),
 ( #88269, #49171, #11335 ),
 ( #107858, #187417, #90861 ),
 ( #209534, #8770, #132571 ),
 ( #71329, #149584, #210818 ),
 ( #89572, #150840, #206967 ),
 ( #68747, #249947, #208266 ) ),
 .UNSPECIFIED., .F., .F., .F. ) 
 B_SPLINE_SURFACE_WITH_KNOTS ( ( 4, 2, 2, 2, 4 ),
 ( 3, 3 ),
 ( 0.002161241639767788603, 0.002579950749617450703, 0.002789305304542281753, 0.002893982582004697712, 0.002998659859467113237 ),
 ( 0.000000000000000000, 1.000000000000000000 ),
 .UNSPECIFIED. ) 
 GEOMETRIC_REPRESENTATION_ITEM ( )  RATIONAL_B_SPLINE_SURFACE ( (
 ( 1.000000000000000000, 0.7071067811864479857, 1.000000000000000000),
 ( 1.000000000000000000, 0.7632447400663979753, 1.000000000000000000),
 ( 1.000000000000000000, 0.8158073005110251241, 1.000000000000000000),
 ( 1.000000000000000000, 0.8906973462395024743, 1.000000000000000000),
 ( 1.000000000000000000, 0.9149408947808339576, 1.000000000000000000),
 ( 1.000000000000000000, 0.9493368785271785182, 1.000000000000000000),
 ( 1.000000000000000000, 0.9605194247157303744, 1.000000000000000000),
 ( 1.000000000000000000, 0.9803630264780529568, 1.000000000000000000),
 ( 1.000000000000000000, 0.9900844824271433087, 1.000000000000000000),
 ( 1.000000000000000000, 0.9894588281429317345, 1.000000000000000000) ) ) 
 REPRESENTATION_ITEM ( '' )  SURFACE ( )  );
#229886 = ORIENTED_EDGE ( 'NONE', *, *, #127769, .F. ) ;
#229887 = CARTESIAN_POINT ( 'NONE',  ( 13.54556439290363556, 66.54940788787835970, -121.4669191657159786 ) ) ;
#229888 = CARTESIAN_POINT ( 'NONE',  ( -16.84419801905645997, 66.05000000001183480, -82.19259733074642327 ) ) ;
#229889 = CARTESIAN_POINT ( 'NONE',  ( -22.39999999999999858, 64.35000000001238618, -170.1231074845244393 ) ) ;
#229890 = ORIENTED_EDGE ( 'NONE', *, *, #48018, .F. ) ;
#229891 = CARTESIAN_POINT ( 'NONE',  ( -20.64999999999999858, 11.58468387039766512, -220.1227639117171861 ) ) ;
#229892 = FACE_OUTER_BOUND ( 'NONE', #193934, .T. ) ;
#229893 = ORIENTED_EDGE ( 'NONE', *, *, #113230, .F. ) ;
#229894 = CARTESIAN_POINT ( 'NONE',  ( 21.05000000000000071, -8.999999999988844479, -143.8939691226524644 ) ) ;
#229895 =( BOUNDED_SURFACE ( )  B_SPLINE_SURFACE ( 3, 2, ( 
 ( #222799, #125015, #241121 ),
 ( #44196, #144549, #123727 ),
 ( #224088, #141986, #23369 ),
 ( #139407, #182426, #41636 ),
 ( #140708, #242371, #220270 ),
 ( #221512, #199427, #178591 ) ),
 .UNSPECIFIED., .F., .F., .F. ) 
 B_SPLINE_SURFACE_WITH_KNOTS ( ( 4, 2, 4 ),
 ( 3, 3 ),
 ( 3.141592653589783346, 3.926990816987233845, 4.712388980384684345 ),
 ( 0.000000000000000000, 1.000000000000000000 ),
 .UNSPECIFIED. ) 
 GEOMETRIC_REPRESENTATION_ITEM ( )  RATIONAL_B_SPLINE_SURFACE ( (
 ( 1.000000000000000000, 0.9238795325112774126, 1.000000000000000000),
 ( 1.000000000000000000, 0.9240297172244186230, 1.000000000000000000),
 ( 1.000000000000000000, 0.9038128468038687524, 1.000000000000000000),
 ( 1.000000000000000000, 0.8282379607649484887, 1.000000000000000000),
 ( 1.000000000000000000, 0.7727932973490982960, 1.000000000000000000),
 ( 1.000000000000000000, 0.7071067811866457165, 1.000000000000000000) ) ) 
 REPRESENTATION_ITEM ( '' )  SURFACE ( )  );
#229896 = CARTESIAN_POINT ( 'NONE',  ( 20.73486653747088582, 7.250000000011182166, -42.75000000000000000 ) ) ;
#229897 = DIRECTION ( 'NONE',  ( 0.000000000000000000, -1.000000000000000000, 0.000000000000000000 ) ) ;
#229898 = VERTEX_POINT ( 'NONE', #14331 ) ;
#229899 = ORIENTED_EDGE ( 'NONE', *, *, #82380, .T. ) ;
#229900 = CARTESIAN_POINT ( 'NONE',  ( -20.85000000000000142, 77.36242903720516040, -95.13422623660308375 ) ) ;
#229901 = FACE_OUTER_BOUND ( 'NONE', #125051, .T. ) ;
#229902 = EDGE_CURVE ( 'NONE', #21979, #20437, #152563, .T. ) ;
#229903 = DIRECTION ( 'NONE',  ( 0.000000000000000000, 0.000000000000000000, 1.000000000000000000 ) ) ;
#229904 = DIRECTION ( 'NONE',  ( 0.000000000000000000, 0.000000000000000000, 1.000000000000000000 ) ) ;
#229905 = DIRECTION ( 'NONE',  ( 1.000000000000000000, -2.952720810173289112E-16, -2.061873921506763405E-30 ) ) ;
#229906 = DIRECTION ( 'NONE',  ( -1.000000000000000000, 2.952720810173289112E-16, 2.061873921506763405E-30 ) ) ;
#229907 = ADVANCED_FACE ( 'NONE', ( #256708 ), #15707, .T. ) ;
#229908 = DIRECTION ( 'NONE',  ( 0.000000000000000000, -0.4088369013363283844, 0.9126074666063769270 ) ) ;
#229909 = CARTESIAN_POINT ( 'NONE',  ( -21.52071067811865746, 29.53393254175612981, -236.9093933209877889 ) ) ;
#229910 = ORIENTED_EDGE ( 'NONE', *, *, #178427, .F. ) ;
#229912 =( BOUNDED_SURFACE ( )  B_SPLINE_SURFACE ( 3, 2, ( 
 ( #47753, #244676, #127312 ),
 ( #206850, #204264, #166471 ),
 ( #167750, #188565, #67336 ),
 ( #107743, #187302, #226385 ) ),
 .UNSPECIFIED., .F., .F., .F. ) 
 B_SPLINE_SURFACE_WITH_KNOTS ( ( 4, 4 ),
 ( 3, 3 ),
 ( 3.658908243880901523, 4.712388980384689674 ),
 ( 0.000000000000000000, 1.000000000000000000 ),
 .UNSPECIFIED. ) 
 GEOMETRIC_REPRESENTATION_ITEM ( )  RATIONAL_B_SPLINE_SURFACE ( (
 ( 1.000000000000000000, 0.8984936768950559927, 1.000000000000000000),
 ( 1.000000000000000000, 0.8646876308615171203, 1.000000000000000000),
 ( 1.000000000000000000, 0.7953136715913529109, 1.000000000000000000),
 ( 1.000000000000000000, 0.7071067811865475727, 1.000000000000000000) ) ) 
 REPRESENTATION_ITEM ( '' )  SURFACE ( )  );
#229911 = DIRECTION ( 'NONE',  ( 0.000000000000000000, 0.000000000000000000, -1.000000000000000000 ) ) ;
#229913 = AXIS2_PLACEMENT_3D ( 'NONE', #96469, #232172, #54786 ) ;
#229915 = ORIENTED_EDGE ( 'NONE', *, *, #92352, .T. ) ;
#229914 = CARTESIAN_POINT ( 'NONE',  ( 21.14999999999999858, 7.128833340093095217, -233.7327013124392749 ) ) ;
#229916 = CARTESIAN_POINT ( 'NONE',  ( 21.05000000000000071, 16.98881331171930498, -224.4946931418895417 ) ) ;
#229917 = DIRECTION ( 'NONE',  ( 0.000000000000000000, -0.8660254037844377084, -0.5000000000000016653 ) ) ;
#229918 = CARTESIAN_POINT ( 'NONE',  ( -20.64999999999999858, 21.35054858842500281, -233.1262234518673893 ) ) ;
#229919 = CARTESIAN_POINT ( 'NONE',  ( -23.25000000000000000, 67.23127455305835554, -235.8551265064784559 ) ) ;
#229920 = EDGE_CURVE ( 'NONE', #54771, #235005, #96383, .T. ) ;
#229921 = EDGE_CURVE ( 'NONE', #253988, #34850, #175969, .T. ) ;
#229922 = FACE_OUTER_BOUND ( 'NONE', #66777, .T. ) ;
#229924 = EDGE_LOOP ( 'NONE', ( #38150, #2972, #19113, #226563 ) ) ;
#229923 = LINE ( 'NONE', #154287, #61151 ) ;
#229925 = DIRECTION ( 'NONE',  ( -0.000000000000000000, -1.000000000000000000, -0.000000000000000000 ) ) ;
#229926 = CARTESIAN_POINT ( 'NONE',  ( -18.50000000000000711, 64.35000000001234355, -163.0083017138704236 ) ) ;
#229927 = CARTESIAN_POINT ( 'NONE',  ( 22.49533356619860669, 11.65000000631534149, -66.93487741967730642 ) ) ;
#229928 = DIRECTION ( 'NONE',  ( 0.000000000000000000, -0.000000000000000000, 1.000000000000000000 ) ) ;
#229929 = VERTEX_POINT ( 'NONE', #216344 ) ;
#229930 = CARTESIAN_POINT ( 'NONE',  ( 18.46947024752519795, -7.804717577830918351, -209.8502511493057909 ) ) ;
#229931 = ORIENTED_EDGE ( 'NONE', *, *, #93294, .T. ) ;
#229933 = AXIS2_PLACEMENT_3D ( 'NONE', #104153, #125031, #3790 ) ;
#229932 = FACE_OUTER_BOUND ( 'NONE', #161560, .T. ) ;
#229934 = ORIENTED_EDGE ( 'NONE', *, *, #60205, .F. ) ;
#229935 = LINE ( 'NONE', #192114, #55267 ) ;
#229936 = EDGE_LOOP ( 'NONE', ( #79378, #125902, #225320, #178499 ) ) ;
#229937 = CIRCLE ( 'NONE', #92367, 0.1000000000000023231 ) ;
#229938 = CARTESIAN_POINT ( 'NONE',  ( 23.15000000000000213, 62.33780030268294325, -247.9091949332902516 ) ) ;
#229939 = SPHERICAL_SURFACE ( 'NONE', #75093, 0.1000000000000000056 ) ;
#229940 = CYLINDRICAL_SURFACE ( 'NONE', #31049, 0.1000000000000021844 ) ;
#229941 = VERTEX_POINT ( 'NONE', #173431 ) ;
#229942 = CARTESIAN_POINT ( 'NONE',  ( -16.88783316861816530, 9.949999999999983302, -12.75226404197977104 ) ) ;
#229943 = CARTESIAN_POINT ( 'NONE',  ( -20.94999999999999929, 68.97833521811233481, -166.3895420826271163 ) ) ;
#229944 = CIRCLE ( 'NONE', #238304, 0.09999999999999939493 ) ;
#229945 = DIRECTION ( 'NONE',  ( 1.000000000000000000, -0.000000000000000000, -0.000000000000000000 ) ) ;
#229946 = CARTESIAN_POINT ( 'NONE',  ( -23.15000000000000213, 28.50120599808395028, -258.2149742250584268 ) ) ;
#229947 = DIRECTION ( 'NONE',  ( 0.000000000000000000, 0.000000000000000000, -1.000000000000000000 ) ) ;
#229949 = VERTEX_POINT ( 'NONE', #92539 ) ;
#229948 = ADVANCED_FACE ( 'NONE', ( #217607 ), #15619, .F. ) ;
#229950 = CARTESIAN_POINT ( 'NONE',  ( 23.14999999999999503, 69.55000000001203375, -114.7731074845243455 ) ) ;
#229951 = ORIENTED_EDGE ( 'NONE', *, *, #243088, .F. ) ;
#229953 = EDGE_LOOP ( 'NONE', ( #124056, #213730, #251699, #166777 ) ) ;
#229952 = DIRECTION ( 'NONE',  ( 1.000000000000000000, 1.836970198721029934E-16, 0.000000000000000000 ) ) ;
#229954 = ORIENTED_EDGE ( 'NONE', *, *, #224730, .T. ) ;
#229955 = DIRECTION ( 'NONE',  ( 0.000000000000000000, 0.000000000000000000, -1.000000000000000000 ) ) ;
#229956 = VERTEX_POINT ( 'NONE', #37742 ) ;
#229957 = DIRECTION ( 'NONE',  ( 1.000000000000000000, 3.190570557967288949E-16, 6.948722487160392945E-17 ) ) ;
#229958 = DIRECTION ( 'NONE',  ( 0.000000000000000000, 0.8814952561688428334, -0.4721928772777349570 ) ) ;
#229959 = FACE_OUTER_BOUND ( 'NONE', #238956, .T. ) ;
#229960 = ORIENTED_EDGE ( 'NONE', *, *, #111407, .T. ) ;
#229961 = DIRECTION ( 'NONE',  ( -1.000000000000000000, -0.000000000000000000, -0.000000000000000000 ) ) ;
#229962 = DIRECTION ( 'NONE',  ( 0.000000000000000000, -0.4721928772776973204, -0.8814952561688629284 ) ) ;
#229963 = DIRECTION ( 'NONE',  ( -1.000000000000000000, 0.000000000000000000, -0.000000000000000000 ) ) ;
#229964 = ADVANCED_FACE ( 'NONE', ( #117258 ), #157710, .F. ) ;
#229965 = VERTEX_POINT ( 'NONE', #161530 ) ;
#229967 = ORIENTED_EDGE ( 'NONE', *, *, #72597, .F. ) ;
#229966 = DIRECTION ( 'NONE',  ( 0.000000000000000000, 1.000000000000000000, 0.000000000000000000 ) ) ;
#229968 = AXIS2_PLACEMENT_3D ( 'NONE', #62594, #23497, #126404 ) ;
#229969 = CIRCLE ( 'NONE', #179912, 0.09999999999999939493 ) ;
#229971 = ADVANCED_FACE ( 'NONE', ( #220212 ), #140553, .T. ) ;
#229970 = DIRECTION ( 'NONE',  ( 1.000000000000000000, 0.000000000000000000, 0.000000000000000000 ) ) ;
#229972 = CYLINDRICAL_SURFACE ( 'NONE', #85704, 0.09999999999998898659 ) ;
#229973 = AXIS2_PLACEMENT_3D ( 'NONE', #195951, #254592, #197208 ) ;
#229974 = ORIENTED_EDGE ( 'NONE', *, *, #246258, .T. ) ;
#229975 = DIRECTION ( 'NONE',  ( 0.000000000000000000, -1.000000000000000000, 0.000000000000000000 ) ) ;
#229977 = EDGE_CURVE ( 'NONE', #244869, #37851, #161436, .T. ) ;
#229976 = DIRECTION ( 'NONE',  ( -1.000000000000000000, 0.000000000000000000, 0.000000000000000000 ) ) ;
#229978 = CARTESIAN_POINT ( 'NONE',  ( 22.39999999999999503, 76.00000000001203659, -114.6726782920691221 ) ) ;
#229979 = EDGE_LOOP ( 'NONE', ( #225065, #71760, #97670, #154761 ) ) ;
#229980 = LINE ( 'NONE', #31817, #209016 ) ;
#229981 = EDGE_CURVE ( 'NONE', #63849, #156342, #218901, .T. ) ;
#229982 = DIRECTION ( 'NONE',  ( 0.000000000000000000, 0.9908441862701791170, -0.1350103645450472789 ) ) ;
#229983 = EDGE_CURVE ( 'NONE', #216369, #182088, #143216, .T. ) ;
#229984 = CIRCLE ( 'NONE', #175837, 2.000000000000001776 ) ;
#229985 = DIRECTION ( 'NONE',  ( -2.915501640297152804E-16, -1.000000000000000000, -6.997203936713167125E-15 ) ) ;
#229986 = ADVANCED_FACE ( 'NONE', ( #148044 ), #62419, .F. ) ;
#229987 = CIRCLE ( 'NONE', #68060, 0.1000000000000028644 ) ;
#229988 = VERTEX_POINT ( 'NONE', #241065 ) ;
#229989 = FACE_OUTER_BOUND ( 'NONE', #108927, .T. ) ;
#229990 = VERTEX_POINT ( 'NONE', #181095 ) ;
#229991 = DIRECTION ( 'NONE',  ( 0.000000000000000000, -7.429790795770647916E-15, 1.000000000000000000 ) ) ;
#229993 = EDGE_CURVE ( 'NONE', #253445, #11088, #173942, .T. ) ;
#229992 = LINE ( 'NONE', #168792, #212299 ) ;
#229994 = AXIS2_PLACEMENT_3D ( 'NONE', #89922, #189041, #169519 ) ;
#229996 = VERTEX_POINT ( 'NONE', #239773 ) ;
#229995 = CARTESIAN_POINT ( 'NONE',  ( 14.87567385445977131, 25.00761986058639508, -232.6112779818446086 ) ) ;
#229997 = CARTESIAN_POINT ( 'NONE',  ( -20.94999999999999929, -11.75000000000000000, -30.39999999999999503 ) ) ;
#229998 = CARTESIAN_POINT ( 'NONE',  ( 0.9000000000000547562, 64.35000000001120668, -7.323107484524793875 ) ) ;
#229999 = CARTESIAN_POINT ( 'NONE',  ( -16.89060415895971090, 22.97504759209065028, -230.9320608734631719 ) ) ;
#230000 = CARTESIAN_POINT ( 'NONE',  ( 23.14999999999999503, 64.25000000001199396, -115.1731074845243796 ) ) ;
#230001 = VECTOR ( 'NONE', #177304, 1000.000000000000000 ) ;
#230002 = FACE_OUTER_BOUND ( 'NONE', #40516, .T. ) ;
#230003 = CARTESIAN_POINT ( 'NONE',  ( -20.54999999999999716, 11.41170713998153019, -246.6906184681487559 ) ) ;
#230005 = ORIENTED_EDGE ( 'NONE', *, *, #6477, .T. ) ;
#230004 = CARTESIAN_POINT ( 'NONE',  ( 18.59999999999999076, 69.35000000001151932, -48.37310748452436826 ) ) ;
#230006 = VECTOR ( 'NONE', #79592, 999.9999999999998863 ) ;
#230007 = VECTOR ( 'NONE', #112380, 1000.000000000000000 ) ;
#230008 = AXIS2_PLACEMENT_3D ( 'NONE', #65253, #82213, #101777 ) ;
#230009 = AXIS2_PLACEMENT_3D ( 'NONE', #55716, #92313, #131444 ) ;
#230010 = AXIS2_PLACEMENT_3D ( 'NONE', #48153, #88549, #85970 ) ;
#230011 = DIRECTION ( 'NONE',  ( -1.000000000000000000, -7.304098846218134667E-16, 0.000000000000000000 ) ) ;
#230012 = DIRECTION ( 'NONE',  ( 0.000000000000000000, 0.000000000000000000, -1.000000000000000000 ) ) ;
#230013 = CARTESIAN_POINT ( 'NONE',  ( 20.51284917709620359, 65.68911337716731680, -195.8506342989327038 ) ) ;
#230014 = DIRECTION ( 'NONE',  ( 2.952720810173289112E-16, 0.9651348961777159730, -0.2617529984165024026 ) ) ;
#230015 = AXIS2_PLACEMENT_3D ( 'NONE', #105043, #145492, #200346 ) ;
#230016 = ORIENTED_EDGE ( 'NONE', *, *, #62770, .F. ) ;
#230017 = VECTOR ( 'NONE', #24977, 1000.000000000000000 ) ;
#230018 = CARTESIAN_POINT ( 'NONE',  ( 13.99999999999999822, 66.15000000001185754, -86.27310748452437394 ) ) ;
#230019 = LINE ( 'NONE', #189623, #111693 ) ;
#230020 = AXIS2_PLACEMENT_3D ( 'NONE', #60646, #202743, #41131 ) ;
#230021 = CIRCLE ( 'NONE', #254907, 0.09999999999998898659 ) ;
#230022 = VERTEX_POINT ( 'NONE', #179810 ) ;
#230023 = CIRCLE ( 'NONE', #175885, 0.09999999999999939493 ) ;
#230025 = EDGE_CURVE ( 'NONE', #89611, #235390, #223935, .T. ) ;
#230024 = CYLINDRICAL_SURFACE ( 'NONE', #255977, 12.87499999999999467 ) ;
#230026 = TOROIDAL_SURFACE ( 'NONE', #72397, 0.2000000000000000111, 0.1000000000000000056 ) ;
#230027 = AXIS2_PLACEMENT_3D ( 'NONE', #54143, #227645, #29495 ) ;
#230028 = CARTESIAN_POINT ( 'NONE',  ( -16.93302609847409457, 9.996682520814371031, -79.58638849536259841 ) ) ;
#230029 = ORIENTED_EDGE ( 'NONE', *, *, #34551, .T. ) ;
#230030 = CARTESIAN_POINT ( 'NONE',  ( 20.94999999999999929, 1.360870587203197646, -75.07299792709100927 ) ) ;
#230031 = EDGE_LOOP ( 'NONE', ( #5437, #160371, #144325, #251935 ) ) ;
#230034 = EDGE_CURVE ( 'NONE', #166706, #240745, #228065, .T. ) ;
#230033 = AXIS2_PLACEMENT_3D ( 'NONE', #230125, #188426, #51460 ) ;
#230032 = DIRECTION ( 'NONE',  ( -1.020425574104004196E-15, 0.000000000000000000, 1.000000000000000000 ) ) ;
#230036 = ORIENTED_EDGE ( 'NONE', *, *, #221632, .F. ) ;
#230035 = DIRECTION ( 'NONE',  ( 0.000000000000000000, 0.000000000000000000, -1.000000000000000000 ) ) ;
#230037 = DIRECTION ( 'NONE',  ( 2.827886303505249259E-16, -0.8660254037844411501, -0.4999999999999956701 ) ) ;
#230038 = VERTEX_POINT ( 'NONE', #128476 ) ;
#230039 = ADVANCED_FACE ( 'NONE', ( #242324 ), #119739, .T. ) ;
#230040 = DIRECTION ( 'NONE',  ( 0.000000000000000000, -0.2617529984165152257, -0.9651348961777124202 ) ) ;
#230041 = EDGE_CURVE ( 'NONE', #48255, #54936, #84488, .T. ) ;
#230042 = EDGE_LOOP ( 'NONE', ( #228438, #141588, #50810, #46945 ) ) ;
#230044 = VERTEX_POINT ( 'NONE', #119843 ) ;
#230043 = ORIENTED_EDGE ( 'NONE', *, *, #210181, .T. ) ;
#230045 = FACE_OUTER_BOUND ( 'NONE', #19712, .T. ) ;
#230047 = VERTEX_POINT ( 'NONE', #222752 ) ;
#230046 = CARTESIAN_POINT ( 'NONE',  ( 23.14999999999999858, 76.52350599684427834, -201.5928376921694678 ) ) ;
#230048 = DIRECTION ( 'NONE',  ( -1.000000000000000000, -0.000000000000000000, -0.000000000000000000 ) ) ;
#230050 = ORIENTED_EDGE ( 'NONE', *, *, #155652, .T. ) ;
#230049 = AXIS2_PLACEMENT_3D ( 'NONE', #110291, #85554, #127296 ) ;
#230051 = CIRCLE ( 'NONE', #84244, 0.2000000000000005107 ) ;
#230052 = ORIENTED_EDGE ( 'NONE', *, *, #169629, .F. ) ;
#230053 = EDGE_CURVE ( 'NONE', #17741, #141916, #19442, .T. ) ;
#230054 = CARTESIAN_POINT ( 'NONE',  ( 20.04142135623730070, 31.44980407958351165, -233.5445995079518866 ) ) ;
#230055 = DIRECTION ( 'NONE',  ( 0.000000000000000000, 0.1350103645451876666, -0.9908441862701600211 ) ) ;
#230056 = CARTESIAN_POINT ( 'NONE',  ( -21.14999999999999858, 64.35000000001190301, -96.23924182154622997 ) ) ;
#230057 = ORIENTED_EDGE ( 'NONE', *, *, #254114, .T. ) ;
#230058 = EDGE_CURVE ( 'NONE', #64566, #4154, #141941, .T. ) ;
#230059 = DIRECTION ( 'NONE',  ( 0.000000000000000000, -6.454785026890489601E-15, 1.000000000000000000 ) ) ;
#230060 = CARTESIAN_POINT ( 'NONE',  ( 20.95512820512820440, 65.37615131629968346, -57.37310748452439668 ) ) ;
#230061 = CARTESIAN_POINT ( 'NONE',  ( 22.39999999999999503, 55.96127771274635876, -232.9022175645438892 ) ) ;
#230062 = ORIENTED_EDGE ( 'NONE', *, *, #73375, .T. ) ;
#230063 = DIRECTION ( 'NONE',  ( 0.000000000000000000, -0.2617529984165152257, -0.9651348961777124202 ) ) ;
#230064 = CYLINDRICAL_SURFACE ( 'NONE', #90512, 0.1000000000000028644 ) ;
#230065 = DIRECTION ( 'NONE',  ( 0.000000000000000000, -1.000000000000000000, -0.000000000000000000 ) ) ;
#230066 = ORIENTED_EDGE ( 'NONE', *, *, #237201, .T. ) ;
#230068 = DIRECTION ( 'NONE',  ( 0.000000000000000000, -0.4721928772777346239, -0.8814952561688430555 ) ) ;
#230067 = AXIS2_PLACEMENT_3D ( 'NONE', #36483, #73053, #95144 ) ;
#230069 = ORIENTED_EDGE ( 'NONE', *, *, #109882, .F. ) ;
#230070 = CARTESIAN_POINT ( 'NONE',  ( -18.50000000000000711, -7.664336336125146865, -210.0813447150619027 ) ) ;
#230071 = VERTEX_POINT ( 'NONE', #104077 ) ;
#230072 = B_SPLINE_CURVE_WITH_KNOTS ( 'NONE', 3,
 ( #42226, #241702, #20096, #181732, #237847, #99589, #57906, #239135, #158350, #159606 ),
 .UNSPECIFIED., .F., .F.,
 ( 4, 3, 3, 4 ),
 ( 1.883833020489685736E-15, 3.877043166999269576E-05, 7.336897548475664402E-05, 7.659383120240691504E-05 ),
 .UNSPECIFIED. ) ;
#230073 = CARTESIAN_POINT ( 'NONE',  ( -21.05000000000000071, 76.00000000001190870, -103.0231074845243029 ) ) ;
#230074 = FACE_OUTER_BOUND ( 'NONE', #5777, .T. ) ;
#230075 = EDGE_CURVE ( 'NONE', #188830, #151273, #148966, .T. ) ;
#230076 = VERTEX_POINT ( 'NONE', #183654 ) ;
#230077 = CIRCLE ( 'NONE', #238450, 0.09999999999999939493 ) ;
#230078 = EDGE_LOOP ( 'NONE', ( #255627, #67763, #198527, #236064 ) ) ;
#230079 = DIRECTION ( 'NONE',  ( -1.000000000000000000, 0.000000000000000000, 0.000000000000000000 ) ) ;
#230080 = EDGE_CURVE ( 'NONE', #231806, #161820, #34599, .T. ) ;
#230081 = DIRECTION ( 'NONE',  ( 1.000000000000000000, 0.000000000000000000, 0.000000000000000000 ) ) ;
#230082 = ORIENTED_EDGE ( 'NONE', *, *, #106340, .F. ) ;
#230083 = EDGE_CURVE ( 'NONE', #214790, #110751, #103138, .T. ) ;
#230084 = DIRECTION ( 'NONE',  ( 1.000000000000000000, 0.000000000000000000, 0.000000000000000000 ) ) ;
#230085 = CARTESIAN_POINT ( 'NONE',  ( -18.54148534481894117, 65.67467670974396299, -63.95317318268840978 ) ) ;
#230086 = ORIENTED_EDGE ( 'NONE', *, *, #176001, .F. ) ;
#230087 = ADVANCED_FACE ( 'NONE', ( #52769 ), #11100, .T. ) ;
#230088 = ORIENTED_EDGE ( 'NONE', *, *, #181829, .T. ) ;
#230089 = CIRCLE ( 'NONE', #13442, 0.09999999999999799327 ) ;
#230090 = CARTESIAN_POINT ( 'NONE',  ( 23.24999999999999289, 64.25000000001172396, -81.27310748452440237 ) ) ;
#230091 = FACE_OUTER_BOUND ( 'NONE', #212419, .T. ) ;
#230092 = DIRECTION ( 'NONE',  ( -1.000000000000000000, 0.000000000000000000, 0.000000000000000000 ) ) ;
#230094 = ORIENTED_EDGE ( 'NONE', *, *, #25365, .F. ) ;
#230093 = CARTESIAN_POINT ( 'NONE',  ( -23.15000000000000213, 87.65000000001165859, -69.52310748452424605 ) ) ;
#230095 = LINE ( 'NONE', #11051, #28646 ) ;
#230096 = CARTESIAN_POINT ( 'NONE',  ( 20.94999999999999929, 76.00000000001213607, -136.5231074845243313 ) ) ;
#230098 = EDGE_CURVE ( 'NONE', #177802, #121353, #57344, .T. ) ;
#230097 = CARTESIAN_POINT ( 'NONE',  ( 18.49999999999999289, 65.67426406872390032, -111.6731074845243796 ) ) ;
#230099 = FACE_OUTER_BOUND ( 'NONE', #33880, .T. ) ;
#230100 = DIRECTION ( 'NONE',  ( -1.000000000000000000, 7.304098846218134667E-16, 5.100424963727256530E-30 ) ) ;
#230101 = CARTESIAN_POINT ( 'NONE',  ( 21.05000000000000071, 76.00000000001215028, -138.5231074845243313 ) ) ;
#230102 = VECTOR ( 'NONE', #148128, 1000.000000000000114 ) ;
#230103 = LINE ( 'NONE', #95717, #218442 ) ;
#230104 = CARTESIAN_POINT ( 'NONE',  ( 18.59999999999999076, 77.83585931145570669, -124.9186683157258244 ) ) ;
#230105 = CIRCLE ( 'NONE', #13466, 0.2000000000000108080 ) ;
#230106 = ORIENTED_EDGE ( 'NONE', *, *, #210180, .T. ) ;
#230108 = VERTEX_POINT ( 'NONE', #69803 ) ;
#230107 = TOROIDAL_SURFACE ( 'NONE', #117691, 0.4000000000000012990, 0.1000000000000000056 ) ;
#230109 = EDGE_CURVE ( 'NONE', #149301, #171330, #192307, .T. ) ;
#230110 = EDGE_LOOP ( 'NONE', ( #15381, #14041, #131690, #47556 ) ) ;
#230111 = DIRECTION ( 'NONE',  ( -2.578261006436899437E-14, 0.3427706569149662208, -0.9394191166662952952 ) ) ;
#230112 = EDGE_CURVE ( 'NONE', #141594, #15975, #6903, .T. ) ;
#230113 = CARTESIAN_POINT ( 'NONE',  ( 18.59999999999999076, 11.75000000000000355, 11.75000000000000000 ) ) ;
#230114 = ORIENTED_EDGE ( 'NONE', *, *, #79147, .F. ) ;
#230115 = CIRCLE ( 'NONE', #76008, 0.1000000000000028644 ) ;
#230117 = CIRCLE ( 'NONE', #242584, 0.09999999999999939493 ) ;
#230116 =( LENGTH_UNIT ( ) NAMED_UNIT ( * ) SI_UNIT ( .MILLI., .METRE. ) );
#230118 = CARTESIAN_POINT ( 'NONE',  ( 20.95000000000005613, 67.65000000001118963, -3.023107484524792277 ) ) ;
#230119 = DIRECTION ( 'NONE',  ( 1.000000000000000000, 0.000000000000000000, 0.000000000000000000 ) ) ;
#230120 = SPHERICAL_SURFACE ( 'NONE', #232847, 0.1000000000000000056 ) ;
#230121 = ORIENTED_EDGE ( 'NONE', *, *, #145097, .F. ) ;
#230122 = ORIENTED_EDGE ( 'NONE', *, *, #141247, .T. ) ;
#230123 = EDGE_CURVE ( 'NONE', #117566, #9216, #253169, .T. ) ;
#230124 = DIRECTION ( 'NONE',  ( 1.000000000000000000, -1.617093283983707315E-14, 3.273910559064800547E-15 ) ) ;
#230125 = CARTESIAN_POINT ( 'NONE',  ( -18.79999999999999716, -11.65000000000000036, 32.89999999999999858 ) ) ;
#230127 = ADVANCED_FACE ( 'NONE', ( #14962 ), #54063, .T. ) ;
#230126 = ORIENTED_EDGE ( 'NONE', *, *, #16062, .F. ) ;
#230128 = AXIS2_PLACEMENT_3D ( 'NONE', #71596, #11617, #72891 ) ;
#230129 = FACE_OUTER_BOUND ( 'NONE', #56750, .T. ) ;
#230131 = ORIENTED_EDGE ( 'NONE', *, *, #252847, .F. ) ;
#230130 = CARTESIAN_POINT ( 'NONE',  ( 23.15000000000000213, -8.999999999988842703, -90.60603087734760663 ) ) ;
#230132 = DIRECTION ( 'NONE',  ( 1.000000000000000000, 0.000000000000000000, 0.000000000000000000 ) ) ;
#230134 = EDGE_LOOP ( 'NONE', ( #84080, #108664, #251891 ) ) ;
#230133 = CARTESIAN_POINT ( 'NONE',  ( -20.94999999999999929, -11.74999999998884448, -69.90000000000004832 ) ) ;
#230135 = CIRCLE ( 'NONE', #138540, 0.09999999999999939493 ) ;
#230136 = DIRECTION ( 'NONE',  ( -0.1538461538461510236, 0.9880948137434718559, 0.000000000000000000 ) ) ;
#230138 = CARTESIAN_POINT ( 'NONE',  ( 20.99780126800921209, 64.39461131213559497, -143.4357549128189646 ) ) ;
#230137 = VECTOR ( 'NONE', #8719, 1000.000000000000000 ) ;
#230139 = AXIS2_PLACEMENT_3D ( 'NONE', #189222, #229629, #210073 ) ;
#230140 = DIRECTION ( 'NONE',  ( 0.000000000000000000, -1.000000000000000000, 0.000000000000000000 ) ) ;
#230141 = CARTESIAN_POINT ( 'NONE',  ( -22.48660254037843487, 55.97436536266719997, -232.8539608197349651 ) ) ;
#230142 = VECTOR ( 'NONE', #21994, 1000.000000000000000 ) ;
#230143 = ADVANCED_FACE ( 'NONE', ( #174063 ), #112765, .T. ) ;
#230145 = CARTESIAN_POINT ( 'NONE',  ( 20.95512820512820440, 8.876151316299269567, -179.6499999999999773 ) ) ;
#230144 = CARTESIAN_POINT ( 'NONE',  ( 20.85000000000000142, 87.75000000001172396, -72.52310748452423184 ) ) ;
#230146 = DIRECTION ( 'NONE',  ( 1.000000000000000000, 0.000000000000000000, 0.000000000000000000 ) ) ;
#230147 = CARTESIAN_POINT ( 'NONE',  ( -21.05000000000000071, 1.115600667400684642E-11, -134.0000000000000284 ) ) ;
#230148 = CARTESIAN_POINT ( 'NONE',  ( 20.85000000000000142, -4.254329952141541860, -236.2118329068272260 ) ) ;
#230149 = DIRECTION ( 'NONE',  ( 0.000000000000000000, 0.000000000000000000, -1.000000000000000000 ) ) ;
#230150 = EDGE_CURVE ( 'NONE', #171424, #159934, #148575, .T. ) ;
#230151 = ORIENTED_EDGE ( 'NONE', *, *, #132721, .F. ) ;
#230152 = CARTESIAN_POINT ( 'NONE',  ( -17.73285935861319373, 10.85798180380184341, -77.24143819021939805 ) ) ;
#230153 = ORIENTED_EDGE ( 'NONE', *, *, #217176, .F. ) ;
#230154 = FACE_BOUND ( 'NONE', #71591, .T. ) ;
#230155 = ORIENTED_EDGE ( 'NONE', *, *, #204811, .T. ) ;
#230156 = EDGE_CURVE ( 'NONE', #67751, #215045, #107429, .T. ) ;
#230157 = CARTESIAN_POINT ( 'NONE',  ( 20.94999999999999929, 87.65000000001192859, -106.0231074845242176 ) ) ;
#230158 = FACE_OUTER_BOUND ( 'NONE', #80370, .T. ) ;
#230159 = EDGE_CURVE ( 'NONE', #200640, #2443, #252257, .T. ) ;
#230160 = ORIENTED_EDGE ( 'NONE', *, *, #176296, .F. ) ;
#230161 = FACE_OUTER_BOUND ( 'NONE', #75801, .T. ) ;
#230162 = EDGE_CURVE ( 'NONE', #83472, #229005, #209287, .T. ) ;
#230163 = CIRCLE ( 'NONE', #117740, 4.000000000000000000 ) ;
#230164 = VERTEX_POINT ( 'NONE', #189735 ) ;
#230165 = EDGE_LOOP ( 'NONE', ( #171370, #253438, #128710, #252549 ) ) ;
#230166 = FACE_OUTER_BOUND ( 'NONE', #102384, .T. ) ;
#230167 = CARTESIAN_POINT ( 'NONE',  ( 21.04999999999999361, 10.50253167713717595, -41.05882981707473078 ) ) ;
#230168 = DIRECTION ( 'NONE',  ( 1.000000000000000000, 0.000000000000000000, 0.000000000000000000 ) ) ;
#230169 = DIRECTION ( 'NONE',  ( 1.000000000000000000, 0.000000000000000000, 0.000000000000000000 ) ) ;
#230170 = DIRECTION ( 'NONE',  ( -0.000000000000000000, 1.000000000000000000, 1.734723475976807292E-15 ) ) ;
#230171 = AXIS2_PLACEMENT_3D ( 'NONE', #214382, #194848, #252211 ) ;
#230173 = CARTESIAN_POINT ( 'NONE',  ( 15.74999999999999645, 9.850000000011137402, -184.2499999999999716 ) ) ;
#230172 = CARTESIAN_POINT ( 'NONE',  ( -18.59999999999999787, 13.44116543737180081, -219.7184420207870801 ) ) ;
#230174 = CARTESIAN_POINT ( 'NONE',  ( 18.58143601961912950, 10.43572941510548624, -58.25000000000000000 ) ) ;
#230176 = ORIENTED_EDGE ( 'NONE', *, *, #96959, .T. ) ;
#230175 = DIRECTION ( 'NONE',  ( -1.000000000000000000, 0.000000000000000000, 0.000000000000000000 ) ) ;
#230178 = CARTESIAN_POINT ( 'NONE',  ( 18.49999999999999289, 10.20857864377385127, -91.65000000000004832 ) ) ;
#230177 = CARTESIAN_POINT ( 'NONE',  ( 20.86036036209908318, 10.62104277658211693, -74.66634841850502369 ) ) ;
#230179 = ADVANCED_FACE ( 'NONE', ( #111479 ), #53277, .T. ) ;
#230180 = CARTESIAN_POINT ( 'NONE',  ( -20.94999999999999929, 11.65000000001115232, -160.7161343370219129 ) ) ;
#230181 = EDGE_CURVE ( 'NONE', #62691, #11112, #233983, .T. ) ;
#230182 = VERTEX_POINT ( 'NONE', #55317 ) ;
#230183 = LINE ( 'NONE', #13700, #163130 ) ;
#230184 = DIRECTION ( 'NONE',  ( 1.000000000000000000, 4.758098676964952635E-14, 0.000000000000000000 ) ) ;
#230185 = DIRECTION ( 'NONE',  ( 1.000000000000000000, -2.952720810173289112E-16, -2.061873921506763405E-30 ) ) ;
#230186 = ORIENTED_EDGE ( 'NONE', *, *, #136692, .F. ) ;
#230188 = DIRECTION ( 'NONE',  ( -0.000000000000000000, 0.8660254037844502539, 0.4999999999999799605 ) ) ;
#230187 = CIRCLE ( 'NONE', #9421, 6.258578643762724880 ) ;
#230189 = CIRCLE ( 'NONE', #205039, 0.1000000000000002554 ) ;
#230190 = DIRECTION ( 'NONE',  ( 0.000000000000000000, 0.2617529984165031243, 0.9651348961777157509 ) ) ;
#230191 = CARTESIAN_POINT ( 'NONE',  ( 14.87567385445976598, 66.56923500458952958, -87.79257008977393184 ) ) ;
#230192 = AXIS2_PLACEMENT_3D ( 'NONE', #124728, #204246, #245962 ) ;
#230193 = ORIENTED_EDGE ( 'NONE', *, *, #46938, .F. ) ;
#230194 = ORIENTED_EDGE ( 'NONE', *, *, #86827, .F. ) ;
#230195 = AXIS2_PLACEMENT_3D ( 'NONE', #152427, #16752, #250215 ) ;
#230196 = LINE ( 'NONE', #148101, #15923 ) ;
#230197 = CARTESIAN_POINT ( 'NONE',  ( -18.34374000495060386, 11.47316190337362585, -176.7499999999999716 ) ) ;
#230198 = CARTESIAN_POINT ( 'NONE',  ( -21.05000000000000071, 70.88170441948386724, -234.2197789011331679 ) ) ;
#230199 = DIRECTION ( 'NONE',  ( -1.000000000000000000, 2.952720810173289112E-16, 2.061873921506763405E-30 ) ) ;
#230200 = ORIENTED_EDGE ( 'NONE', *, *, #50934, .T. ) ;
#230202 = CONICAL_SURFACE ( 'NONE', #59471, 4.000000000000000000, 0.7853981633974487231 ) ;
#230201 = CARTESIAN_POINT ( 'NONE',  ( 14.22821877134045998, 46.49228253827787682, -234.7843890162627360 ) ) ;
#230203 = CARTESIAN_POINT ( 'NONE',  ( 23.14999999999999503, 56.35580082907249277, -225.2769695492280277 ) ) ;
#230204 = CARTESIAN_POINT ( 'NONE',  ( -18.40000000000000213, 15.59003939055400956, -218.9434077809016514 ) ) ;
#230205 = AXIS2_PLACEMENT_3D ( 'NONE', #22902, #161115, #141529 ) ;
#230206 = DIRECTION ( 'NONE',  ( 1.000000000000000000, 0.000000000000000000, 0.000000000000000000 ) ) ;
#230207 = EDGE_CURVE ( 'NONE', #176194, #95630, #244786, .T. ) ;
#230208 = ORIENTED_EDGE ( 'NONE', *, *, #53240, .F. ) ;
#230209 = CARTESIAN_POINT ( 'NONE',  ( 20.94999999999999929, 10.29270135740183179, -38.95736188715193293 ) ) ;
#230210 = CIRCLE ( 'NONE', #72009, 0.1000000000000141609 ) ;
#230211 = AXIS2_PLACEMENT_3D ( 'NONE', #253328, #39464, #16041 ) ;
#230212 = AXIS2_PLACEMENT_3D ( 'NONE', #66779, #147596, #247970 ) ;
#230214 = ORIENTED_EDGE ( 'NONE', *, *, #63485, .T. ) ;
#230213 = CARTESIAN_POINT ( 'NONE',  ( -18.44085059012131822, 64.48598750652882927, -194.2634128036459913 ) ) ;
#230215 = VECTOR ( 'NONE', #83909, 1000.000000000000000 ) ;
#230216 = CARTESIAN_POINT ( 'NONE',  ( 5.899999999999997691, -11.34999999999999964, 13.90000000000000213 ) ) ;
#230217 = FACE_OUTER_BOUND ( 'NONE', #32783, .T. ) ;
#230218 = DIRECTION ( 'NONE',  ( 0.9880948137434723000, 0.1538461538461484146, -0.000000000000000000 ) ) ;
#230219 = DIRECTION ( 'NONE',  ( -1.000000000000000000, 0.000000000000000000, -0.000000000000000000 ) ) ;
#230220 = ORIENTED_EDGE ( 'NONE', *, *, #155311, .T. ) ;
#230221 = DIRECTION ( 'NONE',  ( -3.265361837132813093E-16, -0.4088369013363280513, 0.9126074666063769270 ) ) ;
#230222 = DIRECTION ( 'NONE',  ( -1.000000000000000000, -0.000000000000000000, 0.000000000000000000 ) ) ;
#230223 = DIRECTION ( 'NONE',  ( 0.000000000000000000, 0.000000000000000000, -1.000000000000000000 ) ) ;
#230224 = VERTEX_POINT ( 'NONE', #231443 ) ;
#230225 = CYLINDRICAL_SURFACE ( 'NONE', #213532, 0.09999999999999939493 ) ;
#230226 = FACE_OUTER_BOUND ( 'NONE', #86767, .T. ) ;
#230227 = LINE ( 'NONE', #133694, #21408 ) ;
#230228 = CARTESIAN_POINT ( 'NONE',  ( -16.87304349924914604, 51.64971365025504468, -231.9197784714389741 ) ) ;
#230229 = EDGE_CURVE ( 'NONE', #193487, #195790, #198443, .T. ) ;
#230230 = CYLINDRICAL_SURFACE ( 'NONE', #13501, 0.1000000000000028644 ) ;
#230231 = CIRCLE ( 'NONE', #113710, 0.1000000000000032391 ) ;
#230232 = CIRCLE ( 'NONE', #63633, 3.999999999999994671 ) ;
#230233 = CARTESIAN_POINT ( 'NONE',  ( 13.43663047529819821, 9.446645344706400493, -185.9108064561001754 ) ) ;
#230234 = TOROIDAL_SURFACE ( 'NONE', #51140, 2.100000000000002309, 0.1000000000000000056 ) ;
#230235 = ORIENTED_EDGE ( 'NONE', *, *, #98346, .F. ) ;
#230236 = ORIENTED_EDGE ( 'NONE', *, *, #156845, .T. ) ;
#230237 = DIRECTION ( 'NONE',  ( 1.000000000000000000, 0.000000000000000000, 0.000000000000000000 ) ) ;
#230238 = CARTESIAN_POINT ( 'NONE',  ( 18.59999999999998366, 76.00000000001126921, -203.5231074845248997 ) ) ;
#230239 = DIRECTION ( 'NONE',  ( 0.000000000000000000, 7.056502275159890832E-15, -1.000000000000000000 ) ) ;
#230240 = CARTESIAN_POINT ( 'NONE',  ( 18.44444291854882678, -0.7332650416222138423, -242.2292769306815501 ) ) ;
#230241 = CARTESIAN_POINT ( 'NONE',  ( -21.59780538579341425, 6.847090529954407145, -133.9010213304020454 ) ) ;
#230242 = CARTESIAN_POINT ( 'NONE',  ( -20.94999999999999929, -11.48912529306489994, -64.00000000000000000 ) ) ;
#230243 = CARTESIAN_POINT ( 'NONE',  ( -16.93262454970420094, 10.00202046794151300, -113.0729237737627244 ) ) ;
#230244 = AXIS2_PLACEMENT_3D ( 'NONE', #242662, #100556, #138405 ) ;
#230245 = DIRECTION ( 'NONE',  ( 0.000000000000000000, 0.000000000000000000, 1.000000000000000000 ) ) ;
#230246 = ORIENTED_EDGE ( 'NONE', *, *, #169312, .T. ) ;
#230247 = CARTESIAN_POINT ( 'NONE',  ( 20.95512820512820440, 67.12384868372411972, -148.7731074845244166 ) ) ;
#230248 = ORIENTED_EDGE ( 'NONE', *, *, #116767, .F. ) ;
#230249 = DIRECTION ( 'NONE',  ( 0.000000000000000000, 0.000000000000000000, -1.000000000000000000 ) ) ;
#230250 = DIRECTION ( 'NONE',  ( -1.000000000000000000, -0.000000000000000000, -0.000000000000000000 ) ) ;
#230251 = DIRECTION ( 'NONE',  ( -1.000000000000000000, -0.000000000000000000, -0.000000000000000000 ) ) ;
#230252 = DIRECTION ( 'NONE',  ( 0.000000000000000000, 1.000000000000000000, 0.000000000000000000 ) ) ;
#230253 = CARTESIAN_POINT ( 'NONE',  ( 18.59999996954842771, 85.52320413787062137, -62.64006577260797570 ) ) ;
#230254 = DIRECTION ( 'NONE',  ( 0.000000000000000000, 0.000000000000000000, 1.000000000000000000 ) ) ;
#230255 = ORIENTED_EDGE ( 'NONE', *, *, #77275, .F. ) ;
#230256 = LINE ( 'NONE', #35937, #191386 ) ;
#230257 = DIRECTION ( 'NONE',  ( -1.000000000000000000, -2.952720810173289112E-16, 0.000000000000000000 ) ) ;
#230259 = EDGE_CURVE ( 'NONE', #146449, #237933, #73578, .T. ) ;
#230258 = CARTESIAN_POINT ( 'NONE',  ( -16.94445028196808778, 66.00793639031384430, -56.91577730610593733 ) ) ;
#230260 = CARTESIAN_POINT ( 'NONE',  ( -20.85000000000000142, -1.835859311432479268, -112.0044391687985694 ) ) ;
#230261 = B_SPLINE_CURVE_WITH_KNOTS ( 'NONE', 3,
 ( #5631, #223407, #143874, #222110, #162192, #64359, #202579, #145152, #100857, #181736, #1789, #245567, #183030, #106017, #241705, #240422, #142582, #43512, #104720 ),
 .UNSPECIFIED., .F., .F.,
 ( 4, 3, 3, 3, 3, 3, 4 ),
 ( 0.000000000000000000, 2.646747978908405163E-05, 5.271166642128515082E-05, 9.008788829884125608E-05, 0.0001426648776560996530, 0.0001897378458659833658, 0.0001917382627806356570 ),
 .UNSPECIFIED. ) ;
#230262 = LINE ( 'NONE', #110320, #170607 ) ;
#230263 = CIRCLE ( 'NONE', #234363, 0.2000000000000057288 ) ;
#230264 = ORIENTED_EDGE ( 'NONE', *, *, #203463, .T. ) ;
#230265 = CARTESIAN_POINT ( 'NONE',  ( -21.05000000000000071, 1.851028230152016674, -78.65391326942254580 ) ) ;
#230267 = ADVANCED_FACE ( 'NONE', ( #131036 ), #119945, .F. ) ;
#230266 = CARTESIAN_POINT ( 'NONE',  ( -23.25000000000000000, -1.835859311432481045, -179.1044391687985353 ) ) ;
#230268 = ORIENTED_EDGE ( 'NONE', *, *, #30463, .T. ) ;
#230269 = VERTEX_POINT ( 'NONE', #17502 ) ;
#230271 = EDGE_CURVE ( 'NONE', #154908, #215461, #35815, .T. ) ;
#230270 = DIRECTION ( 'NONE',  ( 1.000000000000000000, 0.000000000000000000, 0.000000000000000000 ) ) ;
#230272 = DIRECTION ( 'NONE',  ( -1.000000000000000000, 0.000000000000000000, 0.000000000000000000 ) ) ;
#230273 = ORIENTED_EDGE ( 'NONE', *, *, #150074, .F. ) ;
#230274 = CARTESIAN_POINT ( 'NONE',  ( 20.94999999999999929, 69.08367151115869831, -247.5088222940653679 ) ) ;
#230275 = DIRECTION ( 'NONE',  ( 0.000000000000000000, 1.000000000000000000, 0.000000000000000000 ) ) ;
#230276 = B_SPLINE_CURVE_WITH_KNOTS ( 'NONE', 3,
 ( #214525, #134971, #114144, #35922, #210683, #32075, #129850, #193699, #111591, #213239, #171591, #71195, #230243, #115427, #75060, #194996, #132436, #249819, #34641 ),
 .UNSPECIFIED., .F., .F.,
 ( 4, 3, 3, 3, 3, 3, 4 ),
 ( 0.0001624081864585820618, 0.0001685232196531672496, 0.0001764526673566887201, 0.0001916878551483116016, 0.0002009890782182490127, 0.0002238845907555078393, 0.0002283406619926233426 ),
 .UNSPECIFIED. ) ;
#230277 = AXIS2_PLACEMENT_3D ( 'NONE', #180536, #61869, #239213 ) ;
#230278 = EDGE_CURVE ( 'NONE', #45686, #242585, #215691, .T. ) ;
#230279 = ORIENTED_EDGE ( 'NONE', *, *, #98480, .T. ) ;
#230280 = AXIS2_PLACEMENT_3D ( 'NONE', #248922, #9013, #231931 ) ;
#230281 = CARTESIAN_POINT ( 'NONE',  ( 18.43709777086140988, -9.682403433465239573, -174.1568433774128835 ) ) ;
#230282 = AXIS2_PLACEMENT_3D ( 'NONE', #52487, #206765, #152924 ) ;
#230283 = EDGE_LOOP ( 'NONE', ( #106427, #168425, #115792, #59403 ) ) ;
#230284 = DIRECTION ( 'NONE',  ( 1.000000000000000000, 0.000000000000000000, 0.000000000000000000 ) ) ;
#230286 = EDGE_CURVE ( 'NONE', #35759, #83651, #27791, .T. ) ;
#230285 = CARTESIAN_POINT ( 'NONE',  ( 11.60000000000000320, -8.350000000000004974, 19.04142135623731136 ) ) ;
#230288 = VERTEX_POINT ( 'NONE', #115320 ) ;
#230287 = DIRECTION ( 'NONE',  ( 1.000000000000000000, 0.000000000000000000, 0.000000000000000000 ) ) ;
#230289 = FACE_OUTER_BOUND ( 'NONE', #67553, .T. ) ;
#230291 = DIRECTION ( 'NONE',  ( 1.000000000000000000, 0.000000000000000000, 0.000000000000000000 ) ) ;
#230290 = UNCERTAINTY_MEASURE_WITH_UNIT (LENGTH_MEASURE( 1.000000000000000082E-05 ), #198401, 'distance_accuracy_value', 'NONE');
#230292 = CYLINDRICAL_SURFACE ( 'NONE', #43465, 0.09999999999999939493 ) ;
#230293 = CARTESIAN_POINT ( 'NONE',  ( -23.15000000000000213, 76.00000000001237765, -170.0231074845243597 ) ) ;
#230294 = VECTOR ( 'NONE', #28452, 1000.000000000000000 ) ;
#230295 = DIRECTION ( 'NONE',  ( 1.000000000000000000, 0.000000000000000000, 0.000000000000000000 ) ) ;
#230297 = CARTESIAN_POINT ( 'NONE',  ( 20.85000000000000142, -1.164121893230052995, -108.4148480855716485 ) ) ;
#230296 = VECTOR ( 'NONE', #98512, 1000.000000000000000 ) ;
#230299 = EDGE_LOOP ( 'NONE', ( #106993, #151416, #46411 ) ) ;
#230298 = DIRECTION ( 'NONE',  ( -1.000000000000000000, 0.000000000000000000, 0.000000000000000000 ) ) ;
#230300 = ORIENTED_EDGE ( 'NONE', *, *, #27769, .T. ) ;
#230303 = DIRECTION ( 'NONE',  ( 0.000000000000000000, -0.8700118002898356018, 0.4930308989875170078 ) ) ;
#230302 = DIRECTION ( 'NONE',  ( -1.000000000000000000, -0.000000000000000000, -0.000000000000000000 ) ) ;
#230301 = AXIS2_PLACEMENT_3D ( 'NONE', #129858, #12516, #251085 ) ;
#230305 = ORIENTED_EDGE ( 'NONE', *, *, #104008, .T. ) ;
#230304 = CARTESIAN_POINT ( 'NONE',  ( 20.94999999999999929, 8.926614585098253229, -75.47168301922316402 ) ) ;
#230306 = ORIENTED_EDGE ( 'NONE', *, *, #132534, .T. ) ;
#230307 = CARTESIAN_POINT ( 'NONE',  ( -22.00411653889204899, 0.7817229495032812503, -230.2203756341760368 ) ) ;
#230308 = FACE_OUTER_BOUND ( 'NONE', #142190, .T. ) ;
#230309 = DIRECTION ( 'NONE',  ( -0.000000000000000000, 6.982962677686266711E-15, -1.000000000000000000 ) ) ;
#230310 = CIRCLE ( 'NONE', #117876, 0.09999999999999939493 ) ;
#230311 = CYLINDRICAL_SURFACE ( 'NONE', #136064, 0.09999999999999939493 ) ;
#230312 = CARTESIAN_POINT ( 'NONE',  ( -18.59117750673697245, 67.49222854868494892, -195.4187676019683693 ) ) ;
#230313 = CARTESIAN_POINT ( 'NONE',  ( 18.59999999999999076, 11.65000000001115943, -58.35000000000000142 ) ) ;
#230314 = CIRCLE ( 'NONE', #188622, 0.1999999999999987899 ) ;
#230315 = TOROIDAL_SURFACE ( 'NONE', #180441, 11.90000000000000391, 0.1000000000000000056 ) ;
#230316 = CIRCLE ( 'NONE', #172114, 0.5999999999999894307 ) ;
#230318 = AXIS2_PLACEMENT_3D ( 'NONE', #166430, #50278, #187263 ) ;
#230317 = CARTESIAN_POINT ( 'NONE',  ( -18.59999999999999787, 1.115600667400684642E-11, -167.5000000000000284 ) ) ;
#230319 = ORIENTED_EDGE ( 'NONE', *, *, #91439, .F. ) ;
#230320 = ORIENTED_EDGE ( 'NONE', *, *, #116481, .F. ) ;
#230321 = FACE_OUTER_BOUND ( 'NONE', #32462, .T. ) ;
#230322 = ORIENTED_EDGE ( 'NONE', *, *, #71002, .F. ) ;
#230323 = DIRECTION ( 'NONE',  ( 0.000000000000000000, 0.000000000000000000, -1.000000000000000000 ) ) ;
#230324 = ORIENTED_EDGE ( 'NONE', *, *, #129975, .F. ) ;
#230325 = DIRECTION ( 'NONE',  ( 0.000000000000000000, -0.9856811345164803173, -0.1686199900910455851 ) ) ;
#230326 = ADVANCED_FACE ( 'NONE', ( #218256 ), #196147, .F. ) ;
#230327 = DIRECTION ( 'NONE',  ( 0.8049926720990051576, -0.5932847527679298016, -4.142885285818778274E-15 ) ) ;
#230328 = DIRECTION ( 'NONE',  ( 1.000000000000000000, 1.734723475976817507E-14, 0.000000000000000000 ) ) ;
#230329 = ORIENTED_EDGE ( 'NONE', *, *, #84884, .F. ) ;
#230331 = ADVANCED_FACE ( 'NONE', ( #496 ), #236547, .F. ) ;
#230330 = DIRECTION ( 'NONE',  ( 0.000000000000000000, 0.000000000000000000, -1.000000000000000000 ) ) ;
#230332 = ORIENTED_EDGE ( 'NONE', *, *, #142987, .T. ) ;
#230333 = FACE_OUTER_BOUND ( 'NONE', #169197, .T. ) ;
#230334 = CARTESIAN_POINT ( 'NONE',  ( 18.50000000000000000, 9.063861706928131312, -245.4572825683437998 ) ) ;
#230335 = AXIS2_PLACEMENT_3D ( 'NONE', #255871, #77270, #57706 ) ;
#230336 = EDGE_CURVE ( 'NONE', #210483, #87546, #100850, .T. ) ;
#230337 = ADVANCED_FACE ( 'NONE', ( #120496 ), #257342, .T. ) ;
#230338 = ORIENTED_EDGE ( 'NONE', *, *, #206818, .T. ) ;
#230339 = AXIS2_PLACEMENT_3D ( 'NONE', #115021, #251957, #194588 ) ;
#230340 = CARTESIAN_POINT ( 'NONE',  ( -18.40000000000000213, 15.91777359887373500, -218.8720307647289758 ) ) ;
#230341 = VERTEX_POINT ( 'NONE', #117886 ) ;
#230344 = ORIENTED_EDGE ( 'NONE', *, *, #149896, .T. ) ;
#230343 = DIRECTION ( 'NONE',  ( 1.000000000000000000, 0.000000000000000000, -0.000000000000000000 ) ) ;
#230342 = PLANE ( 'NONE',  #65903 ) ;
#230345 = B_SPLINE_CURVE_WITH_KNOTS ( 'NONE', 3,
 ( #70613, #210107, #227074, #228381 ),
 .UNSPECIFIED., .F., .F.,
 ( 4, 4 ),
 ( 0.000000000000000000, 7.713889350930799751E-05 ),
 .UNSPECIFIED. ) ;
#230346 = DIRECTION ( 'NONE',  ( 0.000000000000000000, 0.000000000000000000, -1.000000000000000000 ) ) ;
#230347 = ORIENTED_EDGE ( 'NONE', *, *, #66730, .F. ) ;
#230348 = ORIENTED_EDGE ( 'NONE', *, *, #151561, .F. ) ;
#230349 = CIRCLE ( 'NONE', #172149, 0.1000000000000028644 ) ;
#230350 = AXIS2_PLACEMENT_3D ( 'NONE', #108564, #203803, #186830 ) ;
#230352 = EDGE_CURVE ( 'NONE', #77584, #230995, #186561, .T. ) ;
#230351 = LINE ( 'NONE', #11316, #119726 ) ;
#230353 = ORIENTED_EDGE ( 'NONE', *, *, #182440, .T. ) ;
#230354 = EDGE_CURVE ( 'NONE', #151159, #231797, #99584, .T. ) ;
#230355 = CARTESIAN_POINT ( 'NONE',  ( -20.54999999999999716, 65.77012247227901298, -213.5448142138000378 ) ) ;
#230356 = DIRECTION ( 'NONE',  ( 0.000000000000000000, -6.982962677686266711E-15, 1.000000000000000000 ) ) ;
#230357 = CARTESIAN_POINT ( 'NONE',  ( 18.51697539158856642, 67.49317130920637453, -195.4795610751097286 ) ) ;
#230358 = VECTOR ( 'NONE', #121227, 999.9999999999998863 ) ;
#230359 = ADVANCED_FACE ( 'NONE', ( #240417 ), #197423, .F. ) ;
#230360 = CARTESIAN_POINT ( 'NONE',  ( -16.92973740335413169, 66.00749618554472420, -123.9291665197261381 ) ) ;
#230361 = CIRCLE ( 'NONE', #155395, 0.1000000000000021289 ) ;
#230362 = ORIENTED_EDGE ( 'NONE', *, *, #211593, .F. ) ;
#230363 = CIRCLE ( 'NONE', #55362, 0.1000000000000024342 ) ;
#230364 = AXIS2_PLACEMENT_3D ( 'NONE', #41560, #248723, #229164 ) ;
#230365 = CARTESIAN_POINT ( 'NONE',  ( 23.14999999999999858, 4.775700934590584090, -145.8487681040459734 ) ) ;
#230366 = CARTESIAN_POINT ( 'NONE',  ( 18.46905048506370051, 86.89090060965958173, -199.5596611130660847 ) ) ;
#230367 = DIRECTION ( 'NONE',  ( 1.000000000000000000, 0.000000000000000000, 0.000000000000000000 ) ) ;
#230368 = VERTEX_POINT ( 'NONE', #194886 ) ;
#230369 = DIRECTION ( 'NONE',  ( -0.7071067811865475727, 0.6824534298470373850, -0.1850873201762210096 ) ) ;
#230370 = ORIENTED_EDGE ( 'NONE', *, *, #74058, .T. ) ;
#230371 = CARTESIAN_POINT ( 'NONE',  ( -22.39999999999999858, 0.3085173699977072914, -229.9658011520297691 ) ) ;
#230373 = ORIENTED_EDGE ( 'NONE', *, *, #150055, .T. ) ;
#230372 = VECTOR ( 'NONE', #163954, 1000.000000000000000 ) ;
#230374 = EDGE_CURVE ( 'NONE', #93761, #82698, #98290, .T. ) ;
#230375 = DIRECTION ( 'NONE',  ( 0.000000000000000000, -0.4088369013363280513, 0.9126074666063769270 ) ) ;
#230376 = CARTESIAN_POINT ( 'NONE',  ( 20.94999999999999929, 1.115600667400684642E-11, -167.5000000000000284 ) ) ;
#230377 = EDGE_CURVE ( 'NONE', #238921, #170648, #211491, .T. ) ;
#230378 = ORIENTED_EDGE ( 'NONE', *, *, #62731, .T. ) ;
#230379 = ADVANCED_FACE ( 'NONE', ( #59163 ), #95742, .T. ) ;
#230380 = SPHERICAL_SURFACE ( 'NONE', #121424, 0.1000000000000000056 ) ;
#230381 = ORIENTED_EDGE ( 'NONE', *, *, #161425, .T. ) ;
#230383 = EDGE_CURVE ( 'NONE', #179995, #163256, #127732, .T. ) ;
#230382 = B_SPLINE_CURVE_WITH_KNOTS ( 'NONE', 3,
 ( #236267, #197130, #91624, #171210 ),
 .UNSPECIFIED., .F., .F.,
 ( 4, 4 ),
 ( 0.000000000000000000, 7.713889350930586977E-05 ),
 .UNSPECIFIED. ) ;
#230384 = AXIS2_PLACEMENT_3D ( 'NONE', #115059, #236282, #194626 ) ;
#230385 = FACE_OUTER_BOUND ( 'NONE', #199170, .T. ) ;
#230386 = VECTOR ( 'NONE', #135046, 1000.000000000000000 ) ;
#230387 = CARTESIAN_POINT ( 'NONE',  ( -16.97683810757273193, 9.950000000011137047, -113.7635767124605621 ) ) ;
#230388 = VERTEX_POINT ( 'NONE', #179185 ) ;
#230389 = DIRECTION ( 'NONE',  ( 0.000000000000000000, 0.000000000000000000, 1.000000000000000000 ) ) ;
#230390 = LINE ( 'NONE', #51721, #102420 ) ;
#230391 = ORIENTED_EDGE ( 'NONE', *, *, #46394, .F. ) ;
#230392 = LINE ( 'NONE', #72625, #232388 ) ;
#230393 = ORIENTED_EDGE ( 'NONE', *, *, #172243, .T. ) ;
#230394 = VECTOR ( 'NONE', #144923, 999.9999999999998863 ) ;
#230395 = AXIS2_PLACEMENT_3D ( 'NONE', #196347, #155972, #235466 ) ;
#230396 = CARTESIAN_POINT ( 'NONE',  ( 13.54577453029516043, 9.450602096099677496, -118.9438959630967076 ) ) ;
#230397 = AXIS2_PLACEMENT_3D ( 'NONE', #121529, #139754, #24990 ) ;
#230398 = CARTESIAN_POINT ( 'NONE',  ( -21.05000000000000071, 87.48912529308871910, -200.5231074845242745 ) ) ;
#230399 = EDGE_CURVE ( 'NONE', #253186, #230747, #155771, .T. ) ;
#230400 = EDGE_CURVE ( 'NONE', #242024, #231796, #27822, .T. ) ;
#230403 = ORIENTED_EDGE ( 'NONE', *, *, #52992, .F. ) ;
#230402 = VERTEX_POINT ( 'NONE', #223399 ) ;
#230401 = CARTESIAN_POINT ( 'NONE',  ( -23.25000000000000000, -8.999999999988846255, -110.3939691226524786 ) ) ;
#230404 = DIRECTION ( 'NONE',  ( 0.000000000000000000, 0.2128009952263403282, -0.9770955615653358350 ) ) ;
#230405 = DIRECTION ( 'NONE',  ( -7.304098846218134667E-16, 1.000000000000000000, 6.982962677686267499E-15 ) ) ;
#230407 = EDGE_CURVE ( 'NONE', #32954, #229007, #147590, .T. ) ;
#230406 = DIRECTION ( 'NONE',  ( -0.000000000000000000, -0.2617529984165031243, -0.9651348961777157509 ) ) ;
#230409 = CARTESIAN_POINT ( 'NONE',  ( -14.87770893841227249, 66.56936289831479314, -51.25484686646344556 ) ) ;
#230408 = DIRECTION ( 'NONE',  ( -1.000000000000000000, -0.000000000000000000, 0.000000000000000000 ) ) ;
#230410 = LINE ( 'NONE', #255035, #240372 ) ;
#230411 = FACE_OUTER_BOUND ( 'NONE', #33604, .T. ) ;
#230412 = AXIS2_PLACEMENT_3D ( 'NONE', #54595, #134120, #75480 ) ;
#230413 = DIRECTION ( 'NONE',  ( 0.000000000000000000, 0.000000000000000000, -1.000000000000000000 ) ) ;
#230414 = VECTOR ( 'NONE', #42378, 1000.000000000000000 ) ;
#230415 = DIRECTION ( 'NONE',  ( -0.000000000000000000, 1.000000000000000000, -0.000000000000000000 ) ) ;
#230416 = CIRCLE ( 'NONE', #197091, 0.1000000000000002554 ) ;
#230417 = VERTEX_POINT ( 'NONE', #8235 ) ;
#230418 = ORIENTED_EDGE ( 'NONE', *, *, #73020, .F. ) ;
#230419 = PLANE ( 'NONE',  #212452 ) ;
#230421 = ORIENTED_EDGE ( 'NONE', *, *, #39855, .F. ) ;
#230420 = CARTESIAN_POINT ( 'NONE',  ( 21.05000000000000071, 10.42338541492406279, -174.9920519238700649 ) ) ;
#230422 = ORIENTED_EDGE ( 'NONE', *, *, #97216, .F. ) ;
#230423 = DIRECTION ( 'NONE',  ( 0.000000000000000000, -0.4721928772777346239, -0.8814952561688430555 ) ) ;
#230424 = ORIENTED_EDGE ( 'NONE', *, *, #73226, .F. ) ;
#230425 = DIRECTION ( 'NONE',  ( 1.000000000000000000, 0.000000000000000000, 0.000000000000000000 ) ) ;
#230426 = ADVANCED_FACE ( 'NONE', ( #104712 ), #152694, .T. ) ;
#230427 = VERTEX_POINT ( 'NONE', #44784 ) ;
#230428 = LINE ( 'NONE', #71378, #135333 ) ;
#230430 = EDGE_CURVE ( 'NONE', #179524, #150828, #124325, .T. ) ;
#230429 = CARTESIAN_POINT ( 'NONE',  ( -21.05000000000000071, 76.00000000001213607, -136.5231074845243313 ) ) ;
#230432 = ORIENTED_EDGE ( 'NONE', *, *, #6625, .F. ) ;
#230431 = EDGE_LOOP ( 'NONE', ( #233, #255546, #191802, #94399, #8132, #93479 ) ) ;
#230433 = ORIENTED_EDGE ( 'NONE', *, *, #255406, .T. ) ;
#230434 = ORIENTED_EDGE ( 'NONE', *, *, #20863, .F. ) ;
#230435 = ORIENTED_EDGE ( 'NONE', *, *, #144131, .T. ) ;
#230436 = EDGE_CURVE ( 'NONE', #47223, #90118, #118455, .T. ) ;
#230437 = DIRECTION ( 'NONE',  ( 0.000000000000000000, -0.2617529984165152257, -0.9651348961777124202 ) ) ;
#230438 = CARTESIAN_POINT ( 'NONE',  ( 21.14999999999999858, 7.081614052365321932, -233.8208508380561454 ) ) ;
#230439 = CIRCLE ( 'NONE', #238823, 0.09999999999999854838 ) ;
#230440 = CARTESIAN_POINT ( 'NONE',  ( -15.73854595235692599, 9.351413679112548394, -184.4803435675489709 ) ) ;
#230443 = EDGE_CURVE ( 'NONE', #148174, #198296, #185977, .T. ) ;
#230442 = ORIENTED_EDGE ( 'NONE', *, *, #125512, .F. ) ;
#230441 = CYLINDRICAL_SURFACE ( 'NONE', #79166, 0.09999999999999939493 ) ;
#230444 = FACE_OUTER_BOUND ( 'NONE', #238002, .T. ) ;
#230445 = CARTESIAN_POINT ( 'NONE',  ( -23.15000000000000213, 7.128833340093095217, -233.7327013124392749 ) ) ;
#230447 = ORIENTED_EDGE ( 'NONE', *, *, #187811, .F. ) ;
#230446 = DIRECTION ( 'NONE',  ( -0.000000000000000000, -0.1350103645451835865, -0.9908441862701606873 ) ) ;
#230448 = DIRECTION ( 'NONE',  ( 1.000000000000000000, 0.000000000000000000, 0.000000000000000000 ) ) ;
#230449 = ORIENTED_EDGE ( 'NONE', *, *, #68496, .F. ) ;
#230450 = EDGE_CURVE ( 'NONE', #74222, #97650, #220838, .T. ) ;
#230451 = PLANE ( 'NONE',  #103438 ) ;
#230452 = ORIENTED_EDGE ( 'NONE', *, *, #204028, .T. ) ;
#230453 = DIRECTION ( 'NONE',  ( 1.000000000000000000, 0.000000000000000000, 0.000000000000000000 ) ) ;
#230454 = CARTESIAN_POINT ( 'NONE',  ( 23.14999999999999147, 36.65892442174472876, -249.5511627012454596 ) ) ;
#230455 = EDGE_LOOP ( 'NONE', ( #236410, #127379, #124468, #69309 ) ) ;
#230457 = CARTESIAN_POINT ( 'NONE',  ( -23.25000000000000000, 67.23127455305835554, -235.8551265064784559 ) ) ;
#230456 = CARTESIAN_POINT ( 'NONE',  ( 21.05000000000000071, 1.115600667400684642E-11, -171.5000000000000284 ) ) ;
#230458 = VECTOR ( 'NONE', #240298, 1000.000000000000114 ) ;
#230459 = DIRECTION ( 'NONE',  ( -2.827886303505248273E-16, -0.9667078373770112698, -0.2558827019434133376 ) ) ;
#230460 = EDGE_CURVE ( 'NONE', #14463, #177157, #140156, .T. ) ;
#230461 = AXIS2_PLACEMENT_3D ( 'NONE', #71856, #211354, #27612 ) ;
#230462 = CARTESIAN_POINT ( 'NONE',  ( 20.73486653747088937, 10.26442319175629692, -211.7110511407986735 ) ) ;
#230463 = CARTESIAN_POINT ( 'NONE',  ( -23.25000000000000355, 17.95055421627409231, -233.1200372299043693 ) ) ;
#230464 = EDGE_CURVE ( 'NONE', #167773, #183080, #206825, .T. ) ;
#230465 = ORIENTED_EDGE ( 'NONE', *, *, #119522, .T. ) ;
#230467 = ORIENTED_EDGE ( 'NONE', *, *, #130993, .T. ) ;
#230466 = VECTOR ( 'NONE', #20404, 1000.000000000000000 ) ;
#230468 = CARTESIAN_POINT ( 'NONE',  ( -18.50000000000000000, 11.65000000001115232, -121.8500000000000369 ) ) ;
#230469 = CARTESIAN_POINT ( 'NONE',  ( -18.36973785203556275, 62.50337617467221918, -209.4468579031038473 ) ) ;
#230470 = ORIENTED_EDGE ( 'NONE', *, *, #245411, .T. ) ;
#230471 = DIRECTION ( 'NONE',  ( 0.000000000000000000, -0.9856811345164832039, -0.1686199900910280158 ) ) ;
#230472 = EDGE_LOOP ( 'NONE', ( #36740, #194716, #192135, #146930 ) ) ;
#230473 = EDGE_CURVE ( 'NONE', #18469, #130606, #23956, .T. ) ;
#230474 = LINE ( 'NONE', #169253, #77522 ) ;
#230475 = CARTESIAN_POINT ( 'NONE',  ( -21.14999999999994174, 74.14873292176677921, -47.62635315998165453 ) ) ;
#230476 = DIRECTION ( 'NONE',  ( 0.000000000000000000, -0.4999999999999929501, 0.8660254037844427044 ) ) ;
#230477 = VERTEX_POINT ( 'NONE', #126891 ) ;
#230478 = AXIS2_PLACEMENT_3D ( 'NONE', #133404, #115118, #13458 ) ;
#230479 = CARTESIAN_POINT ( 'NONE',  ( -16.85939591225058720, 66.09477352162475938, -190.5630392380553815 ) ) ;
#230480 =( NAMED_UNIT ( * ) SI_UNIT ( $, .STERADIAN. ) SOLID_ANGLE_UNIT ( ) );
#230481 = ADVANCED_FACE ( 'NONE', ( #26519 ), #6933, .T. ) ;
#230482 = VECTOR ( 'NONE', #81474, 1000.000000000000000 ) ;
#230483 = EDGE_LOOP ( 'NONE', ( #9838, #154867, #118458 ) ) ;
#230484 = ORIENTED_EDGE ( 'NONE', *, *, #142962, .F. ) ;
#230485 = CIRCLE ( 'NONE', #213911, 0.2000000000000111688 ) ;
#230486 = ORIENTED_EDGE ( 'NONE', *, *, #61756, .T. ) ;
#230487 = VECTOR ( 'NONE', #61499, 1000.000000000000114 ) ;
#230488 = EDGE_CURVE ( 'NONE', #183114, #50587, #69471, .T. ) ;
#230489 = CARTESIAN_POINT ( 'NONE',  ( -23.49999999999994316, 87.50449464844290048, -34.18759587077607165 ) ) ;
#230490 = DIRECTION ( 'NONE',  ( 0.000000000000000000, 0.9126074666063545004, 0.4088369013363783999 ) ) ;
#230491 = CARTESIAN_POINT ( 'NONE',  ( -21.11101077989000174, 0.01528526892543027871, -127.5763152652739052 ) ) ;
#230492 = CARTESIAN_POINT ( 'NONE',  ( -23.15000000000000213, 1.115648428625851357E-11, -130.1000000000000512 ) ) ;
#230493 = CARTESIAN_POINT ( 'NONE',  ( 18.59999999999999076, 1.115600667400684642E-11, -134.0000000000000284 ) ) ;
#230495 = PLANE ( 'NONE',  #90785 ) ;
#230494 = CARTESIAN_POINT ( 'NONE',  ( 22.46250603428203618, -3.130481585860003690, -228.2130804456526221 ) ) ;
#230496 = EDGE_CURVE ( 'NONE', #216777, #26102, #87489, .T. ) ;
#230498 = ORIENTED_EDGE ( 'NONE', *, *, #1477, .F. ) ;
#230497 = DIRECTION ( 'NONE',  ( 0.000000000000000000, 0.000000000000000000, -1.000000000000000000 ) ) ;
#230499 = LINE ( 'NONE', #90975, #145642 ) ;
#230500 = ORIENTED_EDGE ( 'NONE', *, *, #152117, .T. ) ;
#230501 = CARTESIAN_POINT ( 'NONE',  ( -13.22483237240079568, 9.436674251854009654, -149.1768619309992232 ) ) ;
#230502 = EDGE_CURVE ( 'NONE', #35302, #29489, #108604, .T. ) ;
#230503 = ORIENTED_EDGE ( 'NONE', *, *, #215719, .T. ) ;
#230504 = VERTEX_POINT ( 'NONE', #150317 ) ;
#230505 = CARTESIAN_POINT ( 'NONE',  ( 20.94999999999999929, 6.550000000011156231, -179.6499999999999773 ) ) ;
#230507 = AXIS2_PLACEMENT_3D ( 'NONE', #238147, #222411, #141621 ) ;
#230506 = DIRECTION ( 'NONE',  ( -1.000000000000000000, 0.000000000000000000, -0.000000000000000000 ) ) ;
#230508 = CARTESIAN_POINT ( 'NONE',  ( -16.93301857435210067, 66.02369064527604792, -48.63733191336294226 ) ) ;
#230509 = VECTOR ( 'NONE', #214359, 1000.000000000000000 ) ;
#230510 = DIRECTION ( 'NONE',  ( 1.000000000000000000, 0.000000000000000000, 0.000000000000000000 ) ) ;
#230511 = CIRCLE ( 'NONE', #138870, 0.09999999999999939493 ) ;
#230512 = CARTESIAN_POINT ( 'NONE',  ( 20.94999999999999929, 18.34711819382569686, -236.8747682978092541 ) ) ;
#230513 = VERTEX_POINT ( 'NONE', #211569 ) ;
#230514 = VERTEX_POINT ( 'NONE', #94167 ) ;
#230515 = VECTOR ( 'NONE', #131050, 999.9999999999998863 ) ;
#230516 = DIRECTION ( 'NONE',  ( 0.000000000000000000, -6.982962677686266711E-15, 1.000000000000000000 ) ) ;
#230518 = EDGE_CURVE ( 'NONE', #167911, #185216, #53333, .T. ) ;
#230517 = ORIENTED_EDGE ( 'NONE', *, *, #233925, .T. ) ;
#230519 = CARTESIAN_POINT ( 'NONE',  ( 23.14999999999999858, 4.775700934579435675, -21.65123189595403375 ) ) ;
#230520 = CARTESIAN_POINT ( 'NONE',  ( 20.85000000000000142, 86.48473784507378070, -209.3714211149925575 ) ) ;
#230521 = ORIENTED_EDGE ( 'NONE', *, *, #135250, .T. ) ;
#230522 = DIRECTION ( 'NONE',  ( 0.000000000000000000, -1.000000000000000000, 0.000000000000000000 ) ) ;
#230523 = CARTESIAN_POINT ( 'NONE',  ( -21.05000000000000071, 11.75000000001115552, -60.15839931010295771 ) ) ;
#230524 = LINE ( 'NONE', #74044, #207026 ) ;
#230525 = CARTESIAN_POINT ( 'NONE',  ( 21.14999999999999858, 65.28660755661240955, -157.7731074845244166 ) ) ;
#230526 = VERTEX_POINT ( 'NONE', #207727 ) ;
#230527 = DIRECTION ( 'NONE',  ( 0.000000000000000000, 0.9126074666064005747, 0.4088369013362753712 ) ) ;
#230529 = DIRECTION ( 'NONE',  ( -1.073024830501117725E-15, -0.000000000000000000, -1.000000000000000000 ) ) ;
#230528 = AXIS2_PLACEMENT_3D ( 'NONE', #10669, #11971, #90175 ) ;
#230531 = DIRECTION ( 'NONE',  ( 1.000000000000000000, 0.000000000000000000, 0.000000000000000000 ) ) ;
#230530 = AXIS2_PLACEMENT_3D ( 'NONE', #246003, #105149, #208171 ) ;
#230532 = AXIS2_PLACEMENT_3D ( 'NONE', #99038, #39119, #238574 ) ;
#230533 = DIRECTION ( 'NONE',  ( -1.155739209832885601E-15, -0.9910827722268042983, 0.1332476588733650935 ) ) ;
#230534 = FACE_OUTER_BOUND ( 'NONE', #159932, .T. ) ;
#230535 = DIRECTION ( 'NONE',  ( 0.000000000000000000, 7.026728003956695223E-15, -1.000000000000000000 ) ) ;
#230536 = ORIENTED_EDGE ( 'NONE', *, *, #102886, .T. ) ;
#230538 = ADVANCED_FACE ( 'NONE', ( #151618 ), #188150, .F. ) ;
#230537 = CARTESIAN_POINT ( 'NONE',  ( -23.15000000000000213, 71.65000000001222702, -148.6731074845243938 ) ) ;
#230539 = ORIENTED_EDGE ( 'NONE', *, *, #498, .F. ) ;
#230540 = DIRECTION ( 'NONE',  ( 0.000000000000000000, -0.9126074666063545004, -0.4088369013363783999 ) ) ;
#230541 = FACE_OUTER_BOUND ( 'NONE', #128444, .T. ) ;
#230542 = CARTESIAN_POINT ( 'NONE',  ( 20.94999999999999574, -1.360870587180885716, -75.07299792709100927 ) ) ;
#230543 = DIRECTION ( 'NONE',  ( -1.000000000000000000, -0.000000000000000000, -0.000000000000000000 ) ) ;
#230544 = CARTESIAN_POINT ( 'NONE',  ( -21.05000000000000071, 74.16465844978715438, -57.96795619196135618 ) ) ;
#230545 = LINE ( 'NONE', #233132, #82034 ) ;
#230546 = VERTEX_POINT ( 'NONE', #29118 ) ;
#230547 = CYLINDRICAL_SURFACE ( 'NONE', #38569, 0.1000000000000028644 ) ;
#230548 = CIRCLE ( 'NONE', #134822, 4.149999999999999467 ) ;
#230549 = CARTESIAN_POINT ( 'NONE',  ( -23.25000000000000355, 11.75000000001113953, -42.75000000000000000 ) ) ;
#230550 = LINE ( 'NONE', #231845, #35204 ) ;
#230552 = AXIS2_PLACEMENT_3D ( 'NONE', #52157, #169604, #75614 ) ;
#230551 = CARTESIAN_POINT ( 'NONE',  ( -23.15000000000000213, 24.17260720300848931, -252.6908294531417027 ) ) ;
#230553 = EDGE_CURVE ( 'NONE', #194433, #207476, #48779, .T. ) ;
#230554 = AXIS2_PLACEMENT_3D ( 'NONE', #226756, #127671, #28619 ) ;
#230555 = CARTESIAN_POINT ( 'NONE',  ( -23.25000000000000000, 1.115600667400684642E-11, -100.5000000000000426 ) ) ;
#230556 = ORIENTED_EDGE ( 'NONE', *, *, #65839, .F. ) ;
#230557 = ORIENTED_EDGE ( 'NONE', *, *, #30871, .F. ) ;
#230558 = DIRECTION ( 'NONE',  ( -2.952720810173289112E-16, -1.000000000000000000, -6.982962677686266711E-15 ) ) ;
#230559 = AXIS2_PLACEMENT_3D ( 'NONE', #211406, #113586, #152749 ) ;
#230560 = CARTESIAN_POINT ( 'NONE',  ( -19.89999999999999858, 1.350000000000000089, 21.90000000000000213 ) ) ;
#230561 = CARTESIAN_POINT ( 'NONE',  ( -18.43569575749026512, -9.519327731081288491, -107.4729763765593873 ) ) ;
#230562 = AXIS2_PLACEMENT_3D ( 'NONE', #207376, #246482, #147387 ) ;
#230563 = DIRECTION ( 'NONE',  ( 1.000000000000000000, 0.000000000000000000, 0.000000000000000000 ) ) ;
#230564 = ORIENTED_EDGE ( 'NONE', *, *, #34909, .T. ) ;
#230565 = DIRECTION ( 'NONE',  ( 0.000000000000000000, 0.000000000000000000, -1.000000000000000000 ) ) ;
#230566 = AXIS2_PLACEMENT_3D ( 'NONE', #247554, #31112, #49351 ) ;
#230567 = ITEM_DEFINED_TRANSFORMATION ( 'NONE', 'NONE', #94356,  #2425 ) ;
#230569 = AXIS2_PLACEMENT_3D ( 'NONE', #56523, #52687, #34458 ) ;
#230568 = FACE_OUTER_BOUND ( 'NONE', #104581, .T. ) ;
#230570 = ORIENTED_EDGE ( 'NONE', *, *, #189861, .T. ) ;
#230571 = DIRECTION ( 'NONE',  ( 0.000000000000000000, 0.000000000000000000, 1.000000000000000000 ) ) ;
#230572 = AXIS2_PLACEMENT_3D ( 'NONE', #120253, #21141, #100608 ) ;
#230573 = VECTOR ( 'NONE', #131984, 1000.000000000000000 ) ;
#230574 = PRODUCT_DEFINITION_SHAPE ( 'NONE', 'NONE',  #40537 ) ;
#230575 = AXIS2_PLACEMENT_3D ( 'NONE', #42121, #129033, #64230 ) ;
#230576 = ORIENTED_EDGE ( 'NONE', *, *, #126807, .F. ) ;
#230577 = ORIENTED_EDGE ( 'NONE', *, *, #113535, .F. ) ;
#230578 = ORIENTED_EDGE ( 'NONE', *, *, #14106, .T. ) ;
#230579 = DIRECTION ( 'NONE',  ( 0.000000000000000000, -1.000000000000000000, 0.000000000000000000 ) ) ;
#230580 = DIRECTION ( 'NONE',  ( 0.000000000000000000, -0.9770955615653357240, -0.2128009952263406890 ) ) ;
#230582 = AXIS2_PLACEMENT_3D ( 'NONE', #49639, #50895, #127903 ) ;
#230581 = CARTESIAN_POINT ( 'NONE',  ( 21.05000000000000071, 71.18691588786205671, -57.58158972800053022 ) ) ;
#230583 = CARTESIAN_POINT ( 'NONE',  ( 18.49999999999999289, -9.419078080838366063, -140.8299253502082991 ) ) ;
#230584 = DIRECTION ( 'NONE',  ( -1.000000000000000000, -0.000000000000000000, 0.000000000000000000 ) ) ;
#230585 = CARTESIAN_POINT ( 'NONE',  ( 18.79999999999999716, -11.74999999999999645, 33.00000000000000000 ) ) ;
#230586 = EDGE_CURVE ( 'NONE', #108268, #42982, #210290, .T. ) ;
#230587 = LINE ( 'NONE', #54496, #164121 ) ;
#230589 = DIRECTION ( 'NONE',  ( 1.000000000000000000, -0.000000000000000000, 0.000000000000000000 ) ) ;
#230588 = CARTESIAN_POINT ( 'NONE',  ( 22.88900146558018989, 52.12831263616270405, -233.0836648073824335 ) ) ;
#230590 = AXIS2_PLACEMENT_3D ( 'NONE', #88617, #192888, #249022 ) ;
#230591 = DIRECTION ( 'NONE',  ( -1.000000000000000000, -1.646408749285562691E-14, 0.000000000000000000 ) ) ;
#230592 = CARTESIAN_POINT ( 'NONE',  ( -21.05000000000000071, 76.00000000001213607, -136.5231074845242745 ) ) ;
#230593 = CARTESIAN_POINT ( 'NONE',  ( -18.50000000000000711, 18.81339837015603322, -226.7756228984618190 ) ) ;
#230594 = DIRECTION ( 'NONE',  ( -1.000000000000000000, 0.000000000000000000, 0.000000000000000000 ) ) ;
#230595 = ORIENTED_EDGE ( 'NONE', *, *, #223906, .F. ) ;
#230596 = CARTESIAN_POINT ( 'NONE',  ( -18.31572283045144900, -9.548437830885816879, -40.35062565105839383 ) ) ;
#230597 = VECTOR ( 'NONE', #193546, 1000.000000000000000 ) ;
#230598 = DIRECTION ( 'NONE',  ( -0.7071067811865473507, -0.3338907855510733769, -0.6233112732207618523 ) ) ;
#230599 = CARTESIAN_POINT ( 'NONE',  ( -21.05000000000000071, 76.00000000001237765, -170.0231074845243597 ) ) ;
#230600 = AXIS2_PLACEMENT_3D ( 'NONE', #178305, #99989, #21787 ) ;
#230601 = CARTESIAN_POINT ( 'NONE',  ( -21.00000000000000000, 1.311673547813416718, -7.986648289447971116 ) ) ;
#230603 = ADVANCED_FACE ( 'NONE', ( #69505 ), #149039, .F. ) ;
#230602 = DIRECTION ( 'NONE',  ( 0.000000000000000000, 0.000000000000000000, 1.000000000000000000 ) ) ;
#230604 = DIRECTION ( 'NONE',  ( 0.000000000000000000, 0.8660254037844385966, -0.5000000000000003331 ) ) ;
#230605 = APPLICATION_CONTEXT ( 'automotive_design' ) ;
#230606 = ORIENTED_EDGE ( 'NONE', *, *, #201112, .F. ) ;
#230607 = ORIENTED_EDGE ( 'NONE', *, *, #255155, .T. ) ;
#230608 = EDGE_CURVE ( 'NONE', #219363, #18611, #165312, .T. ) ;
#230609 = ORIENTED_EDGE ( 'NONE', *, *, #222809, .F. ) ;
#230610 = CYLINDRICAL_SURFACE ( 'NONE', #250819, 0.09999999999999939493 ) ;
#230611 = DIRECTION ( 'NONE',  ( 1.000000000000000000, -0.000000000000000000, 0.000000000000000000 ) ) ;
#230612 = EDGE_CURVE ( 'NONE', #146049, #121066, #251966, .T. ) ;
#230613 = CIRCLE ( 'NONE', #97274, 4.100000000000006750 ) ;
#230614 = VECTOR ( 'NONE', #223600, 1000.000000000000000 ) ;
#230615 = AXIS2_PLACEMENT_3D ( 'NONE', #124587, #63304, #161142 ) ;
#230616 = EDGE_CURVE ( 'NONE', #57945, #159851, #36343, .T. ) ;
#230617 = ORIENTED_EDGE ( 'NONE', *, *, #118562, .T. ) ;
#230618 = CARTESIAN_POINT ( 'NONE',  ( 23.15000000000000213, -13.88357498613435048, -191.9982587459959689 ) ) ;
#230619 =( BOUNDED_SURFACE ( )  B_SPLINE_SURFACE ( 3, 2, ( 
 ( #161291, #240814, #216096 ),
 ( #62179, #42605, #122150 ),
 ( #17895, #97407, #77868 ),
 ( #58296, #178296, #10868 ) ),
 .UNSPECIFIED., .F., .F., .F. ) 
 B_SPLINE_SURFACE_WITH_KNOTS ( ( 4, 4 ),
 ( 3, 3 ),
 ( -1.355252715606880543E-20, 0.0003124336117481267463 ),
 ( 0.000000000000000000, 1.000000000000000000 ),
 .UNSPECIFIED. ) 
 GEOMETRIC_REPRESENTATION_ITEM ( )  RATIONAL_B_SPLINE_SURFACE ( (
 ( 1.000000000000000000, 0.7040654476015973939, 1.000000000000000000),
 ( 1.000000000000000000, 0.7039193538781929327, 1.000000000000000000),
 ( 1.000000000000000000, 0.7089171279145388693, 1.000000000000000000),
 ( 1.000000000000000000, 0.7071067811865567876, 1.000000000000000000) ) ) 
 REPRESENTATION_ITEM ( '' )  SURFACE ( )  );
#230620 = ORIENTED_EDGE ( 'NONE', *, *, #257479, .F. ) ;
#230621 = EDGE_CURVE ( 'NONE', #26287, #20561, #215407, .T. ) ;
#230622 = CARTESIAN_POINT ( 'NONE',  ( -18.50000000000000000, 64.35000000001203091, -114.7731074845243882 ) ) ;
#230623 = DIRECTION ( 'NONE',  ( 1.000000000000000000, -0.000000000000000000, -0.000000000000000000 ) ) ;
#230624 = DIRECTION ( 'NONE',  ( 1.000000000000000000, -0.000000000000000000, 0.000000000000000000 ) ) ;
#230625 = CARTESIAN_POINT ( 'NONE',  ( -23.15000000000000213, 73.40000000001276703, -215.2731074845243882 ) ) ;
#230626 = DIRECTION ( 'NONE',  ( 1.000000000000000000, 0.000000000000000000, 0.000000000000000000 ) ) ;
#230627 = FACE_BOUND ( 'NONE', #151605, .T. ) ;
#230628 = EDGE_CURVE ( 'NONE', #90111, #72671, #36813, .T. ) ;
#230629 = CARTESIAN_POINT ( 'NONE',  ( 20.94999999999999574, 1.736257131608553550, -45.06865232901750318 ) ) ;
#230630 = CARTESIAN_POINT ( 'NONE',  ( -20.54999999999999716, 85.40000000001231228, -160.1291383618718385 ) ) ;
#230632 = EDGE_LOOP ( 'NONE', ( #66025, #19479, #174281, #224171 ) ) ;
#230631 = CARTESIAN_POINT ( 'NONE',  ( 18.59999999999999076, 6.550000000011156231, -54.65000000000000568 ) ) ;
#230634 = CARTESIAN_POINT ( 'NONE',  ( -18.39999999999999858, 64.52132590001231449, -60.24841426818374401 ) ) ;
#230633 = DIRECTION ( 'NONE',  ( 0.000000000000000000, -1.000000000000000000, 0.000000000000000000 ) ) ;
#230635 = VERTEX_POINT ( 'NONE', #156755 ) ;
#230637 = ORIENTED_EDGE ( 'NONE', *, *, #243595, .F. ) ;
#230636 = DIRECTION ( 'NONE',  ( 0.000000000000000000, -1.000000000000000000, -6.982962677686266711E-15 ) ) ;
#230638 = VERTEX_POINT ( 'NONE', #236257 ) ;
#230639 = FACE_OUTER_BOUND ( 'NONE', #227901, .T. ) ;
#230640 = DIRECTION ( 'NONE',  ( 0.000000000000000000, 1.000000000000000000, 0.000000000000000000 ) ) ;
#230641 = AXIS2_PLACEMENT_3D ( 'NONE', #238646, #59984, #139529 ) ;
#230642 = CARTESIAN_POINT ( 'NONE',  ( 22.43288208788031568, 75.99510014512635792, -81.17275932824340146 ) ) ;
#230643 = DIRECTION ( 'NONE',  ( 0.000000000000000000, -6.982962677686266711E-15, 1.000000000000000000 ) ) ;
#230644 = DIRECTION ( 'NONE',  ( 0.000000000000000000, 0.2128009952263982818, -0.9770955615653232895 ) ) ;
#230645 = DIRECTION ( 'NONE',  ( 1.000000000000000000, -0.000000000000000000, -0.000000000000000000 ) ) ;
#230646 = CARTESIAN_POINT ( 'NONE',  ( -17.29838795458583434, 12.55891772868854517, -209.9271805838396290 ) ) ;
#230648 = EDGE_CURVE ( 'NONE', #63710, #76531, #95460, .T. ) ;
#230647 = CARTESIAN_POINT ( 'NONE',  ( 21.05000000000000071, 76.00000000001190870, -103.0231074845243029 ) ) ;
#230649 = CARTESIAN_POINT ( 'NONE',  ( -18.59999999999999787, 63.86602797976523505, -212.9247947273492514 ) ) ;
#230650 = ORIENTED_EDGE ( 'NONE', *, *, #12245, .T. ) ;
#230651 = ORIENTED_EDGE ( 'NONE', *, *, #223541, .T. ) ;
#230652 = LINE ( 'NONE', #67717, #48029 ) ;
#230653 = AXIS2_PLACEMENT_3D ( 'NONE', #14546, #193175, #19669 ) ;
#230654 = AXIS2_PLACEMENT_3D ( 'NONE', #80794, #42985, #25992 ) ;
#230655 = VERTEX_POINT ( 'NONE', #75906 ) ;
#230656 = DIRECTION ( 'NONE',  ( -0.7071067811865475727, 0.2890913453342132122, -0.6453109281988448354 ) ) ;
#230657 = ORIENTED_EDGE ( 'NONE', *, *, #14881, .F. ) ;
#230658 = CARTESIAN_POINT ( 'NONE',  ( 18.31572054635735114, -9.548475435778739140, -40.35057016474856795 ) ) ;
#230659 = VECTOR ( 'NONE', #175042, 1000.000000000000000 ) ;
#230660 = EDGE_CURVE ( 'NONE', #25924, #182906, #177605, .T. ) ;
#230661 = DIRECTION ( 'NONE',  ( -0.000000000000000000, 0.000000000000000000, -1.000000000000000000 ) ) ;
#230662 = CARTESIAN_POINT ( 'NONE',  ( 21.14999999999999858, 6.550000000011156231, -45.65000000000000568 ) ) ;
#230663 = DIRECTION ( 'NONE',  ( 1.000000000000000000, -0.000000000000000000, -0.000000000000000000 ) ) ;
#230664 = DIRECTION ( 'NONE',  ( 1.000000000000000000, -5.337610695313232452E-15, 0.000000000000000000 ) ) ;
#230665 = VERTEX_POINT ( 'NONE', #99292 ) ;
#230667 = EDGE_CURVE ( 'NONE', #190151, #120355, #169458, .T. ) ;
#230666 = CARTESIAN_POINT ( 'NONE',  ( 20.85000000000000142, 76.00000000001126921, -203.5231074845248997 ) ) ;
#230668 = B_SPLINE_CURVE_WITH_KNOTS ( 'NONE', 3,
 ( #10309, #166834, #162966, #127678, #45567, #44295, #105500, #85941, #165527, #125120 ),
 .UNSPECIFIED., .F., .F.,
 ( 4, 3, 3, 4 ),
 ( -2.000561356209491534E-06, 0.000000000000000000, 1.787822682428948123E-05, 4.206475347090082037E-05 ),
 .UNSPECIFIED. ) ;
#230669 = CARTESIAN_POINT ( 'NONE',  ( -23.25000000000000000, 73.40000000001253966, -183.2477294072864709 ) ) ;
#230670 = DIRECTION ( 'NONE',  ( -1.000000000000000000, 0.000000000000000000, 0.000000000000000000 ) ) ;
#230671 = DIRECTION ( 'NONE',  ( -1.000000000000000000, 0.000000000000000000, -0.000000000000000000 ) ) ;
#230672 = CYLINDRICAL_SURFACE ( 'NONE', #194854, 0.1000000000000002554 ) ;
#230674 = EDGE_CURVE ( 'NONE', #31422, #149811, #194566, .T. ) ;
#230673 = DIRECTION ( 'NONE',  ( -0.000000000000000000, 0.1022405907414166287, 0.9947597004326451664 ) ) ;
#230675 = VERTEX_POINT ( 'NONE', #178896 ) ;
#230677 = CARTESIAN_POINT ( 'NONE',  ( -20.94999999999999929, 70.56573376625485139, -228.3808404818380779 ) ) ;
#230676 = LINE ( 'NONE', #231969, #104 ) ;
#230679 = ORIENTED_EDGE ( 'NONE', *, *, #200115, .T. ) ;
#230678 = CIRCLE ( 'NONE', #118230, 0.1000000000000028644 ) ;
#230681 = EDGE_LOOP ( 'NONE', ( #93050, #98810, #190093, #206097 ) ) ;
#230680 = CARTESIAN_POINT ( 'NONE',  ( 21.30000000000002558, 3.558777552609281081, -231.8203201594644725 ) ) ;
#230682 = EDGE_CURVE ( 'NONE', #150102, #105021, #56941, .T. ) ;
#230683 = CARTESIAN_POINT ( 'NONE',  ( 20.02499999999999858, 66.25000000001151079, -48.37310748452438958 ) ) ;
#230684 = AXIS2_PLACEMENT_3D ( 'NONE', #187372, #47821, #145647 ) ;
#230685 = VECTOR ( 'NONE', #181008, 1000.000000000000000 ) ;
#230686 = FACE_OUTER_BOUND ( 'NONE', #58351, .T. ) ;
#230687 = ORIENTED_EDGE ( 'NONE', *, *, #225859, .F. ) ;
#230688 = DIRECTION ( 'NONE',  ( 0.000000000000000000, 0.000000000000000000, 1.000000000000000000 ) ) ;
#230690 = ADVANCED_FACE ( 'NONE', ( #255781 ), #58878, .F. ) ;
#230689 = DIRECTION ( 'NONE',  ( -0.000000000000000000, -0.000000000000000000, 1.000000000000000000 ) ) ;
#230692 = DIRECTION ( 'NONE',  ( 0.000000000000000000, 1.000000000000000000, 0.000000000000000000 ) ) ;
#230691 = CARTESIAN_POINT ( 'NONE',  ( -20.94999999999999929, 77.16412189325360771, -162.1082593989527254 ) ) ;
#230693 = VERTEX_POINT ( 'NONE', #134567 ) ;
#230694 = ADVANCED_FACE ( 'NONE', ( #155482 ), #154206, .T. ) ;
#230695 = VECTOR ( 'NONE', #124905, 1000.000000000000000 ) ;
#230696 = EDGE_CURVE ( 'NONE', #185637, #42744, #214135, .T. ) ;
#230697 = EDGE_LOOP ( 'NONE', ( #144656, #198845, #228938, #151188 ) ) ;
#230698 = CARTESIAN_POINT ( 'NONE',  ( 21.05000000000000071, 76.00000000001142553, -36.02310748452432421 ) ) ;
#230699 = CIRCLE ( 'NONE', #214121, 0.1000000000000102612 ) ;
#230700 = LINE ( 'NONE', #152460, #168806 ) ;
#230701 = CARTESIAN_POINT ( 'NONE',  ( -18.50000000000000000, 67.67657779757796277, -227.9615671787948372 ) ) ;
#230702 = ORIENTED_EDGE ( 'NONE', *, *, #242727, .F. ) ;
#230703 = DIRECTION ( 'NONE',  ( 0.000000000000000000, -1.000000000000000000, 0.000000000000000000 ) ) ;
#230704 = EDGE_CURVE ( 'NONE', #41742, #973, #107033, .T. ) ;
#230705 = AXIS2_PLACEMENT_3D ( 'NONE', #219120, #77052, #199602 ) ;
#230706 = CARTESIAN_POINT ( 'NONE',  ( 21.05000000000000071, 30.43677443282724937, -239.5249545687858870 ) ) ;
#230707 = CARTESIAN_POINT ( 'NONE',  ( -23.39999999999994529, 87.51781941433023349, -37.75951082105083145 ) ) ;
#230708 = ORIENTED_EDGE ( 'NONE', *, *, #242385, .F. ) ;
#230709 = CARTESIAN_POINT ( 'NONE',  ( -20.54999999999999716, 74.07476635515175190, -56.79286395139820343 ) ) ;
#230710 = VECTOR ( 'NONE', #79593, 1000.000000000000000 ) ;
#230711 = AXIS2_PLACEMENT_3D ( 'NONE', #87567, #103273, #224524 ) ;
#230712 = AXIS2_PLACEMENT_3D ( 'NONE', #191154, #171602, #248533 ) ;
#230713 = ORIENTED_EDGE ( 'NONE', *, *, #141163, .F. ) ;
#230714 = CARTESIAN_POINT ( 'NONE',  ( 18.59999999999999076, 10.20857864377385127, -91.65000000000004832 ) ) ;
#230715 = CARTESIAN_POINT ( 'NONE',  ( -16.87036670365549895, 66.01058118071021852, -90.50266760182643111 ) ) ;
#230716 = VERTEX_POINT ( 'NONE', #257054 ) ;
#230717 = EDGE_LOOP ( 'NONE', ( #20706, #125163, #196425, #73006 ) ) ;
#230718 =( BOUNDED_SURFACE ( )  B_SPLINE_SURFACE ( 3, 2, ( 
 ( #77897, #60901, #140435 ),
 ( #214847, #19220, #219981 ),
 ( #156194, #6059, #244669 ),
 ( #144269, #2202, #64757 ),
 ( #204258, #223818, #245975 ),
 ( #26952, #243393, #45196 ) ),
 .UNSPECIFIED., .F., .F., .T. ) 
 B_SPLINE_SURFACE_WITH_KNOTS ( ( 4, 2, 4 ),
 ( 3, 3 ),
 ( 0.0001792624049599621759, 0.0003686986002124750849, 0.0005581347954649879938 ),
 ( 0.000000000000000000, 1.000000000000000000 ),
 .UNSPECIFIED. ) 
 GEOMETRIC_REPRESENTATION_ITEM ( )  RATIONAL_B_SPLINE_SURFACE ( (
 ( 1.000000000000000000, 0.9238795325112859613, 1.000000000000000000),
 ( 1.000000000000000000, 0.9229318695237587189, 1.000000000000000000),
 ( 1.000000000000000000, 0.8926288119231937657, 1.000000000000000000),
 ( 1.000000000000000000, 0.8123777807270391449, 1.000000000000000000),
 ( 1.000000000000000000, 0.7629087100932221421, 1.000000000000000000),
 ( 1.000000000000000000, 0.7071067811865475727, 1.000000000000000000) ) ) 
 REPRESENTATION_ITEM ( '' )  SURFACE ( )  );
#230719 = LINE ( 'NONE', #152484, #158294 ) ;
#230720 = ORIENTED_EDGE ( 'NONE', *, *, #207179, .T. ) ;
#230722 = ORIENTED_EDGE ( 'NONE', *, *, #252911, .F. ) ;
#230721 = DIRECTION ( 'NONE',  ( 0.000000000000000000, -6.982962677686266711E-15, 1.000000000000000000 ) ) ;
#230723 = EDGE_CURVE ( 'NONE', #74473, #217587, #35531, .T. ) ;
#230724 = ADVANCED_FACE ( 'NONE', ( #15962 ), #158058, .F. ) ;
#230725 = ORIENTED_EDGE ( 'NONE', *, *, #73864, .F. ) ;
#230728 = EDGE_LOOP ( 'NONE', ( #161103, #102630, #29026, #95739, #221414 ) ) ;
#230727 = ORIENTED_EDGE ( 'NONE', *, *, #71044, .F. ) ;
#230726 = CARTESIAN_POINT ( 'NONE',  ( -23.39999999999994529, 87.60324567546805952, -37.87437456276921210 ) ) ;
#230729 = AXIS2_PLACEMENT_3D ( 'NONE', #198214, #159124, #216496 ) ;
#230730 = VECTOR ( 'NONE', #90157, 1000.000000000000000 ) ;
#230732 = EDGE_CURVE ( 'NONE', #246004, #49603, #184032, .T. ) ;
#230731 = DIRECTION ( 'NONE',  ( 1.000000000000000000, -0.000000000000000000, -0.000000000000000000 ) ) ;
#230733 = VERTEX_POINT ( 'NONE', #224389 ) ;
#230734 = CARTESIAN_POINT ( 'NONE',  ( 21.03675099975490781, 22.18453705941069387, -231.7293054214682115 ) ) ;
#230735 = CARTESIAN_POINT ( 'NONE',  ( -23.25000000000000355, 9.957490673325212427, -220.1701168356097469 ) ) ;
#230736 = AXIS2_PLACEMENT_3D ( 'NONE', #205909, #208506, #27322 ) ;
#230737 = DIRECTION ( 'NONE',  ( 1.000000000000000000, -0.000000000000000000, -0.000000000000000000 ) ) ;
#230738 = CARTESIAN_POINT ( 'NONE',  ( 23.15000000000000213, 85.00000000001251976, -179.9170766071767389 ) ) ;
#230739 = DIRECTION ( 'NONE',  ( 0.000000000000000000, -0.01283462868041992250, -0.9999176327611367654 ) ) ;
#230740 = ORIENTED_EDGE ( 'NONE', *, *, #24405, .F. ) ;
#230741 = ORIENTED_EDGE ( 'NONE', *, *, #179458, .T. ) ;
#230743 = ORIENTED_EDGE ( 'NONE', *, *, #214149, .T. ) ;
#230742 = CIRCLE ( 'NONE', #126679, 12.97499999999998721 ) ;
#230744 = CARTESIAN_POINT ( 'NONE',  ( -20.05000000000000426, 22.38308386859736032, -231.4104522272575082 ) ) ;
#230745 = AXIS2_PLACEMENT_3D ( 'NONE', #203196, #247458, #84484 ) ;
#230747 = VERTEX_POINT ( 'NONE', #144851 ) ;
#230746 = DIRECTION ( 'NONE',  ( -1.000000000000000000, 0.000000000000000000, 0.000000000000000000 ) ) ;
#230748 = LINE ( 'NONE', #211169, #250644 ) ;
#230750 = ORIENTED_EDGE ( 'NONE', *, *, #39366, .F. ) ;
#230749 = CARTESIAN_POINT ( 'NONE',  ( -21.65000000000000213, 10.05000000001113847, -121.3500000000000369 ) ) ;
#230751 = ORIENTED_EDGE ( 'NONE', *, *, #79950, .T. ) ;
#230752 = CARTESIAN_POINT ( 'NONE',  ( 18.49999999999998934, 63.81702857804527440, -209.2850695923107480 ) ) ;
#230753 = CIRCLE ( 'NONE', #164112, 0.09999999999999939493 ) ;
#230754 = CIRCLE ( 'NONE', #55727, 0.09999999999999939493 ) ;
#230755 = CIRCLE ( 'NONE', #97430, 0.09999999999999766020 ) ;
#230756 = ORIENTED_EDGE ( 'NONE', *, *, #73215, .T. ) ;
#230757 = CONICAL_SURFACE ( 'NONE', #109929, 4.299999999999970512, 0.7853981633974466137 ) ;
#230758 = CARTESIAN_POINT ( 'NONE',  ( -16.86445178670593492, 66.03778837089635090, -149.1323300464075601 ) ) ;
#230760 = EDGE_CURVE ( 'NONE', #242360, #34846, #163159, .T. ) ;
#230759 = LINE ( 'NONE', #93785, #194440 ) ;
#230761 = AXIS2_PLACEMENT_3D ( 'NONE', #238386, #59725, #62324 ) ;
#230763 = EDGE_LOOP ( 'NONE', ( #153187, #163531, #176304, #73839, #40564, #119880, #99700, #38168 ) ) ;
#230762 = ORIENTED_EDGE ( 'NONE', *, *, #74158, .T. ) ;
#230764 = ORIENTED_EDGE ( 'NONE', *, *, #19513, .T. ) ;
#230765 = LINE ( 'NONE', #135476, #98610 ) ;
#230766 = ORIENTED_EDGE ( 'NONE', *, *, #256666, .F. ) ;
#230767 = ORIENTED_EDGE ( 'NONE', *, *, #112051, .F. ) ;
#230768 = CARTESIAN_POINT ( 'NONE',  ( -23.15000000000000213, 69.08367151115869831, -247.5088222940653679 ) ) ;
#230771 = EDGE_CURVE ( 'NONE', #36666, #140456, #2767, .T. ) ;
#230770 = ORIENTED_EDGE ( 'NONE', *, *, #224253, .T. ) ;
#230769 = DIRECTION ( 'NONE',  ( 0.000000000000000000, -0.2617529984165033463, -0.9651348961777157509 ) ) ;
#230772 = DIRECTION ( 'NONE',  ( 0.000000000000000000, -1.000000000000000000, 0.000000000000000000 ) ) ;
#230773 = AXIS2_PLACEMENT_3D ( 'NONE', #24028, #184352, #46130 ) ;
#230775 = FACE_OUTER_BOUND ( 'NONE', #88202, .T. ) ;
#230774 = DIRECTION ( 'NONE',  ( 0.000000000000000000, 0.000000000000000000, -1.000000000000000000 ) ) ;
#230776 = LINE ( 'NONE', #194226, #249023 ) ;
#230777 = FACE_OUTER_BOUND ( 'NONE', #203228, .T. ) ;
#230778 = VERTEX_POINT ( 'NONE', #100564 ) ;
#230779 = ADVANCED_FACE ( 'NONE', ( #181443 ), #236042, .F. ) ;
#230780 = ORIENTED_EDGE ( 'NONE', *, *, #158878, .F. ) ;
#230781 = CARTESIAN_POINT ( 'NONE',  ( 18.41815437325348626, 85.49870985315328653, -96.41916164572225512 ) ) ;
#230782 = AXIS2_PLACEMENT_3D ( 'NONE', #72645, #47910, #173054 ) ;
#230783 = DIRECTION ( 'NONE',  ( -0.000000000000000000, 0.9770955615653313941, 0.2128009952263603954 ) ) ;
#230784 = CARTESIAN_POINT ( 'NONE',  ( 23.14999999999999858, 76.00000000001213607, -136.5231074845243313 ) ) ;
#230785 = EDGE_CURVE ( 'NONE', #76888, #94890, #22372, .T. ) ;
#230787 = VERTEX_POINT ( 'NONE', #45761 ) ;
#230786 = B_SPLINE_CURVE_WITH_KNOTS ( 'NONE', 3,
 ( #194991, #95845, #254874, #93292, #150709, #192403, #230240, #13764, #76289, #34635 ),
 .UNSPECIFIED., .F., .F.,
 ( 4, 2, 2, 2, 4 ),
 ( 0.000000000000000000, 0.0001660831991682816685, 0.0002491247987523890822, 0.0002906455985444105611, 0.0003321663983364320401 ),
 .UNSPECIFIED. ) ;
#230788 = AXIS2_PLACEMENT_3D ( 'NONE', #71698, #207352, #46956 ) ;
#230789 = EDGE_CURVE ( 'NONE', #120448, #62457, #23695, .T. ) ;
#230790 = SPHERICAL_SURFACE ( 'NONE', #250945, 0.1000000000000000056 ) ;
#230791 = CIRCLE ( 'NONE', #39077, 12.77499999999999503 ) ;
#230792 = DIRECTION ( 'NONE',  ( 0.000000000000000000, 0.000000000000000000, -1.000000000000000000 ) ) ;
#230794 = EDGE_CURVE ( 'NONE', #5568, #12989, #121482, .T. ) ;
#230793 = EDGE_CURVE ( 'NONE', #107651, #150745, #65322, .T. ) ;
#230795 = ORIENTED_EDGE ( 'NONE', *, *, #75300, .F. ) ;
#230796 = EDGE_LOOP ( 'NONE', ( #160802, #57831, #209582, #47277 ) ) ;
#230797 = DIRECTION ( 'NONE',  ( 0.000000000000000000, 0.9651348961777148627, -0.2617529984165062329 ) ) ;
#230798 = ORIENTED_EDGE ( 'NONE', *, *, #236990, .F. ) ;
#230799 = FACE_OUTER_BOUND ( 'NONE', #44387, .T. ) ;
#230800 = ORIENTED_EDGE ( 'NONE', *, *, #104327, .T. ) ;
#230801 = CARTESIAN_POINT ( 'NONE',  ( 18.31325810956326805, -9.536388475995964953, -140.8684402063051948 ) ) ;
#230802 = PLANE ( 'NONE',  #145459 ) ;
#230804 = CARTESIAN_POINT ( 'NONE',  ( -21.05000000000000071, -1.448735025027834800, -194.7511878402588934 ) ) ;
#230803 = CARTESIAN_POINT ( 'NONE',  ( -20.85000000000000142, 1.115600667400684642E-11, -167.5000000000000284 ) ) ;
#230805 = CARTESIAN_POINT ( 'NONE',  ( -18.59999999999999787, 74.83729825007388570, -94.92310748452432279 ) ) ;
#230806 = CARTESIAN_POINT ( 'NONE',  ( -22.39999999999999858, 7.790779598384560245, -167.3999999999999773 ) ) ;
#230807 = DIRECTION ( 'NONE',  ( -1.000000000000000000, 2.952720810173289112E-16, 2.061873921506763405E-30 ) ) ;
#230808 = DIRECTION ( 'NONE',  ( 0.000000000000000000, -1.000000000000000000, -2.891205793294679805E-16 ) ) ;
#230811 = ORIENTED_EDGE ( 'NONE', *, *, #201847, .F. ) ;
#230810 = AXIS2_PLACEMENT_3D ( 'NONE', #195738, #113605, #193157 ) ;
#230809 = DIRECTION ( 'NONE',  ( 1.186688945009010077E-16, 1.000000000000000000, 6.982962677686266711E-15 ) ) ;
#230813 = EDGE_CURVE ( 'NONE', #185697, #61007, #111146, .T. ) ;
#230812 = AXIS2_PLACEMENT_3D ( 'NONE', #32138, #94643, #192472 ) ;
#230814 = TOROIDAL_SURFACE ( 'NONE', #68475, 6.258578643762700899, 0.1000000000000000056 ) ;
#230815 = EDGE_CURVE ( 'NONE', #34312, #165621, #182727, .T. ) ;
#230817 = ORIENTED_EDGE ( 'NONE', *, *, #238851, .F. ) ;
#230816 = ORIENTED_EDGE ( 'NONE', *, *, #153884, .F. ) ;
#230818 = ORIENTED_EDGE ( 'NONE', *, *, #235370, .F. ) ;
#230819 = EDGE_CURVE ( 'NONE', #3667, #128197, #52871, .T. ) ;
#230820 = CARTESIAN_POINT ( 'NONE',  ( -20.85000000000000142, 75.83895117929270668, -36.30729732888454464 ) ) ;
#230821 = DIRECTION ( 'NONE',  ( 1.000000000000000000, 0.000000000000000000, 0.000000000000000000 ) ) ;
#230823 = DIRECTION ( 'NONE',  ( 1.000000000000000000, 0.000000000000000000, 0.000000000000000000 ) ) ;
#230822 = DIRECTION ( 'NONE',  ( 0.000000000000000000, -0.2128009952263605897, 0.9770955615653315052 ) ) ;
#230824 = FACE_OUTER_BOUND ( 'NONE', #199386, .T. ) ;
#230825 = ORIENTED_EDGE ( 'NONE', *, *, #59916, .F. ) ;
#230826 = CARTESIAN_POINT ( 'NONE',  ( 21.46681500593528824, 69.14248884062956790, -69.52310748452435973 ) ) ;
#230827 = EDGE_CURVE ( 'NONE', #242875, #108030, #123624, .T. ) ;
#230828 = ORIENTED_EDGE ( 'NONE', *, *, #169692, .T. ) ;
#230829 = EDGE_LOOP ( 'NONE', ( #230557, #225437, #75707, #164884, #111147, #251960 ) ) ;
#230830 = DIRECTION ( 'NONE',  ( 0.000000000000000000, 0.000000000000000000, -1.000000000000000000 ) ) ;
#230831 = CARTESIAN_POINT ( 'NONE',  ( 18.59999999999999076, 58.01113881014391893, -224.9619361160449387 ) ) ;
#230832 = EDGE_CURVE ( 'NONE', #57087, #99741, #86173, .T. ) ;
#230833 = DIRECTION ( 'NONE',  ( -1.000000000000000000, -0.000000000000000000, -0.000000000000000000 ) ) ;
#230834 = ORIENTED_EDGE ( 'NONE', *, *, #18643, .T. ) ;
#230835 = DIRECTION ( 'NONE',  ( -1.000000000000000000, -0.000000000000000000, -0.000000000000000000 ) ) ;
#230836 = CIRCLE ( 'NONE', #180927, 11.90000000000000213 ) ;
#230837 = CARTESIAN_POINT ( 'NONE',  ( 22.45463910399148233, 1.026727559903827787E-11, -155.8504291898206020 ) ) ;
#230838 = ORIENTED_EDGE ( 'NONE', *, *, #164980, .T. ) ;
#230839 = ORIENTED_EDGE ( 'NONE', *, *, #245753, .F. ) ;
#230840 = CARTESIAN_POINT ( 'NONE',  ( -16.88853107394619357, 9.950878483358135185, -54.35293634689223552 ) ) ;
#230841 = CARTESIAN_POINT ( 'NONE',  ( -16.87036670365548474, 9.989418819312801290, -54.47956011730205006 ) ) ;
#230842 = DIRECTION ( 'NONE',  ( 1.000000000000000000, -6.938893903907222067E-15, -4.845403715540888588E-29 ) ) ;
#230843 = EDGE_CURVE ( 'NONE', #92492, #152553, #202713, .T. ) ;
#230844 = DIRECTION ( 'NONE',  ( 0.000000000000000000, -0.5000000000000016653, 0.8660254037844377084 ) ) ;
#230845 = DIRECTION ( 'NONE',  ( -0.000000000000000000, 1.000000000000000000, -0.000000000000000000 ) ) ;
#230846 = CARTESIAN_POINT ( 'NONE',  ( -16.86133551771148831, 9.950000000011137047, -188.3013434345466806 ) ) ;
#230847 = EDGE_LOOP ( 'NONE', ( #48561, #170877, #24842, #125219 ) ) ;
#230848 = DIRECTION ( 'NONE',  ( -1.000000000000000000, -0.000000000000000000, -0.000000000000000000 ) ) ;
#230849 = CARTESIAN_POINT ( 'NONE',  ( -21.05000000000000071, -11.29603075032412995, -137.0478991596638991 ) ) ;
#230851 = CARTESIAN_POINT ( 'NONE',  ( -21.05000000000000071, 11.65000000001115055, -174.2838656629781156 ) ) ;
#230850 = CARTESIAN_POINT ( 'NONE',  ( -23.25000000000000000, 10.33248238083634440, -173.0948465439131496 ) ) ;
#230852 = DIRECTION ( 'NONE',  ( -1.000000000000000000, 0.000000000000000000, -0.000000000000000000 ) ) ;
#230854 = EDGE_CURVE ( 'NONE', #35141, #56718, #231977, .T. ) ;
#230853 = CARTESIAN_POINT ( 'NONE',  ( -23.15000000000000213, -11.41227409413852811, -164.5000000000000000 ) ) ;
#230855 = DIRECTION ( 'NONE',  ( 1.734723475976817507E-14, 0.000000000000000000, -1.000000000000000000 ) ) ;
#230856 = DIRECTION ( 'NONE',  ( -1.000000000000000000, -0.000000000000000000, 0.000000000000000000 ) ) ;
#230857 = VECTOR ( 'NONE', #113619, 1000.000000000000114 ) ;
#230859 = ORIENTED_EDGE ( 'NONE', *, *, #79590, .F. ) ;
#230858 = LINE ( 'NONE', #57306, #57240 ) ;
#230860 = TOROIDAL_SURFACE ( 'NONE', #51726, 11.65000000000000036, 0.1000000000000000056 ) ;
#230861 = AXIS2_PLACEMENT_3D ( 'NONE', #105689, #108299, #170890 ) ;
#230862 = AXIS2_PLACEMENT_3D ( 'NONE', #192624, #153544, #54386 ) ;
#230864 = EDGE_CURVE ( 'NONE', #52949, #10056, #11198, .T. ) ;
#230863 = DIRECTION ( 'NONE',  ( 0.000000000000000000, -0.000000000000000000, -1.000000000000000000 ) ) ;
#230865 = LINE ( 'NONE', #90032, #99069 ) ;
#230866 = DIRECTION ( 'NONE',  ( -1.000000000000000000, 0.000000000000000000, 0.000000000000000000 ) ) ;
#230867 = CARTESIAN_POINT ( 'NONE',  ( 15.57250062127604373, 9.370689921613767126, -84.52646512666112244 ) ) ;
#230868 = DIRECTION ( 'NONE',  ( -1.000000000000000000, 0.000000000000000000, 0.000000000000000000 ) ) ;
#230869 = CIRCLE ( 'NONE', #10081, 0.09999999999999939493 ) ;
#230870 = CARTESIAN_POINT ( 'NONE',  ( -20.94999999999999929, 1.249999999999999334, -8.000000000000000000 ) ) ;
#230871 = AXIS2_PLACEMENT_3D ( 'NONE', #110378, #101032, #80205 ) ;
#230872 = CARTESIAN_POINT ( 'NONE',  ( 20.85000000000000142, -11.64999999998883595, -100.5000000000000426 ) ) ;
#230873 = DIRECTION ( 'NONE',  ( 1.000000000000000000, -0.000000000000000000, -0.000000000000000000 ) ) ;
#230874 = VECTOR ( 'NONE', #257590, 1000.000000000000114 ) ;
#230875 = CIRCLE ( 'NONE', #247402, 0.09999999999998898659 ) ;
#230876 = ORIENTED_EDGE ( 'NONE', *, *, #48882, .F. ) ;
#230877 = CARTESIAN_POINT ( 'NONE',  ( -18.59999999999999787, 7.021664781911246322, -204.8335654018972605 ) ) ;
#230879 = ORIENTED_EDGE ( 'NONE', *, *, #172767, .F. ) ;
#230878 = CARTESIAN_POINT ( 'NONE',  ( 23.14999999999999858, 69.35000000001228670, -157.6731074845243938 ) ) ;
#230880 = CARTESIAN_POINT ( 'NONE',  ( -18.39999999999999858, 11.47316190337362762, -42.82594606680797256 ) ) ;
#230881 = FACE_OUTER_BOUND ( 'NONE', #85644, .T. ) ;
#230882 = EDGE_LOOP ( 'NONE', ( #102723, #208212, #41981, #180328 ) ) ;
#230883 = DIRECTION ( 'NONE',  ( -0.000000000000000000, -0.8814952561688430555, 0.4721928772777346239 ) ) ;
#230884 = VECTOR ( 'NONE', #206433, 999.9999999999998863 ) ;
#230885 = APPLICATION_PROTOCOL_DEFINITION ( 'draft international standard', 'automotive_design', 1998, #175775 ) ;
#230887 = CARTESIAN_POINT ( 'NONE',  ( -20.94403535211772294, 65.69367753730635684, -64.01892380663480253 ) ) ;
#230886 = CIRCLE ( 'NONE', #134967, 0.1000000000000092620 ) ;
#230889 = AXIS2_PLACEMENT_3D ( 'NONE', #52931, #172934, #227712 ) ;
#230888 = DIRECTION ( 'NONE',  ( 0.000000000000000000, -0.9887567792719341719, -0.1495327102803664099 ) ) ;
#230890 = DIRECTION ( 'NONE',  ( 0.000000000000000000, -6.982962677686266711E-15, 1.000000000000000000 ) ) ;
#230891 = ORIENTED_EDGE ( 'NONE', *, *, #79951, .T. ) ;
#230892 = CARTESIAN_POINT ( 'NONE',  ( -17.01825945287482966, 12.51174298335651791, -211.2216088517780292 ) ) ;
#230893 = DIRECTION ( 'NONE',  ( 1.000000000000000000, 0.000000000000000000, 0.000000000000000000 ) ) ;
#230894 = B_SPLINE_CURVE_WITH_KNOTS ( 'NONE', 3,
 ( #205541, #85569, #26956, #166468, #127309, #106431, #185999, #2207, #244673, #225098, #226379, #245979, #4763 ),
 .UNSPECIFIED., .F., .F.,
 ( 4, 3, 3, 3, 4 ),
 ( 1.084999851846394554E-16, 1.946463881814392694E-05, 3.922356109944192040E-05, 4.215060953238614744E-05, 4.415117091093003941E-05 ),
 .UNSPECIFIED. ) ;
#230895 = VECTOR ( 'NONE', #147155, 1000.000000000000000 ) ;
#230896 = ORIENTED_EDGE ( 'NONE', *, *, #153407, .T. ) ;
#230897 = ORIENTED_EDGE ( 'NONE', *, *, #182059, .T. ) ;
#230898 = CIRCLE ( 'NONE', #51976, 7.800000000000002487 ) ;
#230899 = CARTESIAN_POINT ( 'NONE',  ( 21.14999999999999858, -0.09999999998884338825, -127.4593430482987912 ) ) ;
#230900 = AXIS2_PLACEMENT_3D ( 'NONE', #65136, #45585, #164263 ) ;
#230901 = VECTOR ( 'NONE', #151739, 1000.000000000000000 ) ;
#230902 = CARTESIAN_POINT ( 'NONE',  ( 20.85000000000000142, 1.115600667400684642E-11, -200.9999999999999432 ) ) ;
#230903 = DIRECTION ( 'NONE',  ( 0.000000000000000000, -0.9908441862701596881, 0.1350103645451904977 ) ) ;
#230904 = CARTESIAN_POINT ( 'NONE',  ( -21.70464131381649509, 68.90464198104409377, -103.0231074845243739 ) ) ;
#230905 = EDGE_CURVE ( 'NONE', #31765, #219381, #2980, .T. ) ;
#230907 = CARTESIAN_POINT ( 'NONE',  ( -18.40000000000000213, 64.52683809664972614, -145.8490535513323891 ) ) ;
#230906 = CARTESIAN_POINT ( 'NONE',  ( 18.50000000000000000, 86.35479209693734504, -109.2665665014504697 ) ) ;
#230908 = DIRECTION ( 'NONE',  ( -1.000000000000000000, 0.000000000000000000, 0.000000000000000000 ) ) ;
#230909 = B_SPLINE_CURVE_WITH_KNOTS ( 'NONE', 3,
 ( #151578, #49869, #208950, #111135, #88981, #107273, #90264, #48583 ),
 .UNSPECIFIED., .F., .F.,
 ( 4, 2, 2, 4 ),
 ( 0.000000000000000000, 6.534141206311710429E-05, 0.0001306828241262342086, 0.0002613656482524441852 ),
 .UNSPECIFIED. ) ;
#230910 = DIRECTION ( 'NONE',  ( 0.000000000000000000, 0.5283051335750404975, -0.8490545835446967615 ) ) ;
#230911 = DIRECTION ( 'NONE',  ( -3.469446951953515108E-14, -1.000000000000000000, 0.000000000000000000 ) ) ;
#230912 = VERTEX_POINT ( 'NONE', #57539 ) ;
#230914 = ORIENTED_EDGE ( 'NONE', *, *, #38183, .F. ) ;
#230913 = CARTESIAN_POINT ( 'NONE',  ( 20.99999999999999645, 66.25000000001190870, -93.77310748452438816 ) ) ;
#230915 = CARTESIAN_POINT ( 'NONE',  ( 21.14999999999999858, 69.45934304831114048, -170.0231074845243882 ) ) ;
#230916 = CARTESIAN_POINT ( 'NONE',  ( -21.14250536705909056, -1.387073526285510061, -194.6311228964526663 ) ) ;
#230918 = CARTESIAN_POINT ( 'NONE',  ( -21.06715728752538652, 11.75000000001115197, -141.0148057706540214 ) ) ;
#230917 = DIRECTION ( 'NONE',  ( 0.000000000000000000, 0.000000000000000000, -1.000000000000000000 ) ) ;
#230919 = EDGE_LOOP ( 'NONE', ( #76370, #126629, #210229, #203663 ) ) ;
#230920 = DIRECTION ( 'NONE',  ( 0.000000000000000000, 0.2617529984164506107, 0.9651348961777299618 ) ) ;
#230922 = ADVANCED_FACE ( 'NONE', ( #238768 ), #135794, .T. ) ;
#230921 = CARTESIAN_POINT ( 'NONE',  ( 19.96984138294275368, 64.25000000001196554, -111.7985354133235063 ) ) ;
#230923 = DIRECTION ( 'NONE',  ( -1.000000000000000000, -0.000000000000000000, -0.000000000000000000 ) ) ;
#230924 = CYLINDRICAL_SURFACE ( 'NONE', #14956, 0.1000000000000122874 ) ;
#230925 = EDGE_LOOP ( 'NONE', ( #111100, #90609, #20988, #24928 ) ) ;
#230926 = ORIENTED_EDGE ( 'NONE', *, *, #110628, .F. ) ;
#230927 = EDGE_CURVE ( 'NONE', #188264, #251940, #131990, .T. ) ;
#230928 = CIRCLE ( 'NONE', #226796, 1.749999999999998002 ) ;
#230929 = CIRCLE ( 'NONE', #143414, 0.1000000000000028644 ) ;
#230930 = DIRECTION ( 'NONE',  ( 0.000000000000000000, 0.000000000000000000, 1.000000000000000000 ) ) ;
#230931 = EDGE_LOOP ( 'NONE', ( #96270, #159573, #46200, #88946 ) ) ;
#230932 = CARTESIAN_POINT ( 'NONE',  ( 20.94999999999999574, -11.48912529306490349, -70.00000000000004263 ) ) ;
#230933 = VECTOR ( 'NONE', #196300, 1000.000000000000114 ) ;
#230934 = DIRECTION ( 'NONE',  ( 0.000000000000000000, -6.938893903907222067E-15, 1.000000000000000000 ) ) ;
#230935 = CARTESIAN_POINT ( 'NONE',  ( -21.09813707148783735, 65.52970697556288826, -242.0093664099801174 ) ) ;
#230936 = AXIS2_PLACEMENT_3D ( 'NONE', #20287, #99779, #196334 ) ;
#230937 = EDGE_CURVE ( 'NONE', #70737, #237439, #117531, .T. ) ;
#230938 = AXIS2_PLACEMENT_3D ( 'NONE', #111815, #250030, #230471 ) ;
#230940 = EDGE_CURVE ( 'NONE', #191212, #211554, #181386, .T. ) ;
#230939 = FACE_OUTER_BOUND ( 'NONE', #115305, .T. ) ;
#230941 = VERTEX_POINT ( 'NONE', #22310 ) ;
#230942 = CARTESIAN_POINT ( 'NONE',  ( -20.64999999999999858, 73.60000000001230092, -156.7984855617622770 ) ) ;
#230943 = TOROIDAL_SURFACE ( 'NONE', #151831, 0.2000000000000000111, 0.1000000000000000056 ) ;
#230944 = EDGE_CURVE ( 'NONE', #152584, #114560, #15497, .T. ) ;
#230945 = DIRECTION ( 'NONE',  ( 0.000000000000000000, -6.938893903907222067E-15, 1.000000000000000000 ) ) ;
#230947 = VECTOR ( 'NONE', #91898, 1000.000000000000000 ) ;
#230946 = LINE ( 'NONE', #107116, #149309 ) ;
#230948 = CARTESIAN_POINT ( 'NONE',  ( -20.94999999999999929, 77.16270174995064224, -195.4231074845243370 ) ) ;
#230950 = CIRCLE ( 'NONE', #22656, 0.09999999999999939493 ) ;
#230949 = CARTESIAN_POINT ( 'NONE',  ( 23.24999999999999289, 6.450000000011156587, -121.6500000000000341 ) ) ;
#230951 = CARTESIAN_POINT ( 'NONE',  ( -20.94999999999999929, 14.05000000001115623, -94.98630492923912527 ) ) ;
#230952 = EDGE_CURVE ( 'NONE', #18724, #108178, #53056, .T. ) ;
#230953 = CARTESIAN_POINT ( 'NONE',  ( -16.80070461187849773, 66.05000000001224691, -149.1700713136813761 ) ) ;
#230954 = VERTEX_POINT ( 'NONE', #2704 ) ;
#230956 = FACE_OUTER_BOUND ( 'NONE', #23752, .T. ) ;
#230955 = CARTESIAN_POINT ( 'NONE',  ( -5.899999999999938183, 64.65000000001120384, -22.12310748452479103 ) ) ;
#230957 = ORIENTED_EDGE ( 'NONE', *, *, #241553, .T. ) ;
#230959 = ORIENTED_EDGE ( 'NONE', *, *, #194805, .F. ) ;
#230958 = CARTESIAN_POINT ( 'NONE',  ( -20.94999999999999929, -11.48912529306490349, -36.50000000000000711 ) ) ;
#230960 = VERTEX_POINT ( 'NONE', #139638 ) ;
#230961 = CARTESIAN_POINT ( 'NONE',  ( -23.25000000000000000, 74.93036000061670165, -233.6816308724374949 ) ) ;
#230962 = ADVANCED_FACE ( 'NONE', ( #58811 ), #219187, .T. ) ;
#230963 = DIRECTION ( 'NONE',  ( 0.000000000000000000, -1.000000000000000000, 0.000000000000000000 ) ) ;
#230964 = CARTESIAN_POINT ( 'NONE',  ( 18.49999999999999289, 65.65621891165865520, -78.19466220664698142 ) ) ;
#230965 = DIRECTION ( 'NONE',  ( -1.000000000000000000, 9.012599976028471648E-15, 6.882867235861662930E-14 ) ) ;
#230966 = ORIENTED_EDGE ( 'NONE', *, *, #225080, .T. ) ;
#230967 = DIRECTION ( 'NONE',  ( -1.000000000000000000, 2.849773892568378313E-16, -7.728835255496647986E-17 ) ) ;
#230969 = FACE_OUTER_BOUND ( 'NONE', #78921, .T. ) ;
#230968 = VECTOR ( 'NONE', #135930, 1000.000000000000000 ) ;
#230970 = ORIENTED_EDGE ( 'NONE', *, *, #105792, .T. ) ;
#230972 = ADVANCED_FACE ( 'NONE', ( #215341 ), #195814, .T. ) ;
#230971 = DIRECTION ( 'NONE',  ( -2.827886303505248766E-16, 0.8660254037844411501, 0.4999999999999956146 ) ) ;
#230973 = DIRECTION ( 'NONE',  ( 0.000000000000000000, 0.000000000000000000, -1.000000000000000000 ) ) ;
#230974 = ORIENTED_EDGE ( 'NONE', *, *, #99395, .T. ) ;
#230975 = CARTESIAN_POINT ( 'NONE',  ( -20.54999999999999716, 20.22419170005074918, -254.0771499268472553 ) ) ;
#230976 = CIRCLE ( 'NONE', #218450, 0.09999999999999939493 ) ;
#230977 = AXIS2_PLACEMENT_3D ( 'NONE', #7522, #83173, #242271 ) ;
#230978 = ORIENTED_EDGE ( 'NONE', *, *, #169798, .F. ) ;
#230979 = AXIS2_PLACEMENT_3D ( 'NONE', #184080, #101946, #244044 ) ;
#230980 = DIRECTION ( 'NONE',  ( -0.000000000000000000, 1.000000000000000000, -0.000000000000000000 ) ) ;
#230981 = ORIENTED_EDGE ( 'NONE', *, *, #41916, .F. ) ;
#230982 = DIRECTION ( 'NONE',  ( -4.701977403289178058E-30, -2.433019743745433765E-14, 1.000000000000000000 ) ) ;
#230983 = CARTESIAN_POINT ( 'NONE',  ( 20.94999999999999929, 5.850000000011160495, -56.86750277572208034 ) ) ;
#230984 = CARTESIAN_POINT ( 'NONE',  ( -23.25000000000000000, 76.00000000001165290, -69.52310748452431710 ) ) ;
#230985 = DIRECTION ( 'NONE',  ( 1.000000000000000000, 0.000000000000000000, 0.000000000000000000 ) ) ;
#230986 = CARTESIAN_POINT ( 'NONE',  ( -23.25000000000000000, 87.75000000001236344, -166.9231074845242802 ) ) ;
#230987 = CARTESIAN_POINT ( 'NONE',  ( 18.31572054635736890, -9.548475435767633357, -73.85057016474850400 ) ) ;
#230988 = LINE ( 'NONE', #234819, #22643 ) ;
#230989 = ORIENTED_EDGE ( 'NONE', *, *, #229300, .F. ) ;
#230990 = CIRCLE ( 'NONE', #52062, 11.90000000000001457 ) ;
#230991 = CARTESIAN_POINT ( 'NONE',  ( -21.05000000000000071, 0.3882413827466408840, -209.1776850584169551 ) ) ;
#230992 = VERTEX_POINT ( 'NONE', #39304 ) ;
#230995 = VERTEX_POINT ( 'NONE', #156694 ) ;
#230994 = FACE_OUTER_BOUND ( 'NONE', #159244, .T. ) ;
#230993 = LINE ( 'NONE', #191877, #207208 ) ;
#230996 = EDGE_CURVE ( 'NONE', #46648, #164969, #176248, .T. ) ;
#230997 = EDGE_LOOP ( 'NONE', ( #13574, #43631, #71277, #251938 ) ) ;
#230998 = CARTESIAN_POINT ( 'NONE',  ( -21.44999999999999929, 7.350000000011155166, -54.75000000000000000 ) ) ;
#230999 = DIRECTION ( 'NONE',  ( -1.000000000000000000, 6.938893903907270030E-14, 0.000000000000000000 ) ) ;
#231000 = DIRECTION ( 'NONE',  ( -1.000000000000000000, 0.000000000000000000, 0.000000000000000000 ) ) ;
#231001 = DIRECTION ( 'NONE',  ( 0.000000000000000000, 0.8814952561688437216, -0.4721928772777334582 ) ) ;
#231002 = CIRCLE ( 'NONE', #126924, 0.1999999999999996503 ) ;
#231003 = ORIENTED_EDGE ( 'NONE', *, *, #133144, .T. ) ;
#231005 = VERTEX_POINT ( 'NONE', #56256 ) ;
#231004 = DIRECTION ( 'NONE',  ( -1.000000000000000000, 0.000000000000000000, 0.000000000000000000 ) ) ;
#231006 = ADVANCED_FACE ( 'NONE', ( #77119 ), #157989, .F. ) ;
#231007 = ADVANCED_FACE ( 'NONE', ( #19731 ), #140963, .F. ) ;
#231009 = CARTESIAN_POINT ( 'NONE',  ( 18.52928932304151033, 15.29497926255971230, -222.9236147070920424 ) ) ;
#231008 = PLANE ( 'NONE',  #92831 ) ;
#231011 = ORIENTED_EDGE ( 'NONE', *, *, #15570, .F. ) ;
#231010 = DIRECTION ( 'NONE',  ( 0.000000000000000000, -0.6728971962617388280, -0.7397360091702248619 ) ) ;
#231012 = EDGE_CURVE ( 'NONE', #91289, #66229, #21027, .T. ) ;
#231013 = EDGE_CURVE ( 'NONE', #245971, #223079, #202901, .T. ) ;
#231014 = ORIENTED_EDGE ( 'NONE', *, *, #80736, .F. ) ;
#231015 = ADVANCED_FACE ( 'NONE', ( #80952 ), #41872, .T. ) ;
#231016 = EDGE_CURVE ( 'NONE', #29625, #34439, #109481, .T. ) ;
#231017 = FACE_OUTER_BOUND ( 'NONE', #257697, .T. ) ;
#231018 = AXIS2_PLACEMENT_3D ( 'NONE', #54245, #215873, #196326 ) ;
#231019 = AXIS2_PLACEMENT_3D ( 'NONE', #111345, #112628, #94330 ) ;
#231020 = LINE ( 'NONE', #32838, #159597 ) ;
#231021 = ORIENTED_EDGE ( 'NONE', *, *, #21237, .F. ) ;
#231022 = CYLINDRICAL_SURFACE ( 'NONE', #35251, 0.1000000000000028644 ) ;
#231023 = ORIENTED_EDGE ( 'NONE', *, *, #232517, .T. ) ;
#231024 = ADVANCED_FACE ( 'NONE', ( #142224 ), #223045, .F. ) ;
#231025 = CARTESIAN_POINT ( 'NONE',  ( 22.39999999999999503, -0.1008583690875579364, -122.2504328765106294 ) ) ;
#231026 = CARTESIAN_POINT ( 'NONE',  ( 18.49999999999999289, 6.450000000011156587, -88.75000000000004263 ) ) ;
#231027 = ORIENTED_EDGE ( 'NONE', *, *, #163950, .F. ) ;
#231028 = CARTESIAN_POINT ( 'NONE',  ( 21.14999999999999858, 11.65000000000000391, -12.15000000000000036 ) ) ;
#231029 = AXIS2_PLACEMENT_3D ( 'NONE', #197971, #14236, #64877 ) ;
#231030 = CARTESIAN_POINT ( 'NONE',  ( 23.15000000000000213, 87.48912529308822172, -139.5231074845243029 ) ) ;
#231031 = CIRCLE ( 'NONE', #160310, 0.09999999999999990841 ) ;
#231032 = VECTOR ( 'NONE', #143250, 1000.000000000000000 ) ;
#231033 = CIRCLE ( 'NONE', #131048, 0.09999999999999939493 ) ;
#231034 = EDGE_CURVE ( 'NONE', #52458, #199951, #185210, .T. ) ;
#231035 = EDGE_LOOP ( 'NONE', ( #74882, #85065 ) ) ;
#231036 = ORIENTED_EDGE ( 'NONE', *, *, #166911, .F. ) ;
#231037 = CARTESIAN_POINT ( 'NONE',  ( 20.84451136049273146, 18.74944765725850004, -227.9096743945612502 ) ) ;
#231038 = EDGE_LOOP ( 'NONE', ( #17923, #79947, #55207, #221516 ) ) ;
#231039 = DIRECTION ( 'NONE',  ( -0.000000000000000000, 6.982962677686266711E-15, -1.000000000000000000 ) ) ;
#231040 = ORIENTED_EDGE ( 'NONE', *, *, #173474, .T. ) ;
#231042 = VERTEX_POINT ( 'NONE', #221738 ) ;
#231041 = CARTESIAN_POINT ( 'NONE',  ( -22.39999999999999858, 11.75000000001115552, -167.3999999999999773 ) ) ;
#231043 = ADVANCED_FACE ( 'NONE', ( #187794 ), #228039, .T. ) ;
#231044 = EDGE_CURVE ( 'NONE', #57517, #1482, #48264, .T. ) ;
#231045 = ORIENTED_EDGE ( 'NONE', *, *, #246271, .T. ) ;
#231046 = CARTESIAN_POINT ( 'NONE',  ( 18.59999999999999076, 64.25000000001232081, -161.9231074845244223 ) ) ;
#231047 = VERTEX_POINT ( 'NONE', #123966 ) ;
#231050 = EDGE_LOOP ( 'NONE', ( #37040, #200869, #110536, #129197 ) ) ;
#231049 = ORIENTED_EDGE ( 'NONE', *, *, #33173, .T. ) ;
#231048 = FACE_OUTER_BOUND ( 'NONE', #231058, .T. ) ;
#231051 = DIRECTION ( 'NONE',  ( 1.000000000000000000, 0.000000000000000000, 0.000000000000000000 ) ) ;
#231052 = EDGE_LOOP ( 'NONE', ( #240840, #196648, #13007, #83764 ) ) ;
#231053 = VECTOR ( 'NONE', #55623, 1000.000000000000000 ) ;
#231054 = AXIS2_PLACEMENT_3D ( 'NONE', #12952, #93743, #170770 ) ;
#231055 = VECTOR ( 'NONE', #74584, 999.9999999999998863 ) ;
#231056 = LINE ( 'NONE', #73278, #63402 ) ;
#231057 = VECTOR ( 'NONE', #96497, 1000.000000000000000 ) ;
#231058 = EDGE_LOOP ( 'NONE', ( #71624, #257004, #53291, #252586 ) ) ;
#231059 = DIRECTION ( 'NONE',  ( -0.000000000000000000, 0.000000000000000000, 1.000000000000000000 ) ) ;
#231061 = ORIENTED_EDGE ( 'NONE', *, *, #237450, .T. ) ;
#231060 = DIRECTION ( 'NONE',  ( -1.836970198721029934E-16, -1.000000000000000000, -6.982962677686266711E-15 ) ) ;
#231062 = CARTESIAN_POINT ( 'NONE',  ( -20.64999999999999858, 68.75000000001230660, -157.6731074845243938 ) ) ;
#231063 = VERTEX_POINT ( 'NONE', #23610 ) ;
#231064 = CARTESIAN_POINT ( 'NONE',  ( -17.11825945287482753, 10.05000000001113847, -46.15000000000000568 ) ) ;
#231065 = CARTESIAN_POINT ( 'NONE',  ( 23.14999999999999503, 69.55000000001277272, -215.2731074845244166 ) ) ;
#231066 = VECTOR ( 'NONE', #168766, 1000.000000000000000 ) ;
#231067 = ORIENTED_EDGE ( 'NONE', *, *, #147739, .F. ) ;
#231068 = CIRCLE ( 'NONE', #6169, 0.1000000000000028644 ) ;
#231069 = FACE_OUTER_BOUND ( 'NONE', #44379, .T. ) ;
#231070 = DIRECTION ( 'NONE',  ( 0.000000000000000000, 1.000000000000000000, 0.000000000000000000 ) ) ;
#231071 = VERTEX_POINT ( 'NONE', #28756 ) ;
#231073 = ORIENTED_EDGE ( 'NONE', *, *, #82380, .F. ) ;
#231072 = DIRECTION ( 'NONE',  ( 1.000000000000000000, 0.000000000000000000, 0.000000000000000000 ) ) ;
#231074 = AXIS2_PLACEMENT_3D ( 'NONE', #182735, #242679, #180164 ) ;
#231077 = ORIENTED_EDGE ( 'NONE', *, *, #225652, .F. ) ;
#231076 = ORIENTED_EDGE ( 'NONE', *, *, #123192, .T. ) ;
#231075 = AXIS2_PLACEMENT_3D ( 'NONE', #218477, #174297, #236768 ) ;
#231078 = VERTEX_POINT ( 'NONE', #242601 ) ;
#231079 = DIRECTION ( 'NONE',  ( 0.000000000000000000, 0.000000000000000000, 1.000000000000000000 ) ) ;
#231080 = ORIENTED_EDGE ( 'NONE', *, *, #224447, .F. ) ;
#231081 = AXIS2_PLACEMENT_3D ( 'NONE', #51586, #15075, #112884 ) ;
#231082 = VERTEX_POINT ( 'NONE', #45694 ) ;
#231083 = PLANE ( 'NONE',  #67499 ) ;
#231084 = VERTEX_POINT ( 'NONE', #203493 ) ;
#231085 = CARTESIAN_POINT ( 'NONE',  ( 23.14999999999999858, 38.50047664313251516, -246.1133312021848951 ) ) ;
#231086 = CIRCLE ( 'NONE', #22981, 0.09999999999999939493 ) ;
#231087 = CIRCLE ( 'NONE', #2085, 0.1000000000000028644 ) ;
#231088 = DIRECTION ( 'NONE',  ( 1.000000000000000000, 0.000000000000000000, 0.000000000000000000 ) ) ;
#231089 = ORIENTED_EDGE ( 'NONE', *, *, #123296, .F. ) ;
#231090 = ADVANCED_FACE ( 'NONE', ( #83506 ), #202212, .T. ) ;
#231091 = ORIENTED_EDGE ( 'NONE', *, *, #191285, .F. ) ;
#231092 = DIRECTION ( 'NONE',  ( 1.000000000000000000, 0.000000000000000000, 0.000000000000000000 ) ) ;
#231093 = EDGE_CURVE ( 'NONE', #41838, #5246, #190023, .T. ) ;
#231094 = EDGE_LOOP ( 'NONE', ( #177673, #115205, #197366, #6685 ) ) ;
#231095 = ADVANCED_FACE ( 'NONE', ( #82218 ), #219648, .T. ) ;
#231096 = DIRECTION ( 'NONE',  ( -1.000000000000000000, 2.952720810173289112E-16, 2.061873921506763405E-30 ) ) ;
#231097 = ADVANCED_FACE ( 'NONE', ( #146070 ), #5255, .T. ) ;
#231098 = ORIENTED_EDGE ( 'NONE', *, *, #257625, .T. ) ;
#231099 = DIRECTION ( 'NONE',  ( 1.000000000000000000, -0.000000000000000000, -0.000000000000000000 ) ) ;
#231101 = EDGE_LOOP ( 'NONE', ( #212107, #100833, #139641, #50729 ) ) ;
#231100 = CARTESIAN_POINT ( 'NONE',  ( -16.97048361161166952, 9.950000000011135270, -120.8588843444304217 ) ) ;
#231102 = CARTESIAN_POINT ( 'NONE',  ( -18.59999999999999787, -1.835341550213255957, -78.55515129256302487 ) ) ;
#231103 = DIRECTION ( 'NONE',  ( 0.000000000000000000, 0.000000000000000000, -1.000000000000000000 ) ) ;
#231104 = DIRECTION ( 'NONE',  ( 0.000000000000000000, 0.1335171055202901413, 0.9910465087640860649 ) ) ;
#231105 = CARTESIAN_POINT ( 'NONE',  ( 18.49999999999999289, 33.89924982463041658, -236.3385223663007366 ) ) ;
#231106 = CYLINDRICAL_SURFACE ( 'NONE', #165147, 0.1000000000000028644 ) ;
#231107 = CARTESIAN_POINT ( 'NONE',  ( -16.87487986503753845, 66.04999244492670130, -157.3731327448377044 ) ) ;
#231108 = AXIS2_PLACEMENT_3D ( 'NONE', #188931, #89811, #168130 ) ;
#231109 = CARTESIAN_POINT ( 'NONE',  ( -5.900000000000003020, -11.25000000000000000, 10.10000000000000142 ) ) ;
#231110 = DIRECTION ( 'NONE',  ( 0.000000000000000000, 0.000000000000000000, -1.000000000000000000 ) ) ;
#231111 = CARTESIAN_POINT ( 'NONE',  ( 18.43466021071393612, 38.00874357722931762, -261.0447760932440815 ) ) ;
#231112 = VECTOR ( 'NONE', #38902, 1000.000000000000000 ) ;
#231113 = DIRECTION ( 'NONE',  ( -0.000000000000000000, -0.000000000000000000, -1.000000000000000000 ) ) ;
#231114 = AXIS2_PLACEMENT_3D ( 'NONE', #257504, #142739, #42374 ) ;
#231115 = ORIENTED_EDGE ( 'NONE', *, *, #14804, .F. ) ;
#231116 = EDGE_CURVE ( 'NONE', #243045, #104543, #46961, .T. ) ;
#231117 = EDGE_CURVE ( 'NONE', #246766, #100635, #57137, .T. ) ;
#231118 = AXIS2_PLACEMENT_3D ( 'NONE', #156936, #99474, #180329 ) ;
#231120 = VERTEX_POINT ( 'NONE', #166970 ) ;
#231119 = EDGE_LOOP ( 'NONE', ( #116744, #87813, #18410, #163284 ) ) ;
#231121 = AXIS2_PLACEMENT_3D ( 'NONE', #238828, #198412, #58874 ) ;
#231122 = ORIENTED_EDGE ( 'NONE', *, *, #223318, .T. ) ;
#231123 = CARTESIAN_POINT ( 'NONE',  ( -18.59999999999999787, -1.162701749926853712, -175.4999999999999716 ) ) ;
#231124 = DIRECTION ( 'NONE',  ( -2.252264143451593525E-15, 0.8127272543710891695, -0.5826443254700338636 ) ) ;
#231126 = CARTESIAN_POINT ( 'NONE',  ( 21.07946286933444213, 1.586026531860189381, -230.6765785263235955 ) ) ;
#231125 = DIRECTION ( 'NONE',  ( 0.000000000000000000, 0.000000000000000000, 1.000000000000000000 ) ) ;
#231127 = ORIENTED_EDGE ( 'NONE', *, *, #149382, .F. ) ;
#231129 = VERTEX_POINT ( 'NONE', #144776 ) ;
#231128 = TOROIDAL_SURFACE ( 'NONE', #185317, 12.77500000000000036, 0.1000000000000000056 ) ;
#231130 = FILL_AREA_STYLE ('',( #154186 ) ) ;
#231131 = ADVANCED_FACE ( 'NONE', ( #246464 ), #161824, .T. ) ;
#231132 = DIRECTION ( 'NONE',  ( -1.000000000000000000, 0.000000000000000000, -0.000000000000000000 ) ) ;
#231133 = VECTOR ( 'NONE', #147295, 1000.000000000000000 ) ;
#231134 = CYLINDRICAL_SURFACE ( 'NONE', #134754, 0.09999999999999939493 ) ;
#231135 = ADVANCED_FACE ( 'NONE', ( #209925, #233350 ), #192919, .T. ) ;
#231136 = CARTESIAN_POINT ( 'NONE',  ( -16.94107738177414291, 65.98576071487592287, -182.5731074845244279 ) ) ;
#231137 = ORIENTED_EDGE ( 'NONE', *, *, #100327, .F. ) ;
#231138 = EDGE_LOOP ( 'NONE', ( #216016, #22073, #219845, #68237 ) ) ;
#231139 = DIRECTION ( 'NONE',  ( -1.000000000000000000, 1.207181226542539700E-16, -2.694675058168174199E-16 ) ) ;
#231140 = DIRECTION ( 'NONE',  ( 1.000000000000000000, 0.000000000000000000, 0.000000000000000000 ) ) ;
#231142 = EDGE_LOOP ( 'NONE', ( #2702, #100416, #27002, #208260 ) ) ;
#231141 = DIRECTION ( 'NONE',  ( -1.000000000000000000, 0.000000000000000000, 0.000000000000000000 ) ) ;
#231143 = VECTOR ( 'NONE', #12322, 1000.000000000000000 ) ;
#231144 = LINE ( 'NONE', #192016, #2853 ) ;
#231145 = EDGE_CURVE ( 'NONE', #253373, #69524, #232152, .T. ) ;
#231146 = FACE_OUTER_BOUND ( 'NONE', #184887, .T. ) ;
#231147 = DIRECTION ( 'NONE',  ( 0.000000000000000000, 0.2617529984165039569, 0.9651348961777155289 ) ) ;
#231148 = DIRECTION ( 'NONE',  ( 0.000000000000000000, -0.9126074666063545004, -0.4088369013363783999 ) ) ;
#231149 = EDGE_LOOP ( 'NONE', ( #14012, #225735, #254697, #226996 ) ) ;
#231150 = DIRECTION ( 'NONE',  ( 1.000000000000000000, 0.000000000000000000, 0.000000000000000000 ) ) ;
#231151 = CARTESIAN_POINT ( 'NONE',  ( -20.85000000000000142, 76.00000000001185185, -95.12310748452429721 ) ) ;
#231152 = ADVANCED_FACE ( 'NONE', ( #170836 ), #194744, .T. ) ;
#231153 = DIRECTION ( 'NONE',  ( 0.000000000000000000, 6.982962677686266711E-15, -1.000000000000000000 ) ) ;
#231155 = CYLINDRICAL_SURFACE ( 'NONE', #178540, 0.09999999999999939493 ) ;
#231154 = CARTESIAN_POINT ( 'NONE',  ( 18.49999999999999289, 1.591682202823531123, -219.1856213577225105 ) ) ;
#231156 = CARTESIAN_POINT ( 'NONE',  ( -18.69999999999999929, -11.75000000000000000, 29.89999999999999858 ) ) ;
#231157 = FACE_OUTER_BOUND ( 'NONE', #70935, .T. ) ;
#231159 = EDGE_CURVE ( 'NONE', #6293, #115921, #173920, .T. ) ;
#231158 = DIRECTION ( 'NONE',  ( 0.000000000000000000, 0.000000000000000000, -1.000000000000000000 ) ) ;
#231160 = DIRECTION ( 'NONE',  ( 1.000000000000000000, 0.000000000000000000, 0.000000000000000000 ) ) ;
#231161 = DIRECTION ( 'NONE',  ( 0.000000000000000000, 0.4930308989874980785, 0.8700118002898462599 ) ) ;
#231163 = ORIENTED_EDGE ( 'NONE', *, *, #144790, .T. ) ;
#231162 = AXIS2_PLACEMENT_3D ( 'NONE', #103715, #4627, #159891 ) ;
#231164 = AXIS2_PLACEMENT_3D ( 'NONE', #134357, #17016, #54823 ) ;
#231165 = ORIENTED_EDGE ( 'NONE', *, *, #186700, .F. ) ;
#231166 = ORIENTED_EDGE ( 'NONE', *, *, #110661, .T. ) ;
#231167 = CARTESIAN_POINT ( 'NONE',  ( 20.51284917709620359, 65.68911337716723153, -95.35063429893224907 ) ) ;
#231168 = CARTESIAN_POINT ( 'NONE',  ( 20.94999999999999929, 4.999999999999997335, -21.49473398108690603 ) ) ;
#231169 = VERTEX_POINT ( 'NONE', #73001 ) ;
#231170 = ADVANCED_FACE ( 'NONE', ( #247749 ), #144633, .T. ) ;
#231171 = CARTESIAN_POINT ( 'NONE',  ( -23.25000000000000000, 77.25000000001165290, -61.72262673010922640 ) ) ;
#231172 = VERTEX_POINT ( 'NONE', #31309 ) ;
#231173 = ADVANCED_FACE ( 'NONE', ( #229480 ), #215555, .F. ) ;
#231174 = SURFACE_STYLE_USAGE ( .BOTH. , #34265 ) ;
#231175 = EDGE_LOOP ( 'NONE', ( #130300, #135459, #66358, #67115 ) ) ;
#231176 = CARTESIAN_POINT ( 'NONE',  ( -23.15000000000000213, -8.596261682231830292, -57.54987248284972878 ) ) ;
#231177 = AXIS2_PLACEMENT_3D ( 'NONE', #237839, #155767, #158340 ) ;
#231178 = ORIENTED_EDGE ( 'NONE', *, *, #96188, .T. ) ;
#231179 = LINE ( 'NONE', #10827, #68073 ) ;
#231180 = CARTESIAN_POINT ( 'NONE',  ( -16.81931177881023132, 30.13250511629065542, -234.7822519458397039 ) ) ;
#231181 = DIRECTION ( 'NONE',  ( 0.000000000000000000, -2.211772431870365684E-13, -1.000000000000000000 ) ) ;
#231182 = AXIS2_PLACEMENT_3D ( 'NONE', #94905, #253977, #191487 ) ;
#231183 = CARTESIAN_POINT ( 'NONE',  ( 18.49999999999999645, 77.83585931145600512, -158.5186683157258187 ) ) ;
#231184 = DIRECTION ( 'NONE',  ( 0.000000000000000000, -0.8127272543710951647, 0.5826443254700257590 ) ) ;
#231186 = ORIENTED_EDGE ( 'NONE', *, *, #90950, .T. ) ;
#231185 = DIRECTION ( 'NONE',  ( 2.557131231893037478E-16, 0.8660254037844420383, -0.4999999999999942824 ) ) ;
#231187 = DIRECTION ( 'NONE',  ( 0.000000000000000000, 0.000000000000000000, -1.000000000000000000 ) ) ;
#231188 = CARTESIAN_POINT ( 'NONE',  ( -22.10000000000000142, -11.64999999999999858, 11.99999999999999645 ) ) ;
#231189 = FACE_OUTER_BOUND ( 'NONE', #182888, .T. ) ;
#231190 = DIRECTION ( 'NONE',  ( 0.000000000000000000, 0.2128009952263485993, -0.9770955615653341697 ) ) ;
#231191 = CARTESIAN_POINT ( 'NONE',  ( -20.54999999999999716, 73.60000000001180354, -82.74772940728642823 ) ) ;
#231192 = ORIENTED_EDGE ( 'NONE', *, *, #92786, .T. ) ;
#231193 = SURFACE_STYLE_FILL_AREA ( #250724 ) ;
#231194 = DIRECTION ( 'NONE',  ( -0.000000000000000000, 0.4088369013363281068, -0.9126074666063770380 ) ) ;
#231195 = CYLINDRICAL_SURFACE ( 'NONE', #169579, 0.1000000000000055844 ) ;
#231196 = ORIENTED_EDGE ( 'NONE', *, *, #151246, .F. ) ;
#231197 = VECTOR ( 'NONE', #68753, 1000.000000000000000 ) ;
#231199 = PLANE ( 'NONE',  #30517 ) ;
#231198 = CIRCLE ( 'NONE', #6307, 0.09999999999999609201 ) ;
#231200 = CARTESIAN_POINT ( 'NONE',  ( -20.85000000000000142, 31.15787740146373253, -259.8205824356103903 ) ) ;
#231201 = LINE ( 'NONE', #210343, #224132 ) ;
#231202 = EDGE_LOOP ( 'NONE', ( #106629, #29998, #180600, #173140 ) ) ;
#231203 = EDGE_LOOP ( 'NONE', ( #171712, #102199, #48104, #176814 ) ) ;
#231204 = CARTESIAN_POINT ( 'NONE',  ( -22.39999999999999858, 11.65000000001115588, -67.00000000000004263 ) ) ;
#231205 = CARTESIAN_POINT ( 'NONE',  ( -21.52071067811865746, 65.28546217739872759, -213.3097576571499872 ) ) ;
#231206 = CARTESIAN_POINT ( 'NONE',  ( -16.87036670365549895, 66.01058118071020431, -90.50266760182644532 ) ) ;
#231207 = EDGE_CURVE ( 'NONE', #250275, #256624, #140535, .T. ) ;
#231210 = CARTESIAN_POINT ( 'NONE',  ( -23.15000000000000213, 85.60000000001252829, -179.9170766071767389 ) ) ;
#231209 = AXIS2_PLACEMENT_3D ( 'NONE', #204077, #221069, #198943 ) ;
#231208 = DIRECTION ( 'NONE',  ( -1.000000000000000000, 0.000000000000000000, 0.000000000000000000 ) ) ;
#231211 = CARTESIAN_POINT ( 'NONE',  ( -21.29999999999995808, 1.115600667400684642E-11, -100.5000000000000284 ) ) ;
#231212 = CIRCLE ( 'NONE', #27225, 4.049999999999994493 ) ;
#231213 = CARTESIAN_POINT ( 'NONE',  ( 15.74999999999998934, 9.350000000011137402, -50.36574316727390510 ) ) ;
#231214 = CARTESIAN_POINT ( 'NONE',  ( 20.27550659511089037, 9.216043722520002035, -154.8500000000000227 ) ) ;
#231216 = VERTEX_POINT ( 'NONE', #69137 ) ;
#231215 = AXIS2_PLACEMENT_3D ( 'NONE', #119556, #199077, #99942 ) ;
#231217 = DIRECTION ( 'NONE',  ( 7.589415207398576792E-15, 1.000000000000000000, 6.982962677686266711E-15 ) ) ;
#231218 = AXIS2_PLACEMENT_3D ( 'NONE', #69635, #172626, #212980 ) ;
#231220 = EDGE_LOOP ( 'NONE', ( #15493, #73570, #125983, #119421 ) ) ;
#231219 = DIRECTION ( 'NONE',  ( 1.000000000000000000, 0.000000000000000000, 0.000000000000000000 ) ) ;
#231221 = DIRECTION ( 'NONE',  ( 0.7071067811865474617, 0.7071067811865474617, 0.000000000000000000 ) ) ;
#231223 = CARTESIAN_POINT ( 'NONE',  ( -18.47140463609786920, -0.9011515821983938634, -242.3107253779298844 ) ) ;
#231222 = CARTESIAN_POINT ( 'NONE',  ( 23.15000000000000213, 85.00000000001232081, -160.1291383618718385 ) ) ;
#231224 = CARTESIAN_POINT ( 'NONE',  ( -16.89155683852404621, 66.05000000001207638, -123.2457356349840722 ) ) ;
#231225 = ADVANCED_FACE ( 'NONE', ( #148665 ), #153838, .F. ) ;
#231226 = CARTESIAN_POINT ( 'NONE',  ( 20.94999999999999929, 11.65000000001115943, -194.2161343370218560 ) ) ;
#231228 = EDGE_LOOP ( 'NONE', ( #208489, #131770, #159728 ) ) ;
#231227 = CARTESIAN_POINT ( 'NONE',  ( -23.15000000000000213, 11.75000000001115552, -155.7499999999999716 ) ) ;
#231229 = CYLINDRICAL_SURFACE ( 'NONE', #17561, 0.1000000000000028644 ) ;
#231230 = DIRECTION ( 'NONE',  ( 0.000000000000000000, 0.000000000000000000, -1.000000000000000000 ) ) ;
#231231 = CARTESIAN_POINT ( 'NONE',  ( -21.14999999999999858, 76.00000000001267608, -203.5231074845243597 ) ) ;
#231232 = CARTESIAN_POINT ( 'NONE',  ( -21.05000000000000071, 10.91926294161908295, -235.7631306847335395 ) ) ;
#231233 = ORIENTED_EDGE ( 'NONE', *, *, #144352, .F. ) ;
#231234 = DIRECTION ( 'NONE',  ( 1.186688945009010077E-16, -1.000000000000000000, -0.000000000000000000 ) ) ;
#231235 = ADVANCED_FACE ( 'NONE', ( #211190 ), #228197, .F. ) ;
#231237 = EDGE_CURVE ( 'NONE', #119326, #109890, #132178, .T. ) ;
#231236 = ORIENTED_EDGE ( 'NONE', *, *, #114734, .T. ) ;
#231238 = DIRECTION ( 'NONE',  ( 1.000000000000000000, 0.000000000000000000, 0.000000000000000000 ) ) ;
#231239 = VERTEX_POINT ( 'NONE', #50806 ) ;
#231240 = DIRECTION ( 'NONE',  ( 1.000000000000000000, 0.000000000000000000, 0.000000000000000000 ) ) ;
#231241 = VECTOR ( 'NONE', #124863, 1000.000000000000000 ) ;
#231242 = ORIENTED_EDGE ( 'NONE', *, *, #123918, .T. ) ;
#231243 = CARTESIAN_POINT ( 'NONE',  ( 18.59999999999999076, 53.37395138337728895, -234.8857996415767104 ) ) ;
#231245 = DIRECTION ( 'NONE',  ( 0.000000000000000000, 1.000000000000000000, -0.000000000000000000 ) ) ;
#231244 = CIRCLE ( 'NONE', #210386, 0.5000000000000004441 ) ;
#231246 = EDGE_CURVE ( 'NONE', #4508, #141594, #157144, .T. ) ;
#231247 = DIRECTION ( 'NONE',  ( 1.000000000000000000, -7.304098846218134667E-16, 0.000000000000000000 ) ) ;
#231248 = ORIENTED_EDGE ( 'NONE', *, *, #231462, .T. ) ;
#231249 = VECTOR ( 'NONE', #194719, 1000.000000000000000 ) ;
#231250 = CIRCLE ( 'NONE', #14779, 0.09999999999998898659 ) ;
#231252 = CARTESIAN_POINT ( 'NONE',  ( -16.77180007708460963, 9.949999999999983302, -12.63561411895481790 ) ) ;
#231251 = VECTOR ( 'NONE', #7163, 1000.000000000000000 ) ;
#231253 = CARTESIAN_POINT ( 'NONE',  ( -16.81744102076749314, 66.05000000001207638, -123.8731074845243683 ) ) ;
#231254 = CARTESIAN_POINT ( 'NONE',  ( -20.00857864376270001, 66.65000000001222702, -148.7731074845244166 ) ) ;
#231255 = CARTESIAN_POINT ( 'NONE',  ( 22.47071067811865319, 7.522163794833003791, -199.2603376134759117 ) ) ;
#231256 = FACE_OUTER_BOUND ( 'NONE', #203477, .T. ) ;
#231257 = ORIENTED_EDGE ( 'NONE', *, *, #232902, .T. ) ;
#231258 = CARTESIAN_POINT ( 'NONE',  ( -18.54260524012593692, 85.62421939008603999, -129.7823344387537361 ) ) ;
#231259 = VERTEX_POINT ( 'NONE', #168261 ) ;
#231261 = ORIENTED_EDGE ( 'NONE', *, *, #44064, .T. ) ;
#231260 = LINE ( 'NONE', #17338, #64793 ) ;
#231262 = CIRCLE ( 'NONE', #185449, 0.09999999999999939493 ) ;
#231263 = EDGE_LOOP ( 'NONE', ( #57021, #24955, #158733, #138677 ) ) ;
#231264 = FACE_OUTER_BOUND ( 'NONE', #62342, .T. ) ;
#231265 = ADVANCED_FACE ( 'NONE', ( #173402, #53401 ), #35163, .T. ) ;
#231266 = CARTESIAN_POINT ( 'NONE',  ( 23.25000000000000000, 87.48912529308822172, -139.6231074845242688 ) ) ;
#231267 = VECTOR ( 'NONE', #4270, 1000.000000000000000 ) ;
#231268 = LINE ( 'NONE', #69618, #49972 ) ;
#231269 = ORIENTED_EDGE ( 'NONE', *, *, #246644, .F. ) ;
#231270 = VECTOR ( 'NONE', #67343, 1000.000000000000000 ) ;
#231271 = DIRECTION ( 'NONE',  ( 0.000000000000000000, 0.4999999999999956701, -0.8660254037844411501 ) ) ;
#231272 = DIRECTION ( 'NONE',  ( 0.000000000000000000, -0.4031292884907143326, -0.9151430362303863975 ) ) ;
#231273 = AXIS2_PLACEMENT_3D ( 'NONE', #67397, #146915, #126071 ) ;
#231274 = ORIENTED_EDGE ( 'NONE', *, *, #182500, .T. ) ;
#231276 = ORIENTED_EDGE ( 'NONE', *, *, #47224, .T. ) ;
#231275 = CARTESIAN_POINT ( 'NONE',  ( -16.94107738177414291, 65.98576071487538286, -115.5731074845243711 ) ) ;
#231277 = CARTESIAN_POINT ( 'NONE',  ( -23.15000000000000213, 1.115648428625851357E-11, -63.10000000000000142 ) ) ;
#231279 = EDGE_CURVE ( 'NONE', #117495, #210038, #19769, .T. ) ;
#231278 = CARTESIAN_POINT ( 'NONE',  ( 18.49999999999999289, 6.650000000011155876, -54.65000000000000568 ) ) ;
#231280 = ORIENTED_EDGE ( 'NONE', *, *, #38873, .F. ) ;
#231281 = CYLINDRICAL_SURFACE ( 'NONE', #22932, 0.5000000000000004441 ) ;
#231282 = CARTESIAN_POINT ( 'NONE',  ( -20.85000000000000142, 18.41524492703432614, -237.0006385043383546 ) ) ;
#231283 = ORIENTED_EDGE ( 'NONE', *, *, #31925, .T. ) ;
#231284 = CARTESIAN_POINT ( 'NONE',  ( -20.54999999999999716, 82.57900542960499024, -215.5587758314583482 ) ) ;
#231285 = DIRECTION ( 'NONE',  ( 0.000000000000000000, 6.938893903907222067E-15, -1.000000000000000000 ) ) ;
#231286 = DIRECTION ( 'NONE',  ( 0.000000000000000000, -6.517943393102675675E-15, 1.000000000000000000 ) ) ;
#231287 = VECTOR ( 'NONE', #29577, 1000.000000000000000 ) ;
#231288 = EDGE_CURVE ( 'NONE', #12130, #120155, #103118, .T. ) ;
#231289 = TOROIDAL_SURFACE ( 'NONE', #206332, 0.2000000000000000111, 0.1000000000000000056 ) ;
#231290 = CIRCLE ( 'NONE', #35495, 1.749999999999998002 ) ;
#231291 = ORIENTED_EDGE ( 'NONE', *, *, #237414, .T. ) ;
#231292 = CARTESIAN_POINT ( 'NONE',  ( 21.09610168723073187, 0.03358950690264430466, -94.12104428477526596 ) ) ;
#231293 = AXIS2_PLACEMENT_3D ( 'NONE', #80900, #157940, #78340 ) ;
#231294 = ADVANCED_FACE ( 'NONE', ( #38987 ), #95093, .F. ) ;
#231295 = AXIS2_PLACEMENT_3D ( 'NONE', #11801, #54740, #251664 ) ;
#231296 = EDGE_CURVE ( 'NONE', #29044, #38549, #189470, .T. ) ;
#231297 = EDGE_LOOP ( 'NONE', ( #146358, #10383, #73863, #218682 ) ) ;
#231298 = DIRECTION ( 'NONE',  ( 0.000000000000000000, 0.8814952561688476074, -0.4721928772777262417 ) ) ;
#231299 = DIRECTION ( 'NONE',  ( -3.265361837132813093E-16, 1.000000000000000000, 0.000000000000000000 ) ) ;
#231300 = ORIENTED_EDGE ( 'NONE', *, *, #113383, .F. ) ;
#231301 = CARTESIAN_POINT ( 'NONE',  ( -23.25000000000000000, 76.00000000001229239, -157.2481074845243540 ) ) ;
#231302 = CARTESIAN_POINT ( 'NONE',  ( 21.11701782572533048, 65.27839088400411072, -57.27807005501318827 ) ) ;
#231304 = EDGE_CURVE ( 'NONE', #215838, #41810, #240509, .T. ) ;
#231303 = DIRECTION ( 'NONE',  ( 1.000000000000000000, 0.000000000000000000, 0.000000000000000000 ) ) ;
#231307 = EDGE_CURVE ( 'NONE', #68890, #252758, #82255, .T. ) ;
#231306 = CARTESIAN_POINT ( 'NONE',  ( -16.88219499860498374, 22.97755642726332681, -230.9345554886729985 ) ) ;
#231305 = CIRCLE ( 'NONE', #206352, 0.1000000000000028644 ) ;
#231308 = CARTESIAN_POINT ( 'NONE',  ( -20.64999999999999858, 82.20113918088273408, -215.0418453737790401 ) ) ;
#231309 = CIRCLE ( 'NONE', #102079, 0.1000000000000046685 ) ;
#231310 = DIRECTION ( 'NONE',  ( 0.000000000000000000, 1.000000000000000000, 6.982962677686266711E-15 ) ) ;
#231311 = CARTESIAN_POINT ( 'NONE',  ( 21.08376601933332495, 6.341947271286813681, -66.93622398907004367 ) ) ;
#231313 = EDGE_LOOP ( 'NONE', ( #256039, #203785, #209803 ) ) ;
#231312 = CARTESIAN_POINT ( 'NONE',  ( -22.39999999999999858, 76.00000000001203659, -114.6726782920691221 ) ) ;
#231314 = VECTOR ( 'NONE', #104148, 1000.000000000000000 ) ;
#231315 = ADVANCED_FACE ( 'NONE', ( #239745 ), #136416, .T. ) ;
#231316 = EDGE_CURVE ( 'NONE', #125361, #43436, #111335, .T. ) ;
#231318 = EDGE_CURVE ( 'NONE', #191054, #109277, #140734, .T. ) ;
#231317 = ADVANCED_FACE ( 'NONE', ( #235875 ), #107415, .F. ) ;
#231319 = DIRECTION ( 'NONE',  ( 0.000000000000000000, -6.982962677686266711E-15, 1.000000000000000000 ) ) ;
#231320 = FACE_OUTER_BOUND ( 'NONE', #6769, .T. ) ;
#231321 = CIRCLE ( 'NONE', #168988, 12.97499999999999964 ) ;
#231322 = DIRECTION ( 'NONE',  ( 0.000000000000000000, 0.8660254037844377084, 0.5000000000000016653 ) ) ;
#231323 = DIRECTION ( 'NONE',  ( 0.000000000000000000, -0.1335171055202901413, -0.9910465087640860649 ) ) ;
#231324 = ORIENTED_EDGE ( 'NONE', *, *, #154764, .F. ) ;
#231325 = EDGE_CURVE ( 'NONE', #69740, #46643, #41563, .T. ) ;
#231326 = LINE ( 'NONE', #35704, #172768 ) ;
#231327 = ORIENTED_EDGE ( 'NONE', *, *, #81973, .T. ) ;
#231328 = ADVANCED_FACE ( 'NONE', ( #40292 ), #19415, .F. ) ;
#231329 = ADVANCED_FACE ( 'NONE', ( #18122 ), #115789, .T. ) ;
#231330 = VECTOR ( 'NONE', #39012, 1000.000000000000114 ) ;
#231331 = LINE ( 'NONE', #76081, #130951 ) ;
#231332 = CIRCLE ( 'NONE', #6453, 0.1999999999999996503 ) ;
#231333 = CARTESIAN_POINT ( 'NONE',  ( -16.93906926870270624, 10.01214687095770906, -79.55345230722686267 ) ) ;
#231334 = EDGE_CURVE ( 'NONE', #240058, #138829, #86539, .T. ) ;
#231335 = ORIENTED_EDGE ( 'NONE', *, *, #80854, .T. ) ;
#231336 = CARTESIAN_POINT ( 'NONE',  ( 18.49999999999999289, 68.97833521811131163, -32.18954208262707795 ) ) ;
#231337 = ORIENTED_EDGE ( 'NONE', *, *, #41215, .T. ) ;
#231338 = DIRECTION ( 'NONE',  ( 1.000000000000000000, 0.000000000000000000, 0.000000000000000000 ) ) ;
#231340 = ORIENTED_EDGE ( 'NONE', *, *, #213310, .F. ) ;
#231339 = FACE_OUTER_BOUND ( 'NONE', #219603, .T. ) ;
#231341 = ADVANCED_FACE ( 'NONE', ( #217581 ), #238454, .F. ) ;
#231342 = CARTESIAN_POINT ( 'NONE',  ( -22.39999999999999858, 11.65000000001115588, -33.60000000000000142 ) ) ;
#231343 = VERTEX_POINT ( 'NONE', #178510 ) ;
#231344 = CARTESIAN_POINT ( 'NONE',  ( -20.54999999999999716, 68.85000000001205933, -124.2731074845243455 ) ) ;
#231345 = ORIENTED_EDGE ( 'NONE', *, *, #159749, .F. ) ;
#231347 = ORIENTED_EDGE ( 'NONE', *, *, #28897, .T. ) ;
#231346 = ORIENTED_EDGE ( 'NONE', *, *, #212430, .T. ) ;
#231348 = DIRECTION ( 'NONE',  ( -1.000000000000000000, 2.952720810173289112E-16, 2.061873921506763405E-30 ) ) ;
#231350 = EDGE_LOOP ( 'NONE', ( #222005, #127081 ) ) ;
#231349 = CARTESIAN_POINT ( 'NONE',  ( 19.75857864376268935, 16.64998792410002793, -222.7039835543563981 ) ) ;
#231351 = PLANE ( 'NONE',  #148064 ) ;
#231352 = AXIS2_PLACEMENT_3D ( 'NONE', #235259, #57896, #38362 ) ;
#231353 = ORIENTED_EDGE ( 'NONE', *, *, #212074, .F. ) ;
#231354 = CIRCLE ( 'NONE', #239721, 11.70000000000000284 ) ;
#231355 = ORIENTED_EDGE ( 'NONE', *, *, #177783, .F. ) ;
#231356 = CARTESIAN_POINT ( 'NONE',  ( -20.94999999999999929, 74.14897176987101091, -91.36919421510182815 ) ) ;
#231357 = CARTESIAN_POINT ( 'NONE',  ( 18.39999999999997371, 64.25000000001233502, -160.7731074845244450 ) ) ;
#231358 = CARTESIAN_POINT ( 'NONE',  ( -21.65000000000000213, 7.249999999999984013, -20.85000000000000142 ) ) ;
#231359 = ORIENTED_EDGE ( 'NONE', *, *, #141008, .T. ) ;
#231360 = FACE_OUTER_BOUND ( 'NONE', #165936, .T. ) ;
#231361 = CARTESIAN_POINT ( 'NONE',  ( -18.40000000000000213, -9.519327731081286714, -73.97297637655937308 ) ) ;
#231362 = ORIENTED_EDGE ( 'NONE', *, *, #117581, .F. ) ;
#231363 = CARTESIAN_POINT ( 'NONE',  ( -21.05000000000000071, -11.48912529306489994, -164.4000000000000057 ) ) ;
#231364 = DIRECTION ( 'NONE',  ( -1.000000000000000000, 0.000000000000000000, 0.000000000000000000 ) ) ;
#231365 = CARTESIAN_POINT ( 'NONE',  ( 20.94999999999999574, 1.115600667400684642E-11, -134.0000000000000000 ) ) ;
#231367 = ORIENTED_EDGE ( 'NONE', *, *, #137384, .F. ) ;
#231366 = B_SPLINE_CURVE_WITH_KNOTS ( 'NONE', 3,
 ( #160362, #237306, #80767, #22124, #241164, #216441, #58637 ),
 .UNSPECIFIED., .F., .F.,
 ( 4, 3, 4 ),
 ( 0.000000000000000000, 3.357501770814703122E-05, 5.199112466349482939E-05 ),
 .UNSPECIFIED. ) ;
#231368 = CARTESIAN_POINT ( 'NONE',  ( 18.49999999999999289, 62.96704557978079464, -212.5773704035085814 ) ) ;
#231369 = VERTEX_POINT ( 'NONE', #79360 ) ;
#231370 = EDGE_LOOP ( 'NONE', ( #126207, #130552, #30997, #142691 ) ) ;
#231371 = AXIS2_PLACEMENT_3D ( 'NONE', #47574, #145398, #46293 ) ;
#231372 = CARTESIAN_POINT ( 'NONE',  ( -12.84409460144754256, 25.17497023110846399, -232.7237055342689303 ) ) ;
#231373 = DIRECTION ( 'NONE',  ( 0.000000000000000000, -7.109473446599835262E-15, 1.000000000000000000 ) ) ;
#231374 = ORIENTED_EDGE ( 'NONE', *, *, #169386, .T. ) ;
#231375 = ORIENTED_EDGE ( 'NONE', *, *, #30576, .T. ) ;
#231376 = CARTESIAN_POINT ( 'NONE',  ( -16.97683809663752896, 9.950000000011140600, -80.27152476867001951 ) ) ;
#231377 = DIRECTION ( 'NONE',  ( 1.000000000000000000, -0.000000000000000000, -0.000000000000000000 ) ) ;
#231378 = ORIENTED_EDGE ( 'NONE', *, *, #237261, .T. ) ;
#231379 = VERTEX_POINT ( 'NONE', #158946 ) ;
#231380 = DIRECTION ( 'NONE',  ( -7.304098846218201720E-16, 1.000000000000000000, 0.000000000000000000 ) ) ;
#231381 = DIRECTION ( 'NONE',  ( 1.000000000000000000, 1.734723475976817507E-14, 0.000000000000000000 ) ) ;
#231382 = ORIENTED_EDGE ( 'NONE', *, *, #46092, .F. ) ;
#231383 = EDGE_CURVE ( 'NONE', #224589, #135929, #165705, .T. ) ;
#231384 = VECTOR ( 'NONE', #108833, 1000.000000000000000 ) ;
#231385 = EDGE_CURVE ( 'NONE', #239900, #252190, #253150, .T. ) ;
#231386 = EDGE_LOOP ( 'NONE', ( #188936, #176120, #98834, #210187 ) ) ;
#231387 = AXIS2_PLACEMENT_3D ( 'NONE', #227974, #46752, #29811 ) ;
#231388 = CIRCLE ( 'NONE', #102338, 4.000000000000003553 ) ;
#231389 = DIRECTION ( 'NONE',  ( 0.000000000000000000, 0.9915357197604982575, -0.1298341882519033486 ) ) ;
#231390 =( GEOMETRIC_REPRESENTATION_CONTEXT ( 3 ) GLOBAL_UNCERTAINTY_ASSIGNED_CONTEXT ( ( #110345 ) ) GLOBAL_UNIT_ASSIGNED_CONTEXT ( ( #71424, #106652, #68855 ) ) REPRESENTATION_CONTEXT ( 'NONE', 'WORKASPACE' ) );
#231391 = ADVANCED_FACE ( 'NONE', ( #147038 ), #203171, .F. ) ;
#231392 = CARTESIAN_POINT ( 'NONE',  ( -23.15000000000000213, 11.39998237908105416, -245.7725481090871540 ) ) ;
#231393 = ADVANCED_FACE ( 'NONE', ( #62388 ), #141910, .F. ) ;
#231394 = DIRECTION ( 'NONE',  ( -1.000000000000000000, -0.000000000000000000, -0.000000000000000000 ) ) ;
#231396 = ORIENTED_EDGE ( 'NONE', *, *, #110781, .T. ) ;
#231395 = FACE_OUTER_BOUND ( 'NONE', #100404, .T. ) ;
#231397 = CARTESIAN_POINT ( 'NONE',  ( -20.90000000000000213, 8.000000000000000000, 1.212568896937007867 ) ) ;
#231398 = DIRECTION ( 'NONE',  ( 1.000000000000000000, 2.952720810173289112E-16, -0.000000000000000000 ) ) ;
#231399 = CARTESIAN_POINT ( 'NONE',  ( -20.65000000000000568, 7.250000000011138646, -109.7500000000000426 ) ) ;
#231401 = CARTESIAN_POINT ( 'NONE',  ( -17.22767730082754767, 60.21573615951074743, -222.1845923959672291 ) ) ;
#231400 = DIRECTION ( 'NONE',  ( 0.000000000000000000, 7.056502275159890832E-15, -1.000000000000000000 ) ) ;
#231402 = FACE_OUTER_BOUND ( 'NONE', #73984, .T. ) ;
#231403 = CARTESIAN_POINT ( 'NONE',  ( 21.72449340488910252, 65.71604372252045323, -56.87310748452438958 ) ) ;
#231404 = FACE_OUTER_BOUND ( 'NONE', #74257, .T. ) ;
#231405 = DIRECTION ( 'NONE',  ( 0.000000000000000000, 0.000000000000000000, -1.000000000000000000 ) ) ;
#231406 = AXIS2_PLACEMENT_3D ( 'NONE', #212110, #173017, #251203 ) ;
#231407 = EDGE_LOOP ( 'NONE', ( #14556, #218300, #240494, #28791 ) ) ;
#231408 = ADVANCED_FACE ( 'NONE', ( #224011 ), #104049, .T. ) ;
#231410 = EDGE_CURVE ( 'NONE', #148843, #88364, #124933, .T. ) ;
#231409 = AXIS2_PLACEMENT_3D ( 'NONE', #45601, #66447, #26049 ) ;
#231411 = ORIENTED_EDGE ( 'NONE', *, *, #27545, .F. ) ;
#231412 = CIRCLE ( 'NONE', #127343, 0.6000000000000033085 ) ;
#231413 =( BOUNDED_CURVE ( )  B_SPLINE_CURVE ( 3, ( #26449, #85087, #150253, #225885 ),
 .UNSPECIFIED., .F., .F. ) 
 B_SPLINE_CURVE_WITH_KNOTS ( ( 4, 4 ),
 ( 3.752122642744585068, 4.712388980384675463 ),
 .UNSPECIFIED. ) 
 CURVE ( )  GEOMETRIC_REPRESENTATION_ITEM ( )  RATIONAL_B_SPLINE_CURVE ( ( 1.000000000000000000, 0.9246222802177217481, 0.9246222802177217481, 1.000000000000000000 ) ) 
 REPRESENTATION_ITEM ( '' )  );
#231414 = CARTESIAN_POINT ( 'NONE',  ( -20.94999999999994600, 67.65000000001118963, -25.49719488170504533 ) ) ;
#231415 = AXIS2_PLACEMENT_3D ( 'NONE', #65131, #3884, #40486 ) ;
#231416 = AXIS2_PLACEMENT_3D ( 'NONE', #94001, #251802, #73202 ) ;
#231417 = VECTOR ( 'NONE', #34179, 1000.000000000000000 ) ;
#231418 = DIRECTION ( 'NONE',  ( 0.000000000000000000, 0.2617529984165031243, 0.9651348961777157509 ) ) ;
#231419 = VERTEX_POINT ( 'NONE', #46651 ) ;
#231420 =( LENGTH_UNIT ( ) NAMED_UNIT ( * ) SI_UNIT ( .MILLI., .METRE. ) );
#231421 = EDGE_CURVE ( 'NONE', #179081, #45747, #203085, .T. ) ;
#231422 = FACE_OUTER_BOUND ( 'NONE', #103759, .T. ) ;
#231423 = EDGE_CURVE ( 'NONE', #139208, #165690, #24051, .T. ) ;
#231424 = DIRECTION ( 'NONE',  ( 0.000000000000000000, 1.000000000000000000, 0.000000000000000000 ) ) ;
#231425 = VERTEX_POINT ( 'NONE', #3685 ) ;
#231426 = ORIENTED_EDGE ( 'NONE', *, *, #91763, .F. ) ;
#231428 = CARTESIAN_POINT ( 'NONE',  ( 21.05000000000000071, 60.06173988932783203, -221.3217724115915814 ) ) ;
#231427 = AXIS2_PLACEMENT_3D ( 'NONE', #6208, #88293, #226524 ) ;
#231429 = CARTESIAN_POINT ( 'NONE',  ( 23.25000000000000000, 85.60000000001221565, -146.4170766071767389 ) ) ;
#231430 = VERTEX_POINT ( 'NONE', #143189 ) ;
#231432 =( BOUNDED_SURFACE ( )  B_SPLINE_SURFACE ( 3, 2, ( 
 ( #105576, #165605, #66488 ),
 ( #222980, #46901, #202150 ),
 ( #181319, #203437, #122633 ),
 ( #160482, #23551, #140896 ) ),
 .UNSPECIFIED., .F., .F., .F. ) 
 B_SPLINE_SURFACE_WITH_KNOTS ( ( 4, 4 ),
 ( 3, 3 ),
 ( 0.04058434257139475337, 0.04256401539001600232 ),
 ( 0.000000000000000000, 1.000000000000000000 ),
 .UNSPECIFIED. ) 
 GEOMETRIC_REPRESENTATION_ITEM ( )  RATIONAL_B_SPLINE_SURFACE ( (
 ( 1.000000000000000000, 0.7103081912008053500, 1.000000000000000000),
 ( 1.000000000000000000, 0.7104998333555551104, 1.000000000000000000),
 ( 1.000000000000000000, 0.7107238315755428637, 1.000000000000000000),
 ( 1.000000000000000000, 0.7110073749539292942, 1.000000000000000000) ) ) 
 REPRESENTATION_ITEM ( '' )  SURFACE ( )  );
#231431 = CIRCLE ( 'NONE', #94045, 0.2000000000000111688 ) ;
#231433 = DIRECTION ( 'NONE',  ( 1.000000000000000000, 0.000000000000000000, 0.000000000000000000 ) ) ;
#231435 = ORIENTED_EDGE ( 'NONE', *, *, #145341, .F. ) ;
#231434 = DIRECTION ( 'NONE',  ( 1.000000000000000000, 2.952720810173289112E-16, -0.000000000000000000 ) ) ;
#231436 = CARTESIAN_POINT ( 'NONE',  ( 20.73486653747088582, 68.75000000001185185, -93.77310748452435973 ) ) ;
#231437 = VECTOR ( 'NONE', #84892, 1000.000000000000114 ) ;
#231438 = ADVANCED_FACE ( 'NONE', ( #21990 ), #4942, .T. ) ;
#231440 = ORIENTED_EDGE ( 'NONE', *, *, #252133, .F. ) ;
#231439 = DIRECTION ( 'NONE',  ( -1.000000000000000000, 3.265361837132813093E-16, 2.280189983783949500E-30 ) ) ;
#231441 = SPHERICAL_SURFACE ( 'NONE', #70766, 0.1000000000000000056 ) ;
#231442 = CARTESIAN_POINT ( 'NONE',  ( 20.99749315643149927, 64.25000000001219291, -143.5379132532823689 ) ) ;
#231443 = CARTESIAN_POINT ( 'NONE',  ( -23.15000000000000213, 73.50000000001199396, -116.2477294072864140 ) ) ;
#231444 = EDGE_CURVE ( 'NONE', #161481, #252623, #65723, .T. ) ;
#231445 = CARTESIAN_POINT ( 'NONE',  ( -22.49231231312462853, 55.97148680618423100, -232.8646322987703456 ) ) ;
#231447 = CARTESIAN_POINT ( 'NONE',  ( 21.11345278033245165, 8.882122073382985761, -179.7460221707566745 ) ) ;
#231446 = CARTESIAN_POINT ( 'NONE',  ( -23.15000000000000213, 61.54970422893871529, -212.2965875311496688 ) ) ;
#231448 = DIRECTION ( 'NONE',  ( 0.000000000000000000, 0.000000000000000000, 1.000000000000000000 ) ) ;
#231449 = CARTESIAN_POINT ( 'NONE',  ( 18.79999999999999716, 0.000000000000000000, 0.000000000000000000 ) ) ;
#231450 = FACE_OUTER_BOUND ( 'NONE', #89031, .T. ) ;
#231451 = CARTESIAN_POINT ( 'NONE',  ( 21.11825140030058279, 1.450638645453875553, -230.6828758114810967 ) ) ;
#231452 = CARTESIAN_POINT ( 'NONE',  ( -20.94999999999999929, 18.71344899777637494, -226.7788045585494103 ) ) ;
#231453 =( BOUNDED_CURVE ( )  B_SPLINE_CURVE ( 3, ( #205483, #105066, #48983, #45137 ),
 .UNSPECIFIED., .F., .F. ) 
 B_SPLINE_CURVE_WITH_KNOTS ( ( 4, 4 ),
 ( 4.712388980384689674, 6.231880751915386263 ),
 .UNSPECIFIED. ) 
 CURVE ( )  GEOMETRIC_REPRESENTATION_ITEM ( )  RATIONAL_B_SPLINE_CURVE ( ( 1.000000000000000000, 0.8166740347213228279, 0.8166740347213228279, 1.000000000000000000 ) ) 
 REPRESENTATION_ITEM ( '' )  );
#231454 = EDGE_LOOP ( 'NONE', ( #4635, #120954, #78333 ) ) ;
#231455 = EDGE_CURVE ( 'NONE', #128154, #36208, #36715, .T. ) ;
#231456 = FACE_OUTER_BOUND ( 'NONE', #1414, .T. ) ;
#231457 = ORIENTED_EDGE ( 'NONE', *, *, #242061, .T. ) ;
#231458 = CARTESIAN_POINT ( 'NONE',  ( -22.50000000000000000, 11.64999999999997549, -3.469446951953614189E-15 ) ) ;
#231459 = ORIENTED_EDGE ( 'NONE', *, *, #176634, .T. ) ;
#231460 = CARTESIAN_POINT ( 'NONE',  ( -23.15000000000000213, 11.65000000001115588, -45.65000000000000568 ) ) ;
#231461 = CARTESIAN_POINT ( 'NONE',  ( 20.94999999999999574, 14.68288696042412589, -236.3611559727223437 ) ) ;
#231462 = EDGE_CURVE ( 'NONE', #240894, #205206, #128277, .T. ) ;
#231463 = CIRCLE ( 'NONE', #114750, 0.09999999999999939493 ) ;
#231464 = AXIS2_PLACEMENT_3D ( 'NONE', #96914, #60387, #255975 ) ;
#231465 = ORIENTED_EDGE ( 'NONE', *, *, #66800, .T. ) ;
#231466 = EDGE_CURVE ( 'NONE', #133237, #16470, #162785, .T. ) ;
#231467 = DIRECTION ( 'NONE',  ( 1.000000000000000000, -0.000000000000000000, -0.000000000000000000 ) ) ;
#231468 = AXIS2_PLACEMENT_3D ( 'NONE', #64841, #42719, #239646 ) ;
#231469 = ORIENTED_EDGE ( 'NONE', *, *, #223654, .T. ) ;
#231470 = EDGE_LOOP ( 'NONE', ( #104643, #163387 ) ) ;
#231471 = VECTOR ( 'NONE', #49181, 1000.000000000000000 ) ;
#231472 = DIRECTION ( 'NONE',  ( 0.000000000000000000, 0.000000000000000000, -1.000000000000000000 ) ) ;
#231473 = CARTESIAN_POINT ( 'NONE',  ( -16.77828822508139694, 66.05377062509082009, -56.86047923315044272 ) ) ;
#231474 = DIRECTION ( 'NONE',  ( -1.000000000000000000, 1.652117596168391700E-15, 0.000000000000000000 ) ) ;
#231475 = DIRECTION ( 'NONE',  ( 0.000000000000000000, 0.4797419643160688585, 0.8774096236502991752 ) ) ;
#231476 = CARTESIAN_POINT ( 'NONE',  ( -23.15000000000000213, 1.115600667400684642E-11, -33.50000000000000000 ) ) ;
#231477 = EDGE_CURVE ( 'NONE', #255460, #81419, #242293, .T. ) ;
#231478 = DIRECTION ( 'NONE',  ( 1.000000000000000000, -0.000000000000000000, -0.000000000000000000 ) ) ;
#231479 = CARTESIAN_POINT ( 'NONE',  ( -13.54795643572457919, 9.450668889178682974, -82.05554649020740499 ) ) ;
#231480 = ORIENTED_EDGE ( 'NONE', *, *, #202453, .F. ) ;
#231482 = CARTESIAN_POINT ( 'NONE',  ( -22.32929514600008503, 65.15191943456896695, -243.1436103818390677 ) ) ;
#231481 = CARTESIAN_POINT ( 'NONE',  ( 22.59999999999999432, 75.95218160930740225, -148.2731299035715153 ) ) ;
#231483 = CARTESIAN_POINT ( 'NONE',  ( -20.85000000000000142, 7.128833340094563376, -233.7327013124401276 ) ) ;
#231484 = VECTOR ( 'NONE', #74620, 1000.000000000000000 ) ;
#231485 = VERTEX_POINT ( 'NONE', #221429 ) ;
#231486 = DIRECTION ( 'NONE',  ( -1.000000000000000000, -7.304098846218135653E-16, -5.100424963727256530E-30 ) ) ;
#231487 = AXIS2_PLACEMENT_3D ( 'NONE', #113111, #251322, #212231 ) ;
#231488 = DIRECTION ( 'NONE',  ( -1.000000000000000000, 0.000000000000000000, 0.000000000000000000 ) ) ;
#231489 = CARTESIAN_POINT ( 'NONE',  ( -20.85000000000000142, 77.16412189325286874, -61.60825939895269698 ) ) ;
#231490 = ORIENTED_EDGE ( 'NONE', *, *, #145496, .T. ) ;
#231491 = AXIS2_PLACEMENT_3D ( 'NONE', #72128, #135915, #134627 ) ;
#231492 = CARTESIAN_POINT ( 'NONE',  ( 20.94999999999999574, 1.162701749949165642, -108.6000000000000227 ) ) ;
#231493 = CARTESIAN_POINT ( 'NONE',  ( 20.94999999999999929, 1.115600667400684642E-11, -134.0000000000000284 ) ) ;
#231494 = CARTESIAN_POINT ( 'NONE',  ( 13.12220780326572012, 66.56936653093907807, -87.79134168970030316 ) ) ;
#231495 = EDGE_LOOP ( 'NONE', ( #243848, #121554, #256780, #19693 ) ) ;
#231496 = ORIENTED_EDGE ( 'NONE', *, *, #164789, .T. ) ;
#231497 = LINE ( 'NONE', #52828, #49398 ) ;
#231498 = CARTESIAN_POINT ( 'NONE',  ( -23.15000000000000213, 82.25348978056602789, -214.8488183945435139 ) ) ;
#231499 = CIRCLE ( 'NONE', #19086, 0.1000000000000028644 ) ;
#231500 = DIRECTION ( 'NONE',  ( 1.000000000000000000, -0.000000000000000000, -0.000000000000000000 ) ) ;
#231501 = FACE_OUTER_BOUND ( 'NONE', #45949, .T. ) ;
#231502 = ORIENTED_EDGE ( 'NONE', *, *, #148382, .F. ) ;
#231503 = DIRECTION ( 'NONE',  ( 0.000000000000000000, -0.3999834006488773852, -0.9165223833629813077 ) ) ;
#231504 = DIRECTION ( 'NONE',  ( 1.000000000000000000, -0.000000000000000000, 0.000000000000000000 ) ) ;
#231505 = DIRECTION ( 'NONE',  ( 1.000000000000000000, 0.000000000000000000, 0.000000000000000000 ) ) ;
#231506 = CARTESIAN_POINT ( 'NONE',  ( 23.24999999999999645, 4.999999999999997335, -21.09473398108690390 ) ) ;
#231507 = TOROIDAL_SURFACE ( 'NONE', #77351, 0.4000000000000003553, 0.1000000000000000056 ) ;
#231508 = VECTOR ( 'NONE', #207060, 1000.000000000000000 ) ;
#231509 = EDGE_CURVE ( 'NONE', #53442, #196016, #90643, .T. ) ;
#231510 = ORIENTED_EDGE ( 'NONE', *, *, #9726, .F. ) ;
#231511 = CIRCLE ( 'NONE', #189809, 7.899999999999990585 ) ;
#231512 = CARTESIAN_POINT ( 'NONE',  ( -18.44448725179915627, -9.490081715472170387, -207.6289602940624661 ) ) ;
#231514 = ORIENTED_EDGE ( 'NONE', *, *, #152094, .T. ) ;
#231513 = DIRECTION ( 'NONE',  ( 2.952720810173289112E-16, 1.000000000000000000, -6.088138035986627436E-46 ) ) ;
#231515 = DIRECTION ( 'NONE',  ( 1.000000000000000000, 0.000000000000000000, 0.000000000000000000 ) ) ;
#231516 = DIRECTION ( 'NONE',  ( 0.000000000000000000, 0.8814952561688166321, -0.4721928772777839733 ) ) ;
#231517 = FACE_OUTER_BOUND ( 'NONE', #86366, .T. ) ;
#231518 = ADVANCED_FACE ( 'NONE', ( #246158 ), #122365, .T. ) ;
#231519 = DIRECTION ( 'NONE',  ( -6.938893903907222067E-15, 1.000000000000000000, 2.891205793294679805E-16 ) ) ;
#231520 = VERTEX_POINT ( 'NONE', #24564 ) ;
#231521 = CARTESIAN_POINT ( 'NONE',  ( 20.95512828230152280, 8.876151312325294640, -12.20243026550310361 ) ) ;
#231522 = CARTESIAN_POINT ( 'NONE',  ( -20.05000000000000426, 9.250000000000001776, -12.34999999999999964 ) ) ;
#231523 = CARTESIAN_POINT ( 'NONE',  ( -18.38639463286148867, 11.48019957383597855, -9.250000000000001776 ) ) ;
#231524 = EDGE_LOOP ( 'NONE', ( #244430, #208314, #186811, #254155 ) ) ;
#231525 = CARTESIAN_POINT ( 'NONE',  ( -23.15000000000000213, 5.900000000011162093, -56.78090023534362984 ) ) ;
#231526 = CARTESIAN_POINT ( 'NONE',  ( -1.739115166359751170E-14, 11.65000000001114699, -158.8500000000000227 ) ) ;
#231527 = EDGE_CURVE ( 'NONE', #83438, #43818, #132348, .T. ) ;
#231528 = EDGE_CURVE ( 'NONE', #28509, #61108, #44107, .T. ) ;
#231529 = FACE_OUTER_BOUND ( 'NONE', #23762, .T. ) ;
#231530 = CIRCLE ( 'NONE', #6649, 0.1999999999999987899 ) ;
#231531 = AXIS2_PLACEMENT_3D ( 'NONE', #205110, #42217, #240413 ) ;
#231532 = CARTESIAN_POINT ( 'NONE',  ( 20.94999999999999929, 8.776282895303632259, -146.1500000000000341 ) ) ;
#231533 = DIRECTION ( 'NONE',  ( 0.000000000000000000, 0.3738317757009345654, 0.9274965247785492695 ) ) ;
#231534 = ORIENTED_EDGE ( 'NONE', *, *, #52889, .T. ) ;
#231535 = EDGE_LOOP ( 'NONE', ( #190304, #198076, #2106, #209124 ) ) ;
#231537 = CARTESIAN_POINT ( 'NONE',  ( -18.46856557590793813, -9.474215907775338508, -141.1019862408823542 ) ) ;
#231536 = AXIS2_PLACEMENT_3D ( 'NONE', #140136, #141436, #220966 ) ;
#231538 = DIRECTION ( 'NONE',  ( 0.000000000000000000, 0.000000000000000000, -1.000000000000000000 ) ) ;
#231539 = ADVANCED_FACE ( 'NONE', ( #230444 ), #92203, .T. ) ;
#231540 = DIRECTION ( 'NONE',  ( 0.000000000000000000, -1.000000000000000000, 0.000000000000000000 ) ) ;
#231541 = DIRECTION ( 'NONE',  ( -1.000000000000000000, 0.000000000000000000, -0.000000000000000000 ) ) ;
#231542 = CYLINDRICAL_SURFACE ( 'NONE', #13582, 0.09999999999999939493 ) ;
#231543 = DIRECTION ( 'NONE',  ( -0.000000000000000000, -0.000000000000000000, 1.000000000000000000 ) ) ;
#231544 = DIRECTION ( 'NONE',  ( 0.000000000000000000, 1.000000000000000000, 0.000000000000000000 ) ) ;
#231545 = LINE ( 'NONE', #174175, #165277 ) ;
#231546 = VECTOR ( 'NONE', #43443, 999.9999999999998863 ) ;
#231547 = VERTEX_POINT ( 'NONE', #11408 ) ;
#231548 = CARTESIAN_POINT ( 'NONE',  ( -18.59999999999999787, 85.32100840337290037, -62.28716923544637751 ) ) ;
#231549 = EDGE_LOOP ( 'NONE', ( #210531, #191960, #240922, #142203 ) ) ;
#231550 = EDGE_CURVE ( 'NONE', #226006, #84528, #72681, .T. ) ;
#231551 = FACE_OUTER_BOUND ( 'NONE', #33609, .T. ) ;
#231552 = EDGE_CURVE ( 'NONE', #91270, #156274, #113064, .T. ) ;
#231553 = CARTESIAN_POINT ( 'NONE',  ( 21.05000000000000071, 10.68429367438713484, -7.526673938637355121 ) ) ;
#231554 = CARTESIAN_POINT ( 'NONE',  ( 21.05995757104869526, 8.775389244732430427, -79.19490512299125839 ) ) ;
#231555 = PRESENTATION_STYLE_ASSIGNMENT (( #13783 ) ) ;
#231556 = SPHERICAL_SURFACE ( 'NONE', #128816, 0.1000000000000000056 ) ;
#231557 = DIRECTION ( 'NONE',  ( -1.000000000000000000, 0.000000000000000000, 0.000000000000000000 ) ) ;
#231558 = ORIENTED_EDGE ( 'NONE', *, *, #129486, .T. ) ;
#231559 = DIRECTION ( 'NONE',  ( 0.000000000000000000, -1.776356839400250465E-15, -1.000000000000000000 ) ) ;
#231560 = CYLINDRICAL_SURFACE ( 'NONE', #75594, 0.1000000000000028644 ) ;
#231561 = CYLINDRICAL_SURFACE ( 'NONE', #94144, 11.80000000000000426 ) ;
#231563 = EDGE_CURVE ( 'NONE', #98003, #155495, #3334, .T. ) ;
#231562 = CARTESIAN_POINT ( 'NONE',  ( 18.39999999999999858, -9.599999999988845900, -207.7001893912220112 ) ) ;
#231564 = AXIS2_PLACEMENT_3D ( 'NONE', #186019, #43940, #148171 ) ;
#231565 = VECTOR ( 'NONE', #189622, 1000.000000000000000 ) ;
#231566 = LINE ( 'NONE', #153353, #237190 ) ;
#231567 = VECTOR ( 'NONE', #64731, 1000.000000000000000 ) ;
#231568 = AXIS2_PLACEMENT_3D ( 'NONE', #92174, #246127, #54322 ) ;
#231569 = EDGE_LOOP ( 'NONE', ( #252865, #145706, #199874, #94190 ) ) ;
#231571 = CARTESIAN_POINT ( 'NONE',  ( -16.77683809663752257, 66.05000000001224691, -149.1731074845244223 ) ) ;
#231570 =( GEOMETRIC_REPRESENTATION_CONTEXT ( 3 ) GLOBAL_UNCERTAINTY_ASSIGNED_CONTEXT ( ( #160080 ) ) GLOBAL_UNIT_ASSIGNED_CONTEXT ( ( #208057, #177910, #151940 ) ) REPRESENTATION_CONTEXT ( 'NONE', 'WORKASPACE' ) );
#231572 = CARTESIAN_POINT ( 'NONE',  ( 20.94999999999999574, 5.899999999999947065, -10.21909976465641456 ) ) ;
#231573 = ORIENTED_EDGE ( 'NONE', *, *, #112376, .T. ) ;
#231574 = ORIENTED_EDGE ( 'NONE', *, *, #83837, .F. ) ;
#231575 = DIRECTION ( 'NONE',  ( 0.000000000000000000, -0.2128009952263605342, 0.9770955615653315052 ) ) ;
#231576 = CARTESIAN_POINT ( 'NONE',  ( 21.04999999999999361, 11.16637775885291894, -211.0297240376519596 ) ) ;
#231577 = EDGE_CURVE ( 'NONE', #42095, #239004, #30995, .T. ) ;
#231578 = ORIENTED_EDGE ( 'NONE', *, *, #208721, .F. ) ;
#231579 = CARTESIAN_POINT ( 'NONE',  ( -18.50000000000000000, 62.46832465249013921, -225.2232495205141731 ) ) ;
#231580 = DIRECTION ( 'NONE',  ( 0.000000000000000000, -1.000000000000000000, 0.000000000000000000 ) ) ;
#231581 = ORIENTED_EDGE ( 'NONE', *, *, #104855, .T. ) ;
#231582 = TOROIDAL_SURFACE ( 'NONE', #244041, 0.2000000000000000111, 0.1000000000000000056 ) ;
#231583 = CIRCLE ( 'NONE', #135879, 7.800000000000001599 ) ;
#231584 = FACE_OUTER_BOUND ( 'NONE', #120755, .T. ) ;
#231585 = ADVANCED_FACE ( 'NONE', ( #152221 ), #188742, .T. ) ;
#231586 = ORIENTED_EDGE ( 'NONE', *, *, #69720, .T. ) ;
#231587 = AXIS2_PLACEMENT_3D ( 'NONE', #176119, #92694, #14480 ) ;
#231588 = CARTESIAN_POINT ( 'NONE',  ( -20.94999999999999929, 87.65000000001212754, -133.6231074845242119 ) ) ;
#231589 = LINE ( 'NONE', #95904, #196102 ) ;
#231591 = ORIENTED_EDGE ( 'NONE', *, *, #148987, .F. ) ;
#231590 = DIRECTION ( 'NONE',  ( 1.000000000000000000, 0.000000000000000000, 0.000000000000000000 ) ) ;
#231592 = DIRECTION ( 'NONE',  ( 0.000000000000000000, 1.000000000000000000, 6.982962677686266711E-15 ) ) ;
#231594 = TOROIDAL_SURFACE ( 'NONE', #135890, 0.2000000000000000111, 0.1000000000000000056 ) ;
#231593 = DIRECTION ( 'NONE',  ( 0.000000000000000000, -1.000000000000000000, -6.982962677686265922E-15 ) ) ;
#231595 = EDGE_CURVE ( 'NONE', #218193, #135203, #219830, .T. ) ;
#231597 = EDGE_CURVE ( 'NONE', #3677, #245148, #257203, .T. ) ;
#231596 = CYLINDRICAL_SURFACE ( 'NONE', #351, 0.09999999999999543976 ) ;
#231598 = AXIS2_PLACEMENT_3D ( 'NONE', #142844, #161164, #15586 ) ;
#231599 = PLANE ( 'NONE',  #68408 ) ;
#231600 = CARTESIAN_POINT ( 'NONE',  ( -16.80438519320023616, 66.05022090354425757, -190.8723692036031423 ) ) ;
#231601 = CARTESIAN_POINT ( 'NONE',  ( 23.14999999999999858, 28.32080209959243788, -238.8452605374484676 ) ) ;
#231602 = CARTESIAN_POINT ( 'NONE',  ( 18.49999999999999289, 7.120270961697594103, -37.15956304183931991 ) ) ;
#231604 = VERTEX_POINT ( 'NONE', #33573 ) ;
#231603 = FACE_OUTER_BOUND ( 'NONE', #144155, .T. ) ;
#231605 = ORIENTED_EDGE ( 'NONE', *, *, #208445, .F. ) ;
#231607 = CARTESIAN_POINT ( 'NONE',  ( -12.30589683808040213, 9.356746017089404788, -84.20335972136423663 ) ) ;
#231606 = DIRECTION ( 'NONE',  ( -3.265361837132813093E-16, 1.000000000000000000, -0.000000000000000000 ) ) ;
#231609 = ORIENTED_EDGE ( 'NONE', *, *, #126837, .T. ) ;
#231608 = CARTESIAN_POINT ( 'NONE',  ( 23.14999999999999858, 70.40000000001261071, -191.1178414656113205 ) ) ;
#231610 = ORIENTED_EDGE ( 'NONE', *, *, #73162, .F. ) ;
#231611 = LINE ( 'NONE', #15128, #114187 ) ;
#231612 = DIRECTION ( 'NONE',  ( 1.000000000000000000, -7.304098846218134667E-16, -4.217023435051625732E-16 ) ) ;
#231613 = EDGE_CURVE ( 'NONE', #80723, #108723, #19949, .T. ) ;
#231614 = AXIS2_PLACEMENT_3D ( 'NONE', #223659, #240671, #62051 ) ;
#231615 = EDGE_CURVE ( 'NONE', #109830, #212015, #81006, .T. ) ;
#231616 = VECTOR ( 'NONE', #18807, 999.9999999999998863 ) ;
#231617 = CIRCLE ( 'NONE', #94223, 0.09999999999999602263 ) ;
#231618 = CARTESIAN_POINT ( 'NONE',  ( 20.94999999999999574, 4.360421613930905771, -245.4659189663672691 ) ) ;
#231619 = CARTESIAN_POINT ( 'NONE',  ( 18.59999999999996945, 7.021664781911246322, -104.3335654018973315 ) ) ;
#231620 = LINE ( 'NONE', #111656, #155418 ) ;
#231621 = EDGE_CURVE ( 'NONE', #245292, #20295, #53252, .T. ) ;
#231622 = FACE_OUTER_BOUND ( 'NONE', #110397, .T. ) ;
#231623 = CARTESIAN_POINT ( 'NONE',  ( -20.94999999999999929, -0.2561057920810652089, -100.4651035583277405 ) ) ;
#231625 = ORIENTED_EDGE ( 'NONE', *, *, #65568, .F. ) ;
#231624 = ADVANCED_FACE ( 'NONE', ( #90923 ), #130039, .F. ) ;
#231626 = ORIENTED_EDGE ( 'NONE', *, *, #117469, .T. ) ;
#231627 = CARTESIAN_POINT ( 'NONE',  ( 21.07928932188134041, 30.84304088366581453, -252.0482413927673235 ) ) ;
#231628 = CIRCLE ( 'NONE', #6763, 0.09999999999999939493 ) ;
#231629 = ORIENTED_EDGE ( 'NONE', *, *, #135250, .F. ) ;
#231630 = ADVANCED_FACE ( 'NONE', ( #209599 ), #251273, .F. ) ;
#231631 = CARTESIAN_POINT ( 'NONE',  ( -18.59999999999999787, -9.399999999988851940, -174.3820418481726904 ) ) ;
#231633 = EDGE_CURVE ( 'NONE', #258105, #193670, #169817, .T. ) ;
#231632 = VERTEX_POINT ( 'NONE', #53081 ) ;
#231634 = DIRECTION ( 'NONE',  ( 1.000000000000000000, -0.000000000000000000, 0.000000000000000000 ) ) ;
#231635 = FACE_OUTER_BOUND ( 'NONE', #134492, .T. ) ;
#231636 = ADVANCED_FACE ( 'NONE', ( #210878 ), #252556, .T. ) ;
#231637 = DIRECTION ( 'NONE',  ( 1.000000000000000000, 0.000000000000000000, 0.000000000000000000 ) ) ;
#231638 = ORIENTED_EDGE ( 'NONE', *, *, #208566, .F. ) ;
#231639 = FACE_OUTER_BOUND ( 'NONE', #229936, .T. ) ;
#231640 = VERTEX_POINT ( 'NONE', #73969 ) ;
#231641 = EDGE_CURVE ( 'NONE', #227863, #24784, #57700, .T. ) ;
#231642 = AXIS2_PLACEMENT_3D ( 'NONE', #161731, #83417, #245092 ) ;
#231643 = FACE_OUTER_BOUND ( 'NONE', #236256, .T. ) ;
#231644 = EDGE_CURVE ( 'NONE', #133244, #72626, #148339, .T. ) ;
#231645 = VECTOR ( 'NONE', #206957, 1000.000000000000000 ) ;
#231646 = FACE_OUTER_BOUND ( 'NONE', #185796, .T. ) ;
#231647 = CIRCLE ( 'NONE', #135765, 0.8750000000000007772 ) ;
#231649 = VERTEX_POINT ( 'NONE', #199016 ) ;
#231648 = ADVANCED_FACE ( 'NONE', ( #158634 ), #115991, .T. ) ;
#231650 = LINE ( 'NONE', #47835, #31923 ) ;
#231651 = EDGE_LOOP ( 'NONE', ( #161960, #79308, #134521, #196222 ) ) ;
#231654 = VERTEX_POINT ( 'NONE', #59460 ) ;
#231653 = CARTESIAN_POINT ( 'NONE',  ( 18.39999999999999503, 8.822561741677553471, -57.75000000000000000 ) ) ;
#231652 = CARTESIAN_POINT ( 'NONE',  ( -18.59999999999999787, 11.65000000001115232, -88.75000000000004263 ) ) ;
#231655 = CARTESIAN_POINT ( 'NONE',  ( -20.94999999999999929, 64.35000000001147669, -42.80697314750250371 ) ) ;
#231656 = EDGE_LOOP ( 'NONE', ( #200887, #140232, #238057, #81628, #152416, #238163 ) ) ;
#231657 = CIRCLE ( 'NONE', #160920, 0.09999999999999939493 ) ;
#231658 = EDGE_LOOP ( 'NONE', ( #93089, #111158, #198343, #233823 ) ) ;
#231659 = CARTESIAN_POINT ( 'NONE',  ( 20.94999999999999929, 69.09936979046463534, -247.6075824278584889 ) ) ;
#231660 = ORIENTED_EDGE ( 'NONE', *, *, #122583, .F. ) ;
#231661 = ADVANCED_FACE ( 'NONE', ( #77761 ), #136812, .T. ) ;
#231662 = FACE_OUTER_BOUND ( 'NONE', #22980, .T. ) ;
#231663 = FACE_OUTER_BOUND ( 'NONE', #84359, .T. ) ;
#231664 = VECTOR ( 'NONE', #250345, 1000.000000000000114 ) ;
#231665 = PLANE ( 'NONE',  #11925 ) ;
#231666 = EDGE_CURVE ( 'NONE', #19842, #7494, #256352, .T. ) ;
#231667 = DIRECTION ( 'NONE',  ( 1.000000000000000000, 0.000000000000000000, 0.000000000000000000 ) ) ;
#231668 = VECTOR ( 'NONE', #224765, 1000.000000000000227 ) ;
#231669 = DIRECTION ( 'NONE',  ( 0.7071067811865487940, 0.6909108974501225742, 0.1504730267678046074 ) ) ;
#231670 = AXIS2_PLACEMENT_3D ( 'NONE', #138473, #99350, #41990 ) ;
#231671 = ORIENTED_EDGE ( 'NONE', *, *, #256933, .F. ) ;
#231672 = CARTESIAN_POINT ( 'NONE',  ( -16.94180778212363236, 44.07631700300555622, -235.2789292040941973 ) ) ;
#231673 = CARTESIAN_POINT ( 'NONE',  ( 21.14999999999999858, 11.75000000001116263, -55.25000000000004974 ) ) ;
#231674 = CARTESIAN_POINT ( 'NONE',  ( 21.05000000000000071, 6.650000000011155876, -45.65000000000000568 ) ) ;
#231675 = ORIENTED_EDGE ( 'NONE', *, *, #24217, .T. ) ;
#231676 = CARTESIAN_POINT ( 'NONE',  ( -22.32929514600008503, 0.09907567811392146984, 7.578647565376503081 ) ) ;
#231677 = EDGE_LOOP ( 'NONE', ( #252080, #93346, #208839, #80534, #60842 ) ) ;
#231678 = CARTESIAN_POINT ( 'NONE',  ( -23.15000000000000213, 2.600000000011154278, -87.27537807723794572 ) ) ;
#231679 = ORIENTED_EDGE ( 'NONE', *, *, #226704, .T. ) ;
#231680 = LINE ( 'NONE', #114279, #105823 ) ;
#231681 = DIRECTION ( 'NONE',  ( 0.000000000000000000, 1.000000000000000000, 1.734723475976807292E-15 ) ) ;
#231682 = AXIS2_PLACEMENT_3D ( 'NONE', #206688, #87994, #241953 ) ;
#231683 = VERTEX_POINT ( 'NONE', #195195 ) ;
#231684 = DIRECTION ( 'NONE',  ( 0.000000000000000000, 0.9126074666063602736, 0.4088369013363654103 ) ) ;
#231685 = ORIENTED_EDGE ( 'NONE', *, *, #23683, .T. ) ;
#231686 = CYLINDRICAL_SURFACE ( 'NONE', #77640, 2.000000000000001776 ) ;
#231687 = CARTESIAN_POINT ( 'NONE',  ( -16.83558968593864336, 9.950000000011137047, -113.1623051876165249 ) ) ;
#231688 = VERTEX_POINT ( 'NONE', #116911 ) ;
#231689 = EDGE_CURVE ( 'NONE', #241979, #173065, #244966, .T. ) ;
#231690 = CYLINDRICAL_SURFACE ( 'NONE', #64256, 0.09999999999999939493 ) ;
#231691 = DIRECTION ( 'NONE',  ( -4.408576920032448588E-17, 0.1350103645451876944, 0.9908441862701601321 ) ) ;
#231692 = ORIENTED_EDGE ( 'NONE', *, *, #203822, .T. ) ;
#231693 = CARTESIAN_POINT ( 'NONE',  ( 21.30000000000002558, 76.00000000001197975, -107.0731074845243143 ) ) ;
#231694 = VECTOR ( 'NONE', #214448, 1000.000000000000000 ) ;
#231695 = ADVANCED_FACE ( 'NONE', ( #213435 ), #172755, .F. ) ;
#231696 = AXIS2_PLACEMENT_3D ( 'NONE', #127695, #65134, #66432 ) ;
#231697 = VECTOR ( 'NONE', #32307, 1000.000000000000000 ) ;
#231698 = ORIENTED_EDGE ( 'NONE', *, *, #233587, .F. ) ;
#231699 = CARTESIAN_POINT ( 'NONE',  ( 12.33938619321247998, 9.360723793997191677, -117.8139271946067907 ) ) ;
#231700 = CARTESIAN_POINT ( 'NONE',  ( 21.05000000000000071, 1.658775325997237315, -230.6916041481598540 ) ) ;
#231703 = ORIENTED_EDGE ( 'NONE', *, *, #208905, .F. ) ;
#231702 = VERTEX_POINT ( 'NONE', #157358 ) ;
#231701 = DIRECTION ( 'NONE',  ( -1.073024830501117725E-15, 0.000000000000000000, 1.000000000000000000 ) ) ;
#231704 = DIRECTION ( 'NONE',  ( 1.000000000000000000, -0.000000000000000000, 0.000000000000000000 ) ) ;
#231705 = CARTESIAN_POINT ( 'NONE',  ( -23.39999999999994529, 82.78482233730476025, -26.42994920107286916 ) ) ;
#231706 = DIRECTION ( 'NONE',  ( 0.000000000000000000, 0.000000000000000000, -1.000000000000000000 ) ) ;
#231707 = CIRCLE ( 'NONE', #248448, 0.09999999999998898659 ) ;
#231709 = CARTESIAN_POINT ( 'NONE',  ( -18.69999999999999929, -11.65000000000000036, 6.000000000000001776 ) ) ;
#231708 = DIRECTION ( 'NONE',  ( 1.000000000000000000, -0.000000000000000000, -0.000000000000000000 ) ) ;
#231711 = EDGE_CURVE ( 'NONE', #53690, #146901, #28544, .T. ) ;
#231710 = DIRECTION ( 'NONE',  ( 0.000000000000000000, -0.9651348961777157509, 0.2617529984165031243 ) ) ;
#231712 = CARTESIAN_POINT ( 'NONE',  ( -21.05000000000000071, -1.835341550213255957, -45.05515129256298223 ) ) ;
#231713 = AXIS2_PLACEMENT_3D ( 'NONE', #100424, #203414, #24805 ) ;
#231714 = LINE ( 'NONE', #167904, #151684 ) ;
#231715 = DIRECTION ( 'NONE',  ( 0.000000000000000000, 0.2617529984165031243, 0.9651348961777157509 ) ) ;
#231716 = ORIENTED_EDGE ( 'NONE', *, *, #140541, .F. ) ;
#231717 = EDGE_LOOP ( 'NONE', ( #201431, #152981, #181372, #206502 ) ) ;
#231718 = CARTESIAN_POINT ( 'NONE',  ( 18.49999999999999645, 74.27191306321728348, -82.63867247935655769 ) ) ;
#231719 = CIRCLE ( 'NONE', #15239, 12.87500000000000000 ) ;
#231721 = EDGE_LOOP ( 'NONE', ( #215332, #45922, #233890, #35418 ) ) ;
#231720 = CARTESIAN_POINT ( 'NONE',  ( -23.15000000000000213, 74.00000000001254818, -183.2477294072864709 ) ) ;
#231722 = ORIENTED_EDGE ( 'NONE', *, *, #178998, .T. ) ;
#231723 = DIRECTION ( 'NONE',  ( 0.000000000000000000, -6.652207440891584540E-15, 1.000000000000000000 ) ) ;
#231724 = ORIENTED_EDGE ( 'NONE', *, *, #127447, .F. ) ;
#231725 = CARTESIAN_POINT ( 'NONE',  ( 21.00023020733439338, 34.04610124266385185, -243.7188077099090719 ) ) ;
#231726 = ORIENTED_EDGE ( 'NONE', *, *, #86801, .F. ) ;
#231727 = CARTESIAN_POINT ( 'NONE',  ( 18.39999999999999503, 64.25000000001207923, -123.8731074845243683 ) ) ;
#231730 = EDGE_LOOP ( 'NONE', ( #140803, #137210, #1978, #205159 ) ) ;
#231729 = EDGE_LOOP ( 'NONE', ( #120000, #12242, #249612, #240019 ) ) ;
#231728 = AXIS2_PLACEMENT_3D ( 'NONE', #12038, #148978, #131956 ) ;
#231731 = EDGE_LOOP ( 'NONE', ( #77846, #219202, #242184 ) ) ;
#231732 = VERTEX_POINT ( 'NONE', #135173 ) ;
#231733 = VERTEX_POINT ( 'NONE', #38661 ) ;
#231734 = CARTESIAN_POINT ( 'NONE',  ( 18.49999999999999645, 1.736257131608553550, -112.0686523290175245 ) ) ;
#231735 = DIRECTION ( 'NONE',  ( 0.000000000000000000, 0.9770955615653548199, 0.2128009952262535920 ) ) ;
#231736 = DIRECTION ( 'NONE',  ( -0.000000000000000000, 0.000000000000000000, -1.000000000000000000 ) ) ;
#231738 = ORIENTED_EDGE ( 'NONE', *, *, #126881, .T. ) ;
#231737 = DIRECTION ( 'NONE',  ( 0.000000000000000000, 0.2128009952263606730, -0.9770955615653313941 ) ) ;
#231739 = DIRECTION ( 'NONE',  ( 0.000000000000000000, -2.775557561562888827E-14, 1.000000000000000000 ) ) ;
#231740 = DIRECTION ( 'NONE',  ( -1.000000000000000000, -0.000000000000000000, 0.000000000000000000 ) ) ;
#231742 = ORIENTED_EDGE ( 'NONE', *, *, #84414, .F. ) ;
#231741 = LINE ( 'NONE', #170530, #39236 ) ;
#231743 = DIRECTION ( 'NONE',  ( 1.000000000000000000, 0.000000000000000000, 0.000000000000000000 ) ) ;
#231744 = EDGE_LOOP ( 'NONE', ( #116376, #93127, #32200, #63565 ) ) ;
#231746 = AXIS2_PLACEMENT_3D ( 'NONE', #142616, #123086, #207772 ) ;
#231745 = CARTESIAN_POINT ( 'NONE',  ( 20.94999999999999574, 87.48912529308817909, -133.6231074845242119 ) ) ;
#231747 = EDGE_CURVE ( 'NONE', #10263, #111464, #49335, .T. ) ;
#231748 = ORIENTED_EDGE ( 'NONE', *, *, #87223, .T. ) ;
#231749 = CARTESIAN_POINT ( 'NONE',  ( -18.59999999999999787, 7.021664781911246322, -171.3335654018973173 ) ) ;
#231750 = FACE_OUTER_BOUND ( 'NONE', #36701, .T. ) ;
#231751 = EDGE_CURVE ( 'NONE', #58672, #76466, #11771, .T. ) ;
#231752 = EDGE_LOOP ( 'NONE', ( #27969, #179624, #247665, #164954 ) ) ;
#231754 = FACE_OUTER_BOUND ( 'NONE', #113825, .T. ) ;
#231753 = CARTESIAN_POINT ( 'NONE',  ( 21.05000000000000071, 74.83729825007431202, -161.9231074845243654 ) ) ;
#231755 = CARTESIAN_POINT ( 'NONE',  ( 18.49999999999999289, 46.32970330538243786, -243.0551226933711746 ) ) ;
#231756 = AXIS2_PLACEMENT_3D ( 'NONE', #104803, #163533, #25330 ) ;
#231757 = LINE ( 'NONE', #135190, #105561 ) ;
#231758 = CARTESIAN_POINT ( 'NONE',  ( 20.12500000000000000, 9.750000000011153745, -41.61177128211428311 ) ) ;
#231759 = ORIENTED_EDGE ( 'NONE', *, *, #15855, .F. ) ;
#231760 = ORIENTED_EDGE ( 'NONE', *, *, #30319, .F. ) ;
#231761 = EDGE_CURVE ( 'NONE', #179033, #240643, #236571, .T. ) ;
#231762 = CARTESIAN_POINT ( 'NONE',  ( -21.64999999999999858, 7.349999999999998757, -21.15000000000000213 ) ) ;
#231763 = DIRECTION ( 'NONE',  ( -0.000000000000000000, 1.000000000000000000, 6.982962677686266711E-15 ) ) ;
#231764 = ORIENTED_EDGE ( 'NONE', *, *, #117155, .T. ) ;
#231765 = DIRECTION ( 'NONE',  ( 1.000000000000000000, 0.000000000000000000, -0.000000000000000000 ) ) ;
#231766 = VERTEX_POINT ( 'NONE', #16544 ) ;
#231767 = CARTESIAN_POINT ( 'NONE',  ( -22.50000000000094147, 0.1000000000110504439, -55.35042919245522341 ) ) ;
#231768 = ADVANCED_FACE ( 'NONE', ( #136445 ), #217620, .T. ) ;
#231769 = CARTESIAN_POINT ( 'NONE',  ( -20.94999999999999929, 1.115600667400684642E-11, -100.5000000000000426 ) ) ;
#231770 = ORIENTED_EDGE ( 'NONE', *, *, #201299, .T. ) ;
#231771 = EDGE_CURVE ( 'NONE', #196072, #119302, #32630, .T. ) ;
#231772 = DIRECTION ( 'NONE',  ( 0.000000000000000000, -0.2617529984165031243, -0.9651348961777157509 ) ) ;
#231773 = AXIS2_PLACEMENT_3D ( 'NONE', #91670, #171263, #152970 ) ;
#231774 = EDGE_LOOP ( 'NONE', ( #19305, #215803, #175932, #154359 ) ) ;
#231775 = EDGE_LOOP ( 'NONE', ( #166204, #115963, #235461, #120332, #73960, #153563, #238744, #192250, #118033, #22528 ) ) ;
#231776 = CIRCLE ( 'NONE', #69469, 0.2000000000000057288 ) ;
#231777 = ORIENTED_EDGE ( 'NONE', *, *, #4982, .T. ) ;
#231778 = AXIS2_PLACEMENT_3D ( 'NONE', #69989, #89510, #205607 ) ;
#231780 = DIRECTION ( 'NONE',  ( 0.000000000000000000, 0.000000000000000000, -1.000000000000000000 ) ) ;
#231779 = VECTOR ( 'NONE', #158343, 1000.000000000000000 ) ;
#231781 = CARTESIAN_POINT ( 'NONE',  ( 13.54556439290364089, 66.54940788787787653, -54.46691916571600700 ) ) ;
#231782 = FACE_OUTER_BOUND ( 'NONE', #234915, .T. ) ;
#231783 = DIRECTION ( 'NONE',  ( 0.000000000000000000, 0.2128009952263603399, -0.9770955615653315052 ) ) ;
#231784 = STYLED_ITEM ( 'NONE', ( #75431 ), #189505 ) ;
#231785 = CYLINDRICAL_SURFACE ( 'NONE', #26120, 0.1000000000000098310 ) ;
#231786 = EDGE_CURVE ( 'NONE', #112033, #111084, #246800, .T. ) ;
#231788 = DIRECTION ( 'NONE',  ( 0.000000000000000000, 0.000000000000000000, -1.000000000000000000 ) ) ;
#231787 = CARTESIAN_POINT ( 'NONE',  ( 21.14999999999999858, 45.11960049378627247, -238.4740710069430349 ) ) ;
#231790 = ORIENTED_EDGE ( 'NONE', *, *, #36092, .F. ) ;
#231789 = CARTESIAN_POINT ( 'NONE',  ( 23.14999999999999503, 6.550000000011156231, -54.75000000000000000 ) ) ;
#231791 = DIRECTION ( 'NONE',  ( 1.000000000000000000, 0.000000000000000000, 0.000000000000000000 ) ) ;
#231792 = ORIENTED_EDGE ( 'NONE', *, *, #46787, .F. ) ;
#231793 = AXIS2_PLACEMENT_3D ( 'NONE', #210755, #249883, #12582 ) ;
#231794 = CARTESIAN_POINT ( 'NONE',  ( -15.39946565075089957, 9.389534562357857439, -149.6748093043899814 ) ) ;
#231795 = CIRCLE ( 'NONE', #44354, 0.1000000000000105804 ) ;
#231796 = VERTEX_POINT ( 'NONE', #22975 ) ;
#231797 = VERTEX_POINT ( 'NONE', #47298 ) ;
#231798 = DIRECTION ( 'NONE',  ( 0.000000000000000000, 0.2128009952263605620, -0.9770955615653315052 ) ) ;
#231799 = CARTESIAN_POINT ( 'NONE',  ( -16.94107738177415712, 10.01423928514777728, -46.04999999999999716 ) ) ;
#231800 = CARTESIAN_POINT ( 'NONE',  ( -16.87036670365549895, 66.01058118070993430, -57.00266760182645243 ) ) ;
#231801 = CARTESIAN_POINT ( 'NONE',  ( -21.37071067811865532, 67.92928932189357738, -148.8731074845244393 ) ) ;
#231802 = TOROIDAL_SURFACE ( 'NONE', #11212, 3.899999999999999467, 0.1000000000000000056 ) ;
#231803 = DIRECTION ( 'NONE',  ( 0.000000000000000000, 1.000000000000000000, 0.000000000000000000 ) ) ;
#231805 = ORIENTED_EDGE ( 'NONE', *, *, #250721, .T. ) ;
#231804 = VECTOR ( 'NONE', #184299, 1000.000000000000000 ) ;
#231806 = VERTEX_POINT ( 'NONE', #102441 ) ;
#231807 = CIRCLE ( 'NONE', #56419, 11.75000000000000355 ) ;
#231808 = DIRECTION ( 'NONE',  ( 0.000000000000000000, 0.2128009952263603677, -0.9770955615653313941 ) ) ;
#231809 = VERTEX_POINT ( 'NONE', #126866 ) ;
#231810 = DIRECTION ( 'NONE',  ( 1.000000000000000000, -2.986185139342070877E-16, 6.665775143889692774E-16 ) ) ;
#231811 = DIRECTION ( 'NONE',  ( 0.000000000000000000, 0.000000000000000000, 1.000000000000000000 ) ) ;
#231812 = EDGE_LOOP ( 'NONE', ( #37619, #111996, #119648, #60751 ) ) ;
#231813 = DIRECTION ( 'NONE',  ( 0.000000000000000000, -0.000000000000000000, -1.000000000000000000 ) ) ;
#231814 = DIRECTION ( 'NONE',  ( 1.000000000000000000, 0.000000000000000000, 0.000000000000000000 ) ) ;
#231815 = CARTESIAN_POINT ( 'NONE',  ( -21.05000000000000071, 6.166536471686127285, -199.6742082547079065 ) ) ;
#231816 = DIRECTION ( 'NONE',  ( -1.000000000000000000, 0.000000000000000000, 0.000000000000000000 ) ) ;
#231817 = VERTEX_POINT ( 'NONE', #10774 ) ;
#231818 = CARTESIAN_POINT ( 'NONE',  ( -20.94999999999999929, 44.18518595211054389, -258.7688298343402380 ) ) ;
#231819 = CARTESIAN_POINT ( 'NONE',  ( -20.94999999999999929, 77.83534155023646406, -124.8679561919612979 ) ) ;
#231820 = CARTESIAN_POINT ( 'NONE',  ( 21.15000000000005542, 76.00000000001119815, -3.023107484524792277 ) ) ;
#231821 = CYLINDRICAL_SURFACE ( 'NONE', #21247, 0.09999999999999939493 ) ;
#231822 = DIRECTION ( 'NONE',  ( 0.000000000000000000, -1.000000000000000000, -0.000000000000000000 ) ) ;
#231823 = VECTOR ( 'NONE', #47597, 1000.000000000000000 ) ;
#231824 = CARTESIAN_POINT ( 'NONE',  ( -20.94999999999999929, 57.84918772656043018, -226.1321410194968280 ) ) ;
#231825 = EDGE_CURVE ( 'NONE', #63242, #199384, #21669, .T. ) ;
#231826 = ORIENTED_EDGE ( 'NONE', *, *, #185670, .F. ) ;
#231827 = CARTESIAN_POINT ( 'NONE',  ( 21.05000000000000426, -0.01681986837452507932, -161.1925747804345974 ) ) ;
#231828 = ORIENTED_EDGE ( 'NONE', *, *, #178234, .T. ) ;
#231829 = PLANE ( 'NONE',  #147272 ) ;
#231830 = ADVANCED_FACE ( 'NONE', ( #227240 ), #95129, .T. ) ;
#231831 = LINE ( 'NONE', #11502, #54327 ) ;
#231832 = CARTESIAN_POINT ( 'NONE',  ( -16.85939681242905763, 66.09477481408649169, -82.48318552933288572 ) ) ;
#231834 = TOROIDAL_SURFACE ( 'NONE', #65211, 0.2000000000000000111, 0.1000000000000000056 ) ;
#231833 = DIRECTION ( 'NONE',  ( 0.000000000000000000, 0.000000000000000000, 1.000000000000000000 ) ) ;
#231835 = CARTESIAN_POINT ( 'NONE',  ( -20.64999999999999858, -8.999999999988844479, -90.60603087734760663 ) ) ;
#231836 = DIRECTION ( 'NONE',  ( -4.408576920032448588E-17, -0.1350103645451807555, -0.9908441862701609093 ) ) ;
#231838 = VERTEX_POINT ( 'NONE', #240712 ) ;
#231837 = CIRCLE ( 'NONE', #90334, 0.1000000000000016431 ) ;
#231839 = CARTESIAN_POINT ( 'NONE',  ( -16.87242674293849021, 66.05000000001224691, -149.1720172381520797 ) ) ;
#231840 = CARTESIAN_POINT ( 'NONE',  ( -16.88593481969334320, 66.04943990992750003, -82.17123522757988496 ) ) ;
#231841 = EDGE_CURVE ( 'NONE', #157707, #219341, #107294, .T. ) ;
#231843 = ADVANCED_FACE ( 'NONE', ( #189413 ), #132544, .F. ) ;
#231842 = AXIS2_PLACEMENT_3D ( 'NONE', #133310, #149034, #246818 ) ;
#231844 = CIRCLE ( 'NONE', #173614, 11.79999999999999361 ) ;
#231845 = CARTESIAN_POINT ( 'NONE',  ( 18.39999999999999503, 59.46930106059529209, -220.6430355403071530 ) ) ;
#231846 = DIRECTION ( 'NONE',  ( 1.000000000000000000, 0.000000000000000000, 0.000000000000000000 ) ) ;
#231847 = DIRECTION ( 'NONE',  ( 0.000000000000000000, 0.000000000000000000, 1.000000000000000000 ) ) ;
#231848 = AXIS2_PLACEMENT_3D ( 'NONE', #170470, #231691, #53027 ) ;
#231849 = VERTEX_POINT ( 'NONE', #87716 ) ;
#231850 = ORIENTED_EDGE ( 'NONE', *, *, #7372, .F. ) ;
#231851 = DIRECTION ( 'NONE',  ( 0.000000000000000000, -6.982962677686266711E-15, 1.000000000000000000 ) ) ;
#231852 = DIRECTION ( 'NONE',  ( -0.000000000000000000, -6.982962677686266711E-15, 1.000000000000000000 ) ) ;
#231853 = CARTESIAN_POINT ( 'NONE',  ( -23.15000000000000213, 71.65000000001259650, -191.1731074845243654 ) ) ;
#231854 = FACE_OUTER_BOUND ( 'NONE', #181329, .T. ) ;
#231855 = CARTESIAN_POINT ( 'NONE',  ( -21.46681500593006930, 69.14248884062519096, -170.0231074845244166 ) ) ;
#231856 = ADVANCED_FACE ( 'NONE', ( #159909 ), #195105, .T. ) ;
#231857 = CIRCLE ( 'NONE', #48665, 0.1000000000000028644 ) ;
#231858 = ORIENTED_EDGE ( 'NONE', *, *, #119979, .T. ) ;
#231859 = CARTESIAN_POINT ( 'NONE',  ( 18.59999999999999076, 74.16465844978787914, -158.4679561919613775 ) ) ;
#231860 = EDGE_CURVE ( 'NONE', #110815, #132129, #70217, .T. ) ;
#231861 = CONTEXT_DEPENDENT_SHAPE_REPRESENTATION ( #117496, #143439 ) ;
#231862 = CIRCLE ( 'NONE', #123704, 0.6000000000000033085 ) ;
#231863 = CARTESIAN_POINT ( 'NONE',  ( -23.25000000000000000, -8.999999999988844479, -57.70603087734755832 ) ) ;
#231864 = CIRCLE ( 'NONE', #57020, 0.5000000000000004441 ) ;
#231865 = ORIENTED_EDGE ( 'NONE', *, *, #139271, .T. ) ;
#231866 = DIRECTION ( 'NONE',  ( 0.000000000000000000, 0.2128009952263403282, -0.9770955615653358350 ) ) ;
#231867 = LINE ( 'NONE', #192728, #62095 ) ;
#231868 = VERTEX_POINT ( 'NONE', #140303 ) ;
#231870 = VERTEX_POINT ( 'NONE', #70775 ) ;
#231869 = CARTESIAN_POINT ( 'NONE',  ( 21.14999999999999858, 11.65000000001116298, -179.6499999999999773 ) ) ;
#231871 = ADVANCED_FACE ( 'NONE', ( #116307 ), #193268, .T. ) ;
#231872 = VECTOR ( 'NONE', #60436, 1000.000000000000000 ) ;
#231873 = VERTEX_POINT ( 'NONE', #133290 ) ;
#231874 = EDGE_CURVE ( 'NONE', #245795, #84708, #53439, .T. ) ;
#231875 = CARTESIAN_POINT ( 'NONE',  ( 21.05000000000000071, 76.00000000001213607, -136.5231074845242745 ) ) ;
#231876 = EDGE_CURVE ( 'NONE', #126429, #74863, #36911, .T. ) ;
#231877 = LINE ( 'NONE', #70244, #34167 ) ;
#231878 = DIRECTION ( 'NONE',  ( 1.000000000000000000, -0.000000000000000000, -0.000000000000000000 ) ) ;
#231879 = CARTESIAN_POINT ( 'NONE',  ( -22.19999999999999929, -11.65000000000000036, 17.70000000000000639 ) ) ;
#231880 = CARTESIAN_POINT ( 'NONE',  ( -23.25000000000000000, 7.128833340093095217, -233.7327013124392749 ) ) ;
#231881 = CARTESIAN_POINT ( 'NONE',  ( 20.94999999999999574, 65.57661458509899433, -95.53105556065429482 ) ) ;
#231882 = CYLINDRICAL_SURFACE ( 'NONE', #255636, 0.09999999999999939493 ) ;
#231884 = CARTESIAN_POINT ( 'NONE',  ( -22.39999999999999858, 11.65000000001115588, -67.10000000000005116 ) ) ;
#231883 = CARTESIAN_POINT ( 'NONE',  ( -6.000000000000003553, -11.34999999999999964, 10.00000000000000178 ) ) ;
#231885 = DIRECTION ( 'NONE',  ( 1.000000000000000000, 0.000000000000000000, 0.000000000000000000 ) ) ;
#231886 = CARTESIAN_POINT ( 'NONE',  ( 21.09546886439511582, 22.10816305914821100, -231.6845674164850948 ) ) ;
#231887 = DIRECTION ( 'NONE',  ( 0.000000000000000000, -0.2128009952264231230, 0.9770955615653178494 ) ) ;
#231888 = AXIS2_PLACEMENT_3D ( 'NONE', #177634, #1516, #240151 ) ;
#231889 = ORIENTED_EDGE ( 'NONE', *, *, #206969, .T. ) ;
#231890 = CIRCLE ( 'NONE', #248608, 0.09999999999999939493 ) ;
#231891 = TOROIDAL_SURFACE ( 'NONE', #227576, 0.4000000000000012990, 0.1000000000000000056 ) ;
#231892 = CARTESIAN_POINT ( 'NONE',  ( -18.41809261886924887, -9.682403314756559354, -40.15684355009123152 ) ) ;
#231893 = DIRECTION ( 'NONE',  ( -1.000000000000000000, -2.952720810173289112E-16, 0.000000000000000000 ) ) ;
#231894 = LINE ( 'NONE', #212329, #245065 ) ;
#231895 = DIRECTION ( 'NONE',  ( 0.000000000000000000, 0.000000000000000000, 1.000000000000000000 ) ) ;
#231896 = DIRECTION ( 'NONE',  ( 0.000000000000000000, -7.487053152578127080E-15, 1.000000000000000000 ) ) ;
#231897 = DIRECTION ( 'NONE',  ( 0.000000000000000000, 0.8814952561688444987, -0.4721928772777320149 ) ) ;
#231898 = VERTEX_POINT ( 'NONE', #92863 ) ;
#231899 = ADVANCED_FACE ( 'NONE', ( #90286 ), #172457, .T. ) ;
#231900 = CARTESIAN_POINT ( 'NONE',  ( -18.69999999999999929, -8.250000000000005329, 30.10000000000000142 ) ) ;
#231901 = VECTOR ( 'NONE', #73415, 1000.000000000000000 ) ;
#231902 = VERTEX_POINT ( 'NONE', #234962 ) ;
#231903 = CARTESIAN_POINT ( 'NONE',  ( 21.13736287352038445, 52.39702576516527444, -233.6834873945836932 ) ) ;
#231904 = DIRECTION ( 'NONE',  ( -1.000000000000000000, 1.836970198721029934E-16, 1.601412966608202925E-30 ) ) ;
#231905 = CIRCLE ( 'NONE', #235581, 0.09999999999999939493 ) ;
#231906 = AXIS2_PLACEMENT_3D ( 'NONE', #33038, #13434, #17289 ) ;
#231907 = CIRCLE ( 'NONE', #119469, 11.64999999999999325 ) ;
#231908 = ORIENTED_EDGE ( 'NONE', *, *, #139499, .T. ) ;
#231909 = CYLINDRICAL_SURFACE ( 'NONE', #164420, 0.1000000000000013933 ) ;
#231910 = EDGE_CURVE ( 'NONE', #23326, #51672, #40985, .T. ) ;
#231911 = ORIENTED_EDGE ( 'NONE', *, *, #194184, .T. ) ;
#231912 = CYLINDRICAL_SURFACE ( 'NONE', #141415, 0.1000000000000000056 ) ;
#231913 = CARTESIAN_POINT ( 'NONE',  ( 21.14999999999999858, 67.21339244341194785, -124.2731074845243597 ) ) ;
#231914 = CARTESIAN_POINT ( 'NONE',  ( 12.25000000000000000, 9.849999999999981881, -16.74999999999999645 ) ) ;
#231915 = EDGE_CURVE ( 'NONE', #43971, #203977, #128445, .T. ) ;
#231916 = DIRECTION ( 'NONE',  ( 0.000000000000000000, -0.8127272543710951647, 0.5826443254700256480 ) ) ;
#231917 = CARTESIAN_POINT ( 'NONE',  ( -16.81453046979149235, 9.939102281440909792, -12.71172652360302635 ) ) ;
#231918 = CARTESIAN_POINT ( 'NONE',  ( -21.46681500597357939, 1.115542391533913547E-11, -60.14248884056706146 ) ) ;
#231919 = DIRECTION ( 'NONE',  ( 1.000000000000000000, -0.000000000000000000, -0.000000000000000000 ) ) ;
#231920 = FACE_OUTER_BOUND ( 'NONE', #149714, .T. ) ;
#231921 = EDGE_CURVE ( 'NONE', #206325, #184497, #170189, .T. ) ;
#231923 = VERTEX_POINT ( 'NONE', #56299 ) ;
#231922 = FACE_OUTER_BOUND ( 'NONE', #89276, .T. ) ;
#231924 = DIRECTION ( 'NONE',  ( 1.000000000000000000, 0.000000000000000000, 0.000000000000000000 ) ) ;
#231925 = ORIENTED_EDGE ( 'NONE', *, *, #46105, .T. ) ;
#231927 = VERTEX_POINT ( 'NONE', #215385 ) ;
#231926 = DIRECTION ( 'NONE',  ( 0.000000000000000000, 0.000000000000000000, 1.000000000000000000 ) ) ;
#231928 = AXIS2_PLACEMENT_3D ( 'NONE', #232707, #249688, #191018 ) ;
#231929 = ORIENTED_EDGE ( 'NONE', *, *, #26073, .T. ) ;
#231930 = CARTESIAN_POINT ( 'NONE',  ( -16.77683809663752257, 23.65833333334447985, -50.25000000000000000 ) ) ;
#231931 = DIRECTION ( 'NONE',  ( 0.000000000000000000, 0.000000000000000000, 1.000000000000000000 ) ) ;
#231932 = EDGE_CURVE ( 'NONE', #76842, #181403, #175035, .T. ) ;
#231933 = EDGE_CURVE ( 'NONE', #257957, #122621, #24413, .T. ) ;
#231934 = CARTESIAN_POINT ( 'NONE',  ( 22.49999999999999645, 75.91119002362479762, -81.17287040255624220 ) ) ;
#231935 = CARTESIAN_POINT ( 'NONE',  ( 18.43473516226073627, -9.494942282758197294, -7.045898683349446578 ) ) ;
#231936 = CARTESIAN_POINT ( 'NONE',  ( 23.14999999999999503, 6.650000000011155876, -155.1500000000000057 ) ) ;
#231938 = LINE ( 'NONE', #196628, #47928 ) ;
#231937 = CIRCLE ( 'NONE', #202689, 12.87499999999999822 ) ;
#231939 = FACE_OUTER_BOUND ( 'NONE', #45801, .T. ) ;
#231941 = AXIS2_PLACEMENT_3D ( 'NONE', #150719, #109003, #228976 ) ;
#231940 = CARTESIAN_POINT ( 'NONE',  ( -18.59999999999999787, 1.162701749949165642, -75.10000000000003695 ) ) ;
#231942 = VERTEX_POINT ( 'NONE', #194575 ) ;
#231943 = VERTEX_POINT ( 'NONE', #13344 ) ;
#231944 = DIRECTION ( 'NONE',  ( 0.000000000000000000, 0.000000000000000000, -1.000000000000000000 ) ) ;
#231945 = AXIS2_PLACEMENT_3D ( 'NONE', #62706, #83511, #142232 ) ;
#231946 = CIRCLE ( 'NONE', #165283, 0.09999999999999939493 ) ;
#231947 = EDGE_CURVE ( 'NONE', #212340, #190315, #36793, .T. ) ;
#231948 = VERTEX_POINT ( 'NONE', #233681 ) ;
#231949 = CARTESIAN_POINT ( 'NONE',  ( -21.05000000000000071, 14.77103648604101060, -236.4083752604501001 ) ) ;
#231951 = EDGE_CURVE ( 'NONE', #139103, #171429, #232411, .T. ) ;
#231950 = EDGE_LOOP ( 'NONE', ( #72141, #13922, #181017, #111681 ) ) ;
#231952 = CARTESIAN_POINT ( 'NONE',  ( 18.50000000000000355, -9.400000000000000355, -40.38204184817267617 ) ) ;
#231953 =( GEOMETRIC_REPRESENTATION_CONTEXT ( 3 ) GLOBAL_UNCERTAINTY_ASSIGNED_CONTEXT ( ( #118375 ) ) GLOBAL_UNIT_ASSIGNED_CONTEXT ( ( #194642, #133361, #35566 ) ) REPRESENTATION_CONTEXT ( 'NONE', 'WORKASPACE' ) );
#231954 = AXIS2_PLACEMENT_3D ( 'NONE', #143499, #202201, #58805 ) ;
#231955 = DIRECTION ( 'NONE',  ( 0.000000000000000000, 0.000000000000000000, -1.000000000000000000 ) ) ;
#231956 = CARTESIAN_POINT ( 'NONE',  ( -21.05000000000000071, 70.10000000001193143, -92.80400771986793984 ) ) ;
#231957 = EDGE_CURVE ( 'NONE', #4469, #71652, #12079, .T. ) ;
#231958 = CIRCLE ( 'NONE', #248682, 4.049999999999998046 ) ;
#231959 = CARTESIAN_POINT ( 'NONE',  ( -21.05000000000000071, -1.162701749938009677, -7.900000000000000355 ) ) ;
#231960 = CARTESIAN_POINT ( 'NONE',  ( 23.14999999999999858, 1.115600667400684642E-11, -167.5000000000000284 ) ) ;
#231961 = ORIENTED_EDGE ( 'NONE', *, *, #239154, .T. ) ;
#231962 = CARTESIAN_POINT ( 'NONE',  ( -18.39999999999999858, -9.682403433465244902, -207.6568433774127413 ) ) ;
#231963 = CARTESIAN_POINT ( 'NONE',  ( -23.15000000000000213, 36.65892442174472876, -249.5511627012454596 ) ) ;
#231964 = EDGE_CURVE ( 'NONE', #186764, #135547, #95439, .T. ) ;
#231965 = CARTESIAN_POINT ( 'NONE',  ( 23.50000000000005684, 83.80000000001119531, -37.18565239344504647 ) ) ;
#231966 = FACE_OUTER_BOUND ( 'NONE', #132972, .T. ) ;
#231968 = ORIENTED_EDGE ( 'NONE', *, *, #250852, .T. ) ;
#231967 = ADVANCED_FACE ( 'NONE', ( #94148 ), #190847, .F. ) ;
#231970 = DIRECTION ( 'NONE',  ( 2.952720810173289112E-16, -1.000000000000000000, 0.000000000000000000 ) ) ;
#231969 = CARTESIAN_POINT ( 'NONE',  ( 21.30000000000002558, 4.959819536546778628E-16, -4.049999999999998934 ) ) ;
#231971 = AXIS2_PLACEMENT_3D ( 'NONE', #147492, #112234, #247871 ) ;
#231972 = ORIENTED_EDGE ( 'NONE', *, *, #130251, .F. ) ;
#231975 = VERTEX_POINT ( 'NONE', #254484 ) ;
#231974 = DIRECTION ( 'NONE',  ( 1.000000000000000000, -0.000000000000000000, -0.000000000000000000 ) ) ;
#231973 = CARTESIAN_POINT ( 'NONE',  ( -16.27683809663751191, 9.350000000011133849, -143.2500000000000000 ) ) ;
#231976 = EDGE_CURVE ( 'NONE', #16861, #11590, #57507, .T. ) ;
#231977 = CIRCLE ( 'NONE', #90276, 0.09999999999999939493 ) ;
#231978 = DIRECTION ( 'NONE',  ( 1.000000000000000000, 0.000000000000000000, 0.000000000000000000 ) ) ;
#231979 = ORIENTED_EDGE ( 'NONE', *, *, #150379, .F. ) ;
#231980 = FACE_OUTER_BOUND ( 'NONE', #179833, .T. ) ;
#231981 = CIRCLE ( 'NONE', #248705, 11.80000000000000426 ) ;
#231982 = FACE_OUTER_BOUND ( 'NONE', #174278, .T. ) ;
#231983 = AXIS2_PLACEMENT_3D ( 'NONE', #22226, #100429, #105554 ) ;
#231984 = CARTESIAN_POINT ( 'NONE',  ( -21.64999999999999858, 10.05000000001113847, -113.2500000000000284 ) ) ;
#231985 = EDGE_CURVE ( 'NONE', #233652, #89621, #203277, .T. ) ;
#231987 = ORIENTED_EDGE ( 'NONE', *, *, #115905, .T. ) ;
#231986 = DIRECTION ( 'NONE',  ( -1.000000000000000000, 0.000000000000000000, -0.000000000000000000 ) ) ;
#231988 = ORIENTED_EDGE ( 'NONE', *, *, #61522, .T. ) ;
#231989 = FACE_OUTER_BOUND ( 'NONE', #207091, .T. ) ;
#231990 = DIRECTION ( 'NONE',  ( 1.000000000000000000, 0.000000000000000000, 0.000000000000000000 ) ) ;
#231991 = DIRECTION ( 'NONE',  ( 0.000000000000000000, 0.4999999999999088507, -0.8660254037844913322 ) ) ;
#231992 = AXIS2_PLACEMENT_3D ( 'NONE', #14626, #234943, #159 ) ;
#231993 = PLANE ( 'NONE',  #34345 ) ;
#231994 = ORIENTED_EDGE ( 'NONE', *, *, #80572, .F. ) ;
#231996 = VECTOR ( 'NONE', #23045, 1000.000000000000227 ) ;
#231995 = CARTESIAN_POINT ( 'NONE',  ( 20.12500000000000000, 14.02742277431099893, -219.5907614236512870 ) ) ;
#231997 = DIRECTION ( 'NONE',  ( 0.000000000000000000, 0.8814952561688428334, -0.4721928772777350125 ) ) ;
#231998 = CARTESIAN_POINT ( 'NONE',  ( 18.54116936837188945, -9.463564198361279267, -141.0485424908882806 ) ) ;
#231999 = ORIENTED_EDGE ( 'NONE', *, *, #8252, .F. ) ;
#232000 = DIRECTION ( 'NONE',  ( 0.000000000000000000, -0.9126074666063753726, -0.4088369013363320481 ) ) ;
#232001 = VECTOR ( 'NONE', #160859, 1000.000000000000000 ) ;
#232002 = VERTEX_POINT ( 'NONE', #177589 ) ;
#232003 = CARTESIAN_POINT ( 'NONE',  ( -11.59999999999994458, 67.75000000001118394, -25.06452884076210452 ) ) ;
#232004 = DIRECTION ( 'NONE',  ( 0.000000000000000000, 0.000000000000000000, 1.000000000000000000 ) ) ;
#232005 = ORIENTED_EDGE ( 'NONE', *, *, #244257, .F. ) ;
#232006 = ORIENTED_EDGE ( 'NONE', *, *, #95101, .F. ) ;
#232007 = AXIS2_PLACEMENT_3D ( 'NONE', #149616, #87021, #46614 ) ;
#232008 = CARTESIAN_POINT ( 'NONE',  ( -21.44999999999999929, 68.75000000001223555, -148.7731074845244166 ) ) ;
#232009 = EDGE_CURVE ( 'NONE', #110239, #145746, #65901, .T. ) ;
#232010 = VERTEX_POINT ( 'NONE', #101831 ) ;
#232012 = ORIENTED_EDGE ( 'NONE', *, *, #159458, .F. ) ;
#232011 = CARTESIAN_POINT ( 'NONE',  ( 22.40000000000010516, 26.02743912001976767, -254.3139371321012163 ) ) ;
#232013 = VERTEX_POINT ( 'NONE', #257036 ) ;
#232014 = CIRCLE ( 'NONE', #48642, 0.09999999999999939493 ) ;
#232015 = VECTOR ( 'NONE', #48852, 999.9999999999998863 ) ;
#232018 = ORIENTED_EDGE ( 'NONE', *, *, #228286, .T. ) ;
#232017 = EDGE_LOOP ( 'NONE', ( #52397, #176734 ) ) ;
#232016 = DIRECTION ( 'NONE',  ( -0.000000000000000000, 0.4791956752371485107, 0.8777080977375185666 ) ) ;
#232019 = AXIS2_PLACEMENT_3D ( 'NONE', #233702, #56316, #257050 ) ;
#232020 = VECTOR ( 'NONE', #166696, 1000.000000000000000 ) ;
#232021 = DIRECTION ( 'NONE',  ( 2.342056488767301376E-15, -0.1350103645451904977, -0.9908441862701596881 ) ) ;
#232022 = ORIENTED_EDGE ( 'NONE', *, *, #130440, .T. ) ;
#232023 = CARTESIAN_POINT ( 'NONE',  ( -20.94999999999999929, 1.835341550235567887, -112.0551512925630249 ) ) ;
#232025 = ADVANCED_FACE ( 'NONE', ( #141006 ), #198395, .T. ) ;
#232024 = DIRECTION ( 'NONE',  ( 1.000000000000000000, -0.000000000000000000, -0.000000000000000000 ) ) ;
#232026 = DIRECTION ( 'NONE',  ( 0.000000000000000000, -0.8814952561688476074, 0.4721928772777262417 ) ) ;
#232027 = AXIS2_PLACEMENT_3D ( 'NONE', #38976, #239733, #55926 ) ;
#232028 = DIRECTION ( 'NONE',  ( -1.000000000000000000, 0.000000000000000000, 0.000000000000000000 ) ) ;
#232029 = DIRECTION ( 'NONE',  ( 0.000000000000000000, -0.2128009952263606452, 0.9770955615653315052 ) ) ;
#232030 = ORIENTED_EDGE ( 'NONE', *, *, #158165, .F. ) ;
#232031 = ORIENTED_EDGE ( 'NONE', *, *, #72837, .T. ) ;
#232032 = ORIENTED_EDGE ( 'NONE', *, *, #217086, .F. ) ;
#232033 = CARTESIAN_POINT ( 'NONE',  ( -18.39999999999999858, 73.22794484573502416, -249.6559397216816478 ) ) ;
#232035 = ORIENTED_EDGE ( 'NONE', *, *, #12656, .F. ) ;
#232034 = LINE ( 'NONE', #71677, #245306 ) ;
#232036 = FACE_OUTER_BOUND ( 'NONE', #252638, .T. ) ;
#232038 = EDGE_LOOP ( 'NONE', ( #93824, #20576, #4214, #197265, #256745, #44081, #47269, #143014, #243373, #16384, #98424, #95229, #225213, #66173, #249997, #91292 ) ) ;
#232037 = CYLINDRICAL_SURFACE ( 'NONE', #19172, 11.79999999999999361 ) ;
#232039 = VERTEX_POINT ( 'NONE', #237532 ) ;
#232040 = DIRECTION ( 'NONE',  ( -0.000000000000000000, -2.891205793294679805E-16, 1.000000000000000000 ) ) ;
#232041 = VECTOR ( 'NONE', #166989, 1000.000000000000227 ) ;
#232042 = CIRCLE ( 'NONE', #132069, 0.1000000000000048767 ) ;
#232043 = ORIENTED_EDGE ( 'NONE', *, *, #31639, .F. ) ;
#232044 = CARTESIAN_POINT ( 'NONE',  ( -16.83558968593869665, 9.950000000011137047, -180.1623051876166812 ) ) ;
#232045 = DIRECTION ( 'NONE',  ( -0.000000000000000000, 6.982962677686266711E-15, -1.000000000000000000 ) ) ;
#232046 = CIRCLE ( 'NONE', #94648, 0.4999999999999944489 ) ;
#232048 = ORIENTED_EDGE ( 'NONE', *, *, #167737, .T. ) ;
#232047 = ORIENTED_EDGE ( 'NONE', *, *, #156421, .T. ) ;
#232049 = EDGE_LOOP ( 'NONE', ( #154490, #234006, #221049 ) ) ;
#232050 = CARTESIAN_POINT ( 'NONE',  ( -20.54999999999999716, 57.22075589414561136, -237.7098882646457128 ) ) ;
#232051 = ORIENTED_EDGE ( 'NONE', *, *, #128232, .T. ) ;
#232052 = ORIENTED_EDGE ( 'NONE', *, *, #33740, .T. ) ;
#232053 = CARTESIAN_POINT ( 'NONE',  ( 20.94999999999999929, 10.68863688179708049, -222.5873974249508933 ) ) ;
#232055 = ORIENTED_EDGE ( 'NONE', *, *, #111010, .T. ) ;
#232054 = CARTESIAN_POINT ( 'NONE',  ( 18.49999999999999289, 10.20857864376268509, -24.76715728752538226 ) ) ;
#232056 = FACE_OUTER_BOUND ( 'NONE', #12688, .T. ) ;
#232058 = CARTESIAN_POINT ( 'NONE',  ( 20.97239005616513552, 11.27841523495330200, -211.0809943295646747 ) ) ;
#232057 = CARTESIAN_POINT ( 'NONE',  ( 22.39999999999999503, 11.75000000001115552, -66.90000000000004832 ) ) ;
#232059 = CARTESIAN_POINT ( 'NONE',  ( -23.25000000000000000, 87.65000000001172964, -72.62310748452422615 ) ) ;
#232060 = CARTESIAN_POINT ( 'NONE',  ( 18.50000000000000000, -9.399999999988843058, -74.29725975966333351 ) ) ;
#232061 = ORIENTED_EDGE ( 'NONE', *, *, #223462, .F. ) ;
#232062 = EDGE_CURVE ( 'NONE', #136369, #192375, #219230, .T. ) ;
#232063 = EDGE_LOOP ( 'NONE', ( #98887, #134614, #249527, #237563 ) ) ;
#232064 = FACE_OUTER_BOUND ( 'NONE', #47694, .T. ) ;
#232065 = FACE_OUTER_BOUND ( 'NONE', #197402, .T. ) ;
#232066 = LINE ( 'NONE', #53409, #145367 ) ;
#232067 = ADVANCED_FACE ( 'NONE', ( #139682 ), #62743, .T. ) ;
#232068 = ORIENTED_EDGE ( 'NONE', *, *, #74182, .F. ) ;
#232069 = VECTOR ( 'NONE', #251696, 1000.000000000000000 ) ;
#232070 = VECTOR ( 'NONE', #212251, 999.9999999999998863 ) ;
#232071 = CARTESIAN_POINT ( 'NONE',  ( 23.14999999999999503, -0.1830918614494220220, -222.4987906021368360 ) ) ;
#232072 = AXIS2_PLACEMENT_3D ( 'NONE', #179057, #53936, #133479 ) ;
#232073 = AXIS2_PLACEMENT_3D ( 'NONE', #138128, #201982, #97707 ) ;
#232074 = CARTESIAN_POINT ( 'NONE',  ( -18.59999999999999787, 77.83585931145526615, -57.91866831572577468 ) ) ;
#232075 = DIRECTION ( 'NONE',  ( 0.7071067811865127117, 0.7071067811865821007, 0.000000000000000000 ) ) ;
#232076 = ORIENTED_EDGE ( 'NONE', *, *, #110996, .T. ) ;
#232077 = VERTEX_POINT ( 'NONE', #181423 ) ;
#232078 = EDGE_CURVE ( 'NONE', #13363, #9380, #116180, .T. ) ;
#232079 = CARTESIAN_POINT ( 'NONE',  ( -16.77828822508139694, 66.05377062509130326, -123.8604792331504143 ) ) ;
#232080 = ORIENTED_EDGE ( 'NONE', *, *, #152951, .F. ) ;
#232081 = FACE_OUTER_BOUND ( 'NONE', #72679, .T. ) ;
#232082 = ORIENTED_EDGE ( 'NONE', *, *, #101839, .F. ) ;
#232083 = CARTESIAN_POINT ( 'NONE',  ( 18.60000000000000142, -9.480686695267809938, -140.9411151687578752 ) ) ;
#232084 = FACE_OUTER_BOUND ( 'NONE', #155464, .T. ) ;
#232086 = CARTESIAN_POINT ( 'NONE',  ( -21.05000000000000426, -1.335570543289804402, -194.7977936451528080 ) ) ;
#232085 = DIRECTION ( 'NONE',  ( 0.000000000000000000, 1.000000000000000000, 6.982962677686266711E-15 ) ) ;
#232087 = EDGE_CURVE ( 'NONE', #127648, #202516, #245157, .T. ) ;
#232088 = DIRECTION ( 'NONE',  ( 1.000000000000000000, 0.000000000000000000, 0.000000000000000000 ) ) ;
#232089 = CARTESIAN_POINT ( 'NONE',  ( 18.50596464788227280, 65.69367753730708159, -164.5189238066348594 ) ) ;
#232090 = CARTESIAN_POINT ( 'NONE',  ( 21.07888907270776002, 65.27493078649663971, -90.80191389769119326 ) ) ;
#232091 = VECTOR ( 'NONE', #135918, 1000.000000000000000 ) ;
#232092 = ADVANCED_FACE ( 'NONE', ( #238813 ), #132747, .T. ) ;
#232094 = VERTEX_POINT ( 'NONE', #61455 ) ;
#232093 = DIRECTION ( 'NONE',  ( 0.000000000000000000, -0.9955484899852913294, 0.09425075112701486457 ) ) ;
#232096 = EDGE_LOOP ( 'NONE', ( #1156, #237237, #128500, #92714 ) ) ;
#232095 = VERTEX_POINT ( 'NONE', #19778 ) ;
#232097 = CIRCLE ( 'NONE', #119653, 0.09999999999999829858 ) ;
#232098 = ORIENTED_EDGE ( 'NONE', *, *, #107701, .T. ) ;
#232099 = FACE_OUTER_BOUND ( 'NONE', #108497, .T. ) ;
#232100 = DIRECTION ( 'NONE',  ( 0.000000000000000000, 0.4999999999999956701, -0.8660254037844411501 ) ) ;
#232101 = EDGE_CURVE ( 'NONE', #86809, #227337, #11949, .T. ) ;
#232103 = CARTESIAN_POINT ( 'NONE',  ( -22.50000000000000000, 11.64987090377452894, -33.41748010912702682 ) ) ;
#232102 = DIRECTION ( 'NONE',  ( 0.000000000000000000, -0.1350103645451876666, -0.9908441862701600211 ) ) ;
#232104 = DIRECTION ( 'NONE',  ( 0.000000000000000000, -0.2128009952263605342, 0.9770955615653315052 ) ) ;
#232105 = ORIENTED_EDGE ( 'NONE', *, *, #57925, .T. ) ;
#232106 = DIRECTION ( 'NONE',  ( -2.915501640297154283E-16, -0.4088369013363279403, 0.9126074666063770380 ) ) ;
#232107 = VERTEX_POINT ( 'NONE', #180130 ) ;
#232108 = ORIENTED_EDGE ( 'NONE', *, *, #113890, .T. ) ;
#232109 = CARTESIAN_POINT ( 'NONE',  ( -21.05000000000000071, 69.74115727647247809, -69.55512117771243652 ) ) ;
#232110 = PLANE ( 'NONE',  #47463 ) ;
#232111 = FACE_OUTER_BOUND ( 'NONE', #155367, .T. ) ;
#232112 = STYLED_ITEM ( 'NONE', ( #159576 ), #105841 ) ;
#232113 = DIRECTION ( 'NONE',  ( -1.000000000000000000, 0.000000000000000000, 0.000000000000000000 ) ) ;
#232114 = CARTESIAN_POINT ( 'NONE',  ( 21.15000000000005187, 76.00000000001119815, -36.02310748452479316 ) ) ;
#232115 = ORIENTED_EDGE ( 'NONE', *, *, #92317, .T. ) ;
#232116 = EDGE_LOOP ( 'NONE', ( #253566, #104924, #189384, #76490 ) ) ;
#232117 = DIRECTION ( 'NONE',  ( -1.000000000000000000, 0.000000000000000000, -0.000000000000000000 ) ) ;
#232118 = DIRECTION ( 'NONE',  ( 0.000000000000000000, 0.1332476588733448597, -0.9910827722268067408 ) ) ;
#232119 = CARTESIAN_POINT ( 'NONE',  ( 18.39999999999999858, -9.499999999999998224, -40.41465834296967330 ) ) ;
#232120 = CYLINDRICAL_SURFACE ( 'NONE', #197948, 1.749999999999999778 ) ;
#232121 = CARTESIAN_POINT ( 'NONE',  ( -15.75000000000000355, 9.850000000011133849, -50.25000000000000711 ) ) ;
#232122 = AXIS2_PLACEMENT_3D ( 'NONE', #242074, #222494, #218655 ) ;
#232123 = DIRECTION ( 'NONE',  ( 0.7071067811865302533, -0.6909108974501196876, -0.1504730267679053324 ) ) ;
#232124 = DIRECTION ( 'NONE',  ( 0.000000000000000000, 0.000000000000000000, 1.000000000000000000 ) ) ;
#232126 = EDGE_CURVE ( 'NONE', #242379, #181359, #7837, .T. ) ;
#232125 = DIRECTION ( 'NONE',  ( 0.000000000000000000, 4.336808689942043768E-15, -1.000000000000000000 ) ) ;
#232128 = CARTESIAN_POINT ( 'NONE',  ( -21.64999999999999858, 65.95000000001230944, -157.2731074845244166 ) ) ;
#232127 = DIRECTION ( 'NONE',  ( -1.000000000000000000, -1.394253735153569469E-16, -2.602809386958778209E-16 ) ) ;
#232129 = CARTESIAN_POINT ( 'NONE',  ( -23.49999999999994316, 83.90000000001120384, -37.18565239344504647 ) ) ;
#232130 = TOROIDAL_SURFACE ( 'NONE', #119687, 0.2000000000000000111, 0.1000000000000000056 ) ;
#232131 = CARTESIAN_POINT ( 'NONE',  ( 20.89999999999999503, -1.212568896937008089, -8.000000000000000000 ) ) ;
#232132 = CARTESIAN_POINT ( 'NONE',  ( 18.59999999999999787, 7.939498413483247141, -209.7295111514051200 ) ) ;
#232133 = FACE_OUTER_BOUND ( 'NONE', #62842, .T. ) ;
#232134 = AXIS2_PLACEMENT_3D ( 'NONE', #184770, #239627, #180934 ) ;
#232136 = ORIENTED_EDGE ( 'NONE', *, *, #13517, .T. ) ;
#232135 = DIRECTION ( 'NONE',  ( 0.000000000000000000, 1.000000000000000000, 0.000000000000000000 ) ) ;
#232137 = CIRCLE ( 'NONE', #153051, 11.74999999999999645 ) ;
#232138 = PRODUCT_DEFINITION_FORMATION_WITH_SPECIFIED_SOURCE ( 'ANY', '', #168068, .NOT_KNOWN. ) ;
#232139 = ADVANCED_FACE ( 'NONE', ( #221778 ), #257556, .T. ) ;
#232140 = AXIS2_PLACEMENT_3D ( 'NONE', #157019, #74922, #194862 ) ;
#232141 = AXIS2_PLACEMENT_3D ( 'NONE', #38722, #180799, #62134 ) ;
#232142 = ADVANCED_FACE ( 'NONE', ( #78438 ), #166073, .F. ) ;
#232143 = DIRECTION ( 'NONE',  ( 0.000000000000000000, 0.9908441862701605762, 0.1350103645451835310 ) ) ;
#232144 = EDGE_CURVE ( 'NONE', #201306, #50342, #157718, .T. ) ;
#232145 = CARTESIAN_POINT ( 'NONE',  ( 12.25000000000000178, 9.350000000011140955, -83.86426760761612798 ) ) ;
#232146 = DIRECTION ( 'NONE',  ( 0.000000000000000000, 0.5826443254699606999, 0.8127272543711416830 ) ) ;
#232147 = CIRCLE ( 'NONE', #144809, 0.2000000000000057288 ) ;
#232148 = CARTESIAN_POINT ( 'NONE',  ( -23.15000000000000213, -11.74999999998884448, -63.89999999999999858 ) ) ;
#232149 = AXIS2_PLACEMENT_3D ( 'NONE', #107550, #248359, #67151 ) ;
#232150 = DIRECTION ( 'NONE',  ( -0.000000000000000000, 0.1350103645451876666, 0.9908441862701600211 ) ) ;
#232151 = CARTESIAN_POINT ( 'NONE',  ( -16.86132326855786800, 66.05000000001156479, -56.82447169985605484 ) ) ;
#232152 = CIRCLE ( 'NONE', #115599, 2.000000000000001776 ) ;
#232153 = EDGE_LOOP ( 'NONE', ( #212232, #48640, #137080, #151174, #141480, #219638, #67403, #26862, #147942, #161571, #163942, #88290, #238483, #204704, #244576, #211547, #37985, #67505, #101586, #153456, #48703, #95906, #246454, #125433, #214363 ) ) ;
#232154 = FACE_OUTER_BOUND ( 'NONE', #169826, .T. ) ;
#232157 = VERTEX_POINT ( 'NONE', #161863 ) ;
#232156 = FACE_OUTER_BOUND ( 'NONE', #34665, .T. ) ;
#232155 = AXIS2_PLACEMENT_3D ( 'NONE', #96569, #131870, #94013 ) ;
#232158 = DIRECTION ( 'NONE',  ( 1.000000000000000000, -0.000000000000000000, -0.000000000000000000 ) ) ;
#232160 = EDGE_CURVE ( 'NONE', #192532, #142373, #37077, .T. ) ;
#232159 =( BOUNDED_CURVE ( )  B_SPLINE_CURVE ( 3, ( #235854, #138027, #55915, #57201 ),
 .UNSPECIFIED., .F., .F. ) 
 B_SPLINE_CURVE_WITH_KNOTS ( ( 4, 4 ),
 ( 5.731445031868800832, 5.983100554402348337 ),
 .UNSPECIFIED. ) 
 CURVE ( )  GEOMETRIC_REPRESENTATION_ITEM ( )  RATIONAL_B_SPLINE_CURVE ( ( 1.000000000000000000, 0.9947294176030465618, 0.9947294176030465618, 1.000000000000000000 ) ) 
 REPRESENTATION_ITEM ( '' )  );
#232161 = AXIS2_PLACEMENT_3D ( 'NONE', #98822, #59710, #2307 ) ;
#232162 = DIRECTION ( 'NONE',  ( 0.000000000000000000, 0.000000000000000000, -1.000000000000000000 ) ) ;
#232163 = ORIENTED_EDGE ( 'NONE', *, *, #212514, .T. ) ;
#232164 = CARTESIAN_POINT ( 'NONE',  ( -16.80070461187793995, 66.05000000001261640, -190.8761436553694182 ) ) ;
#232165 = EDGE_CURVE ( 'NONE', #97927, #67516, #70402, .T. ) ;
#232166 = SHAPE_DEFINITION_REPRESENTATION ( #105440, #73451 ) ;
#232167 = EDGE_CURVE ( 'NONE', #70441, #99245, #79709, .T. ) ;
#232168 = CARTESIAN_POINT ( 'NONE',  ( -18.59999999999999787, 11.75000000001115552, -67.00000000000000000 ) ) ;
#232169 = CARTESIAN_POINT ( 'NONE',  ( -18.41799967126739901, 85.50000000001189449, -95.99103767126818809 ) ) ;
#232170 = VERTEX_POINT ( 'NONE', #126567 ) ;
#232171 = FACE_OUTER_BOUND ( 'NONE', #173813, .T. ) ;
#232172 = DIRECTION ( 'NONE',  ( 0.000000000000000000, 0.000000000000000000, -1.000000000000000000 ) ) ;
#232173 = CIRCLE ( 'NONE', #61466, 0.09999999999998898659 ) ;
#232174 = AXIS2_PLACEMENT_3D ( 'NONE', #224460, #83633, #223174 ) ;
#232175 = AXIS2_PLACEMENT_3D ( 'NONE', #154550, #153271, #15023 ) ;
#232176 = ADVANCED_FACE ( 'NONE', ( #46999 ), #186915, .F. ) ;
#232177 = DIRECTION ( 'NONE',  ( 1.000000000000000000, 0.000000000000000000, 0.000000000000000000 ) ) ;
#232178 = ORIENTED_EDGE ( 'NONE', *, *, #150270, .F. ) ;
#232179 = ORIENTED_EDGE ( 'NONE', *, *, #188260, .F. ) ;
#232180 = ADVANCED_FACE ( 'NONE', ( #4040 ), #69185, .F. ) ;
#232181 = EDGE_CURVE ( 'NONE', #76942, #64097, #61996, .T. ) ;
#232182 = DIRECTION ( 'NONE',  ( -1.000000000000000000, -0.000000000000000000, -0.000000000000000000 ) ) ;
#232183 = DIRECTION ( 'NONE',  ( 0.000000000000000000, 0.000000000000000000, -1.000000000000000000 ) ) ;
#232185 = AXIS2_PLACEMENT_3D ( 'NONE', #19457, #18163, #181108 ) ;
#232184 = DIRECTION ( 'NONE',  ( -0.000000000000000000, 0.000000000000000000, 1.000000000000000000 ) ) ;
#232186 = DIRECTION ( 'NONE',  ( 1.000000000000000000, 0.000000000000000000, 0.000000000000000000 ) ) ;
#232187 = CIRCLE ( 'NONE', #94786, 0.09999999999999892308 ) ;
#232189 = CARTESIAN_POINT ( 'NONE',  ( -21.29999999999995808, 76.00000000001197975, -107.0731074845243143 ) ) ;
#232188 = CARTESIAN_POINT ( 'NONE',  ( -20.85000000000000142, 75.77017861926654518, -203.7552340087416951 ) ) ;
#232190 = DIRECTION ( 'NONE',  ( 1.000000000000000000, -0.000000000000000000, -0.000000000000000000 ) ) ;
#232191 = AXIS2_PLACEMENT_3D ( 'NONE', #184353, #7009, #24030 ) ;
#232192 = DIRECTION ( 'NONE',  ( 1.000000000000000000, 0.000000000000000000, 0.000000000000000000 ) ) ;
#232193 = DIRECTION ( 'NONE',  ( -1.000000000000000000, 0.000000000000000000, -0.000000000000000000 ) ) ;
#232194 = CARTESIAN_POINT ( 'NONE',  ( 23.24999999999999645, 37.65052946403260137, -247.7000226632887916 ) ) ;
#232195 = ORIENTED_EDGE ( 'NONE', *, *, #257165, .F. ) ;
#232197 = ORIENTED_EDGE ( 'NONE', *, *, #105533, .F. ) ;
#232196 = DIRECTION ( 'NONE',  ( -1.000000000000000000, -0.000000000000000000, 0.000000000000000000 ) ) ;
#232198 = DIRECTION ( 'NONE',  ( 1.000000000000000000, 0.000000000000000000, 0.000000000000000000 ) ) ;
#232199 = FACE_OUTER_BOUND ( 'NONE', #18024, .T. ) ;
#232201 = DIRECTION ( 'NONE',  ( -1.000000000000000000, 0.000000000000000000, -0.000000000000000000 ) ) ;
#232200 = CARTESIAN_POINT ( 'NONE',  ( -20.85000000000000142, 76.00000000001170974, -69.52310748452431710 ) ) ;
#232202 = AXIS2_PLACEMENT_3D ( 'NONE', #94436, #149307, #73629 ) ;
#232203 = ADVANCED_FACE ( 'NONE', ( #224370 ), #23648, .T. ) ;
#232204 = VERTEX_POINT ( 'NONE', #206101 ) ;
#232205 = DIRECTION ( 'NONE',  ( 1.000000000000000000, -0.000000000000000000, -0.000000000000000000 ) ) ;
#232207 = EDGE_CURVE ( 'NONE', #98538, #24198, #24605, .T. ) ;
#232206 = DIRECTION ( 'NONE',  ( 0.000000000000000000, -0.9553114395363127009, 0.2956011730204364252 ) ) ;
#232208 = CARTESIAN_POINT ( 'NONE',  ( -0.8999999999999437339, 64.35000000001120668, -12.72310748452478890 ) ) ;
#232209 = DIRECTION ( 'NONE',  ( 0.000000000000000000, 0.8777080977375072424, -0.4791956752371691608 ) ) ;
#232210 = VERTEX_POINT ( 'NONE', #146120 ) ;
#232211 = CIRCLE ( 'NONE', #48825, 0.09999999999999939493 ) ;
#232212 = ORIENTED_EDGE ( 'NONE', *, *, #124243, .T. ) ;
#232213 = CIRCLE ( 'NONE', #228103, 0.09999999999999939493 ) ;
#232214 = CIRCLE ( 'NONE', #227911, 0.09999999999999992228 ) ;
#232215 = EDGE_CURVE ( 'NONE', #185310, #92859, #45231, .T. ) ;
#232216 = DIRECTION ( 'NONE',  ( 1.000000000000000000, 0.000000000000000000, 0.000000000000000000 ) ) ;
#232217 = CIRCLE ( 'NONE', #111387, 0.1000000000000028644 ) ;
#232218 = ORIENTED_EDGE ( 'NONE', *, *, #86659, .T. ) ;
#232219 = DIRECTION ( 'NONE',  ( -1.000000000000000000, -3.265361837132813093E-16, 0.000000000000000000 ) ) ;
#232220 = AXIS2_PLACEMENT_3D ( 'NONE', #54349, #90912, #173073 ) ;
#232221 = LINE ( 'NONE', #53562, #56147 ) ;
#232222 = CARTESIAN_POINT ( 'NONE',  ( -21.09316766718153247, 65.52597334342877389, -241.9929064490658845 ) ) ;
#232223 = ORIENTED_EDGE ( 'NONE', *, *, #90764, .F. ) ;
#232224 = DIRECTION ( 'NONE',  ( 0.000000000000000000, 0.000000000000000000, -1.000000000000000000 ) ) ;
#232225 = DIRECTION ( 'NONE',  ( 0.000000000000000000, 0.9887567792719341719, -0.1495327102803664099 ) ) ;
#232226 = DIRECTION ( 'NONE',  ( -1.000000000000000000, -0.000000000000000000, -0.000000000000000000 ) ) ;
#232227 = VECTOR ( 'NONE', #174186, 1000.000000000000000 ) ;
#232228 = ADVANCED_FACE ( 'NONE', ( #103128 ), #108292, .T. ) ;
#232229 = CARTESIAN_POINT ( 'NONE',  ( -18.50000000000000000, 11.64999999999999680, 11.75000000000000000 ) ) ;
#232230 = DIRECTION ( 'NONE',  ( -1.000000000000000000, -0.000000000000000000, 0.000000000000000000 ) ) ;
#232232 = DIRECTION ( 'NONE',  ( 0.000000000000000000, 1.734723475976997999E-14, -1.000000000000000000 ) ) ;
#232231 = FACE_OUTER_BOUND ( 'NONE', #116252, .T. ) ;
#232233 = FACE_OUTER_BOUND ( 'NONE', #56938, .T. ) ;
#232234 = ADVANCED_FACE ( 'NONE', ( #204796 ), #141117, .F. ) ;
#232235 = EDGE_LOOP ( 'NONE', ( #22176, #163094, #2334, #81426 ) ) ;
#232237 = DIRECTION ( 'NONE',  ( 1.000000000000000000, 3.265361837132813093E-16, -0.000000000000000000 ) ) ;
#232236 = CARTESIAN_POINT ( 'NONE',  ( 23.24999999999999645, 1.115600667400684642E-11, -167.5000000000000284 ) ) ;
#232238 = VERTEX_POINT ( 'NONE', #86117 ) ;
#232240 = ORIENTED_EDGE ( 'NONE', *, *, #5265, .T. ) ;
#232239 = CYLINDRICAL_SURFACE ( 'NONE', #94202, 0.09999999999999939493 ) ;
#232241 = AXIS2_PLACEMENT_3D ( 'NONE', #104534, #65437, #224511 ) ;
#232242 = ORIENTED_EDGE ( 'NONE', *, *, #109712, .T. ) ;
#232243 = CARTESIAN_POINT ( 'NONE',  ( -16.94107738177415712, 10.01423928514777550, -146.5500000000000114 ) ) ;
#232244 = CARTESIAN_POINT ( 'NONE',  ( 18.55807992284871588, 10.32898536001801659, -72.58266832227644727 ) ) ;
#232245 = LINE ( 'NONE', #37895, #51573 ) ;
#232246 = CARTESIAN_POINT ( 'NONE',  ( 21.05000000000000071, 65.52661458509918191, -128.9444530202758301 ) ) ;
#232247 = VERTEX_POINT ( 'NONE', #6608 ) ;
#232248 = EDGE_CURVE ( 'NONE', #24982, #112457, #28720, .T. ) ;
#232249 = DIRECTION ( 'NONE',  ( 0.000000000000000000, -1.000000000000000000, -0.000000000000000000 ) ) ;
#232250 = CARTESIAN_POINT ( 'NONE',  ( -22.39999999999999858, 1.115600667400684642E-11, -127.7500000000000284 ) ) ;
#232251 = EDGE_CURVE ( 'NONE', #43046, #250008, #191010, .T. ) ;
#232252 = ORIENTED_EDGE ( 'NONE', *, *, #162049, .T. ) ;
#232253 = CARTESIAN_POINT ( 'NONE',  ( -21.04999999999994387, 77.36076146337680370, -43.99645795275012006 ) ) ;
#232254 = EDGE_CURVE ( 'NONE', #204898, #202918, #87422, .T. ) ;
#232255 = CARTESIAN_POINT ( 'NONE',  ( 21.14999999999999503, 76.10000000001276987, -215.1726782920691505 ) ) ;
#232256 = ORIENTED_EDGE ( 'NONE', *, *, #110712, .T. ) ;
#232257 = AXIS2_PLACEMENT_3D ( 'NONE', #222161, #102204, #103506 ) ;
#232258 = CARTESIAN_POINT ( 'NONE',  ( -21.64999999999999858, 65.77012247227901298, -213.5448142138000378 ) ) ;
#232259 = CIRCLE ( 'NONE', #228146, 0.1000000000000008937 ) ;
#232260 = EDGE_CURVE ( 'NONE', #54460, #5643, #111896, .T. ) ;
#232261 = VERTEX_POINT ( 'NONE', #187843 ) ;
#232262 = CARTESIAN_POINT ( 'NONE',  ( 18.59999999999996945, 65.66751761918668251, -97.42826094061121012 ) ) ;
#232265 = ADVANCED_FACE ( 'NONE', ( #203535 ), #24918, .F. ) ;
#232264 = ADVANCED_FACE ( 'NONE', ( #88690 ), #168305, .F. ) ;
#232263 = EDGE_LOOP ( 'NONE', ( #154880, #237884, #103912, #16449 ) ) ;
#232266 = DIRECTION ( 'NONE',  ( 0.000000000000000000, 0.2128009952263403282, -0.9770955615653358350 ) ) ;
#232267 =( BOUNDED_CURVE ( )  B_SPLINE_CURVE ( 3, ( #150960, #171843, #130098, #209646 ),
 .UNSPECIFIED., .F., .T. ) 
 B_SPLINE_CURVE_WITH_KNOTS ( ( 4, 4 ),
 ( 2.589852378279006828, 2.850972632318390154 ),
 .UNSPECIFIED. ) 
 CURVE ( )  GEOMETRIC_REPRESENTATION_ITEM ( )  RATIONAL_B_SPLINE_CURVE ( ( 1.000000000000000000, 0.9943260843901262636, 0.9943260843901262636, 1.000000000000000000 ) ) 
 REPRESENTATION_ITEM ( '' )  );
#232268 = CARTESIAN_POINT ( 'NONE',  ( -18.40000000000000213, 11.47316190337310537, -191.7001707515342446 ) ) ;
#232269 = DIRECTION ( 'NONE',  ( -1.000000000000000000, 0.000000000000000000, 0.000000000000000000 ) ) ;
#232270 = LINE ( 'NONE', #31512, #41201 ) ;
#232271 = AXIS2_PLACEMENT_3D ( 'NONE', #196654, #80533, #96263 ) ;
#232273 = CIRCLE ( 'NONE', #40570, 6.329289321881356400 ) ;
#232272 = CARTESIAN_POINT ( 'NONE',  ( -21.76363531954647357, 0.09900187431060442078, -26.48706345212826108 ) ) ;
#232274 = CARTESIAN_POINT ( 'NONE',  ( 18.40000000000000213, -9.499999999988844479, -73.92214984933046651 ) ) ;
#232275 = DIRECTION ( 'NONE',  ( 0.5932847527679299127, -0.8049926720990051576, 6.366092712777055223E-16 ) ) ;
#232277 = EDGE_LOOP ( 'NONE', ( #114877, #142925, #120771, #60103 ) ) ;
#232276 = ADVANCED_FACE ( 'NONE', ( #32642 ), #74333, .F. ) ;
#232279 = ADVANCED_FACE ( 'NONE', ( #114702 ), #211236, .T. ) ;
#232278 = CARTESIAN_POINT ( 'NONE',  ( -21.05000000000000071, 44.43513953521873106, -247.3415577889845736 ) ) ;
#232280 = ORIENTED_EDGE ( 'NONE', *, *, #149992, .T. ) ;
#232283 = ORIENTED_EDGE ( 'NONE', *, *, #147035, .T. ) ;
#232282 = DIRECTION ( 'NONE',  ( -0.000000000000000000, 0.1350103645451876666, 0.9908441862701600211 ) ) ;
#232281 = FACE_OUTER_BOUND ( 'NONE', #158528, .T. ) ;
#232284 = ORIENTED_EDGE ( 'NONE', *, *, #249633, .F. ) ;
#232285 = CIRCLE ( 'NONE', #82382, 0.09999999999999771572 ) ;
#232286 = DIRECTION ( 'NONE',  ( 0.000000000000000000, 0.2128009952263485993, -0.9770955615653341697 ) ) ;
#232287 = DIRECTION ( 'NONE',  ( -3.265361837132813093E-16, -1.000000000000000000, -6.938893903907229955E-15 ) ) ;
#232288 = EDGE_CURVE ( 'NONE', #195613, #223845, #137005, .T. ) ;
#232289 = CARTESIAN_POINT ( 'NONE',  ( 20.95132126680579887, 59.08861302114610936, -225.8029662872950212 ) ) ;
#232290 = ORIENTED_EDGE ( 'NONE', *, *, #134969, .T. ) ;
#232292 = ORIENTED_EDGE ( 'NONE', *, *, #134290, .F. ) ;
#232291 = CARTESIAN_POINT ( 'NONE',  ( 20.95443524775735256, 67.12144573613981891, -194.9893852089242898 ) ) ;
#232293 = EDGE_CURVE ( 'NONE', #156135, #234219, #71743, .T. ) ;
#232294 = CARTESIAN_POINT ( 'NONE',  ( -21.05000000000000071, -11.48912529306489994, -64.10000000000000853 ) ) ;
#232295 = EDGE_CURVE ( 'NONE', #188235, #141837, #49522, .T. ) ;
#232297 = VERTEX_POINT ( 'NONE', #10474 ) ;
#232296 = CARTESIAN_POINT ( 'NONE',  ( 21.15000000000005187, 76.00000000001119815, -36.02310748452479316 ) ) ;
#232298 = ORIENTED_EDGE ( 'NONE', *, *, #80296, .F. ) ;
#232299 = VECTOR ( 'NONE', #172155, 1000.000000000000000 ) ;
#232300 = VECTOR ( 'NONE', #117807, 1000.000000000000114 ) ;
#232301 = CARTESIAN_POINT ( 'NONE',  ( 20.94999999999999574, 11.84624361595475506, -206.1763227999733203 ) ) ;
#232302 = DIRECTION ( 'NONE',  ( 1.000000000000000000, 0.000000000000000000, 0.000000000000000000 ) ) ;
#232303 = EDGE_LOOP ( 'NONE', ( #50359, #115546, #148374, #197102 ) ) ;
#232304 = DIRECTION ( 'NONE',  ( 0.000000000000000000, -0.9910827722268048534, 0.1332476588733589040 ) ) ;
#232305 = VERTEX_POINT ( 'NONE', #229526 ) ;
#232307 = EDGE_CURVE ( 'NONE', #101496, #99805, #194270, .T. ) ;
#232306 = DIRECTION ( 'NONE',  ( 0.000000000000000000, -0.2617529984165152257, -0.9651348961777124202 ) ) ;
#232308 = DIRECTION ( 'NONE',  ( 1.000000000000000000, 0.000000000000000000, 0.000000000000000000 ) ) ;
#232309 = EDGE_CURVE ( 'NONE', #68656, #246412, #236756, .T. ) ;
#232310 = VECTOR ( 'NONE', #158427, 1000.000000000000000 ) ;
#232311 = VERTEX_POINT ( 'NONE', #30059 ) ;
#232312 = LINE ( 'NONE', #13253, #91614 ) ;
#232313 = CIRCLE ( 'NONE', #82224, 0.9750000000000036415 ) ;
#232314 = EDGE_CURVE ( 'NONE', #228778, #100153, #228597, .T. ) ;
#232315 = VECTOR ( 'NONE', #141487, 1000.000000000000000 ) ;
#232316 = CIRCLE ( 'NONE', #86506, 0.09999999999999939493 ) ;
#232317 = CARTESIAN_POINT ( 'NONE',  ( -20.94999999999999929, 1.115600667400684642E-11, -67.00000000000000000 ) ) ;
#232318 = AXIS2_PLACEMENT_3D ( 'NONE', #184739, #6097, #145609 ) ;
#232319 = ORIENTED_EDGE ( 'NONE', *, *, #47369, .F. ) ;
#232320 = ORIENTED_EDGE ( 'NONE', *, *, #224720, .F. ) ;
#232322 = CARTESIAN_POINT ( 'NONE',  ( 20.51284917709620359, 18.76080927800072828, -228.2665908568477278 ) ) ;
#232321 = CIRCLE ( 'NONE', #65698, 11.65000000000000036 ) ;
#232323 = ORIENTED_EDGE ( 'NONE', *, *, #217194, .F. ) ;
#232325 = EDGE_CURVE ( 'NONE', #210192, #131621, #89991, .T. ) ;
#232324 = SPHERICAL_SURFACE ( 'NONE', #192187, 0.1000000000000000056 ) ;
#232326 = ORIENTED_EDGE ( 'NONE', *, *, #183919, .T. ) ;
#232328 = ORIENTED_EDGE ( 'NONE', *, *, #157557, .T. ) ;
#232327 = CARTESIAN_POINT ( 'NONE',  ( 21.12642695952774119, 75.90109671682263581, -109.3987674065594859 ) ) ;
#232329 = ORIENTED_EDGE ( 'NONE', *, *, #98240, .F. ) ;
#232330 = CARTESIAN_POINT ( 'NONE',  ( 18.59999999999999076, 16.67126802362266247, -222.8016931105129004 ) ) ;
#232331 = ORIENTED_EDGE ( 'NONE', *, *, #91700, .T. ) ;
#232334 = ORIENTED_EDGE ( 'NONE', *, *, #93748, .F. ) ;
#232333 = ORIENTED_EDGE ( 'NONE', *, *, #189571, .F. ) ;
#232332 = CARTESIAN_POINT ( 'NONE',  ( -16.93262454970420094, 65.99797953208121726, -56.95018371076170638 ) ) ;
#232336 = VERTEX_POINT ( 'NONE', #11780 ) ;
#232335 = AXIS2_PLACEMENT_3D ( 'NONE', #211688, #64760, #45200 ) ;
#232337 = EDGE_CURVE ( 'NONE', #85468, #153726, #91219, .T. ) ;
#232338 = CIRCLE ( 'NONE', #99008, 1.749999999999999778 ) ;
#232339 = AXIS2_PLACEMENT_3D ( 'NONE', #42825, #67511, #106617 ) ;
#232340 = LINE ( 'NONE', #250585, #230007 ) ;
#232341 = CIRCLE ( 'NONE', #178172, 0.1000000000000028644 ) ;
#232342 = ORIENTED_EDGE ( 'NONE', *, *, #24957, .T. ) ;
#232343 = CIRCLE ( 'NONE', #244774, 6.329289321881352848 ) ;
#232344 = CARTESIAN_POINT ( 'NONE',  ( 23.04999999999999716, 22.44569914438688940, -231.9288948874669529 ) ) ;
#232346 = ORIENTED_EDGE ( 'NONE', *, *, #19503, .T. ) ;
#232345 = CARTESIAN_POINT ( 'NONE',  ( -23.25000000000000000, -1.149570369564537842, -208.8159124845019221 ) ) ;
#232347 = DIRECTION ( 'NONE',  ( -1.000000000000000000, -2.952720810173289112E-16, 0.000000000000000000 ) ) ;
#232348 = EDGE_LOOP ( 'NONE', ( #51279, #1424, #51659, #168479 ) ) ;
#232349 = AXIS2_PLACEMENT_3D ( 'NONE', #32185, #55530, #16469 ) ;
#232350 = ORIENTED_EDGE ( 'NONE', *, *, #25297, .T. ) ;
#232351 = CARTESIAN_POINT ( 'NONE',  ( 21.46681500598108272, 1.115539681028482333E-11, -160.6424888405743729 ) ) ;
#232352 = CARTESIAN_POINT ( 'NONE',  ( -21.05000000000000071, 64.25000000001219291, -143.5379132551784096 ) ) ;
#232353 = VERTEX_POINT ( 'NONE', #250363 ) ;
#232355 = ORIENTED_EDGE ( 'NONE', *, *, #108021, .F. ) ;
#232354 = DIRECTION ( 'NONE',  ( 0.000000000000000000, 0.8814952561688437216, -0.4721928772777334582 ) ) ;
#232356 = FACE_OUTER_BOUND ( 'NONE', #171621, .T. ) ;
#232357 = VECTOR ( 'NONE', #168933, 1000.000000000000114 ) ;
#232358 = AXIS2_PLACEMENT_3D ( 'NONE', #66236, #68811, #126192 ) ;
#232359 = AXIS2_PLACEMENT_3D ( 'NONE', #257402, #99642, #126945 ) ;
#232361 = ORIENTED_EDGE ( 'NONE', *, *, #193284, .F. ) ;
#232360 = EDGE_LOOP ( 'NONE', ( #197765, #175800, #142479, #66546 ) ) ;
#232362 = EDGE_LOOP ( 'NONE', ( #141533, #9104, #103048, #58479 ) ) ;
#232363 = CARTESIAN_POINT ( 'NONE',  ( -20.64999999999999858, 74.00000000001205080, -123.2984855617622060 ) ) ;
#232364 = ORIENTED_EDGE ( 'NONE', *, *, #149491, .T. ) ;
#232365 = EDGE_LOOP ( 'NONE', ( #22148, #163851, #90462, #156539, #67286 ) ) ;
#232366 = CARTESIAN_POINT ( 'NONE',  ( 11.60000000000006004, 64.35000000001120668, -23.62310748452479103 ) ) ;
#232367 = ORIENTED_EDGE ( 'NONE', *, *, #222249, .F. ) ;
#232368 = CARTESIAN_POINT ( 'NONE',  ( -21.05000000000000071, 10.19179799255971375, -228.2265004863033369 ) ) ;
#232369 = DIRECTION ( 'NONE',  ( 0.000000000000000000, 0.000000000000000000, 1.000000000000000000 ) ) ;
#232370 = VERTEX_POINT ( 'NONE', #251645 ) ;
#232371 = CIRCLE ( 'NONE', #215758, 0.09999999999998898659 ) ;
#232372 = ADVANCED_FACE ( 'NONE', ( #249099 ), #162150, .F. ) ;
#232373 = CIRCLE ( 'NONE', #207432, 0.09999999999999971412 ) ;
#232374 = ORIENTED_EDGE ( 'NONE', *, *, #127465, .F. ) ;
#232375 = CARTESIAN_POINT ( 'NONE',  ( 22.57320508075687115, 12.67709964810647882, -223.3751320524553705 ) ) ;
#232376 = VECTOR ( 'NONE', #229917, 1000.000000000000000 ) ;
#232377 = ORIENTED_EDGE ( 'NONE', *, *, #3950, .F. ) ;
#232378 = VECTOR ( 'NONE', #107278, 1000.000000000000000 ) ;
#232379 = LINE ( 'NONE', #56266, #200768 ) ;
#232380 = EDGE_LOOP ( 'NONE', ( #212399, #69003, #63282, #143981 ) ) ;
#232381 = ORIENTED_EDGE ( 'NONE', *, *, #124889, .T. ) ;
#232382 = EDGE_CURVE ( 'NONE', #20260, #10689, #152581, .T. ) ;
#232383 = DIRECTION ( 'NONE',  ( 0.000000000000000000, -0.2617529984165152257, -0.9651348961777124202 ) ) ;
#232385 = EDGE_LOOP ( 'NONE', ( #247353, #252060, #172778, #148220 ) ) ;
#232384 = CARTESIAN_POINT ( 'NONE',  ( -20.85000000000000142, 18.51199663233067483, -231.2535697180530292 ) ) ;
#232386 = LINE ( 'NONE', #173728, #201138 ) ;
#232387 = DIRECTION ( 'NONE',  ( 1.000000000000000000, 0.000000000000000000, 0.000000000000000000 ) ) ;
#232388 = VECTOR ( 'NONE', #152169, 1000.000000000000000 ) ;
#232389 = DIRECTION ( 'NONE',  ( 1.000000000000000000, 0.000000000000000000, 0.000000000000000000 ) ) ;
#232390 = DIRECTION ( 'NONE',  ( 0.7071067811865475727, -0.7071067811865475727, -4.937700262164531476E-15 ) ) ;
#232391 = CARTESIAN_POINT ( 'NONE',  ( -21.44999999999999929, 7.350000000011155166, -146.3500000000000227 ) ) ;
#232392 = EDGE_CURVE ( 'NONE', #13472, #71999, #242168, .T. ) ;
#232393 = CARTESIAN_POINT ( 'NONE',  ( -21.14999999999999858, 64.35000000001238618, -170.0231074845244166 ) ) ;
#232395 = AXIS2_PLACEMENT_3D ( 'NONE', #184645, #105072, #208090 ) ;
#232394 = CARTESIAN_POINT ( 'NONE',  ( -18.40000000000000213, 11.48667500176882861, -57.75000000000000000 ) ) ;
#232396 = CIRCLE ( 'NONE', #15742, 4.049999999999995381 ) ;
#232397 = DIRECTION ( 'NONE',  ( 0.000000000000000000, 0.000000000000000000, 1.000000000000000000 ) ) ;
#232398 = DIRECTION ( 'NONE',  ( 0.000000000000000000, 0.000000000000000000, -1.000000000000000000 ) ) ;
#232399 = AXIS2_PLACEMENT_3D ( 'NONE', #69661, #246984, #113905 ) ;
#232400 = EDGE_CURVE ( 'NONE', #252282, #183838, #157908, .T. ) ;
#232402 = ORIENTED_EDGE ( 'NONE', *, *, #67321, .F. ) ;
#232401 = CIRCLE ( 'NONE', #74204, 0.09999999999999843736 ) ;
#232403 = ADVANCED_FACE ( 'NONE', ( #19461 ), #241263, .F. ) ;
#232405 = ORIENTED_EDGE ( 'NONE', *, *, #139595, .T. ) ;
#232404 = ORIENTED_EDGE ( 'NONE', *, *, #39528, .F. ) ;
#232406 = ORIENTED_EDGE ( 'NONE', *, *, #211818, .T. ) ;
#232407 = EDGE_CURVE ( 'NONE', #166897, #145909, #124721, .T. ) ;
#232408 = FACE_OUTER_BOUND ( 'NONE', #154141, .T. ) ;
#232409 = CARTESIAN_POINT ( 'NONE',  ( -16.87036670365549895, 10.08494996326643189, -180.0499999999999545 ) ) ;
#232410 = ADVANCED_FACE ( 'NONE', ( #22036 ), #158996, .T. ) ;
#232412 = CARTESIAN_POINT ( 'NONE',  ( 21.05000000000005400, 87.50449464844290048, -37.85861909827351468 ) ) ;
#232411 = LINE ( 'NONE', #212834, #199177 ) ;
#232413 = EDGE_LOOP ( 'NONE', ( #199198, #65479, #256504, #213779 ) ) ;
#232414 = ORIENTED_EDGE ( 'NONE', *, *, #176330, .T. ) ;
#232415 = AXIS2_PLACEMENT_3D ( 'NONE', #29874, #45557, #5106 ) ;
#232416 = CARTESIAN_POINT ( 'NONE',  ( 23.14999999999999858, 4.775700934590591196, -189.1512318959539982 ) ) ;
#232417 = ADVANCED_FACE ( 'NONE', ( #196794 ), #175985, .T. ) ;
#232418 = CARTESIAN_POINT ( 'NONE',  ( -23.25000000000000000, 64.35000000001254250, -182.1731074845244507 ) ) ;
#232419 = CYLINDRICAL_SURFACE ( 'NONE', #170526, 0.09999999999999986677 ) ;
#232420 = ORIENTED_EDGE ( 'NONE', *, *, #151544, .T. ) ;
#232421 = ORIENTED_EDGE ( 'NONE', *, *, #211986, .T. ) ;
#232422 = AXIS2_PLACEMENT_3D ( 'NONE', #193104, #155285, #110989 ) ;
#232423 = CARTESIAN_POINT ( 'NONE',  ( 18.79999999999999716, -1.467286812112899463, 28.00000000000000000 ) ) ;
#232424 = CARTESIAN_POINT ( 'NONE',  ( 18.43565242384934777, 8.780520186313291120, -245.4165333277510115 ) ) ;
#232425 = DIRECTION ( 'NONE',  ( 2.952720810173288126E-16, -0.9770955615653313941, -0.2128009952263603677 ) ) ;
#232427 = EDGE_LOOP ( 'NONE', ( #195104, #144729, #3481, #40809 ) ) ;
#232426 = CARTESIAN_POINT ( 'NONE',  ( 18.39999999999999858, 77.13860723519891849, -241.8264964602989266 ) ) ;
#232428 = DIRECTION ( 'NONE',  ( -0.000000000000000000, -0.9910465087640860649, -0.1335171055202901413 ) ) ;
#232429 = CARTESIAN_POINT ( 'NONE',  ( -18.59999999999999787, 11.65000000001115232, -140.9148057706540271 ) ) ;
#232430 = FACE_OUTER_BOUND ( 'NONE', #212798, .T. ) ;
#232431 = VERTEX_POINT ( 'NONE', #235922 ) ;
#232432 = CARTESIAN_POINT ( 'NONE',  ( 12.60873083341396672, 66.61042836546540968, -85.20546677215523346 ) ) ;
#232433 = DIRECTION ( 'NONE',  ( 1.000000000000000000, 0.000000000000000000, 0.000000000000000000 ) ) ;
#232435 = ADVANCED_FACE ( 'NONE', ( #119863 ), #94271, .T. ) ;
#232434 = CARTESIAN_POINT ( 'NONE',  ( 23.14999999999999858, 78.00000000001244871, -170.0231074845243313 ) ) ;
#232437 = CYLINDRICAL_SURFACE ( 'NONE', #203637, 11.74999999999999112 ) ;
#232436 = DIRECTION ( 'NONE',  ( 0.000000000000000000, 1.000000000000000000, 1.265107689135680095E-16 ) ) ;
#232438 = FACE_OUTER_BOUND ( 'NONE', #237483, .T. ) ;
#232439 = DIRECTION ( 'NONE',  ( 0.000000000000000000, 0.000000000000000000, 1.000000000000000000 ) ) ;
#232440 = AXIS2_PLACEMENT_3D ( 'NONE', #18580, #177680, #113817 ) ;
#232441 = CIRCLE ( 'NONE', #15971, 6.329289321881367059 ) ;
#232442 = AXIS2_PLACEMENT_3D ( 'NONE', #226523, #47902, #247385 ) ;
#232443 = CARTESIAN_POINT ( 'NONE',  ( 23.24999999999999645, 0.000000000000000000, -33.50000000000000000 ) ) ;
#232444 = CARTESIAN_POINT ( 'NONE',  ( 21.14999999999999858, 6.540656951712400691, -33.50000000000000000 ) ) ;
#232445 = AXIS2_PLACEMENT_3D ( 'NONE', #105088, #85524, #86824 ) ;
#232446 = ORIENTED_EDGE ( 'NONE', *, *, #229863, .T. ) ;
#232447 = ORIENTED_EDGE ( 'NONE', *, *, #241587, .F. ) ;
#232448 = EDGE_CURVE ( 'NONE', #64218, #125538, #174655, .T. ) ;
#232449 = CARTESIAN_POINT ( 'NONE',  ( -20.94999999999999929, 77.13501884592258762, -162.3061306010920362 ) ) ;
#232450 = CARTESIAN_POINT ( 'NONE',  ( 13.40000000000000036, -8.250000000000005329, 10.95857864376269575 ) ) ;
#232451 = ORIENTED_EDGE ( 'NONE', *, *, #174455, .T. ) ;
#232452 = DIRECTION ( 'NONE',  ( 0.000000000000000000, 0.9421926911474418631, -0.3350715337779995862 ) ) ;
#232453 = ORIENTED_EDGE ( 'NONE', *, *, #85094, .T. ) ;
#232454 = AXIS2_PLACEMENT_3D ( 'NONE', #209060, #64416, #143938 ) ;
#232455 = CIRCLE ( 'NONE', #40926, 1.500000000000001332 ) ;
#232456 = ORIENTED_EDGE ( 'NONE', *, *, #130895, .F. ) ;
#232457 = CARTESIAN_POINT ( 'NONE',  ( 22.37643362114956247, 7.625789993969535274, -66.90091862631867059 ) ) ;
#232458 = EDGE_LOOP ( 'NONE', ( #115930, #194050, #28280, #140973 ) ) ;
#232459 = EDGE_CURVE ( 'NONE', #67694, #144364, #61144, .T. ) ;
#232460 = AXIS2_PLACEMENT_3D ( 'NONE', #20712, #21992, #216314 ) ;
#232461 = CARTESIAN_POINT ( 'NONE',  ( 18.58685178364169488, -7.675193378770480912, -209.9630017811346079 ) ) ;
#232462 = DIRECTION ( 'NONE',  ( 0.000000000000000000, 0.000000000000000000, -1.000000000000000000 ) ) ;
#232463 = CARTESIAN_POINT ( 'NONE',  ( 18.39999999999999503, 11.75000000001113953, -87.85000000000003695 ) ) ;
#232464 = DIRECTION ( 'NONE',  ( 1.000000000000000000, 0.000000000000000000, 0.000000000000000000 ) ) ;
#232465 = CARTESIAN_POINT ( 'NONE',  ( -21.05000000000000071, 11.60000000001115517, -60.07179676972450011 ) ) ;
#232467 = VERTEX_POINT ( 'NONE', #220236 ) ;
#232466 = CARTESIAN_POINT ( 'NONE',  ( -16.80621392010898774, 30.16774654306749426, -234.7952233516700176 ) ) ;
#232469 = CARTESIAN_POINT ( 'NONE',  ( 18.52928932188133970, 10.27928932189250411, -192.2499999999999716 ) ) ;
#232468 = CARTESIAN_POINT ( 'NONE',  ( 21.05000000000326210, 6.351002464453129548, -199.6318190572282845 ) ) ;
#232470 = ADVANCED_FACE ( 'NONE', ( #243630 ), #237143, .T. ) ;
#232471 = CARTESIAN_POINT ( 'NONE',  ( 14.11444803880196908, 66.54256847116313622, -121.5231905466247042 ) ) ;
#232472 = PLANE ( 'NONE',  #160489 ) ;
#232473 = CARTESIAN_POINT ( 'NONE',  ( -21.45000000000000284, 68.29142135624910281, -81.87310748452436826 ) ) ;
#232474 = VERTEX_POINT ( 'NONE', #24619 ) ;
#232475 = ADVANCED_FACE ( 'NONE', ( #222769 ), #62183, .F. ) ;
#232476 = FACE_OUTER_BOUND ( 'NONE', #108818, .T. ) ;
#232477 = ADVANCED_FACE ( 'NONE', ( #242344 ), #28482, .T. ) ;
#232478 = VERTEX_POINT ( 'NONE', #85802 ) ;
#232479 = DIRECTION ( 'NONE',  ( 1.000000000000000000, 0.000000000000000000, -0.000000000000000000 ) ) ;
#232480 = EDGE_CURVE ( 'NONE', #196163, #255102, #253688, .T. ) ;
#232481 = VERTEX_POINT ( 'NONE', #8877 ) ;
#232482 = AXIS2_PLACEMENT_3D ( 'NONE', #78667, #139922, #120420 ) ;
#232483 = VECTOR ( 'NONE', #253965, 1000.000000000000000 ) ;
#232484 = DIRECTION ( 'NONE',  ( 1.000000000000000000, 0.000000000000000000, 0.000000000000000000 ) ) ;
#232485 = EDGE_CURVE ( 'NONE', #171481, #242741, #182990, .T. ) ;
#232486 = CARTESIAN_POINT ( 'NONE',  ( -18.59999999999999787, 67.23127455305841238, -235.8551265064783991 ) ) ;
#232487 = DIRECTION ( 'NONE',  ( 1.000000000000000000, 0.000000000000000000, 0.000000000000000000 ) ) ;
#232488 = ORIENTED_EDGE ( 'NONE', *, *, #96158, .T. ) ;
#232489 = CIRCLE ( 'NONE', #99347, 0.1000000000000001860 ) ;
#232490 = ORIENTED_EDGE ( 'NONE', *, *, #142950, .F. ) ;
#232491 = DIRECTION ( 'NONE',  ( -1.000000000000000000, 2.849773892568378313E-16, -7.728835255496647986E-17 ) ) ;
#232492 = LINE ( 'NONE', #53833, #227547 ) ;
#232493 = CARTESIAN_POINT ( 'NONE',  ( 20.89192007715128341, 65.67101464000555211, -164.4404391622479977 ) ) ;
#232494 = CARTESIAN_POINT ( 'NONE',  ( 23.14999999999999858, 65.59592694771303911, -232.2046966400529584 ) ) ;
#232496 = DIRECTION ( 'NONE',  ( -0.000000000000000000, -1.000000000000000000, -6.982962677686266711E-15 ) ) ;
#232495 = CARTESIAN_POINT ( 'NONE',  ( 23.25000000000000000, -8.999999999988842703, -57.10603087734755690 ) ) ;
#232497 = VECTOR ( 'NONE', #35406, 1000.000000000000114 ) ;
#232499 = CYLINDRICAL_SURFACE ( 'NONE', #11885, 11.80000000000000959 ) ;
#232498 = AXIS2_PLACEMENT_3D ( 'NONE', #31675, #29122, #128178 ) ;
#232500 = CARTESIAN_POINT ( 'NONE',  ( 12.48201962039796165, 9.376659938544690931, -51.12819254821728521 ) ) ;
#232501 = CARTESIAN_POINT ( 'NONE',  ( -18.79999999999999716, 3.461118860469513336, 28.84309995045515507 ) ) ;
#232502 = VERTEX_POINT ( 'NONE', #47990 ) ;
#232503 = CARTESIAN_POINT ( 'NONE',  ( 20.85000000000000142, 67.23127455305835554, -235.8551265064784559 ) ) ;
#232504 = EDGE_CURVE ( 'NONE', #201514, #250305, #183071, .T. ) ;
#232506 = ORIENTED_EDGE ( 'NONE', *, *, #115804, .F. ) ;
#232505 = LINE ( 'NONE', #115102, #83839 ) ;
#232507 = CARTESIAN_POINT ( 'NONE',  ( -21.14999999999999858, 76.10000000001276987, -215.1726782920691505 ) ) ;
#232508 = AXIS2_PLACEMENT_3D ( 'NONE', #152661, #108376, #91379 ) ;
#232509 = CYLINDRICAL_SURFACE ( 'NONE', #140573, 0.1000000000000026007 ) ;
#232510 = DIRECTION ( 'NONE',  ( 0.000000000000000000, -1.000000000000000000, 0.000000000000000000 ) ) ;
#232511 = EDGE_CURVE ( 'NONE', #227124, #237840, #207940, .T. ) ;
#232513 = ORIENTED_EDGE ( 'NONE', *, *, #229517, .F. ) ;
#232512 = CARTESIAN_POINT ( 'NONE',  ( -15.52965525596987462, 62.33660315667519569, -218.0844802857458262 ) ) ;
#232515 = CARTESIAN_POINT ( 'NONE',  ( -18.40000000000000213, 11.47316190337310893, -57.70017075153427299 ) ) ;
#232514 = APPLICATION_CONTEXT ( 'automotive_design' ) ;
#232517 = EDGE_CURVE ( 'NONE', #22805, #224282, #195474, .T. ) ;
#232516 = CARTESIAN_POINT ( 'NONE',  ( -16.97683809663755028, 51.05165077286171282, -232.2005730747396512 ) ) ;
#232518 = CARTESIAN_POINT ( 'NONE',  ( 21.30000000000002558, 1.115600667400684642E-11, -138.0500000000000114 ) ) ;
#232519 = CARTESIAN_POINT ( 'NONE',  ( 23.15000000000000213, -8.596261682231828516, -124.5498724828497501 ) ) ;
#232520 = CARTESIAN_POINT ( 'NONE',  ( 21.05000000000000071, 65.51556651037061840, -162.5663016830325489 ) ) ;
#232521 = ORIENTED_EDGE ( 'NONE', *, *, #93390, .T. ) ;
#232522 = CARTESIAN_POINT ( 'NONE',  ( 18.39999999999999858, -7.785976468740638090, -209.8926132507865816 ) ) ;
#232523 = AXIS2_PLACEMENT_3D ( 'NONE', #86203, #49674, #186633 ) ;
#232524 = EDGE_LOOP ( 'NONE', ( #59242, #7489, #160095, #128075 ) ) ;
#232525 = EDGE_CURVE ( 'NONE', #202405, #247484, #224055, .T. ) ;
#232526 = DIRECTION ( 'NONE',  ( 0.000000000000000000, -0.2128009952263603954, 0.9770955615653315052 ) ) ;
#232527 = CIRCLE ( 'NONE', #182623, 4.000000000000006217 ) ;
#232528 = VERTEX_POINT ( 'NONE', #127539 ) ;
#232529 = CARTESIAN_POINT ( 'NONE',  ( 0.9000000000000547562, 67.65000000001118963, -10.02310748452479139 ) ) ;
#232530 = CIRCLE ( 'NONE', #7071, 0.09999999999998898659 ) ;
#232531 = ORIENTED_EDGE ( 'NONE', *, *, #53846, .F. ) ;
#232532 = VECTOR ( 'NONE', #241388, 1000.000000000000227 ) ;
#232533 = DIRECTION ( 'NONE',  ( -0.7071067811865475727, -0.6909108974501027012, -0.1504730267679016409 ) ) ;
#232535 = DIRECTION ( 'NONE',  ( -0.000000000000000000, 1.000000000000000000, 6.982962677686266711E-15 ) ) ;
#232534 = VECTOR ( 'NONE', #200901, 1000.000000000000000 ) ;
#232536 = AXIS2_PLACEMENT_3D ( 'NONE', #255742, #114990, #39335 ) ;
#232537 = CIRCLE ( 'NONE', #228426, 0.1000000000000067224 ) ;
#232538 = DIRECTION ( 'NONE',  ( 0.000000000000000000, -1.000000000000000000, -6.982962677686266711E-15 ) ) ;
#232539 = ORIENTED_EDGE ( 'NONE', *, *, #68976, .T. ) ;
#232540 = VECTOR ( 'NONE', #67180, 1000.000000000000227 ) ;
#232541 = DIRECTION ( 'NONE',  ( 0.000000000000000000, -0.6728971962616412394, 0.7397360091703134577 ) ) ;
#232542 = ADVANCED_FACE ( 'NONE', ( #244911 ), #241091, .T. ) ;
#232543 = SPHERICAL_SURFACE ( 'NONE', #49136, 0.1000000000000000056 ) ;
#232544 = DIRECTION ( 'NONE',  ( 0.000000000000000000, 0.8700118002898322711, -0.4930308989875231696 ) ) ;
#232545 = CARTESIAN_POINT ( 'NONE',  ( 21.07928932188134397, 6.162520550847347955, -199.5566553493351307 ) ) ;
#232546 = DIRECTION ( 'NONE',  ( 0.000000000000000000, -1.000000000000000000, 0.000000000000000000 ) ) ;
#232547 = VERTEX_POINT ( 'NONE', #106665 ) ;
#232549 = VECTOR ( 'NONE', #188673, 1000.000000000000114 ) ;
#232548 = CARTESIAN_POINT ( 'NONE',  ( -18.48408745364679362, 85.66432225867526995, -129.8400289511960182 ) ) ;
#232550 = AXIS2_PLACEMENT_3D ( 'NONE', #160952, #57958, #61841 ) ;
#232551 = ORIENTED_EDGE ( 'NONE', *, *, #76044, .T. ) ;
#232553 = ORIENTED_EDGE ( 'NONE', *, *, #194858, .T. ) ;
#232552 = CARTESIAN_POINT ( 'NONE',  ( -37.88850191057539973, 11.75000000000000000, 30.00000000000000000 ) ) ;
#232554 = ORIENTED_EDGE ( 'NONE', *, *, #38462, .F. ) ;
#232555 = DIRECTION ( 'NONE',  ( 0.000000000000000000, -0.000000000000000000, 1.000000000000000000 ) ) ;
#232556 = CARTESIAN_POINT ( 'NONE',  ( 20.95512820512820440, 65.37615131630019505, -128.8581939154367717 ) ) ;
#232557 = DIRECTION ( 'NONE',  ( -0.000000000000000000, 6.982962677686266711E-15, -1.000000000000000000 ) ) ;
#232558 = CARTESIAN_POINT ( 'NONE',  ( -22.45354308602431459, 75.99999978013417490, -81.27354037498388095 ) ) ;
#232559 = ORIENTED_EDGE ( 'NONE', *, *, #253274, .F. ) ;
#232560 = DIRECTION ( 'NONE',  ( -1.000000000000000000, 7.801181613359275410E-16, 1.456333823655510085E-15 ) ) ;
#232561 = DIRECTION ( 'NONE',  ( -0.7071067811865475727, 0.7071067811865475727, 4.937700262164531476E-15 ) ) ;
#232562 = ORIENTED_EDGE ( 'NONE', *, *, #182746, .T. ) ;
#232563 = TOROIDAL_SURFACE ( 'NONE', #119953, 11.65000000000000036, 0.1000000000000000056 ) ;
#232564 = EDGE_CURVE ( 'NONE', #54629, #11411, #199392, .T. ) ;
#232566 = VERTEX_POINT ( 'NONE', #66288 ) ;
#232565 = DIRECTION ( 'NONE',  ( -2.952720810173289112E-16, 1.000000000000000000, 0.000000000000000000 ) ) ;
#232567 = DIRECTION ( 'NONE',  ( -1.000000000000000000, 0.000000000000000000, -3.469446951953635015E-14 ) ) ;
#232568 = AXIS2_PLACEMENT_3D ( 'NONE', #45636, #66478, #174620 ) ;
#232569 = DIRECTION ( 'NONE',  ( -0.000000000000000000, 0.4721928772777345684, 0.8814952561688429444 ) ) ;
#232570 = ADVANCED_FACE ( 'NONE', ( #46701 ), #128821, .F. ) ;
#232571 = VECTOR ( 'NONE', #45834, 1000.000000000000000 ) ;
#232572 = CARTESIAN_POINT ( 'NONE',  ( 20.95512820512820440, 60.90483797576754910, -225.2715357783924333 ) ) ;
#232573 = ORIENTED_EDGE ( 'NONE', *, *, #196466, .F. ) ;
#232574 = ORIENTED_EDGE ( 'NONE', *, *, #179867, .F. ) ;
#232575 = CIRCLE ( 'NONE', #207611, 0.2000000000000057288 ) ;
#232576 = DIRECTION ( 'NONE',  ( 0.000000000000000000, -0.1298341882520124002, -0.9915357197604841577 ) ) ;
#232577 = EDGE_CURVE ( 'NONE', #9313, #26083, #177096, .T. ) ;
#232578 = FACE_OUTER_BOUND ( 'NONE', #138992, .T. ) ;
#232580 = ADVANCED_FACE ( 'NONE', ( #89675 ), #149695, .F. ) ;
#232579 = EDGE_LOOP ( 'NONE', ( #230720, #229150, #203122, #175626, #83563, #69023, #37603 ) ) ;
#232581 = PLANE ( 'NONE',  #188176 ) ;
#232582 = CARTESIAN_POINT ( 'NONE',  ( -22.50000000000094147, -2.381330705637573431, -189.5959759702857923 ) ) ;
#232583 = AXIS2_PLACEMENT_3D ( 'NONE', #201250, #242945, #1759 ) ;
#232584 = CARTESIAN_POINT ( 'NONE',  ( 17.23472005113827876, 12.50908554981958076, -209.9975613761644979 ) ) ;
#232585 = AXIS2_PLACEMENT_3D ( 'NONE', #153267, #213188, #154548 ) ;
#232586 = VECTOR ( 'NONE', #2793, 1000.000000000000000 ) ;
#232587 = AXIS2_PLACEMENT_3D ( 'NONE', #50120, #129666, #87943 ) ;
#232588 = AXIS2_PLACEMENT_3D ( 'NONE', #11690, #220775, #185176 ) ;
#232589 = ADVANCED_FACE ( 'NONE', ( #53130 ), #234389, .F. ) ;
#232590 = EDGE_CURVE ( 'NONE', #220389, #246715, #171839, .T. ) ;
#232591 = ORIENTED_EDGE ( 'NONE', *, *, #44978, .T. ) ;
#232592 = DIRECTION ( 'NONE',  ( 1.000000000000000000, -0.000000000000000000, 0.000000000000000000 ) ) ;
#232593 = EDGE_LOOP ( 'NONE', ( #96770, #208648, #20601, #81668 ) ) ;
#232594 = CARTESIAN_POINT ( 'NONE',  ( -20.94999999999999574, 11.62071067812980907, -60.13158334765903845 ) ) ;
#232595 = DIRECTION ( 'NONE',  ( -1.000000000000000000, 0.000000000000000000, 0.000000000000000000 ) ) ;
#232597 = ORIENTED_EDGE ( 'NONE', *, *, #192121, .T. ) ;
#232596 = CARTESIAN_POINT ( 'NONE',  ( 21.05000000000000071, 85.00000000001197975, -112.9170766071766820 ) ) ;
#232598 = DIRECTION ( 'NONE',  ( 1.000000000000000000, -0.000000000000000000, 0.000000000000000000 ) ) ;
#232599 = CARTESIAN_POINT ( 'NONE',  ( 18.59999999999999432, 74.83729825007462466, -195.5231074845243597 ) ) ;
#232600 = DIRECTION ( 'NONE',  ( -0.000000000000000000, 0.1350103645451807555, 0.9908441862701610203 ) ) ;
#232601 = CARTESIAN_POINT ( 'NONE',  ( 5.900000000000059863, 64.65000000001120384, -25.92310748452479174 ) ) ;
#232602 = DIRECTION ( 'NONE',  ( 1.000000000000000000, -0.000000000000000000, 0.000000000000000000 ) ) ;
#232603 = CIRCLE ( 'NONE', #228491, 12.87499999999999822 ) ;
#232604 = CYLINDRICAL_SURFACE ( 'NONE', #151519, 0.1000000000000028644 ) ;
#232606 = EDGE_CURVE ( 'NONE', #169810, #121432, #3920, .T. ) ;
#232605 = CARTESIAN_POINT ( 'NONE',  ( 18.79999999999999361, -11.65000000000000036, 30.09999999999999787 ) ) ;
#232608 = ORIENTED_EDGE ( 'NONE', *, *, #255549, .T. ) ;
#232607 = DIRECTION ( 'NONE',  ( 0.000000000000000000, 0.2617529984165033463, 0.9651348961777157509 ) ) ;
#232609 = EDGE_CURVE ( 'NONE', #34173, #80924, #149681, .T. ) ;
#232610 = DIRECTION ( 'NONE',  ( 1.000000000000000000, 0.000000000000000000, -0.000000000000000000 ) ) ;
#232612 = EDGE_CURVE ( 'NONE', #69236, #204898, #37243, .T. ) ;
#232611 = CARTESIAN_POINT ( 'NONE',  ( -18.36973785203555920, 16.37308737817262028, -222.2525688661744709 ) ) ;
#232613 = CARTESIAN_POINT ( 'NONE',  ( 20.85000000000000142, -11.74999999998883560, -198.0999999999999659 ) ) ;
#232614 = EDGE_LOOP ( 'NONE', ( #168824, #48953, #145766, #34739 ) ) ;
#232615 = DIRECTION ( 'NONE',  ( 0.000000000000000000, 0.2128009952263678062, -0.9770955615653298398 ) ) ;
#232616 = CARTESIAN_POINT ( 'NONE',  ( -20.64999999999999858, 76.00000000001213607, -136.5231074845243313 ) ) ;
#232617 = CYLINDRICAL_SURFACE ( 'NONE', #240877, 0.09999999999998898659 ) ;
#232618 = EDGE_CURVE ( 'NONE', #188307, #154382, #124540, .T. ) ;
#232619 = AXIS2_PLACEMENT_3D ( 'NONE', #36586, #170975, #136927 ) ;
#232620 = VECTOR ( 'NONE', #213098, 1000.000000000000000 ) ;
#232621 = VERTEX_POINT ( 'NONE', #231787 ) ;
#232622 = CIRCLE ( 'NONE', #141201, 0.1000000000000094008 ) ;
#232623 = CARTESIAN_POINT ( 'NONE',  ( 18.59999999999999076, 28.91254064196106910, -237.8576372133405528 ) ) ;
#232624 = CARTESIAN_POINT ( 'NONE',  ( -21.53752568617661467, 60.65518257771915245, -234.1741829020439241 ) ) ;
#232625 = ORIENTED_EDGE ( 'NONE', *, *, #198811, .T. ) ;
#232626 = CARTESIAN_POINT ( 'NONE',  ( 18.59999999999999787, 5.900000000011102586, -177.7190997646563915 ) ) ;
#232627 = ORIENTED_EDGE ( 'NONE', *, *, #21165, .F. ) ;
#232628 = ADVANCED_FACE ( 'NONE', ( #188789 ), #132681, .T. ) ;
#232630 = ORIENTED_EDGE ( 'NONE', *, *, #33008, .T. ) ;
#232629 = DIRECTION ( 'NONE',  ( -1.000000000000000000, 0.000000000000000000, 0.000000000000000000 ) ) ;
#232631 = CARTESIAN_POINT ( 'NONE',  ( -22.39999999999999858, 1.115600667400684642E-11, -60.75000000000004974 ) ) ;
#232632 = EDGE_LOOP ( 'NONE', ( #88555, #2693, #152577, #43079, #229518 ) ) ;
#232633 = CARTESIAN_POINT ( 'NONE',  ( -18.59999999999999787, 21.17283678855158513, -243.7231193059830332 ) ) ;
#232634 = TOROIDAL_SURFACE ( 'NONE', #7768, 4.149999999999999467, 0.1000000000000000056 ) ;
#232635 = AXIS2_PLACEMENT_3D ( 'NONE', #10473, #153883, #150003 ) ;
#232636 = EDGE_LOOP ( 'NONE', ( #252169, #53862, #245195, #77798 ) ) ;
#232638 = VERTEX_POINT ( 'NONE', #252605 ) ;
#232637 = ORIENTED_EDGE ( 'NONE', *, *, #151471, .F. ) ;
#232639 = CARTESIAN_POINT ( 'NONE',  ( 18.39999999999999503, 15.91777359887373500, -218.8720307647289758 ) ) ;
#232641 = ORIENTED_EDGE ( 'NONE', *, *, #119823, .F. ) ;
#232640 = CARTESIAN_POINT ( 'NONE',  ( 23.14999999999999858, 1.115600667400684642E-11, -167.5000000000000284 ) ) ;
#232642 = CARTESIAN_POINT ( 'NONE',  ( -21.05000000000000071, -1.162701749926853712, -108.5000000000000426 ) ) ;
#232643 = ORIENTED_EDGE ( 'NONE', *, *, #198071, .T. ) ;
#232644 = AXIS2_PLACEMENT_3D ( 'NONE', #138999, #218556, #119489 ) ;
#232645 = ORIENTED_EDGE ( 'NONE', *, *, #130909, .F. ) ;
#232646 = DIRECTION ( 'NONE',  ( -1.000000000000000000, 0.000000000000000000, -0.000000000000000000 ) ) ;
#232647 = CARTESIAN_POINT ( 'NONE',  ( 22.01447462590973458, 75.90096299995218487, -76.78690768575422965 ) ) ;
#232648 = DIRECTION ( 'NONE',  ( 0.000000000000000000, 0.8814952561688416122, -0.4721928772777371219 ) ) ;
#232649 = ORIENTED_EDGE ( 'NONE', *, *, #217735, .T. ) ;
#232650 = FACE_OUTER_BOUND ( 'NONE', #17743, .T. ) ;
#232651 = DIRECTION ( 'NONE',  ( 0.000000000000000000, 1.000000000000000000, 6.982962677686266711E-15 ) ) ;
#232652 = LINE ( 'NONE', #171412, #227014 ) ;
#232653 = ORIENTED_EDGE ( 'NONE', *, *, #116759, .F. ) ;
#232654 = CARTESIAN_POINT ( 'NONE',  ( 21.05000000000000071, 77.83534155023599510, -57.96795619196132776 ) ) ;
#232655 = CARTESIAN_POINT ( 'NONE',  ( -18.48179518609190808, 38.23768179355963071, -261.1947912001946861 ) ) ;
#232656 = CARTESIAN_POINT ( 'NONE',  ( 13.99999999999999822, 9.849999999999981881, -16.74999999999999645 ) ) ;
#232657 = AXIS2_PLACEMENT_3D ( 'NONE', #7268, #129788, #11136 ) ;
#232658 = VERTEX_POINT ( 'NONE', #74021 ) ;
#232659 = LINE ( 'NONE', #59096, #159579 ) ;
#232660 = ORIENTED_EDGE ( 'NONE', *, *, #28576, .F. ) ;
#232661 = CARTESIAN_POINT ( 'NONE',  ( -22.39999999999999858, 31.80471377451587500, -238.9601694054148027 ) ) ;
#232662 = ORIENTED_EDGE ( 'NONE', *, *, #127667, .F. ) ;
#232663 = CONICAL_SURFACE ( 'NONE', #170146, 6.250000000000010658, 0.7853981633974431720 ) ;
#232664 = CARTESIAN_POINT ( 'NONE',  ( -21.05000000000000071, 44.09392520544991356, -258.8097135244738638 ) ) ;
#232665 = ORIENTED_EDGE ( 'NONE', *, *, #149124, .F. ) ;
#232666 = ORIENTED_EDGE ( 'NONE', *, *, #257400, .F. ) ;
#232667 = CARTESIAN_POINT ( 'NONE',  ( 18.49999999999999289, 7.021664781911246322, -204.8335654018972605 ) ) ;
#232668 = CARTESIAN_POINT ( 'NONE',  ( -16.94132844910802405, 9.992436755191501874, -188.3962017559823039 ) ) ;
#232669 = ORIENTED_EDGE ( 'NONE', *, *, #246009, .T. ) ;
#232670 = AXIS2_PLACEMENT_3D ( 'NONE', #232208, #53550, #150104 ) ;
#232671 = EDGE_LOOP ( 'NONE', ( #157465, #58257, #184158, #89652 ) ) ;
#232672 = EDGE_LOOP ( 'NONE', ( #172842, #173302, #206055, #209703 ) ) ;
#232673 = EDGE_CURVE ( 'NONE', #249430, #59785, #137180, .T. ) ;
#232674 = AXIS2_PLACEMENT_3D ( 'NONE', #96594, #256929, #78330 ) ;
#232675 = CIRCLE ( 'NONE', #3697, 11.80000000000000249 ) ;
#232677 = EDGE_LOOP ( 'NONE', ( #1271, #116189, #199954, #44923, #173379, #224232, #95611 ) ) ;
#232676 = AXIS2_PLACEMENT_3D ( 'NONE', #65153, #156913, #165563 ) ;
#232679 = CARTESIAN_POINT ( 'NONE',  ( -22.39999999999999858, -0.1008583690875579364, -88.75043287651064361 ) ) ;
#232678 = CIRCLE ( 'NONE', #111876, 0.09999999999999939493 ) ;
#232680 = DIRECTION ( 'NONE',  ( 0.000000000000000000, 0.9126074666063773710, 0.4088369013363274962 ) ) ;
#232681 = CARTESIAN_POINT ( 'NONE',  ( 20.85000000000000142, 77.83585931145570669, -125.0186683157258045 ) ) ;
#232682 = ORIENTED_EDGE ( 'NONE', *, *, #237852, .T. ) ;
#232683 = AXIS2_PLACEMENT_3D ( 'NONE', #56602, #59167, #198716 ) ;
#232685 = VECTOR ( 'NONE', #66367, 1000.000000000000227 ) ;
#232684 = CARTESIAN_POINT ( 'NONE',  ( -21.05000000000000071, 3.047642603966940200, -208.5984958277594785 ) ) ;
#232686 = ADVANCED_FACE ( 'NONE', ( #193942 ), #216110, .T. ) ;
#232687 = CARTESIAN_POINT ( 'NONE',  ( -21.65000000000000213, 68.75000000001207923, -123.8731074845243540 ) ) ;
#232688 = DIRECTION ( 'NONE',  ( -0.000000000000000000, -0.000000000000000000, 1.000000000000000000 ) ) ;
#232690 = CARTESIAN_POINT ( 'NONE',  ( -20.94999999999999929, -11.64999999998884483, -64.00000000000000000 ) ) ;
#232689 = CARTESIAN_POINT ( 'NONE',  ( 23.24999999999999645, 8.822561741666397950, -9.250000000000001776 ) ) ;
#232691 = LINE ( 'NONE', #69766, #174344 ) ;
#232692 = CARTESIAN_POINT ( 'NONE',  ( 18.50000000000000000, -9.399999999988843058, -107.7972597596633193 ) ) ;
#232693 = AXIS2_PLACEMENT_3D ( 'NONE', #20889, #239919, #46815 ) ;
#232694 = CARTESIAN_POINT ( 'NONE',  ( -21.13422380239012810, 76.00000000001243450, -176.5164339993298483 ) ) ;
#232695 = VERTEX_POINT ( 'NONE', #60818 ) ;
#232696 = AXIS2_PLACEMENT_3D ( 'NONE', #216673, #255757, #43182 ) ;
#232697 = VECTOR ( 'NONE', #90070, 1000.000000000000000 ) ;
#232698 = AXIS2_PLACEMENT_3D ( 'NONE', #91286, #189096, #169578 ) ;
#232699 = CIRCLE ( 'NONE', #195303, 0.1000000000000028644 ) ;
#232700 = EDGE_CURVE ( 'NONE', #168131, #255533, #74688, .T. ) ;
#232702 = ORIENTED_EDGE ( 'NONE', *, *, #84595, .F. ) ;
#232701 = SPHERICAL_SURFACE ( 'NONE', #248876, 0.1000000000000000056 ) ;
#232703 = ADVANCED_FACE ( 'NONE', ( #178245 ), #236900, .F. ) ;
#232704 = CIRCLE ( 'NONE', #153640, 0.9750000000000036415 ) ;
#232705 = DIRECTION ( 'NONE',  ( -6.938893903906983515E-14, -0.9394191166662618775, -0.3427706569150580362 ) ) ;
#232706 = ADVANCED_FACE ( 'NONE', ( #135219 ), #156118, .F. ) ;
#232707 = CARTESIAN_POINT ( 'NONE',  ( 21.05000000000000071, 76.00000000001212186, -134.6231074845243256 ) ) ;
#232708 = ORIENTED_EDGE ( 'NONE', *, *, #74921, .F. ) ;
#232709 = CARTESIAN_POINT ( 'NONE',  ( -16.87665923198281348, 63.08573235307424198, -213.1276215869287967 ) ) ;
#232710 = EDGE_CURVE ( 'NONE', #122105, #16882, #80365, .T. ) ;
#232711 = PRODUCT_DEFINITION_SHAPE ( 'NONE', 'NONE',  #2194 ) ;
#232712 = CARTESIAN_POINT ( 'NONE',  ( -18.59999999999999787, 12.87592094156238609, -205.3750039893633073 ) ) ;
#232713 = CIRCLE ( 'NONE', #99404, 0.1000000000000024342 ) ;
#232714 = VERTEX_POINT ( 'NONE', #239483 ) ;
#232715 = DIRECTION ( 'NONE',  ( -0.000000000000000000, -6.982962677686266711E-15, 1.000000000000000000 ) ) ;
#232716 = DIRECTION ( 'NONE',  ( -0.000000000000000000, -6.982962677686266711E-15, 1.000000000000000000 ) ) ;
#232717 = ADVANCED_FACE ( 'NONE', ( #36155 ), #178743, .T. ) ;
#232718 = CARTESIAN_POINT ( 'NONE',  ( 21.05000000000000071, 1.835341550235569663, -78.55515129256303908 ) ) ;
#232720 = EDGE_LOOP ( 'NONE', ( #602, #218341, #222678 ) ) ;
#232719 = CARTESIAN_POINT ( 'NONE',  ( 26.01805557925458956, 8.624264858734573380, -347.0000000000001137 ) ) ;
#232721 = LINE ( 'NONE', #199709, #99653 ) ;
#232723 = ORIENTED_EDGE ( 'NONE', *, *, #10570, .T. ) ;
#232722 = DIRECTION ( 'NONE',  ( 0.000000000000000000, 0.7965107556683636014, -0.6046243595031649543 ) ) ;
#232724 = AXIS2_PLACEMENT_3D ( 'NONE', #75639, #255483, #177319 ) ;
#232725 = CARTESIAN_POINT ( 'NONE',  ( -21.05000000000000071, 10.05878724559879167, -228.1891859451582434 ) ) ;
#232726 = FACE_OUTER_BOUND ( 'NONE', #177090, .T. ) ;
#232727 = DIRECTION ( 'NONE',  ( 2.933373889701419960E-15, -0.8164989248600479366, 0.5773469543544730298 ) ) ;
#232728 = AXIS2_PLACEMENT_3D ( 'NONE', #26351, #245400, #225798 ) ;
#232730 = ADVANCED_FACE ( 'NONE', ( #219907 ), #8027, .F. ) ;
#232729 = DIRECTION ( 'NONE',  ( 1.000000000000000000, 0.000000000000000000, 0.000000000000000000 ) ) ;
#232732 = CARTESIAN_POINT ( 'NONE',  ( 20.85000000000000142, 67.23127455305835554, -235.8551265064784559 ) ) ;
#232731 = CARTESIAN_POINT ( 'NONE',  ( -16.87998658237741978, 9.950000000011137047, -154.6363604322605454 ) ) ;
#232733 = CARTESIAN_POINT ( 'NONE',  ( -23.25000000000000000, 10.33248238082518711, -39.09484654391314962 ) ) ;
#232734 = CIRCLE ( 'NONE', #186760, 6.329289321881356400 ) ;
#232735 = DIRECTION ( 'NONE',  ( -1.000000000000000000, 0.000000000000000000, 0.000000000000000000 ) ) ;
#232736 = CARTESIAN_POINT ( 'NONE',  ( 23.14999999999999503, 23.38726701055792745, -229.1122755113798348 ) ) ;
#232737 = DIRECTION ( 'NONE',  ( 1.000000000000000000, 0.000000000000000000, 0.000000000000000000 ) ) ;
#232738 = DIRECTION ( 'NONE',  ( 0.000000000000000000, 1.000000000000000000, -6.308085367188393199E-16 ) ) ;
#232740 = ORIENTED_EDGE ( 'NONE', *, *, #175324, .T. ) ;
#232739 = AXIS2_PLACEMENT_3D ( 'NONE', #150616, #230146, #21396 ) ;
#232741 = CARTESIAN_POINT ( 'NONE',  ( -17.78241384942103309, 10.85557575279231735, -77.24903767246566133 ) ) ;
#232742 = ORIENTED_EDGE ( 'NONE', *, *, #6766, .T. ) ;
#232743 = ORIENTED_EDGE ( 'NONE', *, *, #8325, .F. ) ;
#232744 = CARTESIAN_POINT ( 'NONE',  ( -22.50000000000000000, 76.00000000001246292, -181.6726782920691505 ) ) ;
#232745 = CARTESIAN_POINT ( 'NONE',  ( 23.24999999999999645, 64.25000000001233502, -160.7731074845244450 ) ) ;
#232746 = ORIENTED_EDGE ( 'NONE', *, *, #93427, .T. ) ;
#232747 = VECTOR ( 'NONE', #209046, 1000.000000000000000 ) ;
#232748 = AXIS2_PLACEMENT_3D ( 'NONE', #189158, #150050, #229576 ) ;
#232749 = EDGE_LOOP ( 'NONE', ( #181472, #198322, #4919, #156769 ) ) ;
#232750 = VECTOR ( 'NONE', #93101, 1000.000000000000000 ) ;
#232751 = CARTESIAN_POINT ( 'NONE',  ( -21.05000000000000071, 30.68987205111127636, -252.2252246220829193 ) ) ;
#232752 = ORIENTED_EDGE ( 'NONE', *, *, #206524, .T. ) ;
#232753 = ORIENTED_EDGE ( 'NONE', *, *, #240549, .T. ) ;
#232754 = ADVANCED_FACE ( 'NONE', ( #98632 ), #256398, .T. ) ;
#232755 = DIRECTION ( 'NONE',  ( 1.000000000000000000, 0.000000000000000000, 0.000000000000000000 ) ) ;
#232756 = CARTESIAN_POINT ( 'NONE',  ( 20.95262331984753956, 10.50415726280101758, -41.06088832959332535 ) ) ;
#232757 = CARTESIAN_POINT ( 'NONE',  ( -23.25000000000000000, 71.75000000001253397, -182.3731074845244109 ) ) ;
#232758 = EDGE_CURVE ( 'NONE', #30729, #4626, #153808, .T. ) ;
#232759 = CARTESIAN_POINT ( 'NONE',  ( 19.58285714285715073, 10.38499851036257837, -41.12968466738995232 ) ) ;
#232760 = CARTESIAN_POINT ( 'NONE',  ( 13.54556439290364445, 9.450592112133699985, -15.05618831880839181 ) ) ;
#232762 = DIRECTION ( 'NONE',  ( -7.304098846218201720E-16, 1.000000000000000000, 0.000000000000000000 ) ) ;
#232761 = DIRECTION ( 'NONE',  ( 0.5932847527679299127, 0.7769265190100951290, -0.2107092456252281365 ) ) ;
#232763 = CARTESIAN_POINT ( 'NONE',  ( 18.50000000000094502, 10.44006789215635322, -58.26711774888727291 ) ) ;
#232765 = EDGE_LOOP ( 'NONE', ( #18695, #28506, #111757, #75107 ) ) ;
#232764 = CARTESIAN_POINT ( 'NONE',  ( 20.95000000000000284, 64.40000000001194280, -109.9513107147998880 ) ) ;
#232767 = CARTESIAN_POINT ( 'NONE',  ( -18.59999999999999787, 76.00000000001244871, -170.0231074845243597 ) ) ;
#232766 = DIRECTION ( 'NONE',  ( 1.000000000000000000, 0.000000000000000000, 0.000000000000000000 ) ) ;
#232768 = EDGE_CURVE ( 'NONE', #11074, #105460, #124903, .T. ) ;
#232769 = DIRECTION ( 'NONE',  ( -3.265361837132814079E-16, 0.4721928772777359007, 0.8814952561688425003 ) ) ;
#232770 = EDGE_CURVE ( 'NONE', #137676, #257876, #79090, .T. ) ;
#232771 = ORIENTED_EDGE ( 'NONE', *, *, #117934, .T. ) ;
#232772 = CARTESIAN_POINT ( 'NONE',  ( -18.49999999999999645, -9.321008403350157678, -174.7359382490778330 ) ) ;
#232773 = VECTOR ( 'NONE', #169082, 1000.000000000000000 ) ;
#232774 = CARTESIAN_POINT ( 'NONE',  ( 21.10710606213542562, 8.776894023904366904, -146.2409965263994422 ) ) ;
#232775 = DIRECTION ( 'NONE',  ( -1.000000000000000000, -0.000000000000000000, -0.000000000000000000 ) ) ;
#232776 = EDGE_LOOP ( 'NONE', ( #166250, #63623, #39053, #71047 ) ) ;
#232777 = EDGE_CURVE ( 'NONE', #171947, #9869, #62360, .T. ) ;
#232778 = DIRECTION ( 'NONE',  ( 1.000000000000000000, -7.125593699324843413E-30, 1.020425574104004196E-15 ) ) ;
#232779 = EDGE_CURVE ( 'NONE', #89072, #58688, #183170, .T. ) ;
#232780 = DIRECTION ( 'NONE',  ( 0.000000000000000000, 0.000000000000000000, 1.000000000000000000 ) ) ;
#232781 = CARTESIAN_POINT ( 'NONE',  ( 12.25000000000000178, 66.65000000001188596, -86.50158811269930936 ) ) ;
#232783 = EDGE_CURVE ( 'NONE', #221539, #195077, #91582, .T. ) ;
#232782 = ADVANCED_FACE ( 'NONE', ( #827 ), #162526, .T. ) ;
#232784 = VERTEX_POINT ( 'NONE', #21718 ) ;
#232785 = ORIENTED_EDGE ( 'NONE', *, *, #244241, .F. ) ;
#232786 = CARTESIAN_POINT ( 'NONE',  ( -20.64999999999999858, 6.878457983866232972, -212.1414458560986986 ) ) ;
#232787 = ADVANCED_FACE ( 'NONE', ( #244596 ), #63386, .F. ) ;
#232788 = CARTESIAN_POINT ( 'NONE',  ( -18.44085059012131822, 64.48598750652851663, -160.7634128036459913 ) ) ;
#232789 = DIRECTION ( 'NONE',  ( -1.000000000000000000, 2.849773892568378313E-16, -7.728835255496647986E-17 ) ) ;
#232790 = DIRECTION ( 'NONE',  ( -0.7071067811865463515, -0.7071067811865487940, -4.937700262164540154E-15 ) ) ;
#232791 = ORIENTED_EDGE ( 'NONE', *, *, #190396, .T. ) ;
#232792 = CARTESIAN_POINT ( 'NONE',  ( 12.47034474403012538, 47.30882569885141464, -234.5067857460874166 ) ) ;
#232793 = ADVANCED_FACE ( 'NONE', ( #243310 ), #12492, .F. ) ;
#232794 = CARTESIAN_POINT ( 'NONE',  ( -22.49999999999999645, 64.25043287652299284, -170.1239658536231616 ) ) ;
#232795 = DIRECTION ( 'NONE',  ( -0.000000000000000000, -1.000000000000000000, -6.982962677686266711E-15 ) ) ;
#232796 = CIRCLE ( 'NONE', #195386, 0.09999999999999344136 ) ;
#232797 = DIRECTION ( 'NONE',  ( 0.000000000000000000, 0.9126074666063660468, 0.4088369013363524762 ) ) ;
#232798 = AXIS2_PLACEMENT_3D ( 'NONE', #228527, #49867, #208948 ) ;
#232799 = ADVANCED_FACE ( 'NONE', ( #65970 ), #133100, .F. ) ;
#232800 = CIRCLE ( 'NONE', #120386, 0.1000000000000021844 ) ;
#232802 = ADVANCED_FACE ( 'NONE', ( #222443 ), #185914, .F. ) ;
#232801 = CIRCLE ( 'NONE', #62096, 0.6000000000000033085 ) ;
#232803 = CARTESIAN_POINT ( 'NONE',  ( -18.79999999999999716, -11.65000000000000036, -15.00000000000000000 ) ) ;
#232804 = EDGE_CURVE ( 'NONE', #4264, #205992, #74521, .T. ) ;
#232805 = VERTEX_POINT ( 'NONE', #47667 ) ;
#232806 = VECTOR ( 'NONE', #221834, 1000.000000000000000 ) ;
#232807 = DIRECTION ( 'NONE',  ( 0.000000000000000000, 0.000000000000000000, 1.000000000000000000 ) ) ;
#232808 = DIRECTION ( 'NONE',  ( -1.000000000000000000, 0.000000000000000000, 0.000000000000000000 ) ) ;
#232809 = CARTESIAN_POINT ( 'NONE',  ( -11.60000000000000320, -11.75000000000000000, 15.00000000000000355 ) ) ;
#232810 = CYLINDRICAL_SURFACE ( 'NONE', #142008, 0.09999999999999939493 ) ;
#232811 = ADVANCED_FACE ( 'NONE', ( #7267 ), #203995, .T. ) ;
#232813 = ORIENTED_EDGE ( 'NONE', *, *, #138525, .F. ) ;
#232812 = FACE_OUTER_BOUND ( 'NONE', #33045, .T. ) ;
#232814 = DIRECTION ( 'NONE',  ( 0.000000000000000000, -6.982962677686266711E-15, 1.000000000000000000 ) ) ;
#232815 = EDGE_CURVE ( 'NONE', #226515, #246507, #123382, .T. ) ;
#232816 = CARTESIAN_POINT ( 'NONE',  ( 18.59999999999999787, 5.900000000011102586, -77.21909976465646253 ) ) ;
#232817 = CARTESIAN_POINT ( 'NONE',  ( -18.59999999999999787, 64.35000000001208775, -129.6083017138703610 ) ) ;
#232818 = ORIENTED_EDGE ( 'NONE', *, *, #79029, .F. ) ;
#232819 = DIRECTION ( 'NONE',  ( 0.000000000000000000, 0.2617529984165152257, 0.9651348961777124202 ) ) ;
#232820 = FACE_OUTER_BOUND ( 'NONE', #248171, .T. ) ;
#232821 = DIRECTION ( 'NONE',  ( 0.000000000000000000, -0.000000000000000000, 1.000000000000000000 ) ) ;
#232822 = TOROIDAL_SURFACE ( 'NONE', #49632, 0.2000000000000000111, 0.1000000000000000056 ) ;
#232823 = CIRCLE ( 'NONE', #137128, 0.1000000000000028644 ) ;
#232824 = CARTESIAN_POINT ( 'NONE',  ( -21.44999999999999929, 68.75000000001151079, -48.37310748452436826 ) ) ;
#232825 = AXIS2_PLACEMENT_3D ( 'NONE', #220041, #37570, #117098 ) ;
#232826 = DIRECTION ( 'NONE',  ( -0.000000000000000000, -1.000000000000000000, -7.272083257015735086E-15 ) ) ;
#232827 = CARTESIAN_POINT ( 'NONE',  ( 18.59999999999999432, -1.835859311432484375, -145.5044391687985694 ) ) ;
#232828 = CIRCLE ( 'NONE', #12071, 0.09999999999999817368 ) ;
#232829 = VERTEX_POINT ( 'NONE', #202909 ) ;
#232830 = ORIENTED_EDGE ( 'NONE', *, *, #249299, .T. ) ;
#232831 = CARTESIAN_POINT ( 'NONE',  ( -18.47653818581421703, -9.465280387751800362, -141.1259608161398944 ) ) ;
#232832 = CARTESIAN_POINT ( 'NONE',  ( -21.05000000000000071, 69.19063053712525857, -247.5666987377248631 ) ) ;
#232833 = CARTESIAN_POINT ( 'NONE',  ( -21.05439746398122836, 38.23414080847646801, -235.9702891712775852 ) ) ;
#232834 = DIRECTION ( 'NONE',  ( 0.000000000000000000, -0.8496786552930077896, -0.5273008465188219196 ) ) ;
#232835 = FACE_OUTER_BOUND ( 'NONE', #206111, .T. ) ;
#232836 = CYLINDRICAL_SURFACE ( 'NONE', #71603, 11.80000000000000426 ) ;
#232837 = DIRECTION ( 'NONE',  ( 1.000000000000000000, 0.000000000000000000, 0.000000000000000000 ) ) ;
#232838 = AXIS2_PLACEMENT_3D ( 'NONE', #243561, #148318, #182325 ) ;
#232840 = CARTESIAN_POINT ( 'NONE',  ( -23.15000000000000213, 1.115600667400684642E-11, -171.4000000000000341 ) ) ;
#232839 = AXIS2_PLACEMENT_3D ( 'NONE', #101637, #220354, #76970 ) ;
#232841 = ORIENTED_EDGE ( 'NONE', *, *, #83829, .T. ) ;
#232842 = DIRECTION ( 'NONE',  ( 0.000000000000000000, -0.8814952561688428334, 0.4721928772777350680 ) ) ;
#232843 = ORIENTED_EDGE ( 'NONE', *, *, #134860, .T. ) ;
#232844 = DIRECTION ( 'NONE',  ( 1.186688945009010077E-16, -1.000000000000000000, -0.000000000000000000 ) ) ;
#232845 = DIRECTION ( 'NONE',  ( 0.000000000000000000, -0.2617529984165031243, -0.9651348961777157509 ) ) ;
#232846 = FACE_OUTER_BOUND ( 'NONE', #225259, .T. ) ;
#232847 = AXIS2_PLACEMENT_3D ( 'NONE', #91890, #51455, #131019 ) ;
#232849 = ORIENTED_EDGE ( 'NONE', *, *, #15958, .T. ) ;
#232848 = DIRECTION ( 'NONE',  ( 0.000000000000000000, 1.000000000000000000, 2.891205793294679805E-16 ) ) ;
#232850 = DIRECTION ( 'NONE',  ( 0.000000000000000000, 0.000000000000000000, 1.000000000000000000 ) ) ;
#232851 = CARTESIAN_POINT ( 'NONE',  ( -18.59999999999999787, 18.11150788191476124, -237.7585516551410478 ) ) ;
#232852 = DIRECTION ( 'NONE',  ( -0.000000000000000000, -6.982962677686266711E-15, 1.000000000000000000 ) ) ;
#232853 = DIRECTION ( 'NONE',  ( 0.000000000000000000, 0.000000000000000000, -1.000000000000000000 ) ) ;
#232854 = ORIENTED_EDGE ( 'NONE', *, *, #238486, .F. ) ;
#232855 = CARTESIAN_POINT ( 'NONE',  ( -23.15000000000000213, 4.250000000011156409, -88.15000000000004832 ) ) ;
#232856 = EDGE_CURVE ( 'NONE', #184365, #133447, #83156, .T. ) ;
#232857 = FACE_OUTER_BOUND ( 'NONE', #247109, .T. ) ;
#232858 = CARTESIAN_POINT ( 'NONE',  ( 11.60000000000006004, 63.75000000001119815, -21.02310748452479316 ) ) ;
#232859 = CARTESIAN_POINT ( 'NONE',  ( -18.40000000000000213, 85.50000000001236344, -163.0237453873441780 ) ) ;
#232860 = AXIS2_PLACEMENT_3D ( 'NONE', #83905, #162234, #22724 ) ;
#232861 = ADVANCED_FACE ( 'NONE', ( #85490 ), #201624, .F. ) ;
#232862 = AXIS2_PLACEMENT_3D ( 'NONE', #209355, #33332, #251035 ) ;
#232863 = LINE ( 'NONE', #238958, #137218 ) ;
#232864 = CIRCLE ( 'NONE', #95472, 0.09999999999998898659 ) ;
#232865 = ORIENTED_EDGE ( 'NONE', *, *, #105393, .F. ) ;
#232866 = CARTESIAN_POINT ( 'NONE',  ( -21.14999999999999858, 76.00000000001165290, -69.52310748452431710 ) ) ;
#232868 = EDGE_CURVE ( 'NONE', #218877, #95340, #3410, .T. ) ;
#232867 = FACE_OUTER_BOUND ( 'NONE', #12270, .T. ) ;
#232870 = ADVANCED_FACE ( 'NONE', ( #245900 ), #122101, .F. ) ;
#232869 = ORIENTED_EDGE ( 'NONE', *, *, #112597, .T. ) ;
#232871 = FACE_OUTER_BOUND ( 'NONE', #104651, .T. ) ;
#232872 = ORIENTED_EDGE ( 'NONE', *, *, #172152, .F. ) ;
#232873 = CARTESIAN_POINT ( 'NONE',  ( 21.10000000000000142, 0.000000000000000000, 0.000000000000000000 ) ) ;
#232874 = CARTESIAN_POINT ( 'NONE',  ( -23.25000000000000000, 11.65000000001115588, -155.7499999999999716 ) ) ;
#232875 = TOROIDAL_SURFACE ( 'NONE', #128815, 4.041421356237312246, 0.1000000000000000056 ) ;
#232876 = AXIS2_PLACEMENT_3D ( 'NONE', #225416, #70249, #147180 ) ;
#232877 = ORIENTED_EDGE ( 'NONE', *, *, #34121, .F. ) ;
#232878 = DIRECTION ( 'NONE',  ( -3.440080580676165868E-14, 0.1298341882520054891, 0.9915357197604850459 ) ) ;
#232879 = CARTESIAN_POINT ( 'NONE',  ( 20.84999999999998721, 65.66751761918619934, -30.42826094061123854 ) ) ;
#232880 = ORIENTED_EDGE ( 'NONE', *, *, #398, .T. ) ;
#232881 = EDGE_CURVE ( 'NONE', #89128, #124170, #241432, .T. ) ;
#232882 = AXIS2_PLACEMENT_3D ( 'NONE', #138097, #117277, #255442 ) ;
#232883 = EDGE_CURVE ( 'NONE', #187202, #39978, #106354, .T. ) ;
#232884 = AXIS2_PLACEMENT_3D ( 'NONE', #206429, #147748, #27829 ) ;
#232885 = AXIS2_PLACEMENT_3D ( 'NONE', #179790, #234612, #18134 ) ;
#232886 =( BOUNDED_CURVE ( )  B_SPLINE_CURVE ( 3, ( #59668, #160106, #21864, #144335 ),
 .UNSPECIFIED., .F., .F. ) 
 B_SPLINE_CURVE_WITH_KNOTS ( ( 4, 4 ),
 ( 1.570796326794895448, 3.141592653589791784 ),
 .UNSPECIFIED. ) 
 CURVE ( )  GEOMETRIC_REPRESENTATION_ITEM ( )  RATIONAL_B_SPLINE_CURVE ( ( 1.000000000000000000, 0.8047378541243650485, 0.8047378541243650485, 1.000000000000000000 ) ) 
 REPRESENTATION_ITEM ( '' )  );
#232887 = ORIENTED_EDGE ( 'NONE', *, *, #190036, .F. ) ;
#232888 = CARTESIAN_POINT ( 'NONE',  ( -20.54999999999999716, -8.999999999988844479, -157.6060308773475924 ) ) ;
#232889 = AXIS2_PLACEMENT_3D ( 'NONE', #236215, #92847, #191986 ) ;
#232890 = DIRECTION ( 'NONE',  ( 0.000000000000000000, -0.2558827019434435912, 0.9667078373770033872 ) ) ;
#232892 = ORIENTED_EDGE ( 'NONE', *, *, #29386, .T. ) ;
#232891 = LINE ( 'NONE', #152067, #104177 ) ;
#232893 = DIRECTION ( 'NONE',  ( 0.000000000000000000, 0.000000000000000000, -1.000000000000000000 ) ) ;
#232895 = DIRECTION ( 'NONE',  ( -0.000000000000000000, -0.000000000000000000, -1.000000000000000000 ) ) ;
#232894 = UNCERTAINTY_MEASURE_WITH_UNIT (LENGTH_MEASURE( 1.000000000000000082E-05 ), #248402, 'distance_accuracy_value', 'NONE');
#232896 = CARTESIAN_POINT ( 'NONE',  ( -20.87600722750343252, 65.66887361445355964, -130.9329845918269370 ) ) ;
#232897 = DIRECTION ( 'NONE',  ( 0.000000000000000000, 0.3589373870825496859, -0.9333616406058007353 ) ) ;
#232898 = FACE_OUTER_BOUND ( 'NONE', #115838, .T. ) ;
#232899 = CARTESIAN_POINT ( 'NONE',  ( 21.05000000000000071, 8.876614585098254295, -108.8850804788447135 ) ) ;
#232900 = CARTESIAN_POINT ( 'NONE',  ( -16.77828822508139694, 66.05377062509154484, -157.3604792331504711 ) ) ;
#232903 = ORIENTED_EDGE ( 'NONE', *, *, #120573, .T. ) ;
#232902 = EDGE_CURVE ( 'NONE', #25976, #21828, #167660, .T. ) ;
#232901 = DIRECTION ( 'NONE',  ( 1.000000000000000000, 0.000000000000000000, 0.000000000000000000 ) ) ;
#232904 = EDGE_LOOP ( 'NONE', ( #187609, #106169, #73603, #140952 ) ) ;
#232906 = CARTESIAN_POINT ( 'NONE',  ( -16.79270642812257108, 51.61029886228697450, -231.9544210554141728 ) ) ;
#232905 = CARTESIAN_POINT ( 'NONE',  ( -20.94999999999999929, 1.115600667400684642E-11, -167.5000000000000284 ) ) ;
#232908 = VERTEX_POINT ( 'NONE', #54098 ) ;
#232907 = DIRECTION ( 'NONE',  ( 0.000000000000000000, 0.9126074666063772600, 0.4088369013363276627 ) ) ;
#232909 = ORIENTED_EDGE ( 'NONE', *, *, #99341, .F. ) ;
#232910 = ADVANCED_FACE ( 'NONE', ( #131072 ), #162325, .T. ) ;
#232911 = CARTESIAN_POINT ( 'NONE',  ( 21.14999999999999503, -11.64999999998883595, -103.4000000000000341 ) ) ;
#232912 = CARTESIAN_POINT ( 'NONE',  ( 21.14999999999999858, 64.08993991385487732, -222.4142553782910454 ) ) ;
#232913 = DIRECTION ( 'NONE',  ( 0.000000000000000000, 0.000000000000000000, 1.000000000000000000 ) ) ;
#232914 = LINE ( 'NONE', #251144, #90103 ) ;
#232915 = CARTESIAN_POINT ( 'NONE',  ( -18.50596464788227635, 67.49374512151688066, -195.5131169347613991 ) ) ;
#232917 = ADVANCED_FACE ( 'NONE', ( #187222 ), #149384, .F. ) ;
#232916 = DIRECTION ( 'NONE',  ( 1.000000000000000000, 0.000000000000000000, 0.000000000000000000 ) ) ;
#232918 = CIRCLE ( 'NONE', #20530, 0.1000000000000075273 ) ;
#232919 = EDGE_CURVE ( 'NONE', #81287, #160449, #20679, .T. ) ;
#232920 = TOROIDAL_SURFACE ( 'NONE', #20534, 0.2000000000000000111, 0.1000000000000000056 ) ;
#232921 = DIRECTION ( 'NONE',  ( 0.000000000000000000, 0.000000000000000000, 1.000000000000000000 ) ) ;
#232922 = ORIENTED_EDGE ( 'NONE', *, *, #4053, .T. ) ;
#232923 = ORIENTED_EDGE ( 'NONE', *, *, #140315, .T. ) ;
#232924 = DIRECTION ( 'NONE',  ( 0.000000000000000000, 0.000000000000000000, 1.000000000000000000 ) ) ;
#232925 = CIRCLE ( 'NONE', #191234, 2.099999999999990763 ) ;
#232926 = EDGE_CURVE ( 'NONE', #118980, #54351, #220580, .T. ) ;
#232927 = ORIENTED_EDGE ( 'NONE', *, *, #68190, .F. ) ;
#232928 = EDGE_LOOP ( 'NONE', ( #19891, #115515, #141002, #215284 ) ) ;
#232929 = CARTESIAN_POINT ( 'NONE',  ( -23.15000000000000213, 73.40000000001259650, -190.2984855617622770 ) ) ;
#232930 = AXIS2_PLACEMENT_3D ( 'NONE', #129465, #250680, #72070 ) ;
#232931 = DIRECTION ( 'NONE',  ( 1.000000000000000000, 0.000000000000000000, 0.000000000000000000 ) ) ;
#232932 = DIRECTION ( 'NONE',  ( -1.000000000000000000, -0.000000000000000000, -0.000000000000000000 ) ) ;
#232933 = ORIENTED_EDGE ( 'NONE', *, *, #222718, .F. ) ;
#232934 = EDGE_CURVE ( 'NONE', #203901, #160493, #228957, .T. ) ;
#232935 = LINE ( 'NONE', #11298, #133774 ) ;
#232936 = VERTEX_POINT ( 'NONE', #153246 ) ;
#232937 = CIRCLE ( 'NONE', #237209, 0.1000000000000028644 ) ;
#232938 = DIRECTION ( 'NONE',  ( 0.000000000000000000, -0.2128009952263485993, 0.9770955615653341697 ) ) ;
#232939 = DIRECTION ( 'NONE',  ( 0.000000000000000000, 0.000000000000000000, -1.000000000000000000 ) ) ;
#232940 = EDGE_CURVE ( 'NONE', #31427, #155438, #166445, .T. ) ;
#232941 = AXIS2_PLACEMENT_3D ( 'NONE', #225565, #66527, #87346 ) ;
#232942 = EDGE_LOOP ( 'NONE', ( #130863, #216801, #8504, #156849 ) ) ;
#232943 = DIRECTION ( 'NONE',  ( 0.000000000000000000, -1.000000000000000000, 0.000000000000000000 ) ) ;
#232944 = EDGE_LOOP ( 'NONE', ( #165749, #173470, #21531, #111648 ) ) ;
#232947 = ORIENTED_EDGE ( 'NONE', *, *, #69272, .F. ) ;
#232946 = CARTESIAN_POINT ( 'NONE',  ( 22.39999999999999858, 75.90000000001199965, -110.8138870828976934 ) ) ;
#232945 = DIRECTION ( 'NONE',  ( -0.7071067811865456854, 0.7071067811865493491, 0.000000000000000000 ) ) ;
#232948 = DIRECTION ( 'NONE',  ( 0.000000000000000000, -6.982962677686266711E-15, 1.000000000000000000 ) ) ;
#232949 = CIRCLE ( 'NONE', #66342, 0.09999999999999864553 ) ;
#232950 = ORIENTED_EDGE ( 'NONE', *, *, #172704, .F. ) ;
#232951 = ORIENTED_EDGE ( 'NONE', *, *, #125702, .F. ) ;
#232952 = CARTESIAN_POINT ( 'NONE',  ( 22.00356870068479154, -2.593051619917821170E-12, 7.254242361760407043 ) ) ;
#232953 = ORIENTED_EDGE ( 'NONE', *, *, #25509, .T. ) ;
#232954 = CARTESIAN_POINT ( 'NONE',  ( -33.72168855820452649, 23.65833333334447985, -184.2499999999999716 ) ) ;
#232955 = DIRECTION ( 'NONE',  ( 0.000000000000000000, 0.000000000000000000, 1.000000000000000000 ) ) ;
#232956 =( BOUNDED_SURFACE ( )  B_SPLINE_SURFACE ( 3, 2, ( 
 ( #166319, #25496, #87997 ),
 ( #104975, #146684, #26797 ),
 ( #48893, #144123, #127153 ),
 ( #145420, #45045, #205383 ),
 ( #106278, #63311, #204109 ),
 ( #184543, #65893, #5899 ) ),
 .UNSPECIFIED., .F., .F., .F. ) 
 B_SPLINE_SURFACE_WITH_KNOTS ( ( 4, 2, 4 ),
 ( 3, 3 ),
 ( 6.719893378900350768E-05, 0.0002757154632485721507, 0.0004842319927081408480 ),
 ( 0.000000000000000000, 1.000000000000000000 ),
 .UNSPECIFIED. ) 
 GEOMETRIC_REPRESENTATION_ITEM ( )  RATIONAL_B_SPLINE_SURFACE ( (
 ( 1.000000000000000000, 0.7250110520818935367, 1.000000000000000000),
 ( 1.000000000000000000, 0.7277932058356478828, 1.000000000000000000),
 ( 1.000000000000000000, 0.7278452872621734571, 1.000000000000000000),
 ( 1.000000000000000000, 0.7221445671545261291, 1.000000000000000000),
 ( 1.000000000000000000, 0.7163662143782721925, 1.000000000000000000),
 ( 1.000000000000000000, 0.7071067811865475727, 1.000000000000000000) ) ) 
 REPRESENTATION_ITEM ( '' )  SURFACE ( )  );
#232957 = DIRECTION ( 'NONE',  ( -0.000000000000000000, 0.4088369013363297166, -0.9126074666063763718 ) ) ;
#232958 = DIRECTION ( 'NONE',  ( 1.000000000000000000, 0.000000000000000000, 0.000000000000000000 ) ) ;
#232959 = ORIENTED_EDGE ( 'NONE', *, *, #89287, .F. ) ;
#232960 = CARTESIAN_POINT ( 'NONE',  ( -16.94445028196808778, 44.07934375239701552, -235.2779890399608576 ) ) ;
#232961 = CARTESIAN_POINT ( 'NONE',  ( 18.59999999999999076, 77.25000000001159606, -61.52310748452431710 ) ) ;
#232962 = VECTOR ( 'NONE', #173266, 1000.000000000000000 ) ;
#232963 = CARTESIAN_POINT ( 'NONE',  ( -20.85000000000000142, 11.75000000001115197, -160.7161343370219129 ) ) ;
#232964 = ORIENTED_EDGE ( 'NONE', *, *, #242859, .T. ) ;
#232965 = CARTESIAN_POINT ( 'NONE',  ( -22.19999999999999929, -11.75000000000000000, 9.900000000000002132 ) ) ;
#232966 = EDGE_LOOP ( 'NONE', ( #109807, #230607, #91545, #104377 ) ) ;
#232967 = FACE_OUTER_BOUND ( 'NONE', #36619, .T. ) ;
#232968 = EDGE_LOOP ( 'NONE', ( #170674, #143284, #184796, #74920 ) ) ;
#232969 = DIRECTION ( 'NONE',  ( 0.000000000000000000, 1.000000000000000000, 0.000000000000000000 ) ) ;
#232971 = ORIENTED_EDGE ( 'NONE', *, *, #202739, .F. ) ;
#232970 = CARTESIAN_POINT ( 'NONE',  ( -23.25000000000000000, 66.17117490947157421, -239.7639228359981303 ) ) ;
#232972 = CARTESIAN_POINT ( 'NONE',  ( -18.59999999999999787, 77.83585931145498193, -24.51866831572578320 ) ) ;
#232973 = ORIENTED_EDGE ( 'NONE', *, *, #137508, .T. ) ;
#232974 = DIRECTION ( 'NONE',  ( 0.000000000000000000, -1.000000000000000000, 0.000000000000000000 ) ) ;
#232975 = DIRECTION ( 'NONE',  ( 0.000000000000000000, 0.008583690987127625890, 0.9999631594459055250 ) ) ;
#232976 = ORIENTED_EDGE ( 'NONE', *, *, #248982, .T. ) ;
#232977 = AXIS2_PLACEMENT_3D ( 'NONE', #137557, #95864, #21505 ) ;
#232979 = AXIS2_PLACEMENT_3D ( 'NONE', #58539, #62418, #217606 ) ;
#232978 = DIRECTION ( 'NONE',  ( 1.000000000000000000, 0.000000000000000000, 0.000000000000000000 ) ) ;
#232980 = DIRECTION ( 'NONE',  ( -1.000000000000000000, 0.000000000000000000, -0.000000000000000000 ) ) ;
#232981 = ORIENTED_EDGE ( 'NONE', *, *, #113183, .F. ) ;
#232982 = AXIS2_PLACEMENT_3D ( 'NONE', #90723, #228974, #54168 ) ;
#232984 = CARTESIAN_POINT ( 'NONE',  ( -16.93772744219066340, 9.993541108763512426, -146.5980619719697415 ) ) ;
#232983 = TOROIDAL_SURFACE ( 'NONE', #49797, 11.70000000000000462, 0.1000000000000000056 ) ;
#232985 = ORIENTED_EDGE ( 'NONE', *, *, #178, .T. ) ;
#232986 =( BOUNDED_CURVE ( )  B_SPLINE_CURVE ( 3, ( #175369, #93222, #174100, #153243 ),
 .UNSPECIFIED., .F., .F. ) 
 B_SPLINE_CURVE_WITH_KNOTS ( ( 4, 4 ),
 ( 3.432212674861197410, 3.693332928900581624 ),
 .UNSPECIFIED. ) 
 CURVE ( )  GEOMETRIC_REPRESENTATION_ITEM ( )  RATIONAL_B_SPLINE_CURVE ( ( 1.000000000000000000, 0.9943260843901261525, 0.9943260843901261525, 1.000000000000000000 ) ) 
 REPRESENTATION_ITEM ( '' )  );
#232987 = CARTESIAN_POINT ( 'NONE',  ( 13.12229106158773284, 9.430637101707896264, -118.7682606180609923 ) ) ;
#232988 = AXIS2_PLACEMENT_3D ( 'NONE', #189163, #211294, #32702 ) ;
#232989 = DIRECTION ( 'NONE',  ( 1.000000000000000000, 0.000000000000000000, 0.000000000000000000 ) ) ;
#232990 = EDGE_CURVE ( 'NONE', #81417, #36999, #224658, .T. ) ;
#232992 = ORIENTED_EDGE ( 'NONE', *, *, #67095, .T. ) ;
#232991 = CARTESIAN_POINT ( 'NONE',  ( -23.25000000000000000, 85.60000000001177511, -79.41707660717668205 ) ) ;
#232993 = EDGE_CURVE ( 'NONE', #168869, #129370, #4089, .T. ) ;
#232995 = LINE ( 'NONE', #133866, #40909 ) ;
#232994 = VECTOR ( 'NONE', #180712, 1000.000000000000000 ) ;
#232997 = ADVANCED_FACE ( 'NONE', ( #211915 ), #88067, .T. ) ;
#232996 = VECTOR ( 'NONE', #14060, 1000.000000000000000 ) ;
#232998 = CARTESIAN_POINT ( 'NONE',  ( 18.49999999999998934, 6.550000000011156231, -188.7499999999999716 ) ) ;
#232999 = CARTESIAN_POINT ( 'NONE',  ( -16.93211319090181632, 9.999986781157469196, -20.92250549927306835 ) ) ;
#233000 = CIRCLE ( 'NONE', #195411, 0.09999999999999939493 ) ;
#233002 = CARTESIAN_POINT ( 'NONE',  ( -23.25000000000000000, 0.000000000000000000, -35.60000000000000853 ) ) ;
#233001 = DIRECTION ( 'NONE',  ( -1.000000000000000000, -0.000000000000000000, -0.000000000000000000 ) ) ;
#233003 = CARTESIAN_POINT ( 'NONE',  ( 20.04142135623730070, 64.35000000001222986, -148.6731074845244507 ) ) ;
#233004 = CARTESIAN_POINT ( 'NONE',  ( -20.64999999999999858, 70.22209180797715078, -215.6584443947398313 ) ) ;
#233006 = B_SPLINE_CURVE_WITH_KNOTS ( 'NONE', 3,
 ( #216628, #18433, #58812, #173709 ),
 .UNSPECIFIED., .F., .F.,
 ( 4, 4 ),
 ( 0.000000000000000000, 0.001767853679387106471 ),
 .UNSPECIFIED. ) ;
#233005 = CARTESIAN_POINT ( 'NONE',  ( -22.59999999999999787, 11.74987124437650721, 0.06542959101367804009 ) ) ;
#233007 = CARTESIAN_POINT ( 'NONE',  ( -18.50000000000000000, 23.34004772283014972, -229.2004250369967338 ) ) ;
#233008 = CIRCLE ( 'NONE', #220348, 0.1000000000000028644 ) ;
#233009 = ORIENTED_EDGE ( 'NONE', *, *, #188921, .F. ) ;
#233010 = ORIENTED_EDGE ( 'NONE', *, *, #108857, .T. ) ;
#233011 = CARTESIAN_POINT ( 'NONE',  ( 20.94999999999999929, 64.35000000001195986, -109.8069731475024753 ) ) ;
#233013 = ORIENTED_EDGE ( 'NONE', *, *, #179698, .T. ) ;
#233012 = DIRECTION ( 'NONE',  ( 0.000000000000000000, 0.000000000000000000, 1.000000000000000000 ) ) ;
#233014 = ORIENTED_EDGE ( 'NONE', *, *, #49690, .F. ) ;
#233015 = EDGE_CURVE ( 'NONE', #66395, #245624, #29079, .T. ) ;
#233016 = DIRECTION ( 'NONE',  ( -0.000000000000000000, -0.1335171055202901413, 0.9910465087640860649 ) ) ;
#233017 = VERTEX_POINT ( 'NONE', #171521 ) ;
#233018 = CARTESIAN_POINT ( 'NONE',  ( 21.13461538461538325, 43.49873268050095021, -234.8559629938181388 ) ) ;
#233019 = ORIENTED_EDGE ( 'NONE', *, *, #79639, .F. ) ;
#233020 = DIRECTION ( 'NONE',  ( -1.000000000000000000, 0.000000000000000000, 0.000000000000000000 ) ) ;
#233021 = CIRCLE ( 'NONE', #120597, 11.74999999999999645 ) ;
#233023 = VERTEX_POINT ( 'NONE', #249743 ) ;
#233022 = EDGE_LOOP ( 'NONE', ( #67192, #211582, #101339, #177433, #191997, #110555, #97204, #204453, #70982, #128486, #256983, #84497, #55531, #168564, #36258, #32834 ) ) ;
#233024 = ORIENTED_EDGE ( 'NONE', *, *, #19477, .T. ) ;
#233025 = VERTEX_POINT ( 'NONE', #33302 ) ;
#233026 = ORIENTED_EDGE ( 'NONE', *, *, #224347, .F. ) ;
#233027 = CARTESIAN_POINT ( 'NONE',  ( 20.85000000000000142, 11.75000000000000355, -26.71613433702190932 ) ) ;
#233028 = CYLINDRICAL_SURFACE ( 'NONE', #53280, 0.09999999999999939493 ) ;
#233029 = CARTESIAN_POINT ( 'NONE',  ( -18.52139480978223318, -9.481358845066894858, -7.024556567119067729 ) ) ;
#233031 = EDGE_LOOP ( 'NONE', ( #148332, #15490, #95082, #49192 ) ) ;
#233030 = PLANE ( 'NONE',  #250067 ) ;
#233032 = ADVANCED_FACE ( 'NONE', ( #227601 ), #216472, .F. ) ;
#233033 = EDGE_CURVE ( 'NONE', #201736, #240390, #249800, .T. ) ;
#233034 = DIRECTION ( 'NONE',  ( -1.000000000000000000, 0.000000000000000000, 0.000000000000000000 ) ) ;
#233035 = DIRECTION ( 'NONE',  ( 1.000000000000000000, 1.186688945009009831E-16, 0.000000000000000000 ) ) ;
#233037 = ORIENTED_EDGE ( 'NONE', *, *, #238619, .F. ) ;
#233036 = CARTESIAN_POINT ( 'NONE',  ( 20.95132126680579887, 10.48994987015794322, -141.5703245384345053 ) ) ;
#233038 = DIRECTION ( 'NONE',  ( -0.000000000000000000, -0.9770955615653316162, -0.2128009952263597848 ) ) ;
#233039 = ORIENTED_EDGE ( 'NONE', *, *, #4434, .T. ) ;
#233040 = CARTESIAN_POINT ( 'NONE',  ( 23.15000000000000213, -9.499999999988844479, -191.1060308773475072 ) ) ;
#233042 = ORIENTED_EDGE ( 'NONE', *, *, #64343, .F. ) ;
#233041 = DIRECTION ( 'NONE',  ( 1.000000000000000000, 0.000000000000000000, 0.000000000000000000 ) ) ;
#233043 = DIRECTION ( 'NONE',  ( -1.000000000000000000, -0.000000000000000000, -0.000000000000000000 ) ) ;
#233044 = DIRECTION ( 'NONE',  ( 0.000000000000000000, 6.982962677686266711E-15, -1.000000000000000000 ) ) ;
#233045 = ADVANCED_FACE ( 'NONE', ( #128514 ), #29451, .F. ) ;
#233046 = ORIENTED_EDGE ( 'NONE', *, *, #11166, .F. ) ;
#233047 = FACE_OUTER_BOUND ( 'NONE', #67669, .T. ) ;
#233048 = VECTOR ( 'NONE', #134344, 1000.000000000000000 ) ;
#233049 = FACE_OUTER_BOUND ( 'NONE', #63932, .T. ) ;
#233050 = CARTESIAN_POINT ( 'NONE',  ( -23.25000000000000000, 42.94477010600543565, -254.3363632230312703 ) ) ;
#233051 = DIRECTION ( 'NONE',  ( -1.000000000000000000, -0.000000000000000000, -0.000000000000000000 ) ) ;
#233052 = CIRCLE ( 'NONE', #78877, 0.1000000000000028644 ) ;
#233053 = ORIENTED_EDGE ( 'NONE', *, *, #7172, .T. ) ;
#233054 = ORIENTED_EDGE ( 'NONE', *, *, #229107, .T. ) ;
#233055 = DIRECTION ( 'NONE',  ( -1.000000000000000000, 0.000000000000000000, 0.000000000000000000 ) ) ;
#233056 = CARTESIAN_POINT ( 'NONE',  ( 21.05000000000000071, 5.000000000011153745, -155.0947339810869323 ) ) ;
#233057 = ORIENTED_EDGE ( 'NONE', *, *, #97780, .F. ) ;
#233059 = DIRECTION ( 'NONE',  ( 0.000000000000000000, -0.2617529984165152257, -0.9651348961777124202 ) ) ;
#233058 = VECTOR ( 'NONE', #76233, 1000.000000000000000 ) ;
#233060 = VERTEX_POINT ( 'NONE', #89365 ) ;
#233061 = DIRECTION ( 'NONE',  ( 0.000000000000000000, 0.2617529984165030132, 0.9651348961777158619 ) ) ;
#233062 = DIRECTION ( 'NONE',  ( 1.000000000000000000, -0.000000000000000000, 0.000000000000000000 ) ) ;
#233063 = AXIS2_PLACEMENT_3D ( 'NONE', #173481, #116030, #211267 ) ;
#233064 = AXIS2_PLACEMENT_3D ( 'NONE', #238263, #157492, #235698 ) ;
#233065 = EDGE_CURVE ( 'NONE', #71039, #54600, #248463, .T. ) ;
#233066 = ORIENTED_EDGE ( 'NONE', *, *, #255162, .T. ) ;
#233067 = CARTESIAN_POINT ( 'NONE',  ( -16.87683809663753465, 66.13508622147418237, -190.2473918488859397 ) ) ;
#233068 = B_SPLINE_CURVE_WITH_KNOTS ( 'NONE', 3,
 ( #167486, #27987, #244421, #206585, #124492, #204010, #107482, #243136 ),
 .UNSPECIFIED., .F., .F.,
 ( 4, 2, 2, 4 ),
 ( 0.000000000000000000, 0.0001306511400391059284, 0.0001959767100586839647, 0.0002613022800782620011 ),
 .UNSPECIFIED. ) ;
#233069 = ORIENTED_EDGE ( 'NONE', *, *, #171634, .T. ) ;
#233070 = ORIENTED_EDGE ( 'NONE', *, *, #118194, .T. ) ;
#233071 = CIRCLE ( 'NONE', #129014, 0.09999999999999439892 ) ;
#233072 = ORIENTED_EDGE ( 'NONE', *, *, #167967, .F. ) ;
#233073 = AXIS2_PLACEMENT_3D ( 'NONE', #77772, #56910, #136458 ) ;
#233074 = AXIS2_PLACEMENT_3D ( 'NONE', #200487, #115815, #256545 ) ;
#233075 = EDGE_CURVE ( 'NONE', #189061, #95642, #150644, .T. ) ;
#233076 = CARTESIAN_POINT ( 'NONE',  ( -21.05000000000000071, 6.300000000011169554, -33.60000000000000142 ) ) ;
#233077 = CARTESIAN_POINT ( 'NONE',  ( -21.08035267497491816, 0.08268862478717949049, -127.6682931602169901 ) ) ;
#233078 = ADVANCED_FACE ( 'NONE', ( #198745 ), #218288, .F. ) ;
#233079 = FACE_OUTER_BOUND ( 'NONE', #254184, .T. ) ;
#233080 = CARTESIAN_POINT ( 'NONE',  ( 15.69410316191959254, 66.64325398293377134, -119.3197477631601942 ) ) ;
#233081 = CIRCLE ( 'NONE', #212228, 7.899999999999994138 ) ;
#233083 = SPHERICAL_SURFACE ( 'NONE', #128400, 0.1000000000000000056 ) ;
#233082 = DIRECTION ( 'NONE',  ( 0.000000000000000000, -0.2128009952263982818, 0.9770955615653232895 ) ) ;
#233085 = VERTEX_POINT ( 'NONE', #16293 ) ;
#233084 = CARTESIAN_POINT ( 'NONE',  ( -18.59999999999999787, 77.83534155023627932, -91.36795619196132634 ) ) ;
#233086 = FACE_OUTER_BOUND ( 'NONE', #18677, .T. ) ;
#233087 = ORIENTED_EDGE ( 'NONE', *, *, #181239, .F. ) ;
#233088 = EDGE_CURVE ( 'NONE', #17154, #112979, #78890, .T. ) ;
#233089 = CARTESIAN_POINT ( 'NONE',  ( -13.77178122865953824, 9.456028260519072859, -149.0111980350657745 ) ) ;
#233090 = ADVANCED_FACE ( 'NONE', ( #114068 ), #245529, .F. ) ;
#233091 = VERTEX_POINT ( 'NONE', #95780 ) ;
#233092 = VERTEX_POINT ( 'NONE', #157076 ) ;
#233093 = DIRECTION ( 'NONE',  ( 0.000000000000000000, 0.8814952561688476074, -0.4721928772777262417 ) ) ;
#233094 = DIRECTION ( 'NONE',  ( 0.7070776581708965169, 0.000000000000000000, 0.7071359030027827286 ) ) ;
#233095 = FACE_OUTER_BOUND ( 'NONE', #184208, .T. ) ;
#233096 = VECTOR ( 'NONE', #112141, 1000.000000000000227 ) ;
#233097 = EDGE_CURVE ( 'NONE', #145606, #47933, #179218, .T. ) ;
#233098 = CARTESIAN_POINT ( 'NONE',  ( 18.59999999999999787, 77.85102823015316176, -158.3691942151018566 ) ) ;
#233099 = EDGE_CURVE ( 'NONE', #241027, #252869, #94505, .T. ) ;
#233100 = ORIENTED_EDGE ( 'NONE', *, *, #157839, .F. ) ;
#233101 = EDGE_LOOP ( 'NONE', ( #112795, #244157, #82209, #251899 ) ) ;
#233102 = CARTESIAN_POINT ( 'NONE',  ( 18.79999999999999716, 1.350000000000000089, 16.50000000000000000 ) ) ;
#233103 = VERTEX_POINT ( 'NONE', #117919 ) ;
#233104 = DIRECTION ( 'NONE',  ( -2.342056488767301376E-15, 0.1350103645451974088, -0.9908441862701587999 ) ) ;
#233105 = CARTESIAN_POINT ( 'NONE',  ( 18.49999999999999289, 10.49142135624846439, -158.8500000000000227 ) ) ;
#233106 = ORIENTED_EDGE ( 'NONE', *, *, #50493, .T. ) ;
#233107 = DIRECTION ( 'NONE',  ( -1.000000000000000000, -2.952720810173289112E-16, 0.000000000000000000 ) ) ;
#233109 = EDGE_CURVE ( 'NONE', #58501, #124582, #159633, .T. ) ;
#233108 = DIRECTION ( 'NONE',  ( 0.000000000000000000, 0.000000000000000000, 1.000000000000000000 ) ) ;
#233110 = DIRECTION ( 'NONE',  ( -0.000000000000000000, 6.982962677686266711E-15, -1.000000000000000000 ) ) ;
#233111 = CARTESIAN_POINT ( 'NONE',  ( 20.95512840106816199, 65.37615130623896675, -157.8206282637254674 ) ) ;
#233112 = ORIENTED_EDGE ( 'NONE', *, *, #123477, .F. ) ;
#233113 = AXIS2_PLACEMENT_3D ( 'NONE', #256576, #174590, #139222 ) ;
#233114 = LINE ( 'NONE', #76574, #196015 ) ;
#233115 = ADVANCED_FACE ( 'NONE', ( #56635 ), #253577, .F. ) ;
#233116 = DIRECTION ( 'NONE',  ( 1.000000000000000000, 0.000000000000000000, 0.000000000000000000 ) ) ;
#233117 = VECTOR ( 'NONE', #180263, 1000.000000000000000 ) ;
#233118 = CARTESIAN_POINT ( 'NONE',  ( -21.00448002041601470, 57.68351327785831018, -226.1699560279491834 ) ) ;
#233119 = EDGE_CURVE ( 'NONE', #61601, #28183, #37135, .T. ) ;
#233120 = ADVANCED_FACE ( 'NONE', ( #239165 ), #57937, .F. ) ;
#233121 = AXIS2_PLACEMENT_3D ( 'NONE', #105711, #124036, #186583 ) ;
#233122 = ORIENTED_EDGE ( 'NONE', *, *, #149709, .T. ) ;
#233123 = ADVANCED_FACE ( 'NONE', ( #116647 ), #197459, .F. ) ;
#233124 = CARTESIAN_POINT ( 'NONE',  ( -23.25000000000000000, 5.950000000011163692, -190.6942976949651438 ) ) ;
#233125 = ORIENTED_EDGE ( 'NONE', *, *, #159583, .F. ) ;
#233126 = CARTESIAN_POINT ( 'NONE',  ( -23.24999999999999645, 37.94390843806124991, -261.1300795796834109 ) ) ;
#233127 = CARTESIAN_POINT ( 'NONE',  ( -20.54999999999999716, 71.65000000001256808, -186.7731074845243882 ) ) ;
#233128 = DIRECTION ( 'NONE',  ( -1.000000000000000000, 3.265361837132813093E-16, 2.280189983783949500E-30 ) ) ;
#233129 = EDGE_CURVE ( 'NONE', #149408, #164185, #8383, .T. ) ;
#233130 = CARTESIAN_POINT ( 'NONE',  ( 18.59999999999999076, 11.65000000001115943, -125.2500000000000284 ) ) ;
#233131 = DIRECTION ( 'NONE',  ( -1.000000000000000000, -1.394253735153569469E-16, -2.602809386958778209E-16 ) ) ;
#233132 = CARTESIAN_POINT ( 'NONE',  ( -21.05000000000000071, 74.16465844978819177, -191.8679561919614116 ) ) ;
#233133 = AXIS2_PLACEMENT_3D ( 'NONE', #22773, #42314, #201380 ) ;
#233134 = EDGE_CURVE ( 'NONE', #116074, #195501, #55072, .T. ) ;
#233135 = EDGE_LOOP ( 'NONE', ( #145387, #94035, #32619, #9772 ) ) ;
#233136 = CARTESIAN_POINT ( 'NONE',  ( -17.11825945287481687, 66.05000000001224691, -149.1731074845244507 ) ) ;
#233137 = TOROIDAL_SURFACE ( 'NONE', #108210, 1.900000000000002576, 0.1000000000000000056 ) ;
#233138 = CARTESIAN_POINT ( 'NONE',  ( 21.08832698747859169, 67.22463560659483051, -124.2943900180602128 ) ) ;
#233140 = EDGE_CURVE ( 'NONE', #99142, #178237, #117473, .T. ) ;
#233139 = CARTESIAN_POINT ( 'NONE',  ( 20.94999999999999929, 6.649999999999999467, -12.15000000000000036 ) ) ;
#233141 = FACE_OUTER_BOUND ( 'NONE', #136723, .T. ) ;
#233142 = VECTOR ( 'NONE', #8511, 1000.000000000000000 ) ;
#233143 = DIRECTION ( 'NONE',  ( -4.239556034732055511E-17, -0.08413937888704771384, 0.9964539953858891908 ) ) ;
#233144 = ORIENTED_EDGE ( 'NONE', *, *, #124514, .F. ) ;
#233145 = ORIENTED_EDGE ( 'NONE', *, *, #189274, .F. ) ;
#233146 = DIRECTION ( 'NONE',  ( 0.000000000000000000, 6.608470384673558123E-15, -1.000000000000000000 ) ) ;
#233147 = FACE_OUTER_BOUND ( 'NONE', #135935, .T. ) ;
#233148 = CARTESIAN_POINT ( 'NONE',  ( -22.39999999999999858, 64.25000000001165290, -69.52310748452438816 ) ) ;
#233149 = DIRECTION ( 'NONE',  ( 1.000000000000000000, -7.304098846218133681E-16, -4.639676173203992654E-30 ) ) ;
#233150 = EDGE_CURVE ( 'NONE', #230665, #126059, #124363, .T. ) ;
#233151 = EDGE_LOOP ( 'NONE', ( #148164, #235962, #129153, #169245 ) ) ;
#233152 = DIRECTION ( 'NONE',  ( 0.000000000000000000, -6.853228547068871147E-15, 1.000000000000000000 ) ) ;
#233153 = CARTESIAN_POINT ( 'NONE',  ( -23.15000000000000213, 2.000000000011154189, -87.77537807723795993 ) ) ;
#233154 = VERTEX_POINT ( 'NONE', #123079 ) ;
#233155 = DIRECTION ( 'NONE',  ( -0.000000000000000000, 0.1350103645451974088, -0.9908441862701587999 ) ) ;
#233156 = CIRCLE ( 'NONE', #29166, 0.09999999999998898659 ) ;
#233157 = VECTOR ( 'NONE', #47178, 1000.000000000000000 ) ;
#233158 = CARTESIAN_POINT ( 'NONE',  ( 21.12769345151713196, 13.08004441897819170, -210.6858836008591140 ) ) ;
#233159 = EDGE_LOOP ( 'NONE', ( #28127, #46910, #22608, #16606, #59361 ) ) ;
#233160 = CARTESIAN_POINT ( 'NONE',  ( -18.34804628011471195, 64.52683809665025194, -194.2731074845244450 ) ) ;
#233161 = EDGE_LOOP ( 'NONE', ( #114853, #146018, #215675, #18572 ) ) ;
#233162 = LINE ( 'NONE', #192736, #22431 ) ;
#233163 = DIRECTION ( 'NONE',  ( 1.000000000000000000, 0.000000000000000000, 0.000000000000000000 ) ) ;
#233164 = DIRECTION ( 'NONE',  ( -1.000000000000000000, 0.000000000000000000, 0.000000000000000000 ) ) ;
#233165 = FACE_OUTER_BOUND ( 'NONE', #135806, .T. ) ;
#233166 = CARTESIAN_POINT ( 'NONE',  ( -21.05000000000000071, 76.00000000001162448, -65.22310748452436258 ) ) ;
#233167 = FACE_OUTER_BOUND ( 'NONE', #188271, .T. ) ;
#233168 = DIRECTION ( 'NONE',  ( 0.000000000000000000, 0.000000000000000000, -1.000000000000000000 ) ) ;
#233170 = DIRECTION ( 'NONE',  ( 0.000000000000000000, 0.9126074666063775931, 0.4088369013363268301 ) ) ;
#233169 = CARTESIAN_POINT ( 'NONE',  ( 20.95576188350343116, 10.60898054497455512, -108.1112337227543350 ) ) ;
#233171 = AXIS2_PLACEMENT_3D ( 'NONE', #241517, #62877, #164560 ) ;
#233172 = EDGE_CURVE ( 'NONE', #110428, #37339, #195844, .T. ) ;
#233173 = DIRECTION ( 'NONE',  ( 0.000000000000000000, 0.000000000000000000, 1.000000000000000000 ) ) ;
#233174 = AXIS2_PLACEMENT_3D ( 'NONE', #140003, #181727, #40958 ) ;
#233175 = CARTESIAN_POINT ( 'NONE',  ( 21.13461538461538325, 10.61458296202553697, -12.35000000000000320 ) ) ;
#233176 = AXIS2_PLACEMENT_3D ( 'NONE', #120595, #116718, #39787 ) ;
#233178 = DIRECTION ( 'NONE',  ( -6.938893903907222856E-15, 1.000000000000000000, 0.000000000000000000 ) ) ;
#233177 = CIRCLE ( 'NONE', #187368, 0.09999999999999939493 ) ;
#233179 = ORIENTED_EDGE ( 'NONE', *, *, #82268, .T. ) ;
#233180 = ADVANCED_FACE ( 'NONE', ( #61818 ), #64385, .T. ) ;
#233181 = CARTESIAN_POINT ( 'NONE',  ( -20.87155475150660777, 11.75000000001115197, -93.59558652915730192 ) ) ;
#233182 = CARTESIAN_POINT ( 'NONE',  ( -21.10000000000000142, -11.75000000000000000, 11.89999999999999680 ) ) ;
#233183 = DIRECTION ( 'NONE',  ( 0.000000000000000000, 1.000000000000000000, 0.000000000000000000 ) ) ;
#233184 = AXIS2_PLACEMENT_3D ( 'NONE', #207145, #130152, #170632 ) ;
#233185 = ORIENTED_EDGE ( 'NONE', *, *, #166432, .F. ) ;
#233186 = CARTESIAN_POINT ( 'NONE',  ( -17.71734398241074615, 62.84618681140459273, -210.6017155954972964 ) ) ;
#233188 = ADVANCED_FACE ( 'NONE', ( #201317 ), #220871, .F. ) ;
#233187 = CARTESIAN_POINT ( 'NONE',  ( -18.59999999999999787, 22.29493434298047205, -231.3632329395297234 ) ) ;
#233189 = DIRECTION ( 'NONE',  ( 0.000000000000000000, -1.565658005757035267E-14, 1.000000000000000000 ) ) ;
#233190 = ADVANCED_FACE ( 'NONE', ( #103480 ), #162222, .T. ) ;
#233191 = ORIENTED_EDGE ( 'NONE', *, *, #109984, .T. ) ;
#233192 = AXIS2_PLACEMENT_3D ( 'NONE', #184652, #244626, #68576 ) ;
#233194 = AXIS2_PLACEMENT_3D ( 'NONE', #8405, #244429, #226124 ) ;
#233193 = FACE_OUTER_BOUND ( 'NONE', #44380, .T. ) ;
#233195 = ORIENTED_EDGE ( 'NONE', *, *, #7946, .F. ) ;
#233196 = LINE ( 'NONE', #151069, #21339 ) ;
#233197 = CARTESIAN_POINT ( 'NONE',  ( -21.55000000000000071, 7.250000000011155521, -79.35000000000005116 ) ) ;
#233198 = CIRCLE ( 'NONE', #120768, 0.09999999999998898659 ) ;
#233199 = ORIENTED_EDGE ( 'NONE', *, *, #241362, .T. ) ;
#233200 = FACE_OUTER_BOUND ( 'NONE', #167804, .T. ) ;
#233201 = VERTEX_POINT ( 'NONE', #164769 ) ;
#233202 = DIRECTION ( 'NONE',  ( 1.000000000000000000, -2.952720810173289112E-16, -2.061873921506763405E-30 ) ) ;
#233203 = CYLINDRICAL_SURFACE ( 'NONE', #103648, 11.74999999999999289 ) ;
#233205 = CARTESIAN_POINT ( 'NONE',  ( 18.59999999999999076, 18.18127959618848166, -237.5711165786817389 ) ) ;
#233204 = UNCERTAINTY_MEASURE_WITH_UNIT (LENGTH_MEASURE( 1.000000000000000082E-05 ), #178182, 'distance_accuracy_value', 'NONE');
#233206 = DIRECTION ( 'NONE',  ( -0.000000000000000000, 0.9072850278296915594, 0.4205162045344698618 ) ) ;
#233207 = LINE ( 'NONE', #156241, #138909 ) ;
#233208 = CARTESIAN_POINT ( 'NONE',  ( 18.54999999999999716, 67.25000000001259082, -194.2731074845244166 ) ) ;
#233209 = DIRECTION ( 'NONE',  ( -0.000000000000000000, -0.000000000000000000, -1.000000000000000000 ) ) ;
#233210 = DIRECTION ( 'NONE',  ( 0.000000000000000000, 0.000000000000000000, -1.000000000000000000 ) ) ;
#233212 = VERTEX_POINT ( 'NONE', #85184 ) ;
#233211 = CARTESIAN_POINT ( 'NONE',  ( 21.04999999999999716, 69.69981666374559381, -103.0744349168653571 ) ) ;
#233214 = CARTESIAN_POINT ( 'NONE',  ( -20.94684162615585166, 64.25000000001162448, -62.68146348457850081 ) ) ;
#233213 = CARTESIAN_POINT ( 'NONE',  ( -20.94999999999994600, 66.25000000001119815, -5.923107484524795296 ) ) ;
#233215 = ORIENTED_EDGE ( 'NONE', *, *, #189777, .T. ) ;
#233217 = ORIENTED_EDGE ( 'NONE', *, *, #229921, .F. ) ;
#233216 = CARTESIAN_POINT ( 'NONE',  ( -18.59999999999999787, 11.72137559264762174, -210.8820217676538391 ) ) ;
#233218 = AXIS2_PLACEMENT_3D ( 'NONE', #150762, #33421, #13817 ) ;
#233219 = ORIENTED_EDGE ( 'NONE', *, *, #214526, .F. ) ;
#233220 = EDGE_CURVE ( 'NONE', #166513, #118333, #224719, .T. ) ;
#233221 = LINE ( 'NONE', #110679, #8208 ) ;
#233222 = CARTESIAN_POINT ( 'NONE',  ( 20.94999999999999929, 1.835341550235569663, -45.05515129256298223 ) ) ;
#233223 = CARTESIAN_POINT ( 'NONE',  ( -23.15000000000000213, 76.00000000001237765, -170.0231074845243597 ) ) ;
#233224 = DIRECTION ( 'NONE',  ( 0.000000000000000000, -7.116814260417693756E-15, 1.000000000000000000 ) ) ;
#233225 = CIRCLE ( 'NONE', #120787, 0.09999999999999724387 ) ;
#233226 = CARTESIAN_POINT ( 'NONE',  ( -21.05000000000000071, 26.06793112591406825, -254.4053733484743418 ) ) ;
#233227 = CARTESIAN_POINT ( 'NONE',  ( 20.94999999999999574, 18.80454058543246276, -232.7833891117047074 ) ) ;
#233229 = EDGE_CURVE ( 'NONE', #48558, #26849, #233265, .T. ) ;
#233228 = DIRECTION ( 'NONE',  ( 1.000000000000000000, 0.000000000000000000, 0.000000000000000000 ) ) ;
#233230 = ADVANCED_FACE ( 'NONE', ( #65655 ), #145184, .F. ) ;
#233231 = FACE_OUTER_BOUND ( 'NONE', #247264, .T. ) ;
#233232 = EDGE_LOOP ( 'NONE', ( #83451, #123242, #83887, #126682 ) ) ;
#233233 = VERTEX_POINT ( 'NONE', #21429 ) ;
#233234 = DIRECTION ( 'NONE',  ( 0.000000000000000000, -0.9908441862701420355, -0.1350103645453197554 ) ) ;
#233235 = CONICAL_SURFACE ( 'NONE', #154143, 4.299999999999966960, 0.7853981633974466137 ) ;
#233236 = ORIENTED_EDGE ( 'NONE', *, *, #171444, .T. ) ;
#233237 = CARTESIAN_POINT ( 'NONE',  ( -23.25000000000000000, 85.60000000001198828, -112.9170766071766820 ) ) ;
#233239 = ORIENTED_EDGE ( 'NONE', *, *, #211006, .F. ) ;
#233238 = CIRCLE ( 'NONE', #241579, 0.1000000000000028644 ) ;
#233240 = CARTESIAN_POINT ( 'NONE',  ( 20.84999999999999432, 77.16412189325286874, -61.60825939895269698 ) ) ;
#233241 = EDGE_CURVE ( 'NONE', #104540, #237894, #129187, .T. ) ;
#233242 = PRESENTATION_LAYER_ASSIGNMENT (  '', '', ( #108331 ) ) ;
#233243 = CARTESIAN_POINT ( 'NONE',  ( 0.000000000000000000, -8.350000000000004974, 33.00000000000000000 ) ) ;
#233244 = DIRECTION ( 'NONE',  ( 0.000000000000000000, -1.000000000000000000, 0.000000000000000000 ) ) ;
#233245 = LINE ( 'NONE', #76696, #14932 ) ;
#233246 = ADVANCED_FACE ( 'NONE', ( #200045 ), #1817, .T. ) ;
#233247 = CARTESIAN_POINT ( 'NONE',  ( 22.47071067811865319, 75.90090754531013317, -211.2431822290224090 ) ) ;
#233248 = VERTEX_POINT ( 'NONE', #46086 ) ;
#233249 = AXIS2_PLACEMENT_3D ( 'NONE', #239178, #60523, #32352 ) ;
#233250 = ADVANCED_FACE ( 'NONE', ( #160927, #43543 ), #42256, .F. ) ;
#233252 = AXIS2_PLACEMENT_3D ( 'NONE', #92684, #236052, #156556 ) ;
#233251 = LINE ( 'NONE', #93707, #100257 ) ;
#233253 = DIRECTION ( 'NONE',  ( 1.000000000000000000, 0.000000000000000000, 0.000000000000000000 ) ) ;
#233254 = CARTESIAN_POINT ( 'NONE',  ( -21.05000000000000426, 76.10000000001171827, -76.00017450564908472 ) ) ;
#233255 = CARTESIAN_POINT ( 'NONE',  ( 23.14999999999999858, 17.01923898301590654, -224.3994341343041867 ) ) ;
#233256 = ADVANCED_FACE ( 'NONE', ( #181763 ), #3096, .T. ) ;
#233257 = DIRECTION ( 'NONE',  ( 0.000000000000000000, 6.982962677686266711E-15, -1.000000000000000000 ) ) ;
#233258 = EDGE_LOOP ( 'NONE', ( #137546, #26453, #168517, #11413 ) ) ;
#233260 = FACE_OUTER_BOUND ( 'NONE', #849, .T. ) ;
#233259 = CARTESIAN_POINT ( 'NONE',  ( -17.11825945287483108, 60.93935776605891874, -221.0417277355861074 ) ) ;
#233261 = EDGE_LOOP ( 'NONE', ( #69692, #38391, #32997, #161756 ) ) ;
#233264 = ORIENTED_EDGE ( 'NONE', *, *, #226178, .F. ) ;
#233263 = CARTESIAN_POINT ( 'NONE',  ( -20.94999999999999929, 1.115600667400684642E-11, -33.50000000000000000 ) ) ;
#233262 = CARTESIAN_POINT ( 'NONE',  ( 20.94999999999999574, 87.41227409416161720, -100.1231074845242262 ) ) ;
#233265 = CIRCLE ( 'NONE', #104216, 0.4999999999999944489 ) ;
#233266 = DIRECTION ( 'NONE',  ( 1.000000000000000000, 0.000000000000000000, 0.000000000000000000 ) ) ;
#233267 = CIRCLE ( 'NONE', #191573, 1.500000000000001332 ) ;
#233268 = AXIS2_PLACEMENT_3D ( 'NONE', #207434, #225662, #148740 ) ;
#233269 = TOROIDAL_SURFACE ( 'NONE', #162518, 6.258578643762712446, 0.1000000000000000056 ) ;
#233270 = CARTESIAN_POINT ( 'NONE',  ( 20.85000000000000142, 1.115600667400684642E-11, -134.0000000000000284 ) ) ;
#233271 = ORIENTED_EDGE ( 'NONE', *, *, #122454, .T. ) ;
#233272 = DIRECTION ( 'NONE',  ( 1.000000000000000000, 0.000000000000000000, 0.000000000000000000 ) ) ;
#233273 = AXIS2_PLACEMENT_3D ( 'NONE', #174067, #157043, #99588 ) ;
#233274 = EDGE_CURVE ( 'NONE', #12719, #174189, #4391, .T. ) ;
#233275 = DIRECTION ( 'NONE',  ( -1.000000000000000000, -0.000000000000000000, -0.000000000000000000 ) ) ;
#233276 = DIRECTION ( 'NONE',  ( 0.000000000000000000, 0.000000000000000000, 1.000000000000000000 ) ) ;
#233277 = ORIENTED_EDGE ( 'NONE', *, *, #136528, .T. ) ;
#233278 = ORIENTED_EDGE ( 'NONE', *, *, #246286, .T. ) ;
#233279 = FACE_OUTER_BOUND ( 'NONE', #123621, .T. ) ;
#233280 = CARTESIAN_POINT ( 'NONE',  ( 18.59999994388910238, -9.363566187059998214, -74.18111723680094372 ) ) ;
#233281 = FACE_OUTER_BOUND ( 'NONE', #75830, .T. ) ;
#233282 = DIRECTION ( 'NONE',  ( 3.469446951953727785E-14, -0.8496786552930157832, -0.5273008465188090410 ) ) ;
#233283 = EDGE_LOOP ( 'NONE', ( #127822, #193401, #182971, #22135 ) ) ;
#233284 = CARTESIAN_POINT ( 'NONE',  ( 21.05000000000000071, 16.44800918141279666, -240.8068063186265135 ) ) ;
#233285 = CARTESIAN_POINT ( 'NONE',  ( -20.64999999999999858, -8.730841121484170131, -124.4019252810157070 ) ) ;
#233286 = DIRECTION ( 'NONE',  ( -0.000000000000000000, 1.000000000000000000, -0.000000000000000000 ) ) ;
#233287 = ORIENTED_EDGE ( 'NONE', *, *, #201611, .T. ) ;
#233288 = CARTESIAN_POINT ( 'NONE',  ( 20.97565083910961548, 59.10540512327582263, -225.7996265934505686 ) ) ;
#233289 = AXIS2_PLACEMENT_3D ( 'NONE', #237725, #77348, #18678 ) ;
#233290 = DIRECTION ( 'NONE',  ( 0.000000000000000000, 0.000000000000000000, -1.000000000000000000 ) ) ;
#233291 = EDGE_LOOP ( 'NONE', ( #189283, #214974, #228450, #233803, #22523, #181844, #888 ) ) ;
#233292 = DIRECTION ( 'NONE',  ( -1.000000000000000000, 0.000000000000000000, 0.000000000000000000 ) ) ;
#233293 = DIRECTION ( 'NONE',  ( 0.000000000000000000, 0.000000000000000000, 1.000000000000000000 ) ) ;
#233294 = CIRCLE ( 'NONE', #137396, 0.1000000000000000472 ) ;
#233295 = EDGE_CURVE ( 'NONE', #34034, #167845, #133180, .T. ) ;
#233296 = ORIENTED_EDGE ( 'NONE', *, *, #235385, .F. ) ;
#233297 = EDGE_LOOP ( 'NONE', ( #27836, #66495, #239631, #56388, #40347 ) ) ;
#233298 = CARTESIAN_POINT ( 'NONE',  ( 21.05000000000000071, -8.663551401857999323, -57.47589888193269303 ) ) ;
#233299 = VERTEX_POINT ( 'NONE', #89064 ) ;
#233301 = ORIENTED_EDGE ( 'NONE', *, *, #99306, .F. ) ;
#233300 = CARTESIAN_POINT ( 'NONE',  ( -18.40000000000000213, 61.75216633358002127, -212.7659468556851436 ) ) ;
#233302 = EDGE_CURVE ( 'NONE', #221915, #168895, #211602, .T. ) ;
#233303 = AXIS2_PLACEMENT_3D ( 'NONE', #55118, #52571, #211679 ) ;
#233306 = EDGE_LOOP ( 'NONE', ( #91014, #170107, #225092 ) ) ;
#233305 = ORIENTED_EDGE ( 'NONE', *, *, #216542, .F. ) ;
#233304 = CARTESIAN_POINT ( 'NONE',  ( -21.65000000000000213, 7.250000000011139534, -54.35000000000000142 ) ) ;
#233307 = CIRCLE ( 'NONE', #108399, 0.1000000000000024342 ) ;
#233308 = EDGE_CURVE ( 'NONE', #208354, #159539, #8459, .T. ) ;
#233309 = EDGE_CURVE ( 'NONE', #154602, #16613, #183347, .T. ) ;
#233310 = CYLINDRICAL_SURFACE ( 'NONE', #60595, 0.09999999999999939493 ) ;
#233311 = DIRECTION ( 'NONE',  ( -0.7071067811865127117, -0.7071067811865821007, 0.000000000000000000 ) ) ;
#233312 = DIRECTION ( 'NONE',  ( -0.000000000000000000, -0.8814952561688430555, 0.4721928772777346239 ) ) ;
#233313 = CIRCLE ( 'NONE', #224890, 0.09999999999999749367 ) ;
#233314 = FACE_OUTER_BOUND ( 'NONE', #44401, .T. ) ;
#233315 =( BOUNDED_CURVE ( )  B_SPLINE_CURVE ( 3, ( #195334, #16686, #175762, #255221 ),
 .UNSPECIFIED., .F., .T. ) 
 B_SPLINE_CURVE_WITH_KNOTS ( ( 4, 4 ),
 ( 1.570796326794908992, 2.617993877991506402 ),
 .UNSPECIFIED. ) 
 CURVE ( )  GEOMETRIC_REPRESENTATION_ITEM ( )  RATIONAL_B_SPLINE_CURVE ( ( 1.000000000000000000, 0.9106836025229592124, 0.9106836025229592124, 1.000000000000000000 ) ) 
 REPRESENTATION_ITEM ( '' )  );
#233316 = CIRCLE ( 'NONE', #141702, 0.1000000000000028644 ) ;
#233317 = DIRECTION ( 'NONE',  ( 0.000000000000000000, 0.000000000000000000, 1.000000000000000000 ) ) ;
#233318 = LINE ( 'NONE', #131618, #67690 ) ;
#233319 = EDGE_LOOP ( 'NONE', ( #193641, #125095, #126177, #141721 ) ) ;
#233320 = VERTEX_POINT ( 'NONE', #188186 ) ;
#233321 = EDGE_LOOP ( 'NONE', ( #181854, #80615, #99858, #223025 ) ) ;
#233323 = ORIENTED_EDGE ( 'NONE', *, *, #25441, .F. ) ;
#233322 = CARTESIAN_POINT ( 'NONE',  ( -20.94999999999999929, 87.48912529308817909, -133.6231074845242119 ) ) ;
#233324 = CARTESIAN_POINT ( 'NONE',  ( 23.14999999999999858, 11.60000000001116227, -93.57179676972454274 ) ) ;
#233325 = VERTEX_POINT ( 'NONE', #229877 ) ;
#233326 = ADVANCED_FACE ( 'NONE', ( #149072 ), #30404, .T. ) ;
#233327 = ORIENTED_EDGE ( 'NONE', *, *, #88027, .F. ) ;
#233328 = CARTESIAN_POINT ( 'NONE',  ( 23.40000000000005187, 77.25000000001119815, -43.92310748452479885 ) ) ;
#233329 = EDGE_CURVE ( 'NONE', #201937, #96904, #132056, .T. ) ;
#233330 = B_SPLINE_CURVE_WITH_KNOTS ( 'NONE', 3,
 ( #14762, #176395, #18589, #255858, #73452, #133402, #117679, #177687, #257137, #212935, #16043, #78541, #218039, #55105, #193389, #158141, #237637, #233792, #175142 ),
 .UNSPECIFIED., .F., .F.,
 ( 4, 3, 3, 3, 3, 3, 4 ),
 ( 0.000000000000000000, 2.646747978908405501E-05, 5.271166642128941309E-05, 9.008788829885368374E-05, 0.0001426648776561097631, 0.0001897378458659760203, 0.0001917382627806482609 ),
 .UNSPECIFIED. ) ;
#233332 = ORIENTED_EDGE ( 'NONE', *, *, #108317, .F. ) ;
#233331 = PRODUCT_RELATED_PRODUCT_CATEGORY ( 'part', '', ( #188868 ) ) ;
#233333 = AXIS2_PLACEMENT_3D ( 'NONE', #56897, #253836, #12704 ) ;
#233334 = AXIS2_PLACEMENT_3D ( 'NONE', #245102, #23525, #61332 ) ;
#233335 = DIRECTION ( 'NONE',  ( 1.000000000000000000, 0.000000000000000000, 0.000000000000000000 ) ) ;
#233336 = CARTESIAN_POINT ( 'NONE',  ( 18.49999999999999645, 68.58368164137472434, -224.2353459317783120 ) ) ;
#233338 = EDGE_LOOP ( 'NONE', ( #215562, #222583 ) ) ;
#233337 = EDGE_LOOP ( 'NONE', ( #39576, #256514, #200602, #199319 ) ) ;
#233339 = ORIENTED_EDGE ( 'NONE', *, *, #106728, .F. ) ;
#233340 = DIRECTION ( 'NONE',  ( -7.304098846218134667E-16, -1.000000000000000000, 0.000000000000000000 ) ) ;
#233341 = VERTEX_POINT ( 'NONE', #10831 ) ;
#233342 = ORIENTED_EDGE ( 'NONE', *, *, #89213, .T. ) ;
#233343 = ADVANCED_FACE ( 'NONE', ( #228604 ), #31705, .T. ) ;
#233344 = FACE_OUTER_BOUND ( 'NONE', #125209, .T. ) ;
#233346 = EDGE_LOOP ( 'NONE', ( #27057, #41554, #119832, #190219 ) ) ;
#233345 = CARTESIAN_POINT ( 'NONE',  ( 21.05000000000000071, 70.15000000001266756, -193.3906102602464330 ) ) ;
#233347 = ADVANCED_FACE ( 'NONE', ( #72098 ), #109910, .F. ) ;
#233348 = CARTESIAN_POINT ( 'NONE',  ( 23.14999999999999858, -3.899999999988843502, -100.5000000000000426 ) ) ;
#233349 = EDGE_CURVE ( 'NONE', #1289, #43098, #130767, .T. ) ;
#233350 = FACE_OUTER_BOUND ( 'NONE', #117865, .T. ) ;
#233351 = CARTESIAN_POINT ( 'NONE',  ( 20.94999999999999574, 62.98661795304985844, -207.1103002134590554 ) ) ;
#233352 = DIRECTION ( 'NONE',  ( 0.000000000000000000, -0.9126074666063772600, -0.4088369013363274407 ) ) ;
#233353 = DIRECTION ( 'NONE',  ( 0.000000000000000000, -2.775557561562888827E-14, 1.000000000000000000 ) ) ;
#233354 = ORIENTED_EDGE ( 'NONE', *, *, #18065, .T. ) ;
#233355 = EDGE_LOOP ( 'NONE', ( #140331, #144372, #79620, #26825, #189226, #235666, #143564, #21326, #225461, #190342, #245831, #30631, #197249, #103327, #103337, #120769, #118132, #100509, #197883, #158006, #248884, #104729, #193631 ) ) ;
#233356 = CARTESIAN_POINT ( 'NONE',  ( 21.15000000000005187, 76.00000000001119815, -31.97310748452479601 ) ) ;
#233358 = TOROIDAL_SURFACE ( 'NONE', #71035, 0.2000000000000000111, 0.1000000000000000056 ) ;
#233357 = DIRECTION ( 'NONE',  ( -0.7071067811865474617, 0.6824534298470372740, -0.1850873201762209819 ) ) ;
#233359 = DIRECTION ( 'NONE',  ( 0.000000000000000000, 0.8814952561688429444, -0.4721928772777349570 ) ) ;
#233360 = AXIS2_PLACEMENT_3D ( 'NONE', #148731, #45759, #129161 ) ;
#233362 = EDGE_CURVE ( 'NONE', #118259, #197543, #29267, .T. ) ;
#233361 = AXIS2_PLACEMENT_3D ( 'NONE', #59466, #221134, #60777 ) ;
#233363 = AXIS2_PLACEMENT_3D ( 'NONE', #15005, #115363, #116652 ) ;
#233364 = EDGE_LOOP ( 'NONE', ( #225026, #202751, #53290, #204866 ) ) ;
#233365 = CARTESIAN_POINT ( 'NONE',  ( -23.25000000000000000, 79.28653038861995128, -235.9126307598797325 ) ) ;
#233366 = DIRECTION ( 'NONE',  ( 0.000000000000000000, 0.000000000000000000, 1.000000000000000000 ) ) ;
#233367 = TOROIDAL_SURFACE ( 'NONE', #229257, 12.97499999999999787, 0.1000000000000000056 ) ;
#233368 = LINE ( 'NONE', #249068, #209309 ) ;
#233369 = ORIENTED_EDGE ( 'NONE', *, *, #245758, .T. ) ;
#233370 = VERTEX_POINT ( 'NONE', #91648 ) ;
#233371 = DIRECTION ( 'NONE',  ( 0.000000000000000000, -1.000000000000000000, 0.000000000000000000 ) ) ;
#233372 = CARTESIAN_POINT ( 'NONE',  ( 21.00000000000000000, 66.25000000001186606, -90.77310748452438816 ) ) ;
#233373 = VERTEX_POINT ( 'NONE', #231183 ) ;
#233374 = DIRECTION ( 'NONE',  ( -0.000000000000000000, -6.982962677686266711E-15, 1.000000000000000000 ) ) ;
#233375 = ORIENTED_EDGE ( 'NONE', *, *, #110845, .T. ) ;
#233376 = CARTESIAN_POINT ( 'NONE',  ( 23.14999999999999503, 69.45000000001157048, -57.17310748452436542 ) ) ;
#233378 = DIRECTION ( 'NONE',  ( 0.000000000000000000, 0.8814952561688429444, -0.4721928772777345684 ) ) ;
#233377 = SHAPE_REPRESENTATION ( 'Snap Open Cable Crossbars 7', ( #2425 ), #135129 ) ;
#233380 = DIRECTION ( 'NONE',  ( 1.186688945009010077E-16, -1.000000000000000000, -0.000000000000000000 ) ) ;
#233379 = DIRECTION ( 'NONE',  ( -1.000000000000000000, -0.000000000000000000, -0.000000000000000000 ) ) ;
#233381 = CARTESIAN_POINT ( 'NONE',  ( 18.58222699835054570, 65.66799936921584901, -164.4299399888601272 ) ) ;
#233382 = EDGE_CURVE ( 'NONE', #603, #183504, #151653, .T. ) ;
#233383 = VECTOR ( 'NONE', #82880, 1000.000000000000000 ) ;
#233384 = CARTESIAN_POINT ( 'NONE',  ( 21.10642757222115407, 65.27684371085327086, -90.78240996073918723 ) ) ;
#233385 = CARTESIAN_POINT ( 'NONE',  ( 23.14999999999999503, 11.65000000001116298, -122.2500000000000284 ) ) ;
#233387 = ORIENTED_EDGE ( 'NONE', *, *, #131256, .T. ) ;
#233386 = VERTEX_POINT ( 'NONE', #47363 ) ;
#233388 = ORIENTED_EDGE ( 'NONE', *, *, #33345, .F. ) ;
#233389 = ADVANCED_FACE ( 'NONE', ( #126925 ), #175023, .F. ) ;
#233390 = CARTESIAN_POINT ( 'NONE',  ( -23.15000000000000213, -11.64999999998884483, -164.4000000000000057 ) ) ;
#233391 = CARTESIAN_POINT ( 'NONE',  ( 22.50000000000000000, 0.09999999999999939493, 11.64957080754479968 ) ) ;
#233392 = FACE_BOUND ( 'NONE', #48918, .T. ) ;
#233394 = CARTESIAN_POINT ( 'NONE',  ( -15.06774609480955363, 66.58234804117083172, -87.66432009208392628 ) ) ;
#233393 = DIRECTION ( 'NONE',  ( 1.000000000000000000, 7.304098846218134667E-16, 5.100424963727256530E-30 ) ) ;
#233395 = FACE_OUTER_BOUND ( 'NONE', #11580, .T. ) ;
#233396 = ORIENTED_EDGE ( 'NONE', *, *, #119219, .F. ) ;
#233397 = EDGE_CURVE ( 'NONE', #60411, #174912, #8270, .T. ) ;
#233398 = DIRECTION ( 'NONE',  ( 0.000000000000000000, 0.000000000000000000, -1.000000000000000000 ) ) ;
#233399 = VERTEX_POINT ( 'NONE', #199437 ) ;
#233400 = VERTEX_POINT ( 'NONE', #2478 ) ;
#233401 = CARTESIAN_POINT ( 'NONE',  ( -20.64999999999999858, 24.17260720300848931, -252.6908294531417027 ) ) ;
#233402 = DIRECTION ( 'NONE',  ( 0.000000000000000000, 0.000000000000000000, -1.000000000000000000 ) ) ;
#233403 = DIRECTION ( 'NONE',  ( 0.000000000000000000, 0.1575844902526835067, 0.9875055080513738259 ) ) ;
#233404 = CIRCLE ( 'NONE', #162649, 0.09999999999998898659 ) ;
#233405 = DIRECTION ( 'NONE',  ( 0.000000000000000000, 0.000000000000000000, -1.000000000000000000 ) ) ;
#233406 = EDGE_CURVE ( 'NONE', #82775, #12289, #58602, .T. ) ;
#233407 = CARTESIAN_POINT ( 'NONE',  ( 22.49999999999999645, 0.04562336060741833954, -155.8494956614523517 ) ) ;
#233408 = EDGE_CURVE ( 'NONE', #114614, #248722, #200704, .T. ) ;
#233409 = ORIENTED_EDGE ( 'NONE', *, *, #228094, .T. ) ;
#233410 = VERTEX_POINT ( 'NONE', #178598 ) ;
#233411 = FACE_OUTER_BOUND ( 'NONE', #174996, .T. ) ;
#233412 = CARTESIAN_POINT ( 'NONE',  ( 18.49999999999999645, 76.00000000001213607, -136.5231074845242745 ) ) ;
#233413 = CARTESIAN_POINT ( 'NONE',  ( 19.90000000000000568, 1.350000000000000089, 21.90000000000000213 ) ) ;
#233414 = CARTESIAN_POINT ( 'NONE',  ( -20.94999999999999929, 76.00000000001213607, -136.5231074845243313 ) ) ;
#233415 = DIRECTION ( 'NONE',  ( 0.000000000000000000, -1.000000000000000000, -6.352154140967427193E-15 ) ) ;
#233416 = LINE ( 'NONE', #255467, #17430 ) ;
#233417 = CARTESIAN_POINT ( 'NONE',  ( 21.05000000000000071, 76.00000000001247713, -174.0231074845243882 ) ) ;
#233418 = CARTESIAN_POINT ( 'NONE',  ( 21.05000000000000071, 76.00000000001259082, -190.5481074845243654 ) ) ;
#233419 = CARTESIAN_POINT ( 'NONE',  ( -20.00857864376270001, 66.65000000001253966, -182.3731074845244393 ) ) ;
#233420 = DIRECTION ( 'NONE',  ( 0.000000000000000000, 0.000000000000000000, -1.000000000000000000 ) ) ;
#233421 = CYLINDRICAL_SURFACE ( 'NONE', #207886, 0.09999999999999939493 ) ;
#233422 = DIRECTION ( 'NONE',  ( 1.000000000000000000, 0.000000000000000000, 0.000000000000000000 ) ) ;
#233423 = CIRCLE ( 'NONE', #25303, 0.09999999999999939493 ) ;
#233425 = ORIENTED_EDGE ( 'NONE', *, *, #89405, .F. ) ;
#233424 = CARTESIAN_POINT ( 'NONE',  ( -21.14999999999999858, 64.25000000001210765, -129.7392418215462158 ) ) ;
#233427 = EDGE_CURVE ( 'NONE', #142820, #3343, #73399, .T. ) ;
#233426 = AXIS2_PLACEMENT_3D ( 'NONE', #230293, #189895, #128650 ) ;
#233428 = AXIS2_PLACEMENT_3D ( 'NONE', #9237, #130468, #227001 ) ;
#233429 = EDGE_CURVE ( 'NONE', #71547, #24899, #208300, .T. ) ;
#233430 = CARTESIAN_POINT ( 'NONE',  ( 23.14999999999999858, 64.35000000001218723, -143.5379132551783812 ) ) ;
#233431 = CIRCLE ( 'NONE', #154350, 0.1000000000000028644 ) ;
#233432 = AXIS2_PLACEMENT_3D ( 'NONE', #187659, #166825, #145927 ) ;
#233433 = CARTESIAN_POINT ( 'NONE',  ( -18.59999999999999787, -1.164121893230052995, -74.81484808557161159 ) ) ;
#233434 = EDGE_CURVE ( 'NONE', #134912, #81995, #20878, .T. ) ;
#233435 = FACE_OUTER_BOUND ( 'NONE', #40079, .T. ) ;
#233437 = ADVANCED_FACE ( 'NONE', ( #118616 ), #241604, .F. ) ;
#233436 = CARTESIAN_POINT ( 'NONE',  ( 20.94999999999999929, 76.00000000001190870, -103.0231074845243029 ) ) ;
#233438 = PLANE ( 'NONE',  #154665 ) ;
#233439 = AXIS2_PLACEMENT_3D ( 'NONE', #243677, #25925, #144561 ) ;
#233440 = CARTESIAN_POINT ( 'NONE',  ( -20.64999999999999858, 66.26558728512915764, -222.7970849955717938 ) ) ;
#233441 = VECTOR ( 'NONE', #1279, 1000.000000000000000 ) ;
#233442 = AXIS2_PLACEMENT_3D ( 'NONE', #51857, #188826, #66320 ) ;
#233443 = CARTESIAN_POINT ( 'NONE',  ( 20.94999999999999574, 62.00000000001210054, -131.0960149541418502 ) ) ;
#233444 = DIRECTION ( 'NONE',  ( 1.000000000000000000, 0.000000000000000000, 0.000000000000000000 ) ) ;
#233445 = VECTOR ( 'NONE', #81966, 1000.000000000000000 ) ;
#233446 = AXIS2_PLACEMENT_3D ( 'NONE', #244477, #202787, #243190 ) ;
#233447 = ORIENTED_EDGE ( 'NONE', *, *, #60027, .F. ) ;
#233448 = DIRECTION ( 'NONE',  ( 1.000000000000000000, 0.000000000000000000, 0.000000000000000000 ) ) ;
#233450 = EDGE_LOOP ( 'NONE', ( #103317, #212121, #254144, #52152, #101067, #159507, #235098, #129374, #2137, #126813, #200061, #200843, #9434, #70421, #181959, #238791, #192588, #130013, #61347, #124305, #37306, #87377, #92435 ) ) ;
#233449 = DIRECTION ( 'NONE',  ( 0.000000000000000000, 0.000000000000000000, -1.000000000000000000 ) ) ;
#233451 = DIRECTION ( 'NONE',  ( 0.000000000000000000, 0.000000000000000000, -1.000000000000000000 ) ) ;
#233452 = CARTESIAN_POINT ( 'NONE',  ( 21.13461538461538325, 23.02743022372036918, -230.2075788195831763 ) ) ;
#233453 = EDGE_CURVE ( 'NONE', #8169, #24665, #91764, .T. ) ;
#233454 = CARTESIAN_POINT ( 'NONE',  ( -20.94999999999999929, 1.115600667400684642E-11, -67.00000000000004263 ) ) ;
#233455 = ORIENTED_EDGE ( 'NONE', *, *, #175080, .F. ) ;
#233456 = DIRECTION ( 'NONE',  ( 0.000000000000000000, -0.4856429311786307212, -0.8741572761215384846 ) ) ;
#233457 = ADVANCED_FACE ( 'NONE', ( #41648 ), #59877, .T. ) ;
#233458 = SHAPE_DEFINITION_REPRESENTATION ( #53639, #170171 ) ;
#233459 = TOROIDAL_SURFACE ( 'NONE', #125114, 11.65000000000000036, 0.1000000000000000056 ) ;
#233460 = LINE ( 'NONE', #53512, #210576 ) ;
#233461 = FACE_OUTER_BOUND ( 'NONE', #182229, .T. ) ;
#233462 = ORIENTED_EDGE ( 'NONE', *, *, #180589, .T. ) ;
#233463 = CARTESIAN_POINT ( 'NONE',  ( 18.49999999999999289, 64.25000000001220712, -145.1731074845244507 ) ) ;
#233464 = CARTESIAN_POINT ( 'NONE',  ( -20.94999999999999929, 77.16270174995010223, -128.6231074845242972 ) ) ;
#233465 = CARTESIAN_POINT ( 'NONE',  ( 21.14999999999999858, 7.216982865709976380, -233.7799206001670598 ) ) ;
#233466 = VERTEX_POINT ( 'NONE', #62483 ) ;
#233467 = ORIENTED_EDGE ( 'NONE', *, *, #134772, .T. ) ;
#233468 = CARTESIAN_POINT ( 'NONE',  ( 21.00000000000000000, 9.750000000011153745, -79.35000000000005116 ) ) ;
#233469 = CIRCLE ( 'NONE', #200133, 0.1000000000000008937 ) ;
#233470 = FACE_OUTER_BOUND ( 'NONE', #70768, .T. ) ;
#233471 = CARTESIAN_POINT ( 'NONE',  ( 21.14999999999999503, 64.35000000001213039, -136.5231074845243597 ) ) ;
#233472 = CARTESIAN_POINT ( 'NONE',  ( -20.85000000000000142, 76.00000000001170974, -69.52310748452431710 ) ) ;
#233473 = AXIS2_PLACEMENT_3D ( 'NONE', #123599, #186135, #67464 ) ;
#233475 = CARTESIAN_POINT ( 'NONE',  ( 20.85000000000000142, 7.882824859404637508, -245.3558965132535832 ) ) ;
#233474 = FACE_OUTER_BOUND ( 'NONE', #54431, .T. ) ;
#233476 = DIRECTION ( 'NONE',  ( 1.000000000000000000, 7.304098846218134667E-16, -0.000000000000000000 ) ) ;
#233477 = DIRECTION ( 'NONE',  ( 0.000000000000000000, 0.2617529984164506107, 0.9651348961777299618 ) ) ;
#233478 = DIRECTION ( 'NONE',  ( 0.000000000000000000, 0.1350103645451876666, -0.9908441862701600211 ) ) ;
#233479 = CARTESIAN_POINT ( 'NONE',  ( -23.25000000000000000, 54.09940989982483472, -238.8890605415484174 ) ) ;
#233480 = ORIENTED_EDGE ( 'NONE', *, *, #133824, .F. ) ;
#233481 = VECTOR ( 'NONE', #86664, 1000.000000000000000 ) ;
#233482 = EDGE_CURVE ( 'NONE', #179279, #223322, #244284, .T. ) ;
#233483 = ORIENTED_EDGE ( 'NONE', *, *, #54054, .F. ) ;
#233484 = DIRECTION ( 'NONE',  ( 0.000000000000000000, 7.147358527629766941E-15, -1.000000000000000000 ) ) ;
#233485 = DIRECTION ( 'NONE',  ( 0.000000000000000000, 0.000000000000000000, 1.000000000000000000 ) ) ;
#233487 = FACE_OUTER_BOUND ( 'NONE', #249769, .T. ) ;
#233486 = CARTESIAN_POINT ( 'NONE',  ( -20.15000000000000568, 9.291421356248463326, -155.1500000000000057 ) ) ;
#233488 = CIRCLE ( 'NONE', #96068, 1.749999999999999778 ) ;
#233489 = CARTESIAN_POINT ( 'NONE',  ( -21.65000000000000213, 7.250000000011138646, -54.35000000000000142 ) ) ;
#233490 = CARTESIAN_POINT ( 'NONE',  ( 20.94999999999999574, 76.00000000001237765, -170.0231074845243597 ) ) ;
#233491 = CARTESIAN_POINT ( 'NONE',  ( 12.25000000000000355, 12.72457643131171423, -215.4883117230867811 ) ) ;
#233492 = EDGE_LOOP ( 'NONE', ( #96850, #23026, #41471, #104324 ) ) ;
#233493 = ORIENTED_EDGE ( 'NONE', *, *, #187401, .F. ) ;
#233494 = AXIS2_PLACEMENT_3D ( 'NONE', #122707, #257006, #182676 ) ;
#233495 = DIRECTION ( 'NONE',  ( 1.000000000000000000, -0.000000000000000000, 0.000000000000000000 ) ) ;
#233496 = ORIENTED_EDGE ( 'NONE', *, *, #37920, .T. ) ;
#233497 = EDGE_CURVE ( 'NONE', #74720, #225917, #42625, .T. ) ;
#233498 = DIRECTION ( 'NONE',  ( -0.000000000000000000, -0.000000000000000000, -1.000000000000000000 ) ) ;
#233499 = AXIS2_PLACEMENT_3D ( 'NONE', #177286, #254201, #237230 ) ;
#233500 = B_SPLINE_CURVE_WITH_KNOTS ( 'NONE', 3,
 ( #48811, #68390, #146609, #86626, #247004, #127072, #168814, #204031 ),
 .UNSPECIFIED., .F., .F.,
 ( 4, 2, 2, 4 ),
 ( 0.000000000000000000, 6.534141206311986901E-05, 0.0001306828241262397380, 0.0002613656482524943296 ),
 .UNSPECIFIED. ) ;
#233501 = AXIS2_PLACEMENT_3D ( 'NONE', #229199, #234313, #55644 ) ;
#233502 = CARTESIAN_POINT ( 'NONE',  ( 20.85000000000000142, 1.115600667400684642E-11, -175.4000000000000341 ) ) ;
#233503 = CARTESIAN_POINT ( 'NONE',  ( 20.95263205890659108, 8.895740107905192318, -142.4895084069416384 ) ) ;
#233504 = VECTOR ( 'NONE', #34818, 1000.000000000000227 ) ;
#233505 = ORIENTED_EDGE ( 'NONE', *, *, #148255, .F. ) ;
#233506 = CARTESIAN_POINT ( 'NONE',  ( 20.85000000000000142, -1.362429037182151470, -74.88888124792120493 ) ) ;
#233507 = DIRECTION ( 'NONE',  ( 0.000000000000000000, -6.982962677686266711E-15, 1.000000000000000000 ) ) ;
#233508 = CARTESIAN_POINT ( 'NONE',  ( 23.25000000000000000, -8.596261682231833845, -143.4501275171502925 ) ) ;
#233509 = FACE_OUTER_BOUND ( 'NONE', #87367, .T. ) ;
#233510 = CYLINDRICAL_SURFACE ( 'NONE', #122211, 4.000000000000003553 ) ;
#233512 = SPHERICAL_SURFACE ( 'NONE', #104020, 0.1000000000000000056 ) ;
#233511 = CYLINDRICAL_SURFACE ( 'NONE', #199739, 0.8750000000000007772 ) ;
#233513 = AXIS2_PLACEMENT_3D ( 'NONE', #57138, #137966, #97540 ) ;
#233514 = CARTESIAN_POINT ( 'NONE',  ( -16.97683810757273193, 66.05000000001224691, -149.7866841969855614 ) ) ;
#233515 = ORIENTED_EDGE ( 'NONE', *, *, #91740, .F. ) ;
#233517 = DIRECTION ( 'NONE',  ( -0.000000000000000000, -0.4791956752371546169, -0.8777080977375152360 ) ) ;
#233516 = DIRECTION ( 'NONE',  ( 1.000000000000000000, 0.000000000000000000, 0.000000000000000000 ) ) ;
#233518 = ORIENTED_EDGE ( 'NONE', *, *, #223648, .T. ) ;
#233520 = ORIENTED_EDGE ( 'NONE', *, *, #93236, .T. ) ;
#233519 = CARTESIAN_POINT ( 'NONE',  ( -21.05000000000000071, 76.00000000001213607, -136.5231074845243313 ) ) ;
#233521 = ORIENTED_EDGE ( 'NONE', *, *, #213221, .F. ) ;
#233522 = CARTESIAN_POINT ( 'NONE',  ( -23.25000000000000000, -1.249999999988843369, -175.3004807544151049 ) ) ;
#233523 = DIRECTION ( 'NONE',  ( -1.000000000000000000, 0.000000000000000000, -0.000000000000000000 ) ) ;
#233524 = CARTESIAN_POINT ( 'NONE',  ( -21.05000000000000071, 30.93333081445676314, -252.0793046437616454 ) ) ;
#233525 = CARTESIAN_POINT ( 'NONE',  ( -23.15000000000000213, -8.596261682242989366, -24.04987248284972523 ) ) ;
#233526 = VERTEX_POINT ( 'NONE', #61187 ) ;
#233527 = CARTESIAN_POINT ( 'NONE',  ( 22.49999999999999645, 64.35042919246788529, -203.6231074845244393 ) ) ;
#233528 = VERTEX_POINT ( 'NONE', #154237 ) ;
#233529 = CARTESIAN_POINT ( 'NONE',  ( -20.00857864376270001, 9.350000000011156942, -112.7500000000000284 ) ) ;
#233530 = VECTOR ( 'NONE', #196295, 1000.000000000000000 ) ;
#233531 = TOROIDAL_SURFACE ( 'NONE', #121119, 11.65000000000000036, 0.1000000000000000056 ) ;
#233532 = EDGE_CURVE ( 'NONE', #180099, #122938, #70949, .T. ) ;
#233534 = AXIS2_PLACEMENT_3D ( 'NONE', #208074, #7273, #168973 ) ;
#233533 = CARTESIAN_POINT ( 'NONE',  ( 21.08198257630413508, 6.336596734015063959, 0.07264332378460747197 ) ) ;
#233535 = ORIENTED_EDGE ( 'NONE', *, *, #104727, .F. ) ;
#233536 = ORIENTED_EDGE ( 'NONE', *, *, #48514, .T. ) ;
#233537 = CARTESIAN_POINT ( 'NONE',  ( 20.94999999999999929, 30.48950451747912993, -239.6099224343151946 ) ) ;
#233538 = ORIENTED_EDGE ( 'NONE', *, *, #137590, .F. ) ;
#233539 = AXIS2_PLACEMENT_3D ( 'NONE', #246898, #82662, #27900 ) ;
#233540 = ORIENTED_EDGE ( 'NONE', *, *, #198549, .F. ) ;
#233541 = CARTESIAN_POINT ( 'NONE',  ( 23.15000000000000213, 87.65000000001172964, -72.62310748452422615 ) ) ;
#233542 = EDGE_CURVE ( 'NONE', #78788, #48124, #121200, .T. ) ;
#233543 = CYLINDRICAL_SURFACE ( 'NONE', #2246, 0.1000000000000028644 ) ;
#233544 = CARTESIAN_POINT ( 'NONE',  ( 20.94999999999999929, 69.55000000001261640, -193.5060803140843859 ) ) ;
#233545 = EDGE_CURVE ( 'NONE', #84743, #211078, #199930, .T. ) ;
#233546 = DIRECTION ( 'NONE',  ( 0.000000000000000000, 0.9908441862701605762, 0.1350103645451835310 ) ) ;
#233547 = VECTOR ( 'NONE', #193038, 1000.000000000000000 ) ;
#233548 = PLANE ( 'NONE',  #71282 ) ;
#233549 = EDGE_CURVE ( 'NONE', #204755, #248722, #58416, .T. ) ;
#233550 = CARTESIAN_POINT ( 'NONE',  ( 18.54271179734059061, -9.624084290087575155, -73.74096485270030144 ) ) ;
#233551 = CARTESIAN_POINT ( 'NONE',  ( 18.59999999999999076, -1.249999999988843369, -142.0000000000000284 ) ) ;
#233552 = ORIENTED_EDGE ( 'NONE', *, *, #238878, .T. ) ;
#233554 = DIRECTION ( 'NONE',  ( 0.000000000000000000, -0.8814952561688430555, 0.4721928772777346239 ) ) ;
#233553 = DIRECTION ( 'NONE',  ( -2.952720810173289112E-16, -1.000000000000000000, -6.982962677686266711E-15 ) ) ;
#233555 = ORIENTED_EDGE ( 'NONE', *, *, #61233, .T. ) ;
#233557 = ORIENTED_EDGE ( 'NONE', *, *, #188346, .T. ) ;
#233556 = CARTESIAN_POINT ( 'NONE',  ( -20.94999999999999929, 43.51422117117169819, -240.0698702536254530 ) ) ;
#233558 = ORIENTED_EDGE ( 'NONE', *, *, #245504, .F. ) ;
#233559 = CYLINDRICAL_SURFACE ( 'NONE', #126851, 0.09999999999999982514 ) ;
#233560 = DIRECTION ( 'NONE',  ( 2.259780016855445309E-14, -0.9875055080513764905, 0.1575844902526679359 ) ) ;
#233561 = CARTESIAN_POINT ( 'NONE',  ( 18.50000000000000000, 37.99112772578902764, -261.0419300540664835 ) ) ;
#233562 = DIRECTION ( 'NONE',  ( -1.000000000000000000, -0.000000000000000000, -0.000000000000000000 ) ) ;
#233563 = ORIENTED_EDGE ( 'NONE', *, *, #32961, .T. ) ;
#233565 = ORIENTED_EDGE ( 'NONE', *, *, #255629, .F. ) ;
#233564 = CARTESIAN_POINT ( 'NONE',  ( 19.97071067811864609, 11.72071067812981404, -192.2499999999999716 ) ) ;
#233566 = ADVANCED_FACE ( 'NONE', ( #74694 ), #19508, .T. ) ;
#233568 = CARTESIAN_POINT ( 'NONE',  ( 20.95378194480896639, 10.53491199154278668, -7.565054148147858371 ) ) ;
#233567 = CARTESIAN_POINT ( 'NONE',  ( -18.59999999999999787, 68.13014604066189861, -227.7202878558733516 ) ) ;
#233570 = ORIENTED_EDGE ( 'NONE', *, *, #110219, .T. ) ;
#233569 = DIRECTION ( 'NONE',  ( -0.7071067811865474617, -0.7071067811865474617, -0.000000000000000000 ) ) ;
#233571 = AXIS2_PLACEMENT_3D ( 'NONE', #34604, #209364, #234055 ) ;
#233572 = ORIENTED_EDGE ( 'NONE', *, *, #22381, .T. ) ;
#233573 = AXIS2_PLACEMENT_3D ( 'NONE', #121005, #161402, #178411 ) ;
#233574 = CARTESIAN_POINT ( 'NONE',  ( 22.49999999999999645, 11.64987090377452184, -167.4174801091270126 ) ) ;
#233575 = LINE ( 'NONE', #134436, #134623 ) ;
#233576 = ORIENTED_EDGE ( 'NONE', *, *, #118348, .T. ) ;
#233577 = FACE_OUTER_BOUND ( 'NONE', #228247, .T. ) ;
#233578 = ORIENTED_EDGE ( 'NONE', *, *, #2175, .T. ) ;
#233579 = VECTOR ( 'NONE', #45782, 1000.000000000000000 ) ;
#233580 = CARTESIAN_POINT ( 'NONE',  ( -16.77683809663752257, 33.06517536918362055, -220.7872234046467952 ) ) ;
#233581 = DIRECTION ( 'NONE',  ( -1.000000000000000000, -2.952720810173289112E-16, 0.000000000000000000 ) ) ;
#233582 = ORIENTED_EDGE ( 'NONE', *, *, #135771, .T. ) ;
#233583 = CARTESIAN_POINT ( 'NONE',  ( 21.05000000000000071, 56.88144095856731752, -233.0481614001508319 ) ) ;
#233584 = VECTOR ( 'NONE', #76316, 1000.000000000000000 ) ;
#233585 = DIRECTION ( 'NONE',  ( -1.000000000000000000, -0.000000000000000000, -0.000000000000000000 ) ) ;
#233586 = AXIS2_PLACEMENT_3D ( 'NONE', #121924, #22839, #3226 ) ;
#233587 = EDGE_CURVE ( 'NONE', #4255, #119770, #50225, .T. ) ;
#233589 = ORIENTED_EDGE ( 'NONE', *, *, #97443, .F. ) ;
#233588 = VECTOR ( 'NONE', #105849, 1000.000000000000000 ) ;
#233590 = EDGE_LOOP ( 'NONE', ( #238309, #246500 ) ) ;
#233591 = CARTESIAN_POINT ( 'NONE',  ( 18.52130828395272033, -9.481395502614633486, -107.5245067238836612 ) ) ;
#233592 = AXIS2_PLACEMENT_3D ( 'NONE', #176049, #216424, #76911 ) ;
#233593 = ORIENTED_EDGE ( 'NONE', *, *, #111678, .F. ) ;
#233594 = ORIENTED_EDGE ( 'NONE', *, *, #13262, .T. ) ;
#233596 = ORIENTED_EDGE ( 'NONE', *, *, #125405, .F. ) ;
#233595 = DIRECTION ( 'NONE',  ( 1.000000000000000000, 0.000000000000000000, -0.000000000000000000 ) ) ;
#233597 = AXIS2_PLACEMENT_3D ( 'NONE', #2356, #83153, #44075 ) ;
#233599 = EDGE_CURVE ( 'NONE', #119433, #124911, #150227, .T. ) ;
#233598 = CIRCLE ( 'NONE', #91926, 0.1000000000000024342 ) ;
#233600 = ORIENTED_EDGE ( 'NONE', *, *, #54019, .F. ) ;
#233601 = DIRECTION ( 'NONE',  ( 1.000000000000000000, 0.000000000000000000, 0.000000000000000000 ) ) ;
#233602 = ORIENTED_EDGE ( 'NONE', *, *, #26632, .F. ) ;
#233605 = ORIENTED_EDGE ( 'NONE', *, *, #64222, .T. ) ;
#233604 = ORIENTED_EDGE ( 'NONE', *, *, #127815, .T. ) ;
#233603 = DIRECTION ( 'NONE',  ( 0.000000000000000000, 1.224646799142185182E-16, 1.000000000000000000 ) ) ;
#233606 = EDGE_CURVE ( 'NONE', #16075, #224301, #148439, .T. ) ;
#233607 = VERTEX_POINT ( 'NONE', #242381 ) ;
#233608 = VECTOR ( 'NONE', #196220, 1000.000000000000114 ) ;
#233609 = VECTOR ( 'NONE', #54884, 1000.000000000000114 ) ;
#233610 = AXIS2_PLACEMENT_3D ( 'NONE', #203597, #45808, #44536 ) ;
#233611 = TOROIDAL_SURFACE ( 'NONE', #142014, 12.97499999999999787, 0.1000000000000000056 ) ;
#233612 = CIRCLE ( 'NONE', #246264, 0.09999999999998898659 ) ;
#233613 = CARTESIAN_POINT ( 'NONE',  ( 21.11747605621531321, 8.778708005504054057, -45.74456316978977810 ) ) ;
#233614 = ORIENTED_EDGE ( 'NONE', *, *, #204837, .F. ) ;
#233615 = CARTESIAN_POINT ( 'NONE',  ( -16.93262454970419384, 10.00202046794151478, -154.9270762262373182 ) ) ;
#233616 = EDGE_CURVE ( 'NONE', #159674, #234753, #222814, .T. ) ;
#233618 = ORIENTED_EDGE ( 'NONE', *, *, #4293, .F. ) ;
#233617 = CARTESIAN_POINT ( 'NONE',  ( -20.94999999999999929, 74.83729825007360148, -61.52310748452433131 ) ) ;
#233619 = CARTESIAN_POINT ( 'NONE',  ( -21.14999999999999858, 87.65000000001238334, -170.0231074845242745 ) ) ;
#233620 = ORIENTED_EDGE ( 'NONE', *, *, #179866, .T. ) ;
#233621 = ORIENTED_EDGE ( 'NONE', *, *, #129390, .F. ) ;
#233622 = ADVANCED_FACE ( 'NONE', ( #3783 ), #102854, .T. ) ;
#233623 = EDGE_CURVE ( 'NONE', #156996, #33770, #229329, .T. ) ;
#233624 = AXIS2_PLACEMENT_3D ( 'NONE', #194200, #174670, #14280 ) ;
#233625 = CARTESIAN_POINT ( 'NONE',  ( 18.50211644919734866, 18.36312997293287097, -236.9042258689303821 ) ) ;
#233626 = ORIENTED_EDGE ( 'NONE', *, *, #227413, .T. ) ;
#233627 = ORIENTED_EDGE ( 'NONE', *, *, #93148, .T. ) ;
#233628 = CARTESIAN_POINT ( 'NONE',  ( 20.94999999999999929, 77.83534155023646406, -124.9679561919612922 ) ) ;
#233629 = FACE_OUTER_BOUND ( 'NONE', #15804, .T. ) ;
#233630 = EDGE_CURVE ( 'NONE', #165825, #59337, #166812, .T. ) ;
#233632 = ORIENTED_EDGE ( 'NONE', *, *, #250444, .T. ) ;
#233631 = ORIENTED_EDGE ( 'NONE', *, *, #78815, .F. ) ;
#233633 = ORIENTED_EDGE ( 'NONE', *, *, #207522, .F. ) ;
#233634 = CARTESIAN_POINT ( 'NONE',  ( 22.39999999999999503, 76.10000000001276987, -215.1726782920691505 ) ) ;
#233635 = ORIENTED_EDGE ( 'NONE', *, *, #87684, .T. ) ;
#233636 = ORIENTED_EDGE ( 'NONE', *, *, #31450, .T. ) ;
#233637 = CARTESIAN_POINT ( 'NONE',  ( -23.25000000000000000, 11.65000000001115588, -93.48519422934609224 ) ) ;
#233638 = ORIENTED_EDGE ( 'NONE', *, *, #42080, .T. ) ;
#233639 = EDGE_CURVE ( 'NONE', #125547, #105539, #127788, .T. ) ;
#233640 = CARTESIAN_POINT ( 'NONE',  ( -16.94445028196808778, 12.44605341304038859, -211.1922452800140775 ) ) ;
#233641 = EDGE_CURVE ( 'NONE', #76960, #170856, #83289, .T. ) ;
#233642 = CARTESIAN_POINT ( 'NONE',  ( -21.05000000000000071, 76.00000000001199396, -114.8231074845243000 ) ) ;
#233643 = CIRCLE ( 'NONE', #382, 0.1000000000000028644 ) ;
#233644 = VERTEX_POINT ( 'NONE', #184989 ) ;
#233645 = VERTEX_POINT ( 'NONE', #46745 ) ;
#233646 = B_SPLINE_CURVE_WITH_KNOTS ( 'NONE', 3,
 ( #177926, #193628, #116651, #256094, #172823, #15004 ),
 .UNSPECIFIED., .F., .F.,
 ( 4, 2, 4 ),
 ( 0.000000000000000000, 0.0001568709654583420778, 0.0003137419309166841557 ),
 .UNSPECIFIED. ) ;
#233647 = FACE_OUTER_BOUND ( 'NONE', #240789, .T. ) ;
#233648 = ORIENTED_EDGE ( 'NONE', *, *, #131007, .F. ) ;
#233649 = AXIS2_PLACEMENT_3D ( 'NONE', #188367, #73590, #230063 ) ;
#233650 = AXIS2_PLACEMENT_3D ( 'NONE', #151946, #253572, #14994 ) ;
#233651 = CARTESIAN_POINT ( 'NONE',  ( 21.05000000000000071, 61.95000000001194707, -108.5368025552853197 ) ) ;
#233652 = VERTEX_POINT ( 'NONE', #224101 ) ;
#233653 = ADVANCED_FACE ( 'NONE', ( #28531 ), #143287, .T. ) ;
#233654 = ORIENTED_EDGE ( 'NONE', *, *, #150565, .F. ) ;
#233655 = ADVANCED_FACE ( 'NONE', ( #128878 ), #126286, .F. ) ;
#233656 = CARTESIAN_POINT ( 'NONE',  ( -20.64999999999999858, 73.60000000001184617, -89.79848556176223440 ) ) ;
#233658 = ORIENTED_EDGE ( 'NONE', *, *, #234929, .T. ) ;
#233657 = CARTESIAN_POINT ( 'NONE',  ( 18.51997666896864914, 85.39233213153103463, -162.8797012970400999 ) ) ;
#233659 = DIRECTION ( 'NONE',  ( 0.000000000000000000, -0.9770955615653357240, -0.2128009952263406890 ) ) ;
#233660 = LINE ( 'NONE', #158008, #180901 ) ;
#233661 = CYLINDRICAL_SURFACE ( 'NONE', #102101, 0.09999999999999939493 ) ;
#233662 = DIRECTION ( 'NONE',  ( 0.000000000000000000, 1.000000000000000000, 0.000000000000000000 ) ) ;
#233663 = DIRECTION ( 'NONE',  ( 1.000000000000000000, -3.265361837132813093E-16, -2.280189983783949500E-30 ) ) ;
#233664 = CARTESIAN_POINT ( 'NONE',  ( -20.85000000000000142, 43.17747518314618560, -245.0773422074893233 ) ) ;
#233665 = DIRECTION ( 'NONE',  ( -1.000000000000000000, 0.000000000000000000, 0.000000000000000000 ) ) ;
#233666 = CARTESIAN_POINT ( 'NONE',  ( 21.70464131381650219, 33.75808023539804736, -243.0758859948899726 ) ) ;
#233667 = CARTESIAN_POINT ( 'NONE',  ( -21.07928932188134041, 69.67148334361836248, -69.62200263017875557 ) ) ;
#233668 = EDGE_CURVE ( 'NONE', #184435, #32558, #100108, .T. ) ;
#233669 = LINE ( 'NONE', #75867, #91036 ) ;
#233670 = CARTESIAN_POINT ( 'NONE',  ( 23.25000000000000000, 85.60000000001222986, -148.2731074845242460 ) ) ;
#233671 = AXIS2_PLACEMENT_3D ( 'NONE', #139385, #218933, #200672 ) ;
#233672 = ORIENTED_EDGE ( 'NONE', *, *, #143343, .T. ) ;
#233673 = AXIS2_PLACEMENT_3D ( 'NONE', #101137, #200296, #137733 ) ;
#233674 = CIRCLE ( 'NONE', #67067, 0.09999999999999642508 ) ;
#233676 = ORIENTED_EDGE ( 'NONE', *, *, #154338, .T. ) ;
#233675 = ORIENTED_EDGE ( 'NONE', *, *, #23373, .F. ) ;
#233677 = EDGE_LOOP ( 'NONE', ( #93737, #115111, #126138, #139649 ) ) ;
#233678 = DIRECTION ( 'NONE',  ( 0.000000000000000000, 0.5868805631290353597, 0.8096735173027127530 ) ) ;
#233679 =( BOUNDED_SURFACE ( )  B_SPLINE_SURFACE ( 3, 2, ( 
 ( #212595, #234717, #35264 ),
 ( #114766, #135591, #153942 ),
 ( #54777, #36549, #134305 ),
 ( #136891, #15698, #173513 ) ),
 .UNSPECIFIED., .F., .F., .F. ) 
 B_SPLINE_SURFACE_WITH_KNOTS ( ( 4, 4 ),
 ( 3, 3 ),
 ( 0.0006461284895273954445, 0.0007503702773986383346 ),
 ( 0.000000000000000000, 1.000000000000000000 ),
 .UNSPECIFIED. ) 
 GEOMETRIC_REPRESENTATION_ITEM ( )  RATIONAL_B_SPLINE_SURFACE ( (
 ( 1.000000000000000000, 0.7071067811865576758, 1.000000000000000000),
 ( 1.000000000000000000, 0.7076476444649448805, 1.000000000000000000),
 ( 1.000000000000000000, 0.7075727925190935519, 1.000000000000000000),
 ( 1.000000000000000000, 0.7071067811866011965, 1.000000000000000000) ) ) 
 REPRESENTATION_ITEM ( '' )  SURFACE ( )  );
#233680 = DIRECTION ( 'NONE',  ( 1.000000000000000000, -7.304098846218133681E-16, 4.607487905232622991E-31 ) ) ;
#233682 = CARTESIAN_POINT ( 'NONE',  ( -22.39999999999999858, 30.95512775545487472, -252.1063933345974988 ) ) ;
#233681 = CARTESIAN_POINT ( 'NONE',  ( 23.24999999999999289, 21.06094381221970124, -233.8786389445302518 ) ) ;
#233683 = ORIENTED_EDGE ( 'NONE', *, *, #135882, .T. ) ;
#233684 = ORIENTED_EDGE ( 'NONE', *, *, #136173, .F. ) ;
#233685 = ADVANCED_FACE ( 'NONE', ( #87152, #24661, #165437 ), #166744, .T. ) ;
#233686 = DIRECTION ( 'NONE',  ( -0.000000000000000000, 1.000000000000000000, -1.224646799147352961E-16 ) ) ;
#233687 = DIRECTION ( 'NONE',  ( -0.000000000000000000, -0.8814952561688432775, 0.4721928772777344019 ) ) ;
#233689 = VECTOR ( 'NONE', #139899, 1000.000000000000000 ) ;
#233688 = CARTESIAN_POINT ( 'NONE',  ( -16.89268316805466341, 9.951721813253341153, -180.1442475214544174 ) ) ;
#233690 = ADVANCED_FACE ( 'NONE', ( #106711 ), #84550, .T. ) ;
#233691 = CARTESIAN_POINT ( 'NONE',  ( 18.59999999999999076, 6.650000000011155876, -54.85000000000000142 ) ) ;
#233692 = ORIENTED_EDGE ( 'NONE', *, *, #247000, .T. ) ;
#233693 = ORIENTED_EDGE ( 'NONE', *, *, #50614, .F. ) ;
#233694 = LINE ( 'NONE', #155472, #213254 ) ;
#233695 = CARTESIAN_POINT ( 'NONE',  ( -23.25000000000000000, 84.59626168225560150, -194.0729799673740104 ) ) ;
#233696 = ADVANCED_FACE ( 'NONE', ( #88421 ), #94859, .F. ) ;
#233697 = EDGE_CURVE ( 'NONE', #18425, #160419, #111882, .T. ) ;
#233698 = ORIENTED_EDGE ( 'NONE', *, *, #26508, .F. ) ;
#233699 = DIRECTION ( 'NONE',  ( 0.000000000000000000, 0.8127272543710951647, -0.5826443254700256480 ) ) ;
#233701 = VERTEX_POINT ( 'NONE', #32367 ) ;
#233700 = DIRECTION ( 'NONE',  ( 0.000000000000000000, -0.9915357197604849349, 0.1298341882520056834 ) ) ;
#233702 = CARTESIAN_POINT ( 'NONE',  ( -23.15000000000000213, 87.65000000001215597, -139.6231074845242688 ) ) ;
#233703 = CARTESIAN_POINT ( 'NONE',  ( -17.11825945287481332, 10.05000000001113847, -188.3499999999999659 ) ) ;
#233704 = EDGE_CURVE ( 'NONE', #122006, #176334, #175199, .T. ) ;
#233705 = ORIENTED_EDGE ( 'NONE', *, *, #236971, .F. ) ;
#233706 = DIRECTION ( 'NONE',  ( 0.000000000000000000, 1.000000000000000000, 0.000000000000000000 ) ) ;
#233707 = DIRECTION ( 'NONE',  ( 0.000000000000000000, -0.2617529984165031243, -0.9651348961777157509 ) ) ;
#233708 = DIRECTION ( 'NONE',  ( -0.000000000000000000, 0.9770955615653313941, 0.2128009952263603954 ) ) ;
#233709 = AXIS2_PLACEMENT_3D ( 'NONE', #244412, #124487, #85316 ) ;
#233712 = DIRECTION ( 'NONE',  ( 0.000000000000000000, -8.881784197001252323E-16, 1.000000000000000000 ) ) ;
#233711 = AXIS2_PLACEMENT_3D ( 'NONE', #171344, #190885, #189582 ) ;
#233710 = CARTESIAN_POINT ( 'NONE',  ( -16.79139129368504513, 66.05505583755036980, -123.8528628516985322 ) ) ;
#233714 = CARTESIAN_POINT ( 'NONE',  ( -23.25000000000000000, 78.06784868750165174, -195.8985418047209350 ) ) ;
#233713 = CIRCLE ( 'NONE', #125544, 0.1000000000000070832 ) ;
#233715 = VECTOR ( 'NONE', #117632, 1000.000000000000000 ) ;
#233716 = DIRECTION ( 'NONE',  ( 0.000000000000000000, 0.2617529984165022361, 0.9651348961777160840 ) ) ;
#233717 = FACE_OUTER_BOUND ( 'NONE', #117542, .T. ) ;
#233718 = CARTESIAN_POINT ( 'NONE',  ( -20.94999999999999929, 6.846123162363745074, -104.2377262668499043 ) ) ;
#233719 = EDGE_LOOP ( 'NONE', ( #185199, #65189, #243703, #40852 ) ) ;
#233720 = ADVANCED_FACE ( 'NONE', ( #89723 ), #14068, .F. ) ;
#233721 = EDGE_CURVE ( 'NONE', #232502, #208402, #187644, .T. ) ;
#233722 = ORIENTED_EDGE ( 'NONE', *, *, #111288, .F. ) ;
#233723 = FACE_OUTER_BOUND ( 'NONE', #36861, .T. ) ;
#233724 = VERTEX_POINT ( 'NONE', #93588 ) ;
#233725 = EDGE_CURVE ( 'NONE', #131422, #86347, #125276, .T. ) ;
#233726 = DIRECTION ( 'NONE',  ( 0.000000000000000000, -0.8814952561688399468, 0.4721928772777404526 ) ) ;
#233727 = VECTOR ( 'NONE', #222846, 1000.000000000000000 ) ;
#233728 = VERTEX_POINT ( 'NONE', #135262 ) ;
#233729 = ORIENTED_EDGE ( 'NONE', *, *, #56886, .F. ) ;
#233730 = EDGE_CURVE ( 'NONE', #142373, #251099, #231831, .T. ) ;
#233731 = CARTESIAN_POINT ( 'NONE',  ( 21.07928932188134397, 6.328516656404459262, -66.90110485434564680 ) ) ;
#233732 = ORIENTED_EDGE ( 'NONE', *, *, #63015, .T. ) ;
#233733 = DIRECTION ( 'NONE',  ( 1.000000000000000000, 0.000000000000000000, 0.000000000000000000 ) ) ;
#233734 = CARTESIAN_POINT ( 'NONE',  ( -23.39999999999994529, 87.50449464844290048, -37.85861909827351468 ) ) ;
#233735 = DIRECTION ( 'NONE',  ( 0.000000000000000000, -0.1350103645451904977, -0.9908441862701596881 ) ) ;
#233736 = ADVANCED_FACE ( 'NONE', ( #131425 ), #71484, .F. ) ;
#233737 = CARTESIAN_POINT ( 'NONE',  ( 18.45068634130097962, 85.48650607335487450, -129.4543290533561901 ) ) ;
#233738 = DIRECTION ( 'NONE',  ( -0.000000000000000000, 6.982962677686266711E-15, -1.000000000000000000 ) ) ;
#233740 = EDGE_LOOP ( 'NONE', ( #193884, #76597, #66448, #81902 ) ) ;
#233739 = DIRECTION ( 'NONE',  ( 1.000000000000000000, 0.000000000000000000, 0.000000000000000000 ) ) ;
#233742 = CARTESIAN_POINT ( 'NONE',  ( -20.94999999999999929, 87.48912529308842068, -167.1231074845242688 ) ) ;
#233741 = DIRECTION ( 'NONE',  ( -0.000000000000000000, 1.000000000000000000, -0.000000000000000000 ) ) ;
#233744 = DIRECTION ( 'NONE',  ( 0.000000000000000000, -6.982962677686266711E-15, 1.000000000000000000 ) ) ;
#233743 = CIRCLE ( 'NONE', #229638, 0.09999999999999939493 ) ;
#233745 = EDGE_CURVE ( 'NONE', #169097, #96084, #191832, .T. ) ;
#233746 = PLANE ( 'NONE',  #194107 ) ;
#233747 = CARTESIAN_POINT ( 'NONE',  ( -13.88555196119803803, 9.457431528860068326, -115.4999169378996839 ) ) ;
#233748 = ORIENTED_EDGE ( 'NONE', *, *, #121236, .F. ) ;
#233749 = ADVANCED_FACE ( 'NONE', ( #192696 ), #37808, .T. ) ;
#233750 = CIRCLE ( 'NONE', #179589, 11.65000000000000746 ) ;
#233751 = CYLINDRICAL_SURFACE ( 'NONE', #196009, 7.899999999999995914 ) ;
#233752 = ORIENTED_EDGE ( 'NONE', *, *, #134058, .F. ) ;
#233753 = AXIS2_PLACEMENT_3D ( 'NONE', #36007, #115518, #257542 ) ;
#233754 = PLANE ( 'NONE',  #160618 ) ;
#233755 = ORIENTED_EDGE ( 'NONE', *, *, #204543, .F. ) ;
#233756 = CARTESIAN_POINT ( 'NONE',  ( -20.65000000000000568, 20.94763808724815846, -234.7254930126486556 ) ) ;
#233758 = CARTESIAN_POINT ( 'NONE',  ( -22.39999999999999858, 64.35000000001268461, -203.6231074845244393 ) ) ;
#233757 = AXIS2_PLACEMENT_3D ( 'NONE', #36530, #178607, #76897 ) ;
#233759 = FACE_OUTER_BOUND ( 'NONE', #194215, .T. ) ;
#233760 = EDGE_CURVE ( 'NONE', #199540, #7969, #151003, .T. ) ;
#233761 = EDGE_LOOP ( 'NONE', ( #125195, #238294, #169996, #130957 ) ) ;
#233762 = EDGE_LOOP ( 'NONE', ( #114460, #61967, #47887, #160007 ) ) ;
#233763 = AXIS2_PLACEMENT_3D ( 'NONE', #48612, #245549, #46043 ) ;
#233765 = ADVANCED_FACE ( 'NONE', ( #230541 ), #51870, .F. ) ;
#233764 = FACE_OUTER_BOUND ( 'NONE', #41704, .T. ) ;
#233766 = DIRECTION ( 'NONE',  ( 7.304098846218134667E-16, -1.000000000000000000, 0.000000000000000000 ) ) ;
#233767 = CARTESIAN_POINT ( 'NONE',  ( -16.80621392010911563, 63.08289460196063203, -213.1678741730786157 ) ) ;
#233768 = DIRECTION ( 'NONE',  ( 0.000000000000000000, -6.982962677686266711E-15, 1.000000000000000000 ) ) ;
#233770 = CARTESIAN_POINT ( 'NONE',  ( -20.85000000000000142, -1.835859311432481045, -212.5044391687984842 ) ) ;
#233769 = CARTESIAN_POINT ( 'NONE',  ( 18.39999999999999503, 5.650000000011139001, -46.15000000000000568 ) ) ;
#233771 = AXIS2_PLACEMENT_3D ( 'NONE', #225470, #46837, #84658 ) ;
#233772 = CARTESIAN_POINT ( 'NONE',  ( -20.94999999999999929, 7.675662554762638479, -241.7139905447625381 ) ) ;
#233773 = VECTOR ( 'NONE', #59693, 1000.000000000000000 ) ;
#233774 = ORIENTED_EDGE ( 'NONE', *, *, #114615, .F. ) ;
#233775 = DIRECTION ( 'NONE',  ( 1.000000000000000000, 0.000000000000000000, 0.000000000000000000 ) ) ;
#233777 = ORIENTED_EDGE ( 'NONE', *, *, #42101, .F. ) ;
#233776 = DIRECTION ( 'NONE',  ( 1.000000000000000000, 0.000000000000000000, 0.000000000000000000 ) ) ;
#233778 = DIRECTION ( 'NONE',  ( 1.000000000000000000, 8.674042436075353235E-17, 1.619280515896125144E-16 ) ) ;
#233779 = FACE_OUTER_BOUND ( 'NONE', #226612, .T. ) ;
#233781 = CARTESIAN_POINT ( 'NONE',  ( -18.69999999999999929, 1.149999999999999911, 21.90000000000000213 ) ) ;
#233780 = CARTESIAN_POINT ( 'NONE',  ( 18.79999999999999716, 11.61130914238355771, 16.50000000000000000 ) ) ;
#233783 =( BOUNDED_SURFACE ( )  B_SPLINE_SURFACE ( 3, 2, ( 
 ( #135617, #75677, #176073 ),
 ( #112236, #215166, #113499 ),
 ( #212613, #253003, #255522 ),
 ( #250438, #254273, #173530 ) ),
 .UNSPECIFIED., .F., .F., .T. ) 
 B_SPLINE_SURFACE_WITH_KNOTS ( ( 4, 4 ),
 ( 3, 3 ),
 ( 3.658908243880887756, 4.712388980384689674 ),
 ( 0.000000000000000000, 1.000000000000000000 ),
 .UNSPECIFIED. ) 
 GEOMETRIC_REPRESENTATION_ITEM ( )  RATIONAL_B_SPLINE_SURFACE ( (
 ( 1.000000000000000000, 0.8984936768950779751, 1.000000000000000000),
 ( 1.000000000000000000, 0.8646876308615198958, 1.000000000000000000),
 ( 1.000000000000000000, 0.7953136715913630139, 1.000000000000000000),
 ( 1.000000000000000000, 0.7071067811864313324, 1.000000000000000000) ) ) 
 REPRESENTATION_ITEM ( '' )  SURFACE ( )  );
#233782 = AXIS2_PLACEMENT_3D ( 'NONE', #15051, #134947, #234072 ) ;
#233784 = EDGE_CURVE ( 'NONE', #89234, #132961, #241783, .T. ) ;
#233786 = ORIENTED_EDGE ( 'NONE', *, *, #49592, .T. ) ;
#233785 = CARTESIAN_POINT ( 'NONE',  ( 22.47071067811864609, 68.27992525551410097, -136.6221999392269595 ) ) ;
#233787 = DIRECTION ( 'NONE',  ( 1.000000000000000000, 0.000000000000000000, 0.000000000000000000 ) ) ;
#233788 = DIRECTION ( 'NONE',  ( 0.000000000000000000, -1.000000000000000000, 0.000000000000000000 ) ) ;
#233789 = DIRECTION ( 'NONE',  ( 1.000000000000000000, 0.000000000000000000, 0.000000000000000000 ) ) ;
#233790 = CARTESIAN_POINT ( 'NONE',  ( -20.54999999999999716, 7.150000000011155876, -88.15000000000004832 ) ) ;
#233792 = CARTESIAN_POINT ( 'NONE',  ( -18.50000000000000000, 10.29288807859935950, -139.4580020160122160 ) ) ;
#233791 = AXIS2_PLACEMENT_3D ( 'NONE', #202725, #24119, #173933 ) ;
#233793 = VERTEX_POINT ( 'NONE', #58288 ) ;
#233794 = CYLINDRICAL_SURFACE ( 'NONE', #247022, 0.09999999999998898659 ) ;
#233795 = EDGE_LOOP ( 'NONE', ( #8835, #8469, #190997, #11841 ) ) ;
#233796 = DIRECTION ( 'NONE',  ( 0.000000000000000000, 0.1350103645451904977, -0.9908441862701596881 ) ) ;
#233797 = VERTEX_POINT ( 'NONE', #60866 ) ;
#233798 = EDGE_CURVE ( 'NONE', #125226, #32455, #129359, .T. ) ;
#233800 = CARTESIAN_POINT ( 'NONE',  ( -20.93302460841142931, 46.41023286455059349, -243.0722154975327385 ) ) ;
#233799 = TOROIDAL_SURFACE ( 'NONE', #42245, 11.70000000000000107, 0.1000000000000000056 ) ;
#233801 = AXIS2_PLACEMENT_3D ( 'NONE', #188977, #88567, #129009 ) ;
#233802 = CIRCLE ( 'NONE', #121395, 0.1000000000000124678 ) ;
#233803 = ORIENTED_EDGE ( 'NONE', *, *, #216870, .T. ) ;
#233804 = AXIS2_PLACEMENT_3D ( 'NONE', #96182, #37524, #135308 ) ;
#233805 = DIRECTION ( 'NONE',  ( -1.000000000000000000, 2.849773892568378313E-16, -7.728835255496647986E-17 ) ) ;
#233806 = DIRECTION ( 'NONE',  ( 0.000000000000000000, 0.000000000000000000, 1.000000000000000000 ) ) ;
#233807 = FACE_OUTER_BOUND ( 'NONE', #167938, .T. ) ;
#233808 = EDGE_LOOP ( 'NONE', ( #145744, #156359, #134337, #218087, #79446, #168652, #26401, #174831, #164264, #85918 ) ) ;
#233809 = CYLINDRICAL_SURFACE ( 'NONE', #196104, 0.1000000000000028644 ) ;
#233810 = CARTESIAN_POINT ( 'NONE',  ( -21.14999999999999858, 11.75000000001115552, -107.2838656629781866 ) ) ;
#233811 = FACE_OUTER_BOUND ( 'NONE', #184671, .T. ) ;
#233812 = DIRECTION ( 'NONE',  ( -1.000000000000000000, -3.265361837132813093E-16, 0.000000000000000000 ) ) ;
#233813 = CARTESIAN_POINT ( 'NONE',  ( -23.24999999999999645, 85.60000000001210196, -129.8229180933022633 ) ) ;
#233814 = EDGE_LOOP ( 'NONE', ( #182589, #219095, #48873, #208229 ) ) ;
#233815 = ORIENTED_EDGE ( 'NONE', *, *, #213643, .T. ) ;
#233817 = ORIENTED_EDGE ( 'NONE', *, *, #27098, .T. ) ;
#233816 = DIRECTION ( 'NONE',  ( 0.000000000000000000, 0.000000000000000000, -1.000000000000000000 ) ) ;
#233818 = EDGE_LOOP ( 'NONE', ( #26833, #114932, #98815, #201890 ) ) ;
#233819 = DIRECTION ( 'NONE',  ( 0.000000000000000000, 0.9999176327611370985, -0.01283462868041286391 ) ) ;
#233820 = CARTESIAN_POINT ( 'NONE',  ( -16.87331047859651179, 66.05000000001261640, -190.8731074845244393 ) ) ;
#233821 = DIRECTION ( 'NONE',  ( 1.000000000000000000, -0.000000000000000000, -0.000000000000000000 ) ) ;
#233822 = CARTESIAN_POINT ( 'NONE',  ( -23.25000000000000000, -1.736705739456431807, -145.5174225876237699 ) ) ;
#233823 = ORIENTED_EDGE ( 'NONE', *, *, #16658, .F. ) ;
#233824 = FACE_OUTER_BOUND ( 'NONE', #170104, .T. ) ;
#233825 = CARTESIAN_POINT ( 'NONE',  ( 21.14999999999999858, 1.115600667400684642E-11, -67.10000000000005116 ) ) ;
#233827 = EDGE_LOOP ( 'NONE', ( #142523, #33169, #214029, #192149 ) ) ;
#233826 = CIRCLE ( 'NONE', #29834, 0.09999999999998898659 ) ;
#233829 = ORIENTED_EDGE ( 'NONE', *, *, #77312, .F. ) ;
#233828 = FACE_OUTER_BOUND ( 'NONE', #125425, .T. ) ;
#233830 = ADVANCED_FACE ( 'NONE', ( #160003 ), #116884, .T. ) ;
#233831 = DIRECTION ( 'NONE',  ( 0.000000000000000000, -0.7071067811865472397, -0.7071067811865479058 ) ) ;
#233832 = LINE ( 'NONE', #254639, #131541 ) ;
#233833 = DIRECTION ( 'NONE',  ( 0.000000000000000000, 0.6728971962616697722, 0.7397360091702875895 ) ) ;
#233834 = VERTEX_POINT ( 'NONE', #120883 ) ;
#233835 = ORIENTED_EDGE ( 'NONE', *, *, #201806, .T. ) ;
#233836 = CARTESIAN_POINT ( 'NONE',  ( -20.93302460841142931, 18.38637412622486877, -236.9471295141160283 ) ) ;
#233837 = VERTEX_POINT ( 'NONE', #56993 ) ;
#233838 = CYLINDRICAL_SURFACE ( 'NONE', #183509, 2.000000000000001776 ) ;
#233839 = EDGE_CURVE ( 'NONE', #155667, #180612, #214810, .T. ) ;
#233840 = CARTESIAN_POINT ( 'NONE',  ( 15.69410316191959254, 66.64325398293328817, -52.31974776316020126 ) ) ;
#233841 = EDGE_CURVE ( 'NONE', #37324, #206150, #179275, .T. ) ;
#233842 = DIRECTION ( 'NONE',  ( 0.000000000000000000, -1.000000000000000000, -6.982962677686266711E-15 ) ) ;
#233843 = AXIS2_PLACEMENT_3D ( 'NONE', #104445, #103170, #129184 ) ;
#233844 = EDGE_CURVE ( 'NONE', #253865, #114232, #212582, .T. ) ;
#233845 = CIRCLE ( 'NONE', #200522, 0.09999999999999749367 ) ;
#233847 = ORIENTED_EDGE ( 'NONE', *, *, #109882, .T. ) ;
#233846 = CIRCLE ( 'NONE', #96450, 0.09999999999999609201 ) ;
#233848 = CARTESIAN_POINT ( 'NONE',  ( -21.14999999999999858, 69.45934304831143891, -203.4231074845244223 ) ) ;
#233849 = ADVANCED_FACE ( 'NONE', ( #118293 ), #97399, .T. ) ;
#233850 = ORIENTED_EDGE ( 'NONE', *, *, #76724, .T. ) ;
#233851 = EDGE_CURVE ( 'NONE', #32631, #129506, #158604, .T. ) ;
#233852 = CARTESIAN_POINT ( 'NONE',  ( -21.52071067811865746, 29.44578301613924154, -236.8621740332600041 ) ) ;
#233853 = FACE_OUTER_BOUND ( 'NONE', #133240, .T. ) ;
#233855 = ORIENTED_EDGE ( 'NONE', *, *, #191303, .T. ) ;
#233854 = FACE_OUTER_BOUND ( 'NONE', #195259, .T. ) ;
#233856 = CARTESIAN_POINT ( 'NONE',  ( -20.94999999999999929, 43.57281345108133053, -239.9888335660389487 ) ) ;
#233857 = LINE ( 'NONE', #117751, #124053 ) ;
#233858 = EDGE_CURVE ( 'NONE', #244837, #196423, #73593, .T. ) ;
#233859 = CYLINDRICAL_SURFACE ( 'NONE', #14540, 0.1000000000000028644 ) ;
#233860 = CARTESIAN_POINT ( 'NONE',  ( -16.81744102076748959, 9.949999999999983302, -20.85000000000000142 ) ) ;
#233861 = FACE_OUTER_BOUND ( 'NONE', #78245, .T. ) ;
#233862 = CARTESIAN_POINT ( 'NONE',  ( 23.14999999999999858, 5.000000000011153745, -121.5947339810869465 ) ) ;
#233863 = DIRECTION ( 'NONE',  ( 0.000000000000000000, 0.000000000000000000, 1.000000000000000000 ) ) ;
#233865 = ORIENTED_EDGE ( 'NONE', *, *, #186537, .F. ) ;
#233864 = LINE ( 'NONE', #36978, #173841 ) ;
#233866 = EDGE_CURVE ( 'NONE', #22210, #201200, #20487, .T. ) ;
#233867 = CIRCLE ( 'NONE', #163146, 0.09999999999999939493 ) ;
#233868 = CARTESIAN_POINT ( 'NONE',  ( -23.15000000000000213, 1.925233644870967487, -121.2697564668739005 ) ) ;
#233869 = CARTESIAN_POINT ( 'NONE',  ( -18.59999999999999787, 67.23127455305835554, -235.8551265064784559 ) ) ;
#233870 = ORIENTED_EDGE ( 'NONE', *, *, #7318, .F. ) ;
#233871 = CYLINDRICAL_SURFACE ( 'NONE', #91443, 0.1000000000000028644 ) ;
#233872 = EDGE_CURVE ( 'NONE', #116513, #242376, #79136, .T. ) ;
#233873 = CIRCLE ( 'NONE', #238137, 0.09999999999999990841 ) ;
#233874 = VECTOR ( 'NONE', #232826, 1000.000000000000000 ) ;
#233875 = CARTESIAN_POINT ( 'NONE',  ( -13.39999999999994351, 67.75000000001118394, -18.42310748452479174 ) ) ;
#233876 = CARTESIAN_POINT ( 'NONE',  ( -20.85000000000000142, -0.3238857010591806307, -133.9575895893140398 ) ) ;
#233877 = CIRCLE ( 'NONE', #9025, 0.09999999999999939493 ) ;
#233878 = EDGE_LOOP ( 'NONE', ( #250714, #49669, #79104, #146452 ) ) ;
#233879 = DIRECTION ( 'NONE',  ( -0.000000000000000000, -0.000000000000000000, -1.000000000000000000 ) ) ;
#233880 = DIRECTION ( 'NONE',  ( 1.000000000000000000, 0.000000000000000000, 0.000000000000000000 ) ) ;
#233881 = EDGE_CURVE ( 'NONE', #8823, #164555, #46152, .T. ) ;
#233882 = VERTEX_POINT ( 'NONE', #76583 ) ;
#233883 = DIRECTION ( 'NONE',  ( 0.000000000000000000, 6.938893903907222067E-15, -1.000000000000000000 ) ) ;
#233884 = EDGE_LOOP ( 'NONE', ( #242272, #156728, #18230, #92689, #120770, #40871, #125332, #250940, #146638 ) ) ;
#233885 = CYLINDRICAL_SURFACE ( 'NONE', #250245, 11.80000000000000426 ) ;
#233887 = ORIENTED_EDGE ( 'NONE', *, *, #14115, .F. ) ;
#233886 = CARTESIAN_POINT ( 'NONE',  ( 21.13422380239053311, 6.493326514816903483, -134.0000000000000284 ) ) ;
#233888 = CIRCLE ( 'NONE', #250462, 0.09999999999999939493 ) ;
#233889 = DIRECTION ( 'NONE',  ( 1.000000000000000000, 0.000000000000000000, 0.000000000000000000 ) ) ;
#233890 = ORIENTED_EDGE ( 'NONE', *, *, #43795, .F. ) ;
#233891 = DIRECTION ( 'NONE',  ( 0.000000000000000000, 1.000000000000000000, 6.352154140967427193E-15 ) ) ;
#233892 = ORIENTED_EDGE ( 'NONE', *, *, #78744, .F. ) ;
#233894 = ORIENTED_EDGE ( 'NONE', *, *, #174578, .T. ) ;
#233893 = EDGE_LOOP ( 'NONE', ( #205815, #202293, #80996, #68526 ) ) ;
#233895 = CARTESIAN_POINT ( 'NONE',  ( 21.05000000000000071, -11.64999999999999147, 0.000000000000000000 ) ) ;
#233897 = ORIENTED_EDGE ( 'NONE', *, *, #53760, .T. ) ;
#233896 = CARTESIAN_POINT ( 'NONE',  ( 21.05563370358598263, 10.72423035585766549, -146.1830908159630837 ) ) ;
#233898 = EDGE_CURVE ( 'NONE', #223761, #1074, #236947, .T. ) ;
#233899 = CARTESIAN_POINT ( 'NONE',  ( -16.94333152882355620, 14.20736394004534553, -219.2875565584338631 ) ) ;
#233900 = ORIENTED_EDGE ( 'NONE', *, *, #154283, .F. ) ;
#233901 = EDGE_CURVE ( 'NONE', #96622, #34317, #133457, .T. ) ;
#233902 = ORIENTED_EDGE ( 'NONE', *, *, #58034, .T. ) ;
#233903 = DIRECTION ( 'NONE',  ( 0.000000000000000000, -6.982962677686266711E-15, 1.000000000000000000 ) ) ;
#233905 = CARTESIAN_POINT ( 'NONE',  ( 20.94999999999999929, 47.95459712139159336, -246.5019368548292675 ) ) ;
#233904 = VECTOR ( 'NONE', #211477, 1000.000000000000114 ) ;
#233906 = EDGE_CURVE ( 'NONE', #86293, #243012, #200099, .T. ) ;
#233907 = PLANE ( 'NONE',  #211429 ) ;
#233908 = VERTEX_POINT ( 'NONE', #199105 ) ;
#233909 = DIRECTION ( 'NONE',  ( 0.000000000000000000, 1.000000000000000000, 0.000000000000000000 ) ) ;
#233910 = CARTESIAN_POINT ( 'NONE',  ( -18.49346865148325492, -9.443073798513720973, -74.18519625531534700 ) ) ;
#233911 = DIRECTION ( 'NONE',  ( 0.000000000000000000, -6.608470384673536035E-15, 1.000000000000000000 ) ) ;
#233912 = CIRCLE ( 'NONE', #92258, 4.049999999999998046 ) ;
#233914 = ORIENTED_EDGE ( 'NONE', *, *, #212609, .F. ) ;
#233913 = EDGE_CURVE ( 'NONE', #111692, #127795, #99970, .T. ) ;
#233916 = ADVANCED_FACE ( 'NONE', ( #37479 ), #217363, .F. ) ;
#233915 = CARTESIAN_POINT ( 'NONE',  ( -18.40000000000000213, 5.649999999999983480, -24.25000000000001066 ) ) ;
#233917 = SURFACE_STYLE_FILL_AREA ( #151841 ) ;
#233918 = CIRCLE ( 'NONE', #179767, 0.09999999999998898659 ) ;
#233919 = ORIENTED_EDGE ( 'NONE', *, *, #93731, .T. ) ;
#233920 = CARTESIAN_POINT ( 'NONE',  ( 18.59999999999999076, 69.35000000001200249, -115.1731074845243512 ) ) ;
#233921 = ORIENTED_EDGE ( 'NONE', *, *, #69256, .F. ) ;
#233922 = EDGE_LOOP ( 'NONE', ( #52553, #246751, #245408, #106893, #220833 ) ) ;
#233923 = CIRCLE ( 'NONE', #196500, 14.30833333333333357 ) ;
#233924 = DIRECTION ( 'NONE',  ( 1.000000000000000000, -0.000000000000000000, 0.000000000000000000 ) ) ;
#233925 = EDGE_CURVE ( 'NONE', #253865, #196016, #37989, .T. ) ;
#233926 = ORIENTED_EDGE ( 'NONE', *, *, #131151, .F. ) ;
#233927 = TOROIDAL_SURFACE ( 'NONE', #229280, 11.65000000000000036, 0.1000000000000000056 ) ;
#233928 = EDGE_LOOP ( 'NONE', ( #33165, #53441, #136434, #193933, #76492, #151908, #57939, #1540, #76046, #206492, #172157, #166938, #140583, #145806 ) ) ;
#233929 = CARTESIAN_POINT ( 'NONE',  ( -23.15000000000000213, 64.25000000001229239, -157.8731074845244393 ) ) ;
#233930 = DIRECTION ( 'NONE',  ( 1.000000000000000000, 0.000000000000000000, 0.000000000000000000 ) ) ;
#233931 = ORIENTED_EDGE ( 'NONE', *, *, #222843, .T. ) ;
#233932 = ORIENTED_EDGE ( 'NONE', *, *, #8493, .F. ) ;
#233933 = AXIS2_PLACEMENT_3D ( 'NONE', #114390, #72727, #167980 ) ;
#233934 = CARTESIAN_POINT ( 'NONE',  ( -20.64999999999999858, 29.19585636832770703, -237.3287400596392445 ) ) ;
#233936 = VERTEX_POINT ( 'NONE', #243358 ) ;
#233935 = AXIS2_PLACEMENT_3D ( 'NONE', #23994, #237880, #241732 ) ;
#233937 = CIRCLE ( 'NONE', #109023, 0.1000000000000028644 ) ;
#233938 = VECTOR ( 'NONE', #161406, 1000.000000000000000 ) ;
#233939 = EDGE_LOOP ( 'NONE', ( #104516, #205827, #56544, #211661 ) ) ;
#233940 = DIRECTION ( 'NONE',  ( 0.000000000000000000, 0.000000000000000000, -1.000000000000000000 ) ) ;
#233941 = VECTOR ( 'NONE', #177011, 1000.000000000000000 ) ;
#233942 = DIRECTION ( 'NONE',  ( 0.000000000000000000, 0.000000000000000000, -1.000000000000000000 ) ) ;
#233943 = EDGE_CURVE ( 'NONE', #109819, #217763, #103830, .T. ) ;
#233944 = EDGE_CURVE ( 'NONE', #123814, #160843, #7319, .T. ) ;
#233945 = CIRCLE ( 'NONE', #242130, 0.8750000000000007772 ) ;
#233946 = CARTESIAN_POINT ( 'NONE',  ( 20.94999999999999929, 1.835341550224413698, -11.55515129256298401 ) ) ;
#233947 = DIRECTION ( 'NONE',  ( 0.000000000000000000, 0.2128009952263603954, -0.9770955615653315052 ) ) ;
#233948 = DIRECTION ( 'NONE',  ( 0.000000000000000000, 1.000000000000000000, -0.000000000000000000 ) ) ;
#233949 = DIRECTION ( 'NONE',  ( 0.000000000000000000, 0.2617529984165152257, 0.9651348961777124202 ) ) ;
#233950 = DIRECTION ( 'NONE',  ( -1.000000000000000000, -0.000000000000000000, -0.000000000000000000 ) ) ;
#233952 = DIRECTION ( 'NONE',  ( 0.000000000000000000, 0.01562499999998609446, -0.9998779222360101304 ) ) ;
#233951 = FACE_OUTER_BOUND ( 'NONE', #167953, .T. ) ;
#233953 = CARTESIAN_POINT ( 'NONE',  ( -21.05000000000000071, 1.115600667400684642E-11, -33.50000000000000000 ) ) ;
#233954 = CARTESIAN_POINT ( 'NONE',  ( -16.88783316861810135, 23.06821272742414664, -230.9833517633470876 ) ) ;
#233955 = EDGE_CURVE ( 'NONE', #104735, #175552, #222491, .T. ) ;
#233956 = DIRECTION ( 'NONE',  ( -0.000000000000000000, -0.9126074666063770380, -0.4088369013363281068 ) ) ;
#233957 = CARTESIAN_POINT ( 'NONE',  ( -21.11833042828134666, 75.99289949095320651, -176.4687521783799298 ) ) ;
#233958 = AXIS2_PLACEMENT_3D ( 'NONE', #164176, #83309, #202014 ) ;
#233959 = ORIENTED_EDGE ( 'NONE', *, *, #158878, .T. ) ;
#233960 = AXIS2_PLACEMENT_3D ( 'NONE', #41929, #165726, #127868 ) ;
#233962 = ORIENTED_EDGE ( 'NONE', *, *, #77672, .F. ) ;
#233961 = FACE_OUTER_BOUND ( 'NONE', #199959, .T. ) ;
#233963 = FACE_OUTER_BOUND ( 'NONE', #70107, .T. ) ;
#233964 = CYLINDRICAL_SURFACE ( 'NONE', #248477, 0.09999999999999939493 ) ;
#233965 = ORIENTED_EDGE ( 'NONE', *, *, #200583, .F. ) ;
#233966 =( NAMED_UNIT ( * ) SI_UNIT ( $, .STERADIAN. ) SOLID_ANGLE_UNIT ( ) );
#233967 = CARTESIAN_POINT ( 'NONE',  ( 21.05000000000000071, 70.60000000001198828, -112.9170766071767815 ) ) ;
#233968 = ADVANCED_FACE ( 'NONE', ( #187264 ), #123422, .T. ) ;
#233969 = FACE_OUTER_BOUND ( 'NONE', #211862, .T. ) ;
#233970 = ORIENTED_EDGE ( 'NONE', *, *, #199523, .F. ) ;
#233971 = DIRECTION ( 'NONE',  ( 0.000000000000000000, 0.2128009952263485993, -0.9770955615653341697 ) ) ;
#233972 = CARTESIAN_POINT ( 'NONE',  ( -19.99999999999999645, 11.61130914238355771, 16.50000000000000000 ) ) ;
#233973 = EDGE_CURVE ( 'NONE', #31369, #17415, #154518, .T. ) ;
#233974 = DIRECTION ( 'NONE',  ( 0.000000000000000000, 0.8814952561688476074, -0.4721928772777262417 ) ) ;
#233976 = ORIENTED_EDGE ( 'NONE', *, *, #121766, .F. ) ;
#233975 = LINE ( 'NONE', #213132, #89252 ) ;
#233977 = DIRECTION ( 'NONE',  ( 0.000000000000000000, 0.9908441862701596881, 0.1350103645451904977 ) ) ;
#233979 = ORIENTED_EDGE ( 'NONE', *, *, #122832, .T. ) ;
#233978 = CARTESIAN_POINT ( 'NONE',  ( 20.84999999999999432, 79.19526988099229925, -196.1889237952725296 ) ) ;
#233981 = ADVANCED_FACE ( 'NONE', ( #204230 ), #24340, .F. ) ;
#233980 = DIRECTION ( 'NONE',  ( -2.557131231893036985E-16, 0.8660254037844384856, -0.5000000000000002220 ) ) ;
#233982 = CARTESIAN_POINT ( 'NONE',  ( -20.94999999999999929, -1.164121893230052995, -208.7148480855715604 ) ) ;
#233983 = LINE ( 'NONE', #89328, #232357 ) ;
#233984 = CARTESIAN_POINT ( 'NONE',  ( -23.15000000000000213, 2.000000000011154189, -54.37537807723790451 ) ) ;
#233986 = CARTESIAN_POINT ( 'NONE',  ( 21.14999999999999858, 65.28660755661196902, -90.67310748452437963 ) ) ;
#233985 = CARTESIAN_POINT ( 'NONE',  ( -16.79270642812296543, 9.946244216949359895, -154.8389332785629904 ) ) ;
#233988 = EDGE_CURVE ( 'NONE', #106299, #214079, #100296, .T. ) ;
#233987 = LINE ( 'NONE', #51476, #124584 ) ;
#233989 = DIRECTION ( 'NONE',  ( 0.000000000000000000, -1.000000000000000000, 0.000000000000000000 ) ) ;
#233990 = CARTESIAN_POINT ( 'NONE',  ( 21.40925344232283223, 0.09895018863080314031, -160.8414811406095453 ) ) ;
#233992 = DIRECTION ( 'NONE',  ( -1.000000000000000000, 0.000000000000000000, 0.000000000000000000 ) ) ;
#233991 = B_SPLINE_CURVE_WITH_KNOTS ( 'NONE', 3,
 ( #190957, #249632, #71009, #166264, #130956, #245772, #51378, #47541, #128392, #107530 ),
 .UNSPECIFIED., .F., .F.,
 ( 4, 2, 2, 2, 4 ),
 ( 0.000000000000000000, 4.221631689688079022E-05, 8.443263379376158043E-05, 0.0001688652675875276603, 0.0003377305351750620969 ),
 .UNSPECIFIED. ) ;
#233993 = DIRECTION ( 'NONE',  ( 0.000000000000000000, -0.4721928772777346239, -0.8814952561688430555 ) ) ;
#233994 = ORIENTED_EDGE ( 'NONE', *, *, #202512, .T. ) ;
#233995 = EDGE_CURVE ( 'NONE', #11322, #26533, #17140, .T. ) ;
#233997 = TOROIDAL_SURFACE ( 'NONE', #242375, 0.2000000000000000111, 0.1000000000000000056 ) ;
#233996 = DIRECTION ( 'NONE',  ( 0.000000000000000000, 0.000000000000000000, -1.000000000000000000 ) ) ;
#233999 = EDGE_CURVE ( 'NONE', #46326, #24103, #247207, .T. ) ;
#233998 = EDGE_CURVE ( 'NONE', #122095, #185020, #43885, .T. ) ;
#234000 = EDGE_LOOP ( 'NONE', ( #19161, #84647, #246552, #246844 ) ) ;
#234001 = ORIENTED_EDGE ( 'NONE', *, *, #144833, .T. ) ;
#234002 = PLANE ( 'NONE',  #223468 ) ;
#234003 = DIRECTION ( 'NONE',  ( 0.000000000000000000, -0.9525900758537790836, 0.3042567129660269099 ) ) ;
#234004 = ORIENTED_EDGE ( 'NONE', *, *, #78483, .T. ) ;
#234005 =( REPRESENTATION_RELATIONSHIP ('NONE','NONE', #36900, #100031 ) REPRESENTATION_RELATIONSHIP_WITH_TRANSFORMATION ( #257762 )SHAPE_REPRESENTATION_RELATIONSHIP( ) );
#234006 = ORIENTED_EDGE ( 'NONE', *, *, #134739, .T. ) ;
#234007 = CARTESIAN_POINT ( 'NONE',  ( -17.73285935862607587, 10.85798180379782352, -144.2414381902258356 ) ) ;
#234008 = SURFACE_SIDE_STYLE ('',( #76209 ) ) ;
#234009 = EDGE_LOOP ( 'NONE', ( #186486, #181295, #168783, #51256 ) ) ;
#234010 = ADVANCED_FACE ( 'NONE', ( #165117 ), #12812, .T. ) ;
#234011 = ADVANCED_FACE ( 'NONE', ( #127273 ), #45162, .F. ) ;
#234012 = ORIENTED_EDGE ( 'NONE', *, *, #51746, .T. ) ;
#234013 = AXIS2_PLACEMENT_3D ( 'NONE', #87555, #225777, #103261 ) ;
#234014 = DIRECTION ( 'NONE',  ( 0.000000000000000000, -1.000000000000000000, 0.000000000000000000 ) ) ;
#234015 = DIRECTION ( 'NONE',  ( 1.000000000000000000, -0.000000000000000000, -0.000000000000000000 ) ) ;
#234016 = CARTESIAN_POINT ( 'NONE',  ( 21.00000000000000000, 61.05385884576949707, -221.3836188041226762 ) ) ;
#234017 = DIRECTION ( 'NONE',  ( 1.000000000000000000, 0.000000000000000000, -0.000000000000000000 ) ) ;
#234018 = CARTESIAN_POINT ( 'NONE',  ( 15.06592377766032698, 9.417789466952205757, -15.35738454397687036 ) ) ;
#234019 = EDGE_CURVE ( 'NONE', #156548, #241136, #75409, .T. ) ;
#234021 = DIRECTION ( 'NONE',  ( -1.646408749285563007E-14, 0.4721928772777346239, 0.8814952561688430555 ) ) ;
#234020 = DIRECTION ( 'NONE',  ( -1.000000000000000000, -0.000000000000000000, -0.000000000000000000 ) ) ;
#234022 = CARTESIAN_POINT ( 'NONE',  ( 23.14999999999999858, 76.00000000001142553, -36.02310748452432421 ) ) ;
#234024 = ORIENTED_EDGE ( 'NONE', *, *, #205126, .T. ) ;
#234023 = DIRECTION ( 'NONE',  ( 0.000000000000000000, 0.000000000000000000, 1.000000000000000000 ) ) ;
#234026 = CARTESIAN_POINT ( 'NONE',  ( -20.85000000000000142, 64.25000000001170974, -69.52310748452438816 ) ) ;
#234025 = DIRECTION ( 'NONE',  ( 0.000000000000000000, 0.000000000000000000, -1.000000000000000000 ) ) ;
#234027 = DIRECTION ( 'NONE',  ( 0.000000000000000000, -0.9999631594459056361, -0.008583690987124413183 ) ) ;
#234028 = ORIENTED_EDGE ( 'NONE', *, *, #68912, .F. ) ;
#234029 = CARTESIAN_POINT ( 'NONE',  ( 21.14999999999999858, 8.786607556611267356, -146.2500000000000284 ) ) ;
#234030 = DIRECTION ( 'NONE',  ( 1.000000000000000000, -0.000000000000000000, -0.000000000000000000 ) ) ;
#234031 = EDGE_LOOP ( 'NONE', ( #68151, #69445, #11905, #109197 ) ) ;
#234032 = EDGE_CURVE ( 'NONE', #88879, #62193, #4622, .T. ) ;
#234033 = AXIS2_PLACEMENT_3D ( 'NONE', #75217, #34813, #114315 ) ;
#234034 = CARTESIAN_POINT ( 'NONE',  ( 20.02499999999999858, 63.35728523183471594, -212.8904317177587870 ) ) ;
#234035 = EDGE_CURVE ( 'NONE', #130496, #216736, #33734, .T. ) ;
#234036 = CARTESIAN_POINT ( 'NONE',  ( -13.39999999999994351, 66.35000000001119247, -18.42310748452479174 ) ) ;
#234037 = DIRECTION ( 'NONE',  ( 1.734723475976817507E-14, -1.000000000000000000, 0.000000000000000000 ) ) ;
#234038 = ORIENTED_EDGE ( 'NONE', *, *, #190363, .F. ) ;
#234039 = ORIENTED_EDGE ( 'NONE', *, *, #160744, .F. ) ;
#234040 = DIRECTION ( 'NONE',  ( 0.000000000000000000, 6.982962677686266711E-15, -1.000000000000000000 ) ) ;
#234041 = CARTESIAN_POINT ( 'NONE',  ( 20.12500000000000000, 9.750000000011153745, -188.7499999999999716 ) ) ;
#234042 = CARTESIAN_POINT ( 'NONE',  ( 23.14999999999999858, 76.00000000001126921, -203.5231074845248997 ) ) ;
#234044 = ADVANCED_FACE ( 'NONE', ( #69887 ), #34610, .T. ) ;
#234043 = DIRECTION ( 'NONE',  ( 0.000000000000000000, 0.000000000000000000, -1.000000000000000000 ) ) ;
#234045 = EDGE_LOOP ( 'NONE', ( #56037, #23911, #234134, #30675 ) ) ;
#234046 = DIRECTION ( 'NONE',  ( -0.7071067811865474617, -0.7071067811865474617, -0.000000000000000000 ) ) ;
#234047 = AXIS2_PLACEMENT_3D ( 'NONE', #231949, #207249, #247640 ) ;
#234049 = CARTESIAN_POINT ( 'NONE',  ( 20.85000000000000142, 76.00000000001126921, -203.5231074845248997 ) ) ;
#234048 = VECTOR ( 'NONE', #175424, 1000.000000000000227 ) ;
#234050 = AXIS2_PLACEMENT_3D ( 'NONE', #235343, #115404, #78827 ) ;
#234052 = EDGE_CURVE ( 'NONE', #250639, #98621, #125457, .T. ) ;
#234051 = FACE_OUTER_BOUND ( 'NONE', #5641, .T. ) ;
#234053 = FACE_OUTER_BOUND ( 'NONE', #204665, .T. ) ;
#234054 = CARTESIAN_POINT ( 'NONE',  ( -18.45140287520617761, -9.486077739518407270, -207.6405231266861051 ) ) ;
#234056 = VERTEX_POINT ( 'NONE', #73740 ) ;
#234055 = DIRECTION ( 'NONE',  ( 0.000000000000000000, 1.000000000000000000, 0.000000000000000000 ) ) ;
#234057 = DIRECTION ( 'NONE',  ( 2.659396599871503635E-15, -0.6132151058540604716, 0.7899159663865477077 ) ) ;
#234058 = DIRECTION ( 'NONE',  ( 7.304098846218134667E-16, 1.000000000000000000, 6.982962677686267499E-15 ) ) ;
#234059 = CARTESIAN_POINT ( 'NONE',  ( -21.05000000000000071, 7.128833340094563376, -233.7327013124401276 ) ) ;
#234060 = CARTESIAN_POINT ( 'NONE',  ( 21.05000000000000071, -0.09999999998884512298, -94.02295361821016684 ) ) ;
#234061 = EDGE_CURVE ( 'NONE', #162902, #69280, #110263, .T. ) ;
#234062 = DIRECTION ( 'NONE',  ( 1.000000000000000000, 0.000000000000000000, 0.000000000000000000 ) ) ;
#234064 = ORIENTED_EDGE ( 'NONE', *, *, #140249, .F. ) ;
#234063 = DIRECTION ( 'NONE',  ( -0.000000000000000000, 0.8814952561688430555, -0.4721928772777346239 ) ) ;
#234065 = DIRECTION ( 'NONE',  ( 1.000000000000000000, 0.000000000000000000, 0.000000000000000000 ) ) ;
#234066 = LINE ( 'NONE', #138781, #71843 ) ;
#234067 = CARTESIAN_POINT ( 'NONE',  ( 23.14999999999999858, 1.115600667400684642E-11, -167.5000000000000284 ) ) ;
#234068 = CIRCLE ( 'NONE', #59241, 0.09999999999998898659 ) ;
#234069 = EDGE_LOOP ( 'NONE', ( #127958, #128250, #26729, #17058 ) ) ;
#234070 = CYLINDRICAL_SURFACE ( 'NONE', #84494, 0.09999999999999939493 ) ;
#234071 = DIRECTION ( 'NONE',  ( 0.000000000000000000, 0.8814952561688429444, -0.4721928772777345684 ) ) ;
#234072 = DIRECTION ( 'NONE',  ( 0.000000000000000000, -0.2617529984165152257, -0.9651348961777124202 ) ) ;
#234073 = DIRECTION ( 'NONE',  ( 0.000000000000000000, 0.000000000000000000, -1.000000000000000000 ) ) ;
#234074 = CARTESIAN_POINT ( 'NONE',  ( -21.64999999999999858, 23.02528674727019364, -230.8469138855057281 ) ) ;
#234075 = VECTOR ( 'NONE', #131966, 1000.000000000000000 ) ;
#234076 = DIRECTION ( 'NONE',  ( -4.408576920032448588E-17, 0.1350103645451876944, 0.9908441862701601321 ) ) ;
#234077 = VERTEX_POINT ( 'NONE', #193668 ) ;
#234078 = VERTEX_POINT ( 'NONE', #171565 ) ;
#234079 = DIRECTION ( 'NONE',  ( 1.000000000000000000, 0.000000000000000000, 0.000000000000000000 ) ) ;
#234080 = CARTESIAN_POINT ( 'NONE',  ( -16.91049119928363709, 66.05000000001201954, -115.6413870913335273 ) ) ;
#234081 = CIRCLE ( 'NONE', #121685, 0.09999999999999230338 ) ;
#234082 = CYLINDRICAL_SURFACE ( 'NONE', #220252, 4.000000000000006217 ) ;
#234083 = CARTESIAN_POINT ( 'NONE',  ( -20.85000000000000142, 1.115600667400684642E-11, -100.5000000000000426 ) ) ;
#234084 = DIRECTION ( 'NONE',  ( 0.7071067811865487940, -0.7071067811865462405, -4.216150419019403701E-15 ) ) ;
#234085 = CIRCLE ( 'NONE', #121693, 0.1000000000000022676 ) ;
#234086 = DIRECTION ( 'NONE',  ( 0.000000000000000000, -0.4930308989875170078, -0.8700118002898356018 ) ) ;
#234087 = AXIS2_PLACEMENT_3D ( 'NONE', #139566, #234842, #198273 ) ;
#234088 = FACE_OUTER_BOUND ( 'NONE', #83674, .T. ) ;
#234089 = TOROIDAL_SURFACE ( 'NONE', #155025, 0.2000000000000000111, 0.1000000000000000056 ) ;
#234091 = AXIS2_PLACEMENT_3D ( 'NONE', #212131, #113021, #153480 ) ;
#234090 = B_SPLINE_CURVE_WITH_KNOTS ( 'NONE', 3,
 ( #152033, #148151, #133720, #247239, #227681, #169042, #89452 ),
 .UNSPECIFIED., .F., .F.,
 ( 4, 3, 4 ),
 ( 0.000000000000000000, 1.860045280645836611E-05, 5.251155757304663829E-05 ),
 .UNSPECIFIED. ) ;
#234092 = CARTESIAN_POINT ( 'NONE',  ( 23.14999999999998437, 1.115650265596050101E-11, -29.45000000000000284 ) ) ;
#234093 = VERTEX_POINT ( 'NONE', #15042 ) ;
#234094 = CYLINDRICAL_SURFACE ( 'NONE', #206840, 14.30833333333334956 ) ;
#234095 = ORIENTED_EDGE ( 'NONE', *, *, #93828, .T. ) ;
#234096 = ORIENTED_EDGE ( 'NONE', *, *, #25918, .F. ) ;
#234097 = DIRECTION ( 'NONE',  ( 0.000000000000000000, 0.9126074666063545004, 0.4088369013363783999 ) ) ;
#234098 = DIRECTION ( 'NONE',  ( -1.000000000000000000, 0.000000000000000000, 0.000000000000000000 ) ) ;
#234099 = DIRECTION ( 'NONE',  ( 1.000000000000000000, 0.000000000000000000, 0.000000000000000000 ) ) ;
#234101 = EDGE_LOOP ( 'NONE', ( #227202, #240760, #41058, #24681 ) ) ;
#234100 = DIRECTION ( 'NONE',  ( 1.000000000000000000, 0.000000000000000000, 0.000000000000000000 ) ) ;
#234102 = CARTESIAN_POINT ( 'NONE',  ( -23.15000000000000213, 64.35000000001222986, -148.6731074845244507 ) ) ;
#234103 = CARTESIAN_POINT ( 'NONE',  ( 23.25000000000000000, 87.75000000001205080, -124.3731074845242119 ) ) ;
#234105 = CARTESIAN_POINT ( 'NONE',  ( 18.50000000000001421, 85.48068669529062902, -62.58199231576637800 ) ) ;
#234104 = AXIS2_PLACEMENT_3D ( 'NONE', #20441, #196478, #115676 ) ;
#234106 = EDGE_LOOP ( 'NONE', ( #1688, #219027, #147859, #167016 ) ) ;
#234107 = CARTESIAN_POINT ( 'NONE',  ( 20.85000000000000142, 76.00000000001165290, -61.62310748452430431 ) ) ;
#234108 = AXIS2_PLACEMENT_3D ( 'NONE', #130769, #154239, #235018 ) ;
#234109 = CARTESIAN_POINT ( 'NONE',  ( 18.49999999999999645, 1.115600667400684642E-11, -200.9999999999999432 ) ) ;
#234110 = ADVANCED_FACE ( 'NONE', ( #150687 ), #192113, .F. ) ;
#234111 = LINE ( 'NONE', #111609, #185547 ) ;
#234112 = DIRECTION ( 'NONE',  ( 0.000000000000000000, -1.000000000000000000, -6.982962677686265922E-15 ) ) ;
#234113 = AXIS2_PLACEMENT_3D ( 'NONE', #241865, #125766, #25411 ) ;
#234114 = AXIS2_PLACEMENT_3D ( 'NONE', #191685, #132974, #213777 ) ;
#234115 = VECTOR ( 'NONE', #236583, 999.9999999999998863 ) ;
#234116 = EDGE_LOOP ( 'NONE', ( #177533, #152687, #113963, #129806 ) ) ;
#234117 = CIRCLE ( 'NONE', #242504, 0.09999999999999080458 ) ;
#234118 = CARTESIAN_POINT ( 'NONE',  ( -16.80438519320023616, 9.949779096479501206, -79.65073828092131691 ) ) ;
#234119 = CARTESIAN_POINT ( 'NONE',  ( -16.83794237512073622, 66.07364077890439091, -90.21956532582547084 ) ) ;
#234120 = ORIENTED_EDGE ( 'NONE', *, *, #3216, .F. ) ;
#234121 = CARTESIAN_POINT ( 'NONE',  ( 21.08035267497491105, 6.331706839794169817, -133.9173113752239033 ) ) ;
#234122 = CIRCLE ( 'NONE', #121723, 0.3999999999999975797 ) ;
#234123 = CARTESIAN_POINT ( 'NONE',  ( 22.48660254037843842, 55.87785187304942980, -232.8277855198933253 ) ) ;
#234124 = CARTESIAN_POINT ( 'NONE',  ( 20.85000000000000142, 36.22724532936083364, -235.9903003947922286 ) ) ;
#234125 = EDGE_CURVE ( 'NONE', #8823, #102962, #209370, .T. ) ;
#234126 = ORIENTED_EDGE ( 'NONE', *, *, #56923, .T. ) ;
#234127 = CARTESIAN_POINT ( 'NONE',  ( 18.48413544395656416, -9.664304033616613054, -174.1831049930383131 ) ) ;
#234128 = DIRECTION ( 'NONE',  ( 1.000000000000000000, -7.304098846218134667E-16, -5.100424963727255829E-30 ) ) ;
#234129 = ORIENTED_EDGE ( 'NONE', *, *, #77794, .T. ) ;
#234130 = AXIS2_PLACEMENT_3D ( 'NONE', #157473, #75363, #55726 ) ;
#234131 = AXIS2_PLACEMENT_3D ( 'NONE', #120617, #21511, #124459 ) ;
#234132 = AXIS2_PLACEMENT_3D ( 'NONE', #173151, #214785, #231803 ) ;
#234133 = EDGE_CURVE ( 'NONE', #94397, #65824, #131113, .T. ) ;
#234134 = ORIENTED_EDGE ( 'NONE', *, *, #161923, .F. ) ;
#234135 = ADVANCED_FACE ( 'NONE', ( #153290 ), #232810, .T. ) ;
#234136 = LINE ( 'NONE', #157206, #197531 ) ;
#234137 = DIRECTION ( 'NONE',  ( 0.000000000000000000, -1.000000000000000000, 0.000000000000000000 ) ) ;
#234138 = ORIENTED_EDGE ( 'NONE', *, *, #123623, .F. ) ;
#234139 = CARTESIAN_POINT ( 'NONE',  ( 18.59999999999999076, 6.450000000011156587, -121.6500000000000341 ) ) ;
#234140 = CARTESIAN_POINT ( 'NONE',  ( 18.59999999999999787, -9.399999999999998579, -40.38204184817267617 ) ) ;
#234141 = EDGE_CURVE ( 'NONE', #28771, #160136, #117076, .T. ) ;
#234142 = FACE_OUTER_BOUND ( 'NONE', #175087, .T. ) ;
#234143 = DIRECTION ( 'NONE',  ( -1.000000000000000000, -1.646408749285562691E-14, 0.000000000000000000 ) ) ;
#234144 = FACE_OUTER_BOUND ( 'NONE', #24003, .T. ) ;
#234145 = CYLINDRICAL_SURFACE ( 'NONE', #51317, 0.09999999999999939493 ) ;
#234146 = LINE ( 'NONE', #215852, #149940 ) ;
#234148 = ORIENTED_EDGE ( 'NONE', *, *, #176352, .F. ) ;
#234147 = DIRECTION ( 'NONE',  ( 1.000000000000000000, -0.000000000000000000, -0.000000000000000000 ) ) ;
#234149 = EDGE_LOOP ( 'NONE', ( #37057, #172125 ) ) ;
#234151 = DIRECTION ( 'NONE',  ( -1.000000000000000000, 0.000000000000000000, 0.000000000000000000 ) ) ;
#234150 = CARTESIAN_POINT ( 'NONE',  ( -21.05000000000000071, -11.48912529306489994, -197.9999999999999432 ) ) ;
#234152 = EDGE_CURVE ( 'NONE', #249408, #157570, #192380, .T. ) ;
#234154 = ORIENTED_EDGE ( 'NONE', *, *, #44357, .F. ) ;
#234153 = LINE ( 'NONE', #171661, #222369 ) ;
#234155 = ORIENTED_EDGE ( 'NONE', *, *, #62349, .F. ) ;
#234156 = CARTESIAN_POINT ( 'NONE',  ( -21.05000000000000426, 6.332272273946816910, -167.5375360632856427 ) ) ;
#234157 = CIRCLE ( 'NONE', #159187, 0.1000000000000028644 ) ;
#234158 = CARTESIAN_POINT ( 'NONE',  ( -18.50000000000000711, 11.65000000001115232, -40.51480577065400013 ) ) ;
#234159 = EDGE_CURVE ( 'NONE', #97848, #73365, #50280, .T. ) ;
#234160 = CARTESIAN_POINT ( 'NONE',  ( -18.59999999999999787, 66.65000000001157332, -57.17310748452438673 ) ) ;
#234161 = FACE_OUTER_BOUND ( 'NONE', #82256, .T. ) ;
#234162 = CARTESIAN_POINT ( 'NONE',  ( -18.51697539158856998, 67.49317130920637453, -195.4795610751097286 ) ) ;
#234163 = CARTESIAN_POINT ( 'NONE',  ( -20.00857864376270001, 9.350000000011156942, -54.75000000000000000 ) ) ;
#234164 = EDGE_CURVE ( 'NONE', #16173, #125683, #207764, .T. ) ;
#234165 = CARTESIAN_POINT ( 'NONE',  ( -20.94999999999999929, 75.74389420791972327, -103.0580039261966050 ) ) ;
#234166 = ORIENTED_EDGE ( 'NONE', *, *, #73056, .F. ) ;
#234167 = ORIENTED_EDGE ( 'NONE', *, *, #240221, .F. ) ;
#234168 = ORIENTED_EDGE ( 'NONE', *, *, #50743, .F. ) ;
#234169 = CARTESIAN_POINT ( 'NONE',  ( -23.25000000000000000, -9.599999999988838795, -191.1060308773475072 ) ) ;
#234170 = CARTESIAN_POINT ( 'NONE',  ( 18.49999999999999289, 68.00366762990589109, -224.2307594727497815 ) ) ;
#234171 = CIRCLE ( 'NONE', #22002, 0.09999999999999939493 ) ;
#234172 = DIRECTION ( 'NONE',  ( 1.000000000000000000, 0.000000000000000000, 0.000000000000000000 ) ) ;
#234173 = ORIENTED_EDGE ( 'NONE', *, *, #247251, .T. ) ;
#234174 = CARTESIAN_POINT ( 'NONE',  ( -14.77538296656415184, 66.56333706821293106, -118.2000707522294505 ) ) ;
#234175 = VERTEX_POINT ( 'NONE', #13743 ) ;
#234176 = DIRECTION ( 'NONE',  ( 0.000000000000000000, 0.8814952561688429444, -0.4721928772777345684 ) ) ;
#234177 = ORIENTED_EDGE ( 'NONE', *, *, #4267, .F. ) ;
#234178 = DIRECTION ( 'NONE',  ( 0.000000000000000000, 0.9126074666063769270, 0.4088369013363280513 ) ) ;
#234179 = CARTESIAN_POINT ( 'NONE',  ( 21.05000000000000071, 6.450000000011156587, -110.5170271704400591 ) ) ;
#234180 = ORIENTED_EDGE ( 'NONE', *, *, #190359, .F. ) ;
#234182 = CARTESIAN_POINT ( 'NONE',  ( -23.25000000000000355, 66.05000000001233218, -160.7731074845244166 ) ) ;
#234181 = TOROIDAL_SURFACE ( 'NONE', #151013, 12.97499999999999787, 0.1000000000000000056 ) ;
#234183 = VERTEX_POINT ( 'NONE', #208113 ) ;
#234185 = ORIENTED_EDGE ( 'NONE', *, *, #190420, .T. ) ;
#234184 = CARTESIAN_POINT ( 'NONE',  ( 22.39999999999999858, 68.20922040163929978, -203.6231074845244109 ) ) ;
#234186 = FACE_OUTER_BOUND ( 'NONE', #24334, .T. ) ;
#234187 = ORIENTED_EDGE ( 'NONE', *, *, #173455, .T. ) ;
#234188 = AXIS2_PLACEMENT_3D ( 'NONE', #140827, #41746, #200800 ) ;
#234189 = EDGE_CURVE ( 'NONE', #60099, #117707, #151998, .T. ) ;
#234190 = ORIENTED_EDGE ( 'NONE', *, *, #131816, .F. ) ;
#234191 = AXIS2_PLACEMENT_3D ( 'NONE', #81951, #145801, #2436 ) ;
#234192 = CARTESIAN_POINT ( 'NONE',  ( -20.85000000000000142, 64.35000000001191722, -103.0231074845243882 ) ) ;
#234193 = ORIENTED_EDGE ( 'NONE', *, *, #67911, .F. ) ;
#234194 = FACE_OUTER_BOUND ( 'NONE', #205094, .T. ) ;
#234195 = ADVANCED_FACE ( 'NONE', ( #52855 ), #89415, .F. ) ;
#234196 = CARTESIAN_POINT ( 'NONE',  ( 22.49066049874202022, 64.12747008008147986, -247.0842118427744651 ) ) ;
#234197 = EDGE_CURVE ( 'NONE', #174969, #91096, #171298, .T. ) ;
#234198 = DIRECTION ( 'NONE',  ( 1.000000000000000000, 0.000000000000000000, 0.000000000000000000 ) ) ;
#234199 = CARTESIAN_POINT ( 'NONE',  ( 18.50000972452444969, 67.49459761544854075, -195.5598716110968951 ) ) ;
#234200 = FACE_OUTER_BOUND ( 'NONE', #38721, .T. ) ;
#234201 = AXIS2_PLACEMENT_3D ( 'NONE', #100820, #240388, #79990 ) ;
#234203 = ORIENTED_EDGE ( 'NONE', *, *, #93184, .T. ) ;
#234202 = EDGE_CURVE ( 'NONE', #159889, #126149, #112842, .T. ) ;
#234204 = VECTOR ( 'NONE', #49486, 1000.000000000000000 ) ;
#234205 = CARTESIAN_POINT ( 'NONE',  ( 21.05000000000000071, -9.499999999988844479, -90.60603087734760663 ) ) ;
#234206 = LINE ( 'NONE', #232961, #157745 ) ;
#234207 = CARTESIAN_POINT ( 'NONE',  ( -20.54999999999999716, 76.00000000001213607, -136.5231074845243313 ) ) ;
#234208 = EDGE_CURVE ( 'NONE', #63429, #128297, #29618, .T. ) ;
#234209 = ORIENTED_EDGE ( 'NONE', *, *, #176925, .T. ) ;
#234211 = EDGE_CURVE ( 'NONE', #102386, #229705, #217051, .T. ) ;
#234210 = ORIENTED_EDGE ( 'NONE', *, *, #106735, .T. ) ;
#234212 = CARTESIAN_POINT ( 'NONE',  ( -22.01447462590973103, 33.59883294982306978, -242.9626543818881430 ) ) ;
#234213 = ORIENTED_EDGE ( 'NONE', *, *, #82305, .T. ) ;
#234214 = CARTESIAN_POINT ( 'NONE',  ( -20.54999999999999716, 76.00000000001213607, -136.5231074845243313 ) ) ;
#234215 = FACE_OUTER_BOUND ( 'NONE', #94668, .T. ) ;
#234216 = ADVANCED_FACE ( 'NONE', ( #138778 ), #245830, .F. ) ;
#234217 = CIRCLE ( 'NONE', #109312, 0.09999999999999700795 ) ;
#234219 = VERTEX_POINT ( 'NONE', #158421 ) ;
#234218 = CARTESIAN_POINT ( 'NONE',  ( -20.15000000000000568, 66.70857864377522617, -182.3731074845244393 ) ) ;
#234220 = LINE ( 'NONE', #195136, #163101 ) ;
#234221 = ORIENTED_EDGE ( 'NONE', *, *, #84236, .T. ) ;
#234222 = CARTESIAN_POINT ( 'NONE',  ( -21.05000000000000071, -11.74999999998884448, -97.50000000000004263 ) ) ;
#234223 = VECTOR ( 'NONE', #78814, 1000.000000000000114 ) ;
#234224 = CIRCLE ( 'NONE', #67830, 0.3999999999999975797 ) ;
#234225 = AXIS2_PLACEMENT_3D ( 'NONE', #196906, #117381, #217739 ) ;
#234226 = CARTESIAN_POINT ( 'NONE',  ( 20.04142135623730070, 11.65000000000000391, 11.75000000000000000 ) ) ;
#234227 = ORIENTED_EDGE ( 'NONE', *, *, #72163, .F. ) ;
#234228 = AXIS2_PLACEMENT_3D ( 'NONE', #202348, #181523, #118975 ) ;
#234229 = CARTESIAN_POINT ( 'NONE',  ( -20.94999999999999929, 11.65000000001115055, -194.2161343370218560 ) ) ;
#234231 = EDGE_LOOP ( 'NONE', ( #179105, #151035, #112876, #249244 ) ) ;
#234230 = EDGE_CURVE ( 'NONE', #172615, #145230, #8742, .T. ) ;
#234232 = CARTESIAN_POINT ( 'NONE',  ( 21.07954763557388489, 10.05941015404899375, -228.1223551902535576 ) ) ;
#234233 = VERTEX_POINT ( 'NONE', #136221 ) ;
#234234 = EDGE_CURVE ( 'NONE', #183191, #57327, #92119, .T. ) ;
#234235 = DIRECTION ( 'NONE',  ( -0.000000000000000000, -0.1350103645451928291, -0.9908441862701594660 ) ) ;
#234236 = CARTESIAN_POINT ( 'NONE',  ( 11.60000000000000320, -11.65000000000000036, 17.60000000000000497 ) ) ;
#234237 = ADVANCED_FACE ( 'NONE', ( #35894 ), #21466, .T. ) ;
#234238 = EDGE_CURVE ( 'NONE', #4508, #91559, #354, .T. ) ;
#234240 = ORIENTED_EDGE ( 'NONE', *, *, #50449, .F. ) ;
#234239 = DIRECTION ( 'NONE',  ( -2.561896900575096011E-15, -0.5907332058517279494, 0.8068669527897025517 ) ) ;
#234241 = DIRECTION ( 'NONE',  ( -1.000000000000000000, 0.000000000000000000, 0.000000000000000000 ) ) ;
#234242 = DIRECTION ( 'NONE',  ( 0.000000000000000000, 0.5000000000000004441, 0.8660254037844384856 ) ) ;
#234243 = CARTESIAN_POINT ( 'NONE',  ( -18.50000000000000000, 11.75000000001115197, -122.2500000000000284 ) ) ;
#234245 = CARTESIAN_POINT ( 'NONE',  ( -22.50000000000000000, 75.90000000001245439, -181.6726782920691505 ) ) ;
#234244 = CARTESIAN_POINT ( 'NONE',  ( 20.04999999999999716, 67.25000000001197975, -115.6731074845243654 ) ) ;
#234246 = FACE_OUTER_BOUND ( 'NONE', #725, .T. ) ;
#234247 = CARTESIAN_POINT ( 'NONE',  ( 20.85000000000000142, 75.83895117929270668, -36.30729732888454464 ) ) ;
#234248 = AXIS2_PLACEMENT_3D ( 'NONE', #91762, #73511, #231286 ) ;
#234249 = CARTESIAN_POINT ( 'NONE',  ( 18.47654891039378455, -9.465274948371154906, -40.62597590519465740 ) ) ;
#234250 = AXIS2_PLACEMENT_3D ( 'NONE', #209940, #93818, #174700 ) ;
#234251 = FACE_OUTER_BOUND ( 'NONE', #512, .T. ) ;
#234252 = ORIENTED_EDGE ( 'NONE', *, *, #51115, .F. ) ;
#234253 = ORIENTED_EDGE ( 'NONE', *, *, #7653, .T. ) ;
#234254 = CARTESIAN_POINT ( 'NONE',  ( 20.94999999999999574, -1.349084418615859482, -74.98649896354552880 ) ) ;
#234256 = ORIENTED_EDGE ( 'NONE', *, *, #186548, .F. ) ;
#234255 = DIRECTION ( 'NONE',  ( 0.000000000000000000, 0.000000000000000000, 1.000000000000000000 ) ) ;
#234257 = ORIENTED_EDGE ( 'NONE', *, *, #126555, .F. ) ;
#234259 = CARTESIAN_POINT ( 'NONE',  ( -18.40000000000000213, 64.51332499825484490, -179.2731074845244450 ) ) ;
#234258 = CIRCLE ( 'NONE', #9408, 2.000000000000001776 ) ;
#234260 = ORIENTED_EDGE ( 'NONE', *, *, #102243, .T. ) ;
#234261 = CARTESIAN_POINT ( 'NONE',  ( 23.15000000000000213, 84.66355140188105111, -93.49900636645693908 ) ) ;
#234262 = AXIS2_PLACEMENT_3D ( 'NONE', #133666, #54120, #150670 ) ;
#234263 = ORIENTED_EDGE ( 'NONE', *, *, #51116, .T. ) ;
#234264 = AXIS2_PLACEMENT_3D ( 'NONE', #183544, #140544, #180977 ) ;
#234265 = DIRECTION ( 'NONE',  ( -0.000000000000000000, 0.000000000000000000, 1.000000000000000000 ) ) ;
#234266 = CIRCLE ( 'NONE', #113486, 0.1000000000000024342 ) ;
#234268 = ORIENTED_EDGE ( 'NONE', *, *, #84155, .T. ) ;
#234267 = ORIENTED_EDGE ( 'NONE', *, *, #145678, .F. ) ;
#234269 = ORIENTED_EDGE ( 'NONE', *, *, #156655, .T. ) ;
#234270 = CIRCLE ( 'NONE', #117764, 0.1000000000000096922 ) ;
#234271 = ORIENTED_EDGE ( 'NONE', *, *, #181626, .T. ) ;
#234273 = ORIENTED_EDGE ( 'NONE', *, *, #93083, .T. ) ;
#234272 = CIRCLE ( 'NONE', #188502, 0.09999999999999939493 ) ;
#234274 = LINE ( 'NONE', #231734, #22112 ) ;
#234275 = DIRECTION ( 'NONE',  ( 0.000000000000000000, 0.000000000000000000, -1.000000000000000000 ) ) ;
#234277 = ORIENTED_EDGE ( 'NONE', *, *, #127277, .T. ) ;
#234276 = DIRECTION ( 'NONE',  ( 0.000000000000000000, 0.9856811345164832039, 0.1686199900910280158 ) ) ;
#234278 = CARTESIAN_POINT ( 'NONE',  ( -23.25000000000000000, 4.150000000011156764, -88.25000000000005684 ) ) ;
#234279 = CARTESIAN_POINT ( 'NONE',  ( 12.25000000000000000, 12.70026017068886937, -215.3766613508543628 ) ) ;
#234281 = VERTEX_POINT ( 'NONE', #239206 ) ;
#234280 = CARTESIAN_POINT ( 'NONE',  ( 20.94999999999999929, -8.999999999988842703, -124.1060308773475924 ) ) ;
#234282 = DIRECTION ( 'NONE',  ( 0.000000000000000000, -6.982962677686266711E-15, 1.000000000000000000 ) ) ;
#234283 = ORIENTED_EDGE ( 'NONE', *, *, #126451, .T. ) ;
#234284 = DIRECTION ( 'NONE',  ( 1.000000000000000000, 0.000000000000000000, -0.000000000000000000 ) ) ;
#234285 = AXIS2_PLACEMENT_3D ( 'NONE', #21425, #40988, #65651 ) ;
#234287 = ORIENTED_EDGE ( 'NONE', *, *, #99677, .F. ) ;
#234286 = DIRECTION ( 'NONE',  ( -0.000000000000000000, 1.000000000000000000, -0.000000000000000000 ) ) ;
#234288 = AXIS2_PLACEMENT_3D ( 'NONE', #243692, #105424, #144575 ) ;
#234289 = LINE ( 'NONE', #251283, #89352 ) ;
#234291 = EDGE_CURVE ( 'NONE', #216916, #91733, #219632, .T. ) ;
#234290 = CARTESIAN_POINT ( 'NONE',  ( -16.94878442675512531, 9.991729103002157331, -113.1117804243621663 ) ) ;
#234292 = ORIENTED_EDGE ( 'NONE', *, *, #66520, .F. ) ;
#234293 = VECTOR ( 'NONE', #121129, 1000.000000000000000 ) ;
#234295 = DIRECTION ( 'NONE',  ( -1.000000000000000000, 0.000000000000000000, 0.000000000000000000 ) ) ;
#234294 = CARTESIAN_POINT ( 'NONE',  ( -16.95709691156173449, 9.950000000011208101, -121.3399424374903219 ) ) ;
#234296 = EDGE_CURVE ( 'NONE', #11112, #56184, #119401, .T. ) ;
#234297 = LINE ( 'NONE', #217288, #226637 ) ;
#234298 = CARTESIAN_POINT ( 'NONE',  ( -20.94999999999999929, -1.162701749938009677, -7.900000000000000355 ) ) ;
#234299 = DIRECTION ( 'NONE',  ( 0.7071067811865475727, 0.7071067811865475727, -0.000000000000000000 ) ) ;
#234301 = ORIENTED_EDGE ( 'NONE', *, *, #182672, .T. ) ;
#234300 = VECTOR ( 'NONE', #18386, 1000.000000000000000 ) ;
#234302 = VERTEX_POINT ( 'NONE', #75030 ) ;
#234303 = AXIS2_PLACEMENT_3D ( 'NONE', #104799, #103534, #61866 ) ;
#234304 = EDGE_CURVE ( 'NONE', #6309, #149328, #55395, .T. ) ;
#234305 = CARTESIAN_POINT ( 'NONE',  ( 15.74999999999999645, 47.91805600923871822, -233.7139610577891631 ) ) ;
#234307 = EDGE_CURVE ( 'NONE', #96705, #165365, #196174, .T. ) ;
#234306 = CARTESIAN_POINT ( 'NONE',  ( 20.94999999999999929, 65.70729864261004138, -97.56574559737244101 ) ) ;
#234308 = ORIENTED_EDGE ( 'NONE', *, *, #45496, .T. ) ;
#234309 = DIRECTION ( 'NONE',  ( 1.000000000000000000, -0.000000000000000000, -0.000000000000000000 ) ) ;
#234310 = ORIENTED_EDGE ( 'NONE', *, *, #128009, .T. ) ;
#234311 = FACE_OUTER_BOUND ( 'NONE', #41123, .T. ) ;
#234312 = TOROIDAL_SURFACE ( 'NONE', #92667, 0.4000000000000009104, 0.1000000000000000056 ) ;
#234313 = DIRECTION ( 'NONE',  ( 1.000000000000000000, 0.000000000000000000, 0.000000000000000000 ) ) ;
#234314 = EDGE_LOOP ( 'NONE', ( #178501, #202354, #2017, #168376 ) ) ;
#234315 = CYLINDRICAL_SURFACE ( 'NONE', #81797, 0.09999999999999939493 ) ;
#234316 = VECTOR ( 'NONE', #84257, 1000.000000000000000 ) ;
#234317 = VECTOR ( 'NONE', #165523, 1000.000000000000000 ) ;
#234318 = EDGE_LOOP ( 'NONE', ( #187236, #182338, #67229, #187381 ) ) ;
#234320 = EDGE_LOOP ( 'NONE', ( #28612, #29045, #165045, #75178 ) ) ;
#234319 = CIRCLE ( 'NONE', #71859, 0.09999999999998898659 ) ;
#234321 = EDGE_CURVE ( 'NONE', #113005, #238125, #175411, .T. ) ;
#234322 = ORIENTED_EDGE ( 'NONE', *, *, #179273, .T. ) ;
#234323 = CARTESIAN_POINT ( 'NONE',  ( -18.59999999999999787, 7.120270961708750512, -70.65956304183931991 ) ) ;
#234324 = DIRECTION ( 'NONE',  ( -0.000000000000000000, -6.982962677686266711E-15, 1.000000000000000000 ) ) ;
#234325 = DIRECTION ( 'NONE',  ( 0.000000000000000000, -1.000000000000000000, 0.000000000000000000 ) ) ;
#234326 = CARTESIAN_POINT ( 'NONE',  ( -20.94999999999999929, 87.75000000001212186, -133.4231074845242233 ) ) ;
#234327 = DIRECTION ( 'NONE',  ( 0.000000000000000000, 0.9126074666063844765, 0.4088369013363113980 ) ) ;
#234329 = CARTESIAN_POINT ( 'NONE',  ( -20.54999999999999716, 2.000000000011154189, -113.7246219227621395 ) ) ;
#234328 = CARTESIAN_POINT ( 'NONE',  ( 21.05000000000000071, 0.03201369319884249387, -161.2411572764626158 ) ) ;
#234331 = ORIENTED_EDGE ( 'NONE', *, *, #192191, .F. ) ;
#234330 = DIRECTION ( 'NONE',  ( 1.000000000000000000, 0.000000000000000000, -0.000000000000000000 ) ) ;
#234332 = PLANE ( 'NONE',  #141556 ) ;
#234333 = EDGE_LOOP ( 'NONE', ( #205338, #88941, #153390, #70474 ) ) ;
#234334 = CARTESIAN_POINT ( 'NONE',  ( -16.87368910959167678, 22.95032871809893749, -230.9074151025751860 ) ) ;
#234335 = ORIENTED_EDGE ( 'NONE', *, *, #102992, .F. ) ;
#234336 = VERTEX_POINT ( 'NONE', #235340 ) ;
#234337 = CARTESIAN_POINT ( 'NONE',  ( -16.93826681692523550, 65.98857127972381420, -48.57764901716495842 ) ) ;
#234338 = SPHERICAL_SURFACE ( 'NONE', #218324, 0.1000000000000000056 ) ;
#234339 = DIRECTION ( 'NONE',  ( 1.000000000000000000, 0.000000000000000000, 0.000000000000000000 ) ) ;
#234340 = EDGE_CURVE ( 'NONE', #61312, #73109, #256130, .T. ) ;
#234341 = DIRECTION ( 'NONE',  ( 0.7071067811865475727, -0.7071067811865475727, -4.937700262164531476E-15 ) ) ;
#234342 = EDGE_CURVE ( 'NONE', #170795, #154304, #82664, .T. ) ;
#234343 = AXIS2_PLACEMENT_3D ( 'NONE', #111489, #94482, #171495 ) ;
#234344 = DIRECTION ( 'NONE',  ( 0.000000000000000000, 0.000000000000000000, 1.000000000000000000 ) ) ;
#234345 = VERTEX_POINT ( 'NONE', #61861 ) ;
#234346 = ORIENTED_EDGE ( 'NONE', *, *, #159485, .T. ) ;
#234347 = CIRCLE ( 'NONE', #209401, 0.09999999999999939493 ) ;
#234348 = DIRECTION ( 'NONE',  ( 0.000000000000000000, 0.000000000000000000, 1.000000000000000000 ) ) ;
#234349 = ORIENTED_EDGE ( 'NONE', *, *, #240256, .T. ) ;
#234350 = CARTESIAN_POINT ( 'NONE',  ( -21.05000000000000071, 36.65892442174935439, -249.5511627012433848 ) ) ;
#234351 = DIRECTION ( 'NONE',  ( 2.952720810173289112E-16, 1.000000000000000000, -6.088138035986627436E-46 ) ) ;
#234352 = ORIENTED_EDGE ( 'NONE', *, *, #147689, .T. ) ;
#234353 = FACE_OUTER_BOUND ( 'NONE', #240737, .T. ) ;
#234354 = FACE_OUTER_BOUND ( 'NONE', #32746, .T. ) ;
#234356 = ADVANCED_FACE ( 'NONE', ( #44864 ), #244332, .T. ) ;
#234355 = CARTESIAN_POINT ( 'NONE',  ( 21.04999999999999716, 65.37127968600792371, -157.8731074845244393 ) ) ;
#234357 = ORIENTED_EDGE ( 'NONE', *, *, #136095, .T. ) ;
#234358 = EDGE_CURVE ( 'NONE', #67207, #84586, #201361, .T. ) ;
#234359 = DIRECTION ( 'NONE',  ( 1.652117596168391700E-15, -1.000000000000000000, -6.982962677686266711E-15 ) ) ;
#234360 = DIRECTION ( 'NONE',  ( 1.000000000000000000, 0.000000000000000000, 0.000000000000000000 ) ) ;
#234361 = EDGE_CURVE ( 'NONE', #45068, #186207, #143948, .T. ) ;
#234362 = CARTESIAN_POINT ( 'NONE',  ( -21.14999999999999858, 57.66663670110953888, -226.2321832927624712 ) ) ;
#234364 = ORIENTED_EDGE ( 'NONE', *, *, #217362, .F. ) ;
#234363 = AXIS2_PLACEMENT_3D ( 'NONE', #193399, #117687, #218048 ) ;
#234365 = CARTESIAN_POINT ( 'NONE',  ( 22.59999999999999787, 11.64957080754479968, 0.09999999999999592548 ) ) ;
#234366 = ORIENTED_EDGE ( 'NONE', *, *, #48003, .F. ) ;
#234367 = DIRECTION ( 'NONE',  ( 0.000000000000000000, -7.272083257015735086E-15, 1.000000000000000000 ) ) ;
#234368 = EDGE_CURVE ( 'NONE', #192659, #106265, #50599, .T. ) ;
#234369 = DIRECTION ( 'NONE',  ( 0.000000000000000000, -0.9915357197604853789, 0.1298341882520022694 ) ) ;
#234370 = DIRECTION ( 'NONE',  ( 0.000000000000000000, 0.1350103645451974088, -0.9908441862701587999 ) ) ;
#234371 = DIRECTION ( 'NONE',  ( 1.000000000000000000, -3.265361837132813093E-16, -2.280189983783949500E-30 ) ) ;
#234372 = LINE ( 'NONE', #257738, #233941 ) ;
#234373 = DIRECTION ( 'NONE',  ( 0.000000000000000000, -6.938893903907229955E-15, 1.000000000000000000 ) ) ;
#234374 = ORIENTED_EDGE ( 'NONE', *, *, #54909, .F. ) ;
#234375 = CARTESIAN_POINT ( 'NONE',  ( -17.05016517655717578, 66.05000000001224691, -149.1958054805180325 ) ) ;
#234376 = EDGE_CURVE ( 'NONE', #67858, #75809, #142652, .T. ) ;
#234377 = DIRECTION ( 'NONE',  ( -1.000000000000000000, 0.000000000000000000, 0.000000000000000000 ) ) ;
#234378 = CARTESIAN_POINT ( 'NONE',  ( 21.00023020733437207, 10.14655627732183873, -228.0991803899404431 ) ) ;
#234379 = CARTESIAN_POINT ( 'NONE',  ( 18.50000000000000000, 73.32445833535280144, -249.6821150215233160 ) ) ;
#234380 = CIRCLE ( 'NONE', #101048, 0.1000000000000032391 ) ;
#234381 = CARTESIAN_POINT ( 'NONE',  ( -20.54999999999999716, 2.000000000011154189, -187.7753780772378889 ) ) ;
#234382 = ORIENTED_EDGE ( 'NONE', *, *, #123322, .T. ) ;
#234383 = ORIENTED_EDGE ( 'NONE', *, *, #190693, .F. ) ;
#234384 = CARTESIAN_POINT ( 'NONE',  ( 20.94999999999999574, 36.65892442174472876, -249.5511627012454596 ) ) ;
#234386 = CARTESIAN_POINT ( 'NONE',  ( -21.00000000000000000, 6.239477252822117848, 11.95447128030241579 ) ) ;
#234385 = CIRCLE ( 'NONE', #230282, 0.09999999999998898659 ) ;
#234387 = CARTESIAN_POINT ( 'NONE',  ( 18.52351027002948314, -9.642162904695185333, -40.21504695050978029 ) ) ;
#234388 = PLANE ( 'NONE',  #130622 ) ;
#234389 =( BOUNDED_SURFACE ( )  B_SPLINE_SURFACE ( 3, 2, ( 
 ( #128833, #31043, #71436 ),
 ( #150956, #191396, #68867 ),
 ( #50538, #33623, #110533 ),
 ( #212229, #190083, #111835 ) ),
 .UNSPECIFIED., .F., .F., .F. ) 
 B_SPLINE_SURFACE_WITH_KNOTS ( ( 4, 4 ),
 ( 3, 3 ),
 ( 0.04058434257139458684, 0.04256401539001586354 ),
 ( 0.000000000000000000, 1.000000000000000000 ),
 .UNSPECIFIED. ) 
 GEOMETRIC_REPRESENTATION_ITEM ( )  RATIONAL_B_SPLINE_SURFACE ( (
 ( 1.000000000000000000, 0.7103081912008379906, 1.000000000000000000),
 ( 1.000000000000000000, 0.7104998333555697654, 1.000000000000000000),
 ( 1.000000000000000000, 0.7107238315754171865, 1.000000000000000000),
 ( 1.000000000000000000, 0.7110073749539332910, 1.000000000000000000) ) ) 
 REPRESENTATION_ITEM ( '' )  SURFACE ( )  );
#234390 = CARTESIAN_POINT ( 'NONE',  ( -21.55000000000000426, 68.29142135624952914, -148.7731074845244166 ) ) ;
#234391 = ORIENTED_EDGE ( 'NONE', *, *, #9014, .T. ) ;
#234392 = DIRECTION ( 'NONE',  ( -0.000000000000000000, 1.000000000000000000, 0.000000000000000000 ) ) ;
#234393 = SPHERICAL_SURFACE ( 'NONE', #229870, 0.1000000000000000056 ) ;
#234394 = AXIS2_PLACEMENT_3D ( 'NONE', #64313, #229493, #145114 ) ;
#234395 = ORIENTED_EDGE ( 'NONE', *, *, #196051, .T. ) ;
#234396 = AXIS2_PLACEMENT_3D ( 'NONE', #8763, #252487, #149578 ) ;
#234397 = DIRECTION ( 'NONE',  ( 2.952720810173289112E-16, 1.000000000000000000, 6.982962677686266711E-15 ) ) ;
#234398 = FACE_BOUND ( 'NONE', #81679, .T. ) ;
#234399 = ORIENTED_EDGE ( 'NONE', *, *, #114055, .F. ) ;
#234400 = DIRECTION ( 'NONE',  ( 1.000000000000000000, 0.000000000000000000, 0.000000000000000000 ) ) ;
#234401 = AXIS2_PLACEMENT_3D ( 'NONE', #183647, #4965, #84481 ) ;
#234402 = ORIENTED_EDGE ( 'NONE', *, *, #56813, .T. ) ;
#234403 = CARTESIAN_POINT ( 'NONE',  ( 23.24999999999999645, 76.00000000001190870, -103.0231074845243029 ) ) ;
#234404 = PLANE ( 'NONE',  #138163 ) ;
#234405 = CARTESIAN_POINT ( 'NONE',  ( 20.94999999999999929, 1.835341550235569663, -45.05515129256298223 ) ) ;
#234406 = CARTESIAN_POINT ( 'NONE',  ( -18.59999999999999787, 76.00000000001190870, -103.0231074845243029 ) ) ;
#234407 = DIRECTION ( 'NONE',  ( 0.000000000000000000, -1.000000000000000000, 0.000000000000000000 ) ) ;
#234408 = CARTESIAN_POINT ( 'NONE',  ( -23.25000000000000355, 10.05000000001113847, -180.2499999999999716 ) ) ;
#234410 = DIRECTION ( 'NONE',  ( 0.000000000000000000, -0.4999999999999689138, 0.8660254037844565822 ) ) ;
#234409 = AXIS2_PLACEMENT_3D ( 'NONE', #55504, #178081, #256236 ) ;
#234411 = AXIS2_PLACEMENT_3D ( 'NONE', #222884, #44270, #2549 ) ;
#234412 = DIRECTION ( 'NONE',  ( 0.000000000000000000, 0.4721928772778128947, 0.8814952561688012000 ) ) ;
#234415 = CARTESIAN_POINT ( 'NONE',  ( 23.15000000000000213, -12.41227409413852811, -197.9999999999999432 ) ) ;
#234414 = AXIS2_PLACEMENT_3D ( 'NONE', #61100, #4946, #42829 ) ;
#234413 = CARTESIAN_POINT ( 'NONE',  ( 20.95539060131842746, 10.62386215766680131, -108.1537338136562312 ) ) ;
#234416 = CYLINDRICAL_SURFACE ( 'NONE', #42090, 0.09999999999999939493 ) ;
#234417 = ADVANCED_FACE ( 'NONE', ( #106088 ), #21416, .T. ) ;
#234418 = CARTESIAN_POINT ( 'NONE',  ( -21.44999999999999929, 7.350000000011155166, -79.35000000000005116 ) ) ;
#234419 = CARTESIAN_POINT ( 'NONE',  ( 21.05000000000000071, 5.000000000011153745, -188.5947339810868755 ) ) ;
#234420 = CARTESIAN_POINT ( 'NONE',  ( 18.50016250449482413, 10.29766095125173386, -206.4743663933278697 ) ) ;
#234421 = ORIENTED_EDGE ( 'NONE', *, *, #30031, .F. ) ;
#234422 = DIRECTION ( 'NONE',  ( 0.000000000000000000, 0.000000000000000000, -1.000000000000000000 ) ) ;
#234423 = DIRECTION ( 'NONE',  ( 1.000000000000000000, -0.000000000000000000, -0.000000000000000000 ) ) ;
#234424 = ORIENTED_EDGE ( 'NONE', *, *, #230083, .F. ) ;
#234425 = CYLINDRICAL_SURFACE ( 'NONE', #18650, 0.09999999999998898659 ) ;
#234426 = CARTESIAN_POINT ( 'NONE',  ( -18.70000000000000639, -9.849999999999994316, 30.00000000000000000 ) ) ;
#234428 = ADVANCED_FACE ( 'NONE', ( #185657 ), #43581, .F. ) ;
#234427 = DIRECTION ( 'NONE',  ( 0.000000000000000000, 0.000000000000000000, 1.000000000000000000 ) ) ;
#234429 = EDGE_LOOP ( 'NONE', ( #190983, #57122, #219687, #190625 ) ) ;
#234430 = EDGE_CURVE ( 'NONE', #188870, #200249, #224764, .T. ) ;
#234431 = ADVANCED_FACE ( 'NONE', ( #180527 ), #42295, .T. ) ;
#234432 = DIRECTION ( 'NONE',  ( 0.000000000000000000, 0.8700118002898393765, -0.4930308989875104575 ) ) ;
#234433 = ORIENTED_EDGE ( 'NONE', *, *, #2812, .T. ) ;
#234434 = DIRECTION ( 'NONE',  ( 0.000000000000000000, 1.000000000000000000, 0.000000000000000000 ) ) ;
#234435 = DIRECTION ( 'NONE',  ( 0.000000000000000000, 0.9126074666063769270, 0.4088369013363282733 ) ) ;
#234436 = VECTOR ( 'NONE', #137430, 1000.000000000000000 ) ;
#234437 = ORIENTED_EDGE ( 'NONE', *, *, #121067, .F. ) ;
#234439 = LINE ( 'NONE', #248897, #51949 ) ;
#234438 = AXIS2_PLACEMENT_3D ( 'NONE', #82817, #157285, #102382 ) ;
#234440 = EDGE_CURVE ( 'NONE', #222817, #8158, #121393, .T. ) ;
#234441 = AXIS2_PLACEMENT_3D ( 'NONE', #193245, #56273, #251920 ) ;
#234442 = EDGE_LOOP ( 'NONE', ( #233921, #244112, #23457, #234785 ) ) ;
#234444 =( BOUNDED_SURFACE ( )  B_SPLINE_SURFACE ( 3, 2, ( 
 ( #99290, #22370, #237547 ),
 ( #118899, #221802, #198414 ),
 ( #223105, #2765, #43202 ),
 ( #100562, #23666, #183987 ) ),
 .UNSPECIFIED., .F., .F., .F. ) 
 B_SPLINE_SURFACE_WITH_KNOTS ( ( 4, 4 ),
 ( 3, 3 ),
 ( 0.3000847527772379508, 0.5552748953338751958 ),
 ( 0.000000000000000000, 1.000000000000000000 ),
 .UNSPECIFIED. ) 
 GEOMETRIC_REPRESENTATION_ITEM ( )  RATIONAL_B_SPLINE_SURFACE ( (
 ( 1.000000000000000000, 0.9152888060719377439, 1.000000000000000000),
 ( 1.000000000000000000, 0.9104333467450277384, 1.000000000000000000),
 ( 1.000000000000000000, 0.9035312726220520174, 1.000000000000000000),
 ( 1.000000000000000000, 0.8946697475932143817, 1.000000000000000000) ) ) 
 REPRESENTATION_ITEM ( '' )  SURFACE ( )  );
#234443 = DIRECTION ( 'NONE',  ( -1.000000000000000000, -0.000000000000000000, 0.000000000000000000 ) ) ;
#234445 = CARTESIAN_POINT ( 'NONE',  ( 21.04999999999999716, 67.12872031401640527, -124.3731074845243540 ) ) ;
#234447 = CIRCLE ( 'NONE', #113656, 0.1000000000000028644 ) ;
#234446 = CARTESIAN_POINT ( 'NONE',  ( -20.65000000000000568, 68.75000000001226397, -149.1731074845244223 ) ) ;
#234448 = CARTESIAN_POINT ( 'NONE',  ( -22.39999999999999858, 33.38250548509083160, -242.4821227592188961 ) ) ;
#234449 = LINE ( 'NONE', #115802, #39024 ) ;
#234450 = DIRECTION ( 'NONE',  ( 0.000000000000000000, -6.982962677686266711E-15, 1.000000000000000000 ) ) ;
#234451 = AXIS2_PLACEMENT_3D ( 'NONE', #229088, #209511, #30915 ) ;
#234452 = LINE ( 'NONE', #55788, #180353 ) ;
#234454 = DIRECTION ( 'NONE',  ( -1.476360405086644309E-16, 1.000000000000000000, 1.445602896647339410E-16 ) ) ;
#234453 = CIRCLE ( 'NONE', #151290, 0.1000000000000013933 ) ;
#234455 = CIRCLE ( 'NONE', #151291, 0.09999999999999939493 ) ;
#234457 = ORIENTED_EDGE ( 'NONE', *, *, #149709, .F. ) ;
#234456 = CARTESIAN_POINT ( 'NONE',  ( 18.60000000000000142, -0.6576273345615386567, -242.5323337003318898 ) ) ;
#234458 = ORIENTED_EDGE ( 'NONE', *, *, #24457, .T. ) ;
#234460 = CARTESIAN_POINT ( 'NONE',  ( -21.05000000000000071, 1.360870587203197646, -142.0729979270909951 ) ) ;
#234459 = CARTESIAN_POINT ( 'NONE',  ( -21.05000000000000071, 6.307425219565403474, -0.01681986838567561815 ) ) ;
#234461 = VERTEX_POINT ( 'NONE', #22754 ) ;
#234462 = EDGE_LOOP ( 'NONE', ( #18916, #56884, #1055, #147049, #81394 ) ) ;
#234463 = CARTESIAN_POINT ( 'NONE',  ( 18.49999999999999289, 10.29270135740183179, -38.95736188715193293 ) ) ;
#234464 = FACE_OUTER_BOUND ( 'NONE', #120610, .T. ) ;
#234465 = AXIS2_PLACEMENT_3D ( 'NONE', #157247, #120688, #197617 ) ;
#234466 = ADVANCED_FACE ( 'NONE', ( #104794 ), #85232, .T. ) ;
#234467 = DIRECTION ( 'NONE',  ( 1.000000000000000000, 0.000000000000000000, 0.000000000000000000 ) ) ;
#234468 = CARTESIAN_POINT ( 'NONE',  ( 18.59999994388910238, -9.363566187071151958, -7.181117236800915293 ) ) ;
#234469 = DIRECTION ( 'NONE',  ( 0.000000000000000000, 0.000000000000000000, 1.000000000000000000 ) ) ;
#234470 = CARTESIAN_POINT ( 'NONE',  ( 18.59999999999999787, -10.64999999999999325, 31.39999999999999858 ) ) ;
#234471 = TOROIDAL_SURFACE ( 'NONE', #159481, 11.65000000000000036, 0.1000000000000000056 ) ;
#234472 = DIRECTION ( 'NONE',  ( -0.000000000000000000, 0.1335171055202901691, 0.9910465087640861759 ) ) ;
#234473 = VECTOR ( 'NONE', #81479, 1000.000000000000000 ) ;
#234474 = ADVANCED_FACE ( 'NONE', ( #7012 ), #1854, .F. ) ;
#234475 = CARTESIAN_POINT ( 'NONE',  ( 20.04999999999999716, 61.20755944685602401, -224.6372899806900989 ) ) ;
#234476 = AXIS2_PLACEMENT_3D ( 'NONE', #195122, #176834, #192536 ) ;
#234477 = EDGE_LOOP ( 'NONE', ( #228204, #130577, #28300, #95575, #100673, #206545, #131880, #190989, #138938, #160832, #196544 ) ) ;
#234478 = EDGE_LOOP ( 'NONE', ( #183528, #60987, #103232, #210316 ) ) ;
#234479 = CARTESIAN_POINT ( 'NONE',  ( 22.94999999999999929, 0.000000000000000000, 0.000000000000000000 ) ) ;
#234480 = ORIENTED_EDGE ( 'NONE', *, *, #49665, .F. ) ;
#234481 = CARTESIAN_POINT ( 'NONE',  ( 20.95483826173899899, 8.876166204781142710, -142.5462755528995444 ) ) ;
#234482 = ORIENTED_EDGE ( 'NONE', *, *, #58447, .F. ) ;
#234484 = AXIS2_PLACEMENT_3D ( 'NONE', #8787, #145708, #107877 ) ;
#234483 = CARTESIAN_POINT ( 'NONE',  ( 18.40916198585732388, -9.500000000000000000, -40.10018963182346852 ) ) ;
#234486 =( BOUNDED_SURFACE ( )  B_SPLINE_SURFACE ( 3, 2, ( 
 ( #149004, #126850, #251930 ),
 ( #68159, #129417, #107282 ),
 ( #190709, #8201, #27784 ),
 ( #90269, #188111, #91578 ) ),
 .UNSPECIFIED., .F., .F., .F. ) 
 B_SPLINE_SURFACE_WITH_KNOTS ( ( 4, 4 ),
 ( 3, 3 ),
 ( -1.044899843732904898E-17, 0.0003124336600439518762 ),
 ( 0.000000000000000000, 1.000000000000000000 ),
 .UNSPECIFIED. ) 
 GEOMETRIC_REPRESENTATION_ITEM ( )  RATIONAL_B_SPLINE_SURFACE ( (
 ( 1.000000000000000000, 0.7071067811865475727, 1.000000000000000000),
 ( 1.000000000000000000, 0.7089187706050192883, 1.000000000000000000),
 ( 1.000000000000000000, 0.7039288185052067215, 1.000000000000000000),
 ( 1.000000000000000000, 0.7040654476015839602, 1.000000000000000000) ) ) 
 REPRESENTATION_ITEM ( '' )  SURFACE ( )  );
#234485 = VECTOR ( 'NONE', #289, 1000.000000000000000 ) ;
#234487 = AXIS2_PLACEMENT_3D ( 'NONE', #115524, #77665, #257547 ) ;
#234488 = VECTOR ( 'NONE', #44540, 1000.000000000000000 ) ;
#234489 = DIRECTION ( 'NONE',  ( 1.000000000000000000, -7.304098846218133681E-16, 4.217023435051677994E-16 ) ) ;
#234490 = CARTESIAN_POINT ( 'NONE',  ( -21.07928932188134041, 69.67148334361938566, -203.6220026301787982 ) ) ;
#234492 = ORIENTED_EDGE ( 'NONE', *, *, #79273, .T. ) ;
#234491 = CARTESIAN_POINT ( 'NONE',  ( -21.05000000000000071, 0.6656436123793491033, -212.6810495496487476 ) ) ;
#234493 = DIRECTION ( 'NONE',  ( -0.000000000000000000, 0.000000000000000000, 1.000000000000000000 ) ) ;
#234494 = VERTEX_POINT ( 'NONE', #39154 ) ;
#234495 = SPHERICAL_SURFACE ( 'NONE', #212725, 0.1000000000000000056 ) ;
#234496 = CARTESIAN_POINT ( 'NONE',  ( -18.54270223418607699, 85.62410550289428102, -29.28217243411683413 ) ) ;
#234497 = CARTESIAN_POINT ( 'NONE',  ( -14.00000000000000178, 9.850000000011133849, -117.2500000000000284 ) ) ;
#234498 = CARTESIAN_POINT ( 'NONE',  ( -20.64999999999999858, 7.249999999999999112, -12.34999999999999964 ) ) ;
#234499 = DIRECTION ( 'NONE',  ( 1.000000000000000000, 1.646408749285562691E-14, 1.073024830501117725E-15 ) ) ;
#234500 = VERTEX_POINT ( 'NONE', #157841 ) ;
#234502 = CARTESIAN_POINT ( 'NONE',  ( -18.44204374631838661, 85.49103638960970386, -29.39690621430322892 ) ) ;
#234501 = CARTESIAN_POINT ( 'NONE',  ( -17.04295772865349079, 60.86706971703560498, -221.0221225864443113 ) ) ;
#234503 = VECTOR ( 'NONE', #246391, 1000.000000000000000 ) ;
#234504 = ORIENTED_EDGE ( 'NONE', *, *, #61150, .T. ) ;
#234507 = EDGE_LOOP ( 'NONE', ( #99078, #147605, #33628 ) ) ;
#234506 = DIRECTION ( 'NONE',  ( 0.000000000000000000, -0.2128009952263603954, 0.9770955615653315052 ) ) ;
#234505 = CARTESIAN_POINT ( 'NONE',  ( 18.59999999999999076, 34.53503747617446606, -235.1972745784239578 ) ) ;
#234508 = CIRCLE ( 'NONE', #9655, 0.1000000000000028644 ) ;
#234509 = AXIS2_PLACEMENT_3D ( 'NONE', #92117, #115530, #76389 ) ;
#234510 = DIRECTION ( 'NONE',  ( 0.000000000000000000, -0.9908441862701620195, -0.1350103645451731504 ) ) ;
#234511 = AXIS2_PLACEMENT_3D ( 'NONE', #177191, #36390, #156344 ) ;
#234512 = EDGE_CURVE ( 'NONE', #103638, #10718, #195663, .T. ) ;
#234513 = CARTESIAN_POINT ( 'NONE',  ( -22.59999999999999787, -2.401771312552908544, -189.4980873520049727 ) ) ;
#234514 = ORIENTED_EDGE ( 'NONE', *, *, #33450, .T. ) ;
#234516 = EDGE_CURVE ( 'NONE', #186482, #199102, #238043, .T. ) ;
#234515 = DIRECTION ( 'NONE',  ( -0.7071067811865475727, -0.7071067811865475727, -0.000000000000000000 ) ) ;
#234517 = CARTESIAN_POINT ( 'NONE',  ( -18.50000000000000000, 22.43030315632513094, -231.3223027016406093 ) ) ;
#234518 = EDGE_CURVE ( 'NONE', #4833, #25796, #96390, .T. ) ;
#234519 = CARTESIAN_POINT ( 'NONE',  ( -17.11825945287482753, 9.949999999999983302, -12.75000000000000178 ) ) ;
#234520 = EDGE_CURVE ( 'NONE', #163777, #167847, #242138, .T. ) ;
#234522 = VERTEX_POINT ( 'NONE', #58666 ) ;
#234521 = DIRECTION ( 'NONE',  ( 1.000000000000000000, 0.000000000000000000, 0.000000000000000000 ) ) ;
#234523 = CARTESIAN_POINT ( 'NONE',  ( 20.85000000000000142, 77.13501884592203339, -95.30613060109196510 ) ) ;
#234525 = ORIENTED_EDGE ( 'NONE', *, *, #58742, .T. ) ;
#234524 = EDGE_CURVE ( 'NONE', #115598, #203961, #138202, .T. ) ;
#234526 = CARTESIAN_POINT ( 'NONE',  ( 18.39999999999999858, -9.599999999988842347, -40.53206939669966857 ) ) ;
#234527 = CARTESIAN_POINT ( 'NONE',  ( -16.77732147278574715, 44.14945876519793444, -235.2970893357522755 ) ) ;
#234528 = EDGE_CURVE ( 'NONE', #249547, #189014, #160389, .T. ) ;
#234529 = ORIENTED_EDGE ( 'NONE', *, *, #79470, .F. ) ;
#234530 = CARTESIAN_POINT ( 'NONE',  ( 18.59999999999999787, -1.835341550213255957, -179.0551512925629538 ) ) ;
#234533 = EDGE_CURVE ( 'NONE', #168738, #133183, #220349, .T. ) ;
#234532 = EDGE_CURVE ( 'NONE', #122037, #80105, #75593, .T. ) ;
#234531 = ORIENTED_EDGE ( 'NONE', *, *, #102683, .T. ) ;
#234534 = CARTESIAN_POINT ( 'NONE',  ( -20.07928932188135107, 9.220710678129810489, -188.6499999999999488 ) ) ;
#234535 = CIRCLE ( 'NONE', #192859, 0.1000000000000075273 ) ;
#234536 = CARTESIAN_POINT ( 'NONE',  ( -21.14999999999999858, 64.35000000001214460, -136.4231074845243938 ) ) ;
#234537 = CARTESIAN_POINT ( 'NONE',  ( -16.87242674293850797, 9.950000000011138823, -46.14890975362765602 ) ) ;
#234538 = EDGE_CURVE ( 'NONE', #140485, #213407, #178680, .T. ) ;
#234539 = ORIENTED_EDGE ( 'NONE', *, *, #121777, .T. ) ;
#234540 = CARTESIAN_POINT ( 'NONE',  ( 20.94999999999997442, 77.26327546522934142, -128.6212428177779543 ) ) ;
#234541 = DIRECTION ( 'NONE',  ( 0.000000000000000000, 0.2617529984165035128, 0.9651348961777155289 ) ) ;
#234542 = EDGE_CURVE ( 'NONE', #130397, #217842, #13219, .T. ) ;
#234543 = VERTEX_POINT ( 'NONE', #140802 ) ;
#234544 = FACE_BOUND ( 'NONE', #243286, .T. ) ;
#234545 = CARTESIAN_POINT ( 'NONE',  ( -20.85000000000000142, 76.00000000001244871, -170.0231074845243597 ) ) ;
#234546 = EDGE_CURVE ( 'NONE', #86168, #88245, #104736, .T. ) ;
#234549 = ADVANCED_FACE ( 'NONE', ( #236040 ), #121279, .F. ) ;
#234548 = DIRECTION ( 'NONE',  ( 0.000000000000000000, 0.4721928772777346239, 0.8814952561688430555 ) ) ;
#234547 = VECTOR ( 'NONE', #20928, 1000.000000000000000 ) ;
#234551 = ORIENTED_EDGE ( 'NONE', *, *, #224602, .T. ) ;
#234550 = AXIS2_PLACEMENT_3D ( 'NONE', #95247, #78242, #157837 ) ;
#234552 = VERTEX_POINT ( 'NONE', #199508 ) ;
#234553 = ADVANCED_FACE ( 'NONE', ( #255554 ), #242761, .T. ) ;
#234554 = FACE_OUTER_BOUND ( 'NONE', #711, .T. ) ;
#234555 = ORIENTED_EDGE ( 'NONE', *, *, #109583, .T. ) ;
#234557 = ORIENTED_EDGE ( 'NONE', *, *, #5405, .T. ) ;
#234556 = CARTESIAN_POINT ( 'NONE',  ( -18.59999999999999787, 9.150000000011157653, -121.6500000000000341 ) ) ;
#234558 = EDGE_CURVE ( 'NONE', #23243, #7494, #167179, .T. ) ;
#234561 = ORIENTED_EDGE ( 'NONE', *, *, #228834, .F. ) ;
#234560 = ORIENTED_EDGE ( 'NONE', *, *, #173253, .T. ) ;
#234559 = CARTESIAN_POINT ( 'NONE',  ( -21.10320863425827298, 0.02502225122710637073, 6.400277386459231721 ) ) ;
#234562 = EDGE_CURVE ( 'NONE', #125918, #68814, #222888, .T. ) ;
#234563 = DIRECTION ( 'NONE',  ( 0.000000000000000000, 0.000000000000000000, -1.000000000000000000 ) ) ;
#234564 = CARTESIAN_POINT ( 'NONE',  ( -16.88783316861821859, 12.43579531710911290, -211.3428106928266743 ) ) ;
#234565 = DIRECTION ( 'NONE',  ( 0.000000000000000000, 0.000000000000000000, -1.000000000000000000 ) ) ;
#234566 = DIRECTION ( 'NONE',  ( 0.000000000000000000, 0.000000000000000000, 1.000000000000000000 ) ) ;
#234567 = AXIS2_PLACEMENT_3D ( 'NONE', #111651, #205602, #88205 ) ;
#234568 = FACE_OUTER_BOUND ( 'NONE', #134919, .T. ) ;
#234569 = CARTESIAN_POINT ( 'NONE',  ( -22.50000000000089173, 26.00803755075855150, -254.2729232455174326 ) ) ;
#234570 = ORIENTED_EDGE ( 'NONE', *, *, #115307, .F. ) ;
#234571 = EDGE_LOOP ( 'NONE', ( #95403, #223398, #58944, #137299 ) ) ;
#234572 = VERTEX_POINT ( 'NONE', #8986 ) ;
#234573 = AXIS2_PLACEMENT_3D ( 'NONE', #18058, #20652, #100136 ) ;
#234574 = CARTESIAN_POINT ( 'NONE',  ( 21.05000000000000071, 36.65892442174935439, -249.5511627012433848 ) ) ;
#234576 = ORIENTED_EDGE ( 'NONE', *, *, #231207, .T. ) ;
#234575 = FACE_OUTER_BOUND ( 'NONE', #173114, .T. ) ;
#234577 = ORIENTED_EDGE ( 'NONE', *, *, #47159, .F. ) ;
#234578 = EDGE_CURVE ( 'NONE', #241989, #56194, #63071, .T. ) ;
#234579 = CARTESIAN_POINT ( 'NONE',  ( -23.25000000000000000, 69.01799029515524353, -65.82695536626808064 ) ) ;
#234580 = ORIENTED_EDGE ( 'NONE', *, *, #191182, .T. ) ;
#234581 = DIRECTION ( 'NONE',  ( 0.000000000000000000, -0.4721928772777346239, -0.8814952561688430555 ) ) ;
#234582 = AXIS2_PLACEMENT_3D ( 'NONE', #235579, #250023, #56919 ) ;
#234583 = CIRCLE ( 'NONE', #188802, 0.1999999999999987899 ) ;
#234584 = VERTEX_POINT ( 'NONE', #243747 ) ;
#234585 = CIRCLE ( 'NONE', #238877, 7.900000000000003908 ) ;
#234586 = PLANE ( 'NONE',  #97901 ) ;
#234587 = CARTESIAN_POINT ( 'NONE',  ( 23.15000000000000213, 85.50000000001179501, -79.41707660717668205 ) ) ;
#234589 = ORIENTED_EDGE ( 'NONE', *, *, #38735, .T. ) ;
#234588 = ORIENTED_EDGE ( 'NONE', *, *, #152737, .T. ) ;
#234590 = ORIENTED_EDGE ( 'NONE', *, *, #137973, .F. ) ;
#234591 = DIRECTION ( 'NONE',  ( 0.000000000000000000, 0.000000000000000000, -1.000000000000000000 ) ) ;
#234592 = EDGE_LOOP ( 'NONE', ( #82460, #120635, #133550, #103369 ) ) ;
#234593 = ORIENTED_EDGE ( 'NONE', *, *, #127464, .T. ) ;
#234595 = CARTESIAN_POINT ( 'NONE',  ( 21.05000000000000071, 8.826429739528350638, -75.41405471294373797 ) ) ;
#234594 = CIRCLE ( 'NONE', #188808, 0.09999999999999939493 ) ;
#234597 = ORIENTED_EDGE ( 'NONE', *, *, #179863, .T. ) ;
#234596 = CARTESIAN_POINT ( 'NONE',  ( 18.31572054635740443, -9.548475435767665331, -107.3505701647485324 ) ) ;
#234598 = CARTESIAN_POINT ( 'NONE',  ( 18.59999999999999432, 1.261786168576181755, -75.08649896354552311 ) ) ;
#234600 = CARTESIAN_POINT ( 'NONE',  ( 21.05000000000000071, 1.115600667400684642E-11, -198.0999999999999659 ) ) ;
#234599 = DIRECTION ( 'NONE',  ( 1.000000000000000000, 0.000000000000000000, 0.000000000000000000 ) ) ;
#234601 = DIRECTION ( 'NONE',  ( 0.000000000000000000, 1.000000000000000000, 0.000000000000000000 ) ) ;
#234602 = FACE_OUTER_BOUND ( 'NONE', #24014, .T. ) ;
#234603 = DIRECTION ( 'NONE',  ( 0.000000000000000000, -0.9998779222360097974, 0.01562500000000363945 ) ) ;
#234604 = ORIENTED_EDGE ( 'NONE', *, *, #149417, .F. ) ;
#234605 = AXIS2_PLACEMENT_3D ( 'NONE', #250445, #71834, #151372 ) ;
#234606 = AXIS2_PLACEMENT_3D ( 'NONE', #24819, #27396, #67762 ) ;
#234607 = CIRCLE ( 'NONE', #34924, 0.09999999999999939493 ) ;
#234608 = VERTEX_POINT ( 'NONE', #104218 ) ;
#234610 = AXIS2_PLACEMENT_3D ( 'NONE', #158420, #59233, #138777 ) ;
#234609 = CARTESIAN_POINT ( 'NONE',  ( -21.05000000000000071, 74.75000000001261924, -195.5231074845243597 ) ) ;
#234611 = DIRECTION ( 'NONE',  ( 1.284434275755705789E-16, -0.7071067811865472397, -0.7071067811865479058 ) ) ;
#234613 = EDGE_CURVE ( 'NONE', #33310, #5863, #44276, .T. ) ;
#234612 = DIRECTION ( 'NONE',  ( 1.000000000000000000, 0.000000000000000000, 0.000000000000000000 ) ) ;
#234614 = ORIENTED_EDGE ( 'NONE', *, *, #2109, .T. ) ;
#234615 = DIRECTION ( 'NONE',  ( 0.000000000000000000, -0.000000000000000000, 1.000000000000000000 ) ) ;
#234616 = EDGE_CURVE ( 'NONE', #168532, #117140, #83883, .T. ) ;
#234617 = CARTESIAN_POINT ( 'NONE',  ( 20.94999999999999929, 53.66153320161009788, -235.9075159595686841 ) ) ;
#234618 = DIRECTION ( 'NONE',  ( -0.000000000000000000, 7.109473446599835262E-15, -1.000000000000000000 ) ) ;
#234619 = ORIENTED_EDGE ( 'NONE', *, *, #45917, .T. ) ;
#234620 = ORIENTED_EDGE ( 'NONE', *, *, #52569, .F. ) ;
#234621 = EDGE_CURVE ( 'NONE', #68788, #126269, #207205, .T. ) ;
#234622 = FACE_OUTER_BOUND ( 'NONE', #162625, .T. ) ;
#234624 = EDGE_CURVE ( 'NONE', #212285, #173670, #79819, .T. ) ;
#234623 = DIRECTION ( 'NONE',  ( 0.000000000000000000, 0.000000000000000000, 1.000000000000000000 ) ) ;
#234625 = ORIENTED_EDGE ( 'NONE', *, *, #189420, .F. ) ;
#234626 = DIRECTION ( 'NONE',  ( -1.000000000000000000, 3.265361837132813093E-16, 2.280189983783949500E-30 ) ) ;
#234627 = ORIENTED_EDGE ( 'NONE', *, *, #122180, .T. ) ;
#234628 = FACE_OUTER_BOUND ( 'NONE', #206963, .T. ) ;
#234629 = DIRECTION ( 'NONE',  ( 0.000000000000000000, -1.000000000000000000, -0.000000000000000000 ) ) ;
#234631 = CARTESIAN_POINT ( 'NONE',  ( -18.34374000495059676, 64.52683809664901560, -45.27310748452439526 ) ) ;
#234630 = CARTESIAN_POINT ( 'NONE',  ( -20.54999999999999716, 11.74265569217025629, -210.9797313238103698 ) ) ;
#234632 = EDGE_CURVE ( 'NONE', #105159, #166958, #127658, .T. ) ;
#234633 = CARTESIAN_POINT ( 'NONE',  ( -18.40000000000000213, 13.19198836721619017, -207.5937580722650466 ) ) ;
#234634 = CARTESIAN_POINT ( 'NONE',  ( -20.65000000000000568, 21.70314669089253812, -233.3151006027785286 ) ) ;
#234635 = AXIS2_PLACEMENT_3D ( 'NONE', #182178, #100033, #179622 ) ;
#234636 = AXIS2_PLACEMENT_3D ( 'NONE', #226958, #206113, #48317 ) ;
#234637 = CYLINDRICAL_SURFACE ( 'NONE', #181624, 0.09999999999999681366 ) ;
#234638 = VECTOR ( 'NONE', #67997, 1000.000000000000000 ) ;
#234639 = EDGE_CURVE ( 'NONE', #98749, #21212, #25676, .T. ) ;
#234641 = ORIENTED_EDGE ( 'NONE', *, *, #21925, .T. ) ;
#234640 = ORIENTED_EDGE ( 'NONE', *, *, #53724, .T. ) ;
#234642 = ORIENTED_EDGE ( 'NONE', *, *, #204115, .T. ) ;
#234643 = CIRCLE ( 'NONE', #113838, 11.80000000000000604 ) ;
#234644 = DIRECTION ( 'NONE',  ( 1.000000000000000000, 0.000000000000000000, 0.000000000000000000 ) ) ;
#234645 = CARTESIAN_POINT ( 'NONE',  ( 21.05000000000000071, 1.115653327213047955E-11, -37.80000000000003268 ) ) ;
#234646 = VECTOR ( 'NONE', #152559, 1000.000000000000000 ) ;
#234647 = DIRECTION ( 'NONE',  ( -1.000000000000000000, 0.000000000000000000, -0.000000000000000000 ) ) ;
#234648 = CARTESIAN_POINT ( 'NONE',  ( -18.50000000000000355, -9.419203418015493767, -107.7477858104286952 ) ) ;
#234650 = DIRECTION ( 'NONE',  ( -1.000000000000000000, 0.000000000000000000, 0.000000000000000000 ) ) ;
#234649 = DIRECTION ( 'NONE',  ( 0.000000000000000000, 0.000000000000000000, 1.000000000000000000 ) ) ;
#234651 = DIRECTION ( 'NONE',  ( -1.000000000000000000, -2.952720810173289112E-16, 0.000000000000000000 ) ) ;
#234652 = VERTEX_POINT ( 'NONE', #144631 ) ;
#234653 = CARTESIAN_POINT ( 'NONE',  ( 20.94999999999999929, 1.115600667400684642E-11, -100.5000000000000426 ) ) ;
#234654 = ORIENTED_EDGE ( 'NONE', *, *, #33845, .T. ) ;
#234655 = VERTEX_POINT ( 'NONE', #108098 ) ;
#234656 = DIRECTION ( 'NONE',  ( -2.952720810173288126E-16, 0.9770955615653313941, 0.2128009952263603677 ) ) ;
#234657 = CIRCLE ( 'NONE', #188863, 0.1999999999999987899 ) ;
#234658 = CARTESIAN_POINT ( 'NONE',  ( -20.94999999999999929, 87.65000000001266756, -200.4231074845242802 ) ) ;
#234659 = VECTOR ( 'NONE', #133255, 1000.000000000000000 ) ;
#234660 = VECTOR ( 'NONE', #155070, 1000.000000000000000 ) ;
#234661 = CARTESIAN_POINT ( 'NONE',  ( 20.94999999999999929, 48.50000630096247534, -244.2465039064066161 ) ) ;
#234662 = AXIS2_PLACEMENT_3D ( 'NONE', #156725, #95432, #94138 ) ;
#234663 = EDGE_CURVE ( 'NONE', #32814, #10416, #224174, .T. ) ;
#234664 = CARTESIAN_POINT ( 'NONE',  ( 20.94999999999999574, 47.95459712139159336, -246.5019368548292675 ) ) ;
#234665 = AXIS2_PLACEMENT_3D ( 'NONE', #149233, #48818, #90503 ) ;
#234666 = FACE_OUTER_BOUND ( 'NONE', #8462, .T. ) ;
#234667 = EDGE_LOOP ( 'NONE', ( #232098, #145663, #49806, #34686 ) ) ;
#234668 = ORIENTED_EDGE ( 'NONE', *, *, #139158, .T. ) ;
#234669 = DIRECTION ( 'NONE',  ( 0.000000000000000000, 0.8814952561688476074, -0.4721928772777262417 ) ) ;
#234670 = CARTESIAN_POINT ( 'NONE',  ( -18.43569575749026157, -9.519327731081286714, -40.47297637655933045 ) ) ;
#234671 = CYLINDRICAL_SURFACE ( 'NONE', #48109, 0.09999999999999939493 ) ;
#234672 = DIRECTION ( 'NONE',  ( 0.000000000000000000, 0.9126074666063632712, 0.4088369013363589710 ) ) ;
#234674 = TOROIDAL_SURFACE ( 'NONE', #105448, 0.2000000000000000111, 0.1000000000000000056 ) ;
#234673 = DIRECTION ( 'NONE',  ( 1.000000000000000000, 0.000000000000000000, 0.000000000000000000 ) ) ;
#234676 = EDGE_CURVE ( 'NONE', #187924, #54334, #85924, .T. ) ;
#234675 = DIRECTION ( 'NONE',  ( 1.000000000000000000, -0.000000000000000000, -0.000000000000000000 ) ) ;
#234677 = FACE_OUTER_BOUND ( 'NONE', #188728, .T. ) ;
#234679 = CARTESIAN_POINT ( 'NONE',  ( -20.85000000000000142, 36.17635217701698025, -235.9630383263116471 ) ) ;
#234678 = CARTESIAN_POINT ( 'NONE',  ( -22.49072729836729678, 0.05648193273361867134, 11.65000824915494171 ) ) ;
#234680 = FACE_OUTER_BOUND ( 'NONE', #242413, .T. ) ;
#234681 = ADVANCED_FACE ( 'NONE', ( #68986 ), #46809, .F. ) ;
#234682 = LINE ( 'NONE', #177311, #237523 ) ;
#234683 = CIRCLE ( 'NONE', #176253, 0.1999999999999987899 ) ;
#234684 = DIRECTION ( 'NONE',  ( 1.000000000000000000, 0.000000000000000000, 0.000000000000000000 ) ) ;
#234685 = DIRECTION ( 'NONE',  ( 0.000000000000000000, -1.000000000000000000, 0.000000000000000000 ) ) ;
#234687 = VERTEX_POINT ( 'NONE', #186356 ) ;
#234686 = LINE ( 'NONE', #135567, #173842 ) ;
#234688 = AXIS2_PLACEMENT_3D ( 'NONE', #29368, #224937, #147991 ) ;
#234689 = CIRCLE ( 'NONE', #122255, 0.3999999999999975797 ) ;
#234690 = ADVANCED_FACE ( 'NONE', ( #7719 ), #147214, .F. ) ;
#234691 = AXIS2_PLACEMENT_3D ( 'NONE', #26934, #185978, #84251 ) ;
#234692 = CYLINDRICAL_SURFACE ( 'NONE', #99421, 0.09999999999999939493 ) ;
#234693 = ORIENTED_EDGE ( 'NONE', *, *, #188434, .T. ) ;
#234694 = EDGE_CURVE ( 'NONE', #44671, #230071, #192282, .T. ) ;
#234695 = EDGE_CURVE ( 'NONE', #2508, #133095, #113161, .T. ) ;
#234696 = CARTESIAN_POINT ( 'NONE',  ( 18.59999999999999076, 6.450000000000001066, -10.01702717044001822 ) ) ;
#234697 = ORIENTED_EDGE ( 'NONE', *, *, #4183, .F. ) ;
#234698 = DIRECTION ( 'NONE',  ( 0.000000000000000000, -6.982962677686266711E-15, 1.000000000000000000 ) ) ;
#234699 = EDGE_CURVE ( 'NONE', #128131, #40157, #70277, .T. ) ;
#234700 = CARTESIAN_POINT ( 'NONE',  ( 13.77030915526558630, 9.456007326080463571, -85.48863349414679647 ) ) ;
#234701 = DIRECTION ( 'NONE',  ( 0.000000000000000000, 0.000000000000000000, 1.000000000000000000 ) ) ;
#234702 = VECTOR ( 'NONE', #130934, 999.9999999999998863 ) ;
#234703 = VECTOR ( 'NONE', #32131, 1000.000000000000000 ) ;
#234704 = AXIS2_PLACEMENT_3D ( 'NONE', #232640, #253448, #74860 ) ;
#234706 = LINE ( 'NONE', #174778, #138945 ) ;
#234705 = VECTOR ( 'NONE', #152176, 1000.000000000000000 ) ;
#234707 = CARTESIAN_POINT ( 'NONE',  ( -21.05000000000000071, 16.98881331171929787, -224.4946931418895417 ) ) ;
#234708 = CARTESIAN_POINT ( 'NONE',  ( -18.50000000000000000, 64.35000000001157616, -57.37310748452439668 ) ) ;
#234709 = ORIENTED_EDGE ( 'NONE', *, *, #195975, .T. ) ;
#234710 = CARTESIAN_POINT ( 'NONE',  ( 20.85000000000000142, 1.115600667400684642E-11, -100.5000000000000426 ) ) ;
#234712 = ORIENTED_EDGE ( 'NONE', *, *, #80848, .T. ) ;
#234711 = CYLINDRICAL_SURFACE ( 'NONE', #76076, 0.09999999999999939493 ) ;
#234713 = DIRECTION ( 'NONE',  ( 0.000000000000000000, -1.000000000000000000, 0.000000000000000000 ) ) ;
#234714 = EDGE_CURVE ( 'NONE', #133700, #45318, #179628, .T. ) ;
#234715 = CARTESIAN_POINT ( 'NONE',  ( 20.94999999999999929, 0.000000000000000000, -33.50000000000000000 ) ) ;
#234716 = B_SPLINE_CURVE_WITH_KNOTS ( 'NONE', 3,
 ( #83392, #6446, #20915, #242491, #161703, #203378, #142110, #165544, #245064, #66433, #2590, #225477, #200811, #63863, #46845, #179974, #1302, #80837, #160428 ),
 .UNSPECIFIED., .F., .F.,
 ( 4, 3, 3, 3, 3, 3, 4 ),
 ( 0.000000000000000000, 7.110282409890467483E-05, 0.0001508797727291509062, 0.0002027344179858535443, 0.0002343294522349110036, 0.0002454816334821511518, 0.0002619873080085817312 ),
 .UNSPECIFIED. ) ;
#234717 = CARTESIAN_POINT ( 'NONE',  ( -22.50000000000000355, 31.76322370622490254, -238.8696546380523955 ) ) ;
#234718 = VERTEX_POINT ( 'NONE', #29865 ) ;
#234719 = DIRECTION ( 'NONE',  ( 1.186688945009009831E-16, -0.9770955615653316162, -0.2128009952263604232 ) ) ;
#234720 = APPLICATION_PROTOCOL_DEFINITION ( 'draft international standard', 'automotive_design', 1998, #78994 ) ;
#234721 = FACE_OUTER_BOUND ( 'NONE', #247334, .T. ) ;
#234722 = FACE_OUTER_BOUND ( 'NONE', #65377, .T. ) ;
#234723 = ORIENTED_EDGE ( 'NONE', *, *, #105065, .F. ) ;
#234724 = LINE ( 'NONE', #230892, #179567 ) ;
#234725 = DIRECTION ( 'NONE',  ( -2.602085213965225788E-14, -0.8814952561688430555, 0.4721928772777346239 ) ) ;
#234726 = AXIS2_PLACEMENT_3D ( 'NONE', #134386, #256869, #99105 ) ;
#234727 = DIRECTION ( 'NONE',  ( 0.000000000000000000, 6.982962677686266711E-15, -1.000000000000000000 ) ) ;
#234728 = ORIENTED_EDGE ( 'NONE', *, *, #210037, .F. ) ;
#234729 = ORIENTED_EDGE ( 'NONE', *, *, #181262, .F. ) ;
#234730 = DIRECTION ( 'NONE',  ( 1.000000000000000000, 0.000000000000000000, 0.000000000000000000 ) ) ;
#234731 = DIRECTION ( 'NONE',  ( 1.000000000000000000, 7.304098846218134667E-16, 0.000000000000000000 ) ) ;
#234732 = DIRECTION ( 'NONE',  ( -5.603264701231743991E-32, -7.172728831056617961E-15, 1.000000000000000000 ) ) ;
#234733 = DIRECTION ( 'NONE',  ( 0.000000000000000000, 0.000000000000000000, 1.000000000000000000 ) ) ;
#234735 = CARTESIAN_POINT ( 'NONE',  ( -23.25000000000000000, 76.00000000001240608, -174.0731074845243711 ) ) ;
#234734 = DIRECTION ( 'NONE',  ( 0.000000000000000000, 0.000000000000000000, -1.000000000000000000 ) ) ;
#234736 = CARTESIAN_POINT ( 'NONE',  ( 20.94999675878240808, 65.70692517833182933, -30.56446533783036656 ) ) ;
#234737 = DIRECTION ( 'NONE',  ( -0.000000000000000000, 0.8700118002898356018, -0.4930308989875170078 ) ) ;
#234738 = CYLINDRICAL_SURFACE ( 'NONE', #8876, 12.87499999999999822 ) ;
#234739 = AXIS2_PLACEMENT_3D ( 'NONE', #216863, #39559, #235160 ) ;
#234740 = ORIENTED_EDGE ( 'NONE', *, *, #17010, .F. ) ;
#234741 = ADVANCED_FACE ( 'NONE', ( #193728 ), #233799, .F. ) ;
#234742 = AXIS2_PLACEMENT_3D ( 'NONE', #105480, #122529, #127893 ) ;
#234743 = ORIENTED_EDGE ( 'NONE', *, *, #236978, .T. ) ;
#234744 = DIRECTION ( 'NONE',  ( -2.952720810173288619E-16, 1.000000000000000000, 0.000000000000000000 ) ) ;
#234745 = CARTESIAN_POINT ( 'NONE',  ( -17.22767730082145832, 65.65075578754345997, -147.8806787939494143 ) ) ;
#234748 = DIRECTION ( 'NONE',  ( 1.000000000000000000, 0.000000000000000000, 0.000000000000000000 ) ) ;
#234747 = DIRECTION ( 'NONE',  ( 0.000000000000000000, 0.3738317757009942399, -0.9274965247785252886 ) ) ;
#234746 = CIRCLE ( 'NONE', #55635, 0.09999999999999939493 ) ;
#234749 = CYLINDRICAL_SURFACE ( 'NONE', #114134, 0.09999999999999850675 ) ;
#234750 = FACE_OUTER_BOUND ( 'NONE', #207334, .T. ) ;
#234752 = EDGE_CURVE ( 'NONE', #16790, #191917, #187995, .T. ) ;
#234751 = CARTESIAN_POINT ( 'NONE',  ( 15.74999999999999645, 12.70026017068886226, -215.3766613508543628 ) ) ;
#234753 = VERTEX_POINT ( 'NONE', #38510 ) ;
#234754 = ORIENTED_EDGE ( 'NONE', *, *, #69519, .T. ) ;
#234755 = EDGE_CURVE ( 'NONE', #243170, #13299, #118035, .T. ) ;
#234756 = EDGE_CURVE ( 'NONE', #42338, #53868, #89793, .T. ) ;
#234757 = CARTESIAN_POINT ( 'NONE',  ( -23.25000000000000000, 4.250000000011156409, -45.65000000000000568 ) ) ;
#234758 = ORIENTED_EDGE ( 'NONE', *, *, #15429, .T. ) ;
#234759 = CARTESIAN_POINT ( 'NONE',  ( 23.14999999999999503, 11.65000000001116298, -193.9851942293460070 ) ) ;
#234760 = VECTOR ( 'NONE', #32820, 1000.000000000000114 ) ;
#234761 = DIRECTION ( 'NONE',  ( 1.000000000000000000, 0.000000000000000000, 0.000000000000000000 ) ) ;
#234763 = AXIS2_PLACEMENT_3D ( 'NONE', #191239, #253730, #12596 ) ;
#234762 = CARTESIAN_POINT ( 'NONE',  ( -21.08035267497491816, 65.49412562536262783, -241.9444337344500298 ) ) ;
#234764 = TOROIDAL_SURFACE ( 'NONE', #218164, 4.099999999999999645, 0.1000000000000000056 ) ;
#234765 = ORIENTED_EDGE ( 'NONE', *, *, #99529, .T. ) ;
#234766 = EDGE_CURVE ( 'NONE', #207854, #74489, #10288, .T. ) ;
#234767 = EDGE_LOOP ( 'NONE', ( #189626, #67362, #90368, #217473 ) ) ;
#234768 = DIRECTION ( 'NONE',  ( -1.000000000000000000, 0.000000000000000000, 0.000000000000000000 ) ) ;
#234769 = DIRECTION ( 'NONE',  ( -1.000000000000000000, 0.000000000000000000, 0.000000000000000000 ) ) ;
#234770 = LINE ( 'NONE', #47450, #7346 ) ;
#234771 = AXIS2_PLACEMENT_3D ( 'NONE', #55326, #133609, #150618 ) ;
#234773 = DIRECTION ( 'NONE',  ( -0.000000000000000000, -0.000000000000000000, 1.000000000000000000 ) ) ;
#234772 = CIRCLE ( 'NONE', #188994, 0.09999999999999939493 ) ;
#234774 = CARTESIAN_POINT ( 'NONE',  ( -23.15000000000000213, 71.85000000001205933, -124.1731074845243228 ) ) ;
#234777 = CYLINDRICAL_SURFACE ( 'NONE', #220923, 0.09999999999999811817 ) ;
#234776 = VECTOR ( 'NONE', #14486, 1000.000000000000000 ) ;
#234775 = CARTESIAN_POINT ( 'NONE',  ( 20.94999999999999929, -1.835341550213257733, -145.5551512925629822 ) ) ;
#234778 = FACE_OUTER_BOUND ( 'NONE', #183066, .T. ) ;
#234779 = ORIENTED_EDGE ( 'NONE', *, *, #13722, .F. ) ;
#234781 = FACE_OUTER_BOUND ( 'NONE', #47764, .T. ) ;
#234780 = CARTESIAN_POINT ( 'NONE',  ( 22.39999999999999503, 0.1000000000111554016, -127.7500000000000284 ) ) ;
#234782 = ORIENTED_EDGE ( 'NONE', *, *, #222801, .F. ) ;
#234784 = VERTEX_POINT ( 'NONE', #128946 ) ;
#234783 = DIRECTION ( 'NONE',  ( 1.000000000000000000, 0.000000000000000000, 0.000000000000000000 ) ) ;
#234785 = ORIENTED_EDGE ( 'NONE', *, *, #20280, .F. ) ;
#234786 = CARTESIAN_POINT ( 'NONE',  ( 23.24999999999999645, 67.17743825834548943, -93.77310748452437394 ) ) ;
#234787 = CARTESIAN_POINT ( 'NONE',  ( -18.59999999999999787, 14.61354176542825201, -235.9279552357344016 ) ) ;
#234788 = DIRECTION ( 'NONE',  ( 1.000000000000000000, 0.000000000000000000, -0.000000000000000000 ) ) ;
#234789 = B_SPLINE_CURVE_WITH_KNOTS ( 'NONE', 3,
 ( #192907, #211179, #11711, #14288, #213741, #250303 ),
 .UNSPECIFIED., .F., .F.,
 ( 4, 2, 4 ),
 ( 0.000000000000000000, 0.0001891491689349668738, 0.0003782983378699337476 ),
 .UNSPECIFIED. ) ;
#234790 = CIRCLE ( 'NONE', #9920, 0.1000000000000028644 ) ;
#234791 = LINE ( 'NONE', #237362, #4355 ) ;
#234792 = ORIENTED_EDGE ( 'NONE', *, *, #225232, .F. ) ;
#234793 = EDGE_CURVE ( 'NONE', #104735, #131734, #71099, .T. ) ;
#234795 = EDGE_CURVE ( 'NONE', #86831, #90426, #1476, .T. ) ;
#234794 = CARTESIAN_POINT ( 'NONE',  ( -15.52965525596987817, 66.62446189796402507, -120.6532316035334986 ) ) ;
#234796 = CARTESIAN_POINT ( 'NONE',  ( -21.14999999999999858, 64.25000000001263345, -196.7392418215462726 ) ) ;
#234797 = CIRCLE ( 'NONE', #1541, 0.2000000000000057288 ) ;
#234798 = ORIENTED_EDGE ( 'NONE', *, *, #227198, .F. ) ;
#234799 = AXIS2_PLACEMENT_3D ( 'NONE', #19616, #177425, #134390 ) ;
#234800 = CARTESIAN_POINT ( 'NONE',  ( -21.14999999999999858, 78.47509609352879068, -238.9045489380306435 ) ) ;
#234801 = CIRCLE ( 'NONE', #247246, 0.9000000000000014655 ) ;
#234802 = ADVANCED_FACE ( 'NONE', ( #232871 ), #216821, .T. ) ;
#234803 = CARTESIAN_POINT ( 'NONE',  ( 21.07933241753356768, 6.328645948379748809, 0.09337959041930479764 ) ) ;
#234804 = ORIENTED_EDGE ( 'NONE', *, *, #47686, .F. ) ;
#234805 = EDGE_LOOP ( 'NONE', ( #136200, #138723, #97361, #161797, #249047, #12951, #68839, #1966, #4931, #109269, #224373 ) ) ;
#234806 = DIRECTION ( 'NONE',  ( 1.000000000000000000, 0.000000000000000000, 0.000000000000000000 ) ) ;
#234807 = ORIENTED_EDGE ( 'NONE', *, *, #143009, .T. ) ;
#234808 = DIRECTION ( 'NONE',  ( 0.000000000000000000, 1.000000000000000000, 0.000000000000000000 ) ) ;
#234809 = ORIENTED_EDGE ( 'NONE', *, *, #178742, .T. ) ;
#234810 = DIRECTION ( 'NONE',  ( 1.000000000000000000, 1.394253735153569469E-16, 2.602809386958778209E-16 ) ) ;
#234811 = LINE ( 'NONE', #215248, #256270 ) ;
#234812 = FACE_OUTER_BOUND ( 'NONE', #181742, .T. ) ;
#234813 = CARTESIAN_POINT ( 'NONE',  ( 16.27683809663750125, 9.350000000011137402, -143.2500000000000284 ) ) ;
#234814 = EDGE_CURVE ( 'NONE', #128969, #138064, #38340, .T. ) ;
#234815 = AXIS2_PLACEMENT_3D ( 'NONE', #26976, #106449, #186018 ) ;
#234816 = AXIS2_PLACEMENT_3D ( 'NONE', #211416, #134416, #52314 ) ;
#234817 = SPHERICAL_SURFACE ( 'NONE', #58762, 0.1000000000000000056 ) ;
#234818 = CARTESIAN_POINT ( 'NONE',  ( 18.58725287972291440, -9.566626910680582796, -73.82250480576544760 ) ) ;
#234819 = CARTESIAN_POINT ( 'NONE',  ( -18.59999999999999787, -1.249999999988843369, -108.3004807544151191 ) ) ;
#234820 = TOROIDAL_SURFACE ( 'NONE', #230736, 0.2000000000000000111, 0.1000000000000000056 ) ;
#234821 = VERTEX_POINT ( 'NONE', #133738 ) ;
#234822 = DIRECTION ( 'NONE',  ( 0.000000000000000000, 0.000000000000000000, -1.000000000000000000 ) ) ;
#234823 = ORIENTED_EDGE ( 'NONE', *, *, #233397, .F. ) ;
#234827 = ORIENTED_EDGE ( 'NONE', *, *, #165292, .T. ) ;
#234826 =( BOUNDED_SURFACE ( )  B_SPLINE_SURFACE ( 3, 2, ( 
 ( #24766, #140833, #219065 ),
 ( #160426, #181264, #65133 ),
 ( #161699, #239942, #120017 ),
 ( #199546, #204634, #20910 ) ),
 .UNSPECIFIED., .F., .F., .T. ) 
 B_SPLINE_SURFACE_WITH_KNOTS ( ( 4, 4 ),
 ( 3, 3 ),
 ( 0.0008258556059633754111, 0.0009616864997633037737 ),
 ( 0.000000000000000000, 1.000000000000000000 ),
 .UNSPECIFIED. ) 
 GEOMETRIC_REPRESENTATION_ITEM ( )  RATIONAL_B_SPLINE_SURFACE ( (
 ( 1.000000000000000000, 0.9152888060719425178, 1.000000000000000000),
 ( 1.000000000000000000, 0.9327727094138008601, 1.000000000000000000),
 ( 1.000000000000000000, 0.9369023509258477267, 1.000000000000000000),
 ( 1.000000000000000000, 0.9246339933864470284, 1.000000000000000000) ) ) 
 REPRESENTATION_ITEM ( '' )  SURFACE ( )  );
#234825 = CARTESIAN_POINT ( 'NONE',  ( -18.49499033040906326, 85.43814877175627487, -62.32495425860083316 ) ) ;
#234824 = DIRECTION ( 'NONE',  ( 1.000000000000000000, 0.000000000000000000, 0.000000000000000000 ) ) ;
#234828 = ORIENTED_EDGE ( 'NONE', *, *, #51005, .T. ) ;
#234829 = CYLINDRICAL_SURFACE ( 'NONE', #189025, 0.1000000000000055844 ) ;
#234830 = DIRECTION ( 'NONE',  ( 0.000000000000000000, -6.982962677686266711E-15, 1.000000000000000000 ) ) ;
#234831 = CIRCLE ( 'NONE', #138914, 0.09999999999998898659 ) ;
#234832 = CYLINDRICAL_SURFACE ( 'NONE', #136000, 0.09999999999998898659 ) ;
#234833 = ADVANCED_FACE ( 'NONE', ( #116749 ), #219692, .T. ) ;
#234834 = CARTESIAN_POINT ( 'NONE',  ( -21.00857864376268935, 64.40000000001208491, -129.5949042542488314 ) ) ;
#234835 = AXIS2_PLACEMENT_3D ( 'NONE', #59810, #58536, #156412 ) ;
#234836 = VERTEX_POINT ( 'NONE', #76318 ) ;
#234838 = ORIENTED_EDGE ( 'NONE', *, *, #117869, .T. ) ;
#234837 = LINE ( 'NONE', #113602, #117801 ) ;
#234839 = CIRCLE ( 'NONE', #151660, 0.09999999999999983902 ) ;
#234840 = EDGE_CURVE ( 'NONE', #56815, #197037, #42356, .T. ) ;
#234842 = DIRECTION ( 'NONE',  ( -1.000000000000000000, -0.000000000000000000, -0.000000000000000000 ) ) ;
#234841 = DIRECTION ( 'NONE',  ( -1.000000000000000000, -0.000000000000000000, 0.000000000000000000 ) ) ;
#234843 = EDGE_CURVE ( 'NONE', #143156, #191501, #254755, .T. ) ;
#234845 = ORIENTED_EDGE ( 'NONE', *, *, #204511, .T. ) ;
#234844 = DIRECTION ( 'NONE',  ( 0.000000000000000000, -0.2617529984165033463, -0.9651348961777157509 ) ) ;
#234846 = AXIS2_PLACEMENT_3D ( 'NONE', #30996, #28437, #29710 ) ;
#234847 = AXIS2_PLACEMENT_3D ( 'NONE', #188883, #31132, #87189 ) ;
#234848 = AXIS2_PLACEMENT_3D ( 'NONE', #40639, #187502, #64010 ) ;
#234849 = ORIENTED_EDGE ( 'NONE', *, *, #14740, .F. ) ;
#234850 = AXIS2_PLACEMENT_3D ( 'NONE', #21921, #180998, #3616 ) ;
#234852 = ADVANCED_FACE ( 'NONE', ( #61920 ), #180583, .T. ) ;
#234851 = CARTESIAN_POINT ( 'NONE',  ( 18.39999999999998082, 40.40989152675300033, -235.2989281452919954 ) ) ;
#234853 = DIRECTION ( 'NONE',  ( 0.000000000000000000, 0.000000000000000000, 1.000000000000000000 ) ) ;
#234855 = EDGE_CURVE ( 'NONE', #155390, #143721, #82725, .T. ) ;
#234854 = ORIENTED_EDGE ( 'NONE', *, *, #253371, .T. ) ;
#234856 = DIRECTION ( 'NONE',  ( -1.000000000000000000, 0.000000000000000000, 0.000000000000000000 ) ) ;
#234857 = ORIENTED_EDGE ( 'NONE', *, *, #99118, .T. ) ;
#234858 = FACE_OUTER_BOUND ( 'NONE', #130541, .T. ) ;
#234859 = FACE_OUTER_BOUND ( 'NONE', #174612, .T. ) ;
#234861 = EDGE_CURVE ( 'NONE', #181985, #132235, #84059, .T. ) ;
#234860 = CIRCLE ( 'NONE', #226442, 0.1000000000000009492 ) ;
#234862 = ORIENTED_EDGE ( 'NONE', *, *, #257406, .T. ) ;
#234863 = DIRECTION ( 'NONE',  ( 0.000000000000000000, 0.9126074666064696306, 0.4088369013361213278 ) ) ;
#234864 = CIRCLE ( 'NONE', #134863, 4.049999999999998934 ) ;
#234865 = EDGE_CURVE ( 'NONE', #171702, #15616, #198852, .T. ) ;
#234866 = CARTESIAN_POINT ( 'NONE',  ( -18.59999999999999787, 0.000000000000000000, 0.000000000000000000 ) ) ;
#234867 = EDGE_CURVE ( 'NONE', #143593, #190389, #75756, .T. ) ;
#234868 = EDGE_CURVE ( 'NONE', #48902, #190074, #46687, .T. ) ;
#234869 = AXIS2_PLACEMENT_3D ( 'NONE', #34488, #54017, #210533 ) ;
#234870 = AXIS2_PLACEMENT_3D ( 'NONE', #125500, #146333, #148932 ) ;
#234871 = ORIENTED_EDGE ( 'NONE', *, *, #187792, .T. ) ;
#234872 = AXIS2_PLACEMENT_3D ( 'NONE', #253633, #158440, #234079 ) ;
#234873 = EDGE_LOOP ( 'NONE', ( #182337, #73268, #165046, #92217 ) ) ;
#234874 = CARTESIAN_POINT ( 'NONE',  ( 20.22894356738334309, 18.79873783012739352, -229.4580867665647759 ) ) ;
#234875 = ORIENTED_EDGE ( 'NONE', *, *, #69030, .F. ) ;
#234876 = ADVANCED_FACE ( 'NONE', ( #78882 ), #200149, .T. ) ;
#234877 = ORIENTED_EDGE ( 'NONE', *, *, #198020, .F. ) ;
#234879 = VERTEX_POINT ( 'NONE', #627 ) ;
#234878 = CARTESIAN_POINT ( 'NONE',  ( 20.85000000000000142, 77.83585931145526615, -58.01866831572577610 ) ) ;
#234880 =( BOUNDED_SURFACE ( )  B_SPLINE_SURFACE ( 3, 2, ( 
 ( #70306, #74161, #153719 ),
 ( #148534, #50678, #248924 ),
 ( #209790, #31193, #110681 ),
 ( #190228, #11601, #257835 ),
 ( #214911, #174566, #235750 ),
 ( #196625, #177103, #79231 ) ),
 .UNSPECIFIED., .F., .F., .F. ) 
 B_SPLINE_SURFACE_WITH_KNOTS ( ( 4, 2, 4 ),
 ( 3, 3 ),
 ( -1.776356839400250465E-15, 0.7853981633974468357, 1.570796326794895448 ),
 ( 0.000000000000000000, 1.000000000000000000 ),
 .UNSPECIFIED. ) 
 GEOMETRIC_REPRESENTATION_ITEM ( )  RATIONAL_B_SPLINE_SURFACE ( (
 ( 1.000000000000000000, 0.4999999999999439337, 1.000000000000000000),
 ( 1.000000000000000000, 0.4993418825329671851, 1.000000000000000000),
 ( 1.000000000000000000, 0.5278258667062272202, 1.000000000000000000),
 ( 1.000000000000000000, 0.6092287576688484307, 1.000000000000000000),
 ( 1.000000000000000000, 0.6611148371785092737, 1.000000000000000000),
 ( 1.000000000000000000, 0.7071067811866070807, 1.000000000000000000) ) ) 
 REPRESENTATION_ITEM ( '' )  SURFACE ( )  );
#234882 = ADVANCED_FACE ( 'NONE', ( #203990 ), #24104, .T. ) ;
#234881 = VERTEX_POINT ( 'NONE', #183162 ) ;
#234883 = LINE ( 'NONE', #14567, #68458 ) ;
#234885 = EDGE_LOOP ( 'NONE', ( #39691, #64623, #53922, #159969 ) ) ;
#234884 = EDGE_CURVE ( 'NONE', #103754, #81962, #250700, .T. ) ;
#234888 = ORIENTED_EDGE ( 'NONE', *, *, #65070, .T. ) ;
#234887 = ORIENTED_EDGE ( 'NONE', *, *, #195618, .T. ) ;
#234886 = DIRECTION ( 'NONE',  ( 0.000000000000000000, 0.2128009952263596460, -0.9770955615653317272 ) ) ;
#234889 = EDGE_CURVE ( 'NONE', #170466, #175208, #140148, .T. ) ;
#234890 = ORIENTED_EDGE ( 'NONE', *, *, #170152, .T. ) ;
#234891 = TOROIDAL_SURFACE ( 'NONE', #172389, 0.2000000000000000111, 0.1000000000000000056 ) ;
#234892 = CARTESIAN_POINT ( 'NONE',  ( -23.25000000000000000, 2.600000000000000089, -13.22462192276210224 ) ) ;
#234893 = AXIS2_PLACEMENT_3D ( 'NONE', #215859, #191216, #210748 ) ;
#234894 = CIRCLE ( 'NONE', #72401, 0.09999999999999642508 ) ;
#234895 = DIRECTION ( 'NONE',  ( 0.000000000000000000, 0.000000000000000000, -1.000000000000000000 ) ) ;
#234896 = DIRECTION ( 'NONE',  ( -5.603264701231743991E-32, 1.897661533703519897E-16, -1.000000000000000000 ) ) ;
#234897 = VERTEX_POINT ( 'NONE', #123181 ) ;
#234898 = DIRECTION ( 'NONE',  ( 1.000000000000000000, 0.000000000000000000, -0.000000000000000000 ) ) ;
#234900 = VERTEX_POINT ( 'NONE', #81447 ) ;
#234899 = DIRECTION ( 'NONE',  ( -1.000000000000000000, 0.000000000000000000, 0.000000000000000000 ) ) ;
#234901 = CARTESIAN_POINT ( 'NONE',  ( -20.94999999999999929, 71.99422445362657186, -246.4870034924427671 ) ) ;
#234902 = VERTEX_POINT ( 'NONE', #159739 ) ;
#234903 = EDGE_CURVE ( 'NONE', #246385, #67031, #163595, .T. ) ;
#234904 = ORIENTED_EDGE ( 'NONE', *, *, #195691, .F. ) ;
#234905 = EDGE_CURVE ( 'NONE', #70426, #172562, #218399, .T. ) ;
#234906 = CARTESIAN_POINT ( 'NONE',  ( 22.00356870070926973, 7.976845382617315661E-12, -160.2457576382639672 ) ) ;
#234907 = DIRECTION ( 'NONE',  ( 1.000000000000000000, 0.000000000000000000, 0.000000000000000000 ) ) ;
#234908 = ORIENTED_EDGE ( 'NONE', *, *, #214883, .F. ) ;
#234909 = EDGE_LOOP ( 'NONE', ( #134498, #66574, #59521, #95661, #200267, #29882 ) ) ;
#234910 = CARTESIAN_POINT ( 'NONE',  ( 17.23472005113827876, 10.30788195451192379, -78.45342313993134553 ) ) ;
#234911 = DIRECTION ( 'NONE',  ( 0.000000000000000000, 0.000000000000000000, 1.000000000000000000 ) ) ;
#234913 = EDGE_LOOP ( 'NONE', ( #56788, #242264, #46624, #707 ) ) ;
#234912 = EDGE_LOOP ( 'NONE', ( #194595, #138000, #90748, #201644 ) ) ;
#234914 = CIRCLE ( 'NONE', #84839, 0.1999999999999987899 ) ;
#234915 = EDGE_LOOP ( 'NONE', ( #19597, #15013, #77601, #110513 ) ) ;
#234916 = FACE_OUTER_BOUND ( 'NONE', #246710, .T. ) ;
#234917 = ORIENTED_EDGE ( 'NONE', *, *, #167214, .F. ) ;
#234918 = VERTEX_POINT ( 'NONE', #141446 ) ;
#234919 = CARTESIAN_POINT ( 'NONE',  ( 18.50000000000000000, 86.35479209693686187, -42.26656650145049099 ) ) ;
#234920 = ORIENTED_EDGE ( 'NONE', *, *, #56844, .F. ) ;
#234921 = DIRECTION ( 'NONE',  ( 0.000000000000000000, 7.147358527629759053E-15, -1.000000000000000000 ) ) ;
#234923 = CARTESIAN_POINT ( 'NONE',  ( -23.25000000000000000, 62.12679871018154643, -248.6611778639222337 ) ) ;
#234922 = DIRECTION ( 'NONE',  ( 1.000000000000000000, 0.000000000000000000, 0.000000000000000000 ) ) ;
#234924 = EDGE_LOOP ( 'NONE', ( #72969, #233010, #63846, #36424 ) ) ;
#234925 = ORIENTED_EDGE ( 'NONE', *, *, #2924, .T. ) ;
#234927 = EDGE_CURVE ( 'NONE', #49697, #994, #219478, .T. ) ;
#234926 = DIRECTION ( 'NONE',  ( 0.000000000000000000, 0.4999999999999608646, 0.8660254037844612451 ) ) ;
#234928 = ORIENTED_EDGE ( 'NONE', *, *, #60521, .T. ) ;
#234929 = EDGE_CURVE ( 'NONE', #60123, #139562, #204910, .T. ) ;
#234930 = CIRCLE ( 'NONE', #218322, 0.09999999999998898659 ) ;
#234931 = CIRCLE ( 'NONE', #122515, 0.1000000000000016709 ) ;
#234932 = VECTOR ( 'NONE', #208353, 1000.000000000000000 ) ;
#234933 = DIRECTION ( 'NONE',  ( 0.000000000000000000, 0.000000000000000000, 1.000000000000000000 ) ) ;
#234934 = ORIENTED_EDGE ( 'NONE', *, *, #20973, .F. ) ;
#234935 = EDGE_LOOP ( 'NONE', ( #218050, #183917, #229268, #222484 ) ) ;
#234936 = CARTESIAN_POINT ( 'NONE',  ( -20.54999999999999716, 7.150000000011155876, -179.8499999999999943 ) ) ;
#234938 = ORIENTED_EDGE ( 'NONE', *, *, #104048, .F. ) ;
#234937 = CARTESIAN_POINT ( 'NONE',  ( 18.52165635395168053, 85.48115071129463161, -162.9982699016619847 ) ) ;
#234939 = CARTESIAN_POINT ( 'NONE',  ( -18.59999999999999787, -1.835859311432481045, -212.5044391687984842 ) ) ;
#234940 = EDGE_LOOP ( 'NONE', ( #144080, #119472 ) ) ;
#234941 = CARTESIAN_POINT ( 'NONE',  ( 20.85000000000000142, -11.64999999998883595, -134.0000000000000284 ) ) ;
#234942 = DIRECTION ( 'NONE',  ( -1.836970198721029934E-16, 1.000000000000000000, 0.000000000000000000 ) ) ;
#234943 = DIRECTION ( 'NONE',  ( 1.224646799147353207E-16, 1.000000000000000000, 0.000000000000000000 ) ) ;
#234944 = DIRECTION ( 'NONE',  ( 0.000000000000000000, 0.9651348961777158619, -0.2617529984165028467 ) ) ;
#234945 = DIRECTION ( 'NONE',  ( 0.000000000000000000, 0.000000000000000000, -1.000000000000000000 ) ) ;
#234946 = FACE_OUTER_BOUND ( 'NONE', #150153, .T. ) ;
#234947 = DIRECTION ( 'NONE',  ( 0.000000000000000000, -0.9126074666063781482, -0.4088369013363255533 ) ) ;
#234948 = AXIS2_PLACEMENT_3D ( 'NONE', #86284, #124174, #160751 ) ;
#234949 = CARTESIAN_POINT ( 'NONE',  ( -18.40000000000000213, 33.90347449973612015, -235.0533218592931348 ) ) ;
#234950 = FACE_OUTER_BOUND ( 'NONE', #254381, .T. ) ;
#234951 = ADVANCED_FACE ( 'NONE', ( #145291 ), #127028, .F. ) ;
#234952 = AXIS2_PLACEMENT_3D ( 'NONE', #6020, #144240, #124707 ) ;
#234953 = ORIENTED_EDGE ( 'NONE', *, *, #218461, .T. ) ;
#234954 = AXIS2_PLACEMENT_3D ( 'NONE', #185452, #6808, #247981 ) ;
#234955 = AXIS2_PLACEMENT_3D ( 'NONE', #158891, #20656, #169166 ) ;
#234957 = ORIENTED_EDGE ( 'NONE', *, *, #211235, .F. ) ;
#234956 = EDGE_LOOP ( 'NONE', ( #247916, #210202, #17387, #20876 ) ) ;
#234959 = EDGE_LOOP ( 'NONE', ( #150620, #95976, #171111, #97942 ) ) ;
#234958 = VECTOR ( 'NONE', #170315, 1000.000000000000000 ) ;
#234960 = CARTESIAN_POINT ( 'NONE',  ( -21.12757541349819590, 0.005161215820883788274, -94.02661942874847512 ) ) ;
#234961 = DIRECTION ( 'NONE',  ( 0.000000000000000000, 0.000000000000000000, -1.000000000000000000 ) ) ;
#234963 = FACE_OUTER_BOUND ( 'NONE', #213201, .T. ) ;
#234962 = CARTESIAN_POINT ( 'NONE',  ( 23.14999999999999503, 11.75000000001116263, -146.1500000000000341 ) ) ;
#234964 = EDGE_LOOP ( 'NONE', ( #71173, #195583, #186899, #27752 ) ) ;
#234965 = AXIS2_PLACEMENT_3D ( 'NONE', #29130, #146437, #143877 ) ;
#234966 = DIRECTION ( 'NONE',  ( 0.000000000000000000, -0.01283462868042125823, -0.9999176327611367654 ) ) ;
#234967 = AXIS2_PLACEMENT_3D ( 'NONE', #19581, #220351, #62554 ) ;
#234969 = VECTOR ( 'NONE', #107475, 1000.000000000000000 ) ;
#234968 = DIRECTION ( 'NONE',  ( 1.000000000000000000, 7.136802563874199107E-16, 1.554319503706929991E-16 ) ) ;
#234970 = CARTESIAN_POINT ( 'NONE',  ( -16.87487986503753845, 9.950007555096753720, -180.1499747396866837 ) ) ;
#234971 = DIRECTION ( 'NONE',  ( 0.000000000000000000, -1.000000000000000000, -6.860497997771532351E-15 ) ) ;
#234973 = ORIENTED_EDGE ( 'NONE', *, *, #195377, .F. ) ;
#234972 = AXIS2_PLACEMENT_3D ( 'NONE', #241564, #81185, #199892 ) ;
#234974 = ORIENTED_EDGE ( 'NONE', *, *, #94096, .T. ) ;
#234975 = DIRECTION ( 'NONE',  ( -1.000000000000000000, -1.387778780781454006E-13, 0.000000000000000000 ) ) ;
#234976 = CARTESIAN_POINT ( 'NONE',  ( -11.60000000000000320, -8.279289321881348584, 11.02928932188134503 ) ) ;
#234977 = VECTOR ( 'NONE', #34757, 1000.000000000000000 ) ;
#234978 = ORIENTED_EDGE ( 'NONE', *, *, #179441, .T. ) ;
#234979 = FACE_OUTER_BOUND ( 'NONE', #93480, .T. ) ;
#234980 = CARTESIAN_POINT ( 'NONE',  ( 20.94999999999999929, 5.400000000011154988, -54.59473398108690390 ) ) ;
#234981 = DIRECTION ( 'NONE',  ( -0.000000000000000000, -1.000000000000000000, 0.000000000000000000 ) ) ;
#234982 = CARTESIAN_POINT ( 'NONE',  ( 21.05000000000000071, 63.99342642423710714, -222.3880800784493772 ) ) ;
#234983 = CIRCLE ( 'NONE', #151613, 11.74999999999999645 ) ;
#234984 = CARTESIAN_POINT ( 'NONE',  ( -20.54999999999999716, 85.40000000001188596, -93.12913836187179584 ) ) ;
#234985 = ORIENTED_EDGE ( 'NONE', *, *, #152304, .T. ) ;
#234986 = CARTESIAN_POINT ( 'NONE',  ( -21.14999999999999858, 30.90801580390628800, -252.0203440857197279 ) ) ;
#234988 = EDGE_CURVE ( 'NONE', #159239, #81429, #107463, .T. ) ;
#234987 = CARTESIAN_POINT ( 'NONE',  ( 20.94999999999999929, 77.83585931145498193, -24.51866831572578320 ) ) ;
#234989 = DIRECTION ( 'NONE',  ( 0.000000000000000000, 0.9126074666063545004, 0.4088369013363783999 ) ) ;
#234990 = VECTOR ( 'NONE', #157485, 1000.000000000000000 ) ;
#234992 = CARTESIAN_POINT ( 'NONE',  ( -22.39999999999999858, 64.25000000001237765, -169.9231074845244507 ) ) ;
#234991 = FACE_OUTER_BOUND ( 'NONE', #132950, .T. ) ;
#234993 = LINE ( 'NONE', #195878, #133139 ) ;
#234994 = EDGE_CURVE ( 'NONE', #71034, #175321, #9649, .T. ) ;
#234995 = CARTESIAN_POINT ( 'NONE',  ( 20.94999999999999929, 76.00000000001126921, -203.5231074845248997 ) ) ;
#234996 = CARTESIAN_POINT ( 'NONE',  ( 21.05000000000000071, 75.90220970870291239, -75.78092209500044873 ) ) ;
#234997 = CARTESIAN_POINT ( 'NONE',  ( 18.79999999999999716, 7.973296578895943121, 1.410778198689824903 ) ) ;
#234998 = ORIENTED_EDGE ( 'NONE', *, *, #158035, .F. ) ;
#234999 = ORIENTED_EDGE ( 'NONE', *, *, #186001, .T. ) ;
#235000 = EDGE_CURVE ( 'NONE', #58156, #81962, #46198, .T. ) ;
#235001 = PLANE ( 'NONE',  #157049 ) ;
#235002 = ORIENTED_EDGE ( 'NONE', *, *, #14134, .T. ) ;
#235003 = ADVANCED_FACE ( 'NONE', ( #205263 ), #89177, .T. ) ;
#235004 = DIRECTION ( 'NONE',  ( -1.000000000000000000, 0.000000000000000000, -0.000000000000000000 ) ) ;
#235005 = VERTEX_POINT ( 'NONE', #125735 ) ;
#235006 = CIRCLE ( 'NONE', #176748, 0.09999999999999939493 ) ;
#235007 = CIRCLE ( 'NONE', #214155, 3.900000000000000799 ) ;
#235008 = ADVANCED_FACE ( 'NONE', ( #70940 ), #90456, .F. ) ;
#235009 = AXIS2_PLACEMENT_3D ( 'NONE', #106472, #89491, #169086 ) ;
#235010 = CARTESIAN_POINT ( 'NONE',  ( -23.25000000000000000, 71.75000000001205080, -124.3731074845243256 ) ) ;
#235011 = VERTEX_POINT ( 'NONE', #166192 ) ;
#235012 = CARTESIAN_POINT ( 'NONE',  ( 21.14999999999999858, 1.115600667400684642E-11, -160.9593430482987344 ) ) ;
#235013 = CARTESIAN_POINT ( 'NONE',  ( -14.22969084473441370, 9.456007326080463571, -51.98863349414677515 ) ) ;
#235014 = LINE ( 'NONE', #112506, #165219 ) ;
#235015 = AXIS2_PLACEMENT_3D ( 'NONE', #221651, #222943, #144690 ) ;
#235016 = AXIS2_PLACEMENT_3D ( 'NONE', #67228, #144180, #244575 ) ;
#235017 = CYLINDRICAL_SURFACE ( 'NONE', #95410, 0.09999999999999939493 ) ;
#235019 = VERTEX_POINT ( 'NONE', #26667 ) ;
#235018 = DIRECTION ( 'NONE',  ( 0.000000000000000000, -6.938893903907222067E-15, 1.000000000000000000 ) ) ;
#235021 = CARTESIAN_POINT ( 'NONE',  ( 19.96984138294323330, 11.75000000001115197, -192.2245720712021466 ) ) ;
#235020 = DIRECTION ( 'NONE',  ( 3.616040088954497272E-32, -1.224646799147352961E-16, 1.000000000000000000 ) ) ;
#235022 = ADVANCED_FACE ( 'NONE', ( #128326 ), #171632, .T. ) ;
#235023 = CARTESIAN_POINT ( 'NONE',  ( -16.81744102076749314, 66.05000000001261640, -190.8731074845244393 ) ) ;
#235024 = CARTESIAN_POINT ( 'NONE',  ( 20.90000000000000213, 11.61130914238355771, -1.800000000000000044 ) ) ;
#235025 = AXIS2_PLACEMENT_3D ( 'NONE', #146528, #85255, #188247 ) ;
#235026 = CARTESIAN_POINT ( 'NONE',  ( 18.49999999999999645, 68.22930980752001062, -227.7331931781284879 ) ) ;
#235027 = LINE ( 'NONE', #152952, #249964 ) ;
#235028 = ORIENTED_EDGE ( 'NONE', *, *, #194827, .T. ) ;
#235029 = CIRCLE ( 'NONE', #247494, 0.5000000000000004441 ) ;
#235030 = SHAPE_REPRESENTATION_RELATIONSHIP ( 'NONE' , 'NONE' ,  #223420, #76170 ) ;
#235031 = LINE ( 'NONE', #257099, #83526 ) ;
#235032 = TOROIDAL_SURFACE ( 'NONE', #205985, 0.2000000000000000111, 0.1000000000000000056 ) ;
#235033 = VECTOR ( 'NONE', #56605, 1000.000000000000000 ) ;
#235034 = ORIENTED_EDGE ( 'NONE', *, *, #202132, .T. ) ;
#235035 = FACE_OUTER_BOUND ( 'NONE', #178760, .T. ) ;
#235036 = ORIENTED_EDGE ( 'NONE', *, *, #147901, .T. ) ;
#235037 = VECTOR ( 'NONE', #161121, 1000.000000000000000 ) ;
#235038 = LINE ( 'NONE', #14726, #67910 ) ;
#235039 = CARTESIAN_POINT ( 'NONE',  ( -16.90128866880176162, 9.953795777202955719, -20.86267618338863983 ) ) ;
#235040 = CYLINDRICAL_SURFACE ( 'NONE', #182648, 11.75000000000001066 ) ;
#235041 = EDGE_LOOP ( 'NONE', ( #143199, #245339, #240715, #59766 ) ) ;
#235042 = CIRCLE ( 'NONE', #122634, 0.1000000000000033223 ) ;
#235043 = EDGE_LOOP ( 'NONE', ( #207092, #148615, #30519 ) ) ;
#235044 = CARTESIAN_POINT ( 'NONE',  ( 18.59999999999999432, 74.83729825007408465, -128.4231074845243086 ) ) ;
#235046 = AXIS2_PLACEMENT_3D ( 'NONE', #22947, #159883, #222366 ) ;
#235045 = CARTESIAN_POINT ( 'NONE',  ( 20.95159278453404283, 10.50942287431401390, -207.3947732279067395 ) ) ;
#235047 = CARTESIAN_POINT ( 'NONE',  ( -16.82055514392382634, 63.07871787671091823, -213.1534853438195398 ) ) ;
#235048 = DIRECTION ( 'NONE',  ( 0.000000000000000000, 1.000000000000000000, 0.000000000000000000 ) ) ;
#235050 = CARTESIAN_POINT ( 'NONE',  ( 18.49999999999998934, 6.550000000011156231, -43.51702717044002355 ) ) ;
#235049 = FACE_OUTER_BOUND ( 'NONE', #206093, .T. ) ;
#235051 = LINE ( 'NONE', #56383, #203399 ) ;
#235052 = CARTESIAN_POINT ( 'NONE',  ( -20.54999999999999716, 1.115600667400684642E-11, -33.50000000000000000 ) ) ;
#235053 = DIRECTION ( 'NONE',  ( 1.000000000000000000, 0.000000000000000000, 0.000000000000000000 ) ) ;
#235054 = EDGE_LOOP ( 'NONE', ( #123958, #68503, #53418, #37750 ) ) ;
#235055 = CARTESIAN_POINT ( 'NONE',  ( 18.39999999999997371, 16.37079970714665933, -222.2530670965321349 ) ) ;
#235056 = CIRCLE ( 'NONE', #39449, 0.1000000000000013933 ) ;
#235057 = EDGE_CURVE ( 'NONE', #200485, #34176, #246967, .T. ) ;
#235059 = EDGE_LOOP ( 'NONE', ( #57472, #226887, #80514, #74590 ) ) ;
#235058 = DIRECTION ( 'NONE',  ( 1.000000000000000000, 0.000000000000000000, 0.000000000000000000 ) ) ;
#235060 = AXIS2_PLACEMENT_3D ( 'NONE', #74760, #118990, #198511 ) ;
#235061 = CARTESIAN_POINT ( 'NONE',  ( -20.94999999999999929, 28.37802281961254636, -258.4449340416662722 ) ) ;
#235062 = DIRECTION ( 'NONE',  ( 0.000000000000000000, 0.000000000000000000, -1.000000000000000000 ) ) ;
#235064 = DIRECTION ( 'NONE',  ( 1.000000000000000000, -0.000000000000000000, -0.000000000000000000 ) ) ;
#235063 = DIRECTION ( 'NONE',  ( 1.000000000000000000, -0.000000000000000000, -0.000000000000000000 ) ) ;
#235066 = EDGE_LOOP ( 'NONE', ( #130064, #220403, #195090, #170725 ) ) ;
#235065 = CARTESIAN_POINT ( 'NONE',  ( 20.94999999999999929, 18.51199663233068193, -231.2535697180530292 ) ) ;
#235068 = DIRECTION ( 'NONE',  ( -0.000000000000000000, 0.000000000000000000, -1.000000000000000000 ) ) ;
#235067 = PLANE ( 'NONE',  #134959 ) ;
#235069 = DIRECTION ( 'NONE',  ( -1.000000000000000000, -0.000000000000000000, -0.000000000000000000 ) ) ;
#235070 = DIRECTION ( 'NONE',  ( 0.000000000000000000, 0.000000000000000000, -1.000000000000000000 ) ) ;
#235071 = LINE ( 'NONE', #139792, #149285 ) ;
#235073 = ADVANCED_FACE ( 'NONE', ( #149183 ), #50770, .F. ) ;
#235072 = CARTESIAN_POINT ( 'NONE',  ( -18.52328366898032996, 85.64232108905312657, -96.30828814695416895 ) ) ;
#235074 = VERTEX_POINT ( 'NONE', #27965 ) ;
#235075 = CARTESIAN_POINT ( 'NONE',  ( 18.42595409746876101, -7.792936377315665908, -209.8606553024481798 ) ) ;
#235076 = ORIENTED_EDGE ( 'NONE', *, *, #90412, .F. ) ;
#235077 = EDGE_CURVE ( 'NONE', #5675, #8746, #168779, .T. ) ;
#235078 = ADVANCED_FACE ( 'NONE', ( #147887 ), #228718, .F. ) ;
#235079 = CARTESIAN_POINT ( 'NONE',  ( 22.40000000000010516, 76.00000000001371347, -215.2735403769832487 ) ) ;
#235080 = VERTEX_POINT ( 'NONE', #129603 ) ;
#235081 = DIRECTION ( 'NONE',  ( 0.000000000000000000, -1.000000000000000000, 0.000000000000000000 ) ) ;
#235082 = CIRCLE ( 'NONE', #164343, 0.09999999999999911737 ) ;
#235083 = ORIENTED_EDGE ( 'NONE', *, *, #190761, .T. ) ;
#235084 = CARTESIAN_POINT ( 'NONE',  ( -21.07928932188134041, 6.328516656404449492, -167.4011048543455615 ) ) ;
#235085 = DIRECTION ( 'NONE',  ( 1.000000000000000000, 2.952720810173289112E-16, -0.000000000000000000 ) ) ;
#235086 = AXIS2_PLACEMENT_3D ( 'NONE', #235052, #215472, #58938 ) ;
#235087 = DIRECTION ( 'NONE',  ( 0.000000000000000000, 0.000000000000000000, 1.000000000000000000 ) ) ;
#235088 = ORIENTED_EDGE ( 'NONE', *, *, #84347, .T. ) ;
#235089 = EDGE_CURVE ( 'NONE', #34172, #40483, #30520, .T. ) ;
#235090 = EDGE_CURVE ( 'NONE', #181633, #102764, #229980, .T. ) ;
#235091 = CARTESIAN_POINT ( 'NONE',  ( -21.95218792049438861, -1.435727727154726185, -193.9423655747830537 ) ) ;
#235092 = DIRECTION ( 'NONE',  ( 0.000000000000000000, 0.000000000000000000, -1.000000000000000000 ) ) ;
#235093 = CARTESIAN_POINT ( 'NONE',  ( -22.39999999999999858, 31.98723526783714988, -238.8784020251475511 ) ) ;
#235094 = CARTESIAN_POINT ( 'NONE',  ( -16.92507428761699728, 60.95595224120684463, -220.9805406349763075 ) ) ;
#235095 = B_SPLINE_CURVE_WITH_KNOTS ( 'NONE', 3,
 ( #83440, #87309, #144714, #41806, #84714, #161752, #164309 ),
 .UNSPECIFIED., .F., .F.,
 ( 4, 3, 4 ),
 ( 0.000000000000000000, 4.520325912680675723E-05, 5.794988040901448781E-05 ),
 .UNSPECIFIED. ) ;
#235096 = ORIENTED_EDGE ( 'NONE', *, *, #197262, .F. ) ;
#235097 = FACE_OUTER_BOUND ( 'NONE', #82137, .T. ) ;
#235098 = ORIENTED_EDGE ( 'NONE', *, *, #92860, .F. ) ;
#235100 = ORIENTED_EDGE ( 'NONE', *, *, #12814, .F. ) ;
#235099 = LINE ( 'NONE', #16074, #60685 ) ;
#235101 = ORIENTED_EDGE ( 'NONE', *, *, #211156, .T. ) ;
#235102 = AXIS2_PLACEMENT_3D ( 'NONE', #200490, #145310, #25399 ) ;
#235103 = DIRECTION ( 'NONE',  ( 2.978066053179067751E-16, -1.000000000000000000, 0.000000000000000000 ) ) ;
#235104 = CARTESIAN_POINT ( 'NONE',  ( 12.84233041328155878, 66.58946139148369525, -188.0904194873834854 ) ) ;
#235105 = DIRECTION ( 'NONE',  ( 1.000000000000000000, 0.000000000000000000, 0.000000000000000000 ) ) ;
#235106 = EDGE_CURVE ( 'NONE', #70695, #214666, #134001, .T. ) ;
#235107 = FACE_OUTER_BOUND ( 'NONE', #230042, .T. ) ;
#235108 = VERTEX_POINT ( 'NONE', #86586 ) ;
#235109 = EDGE_CURVE ( 'NONE', #134581, #39898, #242331, .T. ) ;
#235110 = EDGE_CURVE ( 'NONE', #61026, #183417, #4979, .T. ) ;
#235111 = CARTESIAN_POINT ( 'NONE',  ( -16.92989143108098560, 9.950000000011138823, -146.8824838747567298 ) ) ;
#235112 = FACE_OUTER_BOUND ( 'NONE', #127499, .T. ) ;
#235113 = ORIENTED_EDGE ( 'NONE', *, *, #140851, .F. ) ;
#235115 = ORIENTED_EDGE ( 'NONE', *, *, #205032, .T. ) ;
#235114 = DIRECTION ( 'NONE',  ( 0.000000000000000000, 8.673617379884087537E-15, -1.000000000000000000 ) ) ;
#235116 = DIRECTION ( 'NONE',  ( 1.000000000000000000, 7.304098846218134667E-16, 4.639676173203993355E-30 ) ) ;
#235118 = AXIS2_PLACEMENT_3D ( 'NONE', #72938, #228136, #49490 ) ;
#235117 = CARTESIAN_POINT ( 'NONE',  ( -16.88783316861809780, 9.950000000011137047, -79.75226404197984209 ) ) ;
#235119 = AXIS2_PLACEMENT_3D ( 'NONE', #101984, #62888, #223233 ) ;
#235120 = AXIS2_PLACEMENT_3D ( 'NONE', #87122, #183683, #144527 ) ;
#235121 = VECTOR ( 'NONE', #223533, 1000.000000000000000 ) ;
#235122 = DIRECTION ( 'NONE',  ( 1.000000000000000000, 0.000000000000000000, 0.000000000000000000 ) ) ;
#235123 = ORIENTED_EDGE ( 'NONE', *, *, #148055, .F. ) ;
#235124 = CARTESIAN_POINT ( 'NONE',  ( 20.94999999999999929, 69.15387683765983695, -166.2853812176745691 ) ) ;
#235125 = ADVANCED_FACE ( 'NONE', ( #252104 ), #233838, .F. ) ;
#235126 = CARTESIAN_POINT ( 'NONE',  ( -23.25000000000000000, -11.64999999998884483, -164.5000000000000000 ) ) ;
#235127 = CARTESIAN_POINT ( 'NONE',  ( 11.60000000000000142, -11.65000000000000036, 12.30000000000000426 ) ) ;
#235128 = ADVANCED_FACE ( 'NONE', ( #36954 ), #116464, .F. ) ;
#235129 = AXIS2_PLACEMENT_3D ( 'NONE', #28655, #70329, #229380 ) ;
#235130 = AXIS2_PLACEMENT_3D ( 'NONE', #179483, #257644, #38671 ) ;
#235131 = CIRCLE ( 'NONE', #47840, 0.09999999999998898659 ) ;
#235132 = EDGE_LOOP ( 'NONE', ( #221719, #169383, #90629, #136115 ) ) ;
#235133 = CARTESIAN_POINT ( 'NONE',  ( 21.04999999999987281, 67.10527618163379771, -61.03602316137499884 ) ) ;
#235134 = VERTEX_POINT ( 'NONE', #14816 ) ;
#235135 = DIRECTION ( 'NONE',  ( 0.000000000000000000, 0.000000000000000000, 1.000000000000000000 ) ) ;
#235136 = EDGE_CURVE ( 'NONE', #71322, #149588, #16098, .T. ) ;
#235137 = FACE_OUTER_BOUND ( 'NONE', #65414, .T. ) ;
#235139 = EDGE_LOOP ( 'NONE', ( #48302, #32015, #45437, #166067 ) ) ;
#235138 = FACE_OUTER_BOUND ( 'NONE', #146676, .T. ) ;
#235140 = CARTESIAN_POINT ( 'NONE',  ( -20.54999999999999716, 66.65000000001222702, -148.8731074845244393 ) ) ;
#235141 = DIRECTION ( 'NONE',  ( -1.000000000000000000, 0.000000000000000000, 0.000000000000000000 ) ) ;
#235142 = CYLINDRICAL_SURFACE ( 'NONE', #89507, 0.1000000000000002554 ) ;
#235143 = DIRECTION ( 'NONE',  ( 0.000000000000000000, -0.1350103645451876944, -0.9908441862701601321 ) ) ;
#235144 = DIRECTION ( 'NONE',  ( -3.265361837132813093E-16, -1.000000000000000000, 7.445645354460596589E-46 ) ) ;
#235145 = CIRCLE ( 'NONE', #201809, 0.09999999999999971412 ) ;
#235146 = ADVANCED_FACE ( 'NONE', ( #55158 ), #73509, .F. ) ;
#235147 = CARTESIAN_POINT ( 'NONE',  ( 13.99999999999999822, 62.10905854918434699, -217.1108499610991203 ) ) ;
#235148 = TOROIDAL_SURFACE ( 'NONE', #81000, 0.2000000000000000111, 0.1000000000000000056 ) ;
#235150 = ORIENTED_EDGE ( 'NONE', *, *, #32326, .F. ) ;
#235149 = DIRECTION ( 'NONE',  ( -1.000000000000000000, 0.000000000000000000, 0.000000000000000000 ) ) ;
#235151 = AXIS2_PLACEMENT_3D ( 'NONE', #31828, #153074, #151769 ) ;
#235152 = ADVANCED_FACE ( 'NONE', ( #94310 ), #232581, .F. ) ;
#235153 = AXIS2_PLACEMENT_3D ( 'NONE', #122917, #202444, #120374 ) ;
#235154 = B_SPLINE_CURVE_WITH_KNOTS ( 'NONE', 3,
 ( #160272, #239786, #158992, #61138, #201941, #140673, #45428, #84502, #164099, #104092 ),
 .UNSPECIFIED., .F., .F.,
 ( 4, 3, 3, 4 ),
 ( 0.000000000000000000, 0.0002000000000002884074, 0.001000000000045112589, 0.001967863649472103085 ),
 .UNSPECIFIED. ) ;
#235156 = ADVANCED_FACE ( 'NONE', ( #34379 ), #4605, .T. ) ;
#235155 = LINE ( 'NONE', #252132, #10102 ) ;
#235157 = AXIS2_PLACEMENT_3D ( 'NONE', #7461, #86974, #166571 ) ;
#235158 = ADVANCED_FACE ( 'NONE', ( #135994 ), #17362, .T. ) ;
#235159 = CARTESIAN_POINT ( 'NONE',  ( -22.19999999999999929, -11.65000000000000036, 14.10000000000000142 ) ) ;
#235160 = DIRECTION ( 'NONE',  ( 0.000000000000000000, 0.1495327102803663544, -0.9887567792719339499 ) ) ;
#235161 = AXIS2_PLACEMENT_3D ( 'NONE', #251190, #54280, #95969 ) ;
#235163 = ORIENTED_EDGE ( 'NONE', *, *, #115390, .T. ) ;
#235162 = AXIS2_PLACEMENT_3D ( 'NONE', #175818, #58382, #57102 ) ;
#235164 = CARTESIAN_POINT ( 'NONE',  ( 23.14999999999999858, 76.00000000001244871, -170.0231074845243597 ) ) ;
#235165 = CARTESIAN_POINT ( 'NONE',  ( 20.85000000000000142, 11.65000000001115943, -134.0000000000000284 ) ) ;
#235166 = ORIENTED_EDGE ( 'NONE', *, *, #16340, .T. ) ;
#235168 = EDGE_CURVE ( 'NONE', #221002, #84841, #50385, .T. ) ;
#235167 = CARTESIAN_POINT ( 'NONE',  ( 22.50000000000000000, 0.1000000000111554016, -55.35042919245524473 ) ) ;
#235169 = EDGE_CURVE ( 'NONE', #94125, #229678, #133448, .T. ) ;
#235170 = CARTESIAN_POINT ( 'NONE',  ( -16.94107738177415712, 65.98576071487597972, -190.9731074845244336 ) ) ;
#235171 = ORIENTED_EDGE ( 'NONE', *, *, #28529, .T. ) ;
#235172 = DIRECTION ( 'NONE',  ( 1.000000000000000000, -0.000000000000000000, 0.000000000000000000 ) ) ;
#235173 = EDGE_LOOP ( 'NONE', ( #153824, #165397, #4977, #91755 ) ) ;
#235174 = EDGE_CURVE ( 'NONE', #133539, #42653, #154346, .T. ) ;
#235175 = CARTESIAN_POINT ( 'NONE',  ( -18.59999999999999787, 64.35000000001222986, -148.7731074845244450 ) ) ;
#235177 = ORIENTED_EDGE ( 'NONE', *, *, #99625, .F. ) ;
#235176 = DIRECTION ( 'NONE',  ( -1.000000000000000000, 1.207181226542539700E-16, -2.694675058168174199E-16 ) ) ;
#235178 = CARTESIAN_POINT ( 'NONE',  ( 20.94999999999999574, 1.115600667400684642E-11, -134.0000000000000000 ) ) ;
#235179 = ORIENTED_EDGE ( 'NONE', *, *, #223452, .T. ) ;
#235180 = CIRCLE ( 'NONE', #56089, 0.1000000000000028644 ) ;
#235181 = DIRECTION ( 'NONE',  ( 0.000000000000000000, 0.000000000000000000, -1.000000000000000000 ) ) ;
#235182 = ORIENTED_EDGE ( 'NONE', *, *, #158046, .T. ) ;
#235183 = CIRCLE ( 'NONE', #56091, 0.1000000000000028644 ) ;
#235185 = ORIENTED_EDGE ( 'NONE', *, *, #140021, .F. ) ;
#235184 = ORIENTED_EDGE ( 'NONE', *, *, #108970, .F. ) ;
#235186 = CARTESIAN_POINT ( 'NONE',  ( 18.40000000000000213, 85.50000000001209344, -129.5237453873440927 ) ) ;
#235187 = ORIENTED_EDGE ( 'NONE', *, *, #79979, .T. ) ;
#235188 = EDGE_CURVE ( 'NONE', #215339, #204523, #75394, .T. ) ;
#235189 = DIRECTION ( 'NONE',  ( -1.000000000000000000, 0.000000000000000000, 0.000000000000000000 ) ) ;
#235190 = ORIENTED_EDGE ( 'NONE', *, *, #90033, .T. ) ;
#235191 = CIRCLE ( 'NONE', #197572, 0.1000000000000028644 ) ;
#235192 = ADVANCED_FACE ( 'NONE', ( #151757 ), #132168, .T. ) ;
#235193 = AXIS2_PLACEMENT_3D ( 'NONE', #181439, #141022, #82286 ) ;
#235194 = ORIENTED_EDGE ( 'NONE', *, *, #116483, .T. ) ;
#235195 = CARTESIAN_POINT ( 'NONE',  ( -23.15000000000000213, 6.268811756569107274, -220.3853799378769622 ) ) ;
#235196 = CARTESIAN_POINT ( 'NONE',  ( 18.60000000000000142, 9.105964803472835101, -245.3658845043482586 ) ) ;
#235197 =( BOUNDED_SURFACE ( )  B_SPLINE_SURFACE ( 3, 2, ( 
 ( #161897, #235287, #253568 ),
 ( #121495, #136161, #234007 ),
 ( #124043, #201005, #83580 ),
 ( #196173, #180167, #160619 ) ),
 .UNSPECIFIED., .F., .F., .F. ) 
 B_SPLINE_SURFACE_WITH_KNOTS ( ( 4, 4 ),
 ( 3, 3 ),
 ( 5.727910411845712702, 5.983100554402350113 ),
 ( 0.000000000000000000, 1.000000000000000000 ),
 .UNSPECIFIED. ) 
 GEOMETRIC_REPRESENTATION_ITEM ( )  RATIONAL_B_SPLINE_SURFACE ( (
 ( 1.000000000000000000, 0.8946697475932060550, 1.000000000000000000),
 ( 1.000000000000000000, 0.9035312726220692259, 1.000000000000000000),
 ( 1.000000000000000000, 0.9104333467450208550, 1.000000000000000000),
 ( 1.000000000000000000, 0.9152888060719425178, 1.000000000000000000) ) ) 
 REPRESENTATION_ITEM ( '' )  SURFACE ( )  );
#235198 = CARTESIAN_POINT ( 'NONE',  ( 23.24999999999999645, 13.44928205424795564, -207.5377222505711075 ) ) ;
#235199 = ORIENTED_EDGE ( 'NONE', *, *, #18965, .F. ) ;
#235200 = DIRECTION ( 'NONE',  ( -7.304098846218134667E-16, 1.000000000000000000, 6.982962677686267499E-15 ) ) ;
#235201 = DIRECTION ( 'NONE',  ( 0.000000000000000000, 0.000000000000000000, 1.000000000000000000 ) ) ;
#235202 = EDGE_CURVE ( 'NONE', #208753, #68040, #187808, .T. ) ;
#235203 = DIRECTION ( 'NONE',  ( -3.469446951953772592E-14, -0.9651348961777379554, 0.2617529984164210233 ) ) ;
#235204 = VECTOR ( 'NONE', #181720, 1000.000000000000114 ) ;
#235205 = ORIENTED_EDGE ( 'NONE', *, *, #30844, .F. ) ;
#235206 = DIRECTION ( 'NONE',  ( 1.000000000000000000, 0.000000000000000000, 0.000000000000000000 ) ) ;
#235207 = AXIS2_PLACEMENT_3D ( 'NONE', #190539, #129259, #250476 ) ;
#235208 = CARTESIAN_POINT ( 'NONE',  ( 18.39999999999999503, 64.25000000001256240, -182.6731074845244507 ) ) ;
#235209 = LINE ( 'NONE', #193524, #62018 ) ;
#235210 = AXIS2_PLACEMENT_3D ( 'NONE', #121359, #200855, #146005 ) ;
#235211 = VERTEX_POINT ( 'NONE', #76038 ) ;
#235212 = DIRECTION ( 'NONE',  ( -0.000000000000000000, 1.000000000000000000, 6.982962677686266711E-15 ) ) ;
#235213 = VERTEX_POINT ( 'NONE', #155620 ) ;
#235214 = ORIENTED_EDGE ( 'NONE', *, *, #193902, .F. ) ;
#235215 = ORIENTED_EDGE ( 'NONE', *, *, #14375, .F. ) ;
#235216 = VERTEX_POINT ( 'NONE', #235124 ) ;
#235217 = CARTESIAN_POINT ( 'NONE',  ( 22.39999999999999503, 1.115600667400684642E-11, -126.2092204016266379 ) ) ;
#235218 = FACE_OUTER_BOUND ( 'NONE', #141384, .T. ) ;
#235219 = EDGE_LOOP ( 'NONE', ( #232909, #216377, #118847, #191874 ) ) ;
#235220 = AXIS2_PLACEMENT_3D ( 'NONE', #165808, #60253, #122824 ) ;
#235221 = ORIENTED_EDGE ( 'NONE', *, *, #143935, .T. ) ;
#235222 = CARTESIAN_POINT ( 'NONE',  ( 20.02499999999999858, 66.25000000001223555, -148.7731074845244450 ) ) ;
#235223 = CARTESIAN_POINT ( 'NONE',  ( -23.15000000000000213, 73.40000000001172964, -81.27310748452434552 ) ) ;
#235224 = VERTEX_POINT ( 'NONE', #13513 ) ;
#235225 = ORIENTED_EDGE ( 'NONE', *, *, #73537, .F. ) ;
#235226 = CIRCLE ( 'NONE', #35363, 0.1000000000000008799 ) ;
#235227 = CARTESIAN_POINT ( 'NONE',  ( -21.04999999999994387, 82.84256550613280012, -26.34830530078816935 ) ) ;
#235228 = EDGE_CURVE ( 'NONE', #194806, #248967, #83694, .T. ) ;
#235229 = CARTESIAN_POINT ( 'NONE',  ( -21.44999999999999929, 68.65000000001253966, -182.2731074845244166 ) ) ;
#235230 = CARTESIAN_POINT ( 'NONE',  ( -16.87331047859651179, 9.950000000011142376, -46.15000000000000568 ) ) ;
#235231 = CARTESIAN_POINT ( 'NONE',  ( -20.54999999999999716, 76.00000000001222134, -149.3981074845243313 ) ) ;
#235232 = DIRECTION ( 'NONE',  ( -1.000000000000000000, 0.000000000000000000, 0.000000000000000000 ) ) ;
#235233 = CARTESIAN_POINT ( 'NONE',  ( -20.94999999999999929, 11.75000000000000000, -7.014805770654001016 ) ) ;
#235235 = CARTESIAN_POINT ( 'NONE',  ( -19.89999999999999858, 5.488301202077012775, 16.50000000000000000 ) ) ;
#235234 = DIRECTION ( 'NONE',  ( 3.265361837132813093E-16, -1.000000000000000000, -0.000000000000000000 ) ) ;
#235236 = CARTESIAN_POINT ( 'NONE',  ( 20.94999999999999929, -8.999999999988842703, -90.60603087734760663 ) ) ;
#235237 = CARTESIAN_POINT ( 'NONE',  ( -16.88705144915384082, 23.22574875786642679, -231.0677395022140672 ) ) ;
#235238 = FACE_OUTER_BOUND ( 'NONE', #204513, .T. ) ;
#235239 = ADVANCED_FACE ( 'NONE', ( #78598 ), #60319, .T. ) ;
#235240 = DIRECTION ( 'NONE',  ( 0.7071067811864846231, 0.2890913453341779626, -0.6453109281989296564 ) ) ;
#235241 = AXIS2_PLACEMENT_3D ( 'NONE', #86093, #187819, #154790 ) ;
#235242 = ORIENTED_EDGE ( 'NONE', *, *, #1938, .F. ) ;
#235243 = VECTOR ( 'NONE', #16991, 1000.000000000000000 ) ;
#235245 = ORIENTED_EDGE ( 'NONE', *, *, #51549, .T. ) ;
#235244 = CARTESIAN_POINT ( 'NONE',  ( -20.64999999999999858, 1.115600667400684642E-11, -134.0000000000000284 ) ) ;
#235246 = CARTESIAN_POINT ( 'NONE',  ( 18.59999999999999076, 77.16412189325258453, -28.10825939895270764 ) ) ;
#235247 = CARTESIAN_POINT ( 'NONE',  ( -20.94999999999999929, 70.88170441948386724, -234.2197789011331679 ) ) ;
#235248 = ORIENTED_EDGE ( 'NONE', *, *, #133522, .F. ) ;
#235249 = SURFACE_STYLE_FILL_AREA ( #96984 ) ;
#235250 = CARTESIAN_POINT ( 'NONE',  ( 20.94999675878240808, 10.29307482169071264, -206.4586421466940180 ) ) ;
#235251 = CYLINDRICAL_SURFACE ( 'NONE', #3883, 0.09999999999999939493 ) ;
#235252 = VERTEX_POINT ( 'NONE', #141160 ) ;
#235254 = CARTESIAN_POINT ( 'NONE',  ( -21.05439746398122836, 11.75000000001115197, -140.9899164874850044 ) ) ;
#235253 = AXIS2_PLACEMENT_3D ( 'NONE', #47882, #208271, #46590 ) ;
#235255 = CARTESIAN_POINT ( 'NONE',  ( -23.25000000000000000, 67.23127455305835554, -235.8551265064784559 ) ) ;
#235256 = DIRECTION ( 'NONE',  ( 0.000000000000000000, 0.000000000000000000, 1.000000000000000000 ) ) ;
#235258 = VERTEX_POINT ( 'NONE', #23805 ) ;
#235257 = DIRECTION ( 'NONE',  ( -1.000000000000000000, -0.000000000000000000, 0.000000000000000000 ) ) ;
#235260 = ORIENTED_EDGE ( 'NONE', *, *, #92308, .F. ) ;
#235259 = CARTESIAN_POINT ( 'NONE',  ( 18.59999999999999076, 69.55000000001199112, -115.3731074845243398 ) ) ;
#235261 = DIRECTION ( 'NONE',  ( -1.000000000000000000, -0.000000000000000000, -0.000000000000000000 ) ) ;
#235262 = CARTESIAN_POINT ( 'NONE',  ( 21.05563370358598263, 10.72423035584650997, -12.18309081596307308 ) ) ;
#235263 = EDGE_CURVE ( 'NONE', #244178, #75223, #83697, .T. ) ;
#235264 = CARTESIAN_POINT ( 'NONE',  ( 20.94999999999999929, 5.000000000011153745, -155.0947339810869323 ) ) ;
#235265 = CARTESIAN_POINT ( 'NONE',  ( -22.49436431346200038, 55.96998815520995407, -232.8702878457373231 ) ) ;
#235267 = CARTESIAN_POINT ( 'NONE',  ( 18.59999999999999787, 76.00000000001213607, -136.5231074845242745 ) ) ;
#235266 = CARTESIAN_POINT ( 'NONE',  ( -16.92280123533721792, 9.950000000011137047, -154.6493676859139725 ) ) ;
#235268 = CARTESIAN_POINT ( 'NONE',  ( 18.59999999999999076, 74.25000000001205080, -124.8535959266226598 ) ) ;
#235269 = TOROIDAL_SURFACE ( 'NONE', #181144, 1.900000000000002576, 0.1000000000000000056 ) ;
#235270 = DIRECTION ( 'NONE',  ( 0.000000000000000000, 1.776356839400310418E-15, -1.000000000000000000 ) ) ;
#235271 = FACE_OUTER_BOUND ( 'NONE', #9135, .T. ) ;
#235272 = AXIS2_PLACEMENT_3D ( 'NONE', #2594, #100400, #104253 ) ;
#235273 = CARTESIAN_POINT ( 'NONE',  ( 21.07954640115374900, 1.580764630276365823, -230.6858712634206370 ) ) ;
#235274 = TOROIDAL_SURFACE ( 'NONE', #60312, 0.2000000000000000111, 0.1000000000000000056 ) ;
#235275 = EDGE_LOOP ( 'NONE', ( #2942, #217450, #32029, #17408 ) ) ;
#235276 = AXIS2_PLACEMENT_3D ( 'NONE', #35221, #114724, #155167 ) ;
#235277 = CARTESIAN_POINT ( 'NONE',  ( -21.45000000000000284, 21.65523568329831505, -232.7692078405380300 ) ) ;
#235278 = ORIENTED_EDGE ( 'NONE', *, *, #242143, .T. ) ;
#235279 =( BOUNDED_SURFACE ( )  B_SPLINE_SURFACE ( 3, 2, ( 
 ( #68911, #148436, #208425 ),
 ( #29801, #109279, #51867 ),
 ( #17883, #251368, #16630 ),
 ( #171877, #216082, #154870 ),
 ( #72774, #195278, #170612 ),
 ( #213517, #116998, #113146 ) ),
 .UNSPECIFIED., .F., .F., .T. ) 
 B_SPLINE_SURFACE_WITH_KNOTS ( ( 4, 2, 4 ),
 ( 3, 3 ),
 ( 0.0001342700090130047525, 0.0002909192928057360351, 0.0004475685765984672906 ),
 ( 0.000000000000000000, 1.000000000000000000 ),
 .UNSPECIFIED. ) 
 GEOMETRIC_REPRESENTATION_ITEM ( )  RATIONAL_B_SPLINE_SURFACE ( (
 ( 1.000000000000000000, 0.7250110520819876836, 1.000000000000000000),
 ( 1.000000000000000000, 0.7257599279134024917, 1.000000000000000000),
 ( 1.000000000000000000, 0.7137594617284269694, 1.000000000000000000),
 ( 1.000000000000000000, 0.6959270178809834340, 1.000000000000000000),
 ( 1.000000000000000000, 0.6919879549339010838, 1.000000000000000000),
 ( 1.000000000000000000, 0.7071067811865414665, 1.000000000000000000) ) ) 
 REPRESENTATION_ITEM ( '' )  SURFACE ( )  );
#235280 = EDGE_LOOP ( 'NONE', ( #114158, #162303, #108460, #69594 ) ) ;
#235281 = EDGE_CURVE ( 'NONE', #48358, #56214, #179034, .T. ) ;
#235282 = CARTESIAN_POINT ( 'NONE',  ( -23.15000000000000213, -3.770473190032741062, -225.9805569534692324 ) ) ;
#235283 = DIRECTION ( 'NONE',  ( 1.000000000000000000, 0.000000000000000000, 0.000000000000000000 ) ) ;
#235284 = ORIENTED_EDGE ( 'NONE', *, *, #123370, .F. ) ;
#235285 = EDGE_CURVE ( 'NONE', #192913, #226817, #158589, .T. ) ;
#235286 = ORIENTED_EDGE ( 'NONE', *, *, #79942, .T. ) ;
#235287 = CARTESIAN_POINT ( 'NONE',  ( -18.41431012584569160, 11.48747202921932065, -143.2267639868983622 ) ) ;
#235288 =( NAMED_UNIT ( * ) PLANE_ANGLE_UNIT ( ) SI_UNIT ( $, .RADIAN. ) );
#235289 = EDGE_CURVE ( 'NONE', #49319, #180142, #202406, .T. ) ;
#235290 = B_SPLINE_CURVE_WITH_KNOTS ( 'NONE', 3,
 ( #60227, #58919, #240171, #236301, #156802, #117644, #57650, #118944, #158103, #99337 ),
 .UNSPECIFIED., .F., .F.,
 ( 4, 3, 3, 4 ),
 ( 0.000000000000000000, 1.004626015991452777E-05, 1.831183478182391193E-05, 2.062343583995917743E-05 ),
 .UNSPECIFIED. ) ;
#235291 = ORIENTED_EDGE ( 'NONE', *, *, #130525, .F. ) ;
#235292 = AXIS2_PLACEMENT_3D ( 'NONE', #14543, #36683, #195748 ) ;
#235293 = VERTEX_POINT ( 'NONE', #42071 ) ;
#235294 = CIRCLE ( 'NONE', #252064, 12.97499999999998721 ) ;
#235295 = DIRECTION ( 'NONE',  ( 0.000000000000000000, 0.000000000000000000, 1.000000000000000000 ) ) ;
#235296 = CARTESIAN_POINT ( 'NONE',  ( -22.39999999999999503, -5.963111948670274387E-16, 7.790779598373403836 ) ) ;
#235297 = CARTESIAN_POINT ( 'NONE',  ( -20.94999999999999929, 87.48912529308798014, -99.92310748452423752 ) ) ;
#235298 = AXIS2_PLACEMENT_3D ( 'NONE', #38815, #238275, #40121 ) ;
#235299 = DIRECTION ( 'NONE',  ( 0.000000000000000000, -0.7092521942342977503, -0.7049548389605067023 ) ) ;
#235300 = LINE ( 'NONE', #73699, #90186 ) ;
#235301 = DIRECTION ( 'NONE',  ( -4.408576920032447355E-17, -0.1350103645451945777, 0.9908441862701589109 ) ) ;
#235302 = CARTESIAN_POINT ( 'NONE',  ( -21.14999999999999858, -3.187427350888460076, -228.3200064793908837 ) ) ;
#235304 = EDGE_LOOP ( 'NONE', ( #124210, #37648, #40430 ) ) ;
#235303 = CARTESIAN_POINT ( 'NONE',  ( -21.14999999999999858, 87.65000000001212754, -133.6231074845242119 ) ) ;
#235306 = CARTESIAN_POINT ( 'NONE',  ( -22.37643362114956602, 65.13957426554411256, -243.1891076939221534 ) ) ;
#235305 = CARTESIAN_POINT ( 'NONE',  ( -16.94107738177415712, 22.92025126680846725, -230.8312174982872591 ) ) ;
#235307 = EDGE_CURVE ( 'NONE', #68363, #43683, #219387, .T. ) ;
#235308 = FACE_OUTER_BOUND ( 'NONE', #164977, .T. ) ;
#235309 = ORIENTED_EDGE ( 'NONE', *, *, #3372, .F. ) ;
#235310 = VECTOR ( 'NONE', #4181, 1000.000000000000000 ) ;
#235311 = CARTESIAN_POINT ( 'NONE',  ( -18.41353343127311604, 8.841736820195469804, -245.4273993276876809 ) ) ;
#235312 = DIRECTION ( 'NONE',  ( 1.000000000000000000, 0.000000000000000000, 0.000000000000000000 ) ) ;
#235313 = VECTOR ( 'NONE', #46504, 1000.000000000000000 ) ;
#235315 = ORIENTED_EDGE ( 'NONE', *, *, #89789, .T. ) ;
#235314 = AXIS2_PLACEMENT_3D ( 'NONE', #34483, #108842, #93129 ) ;
#235316 = VECTOR ( 'NONE', #220704, 1000.000000000000000 ) ;
#235317 = EDGE_CURVE ( 'NONE', #34352, #74170, #163293, .T. ) ;
#235318 = DIRECTION ( 'NONE',  ( 0.000000000000000000, -1.000000000000000000, 0.000000000000000000 ) ) ;
#235319 = CARTESIAN_POINT ( 'NONE',  ( -20.64999999999999858, -8.730841121484170131, -57.40192528101567149 ) ) ;
#235320 = CARTESIAN_POINT ( 'NONE',  ( 18.49999999999999289, 43.16354019706792400, -239.5695141926698284 ) ) ;
#235321 = ORIENTED_EDGE ( 'NONE', *, *, #23875, .F. ) ;
#235322 = ORIENTED_EDGE ( 'NONE', *, *, #64935, .T. ) ;
#235323 = CARTESIAN_POINT ( 'NONE',  ( 22.49999999999999645, 64.08545097430041437, -247.0723585184914270 ) ) ;
#235324 = CARTESIAN_POINT ( 'NONE',  ( -18.52309608778515226, -0.8639146907862034208, -242.3454321524539523 ) ) ;
#235325 = DIRECTION ( 'NONE',  ( 1.000000000000000000, 0.000000000000000000, 0.000000000000000000 ) ) ;
#235326 = ORIENTED_EDGE ( 'NONE', *, *, #145678, .T. ) ;
#235327 = AXIS2_PLACEMENT_3D ( 'NONE', #207629, #131921, #108504 ) ;
#235328 = CIRCLE ( 'NONE', #214484, 0.09999999999999939493 ) ;
#235329 = EDGE_CURVE ( 'NONE', #134738, #218279, #101056, .T. ) ;
#235330 = CARTESIAN_POINT ( 'NONE',  ( 15.74999999999999645, 47.91126876242802979, -234.2648823414208152 ) ) ;
#235331 = DIRECTION ( 'NONE',  ( 1.000000000000000000, 0.000000000000000000, -0.000000000000000000 ) ) ;
#235332 = DIRECTION ( 'NONE',  ( 0.000000000000000000, 0.000000000000000000, -1.000000000000000000 ) ) ;
#235333 = CARTESIAN_POINT ( 'NONE',  ( -18.39999999999999858, -9.499999999988849808, -207.6001893912220169 ) ) ;
#235334 = ADVANCED_FACE ( 'NONE', ( #40800 ), #221939, .T. ) ;
#235335 = VERTEX_POINT ( 'NONE', #82425 ) ;
#235336 = DIRECTION ( 'NONE',  ( -1.000000000000000000, 0.000000000000000000, 0.000000000000000000 ) ) ;
#235337 = CARTESIAN_POINT ( 'NONE',  ( -16.93710578446424009, 66.05000000001187743, -90.10430350072498129 ) ) ;
#235338 = LINE ( 'NONE', #215770, #162803 ) ;
#235339 = DIRECTION ( 'NONE',  ( -1.000000000000000000, -0.000000000000000000, -0.000000000000000000 ) ) ;
#235340 = CARTESIAN_POINT ( 'NONE',  ( 20.84999999999998721, 31.11065811373596190, -259.9087319612273177 ) ) ;
#235342 = ORIENTED_EDGE ( 'NONE', *, *, #133988, .T. ) ;
#235341 = CARTESIAN_POINT ( 'NONE',  ( -18.40000000000000213, 9.957490673325212427, -220.1701168356097469 ) ) ;
#235343 = CARTESIAN_POINT ( 'NONE',  ( 21.05000000000000071, 36.65892442174472876, -249.5511627012454596 ) ) ;
#235344 = DIRECTION ( 'NONE',  ( 1.000000000000000000, 0.000000000000000000, 0.000000000000000000 ) ) ;
#235345 = DIRECTION ( 'NONE',  ( 1.000000000000000000, 0.000000000000000000, 0.000000000000000000 ) ) ;
#235346 = ADVANCED_FACE ( 'NONE', ( #21235 ), #100700, .T. ) ;
#235347 = ORIENTED_EDGE ( 'NONE', *, *, #32987, .F. ) ;
#235348 = DIRECTION ( 'NONE',  ( -0.000000000000000000, -6.982962677686266711E-15, 1.000000000000000000 ) ) ;
#235349 = CIRCLE ( 'NONE', #122943, 2.099999999999998757 ) ;
#235350 = LINE ( 'NONE', #252343, #23494 ) ;
#235351 = DIRECTION ( 'NONE',  ( 1.000000000000000000, 3.265361837132813093E-16, -0.000000000000000000 ) ) ;
#235353 = AXIS2_PLACEMENT_3D ( 'NONE', #215899, #138910, #17705 ) ;
#235352 = CARTESIAN_POINT ( 'NONE',  ( 21.00000000000000000, 52.06567329910104291, -231.9654557484363409 ) ) ;
#235354 = EDGE_CURVE ( 'NONE', #17892, #40168, #221089, .T. ) ;
#235355 = AXIS2_PLACEMENT_3D ( 'NONE', #369, #202436, #218121 ) ;
#235356 = DIRECTION ( 'NONE',  ( 1.000000000000000000, 0.000000000000000000, 0.000000000000000000 ) ) ;
#235357 = EDGE_CURVE ( 'NONE', #223382, #133593, #181579, .T. ) ;
#235358 = DIRECTION ( 'NONE',  ( 0.000000000000000000, -0.9908441862701782288, 0.1350103645450542456 ) ) ;
#235359 = ORIENTED_EDGE ( 'NONE', *, *, #152381, .F. ) ;
#235360 = ORIENTED_EDGE ( 'NONE', *, *, #121323, .F. ) ;
#235361 = AXIS2_PLACEMENT_3D ( 'NONE', #49798, #228457, #71946 ) ;
#235362 = CARTESIAN_POINT ( 'NONE',  ( 21.46681500598198156, -1.459285199489900542, -194.2995562827431684 ) ) ;
#235363 = AXIS2_PLACEMENT_3D ( 'NONE', #205807, #126263, #226644 ) ;
#235364 = CARTESIAN_POINT ( 'NONE',  ( -17.04295772865455660, 65.97510057475052747, -115.6731074845243796 ) ) ;
#235365 = ADVANCED_FACE ( 'NONE', ( #223237 ), #62890, .F. ) ;
#235366 = CARTESIAN_POINT ( 'NONE',  ( 20.85000000000000142, 77.83585931145600512, -158.5186683157258187 ) ) ;
#235367 = CARTESIAN_POINT ( 'NONE',  ( -22.47071067811865319, 7.720074744509219933, -133.9009075452974002 ) ) ;
#235369 = VECTOR ( 'NONE', #241093, 1000.000000000000000 ) ;
#235368 = LINE ( 'NONE', #112869, #125988 ) ;
#235370 = EDGE_CURVE ( 'NONE', #154991, #95624, #66981, .T. ) ;
#235372 = ADVANCED_FACE ( 'NONE', ( #61615 ), #166982, .T. ) ;
#235371 = CARTESIAN_POINT ( 'NONE',  ( 20.22894356738504129, 10.82552933503960446, -207.1046633763657496 ) ) ;
#235373 = VECTOR ( 'NONE', #5035, 1000.000000000000000 ) ;
#235374 = CARTESIAN_POINT ( 'NONE',  ( 21.14999999999999503, 76.00000000001169553, -75.77310748452431710 ) ) ;
#235375 = DIRECTION ( 'NONE',  ( 0.000000000000000000, -1.000000000000000000, 0.000000000000000000 ) ) ;
#235376 = EDGE_LOOP ( 'NONE', ( #132667, #212087, #122413, #164351, #59547, #254856, #61802, #123577, #119808, #49784, #156905, #195765 ) ) ;
#235377 = CARTESIAN_POINT ( 'NONE',  ( 21.05000000000000071, 45.93587830916155212, -239.9163948487882863 ) ) ;
#235378 = EDGE_CURVE ( 'NONE', #136295, #192701, #42068, .T. ) ;
#235379 = VERTEX_POINT ( 'NONE', #26347 ) ;
#235380 = ORIENTED_EDGE ( 'NONE', *, *, #46749, .T. ) ;
#235381 = CARTESIAN_POINT ( 'NONE',  ( 21.10257677756355932, 75.97504925044442814, -176.4214892270570942 ) ) ;
#235382 = CYLINDRICAL_SURFACE ( 'NONE', #218384, 0.1000000000000046685 ) ;
#235383 = SPHERICAL_SURFACE ( 'NONE', #232977, 0.1000000000000000056 ) ;
#235384 = VERTEX_POINT ( 'NONE', #185414 ) ;
#235385 = EDGE_CURVE ( 'NONE', #991, #170581, #203697, .T. ) ;
#235386 = ADVANCED_FACE ( 'NONE', ( #227093 ), #68030, .F. ) ;
#235387 = CARTESIAN_POINT ( 'NONE',  ( 18.79999999999999716, 0.000000000000000000, 0.000000000000000000 ) ) ;
#235388 = DIRECTION ( 'NONE',  ( -0.000000000000000000, 0.4721928772777347350, 0.8814952561688429444 ) ) ;
#235389 = DIRECTION ( 'NONE',  ( 1.000000000000000000, 0.000000000000000000, 0.000000000000000000 ) ) ;
#235390 = VERTEX_POINT ( 'NONE', #225794 ) ;
#235391 = CARTESIAN_POINT ( 'NONE',  ( -12.68215100488890812, 9.396630376328875656, -151.9070573928183592 ) ) ;
#235393 = ORIENTED_EDGE ( 'NONE', *, *, #217932, .T. ) ;
#235392 = DIRECTION ( 'NONE',  ( 0.000000000000000000, 0.7397890806274223241, 0.6728388485993012091 ) ) ;
#235394 = LINE ( 'NONE', #212005, #189834 ) ;
#235395 = AXIS2_PLACEMENT_3D ( 'NONE', #103574, #83986, #141437 ) ;
#235396 = ORIENTED_EDGE ( 'NONE', *, *, #153889, .F. ) ;
#235397 = CARTESIAN_POINT ( 'NONE',  ( -18.40000000000000213, 70.35000000001153353, -48.67310748452436542 ) ) ;
#235398 = CARTESIAN_POINT ( 'NONE',  ( -23.24999999999999645, -9.600000000000003197, -40.10018939122204529 ) ) ;
#235399 = ORIENTED_EDGE ( 'NONE', *, *, #196070, .T. ) ;
#235400 = DIRECTION ( 'NONE',  ( 0.000000000000000000, -0.9910827722268048534, -0.1332476588733589040 ) ) ;
#235401 = EDGE_CURVE ( 'NONE', #81429, #93783, #109708, .T. ) ;
#235402 = ADVANCED_FACE ( 'NONE', ( #206264 ), #8071, .F. ) ;
#235403 = CARTESIAN_POINT ( 'NONE',  ( -21.05000000000000071, -11.64999999998884306, -63.89999999999999858 ) ) ;
#235404 = CARTESIAN_POINT ( 'NONE',  ( -20.54999999999999716, 84.73084112150763758, -160.4250327655399531 ) ) ;
#235405 = ORIENTED_EDGE ( 'NONE', *, *, #88253, .F. ) ;
#235406 = CARTESIAN_POINT ( 'NONE',  ( 21.05000000000000071, 8.776282648982402179, -41.98759237851939474 ) ) ;
#235407 = EDGE_CURVE ( 'NONE', #121993, #84354, #246054, .T. ) ;
#235408 = ORIENTED_EDGE ( 'NONE', *, *, #174587, .T. ) ;
#235409 = CIRCLE ( 'NONE', #231352, 0.09999999999999939493 ) ;
#235410 = CIRCLE ( 'NONE', #143667, 12.87499999999999467 ) ;
#235411 = VERTEX_POINT ( 'NONE', #27661 ) ;
#235412 = DIRECTION ( 'NONE',  ( 0.000000000000000000, -0.4999999999999088507, 0.8660254037844913322 ) ) ;
#235413 = CARTESIAN_POINT ( 'NONE',  ( 23.25000000000000000, 1.627786319807483340, -244.0021210468063089 ) ) ;
#235415 = ORIENTED_EDGE ( 'NONE', *, *, #168538, .T. ) ;
#235414 = CARTESIAN_POINT ( 'NONE',  ( 18.55857864376267941, 10.36715728753653565, -158.7500000000000000 ) ) ;
#235416 = CARTESIAN_POINT ( 'NONE',  ( 20.94999999999999574, -1.835341550213255957, -145.6551512925629766 ) ) ;
#235417 = DIRECTION ( 'NONE',  ( 0.000000000000000000, 0.000000000000000000, -1.000000000000000000 ) ) ;
#235418 = CARTESIAN_POINT ( 'NONE',  ( -21.05000000000000071, 14.85285025691667293, -236.4388300032497057 ) ) ;
#235419 = DIRECTION ( 'NONE',  ( 0.000000000000000000, -7.086529944415886769E-15, 1.000000000000000000 ) ) ;
#235420 = ADVANCED_FACE ( 'NONE', ( #25085 ), #186713, .T. ) ;
#235421 = FACE_OUTER_BOUND ( 'NONE', #44537, .T. ) ;
#235422 = DIRECTION ( 'NONE',  ( 0.000000000000000000, 0.9770955615653259541, 0.2128009952263860971 ) ) ;
#235424 = VERTEX_POINT ( 'NONE', #28957 ) ;
#235423 = DIRECTION ( 'NONE',  ( 3.616040088954490704E-32, 7.105427357601001859E-15, -1.000000000000000000 ) ) ;
#235426 = ORIENTED_EDGE ( 'NONE', *, *, #112314, .F. ) ;
#235425 = CARTESIAN_POINT ( 'NONE',  ( 18.49999999999999289, 3.801854678198143933, -188.1465607323988252 ) ) ;
#235428 = CARTESIAN_POINT ( 'NONE',  ( -16.89155683852526479, 51.04631869796540400, -232.2029617786061522 ) ) ;
#235427 = DIRECTION ( 'NONE',  ( -1.000000000000000000, 0.000000000000000000, 0.000000000000000000 ) ) ;
#235430 = ORIENTED_EDGE ( 'NONE', *, *, #72982, .F. ) ;
#235429 = DIRECTION ( 'NONE',  ( -1.000000000000000000, -0.000000000000000000, 0.000000000000000000 ) ) ;
#235431 = ADVANCED_FACE ( 'NONE', ( #47157 ), #246659, .F. ) ;
#235432 = ORIENTED_EDGE ( 'NONE', *, *, #161025, .T. ) ;
#235433 = CARTESIAN_POINT ( 'NONE',  ( -18.50000972452446035, 10.29326151435326508, -105.9592822510415431 ) ) ;
#235434 = CARTESIAN_POINT ( 'NONE',  ( -23.30000000000000426, -11.79999999999999893, 33.00000000000000000 ) ) ;
#235435 = AXIS2_PLACEMENT_3D ( 'NONE', #202808, #43742, #4596 ) ;
#235436 = DIRECTION ( 'NONE',  ( -3.265361837132813093E-16, 1.000000000000000000, 0.000000000000000000 ) ) ;
#235437 = DIRECTION ( 'NONE',  ( 1.000000000000000000, 3.265361837132813093E-16, -0.000000000000000000 ) ) ;
#235438 = EDGE_CURVE ( 'NONE', #138330, #233092, #96193, .T. ) ;
#235439 = DIRECTION ( 'NONE',  ( 0.000000000000000000, -7.272083257015735086E-15, 1.000000000000000000 ) ) ;
#235440 = DIRECTION ( 'NONE',  ( 1.000000000000000000, -3.448943450116723568E-16, -6.438528483529607644E-16 ) ) ;
#235441 = ADVANCED_FACE ( 'NONE', ( #126723 ), #207559, .T. ) ;
#235442 = DIRECTION ( 'NONE',  ( 0.000000000000000000, -0.9908441862701605762, -0.1350103645451835310 ) ) ;
#235443 = EDGE_LOOP ( 'NONE', ( #96505, #162708, #217895, #184070 ) ) ;
#235444 = ORIENTED_EDGE ( 'NONE', *, *, #97080, .T. ) ;
#235445 = EDGE_CURVE ( 'NONE', #107287, #184435, #169740, .T. ) ;
#235446 = CARTESIAN_POINT ( 'NONE',  ( 21.04999999999999716, 30.73564429423252164, -252.2206578267995383 ) ) ;
#235447 = AXIS2_PLACEMENT_3D ( 'NONE', #39285, #77093, #12337 ) ;
#235448 = AXIS2_PLACEMENT_3D ( 'NONE', #206915, #107810, #8716 ) ;
#235449 = VERTEX_POINT ( 'NONE', #129294 ) ;
#235450 = CARTESIAN_POINT ( 'NONE',  ( 18.59999999999999076, -1.164121893230052995, -108.4148480855716485 ) ) ;
#235451 = CARTESIAN_POINT ( 'NONE',  ( -16.93388492042257809, 51.64923346972221196, -231.8906307491038206 ) ) ;
#235452 = AXIS2_PLACEMENT_3D ( 'NONE', #24000, #145194, #66952 ) ;
#235453 = AXIS2_PLACEMENT_3D ( 'NONE', #166932, #146036, #123932 ) ;
#235454 = EDGE_CURVE ( 'NONE', #243775, #33512, #25310, .T. ) ;
#235456 = EDGE_CURVE ( 'NONE', #109498, #44088, #97488, .T. ) ;
#235455 = ADVANCED_FACE ( 'NONE', ( #244090 ), #79440, .F. ) ;
#235457 = CARTESIAN_POINT ( 'NONE',  ( -22.00411653889210584, -1.446770167451707723, -193.8916177604859854 ) ) ;
#235458 = STYLED_ITEM ( 'NONE', ( #152252 ), #144814 ) ;
#235459 = VERTEX_POINT ( 'NONE', #111009 ) ;
#235460 = CARTESIAN_POINT ( 'NONE',  ( -14.87770893841227249, 66.56936289831527631, -118.2548468664633958 ) ) ;
#235461 = ORIENTED_EDGE ( 'NONE', *, *, #211949, .T. ) ;
#235462 = CARTESIAN_POINT ( 'NONE',  ( -17.29838795459022194, 10.37154985796385276, -89.10474128261724047 ) ) ;
#235463 = VERTEX_POINT ( 'NONE', #54866 ) ;
#235464 = FACE_OUTER_BOUND ( 'NONE', #47814, .T. ) ;
#235465 = CARTESIAN_POINT ( 'NONE',  ( 20.90000000000000213, 1.212568896937007645, -8.000000000000000000 ) ) ;
#235466 = DIRECTION ( 'NONE',  ( 0.000000000000000000, 0.000000000000000000, 1.000000000000000000 ) ) ;
#235467 = VERTEX_POINT ( 'NONE', #116161 ) ;
#235468 = DIRECTION ( 'NONE',  ( -0.000000000000000000, 3.469446951953635015E-14, 1.000000000000000000 ) ) ;
#235470 = VERTEX_POINT ( 'NONE', #95295 ) ;
#235469 = DIRECTION ( 'NONE',  ( -1.000000000000000000, 0.000000000000000000, 0.000000000000000000 ) ) ;
#235471 = EDGE_CURVE ( 'NONE', #139087, #87352, #17120, .T. ) ;
#235472 = EDGE_CURVE ( 'NONE', #190272, #205178, #225172, .T. ) ;
#235474 = ORIENTED_EDGE ( 'NONE', *, *, #24391, .F. ) ;
#235473 = AXIS2_PLACEMENT_3D ( 'NONE', #174625, #254086, #75494 ) ;
#235475 = ORIENTED_EDGE ( 'NONE', *, *, #56990, .F. ) ;
#235476 = CIRCLE ( 'NONE', #227294, 1.749999999999999778 ) ;
#235477 = EDGE_CURVE ( 'NONE', #253517, #183242, #35366, .T. ) ;
#235478 = FACE_OUTER_BOUND ( 'NONE', #38058, .T. ) ;
#235479 = ORIENTED_EDGE ( 'NONE', *, *, #239062, .F. ) ;
#235480 = AXIS2_PLACEMENT_3D ( 'NONE', #72183, #73481, #137264 ) ;
#235481 = CARTESIAN_POINT ( 'NONE',  ( -21.05000000000000071, 28.51339163295720169, -258.4040038037771865 ) ) ;
#235482 = CARTESIAN_POINT ( 'NONE',  ( 21.05000000000000071, 69.50331341424364950, -69.50845136601148511 ) ) ;
#235484 = EDGE_CURVE ( 'NONE', #142228, #214061, #126064, .T. ) ;
#235483 = CARTESIAN_POINT ( 'NONE',  ( -23.25000000000000000, 1.115600667400684642E-11, -134.0000000000000284 ) ) ;
#235485 = DIRECTION ( 'NONE',  ( -0.000000000000000000, -0.000000000000000000, 1.000000000000000000 ) ) ;
#235486 = CONICAL_SURFACE ( 'NONE', #173203, 4.049999999999998046, 0.7853981633974604915 ) ;
#235487 = VECTOR ( 'NONE', #99126, 1000.000000000000000 ) ;
#235488 = CARTESIAN_POINT ( 'NONE',  ( -21.08134388332232589, 0.07581891751813461811, -60.66531941948206708 ) ) ;
#235489 = EDGE_CURVE ( 'NONE', #5569, #209893, #190568, .T. ) ;
#235490 = ORIENTED_EDGE ( 'NONE', *, *, #50718, .T. ) ;
#235491 = FACE_OUTER_BOUND ( 'NONE', #109792, .T. ) ;
#235492 = DIRECTION ( 'NONE',  ( 0.000000000000000000, 0.9654421110809058293, 0.2606175937108693996 ) ) ;
#235493 = FACE_OUTER_BOUND ( 'NONE', #231350, .T. ) ;
#235494 = ORIENTED_EDGE ( 'NONE', *, *, #91534, .T. ) ;
#235495 = DIRECTION ( 'NONE',  ( 0.000000000000000000, 0.000000000000000000, 1.000000000000000000 ) ) ;
#235496 = EDGE_LOOP ( 'NONE', ( #8992, #153957, #41025, #31898 ) ) ;
#235497 = FACE_OUTER_BOUND ( 'NONE', #126488, .T. ) ;
#235498 = VERTEX_POINT ( 'NONE', #112307 ) ;
#235499 = AXIS2_PLACEMENT_3D ( 'NONE', #93107, #250892, #207951 ) ;
#235500 = CIRCLE ( 'NONE', #210414, 0.1000000000000028644 ) ;
#235501 = DIRECTION ( 'NONE',  ( -1.000000000000000000, -0.000000000000000000, -0.000000000000000000 ) ) ;
#235502 = LINE ( 'NONE', #193829, #243664 ) ;
#235504 = ORIENTED_EDGE ( 'NONE', *, *, #148958, .T. ) ;
#235503 = CARTESIAN_POINT ( 'NONE',  ( 21.05000000000000071, 86.19075908668452257, -209.4719249499869136 ) ) ;
#235505 = EDGE_CURVE ( 'NONE', #62001, #230912, #251801, .T. ) ;
#235506 = DIRECTION ( 'NONE',  ( 0.000000000000000000, 0.000000000000000000, 1.000000000000000000 ) ) ;
#235507 = ORIENTED_EDGE ( 'NONE', *, *, #35591, .T. ) ;
#235508 = AXIS2_PLACEMENT_3D ( 'NONE', #57042, #216139, #45208 ) ;
#235509 = VECTOR ( 'NONE', #252438, 999.9999999999998863 ) ;
#235510 = LINE ( 'NONE', #121998, #52273 ) ;
#235511 = ORIENTED_EDGE ( 'NONE', *, *, #156272, .F. ) ;
#235512 = EDGE_CURVE ( 'NONE', #169023, #160394, #31509, .T. ) ;
#235513 = FACE_OUTER_BOUND ( 'NONE', #73028, .T. ) ;
#235514 = CARTESIAN_POINT ( 'NONE',  ( -20.94999999999999929, 11.63687328911530727, -194.1782407866749622 ) ) ;
#235515 = ORIENTED_EDGE ( 'NONE', *, *, #17880, .F. ) ;
#235516 = CARTESIAN_POINT ( 'NONE',  ( 21.04999999999999716, 10.20944177074079562, -228.0128234210401104 ) ) ;
#235517 = ORIENTED_EDGE ( 'NONE', *, *, #218500, .T. ) ;
#235518 = CARTESIAN_POINT ( 'NONE',  ( -17.11825945287481687, 65.95000000001152785, -48.67310748452439384 ) ) ;
#235519 = CARTESIAN_POINT ( 'NONE',  ( 18.39999999999999503, 8.212522512469059066, -212.1579332307740344 ) ) ;
#235520 = EDGE_CURVE ( 'NONE', #245302, #65949, #253072, .T. ) ;
#235521 = APPLICATION_CONTEXT ( 'automotive_design' ) ;
#235523 = ORIENTED_EDGE ( 'NONE', *, *, #43092, .T. ) ;
#235522 = PLANE ( 'NONE',  #72218 ) ;
#235524 = VECTOR ( 'NONE', #224541, 1000.000000000000000 ) ;
#235525 = CARTESIAN_POINT ( 'NONE',  ( -20.94999999999999929, 1.835341550235569663, -145.5551512925629822 ) ) ;
#235526 = DIRECTION ( 'NONE',  ( 0.000000000000000000, 0.000000000000000000, 1.000000000000000000 ) ) ;
#235527 = AXIS2_PLACEMENT_3D ( 'NONE', #176511, #215609, #214340 ) ;
#235528 = DIRECTION ( 'NONE',  ( -1.000000000000000000, 0.000000000000000000, 0.000000000000000000 ) ) ;
#235530 = CARTESIAN_POINT ( 'NONE',  ( -22.45372860728439690, 75.98507938046395793, -181.6729046192282340 ) ) ;
#235529 = CARTESIAN_POINT ( 'NONE',  ( 20.95512820512820440, 58.98414156600839675, -225.6766266970810477 ) ) ;
#235531 = CARTESIAN_POINT ( 'NONE',  ( -18.59999999999999787, -9.399999999988851940, -107.3820418481727046 ) ) ;
#235532 = AXIS2_PLACEMENT_3D ( 'NONE', #220081, #30895, #129938 ) ;
#235533 = DIRECTION ( 'NONE',  ( -0.000000000000000000, 1.000000000000000000, -0.000000000000000000 ) ) ;
#235534 = CARTESIAN_POINT ( 'NONE',  ( -20.90000000000000213, 11.49641995933507843, 1.885425182446133885 ) ) ;
#235535 = EDGE_CURVE ( 'NONE', #20407, #188235, #15795, .T. ) ;
#235536 = CARTESIAN_POINT ( 'NONE',  ( -21.14999999999999858, 69.45934304831089889, -136.5231074845243313 ) ) ;
#235537 = EDGE_LOOP ( 'NONE', ( #52672, #28261, #197495, #210060 ) ) ;
#235539 = ORIENTED_EDGE ( 'NONE', *, *, #99747, .T. ) ;
#235538 = CIRCLE ( 'NONE', #202245, 0.9750000000000036415 ) ;
#235540 = CARTESIAN_POINT ( 'NONE',  ( 18.42555734704286152, 85.49715836194906160, -162.9832769867893774 ) ) ;
#235542 = ORIENTED_EDGE ( 'NONE', *, *, #195, .F. ) ;
#235541 = LINE ( 'NONE', #77742, #216720 ) ;
#235543 = ORIENTED_EDGE ( 'NONE', *, *, #117094, .F. ) ;
#235544 = CARTESIAN_POINT ( 'NONE',  ( 18.49999999999996803, 43.30036367478129478, -245.0872390055602352 ) ) ;
#235545 = VERTEX_POINT ( 'NONE', #152736 ) ;
#235546 = CARTESIAN_POINT ( 'NONE',  ( 20.95289811251229750, 8.893168004458594567, -8.501809493918521810 ) ) ;
#235547 = TOROIDAL_SURFACE ( 'NONE', #135776, 4.149999999999999467, 0.1000000000000000056 ) ;
#235548 = VECTOR ( 'NONE', #28161, 1000.000000000000000 ) ;
#235549 = EDGE_LOOP ( 'NONE', ( #58189, #69704, #158024, #4961 ) ) ;
#235550 = DIRECTION ( 'NONE',  ( -1.000000000000000000, 2.952720810173289112E-16, 2.061873921506763405E-30 ) ) ;
#235552 = VERTEX_POINT ( 'NONE', #11933 ) ;
#235551 = VERTEX_POINT ( 'NONE', #131854 ) ;
#235553 = ORIENTED_EDGE ( 'NONE', *, *, #6834, .T. ) ;
#235554 = VERTEX_POINT ( 'NONE', #211397 ) ;
#235555 = ORIENTED_EDGE ( 'NONE', *, *, #137104, .T. ) ;
#235556 = DIRECTION ( 'NONE',  ( -1.000000000000000000, 0.000000000000000000, 0.000000000000000000 ) ) ;
#235557 = DIRECTION ( 'NONE',  ( 1.000000000000000000, 0.000000000000000000, 0.000000000000000000 ) ) ;
#235559 = ORIENTED_EDGE ( 'NONE', *, *, #214239, .F. ) ;
#235558 = CARTESIAN_POINT ( 'NONE',  ( 20.12500000000000000, 18.88320179786139619, -228.9684431863134932 ) ) ;
#235560 = AXIS2_PLACEMENT_3D ( 'NONE', #12981, #112068, #254113 ) ;
#235561 = DIRECTION ( 'NONE',  ( -0.000000000000000000, 0.000000000000000000, -1.000000000000000000 ) ) ;
#235562 = CARTESIAN_POINT ( 'NONE',  ( 12.29592348164038995, 12.60827992760467353, -214.9270390227368637 ) ) ;
#235564 = ORIENTED_EDGE ( 'NONE', *, *, #245727, .F. ) ;
#235563 = CARTESIAN_POINT ( 'NONE',  ( -16.94389599338511943, 60.88850954836924245, -221.0718225180464174 ) ) ;
#235565 = FACE_OUTER_BOUND ( 'NONE', #203076, .T. ) ;
#235566 = ORIENTED_EDGE ( 'NONE', *, *, #108841, .T. ) ;
#235567 = DIRECTION ( 'NONE',  ( -1.000000000000000000, -1.836970198721029934E-16, -0.000000000000000000 ) ) ;
#235569 = VERTEX_POINT ( 'NONE', #51000 ) ;
#235568 = DIRECTION ( 'NONE',  ( 0.000000000000000000, -1.000000000000000000, 0.000000000000000000 ) ) ;
#235570 = DIRECTION ( 'NONE',  ( 0.000000000000000000, 0.9126074666063770380, 0.4088369013363281068 ) ) ;
#235571 = CYLINDRICAL_SURFACE ( 'NONE', #74867, 0.5000000000000004441 ) ;
#235572 = EDGE_CURVE ( 'NONE', #219200, #79629, #13480, .T. ) ;
#235573 = LINE ( 'NONE', #16556, #31591 ) ;
#235574 = ORIENTED_EDGE ( 'NONE', *, *, #77080, .T. ) ;
#235576 = FACE_OUTER_BOUND ( 'NONE', #237503, .T. ) ;
#235575 = CARTESIAN_POINT ( 'NONE',  ( 21.14999999999999503, 76.10085836911117951, -181.7726746080137445 ) ) ;
#235577 = DIRECTION ( 'NONE',  ( 0.000000000000000000, -6.769652589177795712E-15, 1.000000000000000000 ) ) ;
#235578 = AXIS2_PLACEMENT_3D ( 'NONE', #212899, #34289, #92933 ) ;
#235579 = CARTESIAN_POINT ( 'NONE',  ( 21.14999999999999503, 11.65000000001116298, -67.10000000000005116 ) ) ;
#235580 = CIRCLE ( 'NONE', #210648, 0.09999999999999832634 ) ;
#235582 = CARTESIAN_POINT ( 'NONE',  ( 5.899999999999996803, -11.65000000000000036, 14.10000000000000142 ) ) ;
#235581 = AXIS2_PLACEMENT_3D ( 'NONE', #187559, #209665, #250077 ) ;
#235583 = ORIENTED_EDGE ( 'NONE', *, *, #108523, .T. ) ;
#235584 = ORIENTED_EDGE ( 'NONE', *, *, #221273, .T. ) ;
#235585 = CARTESIAN_POINT ( 'NONE',  ( -16.89268316805466341, 9.951721813242185632, -12.64424752145445296 ) ) ;
#235586 = CARTESIAN_POINT ( 'NONE',  ( -18.38204789744325396, 62.49951772298229713, -209.4458114573654655 ) ) ;
#235587 = VERTEX_POINT ( 'NONE', #210126 ) ;
#235588 = FACE_OUTER_BOUND ( 'NONE', #36042, .T. ) ;
#235589 = ORIENTED_EDGE ( 'NONE', *, *, #73852, .T. ) ;
#235590 = EDGE_CURVE ( 'NONE', #175208, #169080, #154040, .T. ) ;
#235591 = CARTESIAN_POINT ( 'NONE',  ( -21.14999999999999858, 78.57160958314655375, -238.9307242378722833 ) ) ;
#235592 = DIRECTION ( 'NONE',  ( 1.000000000000000000, 0.000000000000000000, 0.000000000000000000 ) ) ;
#235593 = EDGE_CURVE ( 'NONE', #236966, #28807, #46955, .T. ) ;
#235594 = VERTEX_POINT ( 'NONE', #255600 ) ;
#235595 = CARTESIAN_POINT ( 'NONE',  ( 20.85000000000000142, 6.933893972137497030, -70.78564583437358237 ) ) ;
#235596 = CIRCLE ( 'NONE', #181464, 0.1000000000000043771 ) ;
#235597 = EDGE_CURVE ( 'NONE', #175048, #230665, #52294, .T. ) ;
#235598 = ORIENTED_EDGE ( 'NONE', *, *, #40651, .F. ) ;
#235599 = ORIENTED_EDGE ( 'NONE', *, *, #62450, .T. ) ;
#235600 = EDGE_LOOP ( 'NONE', ( #36704, #227810, #210721 ) ) ;
#235601 = EDGE_CURVE ( 'NONE', #227912, #142813, #250508, .T. ) ;
#235602 = DIRECTION ( 'NONE',  ( -1.000000000000000000, 0.000000000000000000, 0.000000000000000000 ) ) ;
#235603 = CARTESIAN_POINT ( 'NONE',  ( 22.47110162079220785, 75.97120258721007247, -215.1730434212086891 ) ) ;
#235604 = CARTESIAN_POINT ( 'NONE',  ( -16.94389599338512298, 66.00880201025651672, -56.91546268271414988 ) ) ;
#235606 = EDGE_CURVE ( 'NONE', #206437, #83423, #67637, .T. ) ;
#235605 = DIRECTION ( 'NONE',  ( 0.000000000000000000, 0.6728388485993012091, -0.7397890806274222131 ) ) ;
#235607 = DIRECTION ( 'NONE',  ( 0.000000000000000000, 6.982962677686266711E-15, -1.000000000000000000 ) ) ;
#235609 = CARTESIAN_POINT ( 'NONE',  ( -20.85000000000000142, 11.65000000001115232, -100.5000000000000426 ) ) ;
#235608 = DIRECTION ( 'NONE',  ( 0.000000000000000000, 1.897661533703519897E-16, -1.000000000000000000 ) ) ;
#235611 = ORIENTED_EDGE ( 'NONE', *, *, #135709, .T. ) ;
#235610 = DIRECTION ( 'NONE',  ( -0.000000000000000000, -0.000000000000000000, -1.000000000000000000 ) ) ;
#235612 = CARTESIAN_POINT ( 'NONE',  ( 12.25000000000000000, 9.850000000011137402, -184.2499999999999716 ) ) ;
#235613 = VERTEX_POINT ( 'NONE', #179983 ) ;
#235614 = EDGE_CURVE ( 'NONE', #144975, #71927, #236086, .T. ) ;
#235615 = DIRECTION ( 'NONE',  ( 1.462545276649423285E-15, 0.1686199900910279881, -0.9856811345164833149 ) ) ;
#235616 = ORIENTED_EDGE ( 'NONE', *, *, #23990, .F. ) ;
#235617 = ORIENTED_EDGE ( 'NONE', *, *, #73368, .T. ) ;
#235618 = CARTESIAN_POINT ( 'NONE',  ( -16.93294127766158752, 65.99671989705664998, -48.59320021869516637 ) ) ;
#235619 = CARTESIAN_POINT ( 'NONE',  ( -21.05000000000000071, 6.257814610492680174, -133.9022097086908332 ) ) ;
#235620 = CARTESIAN_POINT ( 'NONE',  ( -16.87845715379269507, 66.04214188611454972, -56.89930683346550211 ) ) ;
#235621 = ORIENTED_EDGE ( 'NONE', *, *, #90496, .F. ) ;
#235622 = DIRECTION ( 'NONE',  ( 1.000000000000000000, 0.000000000000000000, 0.000000000000000000 ) ) ;
#235623 = EDGE_CURVE ( 'NONE', #53539, #68437, #146906, .T. ) ;
#235624 = AXIS2_PLACEMENT_3D ( 'NONE', #49850, #210236, #53703 ) ;
#235625 = AXIS2_PLACEMENT_3D ( 'NONE', #12170, #228646, #91681 ) ;
#235626 = FACE_OUTER_BOUND ( 'NONE', #39280, .T. ) ;
#235627 = ORIENTED_EDGE ( 'NONE', *, *, #103234, .T. ) ;
#235628 = ORIENTED_EDGE ( 'NONE', *, *, #83515, .T. ) ;
#235629 = DIRECTION ( 'NONE',  ( 1.000000000000000000, 2.952720810173289112E-16, -0.000000000000000000 ) ) ;
#235630 = ORIENTED_EDGE ( 'NONE', *, *, #102243, .F. ) ;
#235631 = CARTESIAN_POINT ( 'NONE',  ( -16.94107738177415712, 60.85118289042637940, -221.1214263997032106 ) ) ;
#235632 = DIRECTION ( 'NONE',  ( 0.000000000000000000, 0.000000000000000000, 1.000000000000000000 ) ) ;
#235633 = EDGE_LOOP ( 'NONE', ( #90044, #102246, #73576, #10237 ) ) ;
#235634 = ADVANCED_FACE ( 'NONE', ( #177436 ), #38, .F. ) ;
#235635 = FACE_OUTER_BOUND ( 'NONE', #32947, .T. ) ;
#235636 = CARTESIAN_POINT ( 'NONE',  ( -16.79140778683509794, 9.944941598865719712, -121.3297372337708282 ) ) ;
#235637 = DIRECTION ( 'NONE',  ( -1.000000000000000000, 0.000000000000000000, 0.000000000000000000 ) ) ;
#235638 = ORIENTED_EDGE ( 'NONE', *, *, #25132, .F. ) ;
#235639 = EDGE_CURVE ( 'NONE', #59214, #37771, #51037, .T. ) ;
#235640 = CARTESIAN_POINT ( 'NONE',  ( 18.49999999999999289, 69.35000000001151932, -48.37310748452436826 ) ) ;
#235641 = CARTESIAN_POINT ( 'NONE',  ( 21.05000000000000071, 76.00000000001173817, -73.52310748452431710 ) ) ;
#235642 = CARTESIAN_POINT ( 'NONE',  ( -22.50000000000000000, 25.98945013819915673, -254.2294471341345456 ) ) ;
#235643 = AXIS2_PLACEMENT_3D ( 'NONE', #56494, #13552, #31850 ) ;
#235644 = AXIS2_PLACEMENT_3D ( 'NONE', #60873, #238229, #2173 ) ;
#235645 = CIRCLE ( 'NONE', #23495, 0.1000000000000001860 ) ;
#235646 = ORIENTED_EDGE ( 'NONE', *, *, #255971, .F. ) ;
#235647 = ADVANCED_FACE ( 'NONE', ( #23499 ), #19623, .T. ) ;
#235648 = DIRECTION ( 'NONE',  ( 0.000000000000000000, -0.9770955615653301729, -0.2128009952263661964 ) ) ;
#235649 = ORIENTED_EDGE ( 'NONE', *, *, #86654, .F. ) ;
#235650 = FACE_OUTER_BOUND ( 'NONE', #227932, .T. ) ;
#235651 = DIRECTION ( 'NONE',  ( -1.000000000000000000, 0.000000000000000000, -0.000000000000000000 ) ) ;
#235652 = DIRECTION ( 'NONE',  ( 1.000000000000000000, 2.952720810173289112E-16, -0.000000000000000000 ) ) ;
#235653 = CARTESIAN_POINT ( 'NONE',  ( 21.03675099975492202, 67.12481996722777922, -191.1975653477463766 ) ) ;
#235654 = CARTESIAN_POINT ( 'NONE',  ( -18.59999999999999787, 74.25000000001186606, -91.35359592662267403 ) ) ;
#235655 = DIRECTION ( 'NONE',  ( 1.000000000000000000, 0.000000000000000000, -0.000000000000000000 ) ) ;
#235656 = ORIENTED_EDGE ( 'NONE', *, *, #177505, .F. ) ;
#235657 = DIRECTION ( 'NONE',  ( 0.000000000000000000, 0.000000000000000000, -1.000000000000000000 ) ) ;
#235658 = CARTESIAN_POINT ( 'NONE',  ( 21.09706851349342216, 67.22415748653864398, -124.2875412681247127 ) ) ;
#235659 = DIRECTION ( 'NONE',  ( 0.7071067811865487940, 4.851104656540973741E-15, -0.7071067811865463515 ) ) ;
#235660 = CARTESIAN_POINT ( 'NONE',  ( 20.94999999999999574, 1.162701749949165642, -108.6000000000000227 ) ) ;
#235661 = CIRCLE ( 'NONE', #169072, 0.09999999999999939493 ) ;
#235662 = CARTESIAN_POINT ( 'NONE',  ( 20.21494484322215968, 66.69682926214275653, -61.18284229275413821 ) ) ;
#235663 = EDGE_CURVE ( 'NONE', #238843, #170246, #113233, .T. ) ;
#235664 = AXIS2_PLACEMENT_3D ( 'NONE', #46545, #107819, #126083 ) ;
#235665 = EDGE_LOOP ( 'NONE', ( #240060, #96828, #198309, #246513, #234190, #82113, #177248, #214105, #21852, #66121, #213985, #3936, #83832, #178741, #241340, #40097 ) ) ;
#235666 = ORIENTED_EDGE ( 'NONE', *, *, #30353, .T. ) ;
#235667 = CARTESIAN_POINT ( 'NONE',  ( -21.14999999999999858, 64.25000000001161027, -62.73924182154625129 ) ) ;
#235668 = DIRECTION ( 'NONE',  ( 2.952720810173289112E-16, -1.000000000000000000, 0.000000000000000000 ) ) ;
#235669 = DIRECTION ( 'NONE',  ( -0.000000000000000000, -0.000000000000000000, -1.000000000000000000 ) ) ;
#235670 = FACE_OUTER_BOUND ( 'NONE', #147204, .T. ) ;
#235671 = DIRECTION ( 'NONE',  ( 0.000000000000000000, -0.2868887416115947775, 0.9579639084728169829 ) ) ;
#235672 = AXIS2_PLACEMENT_3D ( 'NONE', #3873, #57409, #79537 ) ;
#235673 = EDGE_CURVE ( 'NONE', #212292, #133095, #13651, .T. ) ;
#235674 = ORIENTED_EDGE ( 'NONE', *, *, #193075, .F. ) ;
#235675 = CARTESIAN_POINT ( 'NONE',  ( -23.15000000000000213, 1.115600667400684642E-11, -67.00000000000004263 ) ) ;
#235676 = CIRCLE ( 'NONE', #31716, 4.000000000000003553 ) ;
#235677 = CIRCLE ( 'NONE', #19209, 0.09999999999998898659 ) ;
#235678 = FACE_OUTER_BOUND ( 'NONE', #92478, .T. ) ;
#235679 = EDGE_CURVE ( 'NONE', #79652, #68241, #26145, .T. ) ;
#235680 = ORIENTED_EDGE ( 'NONE', *, *, #164164, .F. ) ;
#235682 = ADVANCED_FACE ( 'NONE', ( #20924 ), #239955, .T. ) ;
#235681 = CARTESIAN_POINT ( 'NONE',  ( -18.50000000000000000, 74.13328508995425636, -57.77043223824233564 ) ) ;
#235683 = CARTESIAN_POINT ( 'NONE',  ( -21.52071067811865746, 68.22071067813021727, -57.17310748452437963 ) ) ;
#235684 = EDGE_CURVE ( 'NONE', #162687, #46758, #205172, .T. ) ;
#235685 = VECTOR ( 'NONE', #109796, 1000.000000000000000 ) ;
#235686 = ORIENTED_EDGE ( 'NONE', *, *, #44126, .F. ) ;
#235688 = AXIS2_PLACEMENT_3D ( 'NONE', #218024, #79796, #57674 ) ;
#235687 = CARTESIAN_POINT ( 'NONE',  ( -18.37160782347004329, 64.52438358521023076, -194.2731074845244450 ) ) ;
#235689 = EDGE_CURVE ( 'NONE', #58739, #204353, #41767, .T. ) ;
#235690 = ORIENTED_EDGE ( 'NONE', *, *, #106139, .F. ) ;
#235691 = CARTESIAN_POINT ( 'NONE',  ( -20.54999999999999716, 2.000000000011154189, -154.2753780772379173 ) ) ;
#235692 = DIRECTION ( 'NONE',  ( -1.000000000000000000, -2.952720810173289112E-16, 0.000000000000000000 ) ) ;
#235693 = DIRECTION ( 'NONE',  ( -0.000000000000000000, 0.2617529984165031243, 0.9651348961777157509 ) ) ;
#235694 = CIRCLE ( 'NONE', #123281, 0.09999999999998898659 ) ;
#235695 = CARTESIAN_POINT ( 'NONE',  ( 20.94999999999999929, 74.88978653348847558, -233.9025578500150004 ) ) ;
#235696 = DIRECTION ( 'NONE',  ( 0.000000000000000000, -0.8814952561688430555, 0.4721928772777346239 ) ) ;
#235697 = CARTESIAN_POINT ( 'NONE',  ( -12.25000000000000178, 26.54497872210690090, -232.9592037335782209 ) ) ;
#235698 = DIRECTION ( 'NONE',  ( 0.000000000000000000, 0.000000000000000000, -1.000000000000000000 ) ) ;
#235699 = CARTESIAN_POINT ( 'NONE',  ( -23.25000000000000000, 87.65000000001212754, -133.4231074845242233 ) ) ;
#235700 = CARTESIAN_POINT ( 'NONE',  ( -20.85000000000000142, 1.115600667400684642E-11, -134.0000000000000284 ) ) ;
#235701 = DIRECTION ( 'NONE',  ( 0.000000000000000000, 0.000000000000000000, -1.000000000000000000 ) ) ;
#235702 = CARTESIAN_POINT ( 'NONE',  ( 21.12400222705899822, 22.07230102378213132, -231.7788474567792889 ) ) ;
#235703 = DIRECTION ( 'NONE',  ( 1.000000000000000000, 1.734723475976817507E-14, 0.000000000000000000 ) ) ;
#235704 = CARTESIAN_POINT ( 'NONE',  ( -20.65000000000000568, 7.250000000011138646, -87.85000000000003695 ) ) ;
#235705 = CARTESIAN_POINT ( 'NONE',  ( 21.06280952165552378, 10.62713230061206460, -79.20405388677831127 ) ) ;
#235706 = CARTESIAN_POINT ( 'NONE',  ( 20.87155475150661132, 56.12642167632806434, -227.9547677828175551 ) ) ;
#235707 = EDGE_CURVE ( 'NONE', #202898, #218982, #217787, .T. ) ;
#235708 = EDGE_LOOP ( 'NONE', ( #92839, #40471, #48203 ) ) ;
#235709 = CARTESIAN_POINT ( 'NONE',  ( 18.59999999999999076, 80.82423061532404063, -192.8091306798888525 ) ) ;
#235710 = DIRECTION ( 'NONE',  ( 1.000000000000000000, 0.000000000000000000, 0.000000000000000000 ) ) ;
#235711 = CYLINDRICAL_SURFACE ( 'NONE', #2060, 0.5000000000000008882 ) ;
#235712 = ADVANCED_FACE ( 'NONE', ( #161714 ), #80250, .T. ) ;
#235713 = EDGE_CURVE ( 'NONE', #184497, #151457, #62596, .T. ) ;
#235714 = VERTEX_POINT ( 'NONE', #45597 ) ;
#235715 = CARTESIAN_POINT ( 'NONE',  ( -20.54999999999999716, -9.499999999988848032, -143.8939691226524644 ) ) ;
#235716 = VECTOR ( 'NONE', #88563, 1000.000000000000000 ) ;
#235717 = AXIS2_PLACEMENT_3D ( 'NONE', #128711, #208254, #71319 ) ;
#235718 = FACE_OUTER_BOUND ( 'NONE', #55663, .T. ) ;
#235719 = EDGE_LOOP ( 'NONE', ( #191796, #246148, #239851 ) ) ;
#235721 = CIRCLE ( 'NONE', #65041, 4.049999999999998046 ) ;
#235720 = CARTESIAN_POINT ( 'NONE',  ( 21.05000000000000071, 7.872214528623314500, -209.6555322433423498 ) ) ;
#235722 = DIRECTION ( 'NONE',  ( 0.000000000000000000, 0.000000000000000000, -1.000000000000000000 ) ) ;
#235723 = AXIS2_PLACEMENT_3D ( 'NONE', #150512, #69700, #7121 ) ;
#235724 = VECTOR ( 'NONE', #30940, 1000.000000000000000 ) ;
#235725 = ORIENTED_EDGE ( 'NONE', *, *, #241334, .T. ) ;
#235726 = CYLINDRICAL_SURFACE ( 'NONE', #72855, 0.4999999999999944489 ) ;
#235727 = ORIENTED_EDGE ( 'NONE', *, *, #152435, .T. ) ;
#235729 = AXIS2_PLACEMENT_3D ( 'NONE', #52770, #95743, #132318 ) ;
#235728 = CARTESIAN_POINT ( 'NONE',  ( 20.94999999999999929, 85.40000000001262492, -193.6291383618718385 ) ) ;
#235730 = DIRECTION ( 'NONE',  ( 0.000000000000000000, 0.8814952561688438326, -0.4721928772777331806 ) ) ;
#235732 = DIRECTION ( 'NONE',  ( 5.603264701231746180E-32, -0.2617529984165030132, -0.9651348961777158619 ) ) ;
#235731 = PRODUCT_DEFINITION_CONTEXT ( 'detailed design', #152560, 'design' ) ;
#235733 = DIRECTION ( 'NONE',  ( 0.000000000000000000, -0.2128009952263603954, 0.9770955615653315052 ) ) ;
#235734 = CARTESIAN_POINT ( 'NONE',  ( -16.81930730667006912, 9.936998068874046908, -12.72676773053820476 ) ) ;
#235735 = EDGE_CURVE ( 'NONE', #26629, #23601, #213368, .T. ) ;
#235736 = CARTESIAN_POINT ( 'NONE',  ( 21.05000000000000071, 63.38977744132975545, -224.6138528564904107 ) ) ;
#235737 = AXIS2_PLACEMENT_3D ( 'NONE', #25299, #146490, #143934 ) ;
#235738 = CARTESIAN_POINT ( 'NONE',  ( 18.39999999999999503, 70.35000000001261355, -190.8731074845244109 ) ) ;
#235739 = CARTESIAN_POINT ( 'NONE',  ( 20.94999999999999929, 1.115600667400684642E-11, -100.5000000000000426 ) ) ;
#235741 = EDGE_LOOP ( 'NONE', ( #57071, #165985, #222714, #103729 ) ) ;
#235740 = PLANE ( 'NONE',  #102680 ) ;
#235742 = ORIENTED_EDGE ( 'NONE', *, *, #255069, .T. ) ;
#235744 = LINE ( 'NONE', #79223, #201852 ) ;
#235743 = CARTESIAN_POINT ( 'NONE',  ( -21.05000000000000071, 11.60000000001115517, -160.5717967697245285 ) ) ;
#235746 = VERTEX_POINT ( 'NONE', #44322 ) ;
#235745 = DIRECTION ( 'NONE',  ( 1.000000000000000000, 0.000000000000000000, 0.000000000000000000 ) ) ;
#235747 = EDGE_LOOP ( 'NONE', ( #63206, #34513, #148012, #173692 ) ) ;
#235748 = DIRECTION ( 'NONE',  ( 0.000000000000000000, -0.8660254037844377084, -0.5000000000000016653 ) ) ;
#235749 = CARTESIAN_POINT ( 'NONE',  ( 23.14999999999999147, 5.169232899390497238, -237.3909066255399978 ) ) ;
#235750 = CARTESIAN_POINT ( 'NONE',  ( 20.85000000106584750, 62.86809779110724605, -207.0533710558942744 ) ) ;
#235751 = DIRECTION ( 'NONE',  ( -1.000000000000000000, -0.000000000000000000, -0.000000000000000000 ) ) ;
#235753 = DIRECTION ( 'NONE',  ( -1.000000000000000000, -2.952720810173289112E-16, 0.000000000000000000 ) ) ;
#235752 = CIRCLE ( 'NONE', #243953, 0.1000000000000028644 ) ;
#235754 = CARTESIAN_POINT ( 'NONE',  ( 21.05000000000000071, 5.400000000011154988, -90.60603087734760663 ) ) ;
#235755 = CARTESIAN_POINT ( 'NONE',  ( -20.94999999999999929, 5.850000000011160495, -56.86750277572207324 ) ) ;
#235756 = EDGE_CURVE ( 'NONE', #86585, #180491, #154464, .T. ) ;
#235757 = CARTESIAN_POINT ( 'NONE',  ( 20.99999999999999645, 9.750000000011137757, -76.25000000000004263 ) ) ;
#235758 = EDGE_LOOP ( 'NONE', ( #211084, #127070, #20265 ) ) ;
#235759 = ORIENTED_EDGE ( 'NONE', *, *, #158015, .F. ) ;
#235760 = ADVANCED_FACE ( 'NONE', ( #46853 ), #228092, .F. ) ;
#235761 = CARTESIAN_POINT ( 'NONE',  ( -21.04999999999994387, 66.15000000001120384, -4.623107484524796362 ) ) ;
#235762 = CIRCLE ( 'NONE', #56666, 0.4000000000000114575 ) ;
#235763 = AXIS2_PLACEMENT_3D ( 'NONE', #181093, #127523, #183652 ) ;
#235764 = ORIENTED_EDGE ( 'NONE', *, *, #121476, .F. ) ;
#235765 = AXIS2_PLACEMENT_3D ( 'NONE', #80836, #182545, #199547 ) ;
#235767 = CARTESIAN_POINT ( 'NONE',  ( 18.59999999999999076, 77.83585931145570669, -125.0186683157258329 ) ) ;
#235766 = VECTOR ( 'NONE', #122399, 1000.000000000000000 ) ;
#235768 = EDGE_LOOP ( 'NONE', ( #90431, #222567, #3869, #27122 ) ) ;
#235769 = CARTESIAN_POINT ( 'NONE',  ( -16.94226253665224391, 14.09585617079101461, -218.9651344997973581 ) ) ;
#235770 = ADVANCED_FACE ( 'NONE', ( #128990 ), #208535, .F. ) ;
#235771 = EDGE_CURVE ( 'NONE', #178818, #4626, #176005, .T. ) ;
#235772 = CARTESIAN_POINT ( 'NONE',  ( -18.69999999999999929, 1.149999999999999911, -15.00000000000000000 ) ) ;
#235773 = CARTESIAN_POINT ( 'NONE',  ( -23.25000000000000000, -11.64999999998884483, -70.10000000000005116 ) ) ;
#235775 = VERTEX_POINT ( 'NONE', #29907 ) ;
#235774 = DIRECTION ( 'NONE',  ( 1.000000000000000000, 0.000000000000000000, 0.000000000000000000 ) ) ;
#235776 = CARTESIAN_POINT ( 'NONE',  ( 21.05000000000000071, 77.73625713160970463, -158.4544551555068495 ) ) ;
#235777 = ORIENTED_EDGE ( 'NONE', *, *, #24690, .T. ) ;
#235778 = CARTESIAN_POINT ( 'NONE',  ( -23.24999999999999645, 77.27075167199318173, -241.8768735168259241 ) ) ;
#235779 = DIRECTION ( 'NONE',  ( 0.000000000000000000, 0.000000000000000000, 1.000000000000000000 ) ) ;
#235780 = DIRECTION ( 'NONE',  ( 0.000000000000000000, 1.000000000000000000, 0.000000000000000000 ) ) ;
#235781 = CARTESIAN_POINT ( 'NONE',  ( -22.37643362114956602, 75.90091862633136088, -211.1488974784827519 ) ) ;
#235782 = VECTOR ( 'NONE', #30095, 1000.000000000000227 ) ;
#235783 = DIRECTION ( 'NONE',  ( 0.000000000000000000, 0.000000000000000000, 1.000000000000000000 ) ) ;
#235784 = ORIENTED_EDGE ( 'NONE', *, *, #174221, .F. ) ;
#235785 = AXIS2_PLACEMENT_3D ( 'NONE', #241407, #221801, #204818 ) ;
#235786 = DIRECTION ( 'NONE',  ( 0.000000000000000000, -0.9126074666063767049, -0.4088369013363286619 ) ) ;
#235787 = VERTEX_POINT ( 'NONE', #123856 ) ;
#235790 = ORIENTED_EDGE ( 'NONE', *, *, #168038, .F. ) ;
#235789 = DIRECTION ( 'NONE',  ( -0.000000000000000000, -6.982962677686266711E-15, 1.000000000000000000 ) ) ;
#235788 = DIRECTION ( 'NONE',  ( 1.000000000000000000, 0.000000000000000000, 0.000000000000000000 ) ) ;
#235791 = EDGE_CURVE ( 'NONE', #204355, #173321, #127707, .T. ) ;
#235792 = DIRECTION ( 'NONE',  ( 0.000000000000000000, -0.9651348961777379554, 0.2617529984164210233 ) ) ;
#235793 = ADVANCED_FACE ( 'NONE', ( #186402 ), #164271, .F. ) ;
#235794 = DIRECTION ( 'NONE',  ( 0.000000000000000000, 0.000000000000000000, -1.000000000000000000 ) ) ;
#235795 = AXIS2_PLACEMENT_3D ( 'NONE', #37222, #617, #80141 ) ;
#235796 = EDGE_LOOP ( 'NONE', ( #180857, #9322, #98970, #84792 ) ) ;
#235797 = FACE_OUTER_BOUND ( 'NONE', #35218, .T. ) ;
#235798 = FACE_OUTER_BOUND ( 'NONE', #77072, .T. ) ;
#235799 = CARTESIAN_POINT ( 'NONE',  ( -17.11825945287482753, 10.04999999999998295, -12.65000000000000391 ) ) ;
#235801 = ORIENTED_EDGE ( 'NONE', *, *, #64395, .F. ) ;
#235800 = DIRECTION ( 'NONE',  ( -1.000000000000000000, 0.000000000000000000, 0.000000000000000000 ) ) ;
#235802 = DIRECTION ( 'NONE',  ( 0.000000000000000000, 0.000000000000000000, 1.000000000000000000 ) ) ;
#235803 = EDGE_CURVE ( 'NONE', #126699, #195545, #188428, .T. ) ;
#235804 = VERTEX_POINT ( 'NONE', #48152 ) ;
#235806 = EDGE_CURVE ( 'NONE', #135120, #84465, #234217, .T. ) ;
#235805 = CARTESIAN_POINT ( 'NONE',  ( 18.59999999999999787, 1.851028230152016674, -78.65391326942254580 ) ) ;
#235807 = FACE_OUTER_BOUND ( 'NONE', #209649, .T. ) ;
#235808 = PLANE ( 'NONE',  #37871 ) ;
#235809 = AXIS2_PLACEMENT_3D ( 'NONE', #152539, #228198, #189065 ) ;
#235810 = ORIENTED_EDGE ( 'NONE', *, *, #94417, .T. ) ;
#235811 = CARTESIAN_POINT ( 'NONE',  ( -16.86337532320261801, 66.02003279578794093, -157.4720319535072406 ) ) ;
#235812 = ORIENTED_EDGE ( 'NONE', *, *, #234211, .F. ) ;
#235813 = DIRECTION ( 'NONE',  ( -1.000000000000000000, -8.673617379884087537E-15, 0.000000000000000000 ) ) ;
#235814 = CARTESIAN_POINT ( 'NONE',  ( -18.79999999999999716, 10.31653824539117714, -11.82383137372478110 ) ) ;
#235815 = LINE ( 'NONE', #19348, #164379 ) ;
#235816 = ORIENTED_EDGE ( 'NONE', *, *, #16877, .F. ) ;
#235817 = EDGE_CURVE ( 'NONE', #142182, #64792, #125144, .T. ) ;
#235818 = LINE ( 'NONE', #157617, #150450 ) ;
#235819 = CARTESIAN_POINT ( 'NONE',  ( -21.52071067811865746, 7.779289321892505882, -121.6500000000000341 ) ) ;
#235820 = VERTEX_POINT ( 'NONE', #183817 ) ;
#235821 = AXIS2_PLACEMENT_3D ( 'NONE', #45826, #203617, #184049 ) ;
#235822 = EDGE_CURVE ( 'NONE', #123266, #222515, #21856, .T. ) ;
#235823 = DIRECTION ( 'NONE',  ( -1.000000000000000000, 0.000000000000000000, -0.000000000000000000 ) ) ;
#235824 = DIRECTION ( 'NONE',  ( 1.000000000000000000, -0.000000000000000000, -0.000000000000000000 ) ) ;
#235825 = CARTESIAN_POINT ( 'NONE',  ( -18.40000000000000213, 32.67104411594546320, -237.4063322638886859 ) ) ;
#235826 = AXIS2_PLACEMENT_3D ( 'NONE', #11187, #51554, #111570 ) ;
#235827 = AXIS2_PLACEMENT_3D ( 'NONE', #113029, #233001, #157318 ) ;
#235828 = ORIENTED_EDGE ( 'NONE', *, *, #57024, .T. ) ;
#235829 = DIRECTION ( 'NONE',  ( 0.000000000000000000, 0.000000000000000000, -1.000000000000000000 ) ) ;
#235830 = ORIENTED_EDGE ( 'NONE', *, *, #227766, .F. ) ;
#235832 = ORIENTED_EDGE ( 'NONE', *, *, #159720, .F. ) ;
#235831 = CARTESIAN_POINT ( 'NONE',  ( 22.40000000000010161, 25.93539162822990818, -254.3551732743596574 ) ) ;
#235833 = EDGE_CURVE ( 'NONE', #199092, #157944, #5147, .T. ) ;
#235836 = EDGE_LOOP ( 'NONE', ( #215057, #222421, #108457, #118520 ) ) ;
#235835 = EDGE_LOOP ( 'NONE', ( #181709, #7951, #61721, #81010 ) ) ;
#235834 = DIRECTION ( 'NONE',  ( 1.000000000000000000, 0.000000000000000000, 0.000000000000000000 ) ) ;
#235837 = DIRECTION ( 'NONE',  ( -0.000000000000000000, 0.3896596508880124654, 0.9209589331071350582 ) ) ;
#235838 = CARTESIAN_POINT ( 'NONE',  ( -21.08134388332232589, 0.07581891751813138458, -161.1653194194820173 ) ) ;
#235839 = CARTESIAN_POINT ( 'NONE',  ( -18.59999999999999787, 52.27009174976920747, -232.4217594817395138 ) ) ;
#235840 = CARTESIAN_POINT ( 'NONE',  ( -16.77180007708459897, 12.41097209739636398, -211.2288325707822594 ) ) ;
#235841 = LINE ( 'NONE', #152496, #115858 ) ;
#235842 = VECTOR ( 'NONE', #97067, 1000.000000000000000 ) ;
#235843 = DIRECTION ( 'NONE',  ( 1.000000000000000000, 7.304098846218133681E-16, -4.217023435051677501E-16 ) ) ;
#235844 = PLANE ( 'NONE',  #130597 ) ;
#235845 = FACE_OUTER_BOUND ( 'NONE', #241040, .T. ) ;
#235847 = ORIENTED_EDGE ( 'NONE', *, *, #24399, .F. ) ;
#235846 = CIRCLE ( 'NONE', #11000, 0.09999999999999939493 ) ;
#235848 = ORIENTED_EDGE ( 'NONE', *, *, #161702, .T. ) ;
#235849 = ORIENTED_EDGE ( 'NONE', *, *, #187557, .F. ) ;
#235850 = CARTESIAN_POINT ( 'NONE',  ( 20.94999999999999929, 7.120270961708750512, -104.1595630418393768 ) ) ;
#235852 = EDGE_LOOP ( 'NONE', ( #229714, #184071, #73604 ) ) ;
#235851 = CARTESIAN_POINT ( 'NONE',  ( -17.01825945287482966, 10.05000000001113847, -146.6500000000000341 ) ) ;
#235854 = CARTESIAN_POINT ( 'NONE',  ( -18.34374000495060386, 58.57934086597919077, -223.9244941873113817 ) ) ;
#235853 = AXIS2_PLACEMENT_3D ( 'NONE', #253053, #95270, #34054 ) ;
#235855 = VERTEX_POINT ( 'NONE', #105526 ) ;
#235856 = CARTESIAN_POINT ( 'NONE',  ( 23.14999999999999858, 67.23127455305835554, -235.8551265064784559 ) ) ;
#235857 = ORIENTED_EDGE ( 'NONE', *, *, #163974, .T. ) ;
#235858 = CARTESIAN_POINT ( 'NONE',  ( 18.54999999999999716, 9.950000000011153034, -113.1499999999999773 ) ) ;
#235859 = AXIS2_PLACEMENT_3D ( 'NONE', #172758, #230111, #232705 ) ;
#235860 = VERTEX_POINT ( 'NONE', #243792 ) ;
#235861 = DIRECTION ( 'NONE',  ( -1.000000000000000000, 0.000000000000000000, -0.000000000000000000 ) ) ;
#235862 = LINE ( 'NONE', #136760, #82141 ) ;
#235865 = VERTEX_POINT ( 'NONE', #26042 ) ;
#235864 = VERTEX_POINT ( 'NONE', #84675 ) ;
#235863 = TOROIDAL_SURFACE ( 'NONE', #11026, 4.149999999999999467, 0.1000000000000000056 ) ;
#235866 = ORIENTED_EDGE ( 'NONE', *, *, #117581, .T. ) ;
#235867 = DIRECTION ( 'NONE',  ( -4.336808689942053235E-15, -0.8660254037844482555, -0.4999999999999836797 ) ) ;
#235868 = VECTOR ( 'NONE', #248446, 1000.000000000000000 ) ;
#235869 = VERTEX_POINT ( 'NONE', #168154 ) ;
#235870 = AXIS2_PLACEMENT_3D ( 'NONE', #36240, #115751, #195318 ) ;
#235871 = ORIENTED_EDGE ( 'NONE', *, *, #136931, .T. ) ;
#235872 = CARTESIAN_POINT ( 'NONE',  ( 20.84999999999999432, 43.08613539620618837, -254.3146655184800409 ) ) ;
#235873 = EDGE_LOOP ( 'NONE', ( #241079, #85760, #179307, #107227 ) ) ;
#235874 = VECTOR ( 'NONE', #64883, 1000.000000000000000 ) ;
#235876 = DIRECTION ( 'NONE',  ( 0.000000000000000000, 0.4999999999999478195, 0.8660254037844686836 ) ) ;
#235875 = FACE_OUTER_BOUND ( 'NONE', #175949, .T. ) ;
#235877 = CARTESIAN_POINT ( 'NONE',  ( 20.95000000000005258, 64.35000000001120668, -30.12310748452479103 ) ) ;
#235878 = DIRECTION ( 'NONE',  ( 0.000000000000000000, 0.000000000000000000, 1.000000000000000000 ) ) ;
#235879 = DIRECTION ( 'NONE',  ( 0.000000000000000000, 1.084202172485510997E-13, -1.000000000000000000 ) ) ;
#235880 = VERTEX_POINT ( 'NONE', #65145 ) ;
#235881 = ORIENTED_EDGE ( 'NONE', *, *, #9299, .T. ) ;
#235882 = LINE ( 'NONE', #117237, #33072 ) ;
#235883 = CARTESIAN_POINT ( 'NONE',  ( 21.05000000000000071, 76.00000000001170974, -69.52310748452431710 ) ) ;
#235884 = EDGE_CURVE ( 'NONE', #158228, #117707, #92757, .T. ) ;
#235885 = VECTOR ( 'NONE', #193862, 1000.000000000000000 ) ;
#235886 = ORIENTED_EDGE ( 'NONE', *, *, #18183, .T. ) ;
#235887 = FACE_OUTER_BOUND ( 'NONE', #155787, .T. ) ;
#235888 = DIRECTION ( 'NONE',  ( 1.000000000000000000, 0.000000000000000000, 0.000000000000000000 ) ) ;
#235889 = DIRECTION ( 'NONE',  ( 0.000000000000000000, -1.000000000000000000, 3.469446951953614189E-14 ) ) ;
#235890 = ORIENTED_EDGE ( 'NONE', *, *, #179557, .F. ) ;
#235891 = ORIENTED_EDGE ( 'NONE', *, *, #103332, .F. ) ;
#235892 = CARTESIAN_POINT ( 'NONE',  ( 21.05000000000000071, 85.40000000001221281, -146.4170766071767389 ) ) ;
#235893 = ADVANCED_FACE ( 'NONE', ( #251483 ), #63528, .T. ) ;
#235894 = CARTESIAN_POINT ( 'NONE',  ( 23.14999999999999858, 5.950000000011160139, -190.6942976949651438 ) ) ;
#235895 = ORIENTED_EDGE ( 'NONE', *, *, #172099, .F. ) ;
#235896 = DIRECTION ( 'NONE',  ( -1.000000000000000000, 1.335000415235278971E-16, -2.979993593738921214E-16 ) ) ;
#235897 = ORIENTED_EDGE ( 'NONE', *, *, #252395, .T. ) ;
#235898 = DIRECTION ( 'NONE',  ( 0.000000000000000000, -6.853228547068871147E-15, 1.000000000000000000 ) ) ;
#235899 = CARTESIAN_POINT ( 'NONE',  ( -18.50000000000000000, 3.912899247244609580, -178.9818229730109351 ) ) ;
#235901 = CARTESIAN_POINT ( 'NONE',  ( -22.59999999999999787, 55.86495732666938352, -232.8769840133977880 ) ) ;
#235900 = CARTESIAN_POINT ( 'NONE',  ( 18.59999999999999076, 1.750000000011155743, -112.1695115579016857 ) ) ;
#235902 = AXIS2_PLACEMENT_3D ( 'NONE', #122269, #92114, #12611 ) ;
#235903 = ADVANCED_FACE ( 'NONE', ( #250211 ), #34520, .T. ) ;
#235904 = DIRECTION ( 'NONE',  ( 2.694716079187273439E-16, 1.000000000000000000, 6.467318590049456648E-15 ) ) ;
#235905 = CIRCLE ( 'NONE', #15358, 0.1000000000000002831 ) ;
#235906 = DIRECTION ( 'NONE',  ( 1.000000000000000000, 2.952720810173289112E-16, -0.000000000000000000 ) ) ;
#235907 = AXIS2_PLACEMENT_3D ( 'NONE', #5615, #163443, #137764 ) ;
#235908 = VECTOR ( 'NONE', #60376, 1000.000000000000000 ) ;
#235909 = DIRECTION ( 'NONE',  ( -1.000000000000000000, -0.000000000000000000, -0.000000000000000000 ) ) ;
#235910 = VECTOR ( 'NONE', #75828, 1000.000000000000114 ) ;
#235912 = ORIENTED_EDGE ( 'NONE', *, *, #116822, .T. ) ;
#235911 = ORIENTED_EDGE ( 'NONE', *, *, #235484, .F. ) ;
#235913 = EDGE_LOOP ( 'NONE', ( #178322, #108199, #65050, #55008 ) ) ;
#235914 = EDGE_CURVE ( 'NONE', #8981, #160733, #180266, .T. ) ;
#235915 = DIRECTION ( 'NONE',  ( 0.000000000000000000, 0.000000000000000000, -1.000000000000000000 ) ) ;
#235916 = DIRECTION ( 'NONE',  ( 0.000000000000000000, -0.4930308989875575865, -0.8700118002898125091 ) ) ;
#235917 =( BOUNDED_CURVE ( )  B_SPLINE_CURVE ( 3, ( #2674, #215314, #77084, #18399 ),
 .UNSPECIFIED., .F., .F. ) 
 B_SPLINE_CURVE_WITH_KNOTS ( ( 4, 4 ),
 ( 4.712388980384689674, 6.283185307179586232 ),
 .UNSPECIFIED. ) 
 CURVE ( )  GEOMETRIC_REPRESENTATION_ITEM ( )  RATIONAL_B_SPLINE_CURVE ( ( 1.000000000000000000, 0.8047378541243649375, 0.8047378541243649375, 1.000000000000000000 ) ) 
 REPRESENTATION_ITEM ( '' )  );
#235919 = EDGE_CURVE ( 'NONE', #95294, #188149, #172001, .T. ) ;
#235918 = CARTESIAN_POINT ( 'NONE',  ( 23.14999999999999147, 4.054946580507614584, -200.1168758698121053 ) ) ;
#235920 = CARTESIAN_POINT ( 'NONE',  ( -20.64999999999999858, 71.65000000001228386, -157.6731074845243938 ) ) ;
#235921 = AXIS2_PLACEMENT_3D ( 'NONE', #127197, #227568, #85456 ) ;
#235923 = DIRECTION ( 'NONE',  ( 0.000000000000000000, 0.000000000000000000, -1.000000000000000000 ) ) ;
#235922 = CARTESIAN_POINT ( 'NONE',  ( 21.05000000000000071, -8.663551401857999323, -191.4758988819326646 ) ) ;
#235924 = CARTESIAN_POINT ( 'NONE',  ( -16.78493211734303259, 66.05416425680736836, -48.68705650362843329 ) ) ;
#235925 = ORIENTED_EDGE ( 'NONE', *, *, #146571, .F. ) ;
#235926 = EDGE_CURVE ( 'NONE', #47961, #226140, #84331, .T. ) ;
#235927 = AXIS2_PLACEMENT_3D ( 'NONE', #188226, #9578, #30454 ) ;
#235928 = ORIENTED_EDGE ( 'NONE', *, *, #49886, .F. ) ;
#235929 = ORIENTED_EDGE ( 'NONE', *, *, #27637, .F. ) ;
#235930 = CARTESIAN_POINT ( 'NONE',  ( 18.59999999999999787, 76.00000000001165290, -69.52310748452431710 ) ) ;
#235931 = AXIS2_PLACEMENT_3D ( 'NONE', #66676, #9261, #225715 ) ;
#235932 = LINE ( 'NONE', #241100, #156019 ) ;
#235933 = CARTESIAN_POINT ( 'NONE',  ( 23.24999999999999289, 13.96869538424789070, -210.3925794786331949 ) ) ;
#235934 = CARTESIAN_POINT ( 'NONE',  ( 23.15000000000000213, -9.000000000000000000, -23.60603087734755690 ) ) ;
#235935 = DIRECTION ( 'NONE',  ( -1.000000000000000000, -0.000000000000000000, -0.000000000000000000 ) ) ;
#235936 = ORIENTED_EDGE ( 'NONE', *, *, #98678, .T. ) ;
#235938 = ORIENTED_EDGE ( 'NONE', *, *, #73038, .T. ) ;
#235937 = ADVANCED_FACE ( 'NONE', ( #213647 ), #181110, .T. ) ;
#235939 = DIRECTION ( 'NONE',  ( 0.000000000000000000, 0.000000000000000000, -1.000000000000000000 ) ) ;
#235940 = CYLINDRICAL_SURFACE ( 'NONE', #119778, 0.1000000000000028644 ) ;
#235941 = EDGE_LOOP ( 'NONE', ( #218092, #169424, #77433 ) ) ;
#235942 = DIRECTION ( 'NONE',  ( 0.000000000000000000, -1.000000000000000000, -6.982962677686265922E-15 ) ) ;
#235943 = DIRECTION ( 'NONE',  ( 1.186688945009010077E-16, -1.000000000000000000, -0.000000000000000000 ) ) ;
#235944 = DIRECTION ( 'NONE',  ( -1.000000000000000000, -0.000000000000000000, -0.000000000000000000 ) ) ;
#235945 = CARTESIAN_POINT ( 'NONE',  ( 20.95512820512820440, 67.12384868372339497, -48.27310748452438105 ) ) ;
#235946 = DIRECTION ( 'NONE',  ( 0.000000000000000000, -1.000000000000000000, -6.982962677686266711E-15 ) ) ;
#235947 = B_SPLINE_CURVE_WITH_KNOTS ( 'NONE', 3,
 ( #115084, #197173, #193353, #14727, #214187, #58924, #78506, #16009, #75959, #95513, #175108, #235039, #215458 ),
 .UNSPECIFIED., .F., .F.,
 ( 4, 3, 3, 3, 4 ),
 ( -3.224855718277970714E-06, -8.470329472543003391E-22, 6.199515528667107161E-06, 4.034952380127394394E-05, 7.452715123699289962E-05 ),
 .UNSPECIFIED. ) ;
#235949 = CARTESIAN_POINT ( 'NONE',  ( -18.59999999999999787, -1.736705739467587772, -45.01742258762372728 ) ) ;
#235948 = CARTESIAN_POINT ( 'NONE',  ( -22.48479450179659977, 0.04699158118688477603, 11.64999844625161352 ) ) ;
#235950 = DIRECTION ( 'NONE',  ( 0.000000000000000000, -0.2617529984165031243, -0.9651348961777157509 ) ) ;
#235951 = EDGE_CURVE ( 'NONE', #239047, #126429, #100728, .T. ) ;
#235952 = CARTESIAN_POINT ( 'NONE',  ( 21.04999999999999716, 65.31569084252653568, -61.99641069419754302 ) ) ;
#235953 = CARTESIAN_POINT ( 'NONE',  ( 21.07928932188134397, 1.115600667400684642E-11, -134.0000000000000000 ) ) ;
#235954 = CARTESIAN_POINT ( 'NONE',  ( 18.59999999999998366, 76.00000000001213607, -136.5231074845243313 ) ) ;
#235955 = AXIS2_PLACEMENT_3D ( 'NONE', #211914, #176642, #56633 ) ;
#235958 = ORIENTED_EDGE ( 'NONE', *, *, #31454, .T. ) ;
#235957 = VECTOR ( 'NONE', #192323, 999.9999999999998863 ) ;
#235956 = CARTESIAN_POINT ( 'NONE',  ( 23.24999999999999645, 76.00000000001195133, -103.0231074845243171 ) ) ;
#235959 = AXIS2_PLACEMENT_3D ( 'NONE', #98451, #257510, #196306 ) ;
#235960 = TOROIDAL_SURFACE ( 'NONE', #85906, 0.2000000000000000111, 0.1000000000000000056 ) ;
#235961 = CARTESIAN_POINT ( 'NONE',  ( -20.64999999999999858, 74.07476635515247665, -157.2928639513982318 ) ) ;
#235962 = ORIENTED_EDGE ( 'NONE', *, *, #117433, .T. ) ;
#235963 = DIRECTION ( 'NONE',  ( 0.000000000000000000, -0.9654727137038715545, 0.2605042016806676242 ) ) ;
#235964 = ORIENTED_EDGE ( 'NONE', *, *, #1272, .F. ) ;
#235965 = DIRECTION ( 'NONE',  ( 1.652117596168391700E-15, 1.000000000000000000, -0.000000000000000000 ) ) ;
#235966 = CIRCLE ( 'NONE', #123547, 11.64999999999999325 ) ;
#235967 = LINE ( 'NONE', #212580, #198923 ) ;
#235968 = DIRECTION ( 'NONE',  ( 0.000000000000000000, 0.000000000000000000, 1.000000000000000000 ) ) ;
#235969 = AXIS2_PLACEMENT_3D ( 'NONE', #119885, #45453, #140700 ) ;
#235970 = DIRECTION ( 'NONE',  ( 0.000000000000000000, 8.881784197000605457E-16, -1.000000000000000000 ) ) ;
#235971 = DIRECTION ( 'NONE',  ( 0.000000000000000000, 0.8660254037844377084, 0.5000000000000016653 ) ) ;
#235972 = CARTESIAN_POINT ( 'NONE',  ( -23.15000000000000213, 1.925233644870972816, -46.23024353312612789 ) ) ;
#235973 = EDGE_CURVE ( 'NONE', #207750, #224041, #130248, .T. ) ;
#235974 = TOROIDAL_SURFACE ( 'NONE', #148508, 0.2000000000000000111, 0.1000000000000000056 ) ;
#235975 = ADVANCED_FACE ( 'NONE', ( #132844 ), #143155, .F. ) ;
#235976 = ORIENTED_EDGE ( 'NONE', *, *, #176658, .T. ) ;
#235977 = DIRECTION ( 'NONE',  ( 0.000000000000000000, 0.2128009952264665328, -0.9770955615653084125 ) ) ;
#235979 = ORIENTED_EDGE ( 'NONE', *, *, #132698, .F. ) ;
#235978 = DIRECTION ( 'NONE',  ( 0.000000000000000000, -0.000000000000000000, 1.000000000000000000 ) ) ;
#235980 = DIRECTION ( 'NONE',  ( -0.000000000000000000, -0.000000000000000000, 1.000000000000000000 ) ) ;
#235981 = CARTESIAN_POINT ( 'NONE',  ( -20.00857864376270001, 66.85000000001259934, -191.1731074845244223 ) ) ;
#235983 = EDGE_CURVE ( 'NONE', #78394, #216154, #33777, .T. ) ;
#235982 = DIRECTION ( 'NONE',  ( 0.000000000000000000, -6.769652589177795712E-15, 1.000000000000000000 ) ) ;
#235985 = EDGE_CURVE ( 'NONE', #58778, #213938, #80797, .T. ) ;
#235984 =( BOUNDED_SURFACE ( )  B_SPLINE_SURFACE ( 3, 2, ( 
 ( #188147, #87737, #149037 ),
 ( #128174, #207725, #9496 ),
 ( #89029, #228567, #49909 ),
 ( #189437, #51166, #130733 ),
 ( #171196, #129455, #106007 ),
 ( #210288, #31670, #91611 ),
 ( #185571, #166037, #250672 ),
 ( #245558, #172484, #115028 ) ),
 .UNSPECIFIED., .F., .F., .F. ) 
 B_SPLINE_SURFACE_WITH_KNOTS ( ( 4, 2, 2, 4 ),
 ( 3, 3 ),
 ( 0.0001704874539069995342, 0.0003809798300636783679, 0.0004862260181420178119, 0.0005914722062203572016 ),
 ( 0.000000000000000000, 1.000000000000000000 ),
 .UNSPECIFIED. ) 
 GEOMETRIC_REPRESENTATION_ITEM ( )  RATIONAL_B_SPLINE_SURFACE ( (
 ( 1.000000000000000000, 0.7071067811864699681, 1.000000000000000000),
 ( 1.000000000000000000, 0.7670648383568722251, 1.000000000000000000),
 ( 1.000000000000000000, 0.8204820770262503116, 1.000000000000000000),
 ( 1.000000000000000000, 0.8877218296108694284, 1.000000000000000000),
 ( 1.000000000000000000, 0.9080815932666681523, 1.000000000000000000),
 ( 1.000000000000000000, 0.9395541505860662834, 1.000000000000000000),
 ( 1.000000000000000000, 0.9506520335379859965, 1.000000000000000000),
 ( 1.000000000000000000, 0.9504532311154701985, 1.000000000000000000) ) ) 
 REPRESENTATION_ITEM ( '' )  SURFACE ( )  );
#235986 = VERTEX_POINT ( 'NONE', #200503 ) ;
#235987 = CARTESIAN_POINT ( 'NONE',  ( -16.77308656112215246, 66.05000000001258798, -190.8729142928220881 ) ) ;
#235988 = PRODUCT_CONTEXT ( 'NONE', #114050, 'mechanical' ) ;
#235989 = CARTESIAN_POINT ( 'NONE',  ( 23.14999999999999858, 76.00000000001213607, -136.5231074845243313 ) ) ;
#235990 = DIRECTION ( 'NONE',  ( -1.000000000000000000, 0.000000000000000000, 0.000000000000000000 ) ) ;
#235991 = ADVANCED_FACE ( 'NONE', ( #81800 ), #209831, .T. ) ;
#235992 = ORIENTED_EDGE ( 'NONE', *, *, #232564, .F. ) ;
#235993 = DIRECTION ( 'NONE',  ( -0.8049926720990042694, -0.5932847527679310229, 0.000000000000000000 ) ) ;
#235994 = DIRECTION ( 'NONE',  ( 1.000000000000000000, 0.000000000000000000, 0.000000000000000000 ) ) ;
#235995 = EDGE_CURVE ( 'NONE', #84325, #61043, #101342, .T. ) ;
#235996 = AXIS2_PLACEMENT_3D ( 'NONE', #211853, #55295, #214400 ) ;
#235998 = ADVANCED_FACE ( 'NONE', ( #37596 ), #184862, .T. ) ;
#235997 = EDGE_CURVE ( 'NONE', #178804, #213344, #114129, .T. ) ;
#235999 = FACE_OUTER_BOUND ( 'NONE', #117102, .T. ) ;
#236000 = ORIENTED_EDGE ( 'NONE', *, *, #184693, .T. ) ;
#236001 = ORIENTED_EDGE ( 'NONE', *, *, #148072, .F. ) ;
#236002 = DIRECTION ( 'NONE',  ( 0.000000000000000000, -1.000000000000000000, 0.000000000000000000 ) ) ;
#236003 = AXIS2_PLACEMENT_3D ( 'NONE', #135888, #36849, #100598 ) ;
#236004 = DIRECTION ( 'NONE',  ( 1.000000000000000000, -8.673617379884087537E-15, -0.000000000000000000 ) ) ;
#236005 = CARTESIAN_POINT ( 'NONE',  ( 20.94999999999999929, -9.000000000000000000, -23.60603087734755690 ) ) ;
#236006 = CARTESIAN_POINT ( 'NONE',  ( 21.05000000000000071, 85.00000000001179501, -79.41707660717668205 ) ) ;
#236007 = EDGE_CURVE ( 'NONE', #235470, #201306, #118410, .T. ) ;
#236008 = CARTESIAN_POINT ( 'NONE',  ( 22.57320508075688537, 11.65000000001115588, -167.4999999999999716 ) ) ;
#236011 = CARTESIAN_POINT ( 'NONE',  ( -18.59999999999999787, 10.33248238083634440, -206.5948465439131496 ) ) ;
#236010 = AXIS2_PLACEMENT_3D ( 'NONE', #97115, #35923, #254884 ) ;
#236009 = CARTESIAN_POINT ( 'NONE',  ( -23.15000000000000213, 11.65000000001115588, -79.15000000000004832 ) ) ;
#236012 = CARTESIAN_POINT ( 'NONE',  ( -20.94999999999999929, -10.38870553492056104, -206.3818953267866902 ) ) ;
#236014 = ADVANCED_FACE ( 'NONE', ( #178401 ), #79245, .F. ) ;
#236013 = CARTESIAN_POINT ( 'NONE',  ( -20.54999999999999716, 66.65000000001229807, -157.7731074845244166 ) ) ;
#236015 = LINE ( 'NONE', #254279, #75533 ) ;
#236017 = EDGE_CURVE ( 'NONE', #5563, #71875, #209268, .T. ) ;
#236016 = DIRECTION ( 'NONE',  ( 0.000000000000000000, 0.000000000000000000, 1.000000000000000000 ) ) ;
#236018 = AXIS2_PLACEMENT_3D ( 'NONE', #78399, #140970, #44435 ) ;
#236019 = ORIENTED_EDGE ( 'NONE', *, *, #234621, .T. ) ;
#236020 = CIRCLE ( 'NONE', #119511, 0.2000000000000057288 ) ;
#236021 = ORIENTED_EDGE ( 'NONE', *, *, #125859, .F. ) ;
#236022 = DIRECTION ( 'NONE',  ( -0.7071067811865127117, -0.7071067811865821007, 0.000000000000000000 ) ) ;
#236023 = CARTESIAN_POINT ( 'NONE',  ( -18.44085059012132177, 64.48598750652841716, -145.7828021654028987 ) ) ;
#236025 = CYLINDRICAL_SURFACE ( 'NONE', #12041, 0.09999999999998898659 ) ;
#236024 = CARTESIAN_POINT ( 'NONE',  ( 23.24999999999999645, 5.650000000011139001, -121.3500000000000227 ) ) ;
#236026 =( BOUNDED_SURFACE ( )  B_SPLINE_SURFACE ( 3, 2, ( 
 ( #73332, #172441, #208954 ),
 ( #69464, #227227, #189396 ),
 ( #10759, #70759, #151582 ),
 ( #231111, #111139, #12065 ),
 ( #250636, #48588, #72026 ),
 ( #207690, #150283, #147702 ),
 ( #152873, #47285, #52430 ),
 ( #131983, #211531, #32934 ),
 ( #29076, #88986, #92850 ),
 ( #112438, #191988, #168597 ) ),
 .UNSPECIFIED., .F., .F., .F. ) 
 B_SPLINE_SURFACE_WITH_KNOTS ( ( 4, 2, 2, 2, 4 ),
 ( 3, 3 ),
 ( 0.0001701955120502367041, 0.0002247052511886173890, 0.0002792149903269980468, 0.0003882344686037594167, 0.0006062734251572821564 ),
 ( 0.000000000000000000, 1.000000000000000000 ),
 .UNSPECIFIED. ) 
 GEOMETRIC_REPRESENTATION_ITEM ( )  RATIONAL_B_SPLINE_SURFACE ( (
 ( 1.000000000000000000, 0.2966190024561448646, 1.000000000000000000),
 ( 1.000000000000000000, 0.2964522492711734181, 1.000000000000000000),
 ( 1.000000000000000000, 0.3059923531884917169, 1.000000000000000000),
 ( 1.000000000000000000, 0.3355751146943816154, 1.000000000000000000),
 ( 1.000000000000000000, 0.3550672384963678430, 1.000000000000000000),
 ( 1.000000000000000000, 0.4157034672181950663, 1.000000000000000000),
 ( 1.000000000000000000, 0.4588031877658284574, 1.000000000000000000),
 ( 1.000000000000000000, 0.5771441759655042691, 1.000000000000000000),
 ( 1.000000000000000000, 0.6469377121777389883, 1.000000000000000000),
 ( 1.000000000000000000, 0.7071067811865509034, 1.000000000000000000) ) ) 
 REPRESENTATION_ITEM ( '' )  SURFACE ( )  );
#236027 = AXIS2_PLACEMENT_3D ( 'NONE', #47069, #105747, #144888 ) ;
#236028 = EDGE_CURVE ( 'NONE', #24875, #241247, #68355, .T. ) ;
#236029 = CYLINDRICAL_SURFACE ( 'NONE', #93462, 0.1000000000000012546 ) ;
#236030 = CARTESIAN_POINT ( 'NONE',  ( 20.05000000000002913, 68.75000000001230660, -160.7731074845244166 ) ) ;
#236031 = CARTESIAN_POINT ( 'NONE',  ( -20.85000000000000142, 69.15387683765879956, -32.28538121767450519 ) ) ;
#236032 = ORIENTED_EDGE ( 'NONE', *, *, #194612, .T. ) ;
#236033 = EDGE_CURVE ( 'NONE', #216154, #22402, #161391, .T. ) ;
#236034 = ORIENTED_EDGE ( 'NONE', *, *, #202244, .F. ) ;
#236035 = CARTESIAN_POINT ( 'NONE',  ( 20.94999999999999574, -11.74999999998883560, -36.60000000000000853 ) ) ;
#236036 = EDGE_LOOP ( 'NONE', ( #94258, #54549 ) ) ;
#236037 = DIRECTION ( 'NONE',  ( 0.000000000000000000, 0.000000000000000000, 1.000000000000000000 ) ) ;
#236038 = AXIS2_PLACEMENT_3D ( 'NONE', #236312, #17286, #39435 ) ;
#236039 = AXIS2_PLACEMENT_3D ( 'NONE', #181629, #138599, #22555 ) ;
#236040 = FACE_OUTER_BOUND ( 'NONE', #195137, .T. ) ;
#236041 = B_SPLINE_CURVE_WITH_KNOTS ( 'NONE', 3,
 ( #31514, #13217, #53615, #111018 ),
 .UNSPECIFIED., .F., .F.,
 ( 4, 4 ),
 ( 0.000000000000000000, 0.001767853679387101484 ),
 .UNSPECIFIED. ) ;
#236042 = TOROIDAL_SURFACE ( 'NONE', #127907, 0.2000000000000000111, 0.1000000000000000056 ) ;
#236044 = VERTEX_POINT ( 'NONE', #120995 ) ;
#236043 = AXIS2_PLACEMENT_3D ( 'NONE', #118387, #100063, #205272 ) ;
#236045 = CARTESIAN_POINT ( 'NONE',  ( -20.94999999999999929, 4.360421613930902218, -245.4659189663672691 ) ) ;
#236046 = ORIENTED_EDGE ( 'NONE', *, *, #208907, .T. ) ;
#236047 = AXIS2_PLACEMENT_3D ( 'NONE', #41798, #20954, #121349 ) ;
#236048 = DIRECTION ( 'NONE',  ( 0.000000000000000000, -0.4999999999999088507, -0.8660254037844913322 ) ) ;
#236049 = VECTOR ( 'NONE', #41917, 999.9999999999998863 ) ;
#236050 = CARTESIAN_POINT ( 'NONE',  ( 23.14999999999999503, 31.44980407958351876, -233.5445995079518582 ) ) ;
#236051 = DIRECTION ( 'NONE',  ( 0.000000000000000000, -0.9915357197604853789, 0.1298341882520022694 ) ) ;
#236052 = DIRECTION ( 'NONE',  ( 0.000000000000000000, 0.000000000000000000, 1.000000000000000000 ) ) ;
#236053 = CARTESIAN_POINT ( 'NONE',  ( -16.94107738177415712, 65.98576071487568129, -157.4731074845244336 ) ) ;
#236055 = CARTESIAN_POINT ( 'NONE',  ( -18.59999999999999787, 1.115600667400684642E-11, -167.4999999999999716 ) ) ;
#236054 = DIRECTION ( 'NONE',  ( 0.000000000000000000, 0.8660254037844309360, -0.5000000000000134337 ) ) ;
#236056 = CARTESIAN_POINT ( 'NONE',  ( 20.94999999999999929, 5.499999999999998224, -21.09473398108690390 ) ) ;
#236057 = ORIENTED_EDGE ( 'NONE', *, *, #69902, .T. ) ;
#236059 = CYLINDRICAL_SURFACE ( 'NONE', #5830, 0.09999999999998898659 ) ;
#236058 = CARTESIAN_POINT ( 'NONE',  ( -16.87331047859649757, 9.950000000011138823, -188.3499999999999659 ) ) ;
#236060 = EDGE_LOOP ( 'NONE', ( #57028, #246421, #238572, #156493, #132384, #202159, #58974, #85363, #28747, #79624, #109088, #168331, #143898, #64099, #156979, #48636, #227170, #217628, #108195, #41072, #249146, #190207, #229693 ) ) ;
#236062 = VERTEX_POINT ( 'NONE', #58391 ) ;
#236061 = CARTESIAN_POINT ( 'NONE',  ( -21.05000000000000071, 67.23127455305835554, -235.8551265064784559 ) ) ;
#236063 = AXIS2_PLACEMENT_3D ( 'NONE', #147696, #229793, #249375 ) ;
#236064 = ORIENTED_EDGE ( 'NONE', *, *, #178113, .T. ) ;
#236065 = CARTESIAN_POINT ( 'NONE',  ( 20.94999999999999574, 2.859758780633683273, -208.6670499591424459 ) ) ;
#236066 = CARTESIAN_POINT ( 'NONE',  ( 23.24999999999999645, 64.25000000001264766, -194.2731074845244450 ) ) ;
#236067 = AXIS2_PLACEMENT_3D ( 'NONE', #205233, #69611, #87845 ) ;
#236068 = DIRECTION ( 'NONE',  ( -1.000000000000000000, 0.000000000000000000, 0.000000000000000000 ) ) ;
#236069 = CARTESIAN_POINT ( 'NONE',  ( -20.54999999999999716, 73.60000000001200249, -116.2477294072864140 ) ) ;
#236070 = VERTEX_POINT ( 'NONE', #199229 ) ;
#236071 = DIRECTION ( 'NONE',  ( 1.000000000000000000, -0.000000000000000000, 0.000000000000000000 ) ) ;
#236072 = FILL_AREA_STYLE ('',( #255585 ) ) ;
#236073 = FACE_OUTER_BOUND ( 'NONE', #182698, .T. ) ;
#236074 = ORIENTED_EDGE ( 'NONE', *, *, #57400, .F. ) ;
#236075 = DIRECTION ( 'NONE',  ( 1.000000000000000000, 0.000000000000000000, 0.000000000000000000 ) ) ;
#236076 = EDGE_CURVE ( 'NONE', #212340, #209959, #168682, .T. ) ;
#236077 = VECTOR ( 'NONE', #83823, 1000.000000000000000 ) ;
#236078 = DIRECTION ( 'NONE',  ( 0.000000000000000000, -6.982962677686266711E-15, 1.000000000000000000 ) ) ;
#236079 = EDGE_LOOP ( 'NONE', ( #227233, #104301, #219178, #222396 ) ) ;
#236080 = EDGE_LOOP ( 'NONE', ( #176749, #160187, #17749, #216270 ) ) ;
#236081 = EDGE_CURVE ( 'NONE', #115352, #233724, #187604, .T. ) ;
#236082 = DIRECTION ( 'NONE',  ( -1.000000000000000000, 0.000000000000000000, 0.000000000000000000 ) ) ;
#236083 = ORIENTED_EDGE ( 'NONE', *, *, #61692, .T. ) ;
#236084 = CARTESIAN_POINT ( 'NONE',  ( -21.14999999999999858, 25.97741635855165754, -254.4468634167653249 ) ) ;
#236085 = EDGE_LOOP ( 'NONE', ( #234349, #187091 ) ) ;
#236086 = LINE ( 'NONE', #256884, #200915 ) ;
#236087 = EDGE_CURVE ( 'NONE', #54475, #192857, #9896, .T. ) ;
#236088 = EDGE_CURVE ( 'NONE', #46365, #16105, #243124, .T. ) ;
#236089 = CARTESIAN_POINT ( 'NONE',  ( -20.85000000000000142, 11.75000000001115197, -93.65839931010299324 ) ) ;
#236090 = CARTESIAN_POINT ( 'NONE',  ( 21.33487959338958717, 69.27444184810150318, -203.5231074845243882 ) ) ;
#236091 = CARTESIAN_POINT ( 'NONE',  ( -16.87036670365548474, 63.08160062417908165, -212.9922606024214531 ) ) ;
#236092 = AXIS2_PLACEMENT_3D ( 'NONE', #137343, #112673, #35727 ) ;
#236093 = TOROIDAL_SURFACE ( 'NONE', #256892, 12.97499999999999787, 0.1000000000000000056 ) ;
#236094 = AXIS2_PLACEMENT_3D ( 'NONE', #243627, #126240, #106661 ) ;
#236095 = DIRECTION ( 'NONE',  ( -2.952720810173289112E-16, -1.000000000000000000, -6.982962677686266711E-15 ) ) ;
#236096 = DIRECTION ( 'NONE',  ( 0.7071067811865388020, -0.7071067811865561215, 0.000000000000000000 ) ) ;
#236097 = DIRECTION ( 'NONE',  ( 0.000000000000000000, 0.000000000000000000, -1.000000000000000000 ) ) ;
#236098 = ORIENTED_EDGE ( 'NONE', *, *, #89942, .F. ) ;
#236100 = CARTESIAN_POINT ( 'NONE',  ( 20.94999999999999574, 68.22930980752001062, -227.7331931781284879 ) ) ;
#236099 = CARTESIAN_POINT ( 'NONE',  ( 20.95512840106822949, 22.90176656920205289, -230.1297528598131805 ) ) ;
#236101 = ORIENTED_EDGE ( 'NONE', *, *, #100356, .F. ) ;
#236104 = ORIENTED_EDGE ( 'NONE', *, *, #10280, .T. ) ;
#236103 = CARTESIAN_POINT ( 'NONE',  ( -20.54999999999999716, 72.62993014539878800, -215.9492192728129965 ) ) ;
#236102 = CARTESIAN_POINT ( 'NONE',  ( 13.40000000000000036, -8.279289321881350361, 11.02928932188135036 ) ) ;
#236105 = VECTOR ( 'NONE', #146058, 999.9999999999998863 ) ;
#236106 = EDGE_CURVE ( 'NONE', #20661, #57307, #180783, .T. ) ;
#236107 = ORIENTED_EDGE ( 'NONE', *, *, #176667, .F. ) ;
#236108 = DIRECTION ( 'NONE',  ( 0.000000000000000000, 0.000000000000000000, 1.000000000000000000 ) ) ;
#236109 = ADVANCED_FACE ( 'NONE', ( #8722 ), #159951, .T. ) ;
#236110 = CARTESIAN_POINT ( 'NONE',  ( 13.88302573338719803, 66.54258905524487488, -155.0230235107344470 ) ) ;
#236111 = DIRECTION ( 'NONE',  ( 0.000000000000000000, 0.000000000000000000, -1.000000000000000000 ) ) ;
#236112 = CARTESIAN_POINT ( 'NONE',  ( -16.77683809663752257, 9.945835743215301505, -113.1639490191042512 ) ) ;
#236113 = VERTEX_POINT ( 'NONE', #63546 ) ;
#236114 = CARTESIAN_POINT ( 'NONE',  ( 20.95083306685154056, 67.08315735812242053, -195.0457826312660643 ) ) ;
#236116 = DIRECTION ( 'NONE',  ( 1.000000000000000000, -0.000000000000000000, -0.000000000000000000 ) ) ;
#236115 = CIRCLE ( 'NONE', #11069, 0.09999999999999939493 ) ;
#236118 = DIRECTION ( 'NONE',  ( 1.000000000000000000, 0.000000000000000000, 0.000000000000000000 ) ) ;
#236117 = DIRECTION ( 'NONE',  ( 1.000000000000000000, 0.000000000000000000, 0.000000000000000000 ) ) ;
#236119 = VECTOR ( 'NONE', #72150, 1000.000000000000000 ) ;
#236121 = EDGE_LOOP ( 'NONE', ( #209915, #114572, #74094, #160392 ) ) ;
#236120 = DIRECTION ( 'NONE',  ( 0.000000000000000000, -0.2617529984164955192, -0.9651348961777178603 ) ) ;
#236122 = VECTOR ( 'NONE', #108064, 1000.000000000000000 ) ;
#236123 = ADVANCED_FACE ( 'NONE', ( #143073 ), #64066, .F. ) ;
#236124 = ORIENTED_EDGE ( 'NONE', *, *, #33124, .F. ) ;
#236125 = EDGE_CURVE ( 'NONE', #48866, #103901, #1695, .T. ) ;
#236126 = AXIS2_PLACEMENT_3D ( 'NONE', #8969, #132790, #110635 ) ;
#236127 = CARTESIAN_POINT ( 'NONE',  ( 20.95520789717937404, 11.94775306454331698, -206.1558306364165389 ) ) ;
#236128 = DIRECTION ( 'NONE',  ( 0.000000000000000000, 0.9126074666063772600, 0.4088369013363276627 ) ) ;
#236129 = EDGE_LOOP ( 'NONE', ( #257915, #243165, #87045, #130972 ) ) ;
#236130 = DIRECTION ( 'NONE',  ( -0.000000000000000000, 0.000000000000000000, -1.000000000000000000 ) ) ;
#236131 = EDGE_LOOP ( 'NONE', ( #224316, #134415, #100581, #88799 ) ) ;
#236132 = DIRECTION ( 'NONE',  ( 0.000000000000000000, 0.2128009952263604232, -0.9770955615653316162 ) ) ;
#236133 = DIRECTION ( 'NONE',  ( 0.000000000000000000, 0.2128009952263601456, -0.9770955615653316162 ) ) ;
#236134 = CARTESIAN_POINT ( 'NONE',  ( 22.39999999999999503, 55.89093952297024970, -232.7795287750844579 ) ) ;
#236135 = ORIENTED_EDGE ( 'NONE', *, *, #118683, .F. ) ;
#236136 = ADVANCED_FACE ( 'NONE', ( #6131 ), #247397, .T. ) ;
#236137 = CARTESIAN_POINT ( 'NONE',  ( -20.64999999999999858, 2.400000000011155432, -154.2753780772379173 ) ) ;
#236138 = EDGE_CURVE ( 'NONE', #118840, #70072, #252675, .T. ) ;
#236139 = EDGE_CURVE ( 'NONE', #242875, #107696, #203061, .T. ) ;
#236140 = TOROIDAL_SURFACE ( 'NONE', #252693, 11.89999999999999858, 0.1000000000000000056 ) ;
#236141 = TOROIDAL_SURFACE ( 'NONE', #123731, 0.2000000000000000111, 0.1000000000000000056 ) ;
#236142 = CARTESIAN_POINT ( 'NONE',  ( -16.87683809663752754, 9.864913447291344895, -53.72428155130396732 ) ) ;
#236143 = AXIS2_PLACEMENT_3D ( 'NONE', #64212, #60345, #4220 ) ;
#236144 = AXIS2_PLACEMENT_3D ( 'NONE', #165057, #67236, #105033 ) ;
#236145 = ORIENTED_EDGE ( 'NONE', *, *, #232309, .F. ) ;
#236146 = ORIENTED_EDGE ( 'NONE', *, *, #171366, .F. ) ;
#236147 = DIRECTION ( 'NONE',  ( -1.000000000000000000, 0.000000000000000000, 0.000000000000000000 ) ) ;
#236148 = EDGE_LOOP ( 'NONE', ( #201293, #28956, #177750, #110730 ) ) ;
#236149 = ORIENTED_EDGE ( 'NONE', *, *, #191498, .F. ) ;
#236151 = ORIENTED_EDGE ( 'NONE', *, *, #217073, .T. ) ;
#236150 = CARTESIAN_POINT ( 'NONE',  ( -20.54999999999999716, 82.95597230662299637, -222.7647147268955337 ) ) ;
#236152 = EDGE_CURVE ( 'NONE', #216022, #60484, #109843, .T. ) ;
#236153 = ORIENTED_EDGE ( 'NONE', *, *, #104644, .F. ) ;
#236154 = DIRECTION ( 'NONE',  ( -1.000000000000000000, 0.000000000000000000, 0.000000000000000000 ) ) ;
#236156 = EDGE_LOOP ( 'NONE', ( #210717, #177982, #175169, #178047 ) ) ;
#236155 = ORIENTED_EDGE ( 'NONE', *, *, #248326, .T. ) ;
#236157 = ADVANCED_FACE ( 'NONE', ( #4834 ), #255553, .T. ) ;
#236158 = AXIS2_PLACEMENT_3D ( 'NONE', #32343, #216067, #37462 ) ;
#236159 = CIRCLE ( 'NONE', #127849, 0.5000000000000004441 ) ;
#236160 = EDGE_LOOP ( 'NONE', ( #135241, #25128, #64980, #180648 ) ) ;
#236161 = CARTESIAN_POINT ( 'NONE',  ( 18.59999999999999787, 77.83534155023598089, -57.96795619196132776 ) ) ;
#236162 = DIRECTION ( 'NONE',  ( 0.000000000000000000, -1.000000000000000000, -6.982962677686266711E-15 ) ) ;
#236163 = CIRCLE ( 'NONE', #140277, 0.1000000000000028644 ) ;
#236164 = CARTESIAN_POINT ( 'NONE',  ( -16.80070461187863629, 14.15964768823248576, -219.2580391851904267 ) ) ;
#236165 = ORIENTED_EDGE ( 'NONE', *, *, #143138, .T. ) ;
#236166 = CARTESIAN_POINT ( 'NONE',  ( 21.14999999999999503, 67.23127455305841238, -235.8551265064783991 ) ) ;
#236168 = VERTEX_POINT ( 'NONE', #45279 ) ;
#236167 = CARTESIAN_POINT ( 'NONE',  ( 23.24999999999999289, 53.32357432685029153, -235.0179440783709879 ) ) ;
#236169 = CARTESIAN_POINT ( 'NONE',  ( 20.94999999999999929, 76.00000000001165290, -69.52310748452431710 ) ) ;
#236171 = ORIENTED_EDGE ( 'NONE', *, *, #247014, .F. ) ;
#236170 = DIRECTION ( 'NONE',  ( 0.000000000000000000, 1.000000000000000000, 0.000000000000000000 ) ) ;
#236172 = ORIENTED_EDGE ( 'NONE', *, *, #146154, .F. ) ;
#236173 = DIRECTION ( 'NONE',  ( 0.000000000000000000, 0.4721928772776973204, 0.8814952561688629284 ) ) ;
#236174 = PLANE ( 'NONE',  #61812 ) ;
#236175 = VERTEX_POINT ( 'NONE', #126080 ) ;
#236176 = EDGE_LOOP ( 'NONE', ( #196475, #124263, #139088, #254479 ) ) ;
#236177 = DIRECTION ( 'NONE',  ( 0.000000000000000000, 0.000000000000000000, 1.000000000000000000 ) ) ;
#236178 = CARTESIAN_POINT ( 'NONE',  ( 23.24999999999999289, 11.65000000001116298, -33.50000000000000000 ) ) ;
#236179 = AXIS2_PLACEMENT_3D ( 'NONE', #151595, #152887, #172458 ) ;
#236181 = EDGE_LOOP ( 'NONE', ( #125341, #45342, #121784, #248416 ) ) ;
#236180 = ORIENTED_EDGE ( 'NONE', *, *, #185330, .F. ) ;
#236182 = VERTEX_POINT ( 'NONE', #68699 ) ;
#236183 = CARTESIAN_POINT ( 'NONE',  ( -17.11825945287482753, 60.86901957628278836, -220.9190389461266477 ) ) ;
#236184 = ORIENTED_EDGE ( 'NONE', *, *, #10552, .F. ) ;
#236185 = VERTEX_POINT ( 'NONE', #166541 ) ;
#236186 = LINE ( 'NONE', #77114, #217514 ) ;
#236187 = ORIENTED_EDGE ( 'NONE', *, *, #176207, .T. ) ;
#236188 = CARTESIAN_POINT ( 'NONE',  ( -16.94037747912386038, 12.45507804527209927, -211.1327632053331627 ) ) ;
#236189 = AXIS2_PLACEMENT_3D ( 'NONE', #154879, #171885, #251375 ) ;
#236191 = CARTESIAN_POINT ( 'NONE',  ( -22.49806830649814415, 64.35011034517360429, -203.6005718008499628 ) ) ;
#236190 = DIRECTION ( 'NONE',  ( 0.000000000000000000, -0.8814952561688429444, 0.4721928772777345684 ) ) ;
#236192 = ORIENTED_EDGE ( 'NONE', *, *, #194864, .F. ) ;
#236193 = VERTEX_POINT ( 'NONE', #206923 ) ;
#236194 = AXIS2_PLACEMENT_3D ( 'NONE', #89144, #124438, #47437 ) ;
#236195 = CYLINDRICAL_SURFACE ( 'NONE', #220230, 0.09999999999999939493 ) ;
#236196 = VERTEX_POINT ( 'NONE', #246053 ) ;
#236197 = CIRCLE ( 'NONE', #252949, 0.09999999999999939493 ) ;
#236198 = PRODUCT_DEFINITION_FORMATION_WITH_SPECIFIED_SOURCE ( 'ANY', '', #45061, .NOT_KNOWN. ) ;
#236199 = CARTESIAN_POINT ( 'NONE',  ( 18.49999999999999289, 11.75000000001115907, -175.5999999999999659 ) ) ;
#236200 = VECTOR ( 'NONE', #122357, 1000.000000000000000 ) ;
#236201 = EDGE_LOOP ( 'NONE', ( #105020, #74574, #246994, #195146 ) ) ;
#236202 = ORIENTED_EDGE ( 'NONE', *, *, #23322, .T. ) ;
#236203 = CARTESIAN_POINT ( 'NONE',  ( 23.40000000000005187, 74.14873292176677921, -47.62635315998165453 ) ) ;
#236204 = VECTOR ( 'NONE', #149717, 1000.000000000000114 ) ;
#236205 = ADVANCED_FACE ( 'NONE', ( #204336 ), #147457, .T. ) ;
#236206 = EDGE_LOOP ( 'NONE', ( #64034, #131535, #139574, #169598 ) ) ;
#236207 = DIRECTION ( 'NONE',  ( 0.000000000000000000, 0.2617529984165030132, 0.9651348961777157509 ) ) ;
#236208 = DIRECTION ( 'NONE',  ( -1.000000000000000000, 0.000000000000000000, 0.000000000000000000 ) ) ;
#236209 = ORIENTED_EDGE ( 'NONE', *, *, #253395, .T. ) ;
#236210 = CARTESIAN_POINT ( 'NONE',  ( -18.50000000000000000, 9.350000000011156942, -188.8499999999999659 ) ) ;
#236211 = DIRECTION ( 'NONE',  ( 0.000000000000000000, -0.4999999999999799605, 0.8660254037844502539 ) ) ;
#236212 = DIRECTION ( 'NONE',  ( 0.7071067811865127117, 0.7071067811865821007, 0.000000000000000000 ) ) ;
#236213 = SPHERICAL_SURFACE ( 'NONE', #173255, 0.1000000000000000056 ) ;
#236214 = EDGE_CURVE ( 'NONE', #57087, #126102, #43229, .T. ) ;
#236215 = CARTESIAN_POINT ( 'NONE',  ( -20.54999999999999716, 68.85000000001151932, -48.37310748452436826 ) ) ;
#236217 = ADVANCED_FACE ( 'NONE', ( #249900 ), #192493, .T. ) ;
#236216 = DIRECTION ( 'NONE',  ( 0.000000000000000000, 0.01562499999998609446, -0.9998779222360101304 ) ) ;
#236218 = CARTESIAN_POINT ( 'NONE',  ( -16.80469485234340965, 66.05784833687121704, -149.2131406405932808 ) ) ;
#236219 = CARTESIAN_POINT ( 'NONE',  ( 22.60000000000000142, 75.89914163091351895, -148.2726746080136877 ) ) ;
#236220 = CARTESIAN_POINT ( 'NONE',  ( 21.07928932188134397, 1.596973512272234830, -230.6572452218043736 ) ) ;
#236221 = VECTOR ( 'NONE', #165792, 1000.000000000000000 ) ;
#236222 = ORIENTED_EDGE ( 'NONE', *, *, #1473, .F. ) ;
#236223 = CIRCLE ( 'NONE', #207204, 0.1000000000000028644 ) ;
#236226 = ORIENTED_EDGE ( 'NONE', *, *, #180172, .F. ) ;
#236225 = ORIENTED_EDGE ( 'NONE', *, *, #176634, .F. ) ;
#236224 = AXIS2_PLACEMENT_3D ( 'NONE', #110801, #250316, #251601 ) ;
#236227 = ORIENTED_EDGE ( 'NONE', *, *, #177860, .T. ) ;
#236228 = EDGE_LOOP ( 'NONE', ( #218806, #110268, #158580 ) ) ;
#236229 = AXIS2_PLACEMENT_3D ( 'NONE', #47478, #26676, #10954 ) ;
#236230 = EDGE_CURVE ( 'NONE', #63249, #192876, #90808, .T. ) ;
#236231 = CARTESIAN_POINT ( 'NONE',  ( 21.12230431290520016, 75.99479014832370183, -209.9806741378173456 ) ) ;
#236232 = CARTESIAN_POINT ( 'NONE',  ( -23.25000000000000000, -9.599999999988847676, -110.3939691226524786 ) ) ;
#236233 = AXIS2_PLACEMENT_3D ( 'NONE', #64859, #158861, #218793 ) ;
#236235 = CARTESIAN_POINT ( 'NONE',  ( -23.25000000000000000, 7.021664781911246322, -104.3335654018973315 ) ) ;
#236234 = DIRECTION ( 'NONE',  ( 1.000000000000000000, -3.265361837132813093E-16, -2.280189983783949500E-30 ) ) ;
#236236 = EDGE_LOOP ( 'NONE', ( #165678, #229224, #241966, #216877 ) ) ;
#236237 = DIRECTION ( 'NONE',  ( 1.000000000000000000, -0.000000000000000000, -0.000000000000000000 ) ) ;
#236238 = SURFACE_STYLE_FILL_AREA ( #240105 ) ;
#236239 = DIRECTION ( 'NONE',  ( 0.000000000000000000, 0.4797419643160688585, 0.8774096236502991752 ) ) ;
#236240 = DIRECTION ( 'NONE',  ( 0.000000000000000000, 0.000000000000000000, 1.000000000000000000 ) ) ;
#236241 = DIRECTION ( 'NONE',  ( 1.000000000000000000, -0.000000000000000000, -0.000000000000000000 ) ) ;
#236242 = VERTEX_POINT ( 'NONE', #51665 ) ;
#236243 = AXIS2_PLACEMENT_3D ( 'NONE', #108276, #229507, #13045 ) ;
#236244 = VECTOR ( 'NONE', #44559, 1000.000000000000000 ) ;
#236245 = TOROIDAL_SURFACE ( 'NONE', #102958, 4.100000000000000533, 0.1000000000000000056 ) ;
#236246 = DIRECTION ( 'NONE',  ( -1.000000000000000000, 0.000000000000000000, 0.000000000000000000 ) ) ;
#236247 = EDGE_LOOP ( 'NONE', ( #194511, #30020, #119731, #43254 ) ) ;
#236248 = EDGE_CURVE ( 'NONE', #156269, #92927, #218163, .T. ) ;
#236249 = DIRECTION ( 'NONE',  ( 0.000000000000000000, 0.5826443254699606999, 0.8127272543711416830 ) ) ;
#236250 = LINE ( 'NONE', #162838, #56301 ) ;
#236251 = EDGE_CURVE ( 'NONE', #43027, #80050, #105732, .T. ) ;
#236252 = CARTESIAN_POINT ( 'NONE',  ( 20.94999999999999929, 10.72371710470752149, -7.664913569087605794 ) ) ;
#236253 = FACE_OUTER_BOUND ( 'NONE', #54895, .T. ) ;
#236254 = FACE_OUTER_BOUND ( 'NONE', #147644, .T. ) ;
#236255 = DIRECTION ( 'NONE',  ( 0.000000000000000000, 0.1350103645451876666, -0.9908441862701600211 ) ) ;
#236256 = EDGE_LOOP ( 'NONE', ( #208457, #207697, #140554, #67001 ) ) ;
#236257 = CARTESIAN_POINT ( 'NONE',  ( -22.47071067811865319, 68.27992525551360359, -69.62219993922698791 ) ) ;
#236258 = CARTESIAN_POINT ( 'NONE',  ( -20.90000000000000213, 0.000000000000000000, 0.000000000000000000 ) ) ;
#236259 = CYLINDRICAL_SURFACE ( 'NONE', #154173, 0.1000000000000050432 ) ;
#236260 = AXIS2_PLACEMENT_3D ( 'NONE', #229522, #224368, #207400 ) ;
#236262 = FACE_BOUND ( 'NONE', #150064, .T. ) ;
#236261 = CARTESIAN_POINT ( 'NONE',  ( -23.25000000000000000, -11.48912529306489994, -63.89999999999999858 ) ) ;
#236263 = LINE ( 'NONE', #213, #195521 ) ;
#236264 = VECTOR ( 'NONE', #123994, 1000.000000000000000 ) ;
#236265 = EDGE_CURVE ( 'NONE', #56206, #12375, #18279, .T. ) ;
#236266 = DIRECTION ( 'NONE',  ( -1.000000000000000000, -0.000000000000000000, -0.000000000000000000 ) ) ;
#236267 = CARTESIAN_POINT ( 'NONE',  ( -18.39999999999999858, 64.52683809664983983, -160.6971614177164724 ) ) ;
#236268 = CARTESIAN_POINT ( 'NONE',  ( -20.00857864376270001, 9.150000000011157653, -79.25000000000004263 ) ) ;
#236269 = VERTEX_POINT ( 'NONE', #49120 ) ;
#236270 = CIRCLE ( 'NONE', #169685, 0.09999999999999939493 ) ;
#236271 = ORIENTED_EDGE ( 'NONE', *, *, #245769, .F. ) ;
#236272 = DIRECTION ( 'NONE',  ( -0.7071067811865473507, -0.3338907855510732658, -0.6233112732207619633 ) ) ;
#236273 = ORIENTED_EDGE ( 'NONE', *, *, #221581, .T. ) ;
#236274 = LINE ( 'NONE', #139726, #59379 ) ;
#236275 = VECTOR ( 'NONE', #101405, 1000.000000000000114 ) ;
#236276 = AXIS2_PLACEMENT_3D ( 'NONE', #99511, #179117, #94395 ) ;
#236277 = EDGE_CURVE ( 'NONE', #72782, #49547, #47476, .T. ) ;
#236278 = CIRCLE ( 'NONE', #98868, 0.09999999999998898659 ) ;
#236279 = AXIS2_PLACEMENT_3D ( 'NONE', #42542, #176962, #195241 ) ;
#236280 = CARTESIAN_POINT ( 'NONE',  ( -23.15000000000000213, 64.35000000001173248, -81.27310748452440237 ) ) ;
#236281 = EDGE_LOOP ( 'NONE', ( #231968, #150250, #238809, #255959, #97376 ) ) ;
#236282 = DIRECTION ( 'NONE',  ( -1.000000000000000000, 8.995003028460479049E-16, -4.818376878839538654E-16 ) ) ;
#236283 = CARTESIAN_POINT ( 'NONE',  ( -12.25000000000000178, 9.350000000011139178, -50.25000000000000000 ) ) ;
#236284 = CARTESIAN_POINT ( 'NONE',  ( -23.15000000000000213, 85.00000000001251976, -179.3170766071767446 ) ) ;
#236285 = EDGE_CURVE ( 'NONE', #147926, #107466, #193260, .T. ) ;
#236286 = FACE_OUTER_BOUND ( 'NONE', #226195, .T. ) ;
#236288 = VERTEX_POINT ( 'NONE', #71284 ) ;
#236287 = CARTESIAN_POINT ( 'NONE',  ( -16.96982749440706328, 9.950000000011137047, -187.8752215911892165 ) ) ;
#236290 = DIRECTION ( 'NONE',  ( 0.000000000000000000, 0.1495327102803663544, -0.9887567792719339499 ) ) ;
#236289 = LINE ( 'NONE', #53807, #229470 ) ;
#236291 = CARTESIAN_POINT ( 'NONE',  ( 23.14999999999999858, 67.23127455305835554, -235.8551265064784559 ) ) ;
#236292 = CARTESIAN_POINT ( 'NONE',  ( -22.50000000000000000, 64.25000000001165290, -69.52310748452438816 ) ) ;
#236293 = CARTESIAN_POINT ( 'NONE',  ( 18.47149038651512143, 87.08088263100174231, -199.6145014482960960 ) ) ;
#236294 = ADVANCED_FACE ( 'NONE', ( #150796 ), #92101, .T. ) ;
#236295 = EDGE_CURVE ( 'NONE', #35186, #137948, #22571, .T. ) ;
#236296 = VERTEX_POINT ( 'NONE', #89524 ) ;
#236297 = CIRCLE ( 'NONE', #123891, 4.149999999999999467 ) ;
#236298 = DIRECTION ( 'NONE',  ( 0.000000000000000000, 0.000000000000000000, 1.000000000000000000 ) ) ;
#236299 = DIRECTION ( 'NONE',  ( 0.000000000000000000, -0.4721928772777344019, -0.8814952561688432775 ) ) ;
#236300 = ORIENTED_EDGE ( 'NONE', *, *, #96847, .F. ) ;
#236301 = CARTESIAN_POINT ( 'NONE',  ( -16.88328101497759448, 66.04964716579368655, -182.6719279695951457 ) ) ;
#236302 = VERTEX_POINT ( 'NONE', #133795 ) ;
#236303 = AXIS2_PLACEMENT_3D ( 'NONE', #66735, #242784, #185391 ) ;
#236304 = EDGE_CURVE ( 'NONE', #25427, #182610, #54251, .T. ) ;
#236305 = CARTESIAN_POINT ( 'NONE',  ( -18.50000000000000000, -1.164121893230052995, -108.4148480855716485 ) ) ;
#236306 = EDGE_CURVE ( 'NONE', #189878, #102088, #197328, .T. ) ;
#236307 = CARTESIAN_POINT ( 'NONE',  ( -23.15000000000000213, 11.65000000001115588, -21.75000000000000355 ) ) ;
#236308 = CARTESIAN_POINT ( 'NONE',  ( 21.14999999999999858, 2.319530388122574394, -217.8268657444419887 ) ) ;
#236309 = ORIENTED_EDGE ( 'NONE', *, *, #24637, .T. ) ;
#236310 = ADVANCED_FACE ( 'NONE', ( #112961 ), #168177, .T. ) ;
#236311 = VERTEX_POINT ( 'NONE', #248614 ) ;
#236312 = CARTESIAN_POINT ( 'NONE',  ( -20.94999999999999929, 67.23127455305835554, -235.8551265064784559 ) ) ;
#236313 = CARTESIAN_POINT ( 'NONE',  ( 18.59999999999999076, 74.93036000061670165, -233.6816308724374949 ) ) ;
#236314 = EDGE_CURVE ( 'NONE', #248066, #173700, #201428, .T. ) ;
#236315 = CARTESIAN_POINT ( 'NONE',  ( -16.97683810757273193, 62.92512680882908427, -213.7198058836067389 ) ) ;
#236316 = CARTESIAN_POINT ( 'NONE',  ( -16.86445178670653888, 66.03778837089588194, -90.41388492264164256 ) ) ;
#236318 = CARTESIAN_POINT ( 'NONE',  ( 18.59999999999999076, 74.16465844978745281, -91.46795619196133487 ) ) ;
#236317 = DIRECTION ( 'NONE',  ( 0.000000000000000000, 9.769962616701369667E-15, 1.000000000000000000 ) ) ;
#236319 = AXIS2_PLACEMENT_3D ( 'NONE', #35253, #194323, #233444 ) ;
#236320 = AXIS2_PLACEMENT_3D ( 'NONE', #118916, #102836, #182419 ) ;
#236321 = DIRECTION ( 'NONE',  ( -0.000000000000000000, 1.000000000000000000, -0.000000000000000000 ) ) ;
#236323 = ADVANCED_FACE ( 'NONE', ( #75142 ), #208220, .F. ) ;
#236322 = CARTESIAN_POINT ( 'NONE',  ( 21.06089410995835109, 65.27470446788827019, -90.82072675348118196 ) ) ;
#236324 = CIRCLE ( 'NONE', #15604, 0.09999999999998898659 ) ;
#236326 = ADVANCED_FACE ( 'NONE', ( #70001 ), #149539, .T. ) ;
#236325 = DIRECTION ( 'NONE',  ( 0.000000000000000000, 0.000000000000000000, 1.000000000000000000 ) ) ;
#236327 = EDGE_LOOP ( 'NONE', ( #181117, #134096, #183079 ) ) ;
#236328 = CARTESIAN_POINT ( 'NONE',  ( -21.05000000000000071, 74.83729825007360148, -61.52310748452433131 ) ) ;
#236330 = ORIENTED_EDGE ( 'NONE', *, *, #240960, .T. ) ;
#236329 = CARTESIAN_POINT ( 'NONE',  ( 20.99999999999997868, 1.115600667400684642E-11, -67.00000000000004263 ) ) ;
#236331 = CARTESIAN_POINT ( 'NONE',  ( 22.49533356619861024, 11.65000000630418597, 0.06512258032273263164 ) ) ;
#236332 = CARTESIAN_POINT ( 'NONE',  ( -18.50000000000000000, -1.164121893230052995, -74.91484808557160591 ) ) ;
#236334 = LINE ( 'NONE', #197204, #186635 ) ;
#236333 = CARTESIAN_POINT ( 'NONE',  ( -18.40000000000000213, 64.66825945288670141, -90.37310748452438247 ) ) ;
#236335 = EDGE_CURVE ( 'NONE', #251409, #77132, #226741, .T. ) ;
#236336 = ORIENTED_EDGE ( 'NONE', *, *, #55290, .F. ) ;
#236338 = CARTESIAN_POINT ( 'NONE',  ( -18.40000000000000213, 11.48667500176882861, -57.75000000000000000 ) ) ;
#236337 = CARTESIAN_POINT ( 'NONE',  ( -21.14999999999999858, 76.10000000001170406, -76.06376443622556849 ) ) ;
#236339 = LINE ( 'NONE', #163236, #41508 ) ;
#236340 = LINE ( 'NONE', #96798, #221819 ) ;
#236341 = DIRECTION ( 'NONE',  ( -0.000000000000000000, -0.2605042016806452532, -0.9654727137038777718 ) ) ;
#236342 = CARTESIAN_POINT ( 'NONE',  ( 21.05000000000000071, 76.00000000001244871, -170.0231074845243597 ) ) ;
#236343 = EDGE_LOOP ( 'NONE', ( #107549, #21134, #156786, #69488 ) ) ;
#236344 = CARTESIAN_POINT ( 'NONE',  ( -22.49231231312463208, 31.84026337202741530, -238.9442601656825786 ) ) ;
#236345 = ADVANCED_FACE ( 'NONE', ( #180636 ), #116806, .F. ) ;
#236346 = EDGE_LOOP ( 'NONE', ( #52723, #124956, #24419 ) ) ;
#236347 = ADVANCED_FACE ( 'NONE', ( #1971 ), #81491, .F. ) ;
#236348 = CIRCLE ( 'NONE', #69764, 11.74999999999999645 ) ;
#236349 = EDGE_CURVE ( 'NONE', #167256, #206918, #185050, .T. ) ;
#236351 = VECTOR ( 'NONE', #203958, 1000.000000000000000 ) ;
#236350 = LINE ( 'NONE', #137247, #238526 ) ;
#236352 = ORIENTED_EDGE ( 'NONE', *, *, #254966, .F. ) ;
#236353 = CARTESIAN_POINT ( 'NONE',  ( 20.94999999999999929, 1.115600667400684642E-11, -100.5000000000000426 ) ) ;
#236354 = ORIENTED_EDGE ( 'NONE', *, *, #44584, .T. ) ;
#236355 =( BOUNDED_CURVE ( )  B_SPLINE_CURVE ( 3, ( #135552, #33952, #19483, #58576 ),
 .UNSPECIFIED., .F., .T. ) 
 B_SPLINE_CURVE_WITH_KNOTS ( ( 4, 4 ),
 ( -4.796163466380676255E-14, 1.570796326794913211 ),
 .UNSPECIFIED. ) 
 CURVE ( )  GEOMETRIC_REPRESENTATION_ITEM ( )  RATIONAL_B_SPLINE_CURVE ( ( 1.000000000000000000, 0.8047378541243498384, 0.8047378541243498384, 1.000000000000000000 ) ) 
 REPRESENTATION_ITEM ( '' )  );
#236357 = CARTESIAN_POINT ( 'NONE',  ( -23.25000000000000000, 1.115600667400684642E-11, -104.5500000000000256 ) ) ;
#236356 = AXIS2_PLACEMENT_3D ( 'NONE', #144031, #8402, #205287 ) ;
#236358 = DIRECTION ( 'NONE',  ( 2.659396599871503635E-15, -0.6132151058540604716, 0.7899159663865477077 ) ) ;
#236359 = EDGE_LOOP ( 'NONE', ( #70710, #251407 ) ) ;
#236360 = EDGE_CURVE ( 'NONE', #119183, #14612, #200199, .T. ) ;
#236361 = CARTESIAN_POINT ( 'NONE',  ( 23.24999999999999645, 76.00000000001237765, -170.0231074845243597 ) ) ;
#236362 = CYLINDRICAL_SURFACE ( 'NONE', #153233, 0.09999999999999939493 ) ;
#236363 = FACE_OUTER_BOUND ( 'NONE', #150440, .T. ) ;
#236364 = CARTESIAN_POINT ( 'NONE',  ( -20.94999999999999929, 56.46250644710310951, -240.6794019422471251 ) ) ;
#236365 = DIRECTION ( 'NONE',  ( 1.073024830501117725E-15, -0.000000000000000000, -1.000000000000000000 ) ) ;
#236366 = AXIS2_PLACEMENT_3D ( 'NONE', #77157, #78439, #185 ) ;
#236367 = ORIENTED_EDGE ( 'NONE', *, *, #205268, .F. ) ;
#236368 = CARTESIAN_POINT ( 'NONE',  ( -18.48179518608921157, 85.51832530050738512, -129.6334019077617938 ) ) ;
#236370 = ORIENTED_EDGE ( 'NONE', *, *, #178339, .T. ) ;
#236369 = VECTOR ( 'NONE', #216899, 1000.000000000000000 ) ;
#236372 = EDGE_LOOP ( 'NONE', ( #34864, #193120 ) ) ;
#236371 = CARTESIAN_POINT ( 'NONE',  ( 21.07199075132371746, 67.22505500089579300, -90.80957532291151324 ) ) ;
#236373 = ORIENTED_EDGE ( 'NONE', *, *, #46844, .F. ) ;
#236374 = DIRECTION ( 'NONE',  ( 0.000000000000000000, 0.000000000000000000, -1.000000000000000000 ) ) ;
#236375 = CARTESIAN_POINT ( 'NONE',  ( 15.39793903038208001, 66.61031399435691469, -187.8502639781730750 ) ) ;
#236376 = CARTESIAN_POINT ( 'NONE',  ( 22.60000000000000142, 11.74956712348939192, 0.1008583690987087389 ) ) ;
#236377 = DIRECTION ( 'NONE',  ( 2.694716079187273439E-16, 1.000000000000000000, 6.467318590049456648E-15 ) ) ;
#236378 = ORIENTED_EDGE ( 'NONE', *, *, #252819, .F. ) ;
#236379 = DIRECTION ( 'NONE',  ( 1.000000000000000000, 0.000000000000000000, 0.000000000000000000 ) ) ;
#236380 = CIRCLE ( 'NONE', #169784, 0.8750000000000007772 ) ;
#236381 = DIRECTION ( 'NONE',  ( -1.000000000000000000, -0.000000000000000000, -0.000000000000000000 ) ) ;
#236382 = ORIENTED_EDGE ( 'NONE', *, *, #256631, .F. ) ;
#236384 = ORIENTED_EDGE ( 'NONE', *, *, #47150, .F. ) ;
#236383 = CARTESIAN_POINT ( 'NONE',  ( -20.64999999999999858, 1.925233644870972816, -146.7302435331261563 ) ) ;
#236385 = CARTESIAN_POINT ( 'NONE',  ( -23.25000000000000000, 45.93315328338058379, -256.6017782078560003 ) ) ;
#236386 = AXIS2_PLACEMENT_3D ( 'NONE', #236056, #256849, #118702 ) ;
#236387 = EDGE_CURVE ( 'NONE', #249181, #147011, #140943, .T. ) ;
#236388 = CARTESIAN_POINT ( 'NONE',  ( -16.79270642812321412, 9.946244216949081007, -79.66106672143797596 ) ) ;
#236389 = CIRCLE ( 'NONE', #123976, 0.2000000000000057288 ) ;
#236390 = ORIENTED_EDGE ( 'NONE', *, *, #160012, .T. ) ;
#236391 = AXIS2_PLACEMENT_3D ( 'NONE', #120802, #101156, #185875 ) ;
#236392 = EDGE_CURVE ( 'NONE', #144474, #6603, #56032, .T. ) ;
#236393 = AXIS2_PLACEMENT_3D ( 'NONE', #140476, #47785, #110344 ) ;
#236394 = DIRECTION ( 'NONE',  ( 0.000000000000000000, 0.000000000000000000, -1.000000000000000000 ) ) ;
#236396 = ORIENTED_EDGE ( 'NONE', *, *, #163463, .F. ) ;
#236395 = CIRCLE ( 'NONE', #123979, 0.1000000000000013933 ) ;
#236397 = DIRECTION ( 'NONE',  ( 0.000000000000000000, 0.000000000000000000, -1.000000000000000000 ) ) ;
#236398 = AXIS2_PLACEMENT_3D ( 'NONE', #209326, #74991, #232769 ) ;
#236399 = ADVANCED_FACE ( 'NONE', ( #254961 ), #5964, .F. ) ;
#236400 = CARTESIAN_POINT ( 'NONE',  ( -18.50000000000000711, 38.25685495413521409, -235.9601135138701693 ) ) ;
#236401 = DIRECTION ( 'NONE',  ( 1.000000000000000000, 0.000000000000000000, 0.000000000000000000 ) ) ;
#236402 = FACE_OUTER_BOUND ( 'NONE', #152803, .T. ) ;
#236403 = EDGE_CURVE ( 'NONE', #50885, #17161, #56794, .T. ) ;
#236404 = TOROIDAL_SURFACE ( 'NONE', #111506, 0.2000000000000000111, 0.1000000000000000056 ) ;
#236405 = AXIS2_PLACEMENT_3D ( 'NONE', #170151, #50142, #29351 ) ;
#236406 = VERTEX_POINT ( 'NONE', #672 ) ;
#236407 = CYLINDRICAL_SURFACE ( 'NONE', #173748, 0.09999999999999939493 ) ;
#236408 = VECTOR ( 'NONE', #164060, 1000.000000000000000 ) ;
#236409 = COLOUR_RGB ( '', 0.72549020, 0.75294118, 0.79215686) ;
#236410 = ORIENTED_EDGE ( 'NONE', *, *, #74431, .T. ) ;
#236411 = DIRECTION ( 'NONE',  ( 0.000000000000000000, 1.000000000000000000, 0.000000000000000000 ) ) ;
#236412 = DIRECTION ( 'NONE',  ( 0.000000000000000000, -0.4088369013363280513, 0.9126074666063769270 ) ) ;
#236414 = ORIENTED_EDGE ( 'NONE', *, *, #249854, .F. ) ;
#236413 = CARTESIAN_POINT ( 'NONE',  ( 20.95512820512820440, 10.62384868372303259, -146.1500000000000341 ) ) ;
#236415 = DIRECTION ( 'NONE',  ( 0.000000000000000000, 0.000000000000000000, 1.000000000000000000 ) ) ;
#236417 = VECTOR ( 'NONE', #130278, 1000.000000000000000 ) ;
#236416 = DIRECTION ( 'NONE',  ( 0.000000000000000000, 0.000000000000000000, 1.000000000000000000 ) ) ;
#236418 = FACE_OUTER_BOUND ( 'NONE', #50140, .T. ) ;
#236419 = FACE_OUTER_BOUND ( 'NONE', #1604, .T. ) ;
#236420 = CARTESIAN_POINT ( 'NONE',  ( 18.39999999999999858, -9.599999999988845900, -174.1001893912220737 ) ) ;
#236421 = DIRECTION ( 'NONE',  ( 1.000000000000000000, -0.000000000000000000, -0.000000000000000000 ) ) ;
#236422 = CARTESIAN_POINT ( 'NONE',  ( -18.51991288638513211, 85.39243678968493612, -129.3798410805650576 ) ) ;
#236424 = VERTEX_POINT ( 'NONE', #16444 ) ;
#236423 = CARTESIAN_POINT ( 'NONE',  ( 21.05000000000000071, -8.999999999988844479, -177.3939691226524076 ) ) ;
#236425 = CIRCLE ( 'NONE', #107246, 0.09999999999999939493 ) ;
#236426 = AXIS2_PLACEMENT_3D ( 'NONE', #114092, #214478, #192361 ) ;
#236427 = CYLINDRICAL_SURFACE ( 'NONE', #210041, 0.09999999999999939493 ) ;
#236428 = CARTESIAN_POINT ( 'NONE',  ( -18.59999999999999787, 85.48068669529064323, -62.58199231576639932 ) ) ;
#236429 = CARTESIAN_POINT ( 'NONE',  ( -18.39999999999999858, 85.50000000001263345, -196.4910380878246485 ) ) ;
#236430 = ORIENTED_EDGE ( 'NONE', *, *, #167461, .T. ) ;
#236431 = ADVANCED_FACE ( 'NONE', ( #175520 ), #112573, .T. ) ;
#236432 = DIRECTION ( 'NONE',  ( -1.073024830501117725E-15, -6.982962677686266711E-15, 1.000000000000000000 ) ) ;
#236433 = CIRCLE ( 'NONE', #182286, 11.64999999999999325 ) ;
#236434 = ADVANCED_FACE ( 'NONE', ( #128049 ), #239220, .T. ) ;
#236435 = AXIS2_PLACEMENT_3D ( 'NONE', #92544, #156419, #251633 ) ;
#236436 = DIRECTION ( 'NONE',  ( -0.7071067811865475727, 0.2890913453342130457, -0.6453109281988448354 ) ) ;
#236438 = ORIENTED_EDGE ( 'NONE', *, *, #54827, .F. ) ;
#236437 = AXIS2_PLACEMENT_3D ( 'NONE', #4430, #104790, #65699 ) ;
#236439 = LINE ( 'NONE', #198595, #135404 ) ;
#236441 = CARTESIAN_POINT ( 'NONE',  ( 21.05000000000000071, 87.39257802171813694, -173.0970570643562212 ) ) ;
#236440 = CIRCLE ( 'NONE', #49004, 0.1999999999999987899 ) ;
#236442 = EDGE_CURVE ( 'NONE', #105430, #244837, #105918, .T. ) ;
#236443 = ORIENTED_EDGE ( 'NONE', *, *, #217147, .F. ) ;
#236444 = FACE_OUTER_BOUND ( 'NONE', #26846, .T. ) ;
#236445 = VERTEX_POINT ( 'NONE', #246695 ) ;
#236446 = DIRECTION ( 'NONE',  ( 0.000000000000000000, 0.000000000000000000, -1.000000000000000000 ) ) ;
#236448 = EDGE_LOOP ( 'NONE', ( #124617, #208421, #35888, #163186 ) ) ;
#236447 = CYLINDRICAL_SURFACE ( 'NONE', #168109, 0.1000000000000028644 ) ;
#236449 = EDGE_CURVE ( 'NONE', #213760, #251476, #2862, .T. ) ;
#236450 = CIRCLE ( 'NONE', #190701, 0.09999999999999939493 ) ;
#236451 = EDGE_CURVE ( 'NONE', #82698, #99212, #114316, .T. ) ;
#236452 = DIRECTION ( 'NONE',  ( 0.000000000000000000, 0.000000000000000000, -1.000000000000000000 ) ) ;
#236453 = ORIENTED_EDGE ( 'NONE', *, *, #219503, .F. ) ;
#236454 = CARTESIAN_POINT ( 'NONE',  ( 20.94999999999999929, 85.00000000001197975, -112.9170766071766820 ) ) ;
#236455 = AXIS2_PLACEMENT_3D ( 'NONE', #252625, #92270, #153590 ) ;
#236456 = TOROIDAL_SURFACE ( 'NONE', #240752, 11.65000000000000036, 0.1000000000000000056 ) ;
#236457 = ORIENTED_EDGE ( 'NONE', *, *, #80902, .F. ) ;
#236459 = VERTEX_POINT ( 'NONE', #229715 ) ;
#236458 = EDGE_LOOP ( 'NONE', ( #77245, #235504, #203087, #41083 ) ) ;
#236460 = CARTESIAN_POINT ( 'NONE',  ( 18.49999999999999645, 76.00000000001142553, -36.02310748452432421 ) ) ;
#236461 = ADVANCED_FACE ( 'NONE', ( #90177 ), #47198, .T. ) ;
#236462 = AXIS2_PLACEMENT_3D ( 'NONE', #39540, #177758, #156915 ) ;
#236463 = ORIENTED_EDGE ( 'NONE', *, *, #208721, .T. ) ;
#236464 = DIRECTION ( 'NONE',  ( 0.000000000000000000, 0.000000000000000000, 1.000000000000000000 ) ) ;
#236465 = ORIENTED_EDGE ( 'NONE', *, *, #149758, .T. ) ;
#236466 = VECTOR ( 'NONE', #129735, 1000.000000000000000 ) ;
#236467 = ORIENTED_EDGE ( 'NONE', *, *, #75131, .T. ) ;
#236468 = CARTESIAN_POINT ( 'NONE',  ( 21.14999999999999858, 11.65000000001116298, -55.25000000000004974 ) ) ;
#236469 = EDGE_CURVE ( 'NONE', #82580, #79894, #139238, .T. ) ;
#236470 = DIRECTION ( 'NONE',  ( -1.000000000000000000, -0.000000000000000000, 0.000000000000000000 ) ) ;
#236471 = DIRECTION ( 'NONE',  ( 0.000000000000000000, 1.000000000000000000, 6.982962677686266711E-15 ) ) ;
#236472 = DIRECTION ( 'NONE',  ( -0.000000000000000000, 0.9072850278296915594, 0.4205162045344698618 ) ) ;
#236473 = VERTEX_POINT ( 'NONE', #130607 ) ;
#236474 = DIRECTION ( 'NONE',  ( 0.000000000000000000, 0.9915357197604982575, -0.1298341882519033486 ) ) ;
#236475 = CARTESIAN_POINT ( 'NONE',  ( -21.14999999999999858, 11.50215294792677057, -198.5972978622482970 ) ) ;
#236476 = DIRECTION ( 'NONE',  ( -0.000000000000000000, 0.2128009952263604232, -0.9770955615653316162 ) ) ;
#236477 = ORIENTED_EDGE ( 'NONE', *, *, #95180, .T. ) ;
#236478 = DIRECTION ( 'NONE',  ( 1.000000000000000000, 0.000000000000000000, -0.000000000000000000 ) ) ;
#236479 = LINE ( 'NONE', #235208, #211148 ) ;
#236480 = CARTESIAN_POINT ( 'NONE',  ( 20.27550659511088682, 9.216043722520002035, -79.65000000000004832 ) ) ;
#236481 = ORIENTED_EDGE ( 'NONE', *, *, #15944, .F. ) ;
#236482 = FACE_OUTER_BOUND ( 'NONE', #106934, .T. ) ;
#236483 = EDGE_LOOP ( 'NONE', ( #26675, #84446, #116132, #107309 ) ) ;
#236485 = ORIENTED_EDGE ( 'NONE', *, *, #83244, .F. ) ;
#236484 = AXIS2_PLACEMENT_3D ( 'NONE', #87245, #127686, #143383 ) ;
#236486 = FACE_OUTER_BOUND ( 'NONE', #94712, .T. ) ;
#236487 = ORIENTED_EDGE ( 'NONE', *, *, #221080, .T. ) ;
#236488 = ORIENTED_EDGE ( 'NONE', *, *, #79639, .T. ) ;
#236489 = DIRECTION ( 'NONE',  ( 0.000000000000000000, -1.000000000000000000, 0.000000000000000000 ) ) ;
#236490 = FACE_OUTER_BOUND ( 'NONE', #196311, .T. ) ;
#236491 = ORIENTED_EDGE ( 'NONE', *, *, #181227, .T. ) ;
#236492 = ORIENTED_EDGE ( 'NONE', *, *, #5873, .T. ) ;
#236493 = DIRECTION ( 'NONE',  ( -1.000000000000000000, 0.000000000000000000, 0.000000000000000000 ) ) ;
#236494 = LINE ( 'NONE', #81255, #6678 ) ;
#236495 = ORIENTED_EDGE ( 'NONE', *, *, #69283, .F. ) ;
#236496 = ORIENTED_EDGE ( 'NONE', *, *, #4873, .F. ) ;
#236497 = AXIS2_PLACEMENT_3D ( 'NONE', #252657, #111894, #92306 ) ;
#236498 = AXIS2_PLACEMENT_3D ( 'NONE', #228923, #89394, #153270 ) ;
#236499 = VECTOR ( 'NONE', #107688, 1000.000000000000114 ) ;
#236500 = ORIENTED_EDGE ( 'NONE', *, *, #45224, .T. ) ;
#236501 = EDGE_CURVE ( 'NONE', #38279, #197652, #97538, .T. ) ;
#236502 = DIRECTION ( 'NONE',  ( -1.000000000000000000, 0.000000000000000000, 0.000000000000000000 ) ) ;
#236503 = CARTESIAN_POINT ( 'NONE',  ( 21.14999999999999858, 1.115600667400684642E-11, -127.4593430482987912 ) ) ;
#236504 = ADVANCED_FACE ( 'NONE', ( #206302 ), #240603, .F. ) ;
#236505 = CARTESIAN_POINT ( 'NONE',  ( -2.995603634470829482E-16, 20.31234122566763034, -254.1243692145750401 ) ) ;
#236506 = CARTESIAN_POINT ( 'NONE',  ( -21.05000000000000071, 2.923777413779037548, -208.5507632484912222 ) ) ;
#236507 = DIRECTION ( 'NONE',  ( -0.000000000000000000, 0.9126074666063769270, 0.4088369013363280513 ) ) ;
#236508 = DIRECTION ( 'NONE',  ( -1.836970198721029934E-16, 1.000000000000000000, 0.000000000000000000 ) ) ;
#236509 = CARTESIAN_POINT ( 'NONE',  ( 20.46382478191414833, 8.901379558702615213, -8.545728094883093817 ) ) ;
#236510 = ADVANCED_FACE ( 'NONE', ( #88898 ), #126755, .T. ) ;
#236513 = CARTESIAN_POINT ( 'NONE',  ( 23.14999999999999503, 21.06723286205836487, -233.6551206055687260 ) ) ;
#236512 = CIRCLE ( 'NONE', #124119, 0.09999999999998898659 ) ;
#236511 = CARTESIAN_POINT ( 'NONE',  ( -20.64999999999999858, -9.499999999988846255, -90.60603087734760663 ) ) ;
#236515 = EDGE_CURVE ( 'NONE', #125866, #25377, #60143, .T. ) ;
#236514 = CARTESIAN_POINT ( 'NONE',  ( -21.64999999999999858, 65.95000000001201101, -115.6731074845243796 ) ) ;
#236516 = AXIS2_PLACEMENT_3D ( 'NONE', #91726, #81129, #219364 ) ;
#236517 = DIRECTION ( 'NONE',  ( 1.000000000000000000, 0.000000000000000000, 0.000000000000000000 ) ) ;
#236518 = CARTESIAN_POINT ( 'NONE',  ( 21.07199075132371746, 44.21756374323442174, -236.5497397326664384 ) ) ;
#236519 = ORIENTED_EDGE ( 'NONE', *, *, #94992, .F. ) ;
#236521 = VERTEX_POINT ( 'NONE', #148905 ) ;
#236520 = DIRECTION ( 'NONE',  ( 0.000000000000000000, -0.9908441862701596881, -0.1350103645451904977 ) ) ;
#236522 = ADVANCED_FACE ( 'NONE', ( #26388 ), #61973, .F. ) ;
#236523 = DIRECTION ( 'NONE',  ( 0.7071067811865456854, 0.6824534298470390503, -0.1850873201762214815 ) ) ;
#236524 = ADVANCED_FACE ( 'NONE', ( #109749 ), #228446, .T. ) ;
#236525 = DIRECTION ( 'NONE',  ( 0.000000000000000000, 0.9915357197604972583, -0.1298341882519109536 ) ) ;
#236526 = ORIENTED_EDGE ( 'NONE', *, *, #95372, .T. ) ;
#236527 = PRODUCT_DEFINITION ( 'UNKNOWN', '', #252954, #222571 ) ;
#236528 = CARTESIAN_POINT ( 'NONE',  ( 20.94403535211772294, 10.30632246271647467, -206.5041836778895288 ) ) ;
#236529 = VECTOR ( 'NONE', #178246, 1000.000000000000000 ) ;
#236530 = CARTESIAN_POINT ( 'NONE',  ( -16.87665923198281348, 9.949999999999983302, -20.85000000000000142 ) ) ;
#236531 = ORIENTED_EDGE ( 'NONE', *, *, #36050, .T. ) ;
#236532 = VECTOR ( 'NONE', #236471, 1000.000000000000000 ) ;
#236533 = AXIS2_PLACEMENT_3D ( 'NONE', #101593, #183745, #126327 ) ;
#236534 = CARTESIAN_POINT ( 'NONE',  ( -18.50016250449483479, 10.29766095125276415, -206.4743663933275855 ) ) ;
#236535 = CARTESIAN_POINT ( 'NONE',  ( -20.54999999999999716, 71.65000000001207070, -124.1731074845243228 ) ) ;
#236536 = EDGE_CURVE ( 'NONE', #253511, #5127, #93457, .T. ) ;
#236537 = EDGE_CURVE ( 'NONE', #8118, #239144, #22769, .T. ) ;
#236538 = LINE ( 'NONE', #154485, #32939 ) ;
#236540 = ORIENTED_EDGE ( 'NONE', *, *, #24385, .F. ) ;
#236539 = CARTESIAN_POINT ( 'NONE',  ( 18.49999999999999289, 10.29270135741298731, -72.45736188715193293 ) ) ;
#236541 = ADVANCED_FACE ( 'NONE', ( #31550 ), #152777, .T. ) ;
#236542 = AXIS2_PLACEMENT_3D ( 'NONE', #218038, #156839, #39465 ) ;
#236544 = EDGE_LOOP ( 'NONE', ( #58227, #225894, #62601, #18590 ) ) ;
#236543 = DIRECTION ( 'NONE',  ( 0.000000000000000000, 0.2617529984165152257, 0.9651348961777124202 ) ) ;
#236545 = CARTESIAN_POINT ( 'NONE',  ( -20.94999999999999929, 12.87592094156238964, -205.3750039893633073 ) ) ;
#236546 = CARTESIAN_POINT ( 'NONE',  ( -18.40000000000000213, 11.75000000001113953, -87.85000000000003695 ) ) ;
#236547 = SPHERICAL_SURFACE ( 'NONE', #219287, 0.1000000000000000056 ) ;
#236548 = LINE ( 'NONE', #179186, #186037 ) ;
#236550 = DIRECTION ( 'NONE',  ( -0.000000000000000000, 0.9858629823651696711, 0.1675535138457361073 ) ) ;
#236549 = CARTESIAN_POINT ( 'NONE',  ( -16.93710578446422588, 9.950000000011137047, -154.5811960162002094 ) ) ;
#236551 = CARTESIAN_POINT ( 'NONE',  ( 18.49999999999998934, 18.51212680383529374, -217.3114114048737520 ) ) ;
#236552 = DIRECTION ( 'NONE',  ( 1.000000000000000000, 0.000000000000000000, 0.000000000000000000 ) ) ;
#236553 = DIRECTION ( 'NONE',  ( -1.000000000000000000, 0.000000000000000000, 0.000000000000000000 ) ) ;
#236554 = AXIS2_PLACEMENT_3D ( 'NONE', #32842, #249293, #51038 ) ;
#236555 = CIRCLE ( 'NONE', #11741, 10.00000000000000178 ) ;
#236556 = DIRECTION ( 'NONE',  ( -1.000000000000000000, 0.000000000000000000, 0.000000000000000000 ) ) ;
#236557 = TOROIDAL_SURFACE ( 'NONE', #78341, 0.4000000000000010214, 0.1000000000000000056 ) ;
#236558 = ORIENTED_EDGE ( 'NONE', *, *, #189520, .T. ) ;
#236559 = CIRCLE ( 'NONE', #70004, 0.5000000000000005551 ) ;
#236560 = ORIENTED_EDGE ( 'NONE', *, *, #91877, .F. ) ;
#236561 = ORIENTED_EDGE ( 'NONE', *, *, #205337, .T. ) ;
#236562 = CARTESIAN_POINT ( 'NONE',  ( 21.87500000000000355, 9.750000000011153745, -88.25000000000005684 ) ) ;
#236563 = DIRECTION ( 'NONE',  ( -1.000000000000000000, 2.952720810173289112E-16, 2.061873921506763405E-30 ) ) ;
#236564 = EDGE_LOOP ( 'NONE', ( #170220, #93956, #73789, #194305 ) ) ;
#236566 = EDGE_CURVE ( 'NONE', #514, #251797, #37956, .T. ) ;
#236565 = ORIENTED_EDGE ( 'NONE', *, *, #47798, .T. ) ;
#236567 = AXIS2_PLACEMENT_3D ( 'NONE', #156861, #175158, #199828 ) ;
#236568 = ORIENTED_EDGE ( 'NONE', *, *, #115834, .F. ) ;
#236569 = AXIS2_PLACEMENT_3D ( 'NONE', #65557, #145083, #45991 ) ;
#236570 = ORIENTED_EDGE ( 'NONE', *, *, #110, .T. ) ;
#236572 = CARTESIAN_POINT ( 'NONE',  ( -21.55000000000000071, 53.12864924257549148, -234.3382351616128858 ) ) ;
#236571 = CIRCLE ( 'NONE', #61808, 0.8750000000000007772 ) ;
#236573 = DIRECTION ( 'NONE',  ( 4.377807931758638789E-15, 0.2605042016806672911, 0.9654727137038716656 ) ) ;
#236574 = DIRECTION ( 'NONE',  ( -1.000000000000000000, -7.304098846218134667E-16, 0.000000000000000000 ) ) ;
#236575 = AXIS2_PLACEMENT_3D ( 'NONE', #228494, #112392, #150245 ) ;
#236576 = CARTESIAN_POINT ( 'NONE',  ( -21.04999999999994387, 76.00000000001119815, -36.02310748452479316 ) ) ;
#236577 = CARTESIAN_POINT ( 'NONE',  ( 12.84233041328156766, 9.410538608528868920, -15.43268799714089035 ) ) ;
#236578 = EDGE_CURVE ( 'NONE', #218718, #28211, #201798, .T. ) ;
#236579 = DIRECTION ( 'NONE',  ( 0.000000000000000000, 0.000000000000000000, -1.000000000000000000 ) ) ;
#236580 = SPHERICAL_SURFACE ( 'NONE', #170291, 0.1000000000000000056 ) ;
#236582 = ORIENTED_EDGE ( 'NONE', *, *, #113222, .F. ) ;
#236581 = CYLINDRICAL_SURFACE ( 'NONE', #59111, 0.09999999999999939493 ) ;
#236584 = CARTESIAN_POINT ( 'NONE',  ( -21.05000000000000071, 5.850000000011105428, -144.1324972242779836 ) ) ;
#236583 = DIRECTION ( 'NONE',  ( -0.000000000000000000, 0.1298341882519953583, 0.9915357197604862671 ) ) ;
#236585 = CIRCLE ( 'NONE', #157532, 0.1000000000000002831 ) ;
#236586 = CARTESIAN_POINT ( 'NONE',  ( 20.94999999999999929, 4.481636728799211156, -245.1292951062512770 ) ) ;
#236587 = ORIENTED_EDGE ( 'NONE', *, *, #15182, .F. ) ;
#236588 = CARTESIAN_POINT ( 'NONE',  ( -16.90987985657661241, 63.08324549817244531, -213.1069633031077615 ) ) ;
#236590 = ADVANCED_FACE ( 'NONE', ( #233577 ), #215283, .F. ) ;
#236589 = CARTESIAN_POINT ( 'NONE',  ( -21.05000000000000071, 0.5450571430110628945, -208.9664790259058691 ) ) ;
#236591 = EDGE_LOOP ( 'NONE', ( #19599, #169805, #200653, #62634 ) ) ;
#236593 = DIRECTION ( 'NONE',  ( 0.000000000000000000, -1.000000000000000000, 0.000000000000000000 ) ) ;
#236592 = LINE ( 'NONE', #193637, #3295 ) ;
#236594 = ADVANCED_FACE ( 'NONE', ( #71934 ), #130880, .F. ) ;
#236595 = CARTESIAN_POINT ( 'NONE',  ( -22.37643362114956957, 75.90091862633062192, -110.6488974784827093 ) ) ;
#236596 = DIRECTION ( 'NONE',  ( 1.000000000000000000, 0.000000000000000000, 0.000000000000000000 ) ) ;
#236598 = VERTEX_POINT ( 'NONE', #113615 ) ;
#236597 = CIRCLE ( 'NONE', #124204, 0.1000000000000055705 ) ;
#236599 = EDGE_LOOP ( 'NONE', ( #124146, #56149 ) ) ;
#236600 = ADVANCED_FACE ( 'NONE', ( #194466 ), #231022, .T. ) ;
#236602 = EDGE_CURVE ( 'NONE', #155368, #233091, #1868, .T. ) ;
#236601 = CARTESIAN_POINT ( 'NONE',  ( 22.45463910399150009, 64.18196446322802728, -247.0985338208812436 ) ) ;
#236603 = CARTESIAN_POINT ( 'NONE',  ( -18.50000000000000000, -0.5913595841389520658, -242.4574432119242999 ) ) ;
#236604 = FACE_OUTER_BOUND ( 'NONE', #238566, .T. ) ;
#236605 = DIRECTION ( 'NONE',  ( -1.000000000000000000, 0.000000000000000000, -0.000000000000000000 ) ) ;
#236606 = ORIENTED_EDGE ( 'NONE', *, *, #128282, .T. ) ;
#236607 = DIRECTION ( 'NONE',  ( 0.000000000000000000, -2.255140518769784599E-13, 1.000000000000000000 ) ) ;
#236608 = VECTOR ( 'NONE', #162521, 1000.000000000000000 ) ;
#236609 = AXIS2_PLACEMENT_3D ( 'NONE', #163454, #201287, #87747 ) ;
#236610 = CARTESIAN_POINT ( 'NONE',  ( -23.25000000000000000, 71.75000000001229239, -157.8731074845243825 ) ) ;
#236611 = CARTESIAN_POINT ( 'NONE',  ( 18.59999999999999432, 77.63717271298298783, -191.9409541190523214 ) ) ;
#236612 = AXIS2_PLACEMENT_3D ( 'NONE', #245330, #86215, #66690 ) ;
#236613 = CARTESIAN_POINT ( 'NONE',  ( -20.15000000000000568, 9.291421356248463326, -112.7500000000000284 ) ) ;
#236614 = EDGE_CURVE ( 'NONE', #239159, #123863, #64255, .T. ) ;
#236616 = ADVANCED_FACE ( 'NONE', ( #74539 ), #117477, .T. ) ;
#236615 = CARTESIAN_POINT ( 'NONE',  ( 20.94999999999999929, -9.399999999988844834, -191.1060308773475072 ) ) ;
#236617 = CIRCLE ( 'NONE', #124217, 0.1000000000000124678 ) ;
#236619 = ORIENTED_EDGE ( 'NONE', *, *, #256570, .F. ) ;
#236618 = DIRECTION ( 'NONE',  ( 6.938893903907991995E-14, 0.000000000000000000, -1.000000000000000000 ) ) ;
#236620 = CARTESIAN_POINT ( 'NONE',  ( 21.05000000000000071, -11.48912529307605546, -30.50000000000000000 ) ) ;
#236621 = DIRECTION ( 'NONE',  ( 0.000000000000000000, 7.116814260417668513E-15, -1.000000000000000000 ) ) ;
#236622 = CARTESIAN_POINT ( 'NONE',  ( 20.94999999999999929, 5.400000000011154988, -45.90526601891310321 ) ) ;
#236623 = DIRECTION ( 'NONE',  ( 9.044546369203337730E-15, 0.7397360091702647189, 0.6728971962616949742 ) ) ;
#236624 = EDGE_CURVE ( 'NONE', #156778, #118009, #89184, .T. ) ;
#236625 = DIRECTION ( 'NONE',  ( 1.000000000000000000, 0.000000000000000000, 0.000000000000000000 ) ) ;
#236627 = ORIENTED_EDGE ( 'NONE', *, *, #183227, .F. ) ;
#236626 = CARTESIAN_POINT ( 'NONE',  ( -18.59999999999999787, 64.35000000001190301, -96.00830171387039513 ) ) ;
#236628 = CARTESIAN_POINT ( 'NONE',  ( 22.49436431346199683, 64.35004905235891215, -170.0900110142466986 ) ) ;
#236629 = AXIS2_PLACEMENT_3D ( 'NONE', #126863, #51145, #125571 ) ;
#236630 = DIRECTION ( 'NONE',  ( 1.000000000000000000, 1.541880601228652843E-16, 2.878400969107353907E-16 ) ) ;
#236631 = FACE_OUTER_BOUND ( 'NONE', #34106, .T. ) ;
#236632 = ORIENTED_EDGE ( 'NONE', *, *, #137316, .F. ) ;
#236633 = CYLINDRICAL_SURFACE ( 'NONE', #221893, 11.75000000000001066 ) ;
#236634 = LINE ( 'NONE', #257431, #19362 ) ;
#236635 = LINE ( 'NONE', #94558, #154679 ) ;
#236636 = VECTOR ( 'NONE', #251025, 999.9999999999998863 ) ;
#236637 = CIRCLE ( 'NONE', #11824, 0.1000000000000002554 ) ;
#236638 = EDGE_CURVE ( 'NONE', #78910, #61591, #189157, .T. ) ;
#236639 = CARTESIAN_POINT ( 'NONE',  ( 21.05000000000000071, 6.650000000011155876, -177.5170271704400022 ) ) ;
#236640 = AXIS2_PLACEMENT_3D ( 'NONE', #220282, #140723, #41649 ) ;
#236641 = ADVANCED_FACE ( 'NONE', ( #214009 ), #35404, .T. ) ;
#236642 = CARTESIAN_POINT ( 'NONE',  ( -22.60000000000080789, 0.04781698047652398198, -88.74997756884729938 ) ) ;
#236643 = AXIS2_PLACEMENT_3D ( 'NONE', #59751, #79323, #143149 ) ;
#236644 = CARTESIAN_POINT ( 'NONE',  ( 18.59999999999999076, 33.78581792236875003, -236.3841486493325874 ) ) ;
#236645 = ORIENTED_EDGE ( 'NONE', *, *, #47275, .F. ) ;
#236646 = ORIENTED_EDGE ( 'NONE', *, *, #110966, .F. ) ;
#236647 = ADVANCED_FACE ( 'NONE', ( #56190 ), #172359, .F. ) ;
#236648 = DIRECTION ( 'NONE',  ( 0.000000000000000000, 0.2617529984165152257, 0.9651348961777124202 ) ) ;
#236649 = DIRECTION ( 'NONE',  ( -0.000000000000000000, -0.000000000000000000, -1.000000000000000000 ) ) ;
#236650 = CARTESIAN_POINT ( 'NONE',  ( 20.94999999999999929, 76.00000000001244871, -170.0231074845243597 ) ) ;
#236651 = DIRECTION ( 'NONE',  ( -1.000000000000000000, 0.000000000000000000, 0.000000000000000000 ) ) ;
#236652 = ORIENTED_EDGE ( 'NONE', *, *, #61673, .F. ) ;
#236653 = EDGE_CURVE ( 'NONE', #4288, #22691, #185245, .T. ) ;
#236654 = ADVANCED_FACE ( 'NONE', ( #17107, #96590 ), #255645, .F. ) ;
#236655 = CARTESIAN_POINT ( 'NONE',  ( -21.05000000000000071, 6.093673009692400555, -199.5727803633481301 ) ) ;
#236656 = AXIS2_PLACEMENT_3D ( 'NONE', #44286, #168121, #243755 ) ;
#236657 = DIRECTION ( 'NONE',  ( -1.000000000000000000, -1.836970198721029934E-16, -3.186635328391151676E-31 ) ) ;
#236658 = FACE_OUTER_BOUND ( 'NONE', #17982, .T. ) ;
#236659 = DIRECTION ( 'NONE',  ( 1.000000000000000000, 0.000000000000000000, 0.000000000000000000 ) ) ;
#236660 = EDGE_LOOP ( 'NONE', ( #142756, #48813, #172953, #143424 ) ) ;
#236661 = SPHERICAL_SURFACE ( 'NONE', #119368, 0.1000000000000000056 ) ;
#236662 = ORIENTED_EDGE ( 'NONE', *, *, #47565, .T. ) ;
#236663 = ORIENTED_EDGE ( 'NONE', *, *, #203900, .T. ) ;
#236664 = CARTESIAN_POINT ( 'NONE',  ( -21.05000000000000071, 86.48473784507379492, -209.3714211149925575 ) ) ;
#236665 = ORIENTED_EDGE ( 'NONE', *, *, #93407, .F. ) ;
#236666 = CARTESIAN_POINT ( 'NONE',  ( 21.05000000000000071, -8.999999999988842703, -124.6060308773475924 ) ) ;
#236667 = DIRECTION ( 'NONE',  ( 1.000000000000000000, 0.000000000000000000, 0.000000000000000000 ) ) ;
#236668 = DIRECTION ( 'NONE',  ( 1.000000000000000000, 0.000000000000000000, 0.000000000000000000 ) ) ;
#236669 = ORIENTED_EDGE ( 'NONE', *, *, #99661, .F. ) ;
#236670 = CARTESIAN_POINT ( 'NONE',  ( 20.94999999999999929, 1.115600667400684642E-11, -67.00000000000000000 ) ) ;
#236672 = EDGE_LOOP ( 'NONE', ( #184699, #30407, #135458 ) ) ;
#236671 = CARTESIAN_POINT ( 'NONE',  ( 18.49999999999999289, 65.79142135392905288, -145.3206006188949004 ) ) ;
#236673 = FACE_OUTER_BOUND ( 'NONE', #163338, .T. ) ;
#236674 = DIRECTION ( 'NONE',  ( -0.000000000000000000, -0.000000000000000000, -1.000000000000000000 ) ) ;
#236675 = VECTOR ( 'NONE', #40742, 1000.000000000000000 ) ;
#236676 = TOROIDAL_SURFACE ( 'NONE', #41087, 11.89999999999999858, 0.1000000000000000056 ) ;
#236677 = AXIS2_PLACEMENT_3D ( 'NONE', #253604, #131105, #211943 ) ;
#236678 = ADVANCED_FACE ( 'NONE', ( #142161 ), #120070, .T. ) ;
#236679 = VERTEX_POINT ( 'NONE', #242543 ) ;
#236680 = CARTESIAN_POINT ( 'NONE',  ( -20.64999999999999858, 1.115600667400684642E-11, -134.0000000000000284 ) ) ;
#236681 = FACE_OUTER_BOUND ( 'NONE', #24041, .T. ) ;
#236682 = CARTESIAN_POINT ( 'NONE',  ( 20.85000000000000142, 1.115600667400684642E-11, -67.00000000000000000 ) ) ;
#236683 = EDGE_LOOP ( 'NONE', ( #49420, #219891, #124521, #35120 ) ) ;
#236684 = CARTESIAN_POINT ( 'NONE',  ( 21.11101077988997332, 6.423684734737198809, -133.9847147310856883 ) ) ;
#236685 = CARTESIAN_POINT ( 'NONE',  ( 14.22916352759893499, 49.67554723225254065, -233.3568105763834524 ) ) ;
#236686 = DIRECTION ( 'NONE',  ( -1.000000000000000000, 7.304098846218135653E-16, 4.639676173203994055E-30 ) ) ;
#236688 = ORIENTED_EDGE ( 'NONE', *, *, #82280, .T. ) ;
#236687 = B_SPLINE_CURVE_WITH_KNOTS ( 'NONE', 3,
 ( #3801, #44222, #166762, #104162, #183729, #83302, #2495 ),
 .UNSPECIFIED., .F., .F.,
 ( 4, 3, 4 ),
 ( 0.000000000000000000, 3.357501770814691602E-05, 5.199112466349472097E-05 ),
 .UNSPECIFIED. ) ;
#236689 = CIRCLE ( 'NONE', #120035, 0.09999999999999986677 ) ;
#236690 = VECTOR ( 'NONE', #73172, 1000.000000000000000 ) ;
#236691 = ADVANCED_FACE ( 'NONE', ( #121363 ), #226936, .T. ) ;
#236692 = ORIENTED_EDGE ( 'NONE', *, *, #115717, .F. ) ;
#236693 = AXIS2_PLACEMENT_3D ( 'NONE', #29709, #130040, #233035 ) ;
#236694 = ORIENTED_EDGE ( 'NONE', *, *, #219278, .F. ) ;
#236695 = DIRECTION ( 'NONE',  ( -1.000000000000000000, -0.000000000000000000, -0.000000000000000000 ) ) ;
#236696 = CARTESIAN_POINT ( 'NONE',  ( 21.13461538461538680, 8.885417037985614996, -45.85000000000000142 ) ) ;
#236699 = ORIENTED_EDGE ( 'NONE', *, *, #66674, .T. ) ;
#236698 =( BOUNDED_SURFACE ( )  B_SPLINE_SURFACE ( 3, 2, ( 
 ( #98753, #216163, #77937 ),
 ( #37557, #79211, #36281 ),
 ( #100047, #179636, #939 ),
 ( #80474, #160078, #156233 ),
 ( #239599, #220029, #120955 ),
 ( #83042, #67374, #186036 ) ),
 .UNSPECIFIED., .F., .F., .F. ) 
 B_SPLINE_SURFACE_WITH_KNOTS ( ( 4, 2, 4 ),
 ( 3, 3 ),
 ( 0.0001300404313046605199, 0.0003183318589266616056, 0.0005066232865486627185 ),
 ( 0.000000000000000000, 1.000000000000000000 ),
 .UNSPECIFIED. ) 
 GEOMETRIC_REPRESENTATION_ITEM ( )  RATIONAL_B_SPLINE_SURFACE ( (
 ( 1.000000000000000000, 0.7071067811865475727, 1.000000000000000000),
 ( 1.000000000000000000, 0.7625113560539543700, 1.000000000000000000),
 ( 1.000000000000000000, 0.8126073484689319004, 1.000000000000000000),
 ( 1.000000000000000000, 0.8923049332731584071, 1.000000000000000000),
 ( 1.000000000000000000, 0.9231914937770194785, 1.000000000000000000),
 ( 1.000000000000000000, 0.9238795325112901802, 1.000000000000000000) ) ) 
 REPRESENTATION_ITEM ( '' )  SURFACE ( )  );
#236697 = DIRECTION ( 'NONE',  ( -1.000000000000000000, 0.000000000000000000, -0.000000000000000000 ) ) ;
#236700 = CARTESIAN_POINT ( 'NONE',  ( 21.05000000000000071, 8.776282895303632259, -100.5000000000000284 ) ) ;
#236701 = FACE_OUTER_BOUND ( 'NONE', #3440, .T. ) ;
#236702 = PLANE ( 'NONE',  #183714 ) ;
#236703 = CARTESIAN_POINT ( 'NONE',  ( -18.34804628011471195, 11.47316190337353525, -76.25000000000004263 ) ) ;
#236704 = DIRECTION ( 'NONE',  ( 0.000000000000000000, 0.9126074666063751506, 0.4088369013363318816 ) ) ;
#236705 = CARTESIAN_POINT ( 'NONE',  ( -23.25000000000000000, 76.00000000001195133, -103.0231074845243171 ) ) ;
#236707 = ORIENTED_EDGE ( 'NONE', *, *, #107045, .T. ) ;
#236706 = DIRECTION ( 'NONE',  ( -0.000000000000000000, 1.000000000000000000, 6.982962677686266711E-15 ) ) ;
#236709 = VERTEX_POINT ( 'NONE', #3942 ) ;
#236708 = DIRECTION ( 'NONE',  ( -1.000000000000000000, 0.000000000000000000, 0.000000000000000000 ) ) ;
#236711 = CARTESIAN_POINT ( 'NONE',  ( -16.82542659449973499, 51.53883479335955542, -231.9993050559371284 ) ) ;
#236710 = CARTESIAN_POINT ( 'NONE',  ( -16.86445178670630440, 60.91689827996518147, -221.0778870335527415 ) ) ;
#236713 = VERTEX_POINT ( 'NONE', #157929 ) ;
#236712 = FACE_OUTER_BOUND ( 'NONE', #72555, .T. ) ;
#236714 = AXIS2_PLACEMENT_3D ( 'NONE', #60819, #145498, #103784 ) ;
#236715 = EDGE_LOOP ( 'NONE', ( #65362, #189662, #15069, #249295 ) ) ;
#236716 = CARTESIAN_POINT ( 'NONE',  ( -18.58222699835055280, 10.33200063080771969, -106.0931674956643462 ) ) ;
#236718 = CARTESIAN_POINT ( 'NONE',  ( -22.39999999999999858, 67.23127455305841238, -235.8551265064783991 ) ) ;
#236717 = AXIS2_PLACEMENT_3D ( 'NONE', #175918, #15561, #230746 ) ;
#236719 = CARTESIAN_POINT ( 'NONE',  ( -22.48660254037843487, 64.35000000001195986, -103.0731074845243711 ) ) ;
#236720 = DIRECTION ( 'NONE',  ( 0.000000000000000000, -1.000000000000000000, 0.000000000000000000 ) ) ;
#236723 = LINE ( 'NONE', #196319, #230386 ) ;
#236722 = B_SPLINE_CURVE_WITH_KNOTS ( 'NONE', 3,
 ( #64559, #65844, #200229, #124553 ),
 .UNSPECIFIED., .F., .F.,
 ( 4, 4 ),
 ( 3.469446951953614189E-18, 0.0001058379652594603572 ),
 .UNSPECIFIED. ) ;
#236721 = AXIS2_PLACEMENT_3D ( 'NONE', #163238, #227042, #202351 ) ;
#236724 = FACE_OUTER_BOUND ( 'NONE', #72734, .T. ) ;
#236725 = DIRECTION ( 'NONE',  ( 0.000000000000000000, -0.9126074666063770380, -0.4088369013363281068 ) ) ;
#236726 = ORIENTED_EDGE ( 'NONE', *, *, #150804, .F. ) ;
#236727 = ORIENTED_EDGE ( 'NONE', *, *, #230162, .T. ) ;
#236728 = DIRECTION ( 'NONE',  ( 0.000000000000000000, 1.000000000000000000, 0.000000000000000000 ) ) ;
#236729 = ADVANCED_FACE ( 'NONE', ( #80889 ), #181314, .T. ) ;
#236730 = CIRCLE ( 'NONE', #103454, 0.1000000000000002554 ) ;
#236731 = CIRCLE ( 'NONE', #28522, 0.09999999999999939493 ) ;
#236732 = ORIENTED_EDGE ( 'NONE', *, *, #188711, .F. ) ;
#236733 = CARTESIAN_POINT ( 'NONE',  ( 23.40000000000005187, 76.00000000001119815, -31.97310748452479601 ) ) ;
#236734 = CARTESIAN_POINT ( 'NONE',  ( 23.14999999999999858, 76.00000000001195133, -103.0231074845243171 ) ) ;
#236735 = CARTESIAN_POINT ( 'NONE',  ( -15.75000000000000355, 66.65000000001155911, -52.77310748452439526 ) ) ;
#236736 = CIRCLE ( 'NONE', #182800, 0.1000000000000072220 ) ;
#236737 = CARTESIAN_POINT ( 'NONE',  ( -22.39999999999999503, -1.657885652111595665, -193.3876638332971254 ) ) ;
#236738 = ADVANCED_FACE ( 'NONE', ( #182597 ), #39244, .T. ) ;
#236739 = ORIENTED_EDGE ( 'NONE', *, *, #40833, .F. ) ;
#236740 = CARTESIAN_POINT ( 'NONE',  ( -15.57281606413133268, 66.62934494888854431, -118.9972842285434638 ) ) ;
#236741 = ORIENTED_EDGE ( 'NONE', *, *, #87499, .T. ) ;
#236742 = ORIENTED_EDGE ( 'NONE', *, *, #66022, .T. ) ;
#236743 = EDGE_CURVE ( 'NONE', #1224, #36331, #22949, .T. ) ;
#236744 = CIRCLE ( 'NONE', #66067, 0.2000000000000057288 ) ;
#236745 = CARTESIAN_POINT ( 'NONE',  ( -16.88853107394619357, 9.950878483358135185, -87.85293634689227815 ) ) ;
#236746 = CYLINDRICAL_SURFACE ( 'NONE', #175707, 0.09999999999999939493 ) ;
#236747 = CARTESIAN_POINT ( 'NONE',  ( -20.54999999999999716, 1.925233644870972816, -146.7302435331261563 ) ) ;
#236748 = EDGE_LOOP ( 'NONE', ( #144265, #89997, #45360, #211708 ) ) ;
#236749 = DIRECTION ( 'NONE',  ( 0.000000000000000000, -1.000000000000000000, 0.000000000000000000 ) ) ;
#236751 = ADVANCED_FACE ( 'NONE', ( #58750 ), #82160, .F. ) ;
#236750 = CIRCLE ( 'NONE', #132745, 0.09999999999999438505 ) ;
#236753 = ORIENTED_EDGE ( 'NONE', *, *, #88180, .F. ) ;
#236752 = CARTESIAN_POINT ( 'NONE',  ( 17.23472005113827876, 10.30788195450076650, -11.45342313993132599 ) ) ;
#236754 = CARTESIAN_POINT ( 'NONE',  ( 18.39999999999999503, 11.75000000001113953, -146.6500000000000341 ) ) ;
#236755 = ORIENTED_EDGE ( 'NONE', *, *, #109633, .T. ) ;
#236756 = CIRCLE ( 'NONE', #82786, 0.1000000000000013933 ) ;
#236757 = MECHANICAL_DESIGN_GEOMETRIC_PRESENTATION_REPRESENTATION (  '', ( #120305 ), #16056 ) ;
#236758 = CIRCLE ( 'NONE', #124358, 0.1000000000000028644 ) ;
#236759 = CIRCLE ( 'NONE', #199181, 11.64999999999999680 ) ;
#236760 = DIRECTION ( 'NONE',  ( 0.000000000000000000, -6.982962677686266711E-15, 1.000000000000000000 ) ) ;
#236761 = ORIENTED_EDGE ( 'NONE', *, *, #154348, .T. ) ;
#236763 = AXIS2_PLACEMENT_3D ( 'NONE', #21640, #22943, #102413 ) ;
#236762 = DIRECTION ( 'NONE',  ( 0.000000000000000000, -0.000000000000000000, -1.000000000000000000 ) ) ;
#236764 = EDGE_CURVE ( 'NONE', #28455, #234500, #198282, .T. ) ;
#236765 = CARTESIAN_POINT ( 'NONE',  ( 21.13422380239051535, 69.50667348520610744, -69.52310748452435973 ) ) ;
#236766 = CARTESIAN_POINT ( 'NONE',  ( -20.94999999999999929, 87.48912529308871910, -200.5231074845242745 ) ) ;
#236767 = CARTESIAN_POINT ( 'NONE',  ( -16.94445028196808778, 66.00793639031384430, -56.91577730610593733 ) ) ;
#236768 = DIRECTION ( 'NONE',  ( 0.000000000000000000, 0.2128009952263630322, -0.9770955615653309501 ) ) ;
#236769 = B_SPLINE_CURVE_WITH_KNOTS ( 'NONE', 3,
 ( #33897, #249061, #247756, #211198, #32606, #69144, #207364 ),
 .UNSPECIFIED., .F., .F.,
 ( 4, 3, 4 ),
 ( 3.469446951953614189E-18, 3.882884552234413058E-05, 5.798605692158429121E-05 ),
 .UNSPECIFIED. ) ;
#236770 = ORIENTED_EDGE ( 'NONE', *, *, #128832, .F. ) ;
#236771 = CARTESIAN_POINT ( 'NONE',  ( 21.87500000000000355, 9.750000000011153745, -121.7500000000000426 ) ) ;
#236772 = DIRECTION ( 'NONE',  ( -1.000000000000000000, -1.836970198721029934E-16, 0.000000000000000000 ) ) ;
#236773 = CARTESIAN_POINT ( 'NONE',  ( 18.54148534481893407, 10.32532329027886675, -139.5699343018359855 ) ) ;
#236774 = ORIENTED_EDGE ( 'NONE', *, *, #109462, .F. ) ;
#236775 = CARTESIAN_POINT ( 'NONE',  ( -22.39999999999999858, 55.98745301258801987, -232.8057040749261262 ) ) ;
#236777 = ORIENTED_EDGE ( 'NONE', *, *, #128649, .F. ) ;
#236776 = AXIS2_PLACEMENT_3D ( 'NONE', #3287, #42433, #236772 ) ;
#236779 = AXIS2_PLACEMENT_3D ( 'NONE', #225706, #223153, #27577 ) ;
#236778 = CARTESIAN_POINT ( 'NONE',  ( 20.99999999999999645, 66.25000000001261924, -190.8731074845244393 ) ) ;
#236780 = ORIENTED_EDGE ( 'NONE', *, *, #242099, .T. ) ;
#236781 = DIRECTION ( 'NONE',  ( 1.000000000000000000, 0.000000000000000000, 0.000000000000000000 ) ) ;
#236782 = DIRECTION ( 'NONE',  ( -1.000000000000000000, 0.000000000000000000, 0.000000000000000000 ) ) ;
#236784 = VERTEX_POINT ( 'NONE', #143445 ) ;
#236783 = DIRECTION ( 'NONE',  ( -0.7071067811865475727, 0.7071067811865475727, 4.937700262164531476E-15 ) ) ;
#236785 = CARTESIAN_POINT ( 'NONE',  ( -18.43599941264907471, 8.780520693175109415, -245.4165332560983757 ) ) ;
#236786 = VERTEX_POINT ( 'NONE', #60049 ) ;
#236787 = EDGE_CURVE ( 'NONE', #5531, #207164, #40542, .T. ) ;
#236788 = CARTESIAN_POINT ( 'NONE',  ( 21.05000000000000071, 76.00000000001227818, -157.0481074845243938 ) ) ;
#236789 = AXIS2_PLACEMENT_3D ( 'NONE', #183052, #82613, #210004 ) ;
#236790 = CARTESIAN_POINT ( 'NONE',  ( -11.60000000000000320, -9.650000000000005684, 15.00000000000000355 ) ) ;
#236791 = AXIS2_PLACEMENT_3D ( 'NONE', #182875, #6777, #246662 ) ;
#236792 = ORIENTED_EDGE ( 'NONE', *, *, #75961, .T. ) ;
#236793 = ORIENTED_EDGE ( 'NONE', *, *, #42243, .T. ) ;
#236794 = DIRECTION ( 'NONE',  ( 0.000000000000000000, 0.000000000000000000, -1.000000000000000000 ) ) ;
#236795 = CARTESIAN_POINT ( 'NONE',  ( -22.50047199488166072, -3.207573401575996463, -228.1448281418072668 ) ) ;
#236796 = AXIS2_PLACEMENT_3D ( 'NONE', #40433, #138186, #39136 ) ;
#236797 = ORIENTED_EDGE ( 'NONE', *, *, #238272, .T. ) ;
#236798 = CARTESIAN_POINT ( 'NONE',  ( 21.04999999999965610, 10.05849014890098303, -228.1548831405661986 ) ) ;
#236799 = ORIENTED_EDGE ( 'NONE', *, *, #21293, .T. ) ;
#236800 = ORIENTED_EDGE ( 'NONE', *, *, #132175, .F. ) ;
#236801 = CIRCLE ( 'NONE', #165925, 0.09999999999999577283 ) ;
#236802 = ADVANCED_FACE ( 'NONE', ( #160477 ), #122627, .T. ) ;
#236803 = CARTESIAN_POINT ( 'NONE',  ( 22.57856590037848576, 25.93742114931687581, -254.3587877384877345 ) ) ;
#236804 = DIRECTION ( 'NONE',  ( 0.000000000000000000, 0.2617529984165152257, 0.9651348961777124202 ) ) ;
#236805 = AXIS2_PLACEMENT_3D ( 'NONE', #127855, #167011, #246501 ) ;
#236806 = EDGE_CURVE ( 'NONE', #225917, #226855, #99162, .T. ) ;
#236808 = ORIENTED_EDGE ( 'NONE', *, *, #254490, .F. ) ;
#236807 = FACE_OUTER_BOUND ( 'NONE', #60974, .T. ) ;
#236809 = DIRECTION ( 'NONE',  ( -1.000000000000000000, 0.000000000000000000, 0.000000000000000000 ) ) ;
#236810 = AXIS2_PLACEMENT_3D ( 'NONE', #46764, #185010, #24679 ) ;
#236811 = DIRECTION ( 'NONE',  ( 0.000000000000000000, 0.9126074666063660468, 0.4088369013363524762 ) ) ;
#236812 = AXIS2_PLACEMENT_3D ( 'NONE', #79462, #78177, #153935 ) ;
#236813 = CARTESIAN_POINT ( 'NONE',  ( -16.87683809663752399, 52.34166666667894674, -153.2731074845245303 ) ) ;
#236814 = AXIS2_PLACEMENT_3D ( 'NONE', #64259, #223312, #148948 ) ;
#236816 = CYLINDRICAL_SURFACE ( 'NONE', #167619, 12.87499999999999112 ) ;
#236815 = CARTESIAN_POINT ( 'NONE',  ( -21.05000000000000071, -11.74999999998884448, -131.1000000000000227 ) ) ;
#236818 = EDGE_CURVE ( 'NONE', #47775, #79119, #18645, .T. ) ;
#236817 = CARTESIAN_POINT ( 'NONE',  ( -18.79999999999999716, -1.885425182446133885, -11.59641995933507808 ) ) ;
#236819 = DIRECTION ( 'NONE',  ( -0.000000000000000000, -0.000000000000000000, 1.000000000000000000 ) ) ;
#236820 = DIRECTION ( 'NONE',  ( 0.000000000000000000, 0.000000000000000000, 1.000000000000000000 ) ) ;
#236821 = ORIENTED_EDGE ( 'NONE', *, *, #89012, .T. ) ;
#236822 = ORIENTED_EDGE ( 'NONE', *, *, #182922, .F. ) ;
#236823 = CARTESIAN_POINT ( 'NONE',  ( 18.45068634130098673, 85.48650607335510188, -162.9543290533561617 ) ) ;
#236825 = EDGE_LOOP ( 'NONE', ( #229585, #187319, #132808, #252185 ) ) ;
#236824 = PLANE ( 'NONE',  #166885 ) ;
#236826 = ORIENTED_EDGE ( 'NONE', *, *, #253111, .F. ) ;
#236827 = DIRECTION ( 'NONE',  ( -0.000000000000000000, -0.9126074666063770380, -0.4088369013363281068 ) ) ;
#236828 = EDGE_CURVE ( 'NONE', #180506, #16182, #255915, .T. ) ;
#236829 = ORIENTED_EDGE ( 'NONE', *, *, #142375, .T. ) ;
#236830 = CARTESIAN_POINT ( 'NONE',  ( 20.95483826173900255, 8.876166204769987189, -8.546275552899514238 ) ) ;
#236831 = CIRCLE ( 'NONE', #182707, 0.5999999999999968692 ) ;
#236832 = EDGE_CURVE ( 'NONE', #75472, #212207, #93657, .T. ) ;
#236833 = EDGE_CURVE ( 'NONE', #110195, #66925, #239407, .T. ) ;
#236834 = ORIENTED_EDGE ( 'NONE', *, *, #141900, .T. ) ;
#236835 = FILL_AREA_STYLE ('',( #195184 ) ) ;
#236836 = DIRECTION ( 'NONE',  ( -1.000000000000000000, 0.000000000000000000, -0.000000000000000000 ) ) ;
#236838 = ORIENTED_EDGE ( 'NONE', *, *, #30569, .F. ) ;
#236837 = ORIENTED_EDGE ( 'NONE', *, *, #251367, .T. ) ;
#236839 = ORIENTED_EDGE ( 'NONE', *, *, #40743, .T. ) ;
#236840 = VERTEX_POINT ( 'NONE', #140890 ) ;
#236841 = ORIENTED_EDGE ( 'NONE', *, *, #177797, .T. ) ;
#236842 = EDGE_CURVE ( 'NONE', #182384, #46212, #197691, .T. ) ;
#236843 = DIRECTION ( 'NONE',  ( 1.000000000000000000, 0.000000000000000000, 0.000000000000000000 ) ) ;
#236844 = CARTESIAN_POINT ( 'NONE',  ( -18.39999999999999858, -9.519327731092436906, -6.972976376559334888 ) ) ;
#236846 = VERTEX_POINT ( 'NONE', #144718 ) ;
#236845 = LINE ( 'NONE', #58193, #154250 ) ;
#236847 = DIRECTION ( 'NONE',  ( -1.000000000000000000, 0.000000000000000000, 0.000000000000000000 ) ) ;
#236848 = ADVANCED_FACE ( 'NONE', ( #127750 ), #122894, .T. ) ;
#236849 = CARTESIAN_POINT ( 'NONE',  ( -23.25000000000000000, 1.115600667400684642E-11, -167.4999999999999716 ) ) ;
#236851 = ORIENTED_EDGE ( 'NONE', *, *, #115843, .T. ) ;
#236850 = FACE_OUTER_BOUND ( 'NONE', #80312, .T. ) ;
#236852 = CARTESIAN_POINT ( 'NONE',  ( 18.59999999999999787, 77.25000000001185185, -95.22262673010921219 ) ) ;
#236854 = ADVANCED_FACE ( 'NONE', ( #88589 ), #86008, .T. ) ;
#236853 = VERTEX_POINT ( 'NONE', #169477 ) ;
#236855 = DIRECTION ( 'NONE',  ( 1.000000000000000000, 0.000000000000000000, 0.000000000000000000 ) ) ;
#236857 = ORIENTED_EDGE ( 'NONE', *, *, #100388, .F. ) ;
#236856 = DIRECTION ( 'NONE',  ( 0.000000000000000000, -6.982962677686266711E-15, 1.000000000000000000 ) ) ;
#236858 = CARTESIAN_POINT ( 'NONE',  ( 21.13736287352038445, 8.046642376395153562, -146.6500000000000341 ) ) ;
#236859 = DIRECTION ( 'NONE',  ( 0.000000000000000000, 0.8660254037844383745, -0.5000000000000003331 ) ) ;
#236860 = CARTESIAN_POINT ( 'NONE',  ( -20.94999999999999929, 1.162701749949165642, -108.6000000000000227 ) ) ;
#236861 = VERTEX_POINT ( 'NONE', #105571 ) ;
#236862 = AXIS2_PLACEMENT_3D ( 'NONE', #239895, #157824, #219024 ) ;
#236865 = DIRECTION ( 'NONE',  ( 0.000000000000000000, -0.8814952561688476074, 0.4721928772777262417 ) ) ;
#236864 = VECTOR ( 'NONE', #225611, 1000.000000000000000 ) ;
#236863 = CARTESIAN_POINT ( 'NONE',  ( -16.82542659449978473, 9.934499891438610675, -46.24463560002602236 ) ) ;
#236866 = CARTESIAN_POINT ( 'NONE',  ( -14.45422546970484312, 66.54939790392329257, -84.57921152142773735 ) ) ;
#236867 = CIRCLE ( 'NONE', #86826, 0.1000000000000021289 ) ;
#236868 = CARTESIAN_POINT ( 'NONE',  ( 21.14999999999999858, 6.412126976762841046, -199.7058512474018244 ) ) ;
#236869 = CARTESIAN_POINT ( 'NONE',  ( -13.40000000000000036, -11.65000000000000036, 12.30000000000000426 ) ) ;
#236870 = CARTESIAN_POINT ( 'NONE',  ( 20.09999999999999787, 9.750000000011137757, -113.1500000000000483 ) ) ;
#236871 = EDGE_LOOP ( 'NONE', ( #196616, #166588, #35644, #74630 ) ) ;
#236872 = ORIENTED_EDGE ( 'NONE', *, *, #96712, .T. ) ;
#236873 = ORIENTED_EDGE ( 'NONE', *, *, #212609, .T. ) ;
#236874 = DIRECTION ( 'NONE',  ( -2.827886303505248766E-16, -0.8660254037844377084, -0.5000000000000015543 ) ) ;
#236875 = AXIS2_PLACEMENT_3D ( 'NONE', #142610, #43544, #205152 ) ;
#236876 = DIRECTION ( 'NONE',  ( 0.000000000000000000, -6.938893903907222067E-15, 1.000000000000000000 ) ) ;
#236878 = ORIENTED_EDGE ( 'NONE', *, *, #225096, .F. ) ;
#236877 = EDGE_CURVE ( 'NONE', #128733, #236709, #248987, .T. ) ;
#236879 = CARTESIAN_POINT ( 'NONE',  ( -23.25000000000000000, 1.115600667400684642E-11, -134.0000000000000000 ) ) ;
#236880 = ORIENTED_EDGE ( 'NONE', *, *, #27090, .F. ) ;
#236881 = EDGE_CURVE ( 'NONE', #135540, #34933, #64446, .T. ) ;
#236882 = LINE ( 'NONE', #38694, #127443 ) ;
#236883 = DIRECTION ( 'NONE',  ( 1.000000000000000000, 0.000000000000000000, 0.000000000000000000 ) ) ;
#236884 = AXIS2_PLACEMENT_3D ( 'NONE', #17427, #213054, #74875 ) ;
#236885 = CIRCLE ( 'NONE', #86844, 0.1000000000000024342 ) ;
#236887 = EDGE_CURVE ( 'NONE', #102830, #208289, #235131, .T. ) ;
#236886 = VERTEX_POINT ( 'NONE', #183860 ) ;
#236888 = VECTOR ( 'NONE', #205916, 1000.000000000000000 ) ;
#236889 = DIRECTION ( 'NONE',  ( 0.000000000000000000, -0.9915357197604849349, 0.1298341882520056834 ) ) ;
#236890 =( LENGTH_UNIT ( ) NAMED_UNIT ( * ) SI_UNIT ( .MILLI., .METRE. ) );
#236891 = VERTEX_POINT ( 'NONE', #106878 ) ;
#236892 = CIRCLE ( 'NONE', #153562, 0.09999999999999939493 ) ;
#236893 = VERTEX_POINT ( 'NONE', #29950 ) ;
#236894 = ORIENTED_EDGE ( 'NONE', *, *, #7611, .T. ) ;
#236895 = CYLINDRICAL_SURFACE ( 'NONE', #66862, 0.1000000000000013933 ) ;
#236896 = CYLINDRICAL_SURFACE ( 'NONE', #28373, 0.09999999999999804878 ) ;
#236897 = CARTESIAN_POINT ( 'NONE',  ( -16.94445028196808778, 66.00793639031384430, -56.91577730610593733 ) ) ;
#236898 = LINE ( 'NONE', #118241, #65589 ) ;
#236899 = CARTESIAN_POINT ( 'NONE',  ( -20.90000000000000213, 1.212568896937007645, -8.000000000000000000 ) ) ;
#236901 = DIRECTION ( 'NONE',  ( 0.000000000000000000, 0.9908441862701605762, 0.1350103645451835310 ) ) ;
#236900 = CYLINDRICAL_SURFACE ( 'NONE', #12131, 0.1000000000000028644 ) ;
#236903 = VERTEX_POINT ( 'NONE', #108186 ) ;
#236902 = CARTESIAN_POINT ( 'NONE',  ( 23.14999999999999503, 6.450000000011156587, -179.8499999999999943 ) ) ;
#236904 = CARTESIAN_POINT ( 'NONE',  ( -23.25000000000000000, 1.910280373842936141, -46.13136785519893834 ) ) ;
#236905 = VERTEX_POINT ( 'NONE', #50739 ) ;
#236906 = CARTESIAN_POINT ( 'NONE',  ( -21.05000000000000071, 74.25000000001186606, -91.35359592662267403 ) ) ;
#236907 = ORIENTED_EDGE ( 'NONE', *, *, #7036, .F. ) ;
#236908 = VERTEX_POINT ( 'NONE', #165600 ) ;
#236909 = DIRECTION ( 'NONE',  ( -0.000000000000000000, -0.04908394489119836945, -0.9987946567507848261 ) ) ;
#236910 = LINE ( 'NONE', #140370, #85221 ) ;
#236912 = EDGE_CURVE ( 'NONE', #150045, #222817, #146008, .T. ) ;
#236911 = DIRECTION ( 'NONE',  ( 1.000000000000000000, -0.000000000000000000, -0.000000000000000000 ) ) ;
#236913 = VERTEX_POINT ( 'NONE', #203433 ) ;
#236914 = ADVANCED_FACE ( 'NONE', ( #225523 ), #139428, .T. ) ;
#236915 = VECTOR ( 'NONE', #242267, 999.9999999999998863 ) ;
#236916 = AXIS2_PLACEMENT_3D ( 'NONE', #186673, #127974, #47118 ) ;
#236917 = CARTESIAN_POINT ( 'NONE',  ( 20.94999999999999929, 22.90266353732884497, -230.0169390150674076 ) ) ;
#236918 = VERTEX_POINT ( 'NONE', #207297 ) ;
#236919 = ORIENTED_EDGE ( 'NONE', *, *, #255207, .T. ) ;
#236920 = EDGE_CURVE ( 'NONE', #12413, #234336, #246407, .T. ) ;
#236922 = EDGE_CURVE ( 'NONE', #173652, #132976, #156039, .T. ) ;
#236921 = FACE_OUTER_BOUND ( 'NONE', #129995, .T. ) ;
#236923 = ORIENTED_EDGE ( 'NONE', *, *, #124735, .T. ) ;
#236924 = CARTESIAN_POINT ( 'NONE',  ( 19.75857864376268935, 64.35000000001197407, -111.7731074845243739 ) ) ;
#236925 = CARTESIAN_POINT ( 'NONE',  ( 20.94999999999999574, 18.75483929237739744, -228.0790484105328630 ) ) ;
#236926 = ORIENTED_EDGE ( 'NONE', *, *, #41741, .F. ) ;
#236928 = DIRECTION ( 'NONE',  ( 0.000000000000000000, 0.2128009952263552051, -0.9770955615653327264 ) ) ;
#236927 = VECTOR ( 'NONE', #103427, 1000.000000000000000 ) ;
#236929 = CARTESIAN_POINT ( 'NONE',  ( 20.85000000000000142, 77.73670573947892137, -24.50568489690058627 ) ) ;
#236930 = FACE_OUTER_BOUND ( 'NONE', #242962, .T. ) ;
#236931 = VERTEX_POINT ( 'NONE', #149892 ) ;
#236932 = EDGE_CURVE ( 'NONE', #21932, #70242, #226835, .T. ) ;
#236933 = CARTESIAN_POINT ( 'NONE',  ( -23.49999999999994316, 76.00000000001119815, -40.17310748452479174 ) ) ;
#236934 = DIRECTION ( 'NONE',  ( -1.000000000000000000, 7.304098846218133681E-16, -4.217023435051677994E-16 ) ) ;
#236935 = AXIS2_PLACEMENT_3D ( 'NONE', #198928, #20319, #180662 ) ;
#236936 = CARTESIAN_POINT ( 'NONE',  ( -22.41119224318417125, 26.02743912001966464, -254.3139371321002216 ) ) ;
#236937 = VECTOR ( 'NONE', #15662, 1000.000000000000000 ) ;
#236938 = CIRCLE ( 'NONE', #32791, 4.049999999999998046 ) ;
#236939 = EDGE_CURVE ( 'NONE', #131422, #68352, #96987, .T. ) ;
#236940 = ORIENTED_EDGE ( 'NONE', *, *, #118525, .T. ) ;
#236942 = EDGE_CURVE ( 'NONE', #224921, #169291, #143539, .T. ) ;
#236941 = CIRCLE ( 'NONE', #178722, 0.09999999999999749367 ) ;
#236943 = FACE_OUTER_BOUND ( 'NONE', #201424, .T. ) ;
#236944 = ORIENTED_EDGE ( 'NONE', *, *, #34970, .F. ) ;
#236945 = CARTESIAN_POINT ( 'NONE',  ( 20.97239005616515684, 67.12515615866193741, -124.2729546823712070 ) ) ;
#236946 = ADVANCED_FACE ( 'NONE', ( #32530 ), #11661, .F. ) ;
#236947 = LINE ( 'NONE', #38755, #169 ) ;
#236948 = CYLINDRICAL_SURFACE ( 'NONE', #187918, 0.1000000000000013933 ) ;
#236950 = AXIS2_PLACEMENT_3D ( 'NONE', #104430, #21100, #120210 ) ;
#236949 = CARTESIAN_POINT ( 'NONE',  ( 20.95512820512820440, 67.12384868372447499, -191.3731074845244109 ) ) ;
#236951 = DIRECTION ( 'NONE',  ( -0.000000000000000000, -0.000000000000000000, -1.000000000000000000 ) ) ;
#236952 = DIRECTION ( 'NONE',  ( 1.000000000000000000, 0.000000000000000000, 0.000000000000000000 ) ) ;
#236953 = TOROIDAL_SURFACE ( 'NONE', #112063, 0.2000000000000000111, 0.1000000000000000056 ) ;
#236954 = ORIENTED_EDGE ( 'NONE', *, *, #250280, .F. ) ;
#236955 = FACE_OUTER_BOUND ( 'NONE', #16125, .T. ) ;
#236956 = DIRECTION ( 'NONE',  ( 0.000000000000000000, 0.000000000000000000, 1.000000000000000000 ) ) ;
#236957 = CARTESIAN_POINT ( 'NONE',  ( -18.36527282682039441, 77.43243019102997948, -241.6948680535597020 ) ) ;
#236958 = CARTESIAN_POINT ( 'NONE',  ( -21.44999999999999929, 7.150000000011155876, -45.75000000000000000 ) ) ;
#236959 = AXIS2_PLACEMENT_3D ( 'NONE', #178362, #42671, #59635 ) ;
#236960 = EDGE_CURVE ( 'NONE', #8263, #83828, #85248, .T. ) ;
#236961 = EDGE_CURVE ( 'NONE', #172479, #171571, #255328, .T. ) ;
#236962 = CARTESIAN_POINT ( 'NONE',  ( 20.30466543256828160, 66.69576306075612138, -61.26944483313238976 ) ) ;
#236963 = AXIS2_PLACEMENT_3D ( 'NONE', #242646, #64022, #185254 ) ;
#236964 = CIRCLE ( 'NONE', #33003, 0.1000000000000028644 ) ;
#236966 = VERTEX_POINT ( 'NONE', #231995 ) ;
#236965 = AXIS2_PLACEMENT_3D ( 'NONE', #181098, #41596, #80669 ) ;
#236967 = VERTEX_POINT ( 'NONE', #234534 ) ;
#236968 = FACE_OUTER_BOUND ( 'NONE', #90600, .T. ) ;
#236969 = AXIS2_PLACEMENT_3D ( 'NONE', #101789, #86081, #183933 ) ;
#236971 = EDGE_CURVE ( 'NONE', #181378, #212402, #175872, .T. ) ;
#236970 = DIRECTION ( 'NONE',  ( 0.7071067811865474617, 0.7071067811865474617, 0.000000000000000000 ) ) ;
#236972 = CARTESIAN_POINT ( 'NONE',  ( -20.94999999999999929, 0.000000000000000000, -21.80000000000000071 ) ) ;
#236973 = CYLINDRICAL_SURFACE ( 'NONE', #207988, 0.1000000000000028644 ) ;
#236974 = CIRCLE ( 'NONE', #91236, 0.09999999999998898659 ) ;
#236975 = ORIENTED_EDGE ( 'NONE', *, *, #222490, .T. ) ;
#236977 = EDGE_CURVE ( 'NONE', #123927, #201767, #35434, .T. ) ;
#236976 = DIRECTION ( 'NONE',  ( 0.000000000000000000, 0.7397360091702755991, -0.6728971962616832059 ) ) ;
#236978 = EDGE_CURVE ( 'NONE', #104788, #235005, #194153, .T. ) ;
#236979 = CYLINDRICAL_SURFACE ( 'NONE', #175729, 0.5000000000000004441 ) ;
#236980 = ORIENTED_EDGE ( 'NONE', *, *, #64741, .F. ) ;
#236981 = DIRECTION ( 'NONE',  ( -1.000000000000000000, -0.000000000000000000, -0.000000000000000000 ) ) ;
#236983 = B_SPLINE_CURVE_WITH_KNOTS ( 'NONE', 3,
 ( #96274, #136689, #256593, #75478, #255311, #234513 ),
 .UNSPECIFIED., .F., .F.,
 ( 4, 2, 4 ),
 ( 0.000000000000000000, 0.0001568709654583418610, 0.0003137419309166837220 ),
 .UNSPECIFIED. ) ;
#236982 = PRODUCT_DEFINITION_SHAPE ( 'NONE', 'NONE',  #258112 ) ;
#236984 = CARTESIAN_POINT ( 'NONE',  ( 23.14999999999999858, 67.23127455305835554, -235.8551265064784559 ) ) ;
#236985 = CIRCLE ( 'NONE', #224506, 0.09999999999999939493 ) ;
#236986 = AXIS2_PLACEMENT_3D ( 'NONE', #9020, #49429, #51977 ) ;
#236987 = VERTEX_POINT ( 'NONE', #156322 ) ;
#236988 = DIRECTION ( 'NONE',  ( 1.000000000000000000, 0.000000000000000000, 0.000000000000000000 ) ) ;
#236989 = VERTEX_POINT ( 'NONE', #233284 ) ;
#236990 = EDGE_CURVE ( 'NONE', #216113, #171759, #181162, .T. ) ;
#236991 = DIRECTION ( 'NONE',  ( 0.000000000000000000, 0.000000000000000000, -1.000000000000000000 ) ) ;
#236992 = CARTESIAN_POINT ( 'NONE',  ( 23.24999999999999645, 0.000000000000000000, -33.50000000000000000 ) ) ;
#236993 = CARTESIAN_POINT ( 'NONE',  ( -18.39999999999999858, 85.68240343348777799, -29.36626410711146562 ) ) ;
#236994 = DIRECTION ( 'NONE',  ( -1.000000000000000000, 0.000000000000000000, 0.000000000000000000 ) ) ;
#236996 = AXIS2_PLACEMENT_3D ( 'NONE', #230537, #34932, #132727 ) ;
#236995 = CYLINDRICAL_SURFACE ( 'NONE', #256920, 4.000000000000003553 ) ;
#236997 = CARTESIAN_POINT ( 'NONE',  ( 21.05000000000000071, 67.22371710471985295, -161.5351067629400461 ) ) ;
#236998 = CARTESIAN_POINT ( 'NONE',  ( 21.05000000000005400, 66.25000000001119815, -4.623107484524796362 ) ) ;
#236999 = DIRECTION ( 'NONE',  ( 1.000000000000000000, 1.186688945009009831E-16, 0.000000000000000000 ) ) ;
#237000 = CIRCLE ( 'NONE', #220441, 0.1999999999999987899 ) ;
#237001 = DIRECTION ( 'NONE',  ( -1.073024830501117725E-15, 0.2128009952263603954, -0.9770955615653315052 ) ) ;
#237002 = EDGE_CURVE ( 'NONE', #197707, #204139, #52030, .T. ) ;
#237003 = CARTESIAN_POINT ( 'NONE',  ( -20.64999999999999858, -8.999999999988844479, -57.10603087734755690 ) ) ;
#237004 = AXIS2_PLACEMENT_3D ( 'NONE', #213580, #105138, #124762 ) ;
#237005 = FACE_OUTER_BOUND ( 'NONE', #218636, .T. ) ;
#237006 = CARTESIAN_POINT ( 'NONE',  ( -18.39999999999999858, 85.60000000001186038, -96.32291809330219223 ) ) ;
#237007 = DIRECTION ( 'NONE',  ( 1.000000000000000000, -0.000000000000000000, -0.000000000000000000 ) ) ;
#237008 = DIRECTION ( 'NONE',  ( -1.000000000000000000, 0.000000000000000000, 0.000000000000000000 ) ) ;
#237009 = CYLINDRICAL_SURFACE ( 'NONE', #237054, 0.09999999999999939493 ) ;
#237010 = CIRCLE ( 'NONE', #166304, 0.1000000000000033362 ) ;
#237011 = VERTEX_POINT ( 'NONE', #251527 ) ;
#237012 = DIRECTION ( 'NONE',  ( 0.000000000000000000, -0.8096735173027155286, 0.5868805631290315850 ) ) ;
#237013 = CARTESIAN_POINT ( 'NONE',  ( -22.94999999999999929, 1.212568896937007645, -8.000000000000000000 ) ) ;
#237014 = EDGE_CURVE ( 'NONE', #3738, #72694, #131587, .T. ) ;
#237015 = ORIENTED_EDGE ( 'NONE', *, *, #6121, .T. ) ;
#237016 = CARTESIAN_POINT ( 'NONE',  ( -21.55000000000000426, 7.750000000011159074, -121.7500000000000426 ) ) ;
#237017 = AXIS2_PLACEMENT_3D ( 'NONE', #257758, #115740, #253947 ) ;
#237018 = DIRECTION ( 'NONE',  ( 1.000000000000000000, 1.394253735153569469E-16, 2.602809386958778209E-16 ) ) ;
#237019 = VECTOR ( 'NONE', #114942, 1000.000000000000000 ) ;
#237020 = ORIENTED_EDGE ( 'NONE', *, *, #165556, .F. ) ;
#237021 = FACE_OUTER_BOUND ( 'NONE', #152132, .T. ) ;
#237022 = CARTESIAN_POINT ( 'NONE',  ( 23.15000000000000213, 87.65000000001214175, -136.5231074845242176 ) ) ;
#237023 = EDGE_CURVE ( 'NONE', #198612, #79398, #247781, .T. ) ;
#237024 = ORIENTED_EDGE ( 'NONE', *, *, #66823, .F. ) ;
#237025 = AXIS2_PLACEMENT_3D ( 'NONE', #245835, #125871, #237187 ) ;
#237026 = VERTEX_POINT ( 'NONE', #110736 ) ;
#237027 = DIRECTION ( 'NONE',  ( 0.000000000000000000, 1.000000000000000000, 0.000000000000000000 ) ) ;
#237028 = ORIENTED_EDGE ( 'NONE', *, *, #255942, .T. ) ;
#237029 = DIRECTION ( 'NONE',  ( -0.000000000000000000, -0.1298341882520022694, -0.9915357197604853789 ) ) ;
#237030 = CARTESIAN_POINT ( 'NONE',  ( 23.14999999999999858, 76.00000000001244871, -170.0231074845243597 ) ) ;
#237031 = CARTESIAN_POINT ( 'NONE',  ( 21.72449340488910252, 10.28395627750227526, -176.7499999999999716 ) ) ;
#237032 = CARTESIAN_POINT ( 'NONE',  ( -23.49999999999994316, 74.16448838626247664, -47.52760213295649550 ) ) ;
#237033 = CARTESIAN_POINT ( 'NONE',  ( -23.25000000000000000, 78.45218979564165807, -232.7313097695096076 ) ) ;
#237034 = LINE ( 'NONE', #238303, #12468 ) ;
#237035 = CYLINDRICAL_SURFACE ( 'NONE', #38703, 0.09999999999998898659 ) ;
#237036 = CARTESIAN_POINT ( 'NONE',  ( 22.39999999999999503, 0.2612980822699546568, -230.0539506776466965 ) ) ;
#237038 = VERTEX_POINT ( 'NONE', #192858 ) ;
#237037 = CARTESIAN_POINT ( 'NONE',  ( 20.85000000000000142, 87.75000000001190870, -105.9231074845242091 ) ) ;
#237039 = EDGE_LOOP ( 'NONE', ( #22384, #51716, #56817, #114273 ) ) ;
#237042 = DIRECTION ( 'NONE',  ( 0.000000000000000000, -7.086529944415894657E-15, 1.000000000000000000 ) ) ;
#237041 = CARTESIAN_POINT ( 'NONE',  ( 18.59999999999999432, 38.30077178631847801, -261.1858881914067751 ) ) ;
#237040 = CIRCLE ( 'NONE', #24867, 0.09999999999999939493 ) ;
#237044 = ORIENTED_EDGE ( 'NONE', *, *, #9305, .T. ) ;
#237043 = CYLINDRICAL_SURFACE ( 'NONE', #169462, 11.75000000000001066 ) ;
#237045 = ORIENTED_EDGE ( 'NONE', *, *, #223299, .F. ) ;
#237046 = DIRECTION ( 'NONE',  ( -1.000000000000000000, -0.000000000000000000, -0.000000000000000000 ) ) ;
#237047 = DIRECTION ( 'NONE',  ( 1.000000000000000000, 0.000000000000000000, 0.000000000000000000 ) ) ;
#237048 = CARTESIAN_POINT ( 'NONE',  ( 18.51565452909384391, -9.352859338836742253, -7.194909321233445176 ) ) ;
#237049 = CARTESIAN_POINT ( 'NONE',  ( 18.79999999999999716, 6.841561409100513025, 9.675512259591560138 ) ) ;
#237050 = CYLINDRICAL_SURFACE ( 'NONE', #68800, 0.1000000000000028644 ) ;
#237051 = CARTESIAN_POINT ( 'NONE',  ( 20.85000000000000142, 76.00000000001136868, -28.22310748452431994 ) ) ;
#237052 = EDGE_CURVE ( 'NONE', #112216, #164531, #155033, .T. ) ;
#237053 = DIRECTION ( 'NONE',  ( -1.000000000000000000, 0.000000000000000000, 0.000000000000000000 ) ) ;
#237054 = AXIS2_PLACEMENT_3D ( 'NONE', #244685, #124763, #165166 ) ;
#237055 = ORIENTED_EDGE ( 'NONE', *, *, #71482, .F. ) ;
#237056 = ORIENTED_EDGE ( 'NONE', *, *, #40008, .T. ) ;
#237057 = AXIS2_PLACEMENT_3D ( 'NONE', #187823, #10456, #9166 ) ;
#237058 = CARTESIAN_POINT ( 'NONE',  ( 21.05000000000000071, 85.50000000001149658, -45.91707660717669626 ) ) ;
#237059 = AXIS2_PLACEMENT_3D ( 'NONE', #60894, #217394, #38785 ) ;
#237060 = AXIS2_PLACEMENT_3D ( 'NONE', #68500, #148036, #227561 ) ;
#237061 = VERTEX_POINT ( 'NONE', #132886 ) ;
#237062 = CARTESIAN_POINT ( 'NONE',  ( 18.39999999999999503, 11.75000000001113953, -113.1500000000000341 ) ) ;
#237063 = ORIENTED_EDGE ( 'NONE', *, *, #125190, .F. ) ;
#237064 = DIRECTION ( 'NONE',  ( 1.000000000000000000, 0.000000000000000000, 0.000000000000000000 ) ) ;
#237065 = CIRCLE ( 'NONE', #203745, 0.3999999999999975797 ) ;
#237066 = CARTESIAN_POINT ( 'NONE',  ( 20.84999999999998721, 10.33248238082518711, -39.09484654391314962 ) ) ;
#237067 = DIRECTION ( 'NONE',  ( 0.000000000000000000, 0.000000000000000000, 1.000000000000000000 ) ) ;
#237068 = EDGE_CURVE ( 'NONE', #46074, #101102, #110210, .T. ) ;
#237070 = ORIENTED_EDGE ( 'NONE', *, *, #165643, .T. ) ;
#237069 = CARTESIAN_POINT ( 'NONE',  ( 18.52928932188133970, 65.72071067813062939, -111.8731074845243683 ) ) ;
#237071 = DIRECTION ( 'NONE',  ( 0.000000000000000000, 1.000000000000000000, 6.982962677686266711E-15 ) ) ;
#237072 = EDGE_LOOP ( 'NONE', ( #81252, #190716, #18027, #42002, #2142 ) ) ;
#237073 = DIRECTION ( 'NONE',  ( 0.000000000000000000, -0.1495327102803078179, 0.9887567792719429427 ) ) ;
#237074 = EDGE_CURVE ( 'NONE', #109860, #80961, #181347, .T. ) ;
#237076 = CARTESIAN_POINT ( 'NONE',  ( -18.58735405345342429, 85.56647862034795082, -29.20039283825829202 ) ) ;
#237075 = CIRCLE ( 'NONE', #253623, 7.899999999999990585 ) ;
#237077 = CIRCLE ( 'NONE', #57989, 7.800000000000001599 ) ;
#237078 = CARTESIAN_POINT ( 'NONE',  ( -21.05000000000000426, 76.02103547655181615, -75.82756330647198695 ) ) ;
#237079 = CYLINDRICAL_SURFACE ( 'NONE', #46299, 0.09999999999999530098 ) ;
#237080 = DIRECTION ( 'NONE',  ( -0.7071067811865456854, -0.7071067811865493491, -4.937700262164544098E-15 ) ) ;
#237081 = ORIENTED_EDGE ( 'NONE', *, *, #157075, .F. ) ;
#237082 = LINE ( 'NONE', #179685, #77475 ) ;
#237083 = EDGE_CURVE ( 'NONE', #130647, #86168, #106283, .T. ) ;
#237084 = ORIENTED_EDGE ( 'NONE', *, *, #132722, .T. ) ;
#237087 = ORIENTED_EDGE ( 'NONE', *, *, #61700, .T. ) ;
#237086 = DIRECTION ( 'NONE',  ( 1.000000000000000000, 0.000000000000000000, -0.000000000000000000 ) ) ;
#237085 = CARTESIAN_POINT ( 'NONE',  ( 20.73486653747088582, 7.250000000011182166, -146.6500000000000341 ) ) ;
#237088 = CIRCLE ( 'NONE', #124659, 0.8750000000000007772 ) ;
#237089 = DIRECTION ( 'NONE',  ( -0.000000000000000000, 1.000000000000000000, 7.525063763929033127E-15 ) ) ;
#237090 = ADVANCED_FACE ( 'NONE', ( #135426 ), #168894, .T. ) ;
#237091 = DIRECTION ( 'NONE',  ( -1.000000000000000000, 0.000000000000000000, 0.000000000000000000 ) ) ;
#237092 = VERTEX_POINT ( 'NONE', #15518 ) ;
#237093 = CARTESIAN_POINT ( 'NONE',  ( 18.31572054635679336, 85.54847543579123226, -129.6725373197760689 ) ) ;
#237094 = EDGE_CURVE ( 'NONE', #96528, #35640, #89734, .T. ) ;
#237095 = DIRECTION ( 'NONE',  ( -1.000000000000000000, 0.000000000000000000, 0.000000000000000000 ) ) ;
#237096 = EDGE_CURVE ( 'NONE', #6556, #176194, #210381, .T. ) ;
#237097 = CARTESIAN_POINT ( 'NONE',  ( -22.49917693094574389, -3.100161397270361441, -228.1566209120988731 ) ) ;
#237099 = EDGE_LOOP ( 'NONE', ( #65815, #88248, #120322, #251623, #161911, #253103 ) ) ;
#237098 = CARTESIAN_POINT ( 'NONE',  ( -20.94999999999999929, 70.42128727326085880, -228.5349014959848262 ) ) ;
#237100 = DIRECTION ( 'NONE',  ( 0.000000000000000000, -0.9908441862701791170, 0.1350103645450472789 ) ) ;
#237101 = EDGE_CURVE ( 'NONE', #66847, #62193, #139603, .T. ) ;
#237102 = ORIENTED_EDGE ( 'NONE', *, *, #123473, .F. ) ;
#237103 = DIRECTION ( 'NONE',  ( 0.000000000000000000, 0.9868171638914228216, 0.1618390714546044939 ) ) ;
#237104 = DIRECTION ( 'NONE',  ( 0.000000000000000000, 0.000000000000000000, 1.000000000000000000 ) ) ;
#237105 = CARTESIAN_POINT ( 'NONE',  ( -23.25000000000000000, 82.67551891922275331, -215.5849511313000164 ) ) ;
#237106 = CIRCLE ( 'NONE', #112227, 0.2000000000000057288 ) ;
#237107 = ORIENTED_EDGE ( 'NONE', *, *, #161238, .F. ) ;
#237108 = CARTESIAN_POINT ( 'NONE',  ( -23.25000000000000000, 4.250000000000000000, -21.14999999999999858 ) ) ;
#237109 = ORIENTED_EDGE ( 'NONE', *, *, #86334, .F. ) ;
#237110 = DIRECTION ( 'NONE',  ( -1.000000000000000000, -3.265361837132813093E-16, 0.000000000000000000 ) ) ;
#237111 = DIRECTION ( 'NONE',  ( 0.000000000000000000, 0.2617529984165027912, 0.9651348961777157509 ) ) ;
#237112 = CARTESIAN_POINT ( 'NONE',  ( -20.54999999999999716, 68.70534379447684614, -223.0647885566232560 ) ) ;
#237113 = CIRCLE ( 'NONE', #16543, 4.099999999999998757 ) ;
#237114 = EDGE_LOOP ( 'NONE', ( #171513, #110343, #94327 ) ) ;
#237115 = CARTESIAN_POINT ( 'NONE',  ( 21.11701782572532693, 22.98544320335190605, -230.0636731943965287 ) ) ;
#237116 = EDGE_CURVE ( 'NONE', #224583, #182882, #118797, .T. ) ;
#237117 = PLANE ( 'NONE',  #151398 ) ;
#237118 = CARTESIAN_POINT ( 'NONE',  ( -20.05000000000000426, 9.250000000011157297, -112.8500000000000369 ) ) ;
#237119 = ORIENTED_EDGE ( 'NONE', *, *, #114467, .T. ) ;
#237121 = AXIS2_PLACEMENT_3D ( 'NONE', #181778, #143919, #244300 ) ;
#237120 = DIRECTION ( 'NONE',  ( 1.000000000000000000, 0.000000000000000000, 0.000000000000000000 ) ) ;
#237122 = CARTESIAN_POINT ( 'NONE',  ( -21.64999999999999858, 7.349999999999998757, -12.25000000000000000 ) ) ;
#237123 = DIRECTION ( 'NONE',  ( 0.000000000000000000, 0.000000000000000000, 1.000000000000000000 ) ) ;
#237124 = AXIS2_PLACEMENT_3D ( 'NONE', #94253, #173855, #253327 ) ;
#237125 = EDGE_LOOP ( 'NONE', ( #201663, #174837, #134392, #96653 ) ) ;
#237126 = ADVANCED_FACE ( 'NONE', ( #180994 ), #18052, .T. ) ;
#237127 = LINE ( 'NONE', #19367, #66857 ) ;
#237128 = VERTEX_POINT ( 'NONE', #62323 ) ;
#237130 = ORIENTED_EDGE ( 'NONE', *, *, #221705, .F. ) ;
#237129 = CARTESIAN_POINT ( 'NONE',  ( -21.14999999999999858, 1.115600667400684642E-11, -100.5000000000000284 ) ) ;
#237131 = CIRCLE ( 'NONE', #212211, 12.87499999999999822 ) ;
#237132 = VECTOR ( 'NONE', #23100, 1000.000000000000000 ) ;
#237135 = ORIENTED_EDGE ( 'NONE', *, *, #127016, .F. ) ;
#237134 = ORIENTED_EDGE ( 'NONE', *, *, #215541, .F. ) ;
#237133 = CARTESIAN_POINT ( 'NONE',  ( -21.11101077989000174, 0.01528526891428022040, 6.423684734726124113 ) ) ;
#237136 = DIRECTION ( 'NONE',  ( 0.000000000000000000, 0.9209589331071864615, -0.3896596508878908960 ) ) ;
#237137 = CARTESIAN_POINT ( 'NONE',  ( -20.94999999999999929, 65.70711192142317714, -30.56510546851222188 ) ) ;
#237138 = DIRECTION ( 'NONE',  ( 0.000000000000000000, 0.000000000000000000, -1.000000000000000000 ) ) ;
#237139 = CARTESIAN_POINT ( 'NONE',  ( -16.82542659449979183, 12.41902688977936187, -211.3386554145826608 ) ) ;
#237140 = FACE_OUTER_BOUND ( 'NONE', #45378, .T. ) ;
#237141 = CARTESIAN_POINT ( 'NONE',  ( 21.05000000000000071, 65.43728505328415679, -196.0663053788799743 ) ) ;
#237142 = EDGE_CURVE ( 'NONE', #42744, #99142, #115485, .T. ) ;
#237143 = CONICAL_SURFACE ( 'NONE', #28912, 7.750000000000027534, 0.7853981633974531640 ) ;
#237144 = DIRECTION ( 'NONE',  ( 0.000000000000000000, 6.938893903907234689E-15, -1.000000000000000000 ) ) ;
#237146 = CARTESIAN_POINT ( 'NONE',  ( -18.59999999999999787, 7.021664781900089913, -37.33356540189728889 ) ) ;
#237145 = DIRECTION ( 'NONE',  ( 1.000000000000000000, 0.000000000000000000, 0.000000000000000000 ) ) ;
#237148 = ORIENTED_EDGE ( 'NONE', *, *, #206773, .T. ) ;
#237147 = VECTOR ( 'NONE', #245984, 1000.000000000000000 ) ;
#237149 = CIRCLE ( 'NONE', #232884, 0.09999999999998898659 ) ;
#237150 = ORIENTED_EDGE ( 'NONE', *, *, #20114, .F. ) ;
#237151 = AXIS2_PLACEMENT_3D ( 'NONE', #235883, #177237, #218881 ) ;
#237152 = VERTEX_POINT ( 'NONE', #83119 ) ;
#237153 = CARTESIAN_POINT ( 'NONE',  ( 18.59999999999999787, -1.851028230129704522, -112.1539132694225316 ) ) ;
#237155 = ORIENTED_EDGE ( 'NONE', *, *, #230336, .F. ) ;
#237154 = DIRECTION ( 'NONE',  ( -1.000000000000000000, 3.265361837132813093E-16, 2.280189983783949500E-30 ) ) ;
#237156 = CARTESIAN_POINT ( 'NONE',  ( -18.59999999999999787, 77.25000000001189449, -95.02310748452430289 ) ) ;
#237157 = ORIENTED_EDGE ( 'NONE', *, *, #92473, .T. ) ;
#237158 = AXIS2_PLACEMENT_3D ( 'NONE', #75863, #155443, #234945 ) ;
#237159 = CARTESIAN_POINT ( 'NONE',  ( -18.50000000000000000, 66.65000000001187175, -90.67310748452437963 ) ) ;
#237160 = EDGE_CURVE ( 'NONE', #127382, #168864, #110399, .T. ) ;
#237161 = ORIENTED_EDGE ( 'NONE', *, *, #254398, .F. ) ;
#237162 = DIRECTION ( 'NONE',  ( -6.938893903907222856E-15, 1.000000000000000000, 0.000000000000000000 ) ) ;
#237163 = EDGE_CURVE ( 'NONE', #11383, #243045, #127159, .T. ) ;
#237164 = EDGE_CURVE ( 'NONE', #207105, #71370, #243687, .T. ) ;
#237165 = ORIENTED_EDGE ( 'NONE', *, *, #147953, .F. ) ;
#237166 = CARTESIAN_POINT ( 'NONE',  ( -21.05000000000000071, 77.83534155023598089, -57.86795619196132634 ) ) ;
#237167 = DIRECTION ( 'NONE',  ( 0.000000000000000000, -1.000000000000000000, 0.000000000000000000 ) ) ;
#237168 = AXIS2_PLACEMENT_3D ( 'NONE', #121443, #122717, #61437 ) ;
#237170 = EDGE_LOOP ( 'NONE', ( #122457, #16534, #157531, #232292 ) ) ;
#237169 = VERTEX_POINT ( 'NONE', #179713 ) ;
#237171 = ORIENTED_EDGE ( 'NONE', *, *, #167549, .F. ) ;
#237172 = DIRECTION ( 'NONE',  ( 0.000000000000000000, 0.4999999999999949485, -0.8660254037844415942 ) ) ;
#237173 = VERTEX_POINT ( 'NONE', #201824 ) ;
#237174 = ORIENTED_EDGE ( 'NONE', *, *, #119643, .T. ) ;
#237175 = EDGE_CURVE ( 'NONE', #243244, #230941, #18815, .T. ) ;
#237176 = DIRECTION ( 'NONE',  ( 1.000000000000000000, 0.000000000000000000, 0.000000000000000000 ) ) ;
#237178 = EDGE_LOOP ( 'NONE', ( #48217, #44776 ) ) ;
#237177 = CARTESIAN_POINT ( 'NONE',  ( 18.36493879433202281, -9.500000806177402168, -107.4221486603551909 ) ) ;
#237180 = DIRECTION ( 'NONE',  ( 0.000000000000000000, 6.982962677686266711E-15, -1.000000000000000000 ) ) ;
#237179 = DIRECTION ( 'NONE',  ( 0.000000000000000000, -2.771150684185008344E-14, -1.000000000000000000 ) ) ;
#237181 = CARTESIAN_POINT ( 'NONE',  ( 23.14999999999999147, 71.85000000001237197, -170.0231074845243882 ) ) ;
#237182 = CARTESIAN_POINT ( 'NONE',  ( 20.94999999999999929, -1.835341550224413698, -11.55515129256298046 ) ) ;
#237183 = CARTESIAN_POINT ( 'NONE',  ( 22.47071067811865319, 29.57301391503007082, -252.6169816238249552 ) ) ;
#237184 = ORIENTED_EDGE ( 'NONE', *, *, #629, .T. ) ;
#237185 = CIRCLE ( 'NONE', #124753, 0.09999999999998898659 ) ;
#237186 = EDGE_LOOP ( 'NONE', ( #41523, #138040, #198485, #253707, #72971, #17608, #89227 ) ) ;
#237187 = DIRECTION ( 'NONE',  ( 0.000000000000000000, -0.2700277750006208621, -0.9628525332200221776 ) ) ;
#237188 = CARTESIAN_POINT ( 'NONE',  ( 21.14999999999999503, 75.49601185175264106, -250.2710592679604531 ) ) ;
#237189 = DIRECTION ( 'NONE',  ( -1.000000000000000000, -0.000000000000000000, 0.000000000000000000 ) ) ;
#237190 = VECTOR ( 'NONE', #52910, 1000.000000000000114 ) ;
#237191 = ORIENTED_EDGE ( 'NONE', *, *, #124772, .T. ) ;
#237192 = DIRECTION ( 'NONE',  ( 1.000000000000000000, 2.952720810173289112E-16, -0.000000000000000000 ) ) ;
#237193 = AXIS2_PLACEMENT_3D ( 'NONE', #31677, #175062, #69509 ) ;
#237194 = DIRECTION ( 'NONE',  ( 0.000000000000000000, -6.454785026890385471E-15, 1.000000000000000000 ) ) ;
#237195 = LINE ( 'NONE', #161521, #100938 ) ;
#237196 = ORIENTED_EDGE ( 'NONE', *, *, #87986, .F. ) ;
#237197 = ORIENTED_EDGE ( 'NONE', *, *, #87621, .T. ) ;
#237198 = LINE ( 'NONE', #41585, #150920 ) ;
#237199 = CARTESIAN_POINT ( 'NONE',  ( -16.77902162784673834, 66.05358074280420055, -123.8611162404550186 ) ) ;
#237201 = EDGE_CURVE ( 'NONE', #252329, #180736, #52135, .T. ) ;
#237200 = ORIENTED_EDGE ( 'NONE', *, *, #178390, .F. ) ;
#237202 = CARTESIAN_POINT ( 'NONE',  ( -18.40000000000000213, 11.47316190337364183, -124.6740539331920843 ) ) ;
#237203 = ORIENTED_EDGE ( 'NONE', *, *, #96563, .F. ) ;
#237204 = EDGE_CURVE ( 'NONE', #46322, #111978, #102697, .T. ) ;
#237205 = CARTESIAN_POINT ( 'NONE',  ( -21.05000000000000071, 77.16270174995034381, -161.9231074845243370 ) ) ;
#237206 = DIRECTION ( 'NONE',  ( 0.000000000000000000, -7.109473446599835262E-15, 1.000000000000000000 ) ) ;
#237208 = DIRECTION ( 'NONE',  ( 0.000000000000000000, 0.000000000000000000, -1.000000000000000000 ) ) ;
#237207 = DIRECTION ( 'NONE',  ( 0.000000000000000000, 0.000000000000000000, 1.000000000000000000 ) ) ;
#237209 = AXIS2_PLACEMENT_3D ( 'NONE', #219968, #243379, #180855 ) ;
#237210 = CARTESIAN_POINT ( 'NONE',  ( 18.59999999999996945, 65.66751761918722252, -164.4282609406112670 ) ) ;
#237211 = CARTESIAN_POINT ( 'NONE',  ( -23.15000000000000213, 1.115600667400684642E-11, -134.0000000000000284 ) ) ;
#237212 = CIRCLE ( 'NONE', #212277, 0.09999999999999771572 ) ;
#237213 = EDGE_CURVE ( 'NONE', #225348, #94509, #160507, .T. ) ;
#237214 = CARTESIAN_POINT ( 'NONE',  ( -18.59999999999999787, 85.52395432076444592, -62.64109042769693048 ) ) ;
#237215 = VECTOR ( 'NONE', #119820, 1000.000000000000000 ) ;
#237217 = VERTEX_POINT ( 'NONE', #220115 ) ;
#237216 = EDGE_LOOP ( 'NONE', ( #107878, #100261, #145196, #232649 ) ) ;
#237218 = EDGE_LOOP ( 'NONE', ( #54270, #43809, #156729, #176081, #101359 ) ) ;
#237219 = CARTESIAN_POINT ( 'NONE',  ( 20.94999999999999929, 69.45000000001230944, -160.0060803140843859 ) ) ;
#237220 = CARTESIAN_POINT ( 'NONE',  ( -23.49999999999994316, 76.00000000001119815, -40.07310748452479032 ) ) ;
#237221 = CARTESIAN_POINT ( 'NONE',  ( 18.50000000000000000, 85.40000000001232650, -162.7258477248609836 ) ) ;
#237222 = LINE ( 'NONE', #217622, #188412 ) ;
#237224 = FACE_OUTER_BOUND ( 'NONE', #211478, .T. ) ;
#237223 = CARTESIAN_POINT ( 'NONE',  ( 20.12481660106788084, 9.526343992273943684, -8.226141669093042452 ) ) ;
#237225 = DIRECTION ( 'NONE',  ( -1.000000000000000000, 0.000000000000000000, 0.000000000000000000 ) ) ;
#237226 = ORIENTED_EDGE ( 'NONE', *, *, #81045, .T. ) ;
#237227 = DIRECTION ( 'NONE',  ( 0.000000000000000000, -6.547589603894034005E-15, 1.000000000000000000 ) ) ;
#237228 = VERTEX_POINT ( 'NONE', #158877 ) ;
#237229 = ORIENTED_EDGE ( 'NONE', *, *, #223491, .T. ) ;
#237230 = DIRECTION ( 'NONE',  ( 0.000000000000000000, 0.000000000000000000, 1.000000000000000000 ) ) ;
#237231 = DIRECTION ( 'NONE',  ( -1.000000000000000000, 0.000000000000000000, 0.000000000000000000 ) ) ;
#237232 = CARTESIAN_POINT ( 'NONE',  ( -16.87683809663752399, 66.15000000001153069, -49.42547150272071121 ) ) ;
#237233 = CARTESIAN_POINT ( 'NONE',  ( 12.25000000000000000, 9.350000000011140955, -83.75000000000004263 ) ) ;
#237234 = CIRCLE ( 'NONE', #220662, 0.1999999999999987899 ) ;
#237235 = EDGE_CURVE ( 'NONE', #232247, #86058, #31345, .T. ) ;
#237236 = ORIENTED_EDGE ( 'NONE', *, *, #91786, .T. ) ;
#237237 = ORIENTED_EDGE ( 'NONE', *, *, #159042, .F. ) ;
#237238 = CARTESIAN_POINT ( 'NONE',  ( -21.14999999893415250, 11.75000000001115197, -40.34449534352650346 ) ) ;
#237240 = EDGE_CURVE ( 'NONE', #168945, #123176, #157613, .T. ) ;
#237239 = DIRECTION ( 'NONE',  ( 0.000000000000000000, 0.8814952561688476074, -0.4721928772777262417 ) ) ;
#237241 = EDGE_LOOP ( 'NONE', ( #34120, #187698, #165382, #198351, #87686 ) ) ;
#237242 = CARTESIAN_POINT ( 'NONE',  ( -20.07928932188135107, 66.77928932189314537, -81.77310748452437394 ) ) ;
#237243 = FACE_OUTER_BOUND ( 'NONE', #26107, .T. ) ;
#237244 = CARTESIAN_POINT ( 'NONE',  ( 21.15000000000005542, 77.83551161375991967, -47.52760213295649550 ) ) ;
#237245 = CARTESIAN_POINT ( 'NONE',  ( -20.94999999999999929, 74.14897176987071248, -57.86919421510183525 ) ) ;
#237246 = CARTESIAN_POINT ( 'NONE',  ( -16.79184697841823493, 66.05123833835347114, -90.36896521392186798 ) ) ;
#237247 = CYLINDRICAL_SURFACE ( 'NONE', #41910, 0.1000000000000002554 ) ;
#237248 = EDGE_CURVE ( 'NONE', #230787, #253697, #139176, .T. ) ;
#237250 = CARTESIAN_POINT ( 'NONE',  ( -20.64999999999999858, 1.115600667400684642E-11, -67.00000000000000000 ) ) ;
#237249 = FACE_OUTER_BOUND ( 'NONE', #183741, .T. ) ;
#237251 = CYLINDRICAL_SURFACE ( 'NONE', #33548, 0.09999999999999939493 ) ;
#237252 = TOROIDAL_SURFACE ( 'NONE', #216393, 0.6000000000000009770, 0.1000000000000000056 ) ;
#237253 = CIRCLE ( 'NONE', #54067, 11.75000000000000000 ) ;
#237255 = EDGE_CURVE ( 'NONE', #64290, #223354, #61023, .T. ) ;
#237254 = CARTESIAN_POINT ( 'NONE',  ( -22.49544290803720870, 11.74987023786906981, -133.9346880407418894 ) ) ;
#237256 = DIRECTION ( 'NONE',  ( 0.000000000000000000, -6.454785026890510900E-15, 1.000000000000000000 ) ) ;
#237257 = VECTOR ( 'NONE', #87840, 1000.000000000000000 ) ;
#237258 = AXIS2_PLACEMENT_3D ( 'NONE', #73050, #52145, #152583 ) ;
#237260 = ORIENTED_EDGE ( 'NONE', *, *, #203050, .F. ) ;
#237259 = FACE_OUTER_BOUND ( 'NONE', #188813, .T. ) ;
#237261 = EDGE_CURVE ( 'NONE', #47711, #207209, #48048, .T. ) ;
#237262 = VECTOR ( 'NONE', #251700, 1000.000000000000000 ) ;
#237264 = EDGE_CURVE ( 'NONE', #163484, #120569, #139260, .T. ) ;
#237263 = EDGE_CURVE ( 'NONE', #186847, #46846, #38919, .T. ) ;
#237265 = PLANE ( 'NONE',  #191228 ) ;
#237266 = ORIENTED_EDGE ( 'NONE', *, *, #219897, .T. ) ;
#237267 = CARTESIAN_POINT ( 'NONE',  ( 18.49999999999999289, 69.35000000001222986, -148.6731074845243938 ) ) ;
#237268 = CARTESIAN_POINT ( 'NONE',  ( 22.60000000000000142, 64.10951975586338847, -247.1829665668249447 ) ) ;
#237269 = CIRCLE ( 'NONE', #124835, 0.4000000000000045186 ) ;
#237270 = VERTEX_POINT ( 'NONE', #67444 ) ;
#237272 = AXIS2_PLACEMENT_3D ( 'NONE', #167493, #253085, #36653 ) ;
#237271 = CYLINDRICAL_SURFACE ( 'NONE', #125688, 0.09999999999999939493 ) ;
#237273 = CARTESIAN_POINT ( 'NONE',  ( -23.15000000000000213, 64.35000000001245724, -181.7731074845244450 ) ) ;
#237274 = CARTESIAN_POINT ( 'NONE',  ( 22.40736611211992368, 1.115600667400684642E-11, -21.85042919245520210 ) ) ;
#237275 = EDGE_CURVE ( 'NONE', #86168, #22692, #27245, .T. ) ;
#237276 = CARTESIAN_POINT ( 'NONE',  ( -21.05000000000000071, 5.850000000011156942, -123.8675027757221159 ) ) ;
#237277 = EDGE_CURVE ( 'NONE', #150112, #246301, #81326, .T. ) ;
#237278 = CARTESIAN_POINT ( 'NONE',  ( -1.739115166359751801E-14, 64.35000000001259934, -191.2731074845244450 ) ) ;
#237279 = CYLINDRICAL_SURFACE ( 'NONE', #69748, 0.5000000000000014433 ) ;
#237280 = VERTEX_POINT ( 'NONE', #46582 ) ;
#237281 = CARTESIAN_POINT ( 'NONE',  ( -20.54999999999999716, -3.770473190032741062, -225.9805569534692324 ) ) ;
#237283 = ORIENTED_EDGE ( 'NONE', *, *, #175243, .F. ) ;
#237282 = DIRECTION ( 'NONE',  ( -0.000000000000000000, 1.000000000000000000, 6.982962677686267499E-15 ) ) ;
#237284 = DIRECTION ( 'NONE',  ( 0.000000000000000000, 0.000000000000000000, 1.000000000000000000 ) ) ;
#237285 = EDGE_CURVE ( 'NONE', #235467, #241008, #127427, .T. ) ;
#237286 = CARTESIAN_POINT ( 'NONE',  ( -22.47071067811865319, 68.27992525551432834, -170.1221999392270163 ) ) ;
#237287 = CARTESIAN_POINT ( 'NONE',  ( -21.44999999999999929, 63.56320957583155717, -222.0641766000055668 ) ) ;
#237288 = ORIENTED_EDGE ( 'NONE', *, *, #60149, .F. ) ;
#237289 = DIRECTION ( 'NONE',  ( 0.000000000000000000, 0.1618390714546044939, -0.9868171638914228216 ) ) ;
#237290 = SHAPE_DEFINITION_REPRESENTATION ( #65914, #224939 ) ;
#237291 = EDGE_CURVE ( 'NONE', #56614, #136660, #89566, .T. ) ;
#237292 = CARTESIAN_POINT ( 'NONE',  ( -18.50000000000001066, 85.42130820975087602, -95.78074427047334893 ) ) ;
#237293 = ORIENTED_EDGE ( 'NONE', *, *, #103764, .T. ) ;
#237294 = DIRECTION ( 'NONE',  ( 1.000000000000000000, -0.000000000000000000, -0.000000000000000000 ) ) ;
#237295 = CARTESIAN_POINT ( 'NONE',  ( -18.59999999999999787, 67.67657779757796277, -227.9615671787948372 ) ) ;
#237296 = EDGE_CURVE ( 'NONE', #84927, #113219, #185425, .T. ) ;
#237297 = AXIS2_PLACEMENT_3D ( 'NONE', #75106, #35962, #239289 ) ;
#237298 = LINE ( 'NONE', #99033, #120321 ) ;
#237299 = EDGE_LOOP ( 'NONE', ( #142593, #199809, #75849, #246283 ) ) ;
#237300 = CIRCLE ( 'NONE', #258087, 0.1000000000000007133 ) ;
#237301 = ORIENTED_EDGE ( 'NONE', *, *, #215420, .F. ) ;
#237302 = EDGE_CURVE ( 'NONE', #226175, #241424, #60494, .T. ) ;
#237303 = CARTESIAN_POINT ( 'NONE',  ( -23.25000000000000000, 1.115600667400684642E-11, -134.0000000000000000 ) ) ;
#237304 = DIRECTION ( 'NONE',  ( 0.000000000000000000, -0.2128009952263604232, 0.9770955615653316162 ) ) ;
#237305 = CARTESIAN_POINT ( 'NONE',  ( 21.05000000000000071, 76.00000000001267608, -203.5231074845243597 ) ) ;
#237306 = CARTESIAN_POINT ( 'NONE',  ( 22.49999999999999645, 64.35023708198076520, -203.6119174609113713 ) ) ;
#237307 = CARTESIAN_POINT ( 'NONE',  ( 18.39999999999999503, 8.822561741666397950, -24.25000000000000000 ) ) ;
#237309 = FACE_OUTER_BOUND ( 'NONE', #112450, .T. ) ;
#237308 = CARTESIAN_POINT ( 'NONE',  ( 23.14999999999999503, 64.35000000001195986, -110.0379132551783243 ) ) ;
#237310 = EDGE_CURVE ( 'NONE', #169022, #36888, #25758, .T. ) ;
#237311 = DIRECTION ( 'NONE',  ( 0.000000000000000000, 0.8879235499942239596, 0.4599910535713220838 ) ) ;
#237312 = DIRECTION ( 'NONE',  ( 1.000000000000000000, 0.000000000000000000, 0.000000000000000000 ) ) ;
#237313 = CYLINDRICAL_SURFACE ( 'NONE', #4746, 0.09999999999999939493 ) ;
#237314 = LINE ( 'NONE', #58644, #244699 ) ;
#237315 = VECTOR ( 'NONE', #193071, 1000.000000000000000 ) ;
#237316 = EDGE_LOOP ( 'NONE', ( #106212, #199836, #246761, #41096, #84418, #187866 ) ) ;
#237317 = ORIENTED_EDGE ( 'NONE', *, *, #79767, .T. ) ;
#237318 = AXIS2_PLACEMENT_3D ( 'NONE', #190215, #191520, #192779 ) ;
#237319 = DIRECTION ( 'NONE',  ( 0.000000000000000000, -1.000000000000000000, 0.000000000000000000 ) ) ;
#237321 = DIRECTION ( 'NONE',  ( -1.387778780781345459E-13, -0.4999999999999088507, -0.8660254037844913322 ) ) ;
#237320 = CARTESIAN_POINT ( 'NONE',  ( 21.14250536705908345, 69.48182782313092787, -69.52310748452435973 ) ) ;
#237322 = AXIS2_PLACEMENT_3D ( 'NONE', #204195, #225029, #42558 ) ;
#237323 = FACE_OUTER_BOUND ( 'NONE', #107674, .T. ) ;
#237324 = CARTESIAN_POINT ( 'NONE',  ( 21.05000000000000071, 71.00000000001186606, -90.61784146561124942 ) ) ;
#237325 = EDGE_CURVE ( 'NONE', #160493, #219071, #163994, .T. ) ;
#237326 = DIRECTION ( 'NONE',  ( 0.000000000000000000, -1.000000000000000000, -0.000000000000000000 ) ) ;
#237327 = VERTEX_POINT ( 'NONE', #227799 ) ;
#237328 = VECTOR ( 'NONE', #67592, 1000.000000000000000 ) ;
#237329 = AXIS2_PLACEMENT_3D ( 'NONE', #143674, #157175, #236668 ) ;
#237330 = ORIENTED_EDGE ( 'NONE', *, *, #145437, .F. ) ;
#237331 = DIRECTION ( 'NONE',  ( 0.000000000000000000, -1.000000000000000000, -2.891205793294679805E-16 ) ) ;
#237332 = ORIENTED_EDGE ( 'NONE', *, *, #74173, .T. ) ;
#237333 = CARTESIAN_POINT ( 'NONE',  ( -20.64999999999999858, 6.268811756569107274, -220.3853799378769622 ) ) ;
#237334 = AXIS2_PLACEMENT_3D ( 'NONE', #230172, #228899, #132358 ) ;
#237335 = AXIS2_PLACEMENT_3D ( 'NONE', #48753, #207865, #47454 ) ;
#237337 = COLOUR_RGB ( '', 0.31764706, 0.68627451, 0.89019608) ;
#237336 = DIRECTION ( 'NONE',  ( 1.000000000000000000, 0.000000000000000000, 0.000000000000000000 ) ) ;
#237338 = CIRCLE ( 'NONE', #8207, 0.1999999999999987899 ) ;
#237339 = VECTOR ( 'NONE', #152404, 1000.000000000000000 ) ;
#237340 = ORIENTED_EDGE ( 'NONE', *, *, #90668, .F. ) ;
#237341 = DIRECTION ( 'NONE',  ( -1.000000000000000000, 0.000000000000000000, 0.000000000000000000 ) ) ;
#237342 = VECTOR ( 'NONE', #75262, 1000.000000000000000 ) ;
#237343 = ORIENTED_EDGE ( 'NONE', *, *, #34603, .T. ) ;
#237344 = DIRECTION ( 'NONE',  ( 1.000000000000000000, 0.000000000000000000, 0.000000000000000000 ) ) ;
#237345 = CARTESIAN_POINT ( 'NONE',  ( 21.05000000000000071, -0.09999999998884510910, -27.02295361821015263 ) ) ;
#237346 = LINE ( 'NONE', #59958, #61699 ) ;
#237347 = CARTESIAN_POINT ( 'NONE',  ( -18.41418431465368855, 77.13860723519847795, -241.8264964602994098 ) ) ;
#237348 = CARTESIAN_POINT ( 'NONE',  ( 21.09107601085559835, 65.52757369511267882, -241.9868384472909213 ) ) ;
#237350 = CARTESIAN_POINT ( 'NONE',  ( 18.59999999999996945, 65.66751761918692409, -130.9282609406112670 ) ) ;
#237349 = CARTESIAN_POINT ( 'NONE',  ( 18.59999999999999076, 77.85161776048025217, -24.41991776492064758 ) ) ;
#237351 = CARTESIAN_POINT ( 'NONE',  ( -18.40000000000000213, 70.35000000001181775, -82.17310748452435121 ) ) ;
#237352 = EDGE_LOOP ( 'NONE', ( #165411, #29441, #257442 ) ) ;
#237354 = DIRECTION ( 'NONE',  ( -0.000000000000000000, -0.09425075112713271475, -0.9955484899852801162 ) ) ;
#237353 = LINE ( 'NONE', #200792, #74442 ) ;
#237355 = ORIENTED_EDGE ( 'NONE', *, *, #76171, .T. ) ;
#237357 = ORIENTED_EDGE ( 'NONE', *, *, #86508, .F. ) ;
#237356 = CARTESIAN_POINT ( 'NONE',  ( 21.05000000000000071, -11.64999999998883595, -164.4000000000000057 ) ) ;
#237358 = ORIENTED_EDGE ( 'NONE', *, *, #44504, .F. ) ;
#237359 = DIRECTION ( 'NONE',  ( 0.000000000000000000, 0.8814952561688429444, -0.4721928772777345684 ) ) ;
#237360 = DIRECTION ( 'NONE',  ( 0.000000000000000000, 1.598721155460228258E-14, -1.000000000000000000 ) ) ;
#237361 = DIRECTION ( 'NONE',  ( 0.000000000000000000, -6.982962677686266711E-15, 1.000000000000000000 ) ) ;
#237362 = CARTESIAN_POINT ( 'NONE',  ( -20.65000000000000568, 7.250000000011138646, -46.15000000000000568 ) ) ;
#237363 = EDGE_LOOP ( 'NONE', ( #153589, #80489, #68132 ) ) ;
#237364 = LINE ( 'NONE', #140830, #179424 ) ;
#237365 = DIRECTION ( 'NONE',  ( 0.000000000000000000, -0.9915357197604860451, 0.1298341882519964408 ) ) ;
#237366 = CARTESIAN_POINT ( 'NONE',  ( 21.05000000000000071, 69.34766280046808617, -247.6726305063181144 ) ) ;
#237367 = ORIENTED_EDGE ( 'NONE', *, *, #244823, .T. ) ;
#237368 = VECTOR ( 'NONE', #32845, 1000.000000000000000 ) ;
#237369 = DIRECTION ( 'NONE',  ( 1.000000000000000000, 0.000000000000000000, 0.000000000000000000 ) ) ;
#237370 = EDGE_CURVE ( 'NONE', #54116, #29064, #167865, .T. ) ;
#237371 = VECTOR ( 'NONE', #131601, 1000.000000000000000 ) ;
#237372 = CARTESIAN_POINT ( 'NONE',  ( 21.09813707148777340, 6.385062105736502680, 0.03135149952951371555 ) ) ;
#237373 = ORIENTED_EDGE ( 'NONE', *, *, #53896, .F. ) ;
#237374 = ORIENTED_EDGE ( 'NONE', *, *, #142097, .F. ) ;
#237375 = CARTESIAN_POINT ( 'NONE',  ( -18.39999999999999858, 8.794517532467699183, -245.5155488533044945 ) ) ;
#237376 = AXIS2_PLACEMENT_3D ( 'NONE', #228272, #130438, #49620 ) ;
#237377 = ORIENTED_EDGE ( 'NONE', *, *, #152471, .T. ) ;
#237378 = DIRECTION ( 'NONE',  ( 1.000000000000000000, -0.000000000000000000, -0.000000000000000000 ) ) ;
#237379 = ORIENTED_EDGE ( 'NONE', *, *, #132107, .F. ) ;
#237380 = CARTESIAN_POINT ( 'NONE',  ( 20.93302460841142931, 10.31565961587945246, -173.0364194119178478 ) ) ;
#237381 = DIRECTION ( 'NONE',  ( -1.000000000000000000, -0.000000000000000000, 0.000000000000000000 ) ) ;
#237382 = CYLINDRICAL_SURFACE ( 'NONE', #164220, 0.09999999999999933942 ) ;
#237383 = CARTESIAN_POINT ( 'NONE',  ( 20.95224633520496127, 60.86421059253439125, -225.3282306591363522 ) ) ;
#237385 = EDGE_CURVE ( 'NONE', #173680, #23601, #85419, .T. ) ;
#237384 = AXIS2_PLACEMENT_3D ( 'NONE', #15060, #94569, #192401 ) ;
#237386 = ADVANCED_FACE ( 'NONE', ( #103981 ), #126121, .F. ) ;
#237387 = AXIS2_PLACEMENT_3D ( 'NONE', #157654, #100169, #80611 ) ;
#237388 = LINE ( 'NONE', #99132, #4774 ) ;
#237389 = LINE ( 'NONE', #139546, #140466 ) ;
#237390 = CARTESIAN_POINT ( 'NONE',  ( 20.93284271247462414, 56.02567683926421438, -227.9999002286038774 ) ) ;
#237391 = ORIENTED_EDGE ( 'NONE', *, *, #8599, .F. ) ;
#237394 = DIRECTION ( 'NONE',  ( 1.000000000000000000, 0.000000000000000000, 0.000000000000000000 ) ) ;
#237393 = CARTESIAN_POINT ( 'NONE',  ( -22.14074124539699540, 75.90094710416836676, -177.4131853355681301 ) ) ;
#237392 = VECTOR ( 'NONE', #158040, 1000.000000000000000 ) ;
#237395 = ORIENTED_EDGE ( 'NONE', *, *, #194952, .T. ) ;
#237398 = ORIENTED_EDGE ( 'NONE', *, *, #177727, .F. ) ;
#237397 = CARTESIAN_POINT ( 'NONE',  ( -20.07928932188135107, 66.77928932189388433, -182.2731074845244166 ) ) ;
#237396 = CARTESIAN_POINT ( 'NONE',  ( -23.15000000000000213, 74.00000000001156764, -56.29848556176223440 ) ) ;
#237399 = VERTEX_POINT ( 'NONE', #45321 ) ;
#237400 = DIRECTION ( 'NONE',  ( 0.000000000000000000, 0.000000000000000000, 1.000000000000000000 ) ) ;
#237401 = DIRECTION ( 'NONE',  ( 0.000000000000000000, -6.982962677686266711E-15, 1.000000000000000000 ) ) ;
#237402 = EDGE_CURVE ( 'NONE', #74961, #256383, #186116, .T. ) ;
#237403 = DIRECTION ( 'NONE',  ( 1.836970198721029934E-16, 0.9651348961777157509, -0.2617529984165031243 ) ) ;
#237404 = ORIENTED_EDGE ( 'NONE', *, *, #246433, .T. ) ;
#237405 = CARTESIAN_POINT ( 'NONE',  ( 19.96984138294274302, 16.74228639170174304, -222.6578579384645025 ) ) ;
#237406 = EDGE_CURVE ( 'NONE', #75595, #158102, #204381, .T. ) ;
#237407 = CARTESIAN_POINT ( 'NONE',  ( 18.69999999999999929, 1.350000000000000089, 16.60000000000000142 ) ) ;
#237408 = EDGE_CURVE ( 'NONE', #75742, #52970, #114690, .T. ) ;
#237410 = CARTESIAN_POINT ( 'NONE',  ( 20.95203847575071521, 10.50106053927400751, -7.567071348623560567 ) ) ;
#237409 = DIRECTION ( 'NONE',  ( 0.000000000000000000, 0.000000000000000000, 1.000000000000000000 ) ) ;
#237412 = ORIENTED_EDGE ( 'NONE', *, *, #53040, .F. ) ;
#237411 = CARTESIAN_POINT ( 'NONE',  ( 19.97071067811864609, 11.72071067812981404, -192.1499999999999488 ) ) ;
#237413 = CIRCLE ( 'NONE', #8457, 0.1000000000000002554 ) ;
#237414 = EDGE_CURVE ( 'NONE', #255984, #245034, #39700, .T. ) ;
#237415 = CIRCLE ( 'NONE', #166517, 0.09999999999999939493 ) ;
#237416 = ORIENTED_EDGE ( 'NONE', *, *, #197951, .T. ) ;
#237417 = DIRECTION ( 'NONE',  ( -1.000000000000000000, -0.000000000000000000, -0.000000000000000000 ) ) ;
#237418 = ORIENTED_EDGE ( 'NONE', *, *, #188315, .T. ) ;
#237419 = DIRECTION ( 'NONE',  ( 0.000000000000000000, -0.4999999999999689138, -0.8660254037844565822 ) ) ;
#237420 = EDGE_CURVE ( 'NONE', #114879, #233399, #68879, .T. ) ;
#237421 = VERTEX_POINT ( 'NONE', #63594 ) ;
#237422 = DIRECTION ( 'NONE',  ( 0.000000000000000000, -7.056502275159890832E-15, 1.000000000000000000 ) ) ;
#237423 = FACE_OUTER_BOUND ( 'NONE', #237453, .T. ) ;
#237424 = DIRECTION ( 'NONE',  ( 0.000000000000000000, 0.000000000000000000, -1.000000000000000000 ) ) ;
#237425 = ORIENTED_EDGE ( 'NONE', *, *, #157508, .F. ) ;
#237426 = DIRECTION ( 'NONE',  ( 1.000000000000000000, 0.000000000000000000, 0.000000000000000000 ) ) ;
#237427 = EDGE_CURVE ( 'NONE', #57757, #198148, #190347, .T. ) ;
#237428 = CIRCLE ( 'NONE', #224749, 0.09999999999999892308 ) ;
#237429 = AXIS2_PLACEMENT_3D ( 'NONE', #39487, #255876, #119000 ) ;
#237430 = AXIS2_PLACEMENT_3D ( 'NONE', #242038, #43851, #105054 ) ;
#237431 = DIRECTION ( 'NONE',  ( -1.000000000000000000, 0.000000000000000000, 0.000000000000000000 ) ) ;
#237432 = ORIENTED_EDGE ( 'NONE', *, *, #182304, .F. ) ;
#237433 = AXIS2_PLACEMENT_3D ( 'NONE', #234384, #34951, #213537 ) ;
#237434 = VERTEX_POINT ( 'NONE', #36041 ) ;
#237435 = ORIENTED_EDGE ( 'NONE', *, *, #161141, .F. ) ;
#237436 = DIRECTION ( 'NONE',  ( 0.000000000000000000, 0.000000000000000000, -1.000000000000000000 ) ) ;
#237437 = ORIENTED_EDGE ( 'NONE', *, *, #223551, .F. ) ;
#237439 = VERTEX_POINT ( 'NONE', #209527 ) ;
#237438 = CARTESIAN_POINT ( 'NONE',  ( 22.24259225415828567, 75.90093411655917066, -110.5150453550897254 ) ) ;
#237440 = APPLICATION_CONTEXT ( 'automotive_design' ) ;
#237441 = VERTEX_POINT ( 'NONE', #154718 ) ;
#237442 = VECTOR ( 'NONE', #23050, 1000.000000000000000 ) ;
#237445 = EDGE_LOOP ( 'NONE', ( #76830, #183485, #55851, #69580 ) ) ;
#237444 = ORIENTED_EDGE ( 'NONE', *, *, #140901, .F. ) ;
#237443 = DIRECTION ( 'NONE',  ( 1.000000000000000000, 3.190570557967288949E-16, 6.948722487160392945E-17 ) ) ;
#237446 = CIRCLE ( 'NONE', #145284, 0.5000000000000004441 ) ;
#237447 = ORIENTED_EDGE ( 'NONE', *, *, #250046, .T. ) ;
#237448 = DIRECTION ( 'NONE',  ( 0.000000000000000000, -0.4088369013363783999, 0.9126074666063545004 ) ) ;
#237449 = DIRECTION ( 'NONE',  ( 0.000000000000000000, 0.9126074666063753726, 0.4088369013363320481 ) ) ;
#237450 = EDGE_CURVE ( 'NONE', #216955, #197068, #189537, .T. ) ;
#237451 = FACE_OUTER_BOUND ( 'NONE', #231386, .T. ) ;
#237452 = EDGE_CURVE ( 'NONE', #71853, #223851, #143720, .T. ) ;
#237453 = EDGE_LOOP ( 'NONE', ( #42310, #128813, #148929, #72994 ) ) ;
#237454 = DIRECTION ( 'NONE',  ( 0.000000000000000000, 0.000000000000000000, 1.000000000000000000 ) ) ;
#237455 =( BOUNDED_CURVE ( )  B_SPLINE_CURVE ( 3, ( #124811, #141787, #221312, #101332 ),
 .UNSPECIFIED., .F., .F. ) 
 B_SPLINE_CURVE_WITH_KNOTS ( ( 4, 4 ),
 ( 0.000000000000000000, 1.570796326794896558 ),
 .UNSPECIFIED. ) 
 CURVE ( )  GEOMETRIC_REPRESENTATION_ITEM ( )  RATIONAL_B_SPLINE_CURVE ( ( 1.000000000000000000, 0.8047378541243649375, 0.8047378541243649375, 1.000000000000000000 ) ) 
 REPRESENTATION_ITEM ( '' )  );
#237457 = VERTEX_POINT ( 'NONE', #13904 ) ;
#237456 = CARTESIAN_POINT ( 'NONE',  ( 20.27550659511089037, 13.44185616693652996, -219.4112591824391529 ) ) ;
#237458 = LINE ( 'NONE', #1392, #71434 ) ;
#237460 = VERTEX_POINT ( 'NONE', #171720 ) ;
#237459 = DIRECTION ( 'NONE',  ( 0.000000000000000000, -1.000000000000000000, -6.982962677686266711E-15 ) ) ;
#237461 = EDGE_CURVE ( 'NONE', #97681, #110056, #256258, .T. ) ;
#237462 = EDGE_CURVE ( 'NONE', #237818, #123901, #44149, .T. ) ;
#237463 = ORIENTED_EDGE ( 'NONE', *, *, #165420, .T. ) ;
#237464 = CYLINDRICAL_SURFACE ( 'NONE', #40115, 0.1000000000000075273 ) ;
#237465 = CARTESIAN_POINT ( 'NONE',  ( 18.59999999999999076, 10.25000000001115552, -125.2500000000000284 ) ) ;
#237466 = EDGE_CURVE ( 'NONE', #239914, #44452, #52307, .T. ) ;
#237467 = ORIENTED_EDGE ( 'NONE', *, *, #216948, .T. ) ;
#237468 = EDGE_LOOP ( 'NONE', ( #219061, #179067, #252706, #146561, #33339 ) ) ;
#237470 = VECTOR ( 'NONE', #158210, 1000.000000000000000 ) ;
#237469 = CARTESIAN_POINT ( 'NONE',  ( -16.93339986808596365, 10.00510392857707487, -180.0659936718128336 ) ) ;
#237472 = EDGE_CURVE ( 'NONE', #49667, #20965, #235661, .T. ) ;
#237471 = CARTESIAN_POINT ( 'NONE',  ( 21.05000000000000071, 5.400000000011154988, -112.9052660189131245 ) ) ;
#237473 = EDGE_CURVE ( 'NONE', #218618, #243885, #198073, .T. ) ;
#237475 = ORIENTED_EDGE ( 'NONE', *, *, #20288, .F. ) ;
#237474 = ORIENTED_EDGE ( 'NONE', *, *, #91271, .T. ) ;
#237476 = ORIENTED_EDGE ( 'NONE', *, *, #212451, .F. ) ;
#237477 = CARTESIAN_POINT ( 'NONE',  ( -22.39999999999999858, 64.15556351076547514, -247.1958793361846745 ) ) ;
#237478 = ORIENTED_EDGE ( 'NONE', *, *, #174246, .T. ) ;
#237479 = ORIENTED_EDGE ( 'NONE', *, *, #157776, .T. ) ;
#237480 = EDGE_CURVE ( 'NONE', #232474, #22587, #114873, .T. ) ;
#237481 = FACE_OUTER_BOUND ( 'NONE', #11682, .T. ) ;
#237482 = VECTOR ( 'NONE', #186913, 1000.000000000000000 ) ;
#237483 = EDGE_LOOP ( 'NONE', ( #31319, #211500, #126621, #37836 ) ) ;
#237484 = CARTESIAN_POINT ( 'NONE',  ( 20.94999999999999929, 77.83534155023627932, -91.46795619196132066 ) ) ;
#237486 = CARTESIAN_POINT ( 'NONE',  ( -21.05000000000000071, 1.115600667400684642E-11, -122.2000000000000313 ) ) ;
#237485 = DIRECTION ( 'NONE',  ( 0.000000000000000000, 0.1455152366551700771, 0.9893560106964479628 ) ) ;
#237487 = EDGE_LOOP ( 'NONE', ( #65989, #121708, #239286, #15093 ) ) ;
#237488 = ADVANCED_FACE ( 'NONE', ( #135104 ), #85601, .T. ) ;
#237490 = ORIENTED_EDGE ( 'NONE', *, *, #135527, .F. ) ;
#237489 = ORIENTED_EDGE ( 'NONE', *, *, #189678, .T. ) ;
#237491 = DIRECTION ( 'NONE',  ( 1.000000000000000000, -0.000000000000000000, -0.000000000000000000 ) ) ;
#237492 = DIRECTION ( 'NONE',  ( 1.000000000000000000, 0.000000000000000000, 0.000000000000000000 ) ) ;
#237493 = ADVANCED_FACE ( 'NONE', ( #253770 ), #51706, .T. ) ;
#237494 = EDGE_CURVE ( 'NONE', #48558, #254767, #113000, .T. ) ;
#237496 = ORIENTED_EDGE ( 'NONE', *, *, #138512, .F. ) ;
#237495 = CIRCLE ( 'NONE', #12653, 12.97499999999999964 ) ;
#237497 = CIRCLE ( 'NONE', #129335, 0.1000000000000076938 ) ;
#237498 = ADVANCED_FACE ( 'NONE', ( #232967 ), #149580, .T. ) ;
#237499 = LINE ( 'NONE', #97949, #213222 ) ;
#237500 = EDGE_LOOP ( 'NONE', ( #113553, #82627, #29730, #147232, #65205 ) ) ;
#237501 = EDGE_LOOP ( 'NONE', ( #60048, #219019, #129358, #85914, #88835 ) ) ;
#237502 = DIRECTION ( 'NONE',  ( -1.000000000000000000, 0.000000000000000000, 0.000000000000000000 ) ) ;
#237504 = EDGE_CURVE ( 'NONE', #182894, #146851, #118987, .T. ) ;
#237503 = EDGE_LOOP ( 'NONE', ( #12175, #170472, #31827, #122376 ) ) ;
#237505 = CARTESIAN_POINT ( 'NONE',  ( 11.60000000000000142, -8.279289321881350361, 11.02928932188135036 ) ) ;
#237506 = DIRECTION ( 'NONE',  ( -0.000000000000000000, -1.000000000000000000, -6.982962677686266711E-15 ) ) ;
#237507 = ORIENTED_EDGE ( 'NONE', *, *, #144720, .T. ) ;
#237508 = EDGE_CURVE ( 'NONE', #71159, #8352, #11330, .T. ) ;
#237509 = VECTOR ( 'NONE', #79766, 1000.000000000000000 ) ;
#237510 = FACE_OUTER_BOUND ( 'NONE', #38284, .T. ) ;
#237512 = AXIS2_PLACEMENT_3D ( 'NONE', #6423, #48118, #87231 ) ;
#237511 = CARTESIAN_POINT ( 'NONE',  ( 18.43709777086139923, 85.68240343348847432, -129.8662641071115331 ) ) ;
#237514 = CARTESIAN_POINT ( 'NONE',  ( -16.85697194749126027, 9.908543714134777858, -121.0649957323862367 ) ) ;
#237513 = CARTESIAN_POINT ( 'NONE',  ( 20.12500000000000000, 9.750000000011153745, -155.1500000000000057 ) ) ;
#237515 = DIRECTION ( 'NONE',  ( 0.000000000000000000, -1.000000000000000000, -6.982962677686265922E-15 ) ) ;
#237516 = CARTESIAN_POINT ( 'NONE',  ( -21.05000000000000071, -1.162701749926853712, -108.5000000000000426 ) ) ;
#237517 = CARTESIAN_POINT ( 'NONE',  ( 21.09696443733127325, 65.27599011609382273, -157.7883299574762077 ) ) ;
#237518 = CARTESIAN_POINT ( 'NONE',  ( -16.87372397896795562, 66.11940046337051058, -149.6723829744886416 ) ) ;
#237519 = CARTESIAN_POINT ( 'NONE',  ( 18.60000000000000853, -9.364236010355611484, -74.18025440072464960 ) ) ;
#237520 = CARTESIAN_POINT ( 'NONE',  ( -23.15000000000000213, 11.75000000001115907, -160.6583993101029648 ) ) ;
#237521 = ORIENTED_EDGE ( 'NONE', *, *, #150235, .T. ) ;
#237522 = AXIS2_PLACEMENT_3D ( 'NONE', #70865, #229905, #193364 ) ;
#237523 = VECTOR ( 'NONE', #133025, 1000.000000000000000 ) ;
#237524 = AXIS2_PLACEMENT_3D ( 'NONE', #205111, #149036, #168636 ) ;
#237525 = VECTOR ( 'NONE', #167036, 1000.000000000000000 ) ;
#237527 = ORIENTED_EDGE ( 'NONE', *, *, #240695, .F. ) ;
#237526 = ORIENTED_EDGE ( 'NONE', *, *, #193481, .F. ) ;
#237528 = VERTEX_POINT ( 'NONE', #213364 ) ;
#237529 = EDGE_LOOP ( 'NONE', ( #46832, #77963 ) ) ;
#237530 = CARTESIAN_POINT ( 'NONE',  ( -21.05000000000000071, -1.162701749926853712, -75.00000000000004263 ) ) ;
#237531 = DIRECTION ( 'NONE',  ( 0.000000000000000000, 0.000000000000000000, -1.000000000000000000 ) ) ;
#237533 = DIRECTION ( 'NONE',  ( 0.000000000000000000, -0.8814952561688437216, 0.4721928772777334582 ) ) ;
#237532 = CARTESIAN_POINT ( 'NONE',  ( -21.05000000000000071, 69.74218538953657287, -203.6208977758331855 ) ) ;
#237534 = ORIENTED_EDGE ( 'NONE', *, *, #154673, .F. ) ;
#237535 = DIRECTION ( 'NONE',  ( 0.000000000000000000, 0.000000000000000000, -1.000000000000000000 ) ) ;
#237536 = VECTOR ( 'NONE', #225573, 1000.000000000000114 ) ;
#237537 = LINE ( 'NONE', #77161, #99981 ) ;
#237538 = DIRECTION ( 'NONE',  ( 0.000000000000000000, -0.2617529984165152257, -0.9651348961777124202 ) ) ;
#237539 = CARTESIAN_POINT ( 'NONE',  ( 18.47688499308724985, -9.464855950272971441, -73.70134775313735531 ) ) ;
#237540 = VERTEX_POINT ( 'NONE', #191281 ) ;
#237541 = LINE ( 'NONE', #219242, #26541 ) ;
#237542 = ORIENTED_EDGE ( 'NONE', *, *, #120368, .F. ) ;
#237543 = CARTESIAN_POINT ( 'NONE',  ( -23.49999999999994316, 87.50449464844290048, -37.85861909827351468 ) ) ;
#237544 = DIRECTION ( 'NONE',  ( 0.000000000000000000, 0.000000000000000000, 1.000000000000000000 ) ) ;
#237545 = CARTESIAN_POINT ( 'NONE',  ( 22.39999999999999858, 68.20922040163857503, -103.1231074845243540 ) ) ;
#237546 = FACE_OUTER_BOUND ( 'NONE', #236683, .T. ) ;
#237547 = CARTESIAN_POINT ( 'NONE',  ( -16.87036670365548474, 9.989418819301642216, -20.97956011730203940 ) ) ;
#237548 = ORIENTED_EDGE ( 'NONE', *, *, #76817, .T. ) ;
#237549 = CARTESIAN_POINT ( 'NONE',  ( 18.50000000000000711, 47.12421348240935259, -255.1840482521099318 ) ) ;
#237550 = CARTESIAN_POINT ( 'NONE',  ( -23.25000000000000000, 7.021664781911246322, -204.8335654018972605 ) ) ;
#237551 = VECTOR ( 'NONE', #96597, 1000.000000000000000 ) ;
#237552 = CARTESIAN_POINT ( 'NONE',  ( -23.25000000000000000, 78.48087866980282001, -232.8271061603568910 ) ) ;
#237553 = EDGE_CURVE ( 'NONE', #110197, #252869, #6530, .T. ) ;
#237555 = DIRECTION ( 'NONE',  ( 0.000000000000000000, 1.000000000000000000, -0.000000000000000000 ) ) ;
#237554 = FACE_OUTER_BOUND ( 'NONE', #157164, .T. ) ;
#237556 = CARTESIAN_POINT ( 'NONE',  ( 20.05000000000002913, 7.250000000011171508, -79.65000000000004832 ) ) ;
#237557 = AXIS2_PLACEMENT_3D ( 'NONE', #218825, #119767, #199290 ) ;
#237558 = DIRECTION ( 'NONE',  ( -0.000000000000000000, 0.8660254037844383745, -0.5000000000000003331 ) ) ;
#237560 = ADVANCED_FACE ( 'NONE', ( #81534 ), #201508, .T. ) ;
#237559 = DIRECTION ( 'NONE',  ( 0.000000000000000000, -1.000000000000000000, 0.000000000000000000 ) ) ;
#237561 = CARTESIAN_POINT ( 'NONE',  ( 18.46905048506371472, -9.473744257371233601, -207.6759862922554021 ) ) ;
#237563 = ORIENTED_EDGE ( 'NONE', *, *, #107874, .F. ) ;
#237562 = CIRCLE ( 'NONE', #241643, 0.1000000000000046685 ) ;
#237564 =( BOUNDED_SURFACE ( )  B_SPLINE_SURFACE ( 3, 2, ( 
 ( #133437, #156883, #231275 ),
 ( #35658, #36944, #211710 ),
 ( #194721, #95586, #34366 ),
 ( #33098, #52604, #172614 ) ),
 .UNSPECIFIED., .F., .F., .F. ) 
 B_SPLINE_SURFACE_WITH_KNOTS ( ( 4, 4 ),
 ( 3, 3 ),
 ( 0.0008258556059633768206, 0.0009616864997632838244 ),
 ( 0.000000000000000000, 1.000000000000000000 ),
 .UNSPECIFIED. ) 
 GEOMETRIC_REPRESENTATION_ITEM ( )  RATIONAL_B_SPLINE_SURFACE ( (
 ( 1.000000000000000000, 0.9152888060719408525, 1.000000000000000000),
 ( 1.000000000000000000, 0.9327727094137879815, 1.000000000000000000),
 ( 1.000000000000000000, 0.9369023509258773696, 1.000000000000000000),
 ( 1.000000000000000000, 0.9246339933864253791, 1.000000000000000000) ) ) 
 REPRESENTATION_ITEM ( '' )  SURFACE ( )  );
#237565 = ORIENTED_EDGE ( 'NONE', *, *, #103608, .F. ) ;
#237566 = EDGE_CURVE ( 'NONE', #241330, #46619, #77697, .T. ) ;
#237567 = VECTOR ( 'NONE', #75289, 1000.000000000000114 ) ;
#237568 = DIRECTION ( 'NONE',  ( 0.000000000000000000, 0.000000000000000000, 1.000000000000000000 ) ) ;
#237569 = EDGE_CURVE ( 'NONE', #171566, #223079, #202359, .T. ) ;
#237570 = EDGE_LOOP ( 'NONE', ( #209574, #216231, #102070, #56593 ) ) ;
#237571 = CARTESIAN_POINT ( 'NONE',  ( -23.25000000000000000, 64.25000000001244871, -170.0231074845244166 ) ) ;
#237572 = AXIS2_PLACEMENT_3D ( 'NONE', #104025, #167912, #246138 ) ;
#237573 = DIRECTION ( 'NONE',  ( 0.000000000000000000, 0.2965989261549489275, 0.9550021345545417484 ) ) ;
#237574 = DIRECTION ( 'NONE',  ( 1.000000000000000000, 0.000000000000000000, 0.000000000000000000 ) ) ;
#237575 = VECTOR ( 'NONE', #106990, 1000.000000000000114 ) ;
#237576 = ORIENTED_EDGE ( 'NONE', *, *, #89868, .T. ) ;
#237577 = VECTOR ( 'NONE', #81847, 1000.000000000000000 ) ;
#237578 = CARTESIAN_POINT ( 'NONE',  ( 21.10257677756356998, 0.02495074957913955352, -161.1016182574672655 ) ) ;
#237579 = EDGE_CURVE ( 'NONE', #162975, #157226, #160703, .T. ) ;
#237580 = LINE ( 'NONE', #35552, #182507 ) ;
#237582 = DIRECTION ( 'NONE',  ( 0.000000000000000000, -0.9126074666063545004, -0.4088369013363783999 ) ) ;
#237581 = AXIS2_PLACEMENT_3D ( 'NONE', #75225, #114323, #12684 ) ;
#237583 = DIRECTION ( 'NONE',  ( 0.000000000000000000, 0.000000000000000000, -1.000000000000000000 ) ) ;
#237585 = ORIENTED_EDGE ( 'NONE', *, *, #2726, .F. ) ;
#237584 = DIRECTION ( 'NONE',  ( 0.000000000000000000, 0.9998779222360102414, 0.01562499999996356907 ) ) ;
#237587 = DIRECTION ( 'NONE',  ( 0.000000000000000000, 1.000000000000000000, 0.000000000000000000 ) ) ;
#237586 = DIRECTION ( 'NONE',  ( 1.000000000000000000, -1.186688945009010077E-16, -8.286604613020808509E-31 ) ) ;
#237588 = CARTESIAN_POINT ( 'NONE',  ( -23.15000000000000213, 84.59626168225496201, -112.4732350016745102 ) ) ;
#237589 = CARTESIAN_POINT ( 'NONE',  ( 21.05000000000000071, 54.32225538558145672, -236.1594012422037281 ) ) ;
#237590 = CARTESIAN_POINT ( 'NONE',  ( -19.89999999999999858, 5.488301202077012775, 16.50000000000000000 ) ) ;
#237591 = CYLINDRICAL_SURFACE ( 'NONE', #171088, 0.1000000000000026007 ) ;
#237592 = ORIENTED_EDGE ( 'NONE', *, *, #104355, .T. ) ;
#237593 = CARTESIAN_POINT ( 'NONE',  ( 0.000000000000000000, 0.000000000000000000, 0.000000000000000000 ) ) ;
#237594 = CARTESIAN_POINT ( 'NONE',  ( 18.59999999999999076, 77.83585931145546510, -91.51866831572576189 ) ) ;
#237595 = EDGE_CURVE ( 'NONE', #154058, #22444, #10824, .T. ) ;
#237596 = CIRCLE ( 'NONE', #120910, 0.09999999999999609201 ) ;
#237597 = AXIS2_PLACEMENT_3D ( 'NONE', #215269, #139560, #219101 ) ;
#237598 = ORIENTED_EDGE ( 'NONE', *, *, #214755, .F. ) ;
#237599 = CARTESIAN_POINT ( 'NONE',  ( -16.87683809663752399, 66.15000000001158753, -56.87310748452438958 ) ) ;
#237600 = EDGE_CURVE ( 'NONE', #251509, #81897, #189879, .T. ) ;
#237601 = ORIENTED_EDGE ( 'NONE', *, *, #183091, .F. ) ;
#237602 = LINE ( 'NONE', #38127, #18009 ) ;
#237603 = DIRECTION ( 'NONE',  ( -1.000000000000000000, -0.000000000000000000, -0.000000000000000000 ) ) ;
#237604 = CYLINDRICAL_SURFACE ( 'NONE', #115817, 0.09999999999999939493 ) ;
#237605 = VERTEX_POINT ( 'NONE', #121984 ) ;
#237606 = ORIENTED_EDGE ( 'NONE', *, *, #61654, .F. ) ;
#237607 = ADVANCED_FACE ( 'NONE', ( #235497 ), #18994, .F. ) ;
#237608 = EDGE_CURVE ( 'NONE', #206232, #171717, #255002, .T. ) ;
#237609 = DIRECTION ( 'NONE',  ( 0.9880948137434723000, -0.1538461538461484146, -1.074301950413233906E-15 ) ) ;
#237610 = CARTESIAN_POINT ( 'NONE',  ( 20.94999999999999929, -1.164121893241208960, -41.41484808557160591 ) ) ;
#237611 = CIRCLE ( 'NONE', #141734, 0.09999999999998898659 ) ;
#237612 = CARTESIAN_POINT ( 'NONE',  ( 21.05000000000000071, 71.00000000001199396, -115.4283735034374274 ) ) ;
#237614 = DIRECTION ( 'NONE',  ( 1.000000000000000000, -0.000000000000000000, -0.000000000000000000 ) ) ;
#237613 = CIRCLE ( 'NONE', #95934, 0.5000000000000004441 ) ;
#237616 = DIRECTION ( 'NONE',  ( 0.000000000000000000, 0.000000000000000000, 1.000000000000000000 ) ) ;
#237615 = AXIS2_PLACEMENT_3D ( 'NONE', #65660, #228609, #245596 ) ;
#237617 = ADVANCED_FACE ( 'NONE', ( #175559 ), #179405, .F. ) ;
#237618 = DIRECTION ( 'NONE',  ( 0.000000000000000000, 0.8814952561688430555, -0.4721928772777346239 ) ) ;
#237619 = CARTESIAN_POINT ( 'NONE',  ( -21.65000000000000213, 68.75000000001153921, -48.67310748452437252 ) ) ;
#237620 = CARTESIAN_POINT ( 'NONE',  ( 21.05000000000000071, 85.40000000001178648, -79.41707660717668205 ) ) ;
#237621 = VERTEX_POINT ( 'NONE', #239363 ) ;
#237622 = CARTESIAN_POINT ( 'NONE',  ( -20.94999999999999929, 11.60000000001115517, -127.0717967697245143 ) ) ;
#237624 = ORIENTED_EDGE ( 'NONE', *, *, #38548, .F. ) ;
#237623 = FACE_OUTER_BOUND ( 'NONE', #246274, .T. ) ;
#237625 = AXIS2_PLACEMENT_3D ( 'NONE', #151702, #192097, #228657 ) ;
#237626 = DIRECTION ( 'NONE',  ( 1.000000000000000000, 0.000000000000000000, 0.000000000000000000 ) ) ;
#237627 = DIRECTION ( 'NONE',  ( 2.952720810173289112E-16, 0.4088369013363281068, -0.9126074666063770380 ) ) ;
#237629 = LINE ( 'NONE', #19875, #236675 ) ;
#237628 = DIRECTION ( 'NONE',  ( 0.000000000000000000, 0.000000000000000000, 1.000000000000000000 ) ) ;
#237630 = ORIENTED_EDGE ( 'NONE', *, *, #57388, .T. ) ;
#237632 = LINE ( 'NONE', #55101, #129983 ) ;
#237631 = CARTESIAN_POINT ( 'NONE',  ( -16.97683810757273193, 66.05000000001157900, -56.25953077206424524 ) ) ;
#237633 = CYLINDRICAL_SURFACE ( 'NONE', #20480, 0.09999999999999804878 ) ;
#237634 = EDGE_CURVE ( 'NONE', #171475, #142182, #106457, .T. ) ;
#237635 = DIRECTION ( 'NONE',  ( -1.836970198721029934E-16, 1.000000000000000000, 0.000000000000000000 ) ) ;
#237636 = DIRECTION ( 'NONE',  ( 0.000000000000000000, 0.1335171055202867274, 0.9910465087640866200 ) ) ;
#237637 = CARTESIAN_POINT ( 'NONE',  ( -18.50000324121759121, 10.29307482169070198, -139.4586421466940749 ) ) ;
#237638 = ORIENTED_EDGE ( 'NONE', *, *, #11621, .T. ) ;
#237639 = DIRECTION ( 'NONE',  ( 1.000000000000000000, 0.000000000000000000, 0.000000000000000000 ) ) ;
#237640 = B_SPLINE_CURVE_WITH_KNOTS ( 'NONE', 3,
 ( #213735, #113358, #173380, #209905, #212471, #130337, #191648, #33868, #72981, #54653 ),
 .UNSPECIFIED., .F., .F.,
 ( 4, 2, 2, 2, 4 ),
 ( 0.000000000000000000, 4.221631689690473076E-05, 8.443263379380946151E-05, 0.0001688652675875489649, 0.0003377305351750279445 ),
 .UNSPECIFIED. ) ;
#237642 = EDGE_LOOP ( 'NONE', ( #149891, #171441, #89945, #189464 ) ) ;
#237641 = VECTOR ( 'NONE', #84896, 1000.000000000000000 ) ;
#237643 = EDGE_CURVE ( 'NONE', #86769, #216617, #173189, .T. ) ;
#237644 = ORIENTED_EDGE ( 'NONE', *, *, #58973, .T. ) ;
#237645 = DIRECTION ( 'NONE',  ( 1.000000000000000000, 0.000000000000000000, 0.000000000000000000 ) ) ;
#237646 = ORIENTED_EDGE ( 'NONE', *, *, #64697, .F. ) ;
#237647 = CARTESIAN_POINT ( 'NONE',  ( 21.05000000000000071, -11.39257802170566691, -30.42605042016806394 ) ) ;
#237648 = CARTESIAN_POINT ( 'NONE',  ( -20.54999999999999716, 71.65000000001202807, -119.7731074845243313 ) ) ;
#237649 = ORIENTED_EDGE ( 'NONE', *, *, #239552, .T. ) ;
#237650 = TOROIDAL_SURFACE ( 'NONE', #12815, 12.77499999999999858, 0.1000000000000000056 ) ;
#237651 = CARTESIAN_POINT ( 'NONE',  ( -18.50000000000000000, -9.419084502802133940, -174.3299078070254495 ) ) ;
#237652 = CARTESIAN_POINT ( 'NONE',  ( -23.15000000000000213, 67.63082410804655353, -211.8415745842588649 ) ) ;
#237653 = TOROIDAL_SURFACE ( 'NONE', #125224, 0.2000000000000000111, 0.1000000000000000056 ) ;
#237654 = CARTESIAN_POINT ( 'NONE',  ( 16.27683809663750125, 66.65000000001263913, -194.2731074845244166 ) ) ;
#237655 = FACE_OUTER_BOUND ( 'NONE', #8715, .T. ) ;
#237656 = DIRECTION ( 'NONE',  ( 0.000000000000000000, -0.9875102702516471709, 0.1575546449569757979 ) ) ;
#237658 = CARTESIAN_POINT ( 'NONE',  ( 19.86930884467592406, 62.42739552316976415, -208.9193556810753591 ) ) ;
#237657 = AXIS2_PLACEMENT_3D ( 'NONE', #18018, #177125, #81804 ) ;
#237659 = EDGE_LOOP ( 'NONE', ( #147372, #83248, #230609, #225255 ) ) ;
#237660 = CYLINDRICAL_SURFACE ( 'NONE', #190770, 0.09999999999999939493 ) ;
#237661 = VERTEX_POINT ( 'NONE', #97235 ) ;
#237663 = ORIENTED_EDGE ( 'NONE', *, *, #257096, .T. ) ;
#237662 = CARTESIAN_POINT ( 'NONE',  ( 23.14999999999998437, 2.048861642965144398E-30, -4.049999999999998934 ) ) ;
#237664 = ORIENTED_EDGE ( 'NONE', *, *, #97754, .F. ) ;
#237665 = CARTESIAN_POINT ( 'NONE',  ( 18.39999999999999858, -9.519327731092436906, -6.972976376559336664 ) ) ;
#237666 = LINE ( 'NONE', #198530, #233117 ) ;
#237667 = CARTESIAN_POINT ( 'NONE',  ( 21.05000000000000071, 5.000000000011153745, -121.5947339810869465 ) ) ;
#237668 = FACE_OUTER_BOUND ( 'NONE', #185257, .T. ) ;
#237669 = CYLINDRICAL_SURFACE ( 'NONE', #66746, 0.09999999999999781286 ) ;
#237670 = CIRCLE ( 'NONE', #29403, 12.87499999999999822 ) ;
#237671 = ORIENTED_EDGE ( 'NONE', *, *, #4107, .T. ) ;
#237672 = FACE_OUTER_BOUND ( 'NONE', #218328, .T. ) ;
#237673 = ORIENTED_EDGE ( 'NONE', *, *, #7862, .T. ) ;
#237674 = B_SPLINE_CURVE_WITH_KNOTS ( 'NONE', 3,
 ( #129717, #89294, #168888, #248384, #189695, #51431, #205381, #209248 ),
 .UNSPECIFIED., .F., .F.,
 ( 4, 2, 2, 4 ),
 ( 0.000000000000000000, 0.0001094981963948460927, 0.0002189963927896921853, 0.0004379927855793843707 ),
 .UNSPECIFIED. ) ;
#237676 = ORIENTED_EDGE ( 'NONE', *, *, #241836, .T. ) ;
#237675 = CARTESIAN_POINT ( 'NONE',  ( 23.14999999999999147, 34.96225128119897363, -245.7638417148289989 ) ) ;
#237677 = CARTESIAN_POINT ( 'NONE',  ( -23.15000000000000213, 35.97645343225767789, -235.9694016464868298 ) ) ;
#237678 = ADVANCED_FACE ( 'NONE', ( #138936 ), #39880, .F. ) ;
#237679 = CARTESIAN_POINT ( 'NONE',  ( -16.82542659449987354, 9.934499891438514751, -79.74463560002654106 ) ) ;
#237680 = CIRCLE ( 'NONE', #191911, 0.1000000000000028644 ) ;
#237681 = EDGE_LOOP ( 'NONE', ( #95772, #212593, #210518, #239070 ) ) ;
#237682 = AXIS2_PLACEMENT_3D ( 'NONE', #196956, #41778, #18334 ) ;
#237683 = AXIS2_PLACEMENT_3D ( 'NONE', #237686, #59009, #1624 ) ;
#237684 = CARTESIAN_POINT ( 'NONE',  ( 21.05000000000000071, 64.40000000001194280, -109.9513107147998880 ) ) ;
#237685 = ORIENTED_EDGE ( 'NONE', *, *, #115781, .T. ) ;
#237686 = CARTESIAN_POINT ( 'NONE',  ( -20.64999999999999858, 2.000000000011154189, -80.22462192276213955 ) ) ;
#237687 = AXIS2_PLACEMENT_3D ( 'NONE', #18543, #115073, #173819 ) ;
#237688 = EDGE_CURVE ( 'NONE', #240985, #215522, #196374, .T. ) ;
#237689 = CARTESIAN_POINT ( 'NONE',  ( -23.25000000000000000, 10.74948822439029250, -222.3968794097801549 ) ) ;
#237690 = CARTESIAN_POINT ( 'NONE',  ( 12.25000000000000000, 66.65000000001155911, -52.65883987690830281 ) ) ;
#237691 = CIRCLE ( 'NONE', #187821, 4.299999999999956302 ) ;
#237692 = AXIS2_PLACEMENT_3D ( 'NONE', #79215, #80479, #101309 ) ;
#237693 = CARTESIAN_POINT ( 'NONE',  ( -23.15000000000000213, 68.59518897103603763, -214.2073844195901131 ) ) ;
#237694 = EDGE_CURVE ( 'NONE', #182152, #227126, #189701, .T. ) ;
#237695 = EDGE_CURVE ( 'NONE', #248438, #249345, #206448, .T. ) ;
#237696 = AXIS2_PLACEMENT_3D ( 'NONE', #53174, #191442, #91020 ) ;
#237697 = AXIS2_PLACEMENT_3D ( 'NONE', #253089, #37932, #137003 ) ;
#237698 = VECTOR ( 'NONE', #97387, 1000.000000000000000 ) ;
#237699 = ORIENTED_EDGE ( 'NONE', *, *, #15627, .T. ) ;
#237701 = CARTESIAN_POINT ( 'NONE',  ( 23.15000000000000213, 87.48912529308779540, -72.62310748452422615 ) ) ;
#237700 = AXIS2_PLACEMENT_3D ( 'NONE', #211566, #258019, #18179 ) ;
#237702 = VECTOR ( 'NONE', #87139, 1000.000000000000000 ) ;
#237703 = ORIENTED_EDGE ( 'NONE', *, *, #30549, .F. ) ;
#237704 = CARTESIAN_POINT ( 'NONE',  ( -23.25000000000000000, 20.06933876993645782, -235.7297789824848451 ) ) ;
#237705 = EDGE_CURVE ( 'NONE', #183554, #5736, #218908, .T. ) ;
#237706 = CARTESIAN_POINT ( 'NONE',  ( -22.60000000000080789, 0.04781698047652394035, -21.74997756884724964 ) ) ;
#237708 = ORIENTED_EDGE ( 'NONE', *, *, #252701, .F. ) ;
#237707 = DIRECTION ( 'NONE',  ( -0.000000000000000000, -0.000000000000000000, -1.000000000000000000 ) ) ;
#237709 = FACE_OUTER_BOUND ( 'NONE', #92562, .T. ) ;
#237710 = CARTESIAN_POINT ( 'NONE',  ( 21.14999999999999503, 0.000000000000000000, 0.000000000000000000 ) ) ;
#237711 = CARTESIAN_POINT ( 'NONE',  ( 22.49999999999999645, 64.35023708198002623, -103.1119174609113145 ) ) ;
#237712 = DIRECTION ( 'NONE',  ( 0.000000000000000000, -0.9274965247785555977, 0.3738317757009190223 ) ) ;
#237713 = CARTESIAN_POINT ( 'NONE',  ( -20.64999999999999858, 54.22301550979020845, -237.0256805049050115 ) ) ;
#237714 = CARTESIAN_POINT ( 'NONE',  ( -18.40000000000000568, 64.52683809665006720, -182.6316861282871287 ) ) ;
#237715 = CARTESIAN_POINT ( 'NONE',  ( 21.05000000000000071, 1.115600667400684642E-11, -205.0999999999999375 ) ) ;
#237716 = AXIS2_PLACEMENT_3D ( 'NONE', #93469, #11384, #90908 ) ;
#237718 = ORIENTED_EDGE ( 'NONE', *, *, #57178, .T. ) ;
#237717 = CARTESIAN_POINT ( 'NONE',  ( 0.8999999999999992450, -8.350000000000004974, 30.04142135623731136 ) ) ;
#237719 = DIRECTION ( 'NONE',  ( 1.000000000000000000, 7.304098846218134667E-16, -0.000000000000000000 ) ) ;
#237720 = EDGE_LOOP ( 'NONE', ( #95396, #119468, #148861, #90705, #227080, #232115, #34573 ) ) ;
#237721 = EDGE_CURVE ( 'NONE', #68804, #87416, #176840, .T. ) ;
#237722 = VERTEX_POINT ( 'NONE', #47560 ) ;
#237723 = EDGE_CURVE ( 'NONE', #7823, #134789, #40994, .T. ) ;
#237724 = ORIENTED_EDGE ( 'NONE', *, *, #171600, .T. ) ;
#237725 = CARTESIAN_POINT ( 'NONE',  ( -21.05000000000000071, 1.115600667400684642E-11, -33.50000000000000000 ) ) ;
#237726 = AXIS2_PLACEMENT_3D ( 'NONE', #97878, #41816, #178775 ) ;
#237728 = ADVANCED_FACE ( 'NONE', ( #184508 ), #26760, .T. ) ;
#237727 = CARTESIAN_POINT ( 'NONE',  ( -18.52186455168989454, 85.48101848145425663, -62.49809100660993977 ) ) ;
#237729 = ORIENTED_EDGE ( 'NONE', *, *, #174155, .T. ) ;
#237730 = CIRCLE ( 'NONE', #37850, 11.75000000000001066 ) ;
#237731 = CARTESIAN_POINT ( 'NONE',  ( 21.05000000000000071, 1.115600667400684642E-11, -167.5000000000000284 ) ) ;
#237732 = CARTESIAN_POINT ( 'NONE',  ( 22.39999999999999503, 55.91711482281188950, -232.6830152854666949 ) ) ;
#237734 = EDGE_LOOP ( 'NONE', ( #24807, #144341, #128926, #103712 ) ) ;
#237733 = VECTOR ( 'NONE', #69836, 1000.000000000000000 ) ;
#237735 = FACE_OUTER_BOUND ( 'NONE', #178059, .T. ) ;
#237736 = ORIENTED_EDGE ( 'NONE', *, *, #208341, .F. ) ;
#237737 = CARTESIAN_POINT ( 'NONE',  ( 22.50000000000000000, 0.09999999999999939493, 11.75000000000000000 ) ) ;
#237739 = ORIENTED_EDGE ( 'NONE', *, *, #197398, .F. ) ;
#237738 = CARTESIAN_POINT ( 'NONE',  ( -20.64999999999999858, 1.925233644870972816, -79.73024353312617052 ) ) ;
#237740 = DIRECTION ( 'NONE',  ( 1.000000000000000000, 0.000000000000000000, 0.000000000000000000 ) ) ;
#237741 = ORIENTED_EDGE ( 'NONE', *, *, #99690, .F. ) ;
#237742 = AXIS2_PLACEMENT_3D ( 'NONE', #73321, #137114, #135807 ) ;
#237743 = DIRECTION ( 'NONE',  ( 1.000000000000000000, 0.000000000000000000, 0.000000000000000000 ) ) ;
#237744 = EDGE_LOOP ( 'NONE', ( #79628, #7856, #161915, #142355 ) ) ;
#237746 = ORIENTED_EDGE ( 'NONE', *, *, #236106, .F. ) ;
#237745 = VERTEX_POINT ( 'NONE', #181963 ) ;
#237747 = DIRECTION ( 'NONE',  ( -1.000000000000000000, 3.265361837132813093E-16, 2.280189983783949500E-30 ) ) ;
#237748 = EDGE_LOOP ( 'NONE', ( #163834, #202735, #78088, #47515 ) ) ;
#237749 = CYLINDRICAL_SURFACE ( 'NONE', #164828, 0.1000000000000028644 ) ;
#237750 = VECTOR ( 'NONE', #256408, 1000.000000000000000 ) ;
#237751 = ORIENTED_EDGE ( 'NONE', *, *, #232804, .T. ) ;
#237752 = CIRCLE ( 'NONE', #183590, 0.1000000000000028644 ) ;
#237753 = EDGE_CURVE ( 'NONE', #17420, #95339, #148178, .T. ) ;
#237754 = EDGE_CURVE ( 'NONE', #73463, #121293, #81510, .T. ) ;
#237755 = ORIENTED_EDGE ( 'NONE', *, *, #1134, .T. ) ;
#237756 = CARTESIAN_POINT ( 'NONE',  ( -21.64999999999999858, 7.350000000011155166, -88.25000000000005684 ) ) ;
#237757 = CARTESIAN_POINT ( 'NONE',  ( -22.50000000000000000, 11.65000000001113278, -33.50000000000000000 ) ) ;
#237759 = ORIENTED_EDGE ( 'NONE', *, *, #39594, .T. ) ;
#237758 = DIRECTION ( 'NONE',  ( -0.000000000000000000, 0.000000000000000000, 1.000000000000000000 ) ) ;
#237760 = DIRECTION ( 'NONE',  ( -4.163336342344447088E-13, 0.4205162045344795763, -0.9072850278296868964 ) ) ;
#237761 = VERTEX_POINT ( 'NONE', #127113 ) ;
#237762 = EDGE_CURVE ( 'NONE', #15753, #162643, #226176, .T. ) ;
#237764 = ADVANCED_FACE ( 'NONE', ( #162410 ), #187115, .F. ) ;
#237763 = DIRECTION ( 'NONE',  ( -0.000000000000000000, 0.4088369013363281068, -0.9126074666063770380 ) ) ;
#237765 = DIRECTION ( 'NONE',  ( -1.000000000000000000, -0.000000000000000000, -0.000000000000000000 ) ) ;
#237766 = DIRECTION ( 'NONE',  ( -0.000000000000000000, 0.7397360091702708251, 0.6728971962616883129 ) ) ;
#237767 = ORIENTED_EDGE ( 'NONE', *, *, #35913, .T. ) ;
#237768 = DIRECTION ( 'NONE',  ( 1.000000000000000000, 0.000000000000000000, 0.000000000000000000 ) ) ;
#237769 = CARTESIAN_POINT ( 'NONE',  ( 20.94999999999999574, 87.65000000001212754, -133.5231074845242176 ) ) ;
#237770 = FACE_OUTER_BOUND ( 'NONE', #97807, .T. ) ;
#237771 = AXIS2_PLACEMENT_3D ( 'NONE', #1000, #63571, #41477 ) ;
#237772 = EDGE_CURVE ( 'NONE', #160483, #118763, #135703, .T. ) ;
#237773 = ORIENTED_EDGE ( 'NONE', *, *, #76310, .T. ) ;
#237774 = CARTESIAN_POINT ( 'NONE',  ( -16.94275863009466576, 66.01050395134947735, -90.41480486656550397 ) ) ;
#237775 = ORIENTED_EDGE ( 'NONE', *, *, #80478, .F. ) ;
#237776 = ORIENTED_EDGE ( 'NONE', *, *, #52279, .F. ) ;
#237777 = EDGE_CURVE ( 'NONE', #179299, #83901, #209086, .T. ) ;
#237779 = ADVANCED_FACE ( 'NONE', ( #128404 ), #200891, .T. ) ;
#237778 = EDGE_CURVE ( 'NONE', #73683, #19112, #85790, .T. ) ;
#237780 = CARTESIAN_POINT ( 'NONE',  ( 21.05000000000000071, 71.14953271029189352, -48.05737489352603120 ) ) ;
#237781 = EDGE_LOOP ( 'NONE', ( #142087, #145086, #72998, #113493 ) ) ;
#237782 = VERTEX_POINT ( 'NONE', #250903 ) ;
#237783 = DIRECTION ( 'NONE',  ( -1.186688945009010077E-16, 1.000000000000000000, 0.000000000000000000 ) ) ;
#237784 = DIRECTION ( 'NONE',  ( 0.000000000000000000, -9.769962616701387022E-15, 1.000000000000000000 ) ) ;
#237785 = ORIENTED_EDGE ( 'NONE', *, *, #95572, .F. ) ;
#237786 = EDGE_CURVE ( 'NONE', #161922, #71516, #110767, .T. ) ;
#237787 = VERTEX_POINT ( 'NONE', #52703 ) ;
#237788 = DIRECTION ( 'NONE',  ( 0.000000000000000000, 0.000000000000000000, 1.000000000000000000 ) ) ;
#237789 = DIRECTION ( 'NONE',  ( -0.000000000000000000, 1.000000000000000000, 6.982962677686266711E-15 ) ) ;
#237790 = ORIENTED_EDGE ( 'NONE', *, *, #152958, .F. ) ;
#237791 = CIRCLE ( 'NONE', #133725, 4.041421356237306917 ) ;
#237792 = EDGE_CURVE ( 'NONE', #286, #256585, #52493, .T. ) ;
#237793 = AXIS2_PLACEMENT_3D ( 'NONE', #152603, #250382, #234673 ) ;
#237794 = VECTOR ( 'NONE', #240231, 1000.000000000000000 ) ;
#237795 = VERTEX_POINT ( 'NONE', #31899 ) ;
#237796 = CIRCLE ( 'NONE', #96126, 0.09999999999998898659 ) ;
#237797 = ADVANCED_FACE ( 'NONE', ( #71023 ), #252398, .T. ) ;
#237798 = ADVANCED_FACE ( 'NONE', ( #132252 ), #231582, .T. ) ;
#237799 = EDGE_LOOP ( 'NONE', ( #253615, #203002, #241921 ) ) ;
#237800 = AXIS2_PLACEMENT_3D ( 'NONE', #7010, #126964, #103524 ) ;
#237801 = EDGE_CURVE ( 'NONE', #35945, #213275, #72296, .T. ) ;
#237802 = FACE_OUTER_BOUND ( 'NONE', #16037, .T. ) ;
#237803 = DIRECTION ( 'NONE',  ( -0.000000000000000000, 0.000000000000000000, -1.000000000000000000 ) ) ;
#237804 = FACE_OUTER_BOUND ( 'NONE', #105412, .T. ) ;
#237805 = EDGE_CURVE ( 'NONE', #206018, #29639, #98258, .T. ) ;
#237806 = DIRECTION ( 'NONE',  ( 0.000000000000000000, -0.8814952561688430555, 0.4721928772777346239 ) ) ;
#237807 = AXIS2_PLACEMENT_3D ( 'NONE', #178629, #181185, #238568 ) ;
#237808 = CARTESIAN_POINT ( 'NONE',  ( -21.07928932188134041, 33.98134083355423485, -243.8161431329846778 ) ) ;
#237810 = DIRECTION ( 'NONE',  ( 1.000000000000000000, 0.000000000000000000, 0.000000000000000000 ) ) ;
#237809 = DIRECTION ( 'NONE',  ( 0.000000000000000000, -8.556632174375002828E-15, 1.000000000000000000 ) ) ;
#237811 = CARTESIAN_POINT ( 'NONE',  ( 20.04142135623730070, 11.75000000001115907, -91.65000000000004832 ) ) ;
#237813 = EDGE_CURVE ( 'NONE', #8134, #115956, #9729, .T. ) ;
#237812 = DIRECTION ( 'NONE',  ( 3.616040088954490704E-32, 7.105427357601001859E-15, -1.000000000000000000 ) ) ;
#237814 = CYLINDRICAL_SURFACE ( 'NONE', #238754, 11.74999999999999645 ) ;
#237815 = CARTESIAN_POINT ( 'NONE',  ( 21.05000000000000071, 44.15903683684981473, -236.5744930507153185 ) ) ;
#237816 = EDGE_LOOP ( 'NONE', ( #213594, #234383, #112056, #1310 ) ) ;
#237818 = VERTEX_POINT ( 'NONE', #228800 ) ;
#237817 = CARTESIAN_POINT ( 'NONE',  ( 21.14999999999999503, 76.00000000001271871, -209.7731074845243597 ) ) ;
#237819 = EDGE_CURVE ( 'NONE', #19871, #242236, #67622, .T. ) ;
#237820 = CARTESIAN_POINT ( 'NONE',  ( 21.05563370358598263, 43.39284295883493314, -234.7832529069957559 ) ) ;
#237821 = CIRCLE ( 'NONE', #108809, 0.3999999999999983569 ) ;
#237822 = CYLINDRICAL_SURFACE ( 'NONE', #15320, 0.09999999999999939493 ) ;
#237823 = FILL_AREA_STYLE_COLOUR ( '', #244537 ) ;
#237824 = ORIENTED_EDGE ( 'NONE', *, *, #41725, .T. ) ;
#237825 = AXIS2_PLACEMENT_3D ( 'NONE', #149110, #49988, #70871 ) ;
#237826 = CARTESIAN_POINT ( 'NONE',  ( 20.94999999999999929, 77.83534155023701828, -191.9679561919613491 ) ) ;
#237828 = AXIS2_PLACEMENT_3D ( 'NONE', #100717, #1639, #65476 ) ;
#237827 = ADVANCED_BREP_SHAPE_REPRESENTATION ( '', ( #198047, #2425 ), #185768 ) ;
#237829 = CARTESIAN_POINT ( 'NONE',  ( -16.92973740335397181, 66.00749618554532105, -157.4291665197260102 ) ) ;
#237830 = ORIENTED_EDGE ( 'NONE', *, *, #157054, .T. ) ;
#237831 = CARTESIAN_POINT ( 'NONE',  ( -21.05000000000000071, 0.9150442794848296924, -205.2015109147324097 ) ) ;
#237832 = DIRECTION ( 'NONE',  ( 0.000000000000000000, 0.9126074666063783702, 0.4088369013363252757 ) ) ;
#237833 = VECTOR ( 'NONE', #151956, 1000.000000000000000 ) ;
#237834 = DIRECTION ( 'NONE',  ( 0.000000000000000000, 0.000000000000000000, -1.000000000000000000 ) ) ;
#237835 = AXIS2_PLACEMENT_3D ( 'NONE', #130454, #113460, #52190 ) ;
#237836 = DIRECTION ( 'NONE',  ( 0.000000000000000000, -0.4088369013363280513, 0.9126074666063771490 ) ) ;
#237838 = VERTEX_POINT ( 'NONE', #129683 ) ;
#237837 = CARTESIAN_POINT ( 'NONE',  ( -21.05000000000000071, 70.15000000001163016, -59.39061026024639744 ) ) ;
#237840 = VERTEX_POINT ( 'NONE', #206217 ) ;
#237839 = CARTESIAN_POINT ( 'NONE',  ( -23.25000000000000000, 36.65892442174935439, -249.5511627012433848 ) ) ;
#237841 = DIRECTION ( 'NONE',  ( 1.000000000000000000, -0.000000000000000000, 0.000000000000000000 ) ) ;
#237842 = CARTESIAN_POINT ( 'NONE',  ( -23.25000000000000000, 85.60000000001220144, -146.4170766071767389 ) ) ;
#237843 = DIRECTION ( 'NONE',  ( 1.000000000000000000, 0.000000000000000000, 0.000000000000000000 ) ) ;
#237844 = DIRECTION ( 'NONE',  ( 1.000000000000000000, 0.000000000000000000, 0.000000000000000000 ) ) ;
#237845 = ADVANCED_FACE ( 'NONE', ( #28916 ), #108408, .T. ) ;
#237846 = CARTESIAN_POINT ( 'NONE',  ( -23.25000000000000000, -8.999999999988844479, -191.1060308773475356 ) ) ;
#237847 = CARTESIAN_POINT ( 'NONE',  ( -16.92925196614875105, 66.02766820360247380, -190.9063626368076427 ) ) ;
#237848 = CARTESIAN_POINT ( 'NONE',  ( 20.95083306685154056, 40.74986006426208718, -237.9477423030747616 ) ) ;
#237850 = DIRECTION ( 'NONE',  ( 2.952720810173290098E-16, -0.4721928772777333472, -0.8814952561688437216 ) ) ;
#237849 = AXIS2_PLACEMENT_3D ( 'NONE', #12238, #7069, #229976 ) ;
#237851 = CARTESIAN_POINT ( 'NONE',  ( -23.15000000000000213, 85.50000000001149658, -45.91707660717669626 ) ) ;
#237852 = EDGE_CURVE ( 'NONE', #82492, #123641, #187944, .T. ) ;
#237853 = CARTESIAN_POINT ( 'NONE',  ( 21.08884785362045378, 10.08677120552972362, -228.1053582936064856 ) ) ;
#237854 = TOROIDAL_SURFACE ( 'NONE', #54692, 0.6000000000000006439, 0.1000000000000000056 ) ;
#237855 = ORIENTED_EDGE ( 'NONE', *, *, #78976, .F. ) ;
#237856 = DIRECTION ( 'NONE',  ( 0.000000000000000000, 0.000000000000000000, -1.000000000000000000 ) ) ;
#237857 = ORIENTED_EDGE ( 'NONE', *, *, #77886, .T. ) ;
#237858 = MECHANICAL_DESIGN_GEOMETRIC_PRESENTATION_REPRESENTATION (  '', ( #62894 ), #138071 ) ;
#237859 = ORIENTED_EDGE ( 'NONE', *, *, #79109, .F. ) ;
#237860 = ADVANCED_FACE ( 'NONE', ( #125404 ), #65417, .F. ) ;
#237861 = DIRECTION ( 'NONE',  ( 0.000000000000000000, -0.9651348961777379554, 0.2617529984164210233 ) ) ;
#237862 = EDGE_CURVE ( 'NONE', #172081, #224073, #144938, .T. ) ;
#237863 = DIRECTION ( 'NONE',  ( 0.000000000000000000, -0.4930308989875248349, -0.8700118002898312719 ) ) ;
#237864 = ORIENTED_EDGE ( 'NONE', *, *, #31148, .F. ) ;
#237865 = VECTOR ( 'NONE', #79882, 1000.000000000000000 ) ;
#237866 = ORIENTED_EDGE ( 'NONE', *, *, #227957, .T. ) ;
#237868 = VERTEX_POINT ( 'NONE', #185367 ) ;
#237867 = AXIS2_PLACEMENT_3D ( 'NONE', #201666, #182116, #163837 ) ;
#237869 = VECTOR ( 'NONE', #184027, 1000.000000000000000 ) ;
#237870 = EDGE_LOOP ( 'NONE', ( #153052, #41322, #239887, #7196 ) ) ;
#237871 = CIRCLE ( 'NONE', #125464, 0.09999999999999939493 ) ;
#237872 = ADVANCED_FACE ( 'NONE', ( #129253 ), #107109, .F. ) ;
#237873 = DIRECTION ( 'NONE',  ( -1.000000000000000000, 0.000000000000000000, 0.000000000000000000 ) ) ;
#237874 = CYLINDRICAL_SURFACE ( 'NONE', #153468, 0.09999999999998898659 ) ;
#237875 = FACE_OUTER_BOUND ( 'NONE', #117282, .T. ) ;
#237876 = CYLINDRICAL_SURFACE ( 'NONE', #149003, 0.09999999999999939493 ) ;
#237877 = DIRECTION ( 'NONE',  ( 0.000000000000000000, 1.000000000000000000, 7.272083257015735086E-15 ) ) ;
#237878 = CARTESIAN_POINT ( 'NONE',  ( 21.10257677756355577, 65.53239810784317854, -242.0238970717508380 ) ) ;
#237879 = DIRECTION ( 'NONE',  ( 0.000000000000000000, 1.000000000000000000, 6.938893903907222067E-15 ) ) ;
#237881 = ORIENTED_EDGE ( 'NONE', *, *, #65544, .T. ) ;
#237880 = DIRECTION ( 'NONE',  ( 0.000000000000000000, -0.8814952561688430555, 0.4721928772777346239 ) ) ;
#237882 = CARTESIAN_POINT ( 'NONE',  ( -17.73285935860488038, 62.83985570472179205, -210.5653675750546086 ) ) ;
#237883 = CARTESIAN_POINT ( 'NONE',  ( -23.15000000000000213, 38.42191493408704872, -250.4955484557988541 ) ) ;
#237884 = ORIENTED_EDGE ( 'NONE', *, *, #76995, .T. ) ;
#237885 = PLANE ( 'NONE',  #77063 ) ;
#237886 = DIRECTION ( 'NONE',  ( 0.000000000000000000, -0.9770955615653320603, -0.2128009952263585081 ) ) ;
#237887 = B_SPLINE_CURVE_WITH_KNOTS ( 'NONE', 3,
 ( #136820, #33935, #192962, #132996, #75600, #195546, #92555, #134244, #11776, #16896, #194266, #71739, #131695, #74329, #55980, #233391 ),
 .UNSPECIFIED., .F., .F.,
 ( 4, 3, 3, 3, 3, 4 ),
 ( 0.000000000000000000, 2.209833635978076120E-05, 5.595056164119271882E-05, 8.979992002655370561E-05, 0.0001236482757198912198, 0.0001574984039362985287 ),
 .UNSPECIFIED. ) ;
#237888 = VERTEX_POINT ( 'NONE', #86241 ) ;
#237890 = CARTESIAN_POINT ( 'NONE',  ( -20.54999999999999716, 19.73066058418984170, -238.2142830767208466 ) ) ;
#237889 = CARTESIAN_POINT ( 'NONE',  ( -18.50000000000000000, 9.250000000011157297, -121.6500000000000341 ) ) ;
#237891 = CARTESIAN_POINT ( 'NONE',  ( -22.47071067811865319, 75.90090754530939421, -110.7431822290223806 ) ) ;
#237892 = EDGE_CURVE ( 'NONE', #233701, #184752, #173365, .T. ) ;
#237893 = DIRECTION ( 'NONE',  ( 0.000000000000000000, 3.552713678800413366E-15, -1.000000000000000000 ) ) ;
#237894 = VERTEX_POINT ( 'NONE', #247904 ) ;
#237895 = CARTESIAN_POINT ( 'NONE',  ( 18.59999999999999076, 10.20857864377385127, -125.1500000000000341 ) ) ;
#237896 = CARTESIAN_POINT ( 'NONE',  ( 21.14999999999999503, 30.95512775545487472, -252.1063933345974988 ) ) ;
#237897 = CARTESIAN_POINT ( 'NONE',  ( -21.05000000000000071, 0.09779029131994770863, -127.7421853895239252 ) ) ;
#237898 = CARTESIAN_POINT ( 'NONE',  ( -18.79999999999999716, 4.513204987021268266, 22.10000000000000142 ) ) ;
#237899 = ORIENTED_EDGE ( 'NONE', *, *, #198648, .F. ) ;
#237900 = ADVANCED_FACE ( 'NONE', ( #165830 ), #6727, .T. ) ;
#237901 = AXIS2_PLACEMENT_3D ( 'NONE', #151171, #209860, #31257 ) ;
#237902 = CARTESIAN_POINT ( 'NONE',  ( 21.08489247129320887, 8.877675190881227252, -179.8500000000000227 ) ) ;
#237903 = ADVANCED_FACE ( 'NONE', ( #83657 ), #131615, .F. ) ;
#237904 = FACE_OUTER_BOUND ( 'NONE', #46206, .T. ) ;
#237905 = CARTESIAN_POINT ( 'NONE',  ( 20.94999999999999929, 77.83534155023627932, -91.46795619196132066 ) ) ;
#237906 = DIRECTION ( 'NONE',  ( 1.000000000000000000, 0.000000000000000000, 0.000000000000000000 ) ) ;
#237907 = CARTESIAN_POINT ( 'NONE',  ( -18.50000000000000711, 85.41920341803901806, -162.7753216740956645 ) ) ;
#237908 = ADVANCED_FACE ( 'NONE', ( #25038 ), #208792, .F. ) ;
#237909 = AXIS2_PLACEMENT_3D ( 'NONE', #202601, #20122, #59190 ) ;
#237911 = ORIENTED_EDGE ( 'NONE', *, *, #235791, .F. ) ;
#237910 = DIRECTION ( 'NONE',  ( -1.000000000000000000, -0.000000000000000000, 0.000000000000000000 ) ) ;
#237912 = DIRECTION ( 'NONE',  ( 0.000000000000000000, 0.000000000000000000, -1.000000000000000000 ) ) ;
#237913 = CARTESIAN_POINT ( 'NONE',  ( -16.82542659449982736, 66.06550010858451571, -90.27847188449790394 ) ) ;
#237914 = DIRECTION ( 'NONE',  ( 1.000000000000000000, 0.000000000000000000, 0.000000000000000000 ) ) ;
#237915 = CARTESIAN_POINT ( 'NONE',  ( -21.05000000000000071, -11.48912529306490349, -36.50000000000000711 ) ) ;
#237916 = DIRECTION ( 'NONE',  ( -1.000000000000000000, 0.000000000000000000, 0.000000000000000000 ) ) ;
#237917 = EDGE_CURVE ( 'NONE', #123588, #44645, #167123, .T. ) ;
#237919 = ORIENTED_EDGE ( 'NONE', *, *, #174402, .T. ) ;
#237918 = CARTESIAN_POINT ( 'NONE',  ( -21.65000000000000213, 65.69159657275406516, -213.8343546826533839 ) ) ;
#237920 = CARTESIAN_POINT ( 'NONE',  ( 22.49806830649814060, 64.35011034517329165, -170.1005718008499343 ) ) ;
#237921 = EDGE_CURVE ( 'NONE', #104735, #221499, #210726, .T. ) ;
#237922 = DIRECTION ( 'NONE',  ( 0.000000000000000000, 0.1335171055202901691, -0.9910465087640861759 ) ) ;
#237923 = DIRECTION ( 'NONE',  ( 0.000000000000000000, -1.000000000000000000, 0.000000000000000000 ) ) ;
#237924 = VERTEX_POINT ( 'NONE', #204917 ) ;
#237925 = CARTESIAN_POINT ( 'NONE',  ( -12.60829076262180060, 66.61047060254553287, -152.2059995716306844 ) ) ;
#237926 = DIRECTION ( 'NONE',  ( 0.000000000000000000, 0.000000000000000000, 1.000000000000000000 ) ) ;
#237927 = DIRECTION ( 'NONE',  ( -1.000000000000000000, 0.000000000000000000, 0.000000000000000000 ) ) ;
#237928 = DIRECTION ( 'NONE',  ( 1.000000000000000000, 0.000000000000000000, 0.000000000000000000 ) ) ;
#237929 = ADVANCED_FACE ( 'NONE', ( #246616 ), #227053, .T. ) ;
#237930 = AXIS2_PLACEMENT_3D ( 'NONE', #91345, #7956, #207443 ) ;
#237932 = AXIS2_PLACEMENT_3D ( 'NONE', #2072, #161173, #82871 ) ;
#237931 = DIRECTION ( 'NONE',  ( 0.000000000000000000, 0.000000000000000000, -1.000000000000000000 ) ) ;
#237933 = VERTEX_POINT ( 'NONE', #5414 ) ;
#237934 = VERTEX_POINT ( 'NONE', #45857 ) ;
#237935 = AXIS2_PLACEMENT_3D ( 'NONE', #188895, #205881, #234097 ) ;
#237936 = CARTESIAN_POINT ( 'NONE',  ( -18.34804628011471195, 64.52683809664993930, -160.7731074845244450 ) ) ;
#237937 = CARTESIAN_POINT ( 'NONE',  ( -21.13614978966382196, 34.00185059398663867, -243.6200312240952712 ) ) ;
#237938 = ADVANCED_FACE ( 'NONE', ( #30169 ), #113533, .F. ) ;
#237939 = CARTESIAN_POINT ( 'NONE',  ( 18.39999999999999858, 29.77885356168128439, -262.9335064780472635 ) ) ;
#237940 = ORIENTED_EDGE ( 'NONE', *, *, #107191, .F. ) ;
#237941 = CARTESIAN_POINT ( 'NONE',  ( -22.39999999999999858, 76.00000000001200817, -110.8138870828977218 ) ) ;
#237942 = CARTESIAN_POINT ( 'NONE',  ( 20.50589344624626165, 11.85461726721770326, -206.1687069564524393 ) ) ;
#237943 = CARTESIAN_POINT ( 'NONE',  ( -16.77902162784673479, 9.946419257207841369, -12.66199124406934118 ) ) ;
#237944 = CARTESIAN_POINT ( 'NONE',  ( -16.87683809663752044, 9.949999999999983302, -20.09763598180368405 ) ) ;
#237945 = EDGE_LOOP ( 'NONE', ( #24307, #109541, #227943, #176504 ) ) ;
#237946 = DIRECTION ( 'NONE',  ( 1.000000000000000000, 0.000000000000000000, 0.000000000000000000 ) ) ;
#237947 = EDGE_LOOP ( 'NONE', ( #138193, #156126, #143213, #62979 ) ) ;
#237948 = B_SPLINE_CURVE_WITH_KNOTS ( 'NONE', 3,
 ( #102687, #3606, #242215, #63578, #222639, #123566, #203097, #89554 ),
 .UNSPECIFIED., .F., .F.,
 ( 4, 2, 2, 4 ),
 ( 0.000000000000000000, 0.0001049670497869917491, 0.0002099340995739834982, 0.0004198681991479925294 ),
 .UNSPECIFIED. ) ;
#237949 = CARTESIAN_POINT ( 'NONE',  ( -16.85939681242906119, 9.905225185925303322, -20.53992195519148467 ) ) ;
#237950 = ORIENTED_EDGE ( 'NONE', *, *, #250545, .F. ) ;
#237951 = CARTESIAN_POINT ( 'NONE',  ( -21.05000000000000071, -0.01771943329748255566, -27.05891531152877860 ) ) ;
#237952 = CARTESIAN_POINT ( 'NONE',  ( -20.94999999999999929, 64.30000000001176375, -76.27810563404301547 ) ) ;
#237953 = CARTESIAN_POINT ( 'NONE',  ( -16.87331047859651179, 66.05000000001187743, -90.37310748452438247 ) ) ;
#237954 = ORIENTED_EDGE ( 'NONE', *, *, #18813, .F. ) ;
#237955 = DIRECTION ( 'NONE',  ( 0.000000000000000000, -0.2128009952263603677, 0.9770955615653313941 ) ) ;
#237956 = CARTESIAN_POINT ( 'NONE',  ( -16.97683809663752186, 13.90118822005492660, -218.5412211127979845 ) ) ;
#237957 = EDGE_LOOP ( 'NONE', ( #71560, #228613, #111809, #224320 ) ) ;
#237958 = CARTESIAN_POINT ( 'NONE',  ( -12.30589683808040924, 9.356746017089404788, -151.2033597213641940 ) ) ;
#237960 = ORIENTED_EDGE ( 'NONE', *, *, #181485, .T. ) ;
#237959 = CYLINDRICAL_SURFACE ( 'NONE', #242333, 0.09999999999999939493 ) ;
#237961 = AXIS2_PLACEMENT_3D ( 'NONE', #51381, #167543, #25449 ) ;
#237962 = AXIS2_PLACEMENT_3D ( 'NONE', #20557, #167774, #4789 ) ;
#237963 = DIRECTION ( 'NONE',  ( 0.000000000000000000, 0.000000000000000000, -1.000000000000000000 ) ) ;
#237964 = CARTESIAN_POINT ( 'NONE',  ( -18.52186455169013612, 85.48101848145468296, -162.9980910066095987 ) ) ;
#237965 = VECTOR ( 'NONE', #8614, 1000.000000000000000 ) ;
#237966 = ORIENTED_EDGE ( 'NONE', *, *, #189403, .F. ) ;
#237967 = DIRECTION ( 'NONE',  ( 0.000000000000000000, 0.8777080977375072424, -0.4791956752371691608 ) ) ;
#237968 = FACE_OUTER_BOUND ( 'NONE', #171980, .T. ) ;
#237969 = DIRECTION ( 'NONE',  ( -1.000000000000000000, 0.000000000000000000, 0.000000000000000000 ) ) ;
#237970 = ORIENTED_EDGE ( 'NONE', *, *, #143698, .T. ) ;
#237971 = DIRECTION ( 'NONE',  ( 1.000000000000000000, 0.000000000000000000, 0.000000000000000000 ) ) ;
#237972 = ADVANCED_FACE ( 'NONE', ( #15750 ), #109666, .F. ) ;
#237973 = CARTESIAN_POINT ( 'NONE',  ( 12.60873083341396317, 49.08063300121914807, -233.6976605013539654 ) ) ;
#237974 = FACE_OUTER_BOUND ( 'NONE', #179029, .T. ) ;
#237975 = AXIS2_PLACEMENT_3D ( 'NONE', #217392, #98705, #59584 ) ;
#237976 = ADVANCED_FACE ( 'NONE', ( #193083 ), #151397, .T. ) ;
#237977 = EDGE_LOOP ( 'NONE', ( #205000, #85672, #152848, #205255 ) ) ;
#237978 = ADVANCED_FACE ( 'NONE', ( #73156 ), #90096, .T. ) ;
#237979 = ORIENTED_EDGE ( 'NONE', *, *, #127127, .F. ) ;
#237980 = VERTEX_POINT ( 'NONE', #11893 ) ;
#237981 = EDGE_LOOP ( 'NONE', ( #156812, #88418, #70880, #42725 ) ) ;
#237982 = CARTESIAN_POINT ( 'NONE',  ( 18.49999999999999289, 62.46832465249013921, -225.2232495205141731 ) ) ;
#237983 = ADVANCED_FACE ( 'NONE', ( #155263 ), #134359, .F. ) ;
#237984 = PLANE ( 'NONE',  #79550 ) ;
#237985 = CIRCLE ( 'NONE', #125572, 3.999999999999999112 ) ;
#237987 = EDGE_LOOP ( 'NONE', ( #161816, #189644, #178284, #110163 ) ) ;
#237986 = CARTESIAN_POINT ( 'NONE',  ( -16.77683809663752257, 9.945835743215301505, -146.6639490191042228 ) ) ;
#237988 = DIRECTION ( 'NONE',  ( 0.000000000000000000, -0.8814952561688430555, 0.4721928772777346239 ) ) ;
#237989 = DIRECTION ( 'NONE',  ( 0.000000000000000000, 0.9126074666063844765, 0.4088369013363114535 ) ) ;
#237990 = EDGE_CURVE ( 'NONE', #84395, #151423, #218278, .T. ) ;
#237991 = CARTESIAN_POINT ( 'NONE',  ( 20.90000000000000213, 1.885425182446133885, -11.49641995933507843 ) ) ;
#237992 = CARTESIAN_POINT ( 'NONE',  ( -16.88593481969334320, 51.62034258236364082, -231.9451924255289441 ) ) ;
#237993 = CARTESIAN_POINT ( 'NONE',  ( -18.50000000000000000, 74.13328508995475374, -124.7704322382423072 ) ) ;
#237994 = CIRCLE ( 'NONE', #46456, 0.1000000000000028644 ) ;
#237995 = CARTESIAN_POINT ( 'NONE',  ( 23.14999999999999503, 6.550000000011156231, -155.1500000000000057 ) ) ;
#237997 = VERTEX_POINT ( 'NONE', #52252 ) ;
#237996 = DIRECTION ( 'NONE',  ( 1.000000000000000000, 0.000000000000000000, 0.000000000000000000 ) ) ;
#238000 = ORIENTED_EDGE ( 'NONE', *, *, #107280, .T. ) ;
#237999 = FACE_OUTER_BOUND ( 'NONE', #71130, .T. ) ;
#237998 = PRODUCT_RELATED_PRODUCT_CATEGORY ( 'part', '', ( #122620 ) ) ;
#238001 = LINE ( 'NONE', #59335, #95430 ) ;
#238002 = EDGE_LOOP ( 'NONE', ( #143068, #131255, #196076, #146306 ) ) ;
#238003 = AXIS2_PLACEMENT_3D ( 'NONE', #213329, #193787, #94671 ) ;
#238004 = EDGE_LOOP ( 'NONE', ( #61039, #113981, #162582, #137138 ) ) ;
#238005 = CARTESIAN_POINT ( 'NONE',  ( -18.51697539158857353, 10.31565961587945779, -106.0364194119178762 ) ) ;
#238006 = DIRECTION ( 'NONE',  ( -1.000000000000000000, 0.000000000000000000, 0.000000000000000000 ) ) ;
#238008 = EDGE_CURVE ( 'NONE', #117799, #166513, #253035, .T. ) ;
#238007 = DIRECTION ( 'NONE',  ( 1.000000000000000000, 0.000000000000000000, 0.000000000000000000 ) ) ;
#238009 = AXIS2_PLACEMENT_3D ( 'NONE', #88431, #248834, #166755 ) ;
#238010 = CARTESIAN_POINT ( 'NONE',  ( 18.59999999999999076, 69.55000000001207638, -126.5060803140843291 ) ) ;
#238011 = ADVANCED_FACE ( 'NONE', ( #153995 ), #120953, .F. ) ;
#238012 = EDGE_CURVE ( 'NONE', #187086, #115342, #56625, .T. ) ;
#238013 = CARTESIAN_POINT ( 'NONE',  ( 21.05000000000000071, 36.65892442174472876, -249.5511627012454596 ) ) ;
#238014 = DIRECTION ( 'NONE',  ( 1.000000000000000000, 0.000000000000000000, 0.000000000000000000 ) ) ;
#238015 = AXIS2_PLACEMENT_3D ( 'NONE', #121758, #164721, #219537 ) ;
#238016 = DIRECTION ( 'NONE',  ( 0.000000000000000000, -0.3738317757009345654, 0.9274965247785492695 ) ) ;
#238017 = EDGE_LOOP ( 'NONE', ( #186787, #193893, #95240, #228805 ) ) ;
#238018 = ORIENTED_EDGE ( 'NONE', *, *, #28915, .T. ) ;
#238019 = LINE ( 'NONE', #24139, #52475 ) ;
#238020 = B_SPLINE_CURVE_WITH_KNOTS ( 'NONE', 3,
 ( #2637, #27393, #101719, #222970, #220428, #183856 ),
 .UNSPECIFIED., .F., .F.,
 ( 4, 2, 4 ),
 ( 1.301042606982605513E-18, 0.0001569047307838624067, 0.0003138094615677235123 ),
 .UNSPECIFIED. ) ;
#238021 = ADVANCED_FACE ( 'NONE', ( #175399 ), #94192, .F. ) ;
#238022 = CIRCLE ( 'NONE', #233771, 0.09999999999999939493 ) ;
#238023 = EDGE_LOOP ( 'NONE', ( #215856, #27455, #70105, #205040 ) ) ;
#238024 = CIRCLE ( 'NONE', #200441, 0.09999999999998986089 ) ;
#238025 = DIRECTION ( 'NONE',  ( 0.000000000000000000, 7.056502275159890832E-15, -1.000000000000000000 ) ) ;
#238026 = CARTESIAN_POINT ( 'NONE',  ( -12.25000000000000178, 66.65000000001155911, -52.77310748452439526 ) ) ;
#238027 = VECTOR ( 'NONE', #88116, 1000.000000000000000 ) ;
#238028 = DIRECTION ( 'NONE',  ( -0.7071067811865475727, -0.7071067811865475727, 0.000000000000000000 ) ) ;
#238029 = EDGE_LOOP ( 'NONE', ( #33073, #249414, #67789, #19648 ) ) ;
#238030 = CARTESIAN_POINT ( 'NONE',  ( -16.93826681692523195, 65.98857127972452474, -149.0776490171649868 ) ) ;
#238031 = ORIENTED_EDGE ( 'NONE', *, *, #56966, .F. ) ;
#238033 = AXIS2_PLACEMENT_3D ( 'NONE', #136673, #94988, #174594 ) ;
#238032 = PLANE ( 'NONE',  #104692 ) ;
#238034 = ORIENTED_EDGE ( 'NONE', *, *, #6731, .T. ) ;
#238035 = DIRECTION ( 'NONE',  ( -1.000000000000000000, -2.952720810173289112E-16, 0.000000000000000000 ) ) ;
#238036 = EDGE_CURVE ( 'NONE', #146041, #170888, #10998, .T. ) ;
#238037 = CARTESIAN_POINT ( 'NONE',  ( -18.59999999999999787, -1.835341550224411922, -11.55515129256297868 ) ) ;
#238038 = CARTESIAN_POINT ( 'NONE',  ( -18.59999999999999787, 18.71344899777637494, -226.7788045585494103 ) ) ;
#238039 = ORIENTED_EDGE ( 'NONE', *, *, #61382, .F. ) ;
#238040 = CARTESIAN_POINT ( 'NONE',  ( 23.14999999999999503, 64.35000000001176090, -76.53791325517833855 ) ) ;
#238042 = ORIENTED_EDGE ( 'NONE', *, *, #104138, .T. ) ;
#238041 = DIRECTION ( 'NONE',  ( -1.000000000000000000, -0.000000000000000000, -0.000000000000000000 ) ) ;
#238043 = CIRCLE ( 'NONE', #208838, 0.1000000000000028644 ) ;
#238044 = DIRECTION ( 'NONE',  ( 1.000000000000000000, -2.952720810173289112E-16, -2.061873921506763405E-30 ) ) ;
#238045 = ORIENTED_EDGE ( 'NONE', *, *, #300, .T. ) ;
#238046 = AXIS2_PLACEMENT_3D ( 'NONE', #30812, #167754, #128604 ) ;
#238047 = VECTOR ( 'NONE', #235935, 1000.000000000000000 ) ;
#238048 = EDGE_CURVE ( 'NONE', #250042, #171580, #214487, .T. ) ;
#238049 = CARTESIAN_POINT ( 'NONE',  ( -16.92989143108097849, 66.05000000001261640, -190.6406236097677720 ) ) ;
#238050 = ORIENTED_EDGE ( 'NONE', *, *, #185984, .T. ) ;
#238051 = FACE_BOUND ( 'NONE', #211498, .T. ) ;
#238052 = CARTESIAN_POINT ( 'NONE',  ( 22.43288208788031213, 26.02536192431362139, -254.3094986185249127 ) ) ;
#238053 = CARTESIAN_POINT ( 'NONE',  ( -20.85000000000000142, 78.48087866980282001, -232.8271061603568910 ) ) ;
#238054 = CARTESIAN_POINT ( 'NONE',  ( -21.65000000000000213, 66.05000000001230376, -157.3731074845244393 ) ) ;
#238055 = ADVANCED_FACE ( 'NONE', ( #177949 ), #257410, .T. ) ;
#238056 = DIRECTION ( 'NONE',  ( 0.000000000000000000, 0.000000000000000000, -1.000000000000000000 ) ) ;
#238057 = ORIENTED_EDGE ( 'NONE', *, *, #248299, .T. ) ;
#238058 = CARTESIAN_POINT ( 'NONE',  ( 20.95512820512820440, 18.86447962780959386, -229.9497396848627204 ) ) ;
#238059 = FACE_OUTER_BOUND ( 'NONE', #51828, .T. ) ;
#238060 = DIRECTION ( 'NONE',  ( 1.000000000000000000, -0.000000000000000000, -0.000000000000000000 ) ) ;
#238061 = ORIENTED_EDGE ( 'NONE', *, *, #42030, .T. ) ;
#238063 = LINE ( 'NONE', #196372, #230296 ) ;
#238062 = CIRCLE ( 'NONE', #113182, 0.1000000000000028644 ) ;
#238064 = VERTEX_POINT ( 'NONE', #254843 ) ;
#238065 = DIRECTION ( 'NONE',  ( 0.000000000000000000, -6.853228547068871147E-15, 1.000000000000000000 ) ) ;
#238066 = EDGE_LOOP ( 'NONE', ( #235727, #130305, #181540, #6295 ) ) ;
#238067 = ADVANCED_FACE ( 'NONE', ( #179244 ), #127529, .T. ) ;
#238068 = ADVANCED_FACE ( 'NONE', ( #116672, #234051 ), #239191, .T. ) ;
#238069 = DIRECTION ( 'NONE',  ( -1.000000000000000000, 0.000000000000000000, 0.000000000000000000 ) ) ;
#238070 = DIRECTION ( 'NONE',  ( 0.000000000000000000, -0.9930108503404238007, -0.1180230956473711790 ) ) ;
#238072 = EDGE_LOOP ( 'NONE', ( #167103, #41753, #59106 ) ) ;
#238071 = DIRECTION ( 'NONE',  ( 0.000000000000000000, -1.000000000000000000, -8.717686153663073805E-15 ) ) ;
#238073 = CARTESIAN_POINT ( 'NONE',  ( -18.50000000000000355, 9.122720154857383079, -245.4644708025848274 ) ) ;
#238074 = ORIENTED_EDGE ( 'NONE', *, *, #139725, .F. ) ;
#238075 = FACE_OUTER_BOUND ( 'NONE', #130123, .T. ) ;
#238076 = DIRECTION ( 'NONE',  ( 1.000000000000000000, 0.000000000000000000, 0.000000000000000000 ) ) ;
#238077 = EDGE_LOOP ( 'NONE', ( #140191, #195459, #123427, #243810 ) ) ;
#238078 = ORIENTED_EDGE ( 'NONE', *, *, #188048, .T. ) ;
#238079 = EDGE_CURVE ( 'NONE', #178529, #178867, #156777, .T. ) ;
#238080 = CARTESIAN_POINT ( 'NONE',  ( -20.96428641294188111, 11.75000000001171863, -194.1748931779392535 ) ) ;
#238081 = ORIENTED_EDGE ( 'NONE', *, *, #216150, .T. ) ;
#238082 = DIRECTION ( 'NONE',  ( 1.000000000000000000, 0.000000000000000000, 0.000000000000000000 ) ) ;
#238083 = EDGE_CURVE ( 'NONE', #168523, #99277, #39740, .T. ) ;
#238084 = EDGE_LOOP ( 'NONE', ( #22615, #141525, #76436, #247268 ) ) ;
#238085 = ORIENTED_EDGE ( 'NONE', *, *, #242558, .F. ) ;
#238086 = AXIS2_PLACEMENT_3D ( 'NONE', #173521, #234725, #35279 ) ;
#238087 = PLANE ( 'NONE',  #101343 ) ;
#238088 = ADVANCED_FACE ( 'NONE', ( #41017 ), #78806, .T. ) ;
#238090 = ORIENTED_EDGE ( 'NONE', *, *, #232517, .F. ) ;
#238089 = CARTESIAN_POINT ( 'NONE',  ( -23.49999999999994316, 64.25000000001119815, -51.02310748452479316 ) ) ;
#238091 = DIRECTION ( 'NONE',  ( 0.000000000000000000, 0.000000000000000000, -1.000000000000000000 ) ) ;
#238092 = DIRECTION ( 'NONE',  ( -1.000000000000000000, -0.000000000000000000, 0.000000000000000000 ) ) ;
#238093 = EDGE_CURVE ( 'NONE', #103997, #181633, #160861, .T. ) ;
#238094 = DIRECTION ( 'NONE',  ( -1.000000000000000000, 3.265361837132813093E-16, 2.280189983783949500E-30 ) ) ;
#238096 = LINE ( 'NONE', #75212, #13658 ) ;
#238095 = DIRECTION ( 'NONE',  ( -0.000000000000000000, -1.897661533703519897E-16, 1.000000000000000000 ) ) ;
#238097 = CARTESIAN_POINT ( 'NONE',  ( -21.05000000000000071, 76.01771943332060744, -142.9641921729960075 ) ) ;
#238099 = ADVANCED_FACE ( 'NONE', ( #237904 ), #102609, .T. ) ;
#238098 = DIRECTION ( 'NONE',  ( 1.000000000000000000, -0.000000000000000000, 0.000000000000000000 ) ) ;
#238100 = AXIS2_PLACEMENT_3D ( 'NONE', #19512, #193010, #39086 ) ;
#238101 = CARTESIAN_POINT ( 'NONE',  ( 23.04999999999999716, 67.17743825834520521, -60.27310748452438816 ) ) ;
#238102 = AXIS2_PLACEMENT_3D ( 'NONE', #117272, #58552, #37752 ) ;
#238103 = CARTESIAN_POINT ( 'NONE',  ( 22.49999999999999645, -3.092988775432923720, -228.1437074281570858 ) ) ;
#238104 = CIRCLE ( 'NONE', #163303, 2.100000000000002309 ) ;
#238105 = ORIENTED_EDGE ( 'NONE', *, *, #52909, .T. ) ;
#238107 = ORIENTED_EDGE ( 'NONE', *, *, #83553, .T. ) ;
#238106 = DIRECTION ( 'NONE',  ( 0.000000000000000000, 0.2128009952263604232, -0.9770955615653316162 ) ) ;
#238108 = ORIENTED_EDGE ( 'NONE', *, *, #8061, .F. ) ;
#238109 = FACE_OUTER_BOUND ( 'NONE', #161758, .T. ) ;
#238110 = EDGE_LOOP ( 'NONE', ( #84192, #104607, #64162, #255194 ) ) ;
#238111 = CARTESIAN_POINT ( 'NONE',  ( 18.59999999999999076, 76.00000000001126921, -203.5231074845248997 ) ) ;
#238112 = ADVANCED_FACE ( 'NONE', ( #215760 ), #37161, .T. ) ;
#238113 = ADVANCED_FACE ( 'NONE', ( #145212 ), #25298, .T. ) ;
#238114 = EDGE_LOOP ( 'NONE', ( #88606, #193612, #88242, #102406 ) ) ;
#238115 = AXIS2_PLACEMENT_3D ( 'NONE', #137864, #255205, #2204 ) ;
#238116 = SHAPE_REPRESENTATION_RELATIONSHIP ( 'NONE' , 'NONE' ,  #63487, #132346 ) ;
#238117 = DIRECTION ( 'NONE',  ( 1.000000000000000000, 0.000000000000000000, 0.000000000000000000 ) ) ;
#238119 = ORIENTED_EDGE ( 'NONE', *, *, #18445, .T. ) ;
#238118 = ORIENTED_EDGE ( 'NONE', *, *, #24405, .T. ) ;
#238120 = VERTEX_POINT ( 'NONE', #22737 ) ;
#238121 = ORIENTED_EDGE ( 'NONE', *, *, #163282, .F. ) ;
#238122 = CARTESIAN_POINT ( 'NONE',  ( 20.94999999999999929, 20.61385802457731131, -234.8303051839938007 ) ) ;
#238123 = DIRECTION ( 'NONE',  ( 0.000000000000000000, 0.2617529984165180013, 0.9651348961777117541 ) ) ;
#238125 = VERTEX_POINT ( 'NONE', #243035 ) ;
#238124 = CARTESIAN_POINT ( 'NONE',  ( -18.59999999999999787, -1.835859311432481045, -78.50443916879852679 ) ) ;
#238126 = CARTESIAN_POINT ( 'NONE',  ( -21.14999999999999858, 1.148907358139439339E-11, -201.0000000000015064 ) ) ;
#238127 = CARTESIAN_POINT ( 'NONE',  ( -20.94999999999999929, 64.35000000001251408, -176.8069731475025321 ) ) ;
#238129 = ORIENTED_EDGE ( 'NONE', *, *, #91189, .T. ) ;
#238128 = LINE ( 'NONE', #59462, #222521 ) ;
#238130 = CARTESIAN_POINT ( 'NONE',  ( 19.87657994471988232, 11.75000000001116263, -125.2657881246251037 ) ) ;
#238131 = ORIENTED_EDGE ( 'NONE', *, *, #118099, .T. ) ;
#238132 = DIRECTION ( 'NONE',  ( -1.000000000000000000, -0.000000000000000000, 0.000000000000000000 ) ) ;
#238134 = ORIENTED_EDGE ( 'NONE', *, *, #61241, .T. ) ;
#238133 = CARTESIAN_POINT ( 'NONE',  ( 21.14999999999999503, 87.65000000001172964, -81.27310748452423184 ) ) ;
#238135 = DIRECTION ( 'NONE',  ( 1.000000000000000000, 0.000000000000000000, 0.000000000000000000 ) ) ;
#238136 = DIRECTION ( 'NONE',  ( 1.000000000000000000, -0.000000000000000000, -0.000000000000000000 ) ) ;
#238137 = AXIS2_PLACEMENT_3D ( 'NONE', #95599, #116462, #59007 ) ;
#238138 = CIRCLE ( 'NONE', #13308, 0.09999999999998898659 ) ;
#238139 = CARTESIAN_POINT ( 'NONE',  ( 21.05000000000000071, 11.75000000001115907, -59.98519422934606382 ) ) ;
#238140 = VECTOR ( 'NONE', #256133, 1000.000000000000000 ) ;
#238141 = ORIENTED_EDGE ( 'NONE', *, *, #35042, .F. ) ;
#238143 = CARTESIAN_POINT ( 'NONE',  ( -16.89268316805466341, 44.12952801035616801, -235.2997120924900969 ) ) ;
#238142 = CARTESIAN_POINT ( 'NONE',  ( -16.87683809663752754, 9.865889849343568940, -46.76742680706958311 ) ) ;
#238144 = DIRECTION ( 'NONE',  ( 0.000000000000000000, 0.4999999999999478195, -0.8660254037844686836 ) ) ;
#238145 = CARTESIAN_POINT ( 'NONE',  ( 18.40916198585734165, 85.50000000001240608, -163.4229178527016586 ) ) ;
#238146 = ADVANCED_FACE ( 'NONE', ( #102209 ), #82648, .F. ) ;
#238147 = CARTESIAN_POINT ( 'NONE',  ( -23.15000000000000213, 1.115600667400684642E-11, -167.5000000000000284 ) ) ;
#238148 = FACE_OUTER_BOUND ( 'NONE', #4189, .T. ) ;
#238149 = ORIENTED_EDGE ( 'NONE', *, *, #228048, .T. ) ;
#238150 = ORIENTED_EDGE ( 'NONE', *, *, #255409, .F. ) ;
#238151 = ORIENTED_EDGE ( 'NONE', *, *, #199429, .F. ) ;
#238152 = CARTESIAN_POINT ( 'NONE',  ( -16.94445028196808778, 9.992063609708889516, -180.1073301784184366 ) ) ;
#238153 = ORIENTED_EDGE ( 'NONE', *, *, #105804, .F. ) ;
#238154 = DIRECTION ( 'NONE',  ( 0.000000000000000000, -0.2605042016806647931, -0.9654727137038724427 ) ) ;
#238155 = EDGE_LOOP ( 'NONE', ( #255746, #191289, #173824, #208195 ) ) ;
#238156 = DIRECTION ( 'NONE',  ( 2.952720810173289112E-16, -1.000000000000000000, 0.000000000000000000 ) ) ;
#238157 = CARTESIAN_POINT ( 'NONE',  ( -22.39999999999999503, 76.00000000001243450, -177.8138870828977360 ) ) ;
#238158 = AXIS2_PLACEMENT_3D ( 'NONE', #206834, #144261, #107727 ) ;
#238159 = ORIENTED_EDGE ( 'NONE', *, *, #202651, .F. ) ;
#238160 = DIRECTION ( 'NONE',  ( 0.000000000000000000, 1.000000000000000000, 0.000000000000000000 ) ) ;
#238161 =( NAMED_UNIT ( * ) PLANE_ANGLE_UNIT ( ) SI_UNIT ( $, .RADIAN. ) );
#238162 = ADVANCED_FACE ( 'NONE', ( #180510 ), #129312, .F. ) ;
#238163 = ORIENTED_EDGE ( 'NONE', *, *, #205164, .T. ) ;
#238164 = ORIENTED_EDGE ( 'NONE', *, *, #51420, .T. ) ;
#238165 = ORIENTED_EDGE ( 'NONE', *, *, #182945, .T. ) ;
#238166 = CARTESIAN_POINT ( 'NONE',  ( -22.50000000000000000, 64.25000000001195133, -103.0231074845244024 ) ) ;
#238167 = DIRECTION ( 'NONE',  ( -1.000000000000000000, 0.000000000000000000, 0.000000000000000000 ) ) ;
#238168 = CARTESIAN_POINT ( 'NONE',  ( -20.54999999999999716, 85.00000000001207923, -126.6291383618717816 ) ) ;
#238169 = DIRECTION ( 'NONE',  ( 0.000000000000000000, 0.7397890806274222131, 0.6728388485993012091 ) ) ;
#238170 = DIRECTION ( 'NONE',  ( -1.000000000000000000, 0.000000000000000000, 0.000000000000000000 ) ) ;
#238171 = AXIS2_PLACEMENT_3D ( 'NONE', #92496, #72977, #149933 ) ;
#238173 = CARTESIAN_POINT ( 'NONE',  ( 20.94999999999999574, 74.15091558138504979, -124.8670969630771879 ) ) ;
#238172 = CARTESIAN_POINT ( 'NONE',  ( 20.05000000000002913, 62.65526179112260508, -225.0299194783148664 ) ) ;
#238174 = DIRECTION ( 'NONE',  ( 1.000000000000000000, 0.000000000000000000, 0.000000000000000000 ) ) ;
#238176 = EDGE_LOOP ( 'NONE', ( #32633, #141934, #217562 ) ) ;
#238175 = DIRECTION ( 'NONE',  ( 0.000000000000000000, 1.000000000000000000, 1.224646799147353207E-16 ) ) ;
#238177 = CARTESIAN_POINT ( 'NONE',  ( 21.05000000000000071, 1.115600667400684642E-11, -33.50000000000000000 ) ) ;
#238178 = VERTEX_POINT ( 'NONE', #63106 ) ;
#238179 = CARTESIAN_POINT ( 'NONE',  ( -18.42609945526410442, -9.499999710479542614, -140.9993624902473925 ) ) ;
#238180 = ORIENTED_EDGE ( 'NONE', *, *, #51115, .T. ) ;
#238181 = ORIENTED_EDGE ( 'NONE', *, *, #53311, .F. ) ;
#238182 = CARTESIAN_POINT ( 'NONE',  ( -16.94445028196807002, 66.00793639031378746, -48.63043766294283898 ) ) ;
#238183 = TOROIDAL_SURFACE ( 'NONE', #217329, 0.4000000000000012990, 0.1000000000000000056 ) ;
#238184 = CARTESIAN_POINT ( 'NONE',  ( -21.05000000000000071, 87.48912529308779540, -72.42310748452423752 ) ) ;
#238185 = DIRECTION ( 'NONE',  ( 0.000000000000000000, 0.000000000000000000, 1.000000000000000000 ) ) ;
#238186 = VERTEX_POINT ( 'NONE', #124393 ) ;
#238187 = CIRCLE ( 'NONE', #142504, 0.09999999999998898659 ) ;
#238188 = AXIS2_PLACEMENT_3D ( 'NONE', #204875, #165790, #127932 ) ;
#238189 = AXIS2_PLACEMENT_3D ( 'NONE', #185514, #181672, #241633 ) ;
#238190 = LINE ( 'NONE', #119562, #17647 ) ;
#238191 = CIRCLE ( 'NONE', #21738, 0.09999999999999939493 ) ;
#238192 = EDGE_LOOP ( 'NONE', ( #236463, #187545, #3744, #107717 ) ) ;
#238193 = EDGE_LOOP ( 'NONE', ( #37181, #198101, #212111, #57759 ) ) ;
#238194 = B_SPLINE_CURVE_WITH_KNOTS ( 'NONE', 3,
 ( #180947, #42711, #240918, #182235, #218764, #122257, #178405, #40178, #256571, #179671, #98797, #100088, #221327, #257857, #117124, #20606, #201778, #37599, #80521, #79247, #200505, #77977, #119699, #157573, #41454, #177119, #978, #57115, #62277, #196643 ),
 .UNSPECIFIED., .F., .F.,
 ( 4, 2, 2, 2, 2, 2, 2, 2, 2, 2, 2, 2, 2, 2, 4 ),
 ( 0.000000000000000000, 0.0003422764154113468963, 0.0006845528308226937926, 0.001026829246234040689, 0.001369105661645387585, 0.002053658492468048852, 0.002738211323290710986, 0.003080487738702042053, 0.003422764154113372686, 0.003765040569524704187, 0.004107316984936035253, 0.004449593400347366320, 0.004791869815758697387, 0.005134146231170028454, 0.005476422646581359521 ),
 .UNSPECIFIED. ) ;
#238195 = CIRCLE ( 'NONE', #196503, 6.329289321881370611 ) ;
#238196 = DIRECTION ( 'NONE',  ( -0.000000000000000000, -0.7397360091702755991, -0.6728971962616832059 ) ) ;
#238197 = EDGE_LOOP ( 'NONE', ( #105154, #226387, #115604, #11654, #102096 ) ) ;
#238198 = CARTESIAN_POINT ( 'NONE',  ( 20.00000000000000355, 5.472724050409166985, 16.54552871969762506 ) ) ;
#238199 = CARTESIAN_POINT ( 'NONE',  ( -20.94999999999999929, 76.00000000001126921, -203.5231074845248997 ) ) ;
#238200 = EDGE_LOOP ( 'NONE', ( #136385, #78670, #34858, #179327 ) ) ;
#238201 = CARTESIAN_POINT ( 'NONE',  ( 20.94999999999999929, -8.730841121484171907, -43.09807471898433562 ) ) ;
#238202 = LINE ( 'NONE', #139076, #69862 ) ;
#238203 = CARTESIAN_POINT ( 'NONE',  ( -21.05000000000000071, 74.83729825007462466, -195.5231074845243597 ) ) ;
#238204 = ORIENTED_EDGE ( 'NONE', *, *, #236017, .T. ) ;
#238205 = AXIS2_PLACEMENT_3D ( 'NONE', #95450, #32958, #112465 ) ;
#238207 = CIRCLE ( 'NONE', #125774, 0.09999999999998898659 ) ;
#238206 = CARTESIAN_POINT ( 'NONE',  ( -20.64999999999999858, 68.85000000001205933, -124.2731074845243455 ) ) ;
#238208 = CARTESIAN_POINT ( 'NONE',  ( -23.15000000000000213, 69.19063053712525857, -247.5666987377248631 ) ) ;
#238209 = EDGE_CURVE ( 'NONE', #99799, #101967, #69286, .T. ) ;
#238210 = CIRCLE ( 'NONE', #9086, 0.1000000000000060979 ) ;
#238211 = DIRECTION ( 'NONE',  ( 0.000000000000000000, 0.4088369013363281623, -0.9126074666063771490 ) ) ;
#238212 = AXIS2_PLACEMENT_3D ( 'NONE', #66137, #103952, #225186 ) ;
#238213 = VERTEX_POINT ( 'NONE', #141367 ) ;
#238214 = AXIS2_PLACEMENT_3D ( 'NONE', #230544, #31091, #109284 ) ;
#238215 = EDGE_CURVE ( 'NONE', #143179, #62956, #163510, .T. ) ;
#238217 = ORIENTED_EDGE ( 'NONE', *, *, #192520, .T. ) ;
#238216 = DIRECTION ( 'NONE',  ( 0.000000000000000000, 0.6728971962617172897, -0.7397360091702445128 ) ) ;
#238218 = ORIENTED_EDGE ( 'NONE', *, *, #70087, .F. ) ;
#238219 = DIRECTION ( 'NONE',  ( 1.000000000000000000, 0.000000000000000000, 0.000000000000000000 ) ) ;
#238220 = CIRCLE ( 'NONE', #9285, 0.09999999999999939493 ) ;
#238221 = DIRECTION ( 'NONE',  ( 0.000000000000000000, -7.116814260417668513E-15, 1.000000000000000000 ) ) ;
#238222 = EDGE_CURVE ( 'NONE', #64278, #65335, #245615, .T. ) ;
#238223 = DIRECTION ( 'NONE',  ( -1.000000000000000000, 0.000000000000000000, 0.000000000000000000 ) ) ;
#238224 = DIRECTION ( 'NONE',  ( 0.000000000000000000, -1.000000000000000000, 0.000000000000000000 ) ) ;
#238225 = CARTESIAN_POINT ( 'NONE',  ( -16.94878442675512886, 9.991729103002159107, -46.11178042436211655 ) ) ;
#238226 = DIRECTION ( 'NONE',  ( 0.000000000000000000, 0.000000000000000000, -1.000000000000000000 ) ) ;
#238227 = ORIENTED_EDGE ( 'NONE', *, *, #253562, .F. ) ;
#238228 = CARTESIAN_POINT ( 'NONE',  ( -16.91256925476570316, 63.08204023972218266, -213.0047279777396625 ) ) ;
#238229 = DIRECTION ( 'NONE',  ( 1.000000000000000000, -0.000000000000000000, -0.000000000000000000 ) ) ;
#238230 = LINE ( 'NONE', #180843, #193958 ) ;
#238231 = CARTESIAN_POINT ( 'NONE',  ( 21.05000000000000071, 53.66153320161009788, -235.9075159595686841 ) ) ;
#238232 = EDGE_CURVE ( 'NONE', #47571, #181753, #219280, .T. ) ;
#238233 = AXIS2_PLACEMENT_3D ( 'NONE', #63184, #240557, #102287 ) ;
#238234 = AXIS2_PLACEMENT_3D ( 'NONE', #163861, #102559, #222520 ) ;
#238235 = CARTESIAN_POINT ( 'NONE',  ( 20.52683494730046476, 67.01946918171023526, -61.01785476198719493 ) ) ;
#238236 = CIRCLE ( 'NONE', #246614, 0.09999999999998898659 ) ;
#238237 = VECTOR ( 'NONE', #138109, 1000.000000000000000 ) ;
#238238 = ORIENTED_EDGE ( 'NONE', *, *, #182641, .T. ) ;
#238239 = ORIENTED_EDGE ( 'NONE', *, *, #212472, .F. ) ;
#238240 = DIRECTION ( 'NONE',  ( -1.000000000000000000, -9.012599976027990443E-15, -6.882867235861669241E-14 ) ) ;
#238241 = CARTESIAN_POINT ( 'NONE',  ( -18.59999999999999787, 1.115600667400684642E-11, -67.00000000000000000 ) ) ;
#238242 = CARTESIAN_POINT ( 'NONE',  ( 18.54286124688533377, -9.623917578797810179, -40.24120233186267370 ) ) ;
#238243 = CARTESIAN_POINT ( 'NONE',  ( -21.05000000000000782, 69.66772772607704667, -203.4855714212387738 ) ) ;
#238244 = CARTESIAN_POINT ( 'NONE',  ( -20.54999999999999716, 54.82645269529697885, -239.3027372265576957 ) ) ;
#238245 = ADVANCED_FACE ( 'NONE', ( #143933 ), #155981, .T. ) ;
#238246 =( BOUNDED_CURVE ( )  B_SPLINE_CURVE ( 3, ( #57641, #58909, #17264, #35559 ),
 .UNSPECIFIED., .F., .F. ) 
 B_SPLINE_CURVE_WITH_KNOTS ( ( 4, 4 ),
 ( 4.937700262164173333E-15, 1.570796326794912323 ),
 .UNSPECIFIED. ) 
 CURVE ( )  GEOMETRIC_REPRESENTATION_ITEM ( )  RATIONAL_B_SPLINE_CURVE ( ( 1.000000000000000000, 0.8047378541243623840, 0.8047378541243623840, 1.000000000000000000 ) ) 
 REPRESENTATION_ITEM ( '' )  );
#238247 = ORIENTED_EDGE ( 'NONE', *, *, #102913, .T. ) ;
#238248 = DIRECTION ( 'NONE',  ( -0.000000000000000000, -0.8096735173027138632, 0.5868805631290339164 ) ) ;
#238249 = DIRECTION ( 'NONE',  ( 0.000000000000000000, -0.8814952561688430555, 0.4721928772777346239 ) ) ;
#238250 = CARTESIAN_POINT ( 'NONE',  ( -20.64999999999999858, 85.40000000001188596, -93.12913836187179584 ) ) ;
#238251 = CARTESIAN_POINT ( 'NONE',  ( -22.50000000000000000, 1.115600667400684642E-11, -66.90000000000004832 ) ) ;
#238252 = CIRCLE ( 'NONE', #117645, 0.09999999999999939493 ) ;
#238253 = ORIENTED_EDGE ( 'NONE', *, *, #174070, .F. ) ;
#238255 =( BOUNDED_SURFACE ( )  B_SPLINE_SURFACE ( 3, 2, ( 
 ( #106097, #226036, #185665 ),
 ( #47418, #7020, #107402 ),
 ( #27907, #245639, #126975 ),
 ( #246909, #68293, #150411 ),
 ( #113826, #116411, #10890 ),
 ( #75992, #194689, #229930 ),
 ( #73454, #235075, #90406 ),
 ( #232522, #33063, #35615 ) ),
 .UNSPECIFIED., .F., .F., .F. ) 
 B_SPLINE_SURFACE_WITH_KNOTS ( ( 4, 2, 2, 4 ),
 ( 3, 3 ),
 ( 0.0001704874539069819431, 0.0003809798300636536481, 0.0004862260181419895142, 0.0005914722062203253260 ),
 ( 0.000000000000000000, 1.000000000000000000 ),
 .UNSPECIFIED. ) 
 GEOMETRIC_REPRESENTATION_ITEM ( )  RATIONAL_B_SPLINE_SURFACE ( (
 ( 1.000000000000000000, 0.7071067811865795472, 1.000000000000000000),
 ( 1.000000000000000000, 0.7670648383563467565, 1.000000000000000000),
 ( 1.000000000000000000, 0.8204820770268871355, 1.000000000000000000),
 ( 1.000000000000000000, 0.8877218296105150452, 1.000000000000000000),
 ( 1.000000000000000000, 0.9080815932665030621, 1.000000000000000000),
 ( 1.000000000000000000, 0.9395541505862222698, 1.000000000000000000),
 ( 1.000000000000000000, 0.9506520335379197162, 1.000000000000000000),
 ( 1.000000000000000000, 0.9504532311154330060, 1.000000000000000000) ) ) 
 REPRESENTATION_ITEM ( '' )  SURFACE ( )  );
#238254 = CARTESIAN_POINT ( 'NONE',  ( -18.40000000000000213, 64.51332499825495859, -194.2731074845244450 ) ) ;
#238256 = ORIENTED_EDGE ( 'NONE', *, *, #122902, .F. ) ;
#238257 = CARTESIAN_POINT ( 'NONE',  ( 20.94999999999999929, 11.60058429089262333, -246.3380203656811887 ) ) ;
#238258 = DIRECTION ( 'NONE',  ( 1.000000000000000000, 0.000000000000000000, 0.000000000000000000 ) ) ;
#238259 = CYLINDRICAL_SURFACE ( 'NONE', #199138, 0.09999999999999986677 ) ;
#238260 = LINE ( 'NONE', #42633, #107222 ) ;
#238261 = LINE ( 'NONE', #80436, #15569 ) ;
#238262 = CARTESIAN_POINT ( 'NONE',  ( 21.05000000000000071, 18.75483929237739389, -228.0790484105328630 ) ) ;
#238263 = CARTESIAN_POINT ( 'NONE',  ( -23.25000000000000000, 1.115600667400684642E-11, -33.50000000000000000 ) ) ;
#238264 = FACE_OUTER_BOUND ( 'NONE', #155905, .T. ) ;
#238265 = CARTESIAN_POINT ( 'NONE',  ( 20.73486653747088582, 68.75000000001259082, -194.2731074845244166 ) ) ;
#238266 = FACE_OUTER_BOUND ( 'NONE', #36439, .T. ) ;
#238267 = LINE ( 'NONE', #256493, #31287 ) ;
#238268 = FACE_OUTER_BOUND ( 'NONE', #73335, .T. ) ;
#238269 = CARTESIAN_POINT ( 'NONE',  ( 21.14999999999999858, 10.71339244341104013, -45.85000000000000142 ) ) ;
#238270 = CARTESIAN_POINT ( 'NONE',  ( 21.05000000000000071, 56.16603649944111254, -228.1013850343386480 ) ) ;
#238271 =( BOUNDED_CURVE ( )  B_SPLINE_CURVE ( 3, ( #157620, #119755, #61030, #97571 ),
 .UNSPECIFIED., .F., .F. ) 
 B_SPLINE_CURVE_WITH_KNOTS ( ( 4, 4 ),
 ( 3.141592653589793116, 4.712388980384689674 ),
 .UNSPECIFIED. ) 
 CURVE ( )  GEOMETRIC_REPRESENTATION_ITEM ( )  RATIONAL_B_SPLINE_CURVE ( ( 1.000000000000000000, 0.8047378541243649375, 0.8047378541243649375, 1.000000000000000000 ) ) 
 REPRESENTATION_ITEM ( '' )  );
#238272 = EDGE_CURVE ( 'NONE', #246496, #17682, #90272, .T. ) ;
#238273 = AXIS2_PLACEMENT_3D ( 'NONE', #35910, #134954, #256146 ) ;
#238274 = ORIENTED_EDGE ( 'NONE', *, *, #69153, .T. ) ;
#238275 = DIRECTION ( 'NONE',  ( -1.000000000000000000, -0.000000000000000000, -0.000000000000000000 ) ) ;
#238276 = CARTESIAN_POINT ( 'NONE',  ( -21.44999999999999929, 7.350000000011155166, -79.25000000000004263 ) ) ;
#238277 = CARTESIAN_POINT ( 'NONE',  ( 20.22894356738450838, 9.278498222849625776, -41.76852290624416497 ) ) ;
#238278 = ADVANCED_FACE ( 'NONE', ( #92948 ), #8299, .F. ) ;
#238279 = ORIENTED_EDGE ( 'NONE', *, *, #213436, .F. ) ;
#238280 = DIRECTION ( 'NONE',  ( 1.000000000000000000, 0.000000000000000000, 0.000000000000000000 ) ) ;
#238281 = DIRECTION ( 'NONE',  ( 1.000000000000000000, -7.304098846218134667E-16, -4.217023435051626718E-16 ) ) ;
#238282 = EDGE_CURVE ( 'NONE', #192523, #204747, #248184, .T. ) ;
#238283 = EDGE_LOOP ( 'NONE', ( #58623, #32566, #50531, #105281 ) ) ;
#238285 = EDGE_CURVE ( 'NONE', #196401, #159975, #252593, .T. ) ;
#238284 = DIRECTION ( 'NONE',  ( 0.000000000000000000, 0.000000000000000000, -1.000000000000000000 ) ) ;
#238286 = CARTESIAN_POINT ( 'NONE',  ( -18.59999999999999787, 74.16465844978745281, -91.36795619196134055 ) ) ;
#238287 = AXIS2_PLACEMENT_3D ( 'NONE', #96141, #175723, #137835 ) ;
#238288 = ORIENTED_EDGE ( 'NONE', *, *, #14823, .F. ) ;
#238289 = AXIS2_PLACEMENT_3D ( 'NONE', #106815, #186384, #222913 ) ;
#238290 = VERTEX_POINT ( 'NONE', #228638 ) ;
#238291 = CARTESIAN_POINT ( 'NONE',  ( -20.64999999999999858, 74.00000000001156764, -56.29848556176223440 ) ) ;
#238292 = AXIS2_PLACEMENT_3D ( 'NONE', #39032, #58555, #178557 ) ;
#238293 = EDGE_CURVE ( 'NONE', #86497, #223695, #189497, .T. ) ;
#238294 = ORIENTED_EDGE ( 'NONE', *, *, #76404, .F. ) ;
#238295 = EDGE_CURVE ( 'NONE', #147404, #22985, #112528, .T. ) ;
#238296 = CARTESIAN_POINT ( 'NONE',  ( -18.59999999999999787, -1.249999999999999334, -41.30048075441507649 ) ) ;
#238297 = FACE_BOUND ( 'NONE', #124265, .T. ) ;
#238299 = CARTESIAN_POINT ( 'NONE',  ( 18.49999999999999289, 14.80545736607782814, -235.9842437978701639 ) ) ;
#238298 = PRODUCT_DEFINITION_CONTEXT ( 'detailed design', #55765, 'design' ) ;
#238300 = EDGE_CURVE ( 'NONE', #230635, #514, #52679, .T. ) ;
#238301 = CARTESIAN_POINT ( 'NONE',  ( 20.94999999999999929, 76.00000000001239187, -162.2231074845243768 ) ) ;
#238302 = DIRECTION ( 'NONE',  ( 0.000000000000000000, 0.9908441862701791170, -0.1350103645450472789 ) ) ;
#238303 = CARTESIAN_POINT ( 'NONE',  ( -23.15000000000000213, 2.500000000011154633, -120.7753780772379457 ) ) ;
#238304 = AXIS2_PLACEMENT_3D ( 'NONE', #209571, #173055, #131308 ) ;
#238305 = FACE_OUTER_BOUND ( 'NONE', #89094, .T. ) ;
#238307 = CARTESIAN_POINT ( 'NONE',  ( 20.04142135623730070, 11.75000000001115907, -192.1499999999999488 ) ) ;
#238306 = AXIS2_PLACEMENT_3D ( 'NONE', #72933, #208579, #9071 ) ;
#238309 = ORIENTED_EDGE ( 'NONE', *, *, #60183, .T. ) ;
#238308 = CARTESIAN_POINT ( 'NONE',  ( -18.40000000000000213, -9.499999999988851584, -40.53206939669966147 ) ) ;
#238310 = EDGE_LOOP ( 'NONE', ( #49811, #78301, #10060, #198615 ) ) ;
#238312 = CYLINDRICAL_SURFACE ( 'NONE', #89422, 0.5000000000000004441 ) ;
#238311 = CARTESIAN_POINT ( 'NONE',  ( 22.59999954896768770, -0.008828232244170662948, 11.75050867406799604 ) ) ;
#238315 = ORIENTED_EDGE ( 'NONE', *, *, #38426, .T. ) ;
#238314 = DIRECTION ( 'NONE',  ( -1.000000000000000000, 0.000000000000000000, 0.000000000000000000 ) ) ;
#238313 = DIRECTION ( 'NONE',  ( -0.000000000000000000, 0.000000000000000000, 1.000000000000000000 ) ) ;
#238316 = ORIENTED_EDGE ( 'NONE', *, *, #140784, .F. ) ;
#238317 = DIRECTION ( 'NONE',  ( 0.000000000000000000, 0.000000000000000000, 1.000000000000000000 ) ) ;
#238318 = CYLINDRICAL_SURFACE ( 'NONE', #217800, 0.09999999999999939493 ) ;
#238319 = EDGE_CURVE ( 'NONE', #93396, #80057, #177629, .T. ) ;
#238321 = EDGE_CURVE ( 'NONE', #234821, #212829, #252023, .T. ) ;
#238320 = DIRECTION ( 'NONE',  ( -0.000000000000000000, -6.982962677686266711E-15, 1.000000000000000000 ) ) ;
#238322 = SURFACE_SIDE_STYLE ('',( #158821 ) ) ;
#238323 = CARTESIAN_POINT ( 'NONE',  ( 20.94999999999999929, 28.32080209959243788, -238.8452605374484676 ) ) ;
#238324 = EDGE_CURVE ( 'NONE', #152104, #159875, #2788, .T. ) ;
#238325 = EDGE_CURVE ( 'NONE', #121302, #81650, #108667, .T. ) ;
#238326 = DIRECTION ( 'NONE',  ( 1.000000000000000000, 0.000000000000000000, 0.000000000000000000 ) ) ;
#238327 = CARTESIAN_POINT ( 'NONE',  ( 23.24999999999999645, 28.17589918783266967, -238.5974746063260739 ) ) ;
#238328 = AXIS2_PLACEMENT_3D ( 'NONE', #82117, #182555, #61303 ) ;
#238329 = AXIS2_PLACEMENT_3D ( 'NONE', #95832, #37190, #18881 ) ;
#238331 = AXIS2_PLACEMENT_3D ( 'NONE', #73447, #194682, #14758 ) ;
#238330 = FACE_OUTER_BOUND ( 'NONE', #255996, .T. ) ;
#238332 = ORIENTED_EDGE ( 'NONE', *, *, #94194, .F. ) ;
#238333 = EDGE_LOOP ( 'NONE', ( #110706, #90239, #76697, #235830 ) ) ;
#238334 = FACE_OUTER_BOUND ( 'NONE', #115577, .T. ) ;
#238335 = EDGE_LOOP ( 'NONE', ( #193605, #171700, #220512, #238759, #102342 ) ) ;
#238336 = CARTESIAN_POINT ( 'NONE',  ( 20.94999999999999574, 65.52661458509973613, -195.9444530202758870 ) ) ;
#238337 = ORIENTED_EDGE ( 'NONE', *, *, #42330, .F. ) ;
#238338 = CARTESIAN_POINT ( 'NONE',  ( 20.94999999999999929, 85.00000000001197975, -112.9170766071766820 ) ) ;
#238339 = EDGE_CURVE ( 'NONE', #161837, #57945, #72127, .T. ) ;
#238340 = DIRECTION ( 'NONE',  ( 0.000000000000000000, -0.1022405907414166287, -0.9947597004326451664 ) ) ;
#238341 = CARTESIAN_POINT ( 'NONE',  ( -20.94999999999999929, 87.48912529308817909, -133.4231074845242233 ) ) ;
#238342 = ADVANCED_FACE ( 'NONE', ( #70857 ), #128240, .F. ) ;
#238343 = CARTESIAN_POINT ( 'NONE',  ( 23.24999999999999289, 11.65000000001116298, -146.1500000000000341 ) ) ;
#238344 = DIRECTION ( 'NONE',  ( 0.000000000000000000, 0.000000000000000000, -1.000000000000000000 ) ) ;
#238345 = ORIENTED_EDGE ( 'NONE', *, *, #254559, .F. ) ;
#238346 = CARTESIAN_POINT ( 'NONE',  ( -21.14999999999999858, 11.74999999999999645, -6.783865662978151967 ) ) ;
#238347 = AXIS2_PLACEMENT_3D ( 'NONE', #172592, #9602, #214240 ) ;
#238348 = FACE_OUTER_BOUND ( 'NONE', #156985, .T. ) ;
#238349 = DIRECTION ( 'NONE',  ( 1.000000000000000000, -0.000000000000000000, -0.000000000000000000 ) ) ;
#238350 = EDGE_CURVE ( 'NONE', #109724, #86120, #13431, .T. ) ;
#238351 = CARTESIAN_POINT ( 'NONE',  ( -22.47071067811865319, 75.90090754531013317, -211.2431822290224090 ) ) ;
#238352 = ORIENTED_EDGE ( 'NONE', *, *, #37678, .F. ) ;
#238353 = CARTESIAN_POINT ( 'NONE',  ( -18.48408745364680072, 85.66432225867450256, -29.34002895119592225 ) ) ;
#238354 = ORIENTED_EDGE ( 'NONE', *, *, #190262, .F. ) ;
#238357 = ORIENTED_EDGE ( 'NONE', *, *, #97431, .F. ) ;
#238356 = DIRECTION ( 'NONE',  ( 1.734723475976817507E-14, -6.982962677686266711E-15, 1.000000000000000000 ) ) ;
#238355 = FACE_OUTER_BOUND ( 'NONE', #38390, .T. ) ;
#238358 = VECTOR ( 'NONE', #132971, 1000.000000000000000 ) ;
#238359 = CARTESIAN_POINT ( 'NONE',  ( -20.54999999999999716, 68.76258920191057200, -222.5680764032308048 ) ) ;
#238360 = DIRECTION ( 'NONE',  ( 0.000000000000000000, -0.1332476588733650935, 0.9910827722268042983 ) ) ;
#238361 = ORIENTED_EDGE ( 'NONE', *, *, #225220, .T. ) ;
#238362 = DIRECTION ( 'NONE',  ( 0.000000000000000000, -0.8700118002898359348, 0.4930308989875165082 ) ) ;
#238363 = AXIS2_PLACEMENT_3D ( 'NONE', #248376, #51422, #50158 ) ;
#238364 = CARTESIAN_POINT ( 'NONE',  ( -16.93433913041102912, 10.00597842153509376, -54.43536542739516904 ) ) ;
#238365 = DIRECTION ( 'NONE',  ( 1.000000000000000000, 0.000000000000000000, -0.000000000000000000 ) ) ;
#238367 = VERTEX_POINT ( 'NONE', #151682 ) ;
#238366 = FACE_OUTER_BOUND ( 'NONE', #212267, .T. ) ;
#238368 = ADVANCED_FACE ( 'NONE', ( #12163 ), #186950, .F. ) ;
#238369 = DIRECTION ( 'NONE',  ( 0.000000000000000000, 6.982962677686266711E-15, -1.000000000000000000 ) ) ;
#238370 = AXIS2_PLACEMENT_3D ( 'NONE', #64861, #223926, #42738 ) ;
#238371 = ORIENTED_EDGE ( 'NONE', *, *, #13341, .T. ) ;
#238372 = AXIS2_PLACEMENT_3D ( 'NONE', #10559, #153961, #169666 ) ;
#238373 = EDGE_CURVE ( 'NONE', #205992, #15539, #106849, .T. ) ;
#238374 = AXIS2_PLACEMENT_3D ( 'NONE', #178824, #242597, #220493 ) ;
#238375 = CARTESIAN_POINT ( 'NONE',  ( -16.86445178670579992, 9.962211629127164514, -180.1092225618826319 ) ) ;
#238376 = FACE_OUTER_BOUND ( 'NONE', #127515, .T. ) ;
#238377 = DIRECTION ( 'NONE',  ( 0.000000000000000000, 6.982962677686266711E-15, -1.000000000000000000 ) ) ;
#238378 = ORIENTED_EDGE ( 'NONE', *, *, #4383, .T. ) ;
#238379 = CARTESIAN_POINT ( 'NONE',  ( -21.64999999999999858, 10.05000000001113847, -79.65000000000004832 ) ) ;
#238381 = VERTEX_POINT ( 'NONE', #231204 ) ;
#238380 = VECTOR ( 'NONE', #95540, 1000.000000000000000 ) ;
#238382 = DIRECTION ( 'NONE',  ( 0.000000000000000000, 0.000000000000000000, -1.000000000000000000 ) ) ;
#238383 = VECTOR ( 'NONE', #213653, 1000.000000000000000 ) ;
#238384 = ADVANCED_FACE ( 'NONE', ( #52532 ), #119334, .F. ) ;
#238385 = EDGE_CURVE ( 'NONE', #192458, #113184, #98430, .T. ) ;
#238386 = CARTESIAN_POINT ( 'NONE',  ( -21.14999999999994174, 67.75000000001118394, -43.82310748452479743 ) ) ;
#238387 = CARTESIAN_POINT ( 'NONE',  ( 0.8999999999999993561, -9.650000000000003908, 26.00000000000000355 ) ) ;
#238388 = ORIENTED_EDGE ( 'NONE', *, *, #40302, .F. ) ;
#238389 = CARTESIAN_POINT ( 'NONE',  ( 23.14999999999998437, 64.25000000001237765, -170.0231074845244166 ) ) ;
#238390 = EDGE_CURVE ( 'NONE', #154962, #102511, #215194, .T. ) ;
#238391 = AXIS2_PLACEMENT_3D ( 'NONE', #212225, #213481, #110529 ) ;
#238392 = CARTESIAN_POINT ( 'NONE',  ( 20.94999999999999574, 4.273531877263399892, -211.9976340888692050 ) ) ;
#238393 = LINE ( 'NONE', #237118, #12743 ) ;
#238394 = VERTEX_POINT ( 'NONE', #98051 ) ;
#238395 = CIRCLE ( 'NONE', #118261, 12.87499999999999112 ) ;
#238396 = AXIS2_PLACEMENT_3D ( 'NONE', #212515, #233371, #255416 ) ;
#238397 = CARTESIAN_POINT ( 'NONE',  ( 20.97239005616515328, 8.874843841350120499, -12.25015280215317048 ) ) ;
#238398 = DIRECTION ( 'NONE',  ( -0.000000000000000000, -0.000000000000000000, -1.000000000000000000 ) ) ;
#238400 = DIRECTION ( 'NONE',  ( 0.000000000000000000, 0.000000000000000000, 1.000000000000000000 ) ) ;
#238399 = AXIS2_PLACEMENT_3D ( 'NONE', #67255, #248467, #205472 ) ;
#238401 = ADVANCED_FACE ( 'NONE', ( #233764 ), #58929, .T. ) ;
#238402 = ORIENTED_EDGE ( 'NONE', *, *, #115012, .F. ) ;
#238403 = EDGE_CURVE ( 'NONE', #46937, #121101, #56160, .T. ) ;
#238404 = AXIS2_PLACEMENT_3D ( 'NONE', #240320, #45956, #203752 ) ;
#238405 = VECTOR ( 'NONE', #60560, 1000.000000000000000 ) ;
#238406 = DIRECTION ( 'NONE',  ( 0.000000000000000000, 0.000000000000000000, -1.000000000000000000 ) ) ;
#238407 = VERTEX_POINT ( 'NONE', #257111 ) ;
#238409 = ORIENTED_EDGE ( 'NONE', *, *, #8531, .T. ) ;
#238408 = DIRECTION ( 'NONE',  ( 1.000000000000000000, 0.000000000000000000, 0.000000000000000000 ) ) ;
#238410 = EDGE_CURVE ( 'NONE', #236269, #185078, #56376, .T. ) ;
#238411 = CIRCLE ( 'NONE', #212907, 0.1000000000000028644 ) ;
#238414 = ORIENTED_EDGE ( 'NONE', *, *, #136801, .T. ) ;
#238413 = VERTEX_POINT ( 'NONE', #215462 ) ;
#238412 = CARTESIAN_POINT ( 'NONE',  ( -21.08078803292166725, 0.07918598715770600038, 6.333012964437140901 ) ) ;
#238415 = FACE_OUTER_BOUND ( 'NONE', #231094, .T. ) ;
#238416 = CARTESIAN_POINT ( 'NONE',  ( -21.09316766718153247, 0.03926340232583241247, -161.1298466875252586 ) ) ;
#238417 = FACE_OUTER_BOUND ( 'NONE', #73012, .T. ) ;
#238418 = CARTESIAN_POINT ( 'NONE',  ( 20.87600722750343252, 46.46487552657982434, -243.0839400145317200 ) ) ;
#238419 = PLANE ( 'NONE',  #170067 ) ;
#238420 = EDGE_CURVE ( 'NONE', #71691, #215984, #127723, .T. ) ;
#238421 = AXIS2_PLACEMENT_3D ( 'NONE', #1879, #18894, #219657 ) ;
#238422 = DIRECTION ( 'NONE',  ( -1.000000000000000000, -0.000000000000000000, -0.000000000000000000 ) ) ;
#238423 = AXIS2_PLACEMENT_3D ( 'NONE', #139840, #104229, #238967 ) ;
#238424 = CARTESIAN_POINT ( 'NONE',  ( 19.90000000000000568, 1.350000000000000089, 21.90000000000000213 ) ) ;
#238427 = CARTESIAN_POINT ( 'NONE',  ( 21.05000000000000071, 40.88152484246180052, -238.0427780438910474 ) ) ;
#238426 = CARTESIAN_POINT ( 'NONE',  ( 20.94999999999999929, 78.93126476241668854, -235.8702625865613243 ) ) ;
#238425 = CIRCLE ( 'NONE', #167909, 0.09999999999999543976 ) ;
#238428 = VERTEX_POINT ( 'NONE', #194658 ) ;
#238429 = ORIENTED_EDGE ( 'NONE', *, *, #198986, .F. ) ;
#238430 = EDGE_CURVE ( 'NONE', #190383, #36747, #181876, .T. ) ;
#238431 = DIRECTION ( 'NONE',  ( 0.000000000000000000, -0.01283462868041992250, -0.9999176327611367654 ) ) ;
#238433 = EDGE_LOOP ( 'NONE', ( #139588, #180080, #37573, #59674 ) ) ;
#238432 = DIRECTION ( 'NONE',  ( 0.000000000000000000, -0.8777080977375715243, 0.4791956752370512551 ) ) ;
#238434 = CARTESIAN_POINT ( 'NONE',  ( -23.15000000000000213, 1.115600667400684642E-11, -37.65000000000000568 ) ) ;
#238435 = ORIENTED_EDGE ( 'NONE', *, *, #72631, .T. ) ;
#238436 = CYLINDRICAL_SURFACE ( 'NONE', #201721, 0.09999999999999939493 ) ;
#238437 = EDGE_LOOP ( 'NONE', ( #222989, #53133, #159196, #76130 ) ) ;
#238438 = EDGE_CURVE ( 'NONE', #239104, #252537, #138472, .T. ) ;
#238439 = EDGE_CURVE ( 'NONE', #157096, #22805, #19855, .T. ) ;
#238440 = VERTEX_POINT ( 'NONE', #99349 ) ;
#238441 = DIRECTION ( 'NONE',  ( 1.734723475976817507E-14, 0.000000000000000000, -1.000000000000000000 ) ) ;
#238442 = VECTOR ( 'NONE', #38682, 1000.000000000000114 ) ;
#238444 = ORIENTED_EDGE ( 'NONE', *, *, #45890, .T. ) ;
#238443 = ORIENTED_EDGE ( 'NONE', *, *, #231334, .F. ) ;
#238445 = ORIENTED_EDGE ( 'NONE', *, *, #125816, .F. ) ;
#238446 = DIRECTION ( 'NONE',  ( 0.000000000000000000, 0.000000000000000000, -1.000000000000000000 ) ) ;
#238447 = VERTEX_POINT ( 'NONE', #55081 ) ;
#238448 = VERTEX_POINT ( 'NONE', #193358 ) ;
#238449 = CARTESIAN_POINT ( 'NONE',  ( -18.59999999999999787, 68.75000000001223555, -148.6731074845244223 ) ) ;
#238450 = AXIS2_PLACEMENT_3D ( 'NONE', #55096, #214214, #17303 ) ;
#238452 = ORIENTED_EDGE ( 'NONE', *, *, #105037, .T. ) ;
#238451 = CARTESIAN_POINT ( 'NONE',  ( 18.44208962362733573, -9.552340496897292255, -107.3421730554639026 ) ) ;
#238453 = EDGE_CURVE ( 'NONE', #83539, #187924, #96772, .T. ) ;
#238455 = DIRECTION ( 'NONE',  ( 0.000000000000000000, -6.467318590049456648E-15, 1.000000000000000000 ) ) ;
#238454 = PLANE ( 'NONE',  #190644 ) ;
#238456 = DIRECTION ( 'NONE',  ( 0.000000000000000000, -0.9947597004326491632, 0.1022405907413782566 ) ) ;
#238457 = DIRECTION ( 'NONE',  ( -0.000000000000000000, 1.000000000000000000, -0.000000000000000000 ) ) ;
#238458 = CARTESIAN_POINT ( 'NONE',  ( 21.78635804494511419, 30.19765029368026887, -252.3372479796726680 ) ) ;
#238459 = VERTEX_POINT ( 'NONE', #261 ) ;
#238460 = VERTEX_POINT ( 'NONE', #77228 ) ;
#238461 = CARTESIAN_POINT ( 'NONE',  ( 20.95512820512820440, 13.19486920349904224, -219.8744268493789491 ) ) ;
#238462 = FACE_OUTER_BOUND ( 'NONE', #80636, .T. ) ;
#238463 = DIRECTION ( 'NONE',  ( 1.000000000000000000, 7.304098846218135653E-16, 5.311601492717085047E-30 ) ) ;
#238464 = EDGE_LOOP ( 'NONE', ( #192545, #126705, #226734, #198644 ) ) ;
#238465 = CARTESIAN_POINT ( 'NONE',  ( 23.14999999999999858, 67.23127455305835554, -235.8551265064784559 ) ) ;
#238466 = CIRCLE ( 'NONE', #72079, 0.5000000000000007772 ) ;
#238467 = CARTESIAN_POINT ( 'NONE',  ( -17.11825945287481332, 10.04999999999998295, -20.85000000000000142 ) ) ;
#238468 = DIRECTION ( 'NONE',  ( 0.000000000000000000, -0.9876197685951263461, 0.1568667991644794590 ) ) ;
#238469 = ORIENTED_EDGE ( 'NONE', *, *, #152203, .F. ) ;
#238470 = EDGE_LOOP ( 'NONE', ( #75782, #222659, #197562, #7309 ) ) ;
#238471 = CARTESIAN_POINT ( 'NONE',  ( 20.95000000000000284, 11.60000000000000675, -26.57179676972450011 ) ) ;
#238472 = EDGE_CURVE ( 'NONE', #111624, #94854, #216744, .T. ) ;
#238473 = DIRECTION ( 'NONE',  ( 0.000000000000000000, 0.000000000000000000, 1.000000000000000000 ) ) ;
#238474 = ORIENTED_EDGE ( 'NONE', *, *, #116633, .T. ) ;
#238475 = DIRECTION ( 'NONE',  ( 0.000000000000000000, 1.040834085586079681E-14, -1.000000000000000000 ) ) ;
#238476 = ORIENTED_EDGE ( 'NONE', *, *, #250710, .F. ) ;
#238477 = CARTESIAN_POINT ( 'NONE',  ( -20.94999999999999929, -1.835341550213255957, -112.0551512925630249 ) ) ;
#238478 = CARTESIAN_POINT ( 'NONE',  ( 18.57071067811864040, 10.17928932189250091, -121.8500000000000369 ) ) ;
#238480 = CARTESIAN_POINT ( 'NONE',  ( -22.50000000000000000, 55.96169194136206215, -232.9023299069559130 ) ) ;
#238479 = DIRECTION ( 'NONE',  ( 0.000000000000000000, -1.000000000000000000, -0.000000000000000000 ) ) ;
#238481 = DIRECTION ( 'NONE',  ( 0.000000000000000000, 0.000000000000000000, 1.000000000000000000 ) ) ;
#238482 = LINE ( 'NONE', #160263, #33004 ) ;
#238483 = ORIENTED_EDGE ( 'NONE', *, *, #108035, .F. ) ;
#238484 = CIRCLE ( 'NONE', #225969, 0.09999999999999036049 ) ;
#238485 = CARTESIAN_POINT ( 'NONE',  ( 23.14999999999998437, 87.75000000001237765, -170.0231074845242745 ) ) ;
#238486 = EDGE_CURVE ( 'NONE', #148690, #244782, #6900, .T. ) ;
#238487 = AXIS2_PLACEMENT_3D ( 'NONE', #120976, #105183, #184763 ) ;
#238489 = VERTEX_POINT ( 'NONE', #34298 ) ;
#238488 = ORIENTED_EDGE ( 'NONE', *, *, #26948, .T. ) ;
#238490 = ORIENTED_EDGE ( 'NONE', *, *, #253635, .F. ) ;
#238491 = AXIS2_PLACEMENT_3D ( 'NONE', #19137, #115678, #59513 ) ;
#238492 = CARTESIAN_POINT ( 'NONE',  ( 21.14999999999999858, 65.51923798433685420, -242.1677427744926092 ) ) ;
#238493 = CARTESIAN_POINT ( 'NONE',  ( 18.49999999999998934, 43.12265650693429819, -239.4782534460092052 ) ) ;
#238494 = LINE ( 'NONE', #258004, #194259 ) ;
#238495 = DIRECTION ( 'NONE',  ( 0.000000000000000000, 0.9126074666063769270, 0.4088369013363282733 ) ) ;
#238497 = CARTESIAN_POINT ( 'NONE',  ( -14.45443560709636266, 66.54940788787816075, -87.96691916571600700 ) ) ;
#238496 = CARTESIAN_POINT ( 'NONE',  ( 20.12518398540832365, 9.975088720668688680, -7.996668252469905980 ) ) ;
#238498 = ORIENTED_EDGE ( 'NONE', *, *, #157873, .F. ) ;
#238499 = CARTESIAN_POINT ( 'NONE',  ( 23.14999999999999858, 1.115600667400684642E-11, -67.00000000000000000 ) ) ;
#238500 = VERTEX_POINT ( 'NONE', #14731 ) ;
#238501 = CARTESIAN_POINT ( 'NONE',  ( 21.07016717456946253, 69.67905916191141102, -69.52310748452435973 ) ) ;
#238502 = VERTEX_POINT ( 'NONE', #173830 ) ;
#238503 = EDGE_LOOP ( 'NONE', ( #31799, #6818, #185595, #171765, #166497, #251545, #160457, #225153, #34324, #254955, #123924 ) ) ;
#238504 = DIRECTION ( 'NONE',  ( -0.000000000000000000, 1.000000000000000000, -0.000000000000000000 ) ) ;
#238506 = AXIS2_PLACEMENT_3D ( 'NONE', #241960, #43766, #88001 ) ;
#238505 = CARTESIAN_POINT ( 'NONE',  ( -21.05000000000000071, -11.64999999998884306, -131.0000000000000284 ) ) ;
#238507 = CARTESIAN_POINT ( 'NONE',  ( -23.25000000000000000, 70.79044367282321559, -234.2606625912667937 ) ) ;
#238508 = AXIS2_PLACEMENT_3D ( 'NONE', #66165, #145687, #225212 ) ;
#238509 = DIRECTION ( 'NONE',  ( 1.000000000000000000, 0.000000000000000000, 0.000000000000000000 ) ) ;
#238510 = CARTESIAN_POINT ( 'NONE',  ( 18.49999999999999645, 36.65892442174935439, -249.5511627012433848 ) ) ;
#238511 = ORIENTED_EDGE ( 'NONE', *, *, #230696, .F. ) ;
#238512 = VERTEX_POINT ( 'NONE', #255831 ) ;
#238513 = CARTESIAN_POINT ( 'NONE',  ( 18.59999999999999076, -1.835859311432481045, -212.6044391687984785 ) ) ;
#238514 = AXIS2_PLACEMENT_3D ( 'NONE', #143405, #144675, #67722 ) ;
#238515 = CARTESIAN_POINT ( 'NONE',  ( 21.05000000000000071, 77.16270174995034381, -161.9231074845243370 ) ) ;
#238516 = ORIENTED_EDGE ( 'NONE', *, *, #66157, .T. ) ;
#238517 = CYLINDRICAL_SURFACE ( 'NONE', #110465, 0.09999999999999939493 ) ;
#238518 = DIRECTION ( 'NONE',  ( 1.000000000000000000, 0.000000000000000000, 0.000000000000000000 ) ) ;
#238519 = CARTESIAN_POINT ( 'NONE',  ( -21.53551880898957904, 75.90103026544052511, -143.3079052459406171 ) ) ;
#238520 = CARTESIAN_POINT ( 'NONE',  ( -23.15000000000000213, 64.35000000001258513, -191.3731074845244393 ) ) ;
#238521 = CARTESIAN_POINT ( 'NONE',  ( -6.099999999999939249, 64.25000000001119815, -22.12310748452479103 ) ) ;
#238522 = CIRCLE ( 'NONE', #26155, 11.70000000000000284 ) ;
#238525 = DIRECTION ( 'NONE',  ( 1.000000000000000000, 0.000000000000000000, 0.000000000000000000 ) ) ;
#238524 = CIRCLE ( 'NONE', #88465, 0.09999999999999459321 ) ;
#238523 = CARTESIAN_POINT ( 'NONE',  ( -21.44999999999999929, 7.150000000011155876, -155.2500000000000284 ) ) ;
#238528 = EDGE_CURVE ( 'NONE', #51580, #229370, #185971, .T. ) ;
#238527 = CARTESIAN_POINT ( 'NONE',  ( -18.59999999999999787, 55.32469252163839712, -244.8004216010555183 ) ) ;
#238526 = VECTOR ( 'NONE', #74754, 1000.000000000000000 ) ;
#238529 = AXIS2_PLACEMENT_3D ( 'NONE', #247206, #227641, #192379 ) ;
#238530 = DIRECTION ( 'NONE',  ( -0.000000000000000000, -0.000000000000000000, 1.000000000000000000 ) ) ;
#238531 = DIRECTION ( 'NONE',  ( 0.000000000000000000, 0.000000000000000000, -1.000000000000000000 ) ) ;
#238532 = CARTESIAN_POINT ( 'NONE',  ( -18.37013991200266005, 11.49974761622313224, -57.79302301051711765 ) ) ;
#238533 = VERTEX_POINT ( 'NONE', #95519 ) ;
#238534 = EDGE_CURVE ( 'NONE', #248043, #179727, #61057, .T. ) ;
#238535 = CARTESIAN_POINT ( 'NONE',  ( 20.95556889135987788, 10.62194358774625336, -41.14239422185752204 ) ) ;
#238536 = ORIENTED_EDGE ( 'NONE', *, *, #244962, .F. ) ;
#238537 = CARTESIAN_POINT ( 'NONE',  ( -23.25000000000000000, 1.115600667400684642E-11, -67.00000000000004263 ) ) ;
#238538 = EDGE_CURVE ( 'NONE', #220463, #107823, #254565, .T. ) ;
#238539 = CARTESIAN_POINT ( 'NONE',  ( -21.95218792049438861, 0.09902843981107177507, -93.29849243875335674 ) ) ;
#238540 = DIRECTION ( 'NONE',  ( -7.304098846218134667E-16, -1.000000000000000000, -6.982962677686267499E-15 ) ) ;
#238541 = ORIENTED_EDGE ( 'NONE', *, *, #108446, .F. ) ;
#238542 = CARTESIAN_POINT ( 'NONE',  ( -18.59999999999999787, 1.866714910068465239, -45.25267524628200988 ) ) ;
#238543 = CARTESIAN_POINT ( 'NONE',  ( 23.24999999999999645, 11.75000000001113953, -146.6500000000000341 ) ) ;
#238545 = VECTOR ( 'NONE', #179039, 1000.000000000000000 ) ;
#238544 = DIRECTION ( 'NONE',  ( -1.000000000000000000, 0.000000000000000000, -0.000000000000000000 ) ) ;
#238546 = EDGE_CURVE ( 'NONE', #21653, #25805, #136053, .T. ) ;
#238547 = CARTESIAN_POINT ( 'NONE',  ( 22.39999999999999503, 11.36188319272497438, -198.4231588494578773 ) ) ;
#238548 = DIRECTION ( 'NONE',  ( 0.000000000000000000, 0.000000000000000000, 1.000000000000000000 ) ) ;
#238549 = DIRECTION ( 'NONE',  ( 0.000000000000000000, 0.000000000000000000, 1.000000000000000000 ) ) ;
#238550 = EDGE_LOOP ( 'NONE', ( #49591, #78145, #251660, #225752, #124629 ) ) ;
#238551 = CARTESIAN_POINT ( 'NONE',  ( 21.33487959338958717, 69.27444184810096317, -136.5231074845243313 ) ) ;
#238553 = ORIENTED_EDGE ( 'NONE', *, *, #63235, .T. ) ;
#238552 = FACE_OUTER_BOUND ( 'NONE', #64075, .T. ) ;
#238554 = DIRECTION ( 'NONE',  ( -1.000000000000000000, 0.000000000000000000, 0.000000000000000000 ) ) ;
#238555 = AXIS2_PLACEMENT_3D ( 'NONE', #61731, #452, #201230 ) ;
#238556 = DIRECTION ( 'NONE',  ( 0.000000000000000000, 0.01283462868040404978, 0.9999176327611370985 ) ) ;
#238557 = EDGE_CURVE ( 'NONE', #211426, #45318, #45819, .T. ) ;
#238558 = LINE ( 'NONE', #122481, #21236 ) ;
#238559 = ORIENTED_EDGE ( 'NONE', *, *, #10285, .T. ) ;
#238560 = DIRECTION ( 'NONE',  ( 0.000000000000000000, 0.000000000000000000, -1.000000000000000000 ) ) ;
#238561 = VECTOR ( 'NONE', #18239, 1000.000000000000000 ) ;
#238562 = APPLICATION_PROTOCOL_DEFINITION ( 'draft international standard', 'automotive_design', 1998, #197444 ) ;
#238565 = EDGE_CURVE ( 'NONE', #162952, #154016, #190268, .T. ) ;
#238564 = AXIS2_PLACEMENT_3D ( 'NONE', #7138, #247032, #146640 ) ;
#238563 = CARTESIAN_POINT ( 'NONE',  ( -18.60000000000000142, 85.32100840337318459, -95.78716923544635620 ) ) ;
#238566 = EDGE_LOOP ( 'NONE', ( #6220, #60808, #103342, #138270 ) ) ;
#238567 = CIRCLE ( 'NONE', #126113, 0.2000000000000041744 ) ;
#238568 = DIRECTION ( 'NONE',  ( -1.000000000000000000, 0.000000000000000000, 0.000000000000000000 ) ) ;
#238569 = CARTESIAN_POINT ( 'NONE',  ( -23.25000000000000000, -0.1008583690875562017, -21.75043287651061164 ) ) ;
#238570 = CIRCLE ( 'NONE', #42945, 4.100000000000000533 ) ;
#238571 = CARTESIAN_POINT ( 'NONE',  ( -16.78270389226384296, 9.947372616628161524, -121.3412070369114986 ) ) ;
#238572 = ORIENTED_EDGE ( 'NONE', *, *, #184297, .T. ) ;
#238573 = ORIENTED_EDGE ( 'NONE', *, *, #180316, .F. ) ;
#238574 = DIRECTION ( 'NONE',  ( 0.000000000000000000, -1.000000000000000000, 0.000000000000000000 ) ) ;
#238576 = TOROIDAL_SURFACE ( 'NONE', #167871, 7.800000000000000711, 0.1000000000000000056 ) ;
#238575 = DIRECTION ( 'NONE',  ( -3.265361837132813093E-16, 1.000000000000000000, 0.000000000000000000 ) ) ;
#238577 = EDGE_CURVE ( 'NONE', #249034, #94242, #242724, .T. ) ;
#238579 = CONICAL_SURFACE ( 'NONE', #126132, 4.049999999999998046, 0.7853981633974604915 ) ;
#238578 = DIRECTION ( 'NONE',  ( -0.000000000000000000, -6.982962677686266711E-15, 1.000000000000000000 ) ) ;
#238580 = DIRECTION ( 'NONE',  ( 0.000000000000000000, -6.982962677686266711E-15, 1.000000000000000000 ) ) ;
#238581 = CARTESIAN_POINT ( 'NONE',  ( -18.40000000000000213, 64.58541674041178737, -56.87310748452438958 ) ) ;
#238582 = CARTESIAN_POINT ( 'NONE',  ( 22.50497660315938475, -3.265725704392756334, -228.2539210476268750 ) ) ;
#238584 = FACE_OUTER_BOUND ( 'NONE', #221035, .T. ) ;
#238583 = CARTESIAN_POINT ( 'NONE',  ( -18.59999999999999787, -1.736257131586239844, -112.0686523290175245 ) ) ;
#238585 = CIRCLE ( 'NONE', #213638, 0.09999999999999939493 ) ;
#238586 = CARTESIAN_POINT ( 'NONE',  ( -23.15000000000000213, 4.617781596423511381, -222.2029736859691980 ) ) ;
#238587 = FACE_OUTER_BOUND ( 'NONE', #66501, .T. ) ;
#238588 = CARTESIAN_POINT ( 'NONE',  ( 18.50596464788227280, 65.69367753730605841, -30.51892380663480253 ) ) ;
#238589 = DIRECTION ( 'NONE',  ( 1.000000000000000000, 0.000000000000000000, 0.000000000000000000 ) ) ;
#238590 = ORIENTED_EDGE ( 'NONE', *, *, #23549, .F. ) ;
#238591 = ORIENTED_EDGE ( 'NONE', *, *, #194030, .F. ) ;
#238592 = TOROIDAL_SURFACE ( 'NONE', #184417, 0.2000000000000000111, 0.1000000000000000056 ) ;
#238593 = CARTESIAN_POINT ( 'NONE',  ( -21.14999999999999858, -0.09999999998884338825, -155.8504291924551808 ) ) ;
#238595 = CARTESIAN_POINT ( 'NONE',  ( -22.16821283564876666, 7.558973340780778649, 1.462253661542743006E-16 ) ) ;
#238594 = DIRECTION ( 'NONE',  ( 0.7071067811865388020, -0.7071067811865561215, 0.000000000000000000 ) ) ;
#238596 = AXIS2_PLACEMENT_3D ( 'NONE', #192102, #228662, #8326 ) ;
#238597 = CIRCLE ( 'NONE', #209958, 0.1000000000000001860 ) ;
#238598 = EDGE_CURVE ( 'NONE', #80343, #113334, #123616, .T. ) ;
#238599 = AXIS2_PLACEMENT_3D ( 'NONE', #138464, #253294, #113789 ) ;
#238601 = B_SPLINE_CURVE_WITH_KNOTS ( 'NONE', 3,
 ( #219507, #159559, #222054, #120458 ),
 .UNSPECIFIED., .F., .F.,
 ( 4, 4 ),
 ( 0.000000000000000000, 0.001767853679387109507 ),
 .UNSPECIFIED. ) ;
#238600 = FACE_OUTER_BOUND ( 'NONE', #149083, .T. ) ;
#238602 = DIRECTION ( 'NONE',  ( 0.000000000000000000, -0.2128009952263485993, 0.9770955615653341697 ) ) ;
#238603 = DIRECTION ( 'NONE',  ( 0.000000000000000000, 0.9876197685951252359, -0.1568667991644863424 ) ) ;
#238604 = ORIENTED_EDGE ( 'NONE', *, *, #70239, .T. ) ;
#238605 = LINE ( 'NONE', #3847, #26747 ) ;
#238606 = EDGE_CURVE ( 'NONE', #35113, #60388, #6687, .T. ) ;
#238607 = ORIENTED_EDGE ( 'NONE', *, *, #254801, .F. ) ;
#238608 = DIRECTION ( 'NONE',  ( 0.000000000000000000, 0.000000000000000000, 1.000000000000000000 ) ) ;
#238609 = ORIENTED_EDGE ( 'NONE', *, *, #207301, .T. ) ;
#238610 = ADVANCED_FACE ( 'NONE', ( #61538 ), #2823, .T. ) ;
#238611 = CARTESIAN_POINT ( 'NONE',  ( -23.25000000000000000, 78.06784868750165174, -195.8985418047209350 ) ) ;
#238612 = AXIS2_PLACEMENT_3D ( 'NONE', #250537, #11958, #95324 ) ;
#238613 = CIRCLE ( 'NONE', #47051, 1.900000000000012790 ) ;
#238614 = EDGE_CURVE ( 'NONE', #27375, #196020, #223544, .T. ) ;
#238615 = AXIS2_PLACEMENT_3D ( 'NONE', #199296, #179736, #41521 ) ;
#238616 = CARTESIAN_POINT ( 'NONE',  ( 18.41832399655374175, 85.68240326668549756, -29.36626386449693982 ) ) ;
#238617 = ORIENTED_EDGE ( 'NONE', *, *, #86419, .T. ) ;
#238618 = CARTESIAN_POINT ( 'NONE',  ( -18.50000000000000000, 11.75000000001115197, -55.25000000000004974 ) ) ;
#238619 = EDGE_CURVE ( 'NONE', #138157, #173065, #25000, .T. ) ;
#238620 = ORIENTED_EDGE ( 'NONE', *, *, #21573, .T. ) ;
#238621 = DIRECTION ( 'NONE',  ( -2.952720810173289112E-16, 1.000000000000000000, -0.000000000000000000 ) ) ;
#238622 = CARTESIAN_POINT ( 'NONE',  ( 21.04999999999999716, -0.03753606327451294855, -27.16772772606433861 ) ) ;
#238623 = CARTESIAN_POINT ( 'NONE',  ( 18.54999999999999716, 8.750000000011182166, -109.7500000000000426 ) ) ;
#238624 = EDGE_CURVE ( 'NONE', #242308, #5184, #141076, .T. ) ;
#238625 = CARTESIAN_POINT ( 'NONE',  ( 20.94999999999999929, 74.63912941281955682, -61.45010955743337178 ) ) ;
#238626 = EDGE_CURVE ( 'NONE', #106612, #189559, #44548, .T. ) ;
#238627 = DIRECTION ( 'NONE',  ( 3.469446951953728416E-14, 0.8660254037844343777, -0.5000000000000074385 ) ) ;
#238629 = CARTESIAN_POINT ( 'NONE',  ( 20.94999999999999574, 10.62357026048281128, -7.491945203230555350 ) ) ;
#238628 = DIRECTION ( 'NONE',  ( 0.000000000000000000, -0.8814952561688437216, 0.4721928772777334582 ) ) ;
#238630 = LINE ( 'NONE', #2567, #140707 ) ;
#238632 = ORIENTED_EDGE ( 'NONE', *, *, #175577, .F. ) ;
#238631 = CARTESIAN_POINT ( 'NONE',  ( 20.51284917709620359, 65.68911337716677679, -128.8506342989326470 ) ) ;
#238633 = TOROIDAL_SURFACE ( 'NONE', #179822, 11.70000000000000462, 0.1000000000000000056 ) ;
#238635 = CARTESIAN_POINT ( 'NONE',  ( -16.77683809663752257, 66.05416425680785153, -115.6870565036285683 ) ) ;
#238634 = CARTESIAN_POINT ( 'NONE',  ( -16.87665923198281348, 9.950000000011138823, -188.3499999999999659 ) ) ;
#238636 = ORIENTED_EDGE ( 'NONE', *, *, #41371, .T. ) ;
#238638 = ORIENTED_EDGE ( 'NONE', *, *, #140237, .T. ) ;
#238637 = CARTESIAN_POINT ( 'NONE',  ( 20.85000000000000142, 11.65000000000000391, -33.50000000000000000 ) ) ;
#238639 = ORIENTED_EDGE ( 'NONE', *, *, #76201, .T. ) ;
#238640 = CARTESIAN_POINT ( 'NONE',  ( 23.14999999999999503, 64.35000000001150511, -48.27310748452440237 ) ) ;
#238641 = CARTESIAN_POINT ( 'NONE',  ( 19.75857864376268935, 11.65000000001115943, -158.7500000000000284 ) ) ;
#238642 = ADVANCED_FACE ( 'NONE', ( #103203 ), #161938, .F. ) ;
#238643 = AXIS2_PLACEMENT_3D ( 'NONE', #132147, #31800, #192146 ) ;
#238644 = ORIENTED_EDGE ( 'NONE', *, *, #206821, .F. ) ;
#238645 = DIRECTION ( 'NONE',  ( 1.000000000000000000, -2.952720810173289112E-16, -2.061873921506763405E-30 ) ) ;
#238646 = CARTESIAN_POINT ( 'NONE',  ( -23.49999999999994316, 83.90000000001120384, -37.27310748452479316 ) ) ;
#238647 = DIRECTION ( 'NONE',  ( 1.000000000000000000, 0.000000000000000000, 0.000000000000000000 ) ) ;
#238648 = EDGE_CURVE ( 'NONE', #240452, #167398, #86167, .T. ) ;
#238649 = ORIENTED_EDGE ( 'NONE', *, *, #21489, .F. ) ;
#238650 = CARTESIAN_POINT ( 'NONE',  ( -20.94999999999999929, 74.16465844978787914, -158.4679561919613775 ) ) ;
#238651 = FACE_OUTER_BOUND ( 'NONE', #150981, .T. ) ;
#238652 = ORIENTED_EDGE ( 'NONE', *, *, #189624, .F. ) ;
#238653 = EDGE_LOOP ( 'NONE', ( #225678, #18471, #208310, #110118 ) ) ;
#238654 = CARTESIAN_POINT ( 'NONE',  ( -18.50000000000000000, 12.71802988599559114, -223.5105008658000543 ) ) ;
#238655 = CIRCLE ( 'NONE', #84671, 0.2000000000000090317 ) ;
#238656 = ORIENTED_EDGE ( 'NONE', *, *, #226217, .T. ) ;
#238657 = CARTESIAN_POINT ( 'NONE',  ( -18.59999999999999787, 11.75000000001115197, -188.8499999999999659 ) ) ;
#238658 = EDGE_LOOP ( 'NONE', ( #135076, #188818, #185501, #45963 ) ) ;
#238659 = CARTESIAN_POINT ( 'NONE',  ( 20.94999999999999929, 10.29270135741298731, -172.9573618871519329 ) ) ;
#238660 = EDGE_CURVE ( 'NONE', #71326, #206237, #124090, .T. ) ;
#238661 = DIRECTION ( 'NONE',  ( -1.000000000000000000, -0.000000000000000000, -0.000000000000000000 ) ) ;
#238662 = CARTESIAN_POINT ( 'NONE',  ( -23.15000000000000213, -11.64999999998884483, -122.2500000000000284 ) ) ;
#238663 = ADVANCED_FACE ( 'NONE', ( #84910 ), #244006, .T. ) ;
#238664 = CARTESIAN_POINT ( 'NONE',  ( 20.95159278453404283, 60.85485389494746755, -225.3345583954844358 ) ) ;
#238665 = EDGE_CURVE ( 'NONE', #55613, #107956, #105766, .T. ) ;
#238667 = AXIS2_PLACEMENT_3D ( 'NONE', #135943, #193391, #151711 ) ;
#238666 = LINE ( 'NONE', #219085, #133793 ) ;
#238668 = CARTESIAN_POINT ( 'NONE',  ( -23.25000000000000000, 1.148907358139439339E-11, -201.0000000000015064 ) ) ;
#238669 = CARTESIAN_POINT ( 'NONE',  ( -20.00857864376270001, 66.75000000001223555, -148.8731074845244393 ) ) ;
#238670 = ORIENTED_EDGE ( 'NONE', *, *, #250205, .T. ) ;
#238672 = CYLINDRICAL_SURFACE ( 'NONE', #60564, 0.09999999999999939493 ) ;
#238671 = CARTESIAN_POINT ( 'NONE',  ( -21.95218792049438861, 75.90097156021251124, -177.2246150457710314 ) ) ;
#238674 = ORIENTED_EDGE ( 'NONE', *, *, #128933, .F. ) ;
#238673 = CIRCLE ( 'NONE', #92909, 4.099999999999999645 ) ;
#238676 = ORIENTED_EDGE ( 'NONE', *, *, #188872, .T. ) ;
#238675 = DIRECTION ( 'NONE',  ( -1.073024830501117725E-15, 0.2617529984165031243, 0.9651348961777157509 ) ) ;
#238677 = ORIENTED_EDGE ( 'NONE', *, *, #148817, .T. ) ;
#238678 = CARTESIAN_POINT ( 'NONE',  ( -20.99142135623731065, 11.60000000001115161, -127.0717967697245570 ) ) ;
#238679 = CARTESIAN_POINT ( 'NONE',  ( 20.27550659511089037, 11.69688800608038193, -211.3990755776034405 ) ) ;
#238681 = CARTESIAN_POINT ( 'NONE',  ( -20.94999999999999929, 4.136903274969360389, -245.4596299165286268 ) ) ;
#238680 = CIRCLE ( 'NONE', #34681, 4.000000000000003553 ) ;
#238682 = CARTESIAN_POINT ( 'NONE',  ( -16.87683809663752399, 9.850000000011144508, -113.9023640181963373 ) ) ;
#238683 = EDGE_LOOP ( 'NONE', ( #116346, #182103, #25230, #231362, #130947 ) ) ;
#238684 = CARTESIAN_POINT ( 'NONE',  ( 19.97071067695815572, 16.70338566981720518, -222.6168788084382868 ) ) ;
#238685 = DIRECTION ( 'NONE',  ( 1.000000000000000000, 0.000000000000000000, 0.000000000000000000 ) ) ;
#238687 = CARTESIAN_POINT ( 'NONE',  ( -18.40000000000000213, 11.47867409999990329, -24.22530678365939494 ) ) ;
#238686 = DIRECTION ( 'NONE',  ( 0.000000000000000000, 1.000000000000000000, -0.000000000000000000 ) ) ;
#238689 = ORIENTED_EDGE ( 'NONE', *, *, #120333, .F. ) ;
#238688 = CARTESIAN_POINT ( 'NONE',  ( -16.87036670365548474, 10.08494996326643189, -87.95000000000004547 ) ) ;
#238690 = CIRCLE ( 'NONE', #167793, 0.09999999999999939493 ) ;
#238691 = ADVANCED_FACE ( 'NONE', ( #26268 ), #157139, .F. ) ;
#238692 = VECTOR ( 'NONE', #108825, 1000.000000000000000 ) ;
#238693 = ORIENTED_EDGE ( 'NONE', *, *, #216413, .F. ) ;
#238694 = EDGE_CURVE ( 'NONE', #160189, #213743, #81109, .T. ) ;
#238695 = CARTESIAN_POINT ( 'NONE',  ( 20.85000000000000142, 76.00000000001190870, -103.0231074845243029 ) ) ;
#238696 = ORIENTED_EDGE ( 'NONE', *, *, #204840, .T. ) ;
#238697 = DIRECTION ( 'NONE',  ( 0.000000000000000000, -0.4999999999999608646, 0.8660254037844612451 ) ) ;
#238698 = EDGE_LOOP ( 'NONE', ( #186465, #8166, #69556, #152572 ) ) ;
#238700 = VECTOR ( 'NONE', #21695, 1000.000000000000000 ) ;
#238699 = FACE_OUTER_BOUND ( 'NONE', #59671, .T. ) ;
#238701 = EDGE_CURVE ( 'NONE', #20940, #68680, #146193, .T. ) ;
#238702 = CARTESIAN_POINT ( 'NONE',  ( 23.24999999999999289, 64.35000000001213039, -136.4231074845243938 ) ) ;
#238703 = CYLINDRICAL_SURFACE ( 'NONE', #180759, 0.09999999999999939493 ) ;
#238704 = ORIENTED_EDGE ( 'NONE', *, *, #155252, .F. ) ;
#238705 = FACE_OUTER_BOUND ( 'NONE', #257574, .T. ) ;
#238706 = AXIS2_PLACEMENT_3D ( 'NONE', #130801, #190819, #135924 ) ;
#238707 = EDGE_CURVE ( 'NONE', #255725, #17623, #40451, .T. ) ;
#238708 = AXIS2_PLACEMENT_3D ( 'NONE', #114235, #118087, #197611 ) ;
#238709 = AXIS2_PLACEMENT_3D ( 'NONE', #15743, #232216, #95243 ) ;
#238710 = AXIS2_PLACEMENT_3D ( 'NONE', #219629, #82663, #140084 ) ;
#238711 = ADVANCED_FACE ( 'NONE', ( #225713 ), #9259, .F. ) ;
#238712 = LINE ( 'NONE', #177491, #14827 ) ;
#238713 = EDGE_CURVE ( 'NONE', #115527, #77194, #27972, .T. ) ;
#238714 = VERTEX_POINT ( 'NONE', #228319 ) ;
#238715 = VERTEX_POINT ( 'NONE', #186629 ) ;
#238717 = EDGE_CURVE ( 'NONE', #188520, #70041, #198617, .T. ) ;
#238716 = ADVANCED_FACE ( 'NONE', ( #69253 ), #207000, .T. ) ;
#238718 = ORIENTED_EDGE ( 'NONE', *, *, #16707, .T. ) ;
#238719 = LINE ( 'NONE', #60069, #141678 ) ;
#238720 = ORIENTED_EDGE ( 'NONE', *, *, #35582, .T. ) ;
#238722 = ORIENTED_EDGE ( 'NONE', *, *, #222644, .F. ) ;
#238721 = CARTESIAN_POINT ( 'NONE',  ( 20.94999999999999574, 74.16465844978715438, -57.96795619196134908 ) ) ;
#238723 = EDGE_LOOP ( 'NONE', ( #147311, #16849, #162942 ) ) ;
#238726 = VERTEX_POINT ( 'NONE', #87495 ) ;
#238725 = EDGE_LOOP ( 'NONE', ( #239188, #36789, #97474 ) ) ;
#238724 = DIRECTION ( 'NONE',  ( 1.000000000000000000, 0.000000000000000000, 0.000000000000000000 ) ) ;
#238727 = AXIS2_PLACEMENT_3D ( 'NONE', #88811, #115780, #168431 ) ;
#238728 = AXIS2_PLACEMENT_3D ( 'NONE', #60464, #22665, #486 ) ;
#238729 = EDGE_LOOP ( 'NONE', ( #77250, #54530, #12030, #45072 ) ) ;
#238730 = DIRECTION ( 'NONE',  ( -1.000000000000000000, 0.000000000000000000, 0.000000000000000000 ) ) ;
#238731 = EDGE_CURVE ( 'NONE', #121380, #7048, #169637, .T. ) ;
#238732 = EDGE_CURVE ( 'NONE', #107540, #226855, #124536, .T. ) ;
#238733 = CARTESIAN_POINT ( 'NONE',  ( -21.05000000000000071, 65.61575147395463148, -242.1939180743342774 ) ) ;
#238734 = CARTESIAN_POINT ( 'NONE',  ( -16.83233564386405590, 14.11297426559041845, -219.1366760747206399 ) ) ;
#238735 = VERTEX_POINT ( 'NONE', #167088 ) ;
#238736 = AXIS2_PLACEMENT_3D ( 'NONE', #171425, #130975, #210516 ) ;
#238737 = EDGE_CURVE ( 'NONE', #72194, #174834, #119531, .T. ) ;
#238738 = CIRCLE ( 'NONE', #205575, 0.09999999999998898659 ) ;
#238740 = ORIENTED_EDGE ( 'NONE', *, *, #102296, .F. ) ;
#238739 = CARTESIAN_POINT ( 'NONE',  ( -18.40000000000000213, 11.48667500176882328, -76.25000000000004263 ) ) ;
#238741 = FACE_OUTER_BOUND ( 'NONE', #222077, .T. ) ;
#238743 = ORIENTED_EDGE ( 'NONE', *, *, #185618, .F. ) ;
#238742 = CARTESIAN_POINT ( 'NONE',  ( 21.14999999999999858, 76.10000000001203091, -114.6726782920691079 ) ) ;
#238744 = ORIENTED_EDGE ( 'NONE', *, *, #186367, .T. ) ;
#238745 = EDGE_CURVE ( 'NONE', #163431, #171037, #246579, .T. ) ;
#238746 = AXIS2_PLACEMENT_3D ( 'NONE', #179585, #199130, #157472 ) ;
#238748 = ADVANCED_FACE ( 'NONE', ( #50927 ), #151363, .F. ) ;
#238747 = DIRECTION ( 'NONE',  ( 0.000000000000000000, -6.853228547068871147E-15, 1.000000000000000000 ) ) ;
#238749 = CIRCLE ( 'NONE', #39045, 0.1000000000000028644 ) ;
#238750 = TOROIDAL_SURFACE ( 'NONE', #30482, 3.900000000000000355, 0.1000000000000000056 ) ;
#238752 = ORIENTED_EDGE ( 'NONE', *, *, #209169, .T. ) ;
#238751 = TOROIDAL_SURFACE ( 'NONE', #126318, 0.2000000000000000111, 0.1000000000000000056 ) ;
#238753 = ORIENTED_EDGE ( 'NONE', *, *, #203529, .F. ) ;
#238754 = AXIS2_PLACEMENT_3D ( 'NONE', #174032, #236517, #136109 ) ;
#238755 = DIRECTION ( 'NONE',  ( 0.000000000000000000, 0.000000000000000000, -1.000000000000000000 ) ) ;
#238756 = CYLINDRICAL_SURFACE ( 'NONE', #135956, 0.09999999999999939493 ) ;
#238758 = ORIENTED_EDGE ( 'NONE', *, *, #219778, .F. ) ;
#238757 = ORIENTED_EDGE ( 'NONE', *, *, #44148, .T. ) ;
#238759 = ORIENTED_EDGE ( 'NONE', *, *, #185934, .F. ) ;
#238760 = FACE_OUTER_BOUND ( 'NONE', #175493, .T. ) ;
#238761 = ORIENTED_EDGE ( 'NONE', *, *, #150792, .T. ) ;
#238762 = ORIENTED_EDGE ( 'NONE', *, *, #245809, .T. ) ;
#238763 = DIRECTION ( 'NONE',  ( 0.000000000000000000, 0.000000000000000000, -1.000000000000000000 ) ) ;
#238764 = ORIENTED_EDGE ( 'NONE', *, *, #157772, .T. ) ;
#238765 = EDGE_CURVE ( 'NONE', #79629, #105518, #177805, .T. ) ;
#238766 = CARTESIAN_POINT ( 'NONE',  ( -16.93230518875208190, 12.44782693869981927, -211.1595675772403524 ) ) ;
#238767 = CIRCLE ( 'NONE', #1418, 0.09999999999999939493 ) ;
#238769 = DIRECTION ( 'NONE',  ( 0.7071067811865474617, -0.7071067811865474617, -4.937700262164531476E-15 ) ) ;
#238768 = FACE_OUTER_BOUND ( 'NONE', #189478, .T. ) ;
#238771 = ORIENTED_EDGE ( 'NONE', *, *, #88699, .T. ) ;
#238770 = AXIS2_PLACEMENT_3D ( 'NONE', #8711, #127375, #167810 ) ;
#238773 = ORIENTED_EDGE ( 'NONE', *, *, #141766, .F. ) ;
#238772 = EDGE_LOOP ( 'NONE', ( #186803, #78327, #149013, #221613 ) ) ;
#238774 = EDGE_CURVE ( 'NONE', #74786, #17092, #223729, .T. ) ;
#238775 = VECTOR ( 'NONE', #48228, 1000.000000000000000 ) ;
#238776 = CYLINDRICAL_SURFACE ( 'NONE', #27955, 11.80000000000000249 ) ;
#238777 = FACE_OUTER_BOUND ( 'NONE', #204461, .T. ) ;
#238778 = ORIENTED_EDGE ( 'NONE', *, *, #147185, .T. ) ;
#238779 = VECTOR ( 'NONE', #184843, 1000.000000000000114 ) ;
#238780 = VECTOR ( 'NONE', #98718, 1000.000000000000000 ) ;
#238781 = VECTOR ( 'NONE', #127739, 1000.000000000000000 ) ;
#238782 = AXIS2_PLACEMENT_3D ( 'NONE', #22421, #122801, #84898 ) ;
#238783 = CARTESIAN_POINT ( 'NONE',  ( -20.94999999999999929, 1.115600667400684642E-11, -67.00000000000000000 ) ) ;
#238784 = ORIENTED_EDGE ( 'NONE', *, *, #171891, .T. ) ;
#238785 = ORIENTED_EDGE ( 'NONE', *, *, #237472, .T. ) ;
#238786 = DIRECTION ( 'NONE',  ( 1.000000000000000000, 3.469446951953704435E-14, -2.003086131649669752E-14 ) ) ;
#238787 = ADVANCED_FACE ( 'NONE', ( #190495 ), #206181, .T. ) ;
#238788 = ORIENTED_EDGE ( 'NONE', *, *, #122490, .F. ) ;
#238789 = DIRECTION ( 'NONE',  ( 0.000000000000000000, 0.1495327102803689356, 0.9887567792719336168 ) ) ;
#238790 = FACE_OUTER_BOUND ( 'NONE', #75233, .T. ) ;
#238791 = ORIENTED_EDGE ( 'NONE', *, *, #121370, .F. ) ;
#238792 = CARTESIAN_POINT ( 'NONE',  ( -20.64999999999999858, -8.999999999988844479, -57.10603087734755690 ) ) ;
#238793 = CARTESIAN_POINT ( 'NONE',  ( -17.29838795458562473, 10.37154985795925199, -44.89525871738297980 ) ) ;
#238795 = CARTESIAN_POINT ( 'NONE',  ( -16.92280123533709357, 9.950000000011137047, -121.1493676859149531 ) ) ;
#238794 = FACE_OUTER_BOUND ( 'NONE', #83546, .T. ) ;
#238796 = DIRECTION ( 'NONE',  ( -1.000000000000000000, 0.000000000000000000, 0.000000000000000000 ) ) ;
#238797 = CYLINDRICAL_SURFACE ( 'NONE', #107977, 0.1000000000000028644 ) ;
#238798 = CARTESIAN_POINT ( 'NONE',  ( -16.97683809663754317, 62.92304522977585890, -213.7274810758511592 ) ) ;
#238799 = CARTESIAN_POINT ( 'NONE',  ( 20.85000000000000142, 1.115600667400684642E-11, -200.9999999999999432 ) ) ;
#238800 = CARTESIAN_POINT ( 'NONE',  ( 23.15000000000000213, 87.48912529308852015, -173.1231074845242688 ) ) ;
#238801 = DIRECTION ( 'NONE',  ( -1.000000000000000000, 0.000000000000000000, 0.000000000000000000 ) ) ;
#238802 = CIRCLE ( 'NONE', #155625, 0.09999999999999939493 ) ;
#238804 = ORIENTED_EDGE ( 'NONE', *, *, #205482, .T. ) ;
#238803 = AXIS2_PLACEMENT_3D ( 'NONE', #124495, #104876, #204013 ) ;
#238805 = AXIS2_PLACEMENT_3D ( 'NONE', #189948, #11308, #186097 ) ;
#238806 = VECTOR ( 'NONE', #247381, 1000.000000000000000 ) ;
#238808 = VERTEX_POINT ( 'NONE', #195630 ) ;
#238807 = EDGE_LOOP ( 'NONE', ( #239782, #115922, #118917, #33161 ) ) ;
#238809 = ORIENTED_EDGE ( 'NONE', *, *, #171520, .F. ) ;
#238810 = ORIENTED_EDGE ( 'NONE', *, *, #164468, .F. ) ;
#238811 = DIRECTION ( 'NONE',  ( -1.000000000000000000, -0.000000000000000000, -0.000000000000000000 ) ) ;
#238812 = CARTESIAN_POINT ( 'NONE',  ( -21.05000000000000071, -11.64999999998884306, -197.9999999999999432 ) ) ;
#238814 = DIRECTION ( 'NONE',  ( -0.000000000000000000, -0.4721928772777346239, -0.8814952561688430555 ) ) ;
#238813 = FACE_OUTER_BOUND ( 'NONE', #192002, .T. ) ;
#238815 = CARTESIAN_POINT ( 'NONE',  ( -20.54999999999999716, 84.10768549965561647, -218.5181211837136175 ) ) ;
#238816 = ORIENTED_EDGE ( 'NONE', *, *, #150629, .T. ) ;
#238817 = CARTESIAN_POINT ( 'NONE',  ( -20.94983749550516450, 10.29766095125292402, -105.9743663933276139 ) ) ;
#238818 =( NAMED_UNIT ( * ) PLANE_ANGLE_UNIT ( ) SI_UNIT ( $, .RADIAN. ) );
#238819 = DIRECTION ( 'NONE',  ( 0.000000000000000000, -0.5774316882803290918, -0.8164390028469542537 ) ) ;
#238820 = FACE_OUTER_BOUND ( 'NONE', #46579, .T. ) ;
#238821 = VERTEX_POINT ( 'NONE', #92639 ) ;
#238822 = CARTESIAN_POINT ( 'NONE',  ( -20.54999999999999716, 6.878457983866232972, -212.1414458560986986 ) ) ;
#238823 = AXIS2_PLACEMENT_3D ( 'NONE', #199848, #103266, #182857 ) ;
#238824 = DIRECTION ( 'NONE',  ( 0.000000000000000000, -1.000000000000000000, 0.000000000000000000 ) ) ;
#238825 = ORIENTED_EDGE ( 'NONE', *, *, #226984, .F. ) ;
#238826 = DIRECTION ( 'NONE',  ( 0.000000000000000000, -0.008583690987162452199, -0.9999631594459053030 ) ) ;
#238827 = FACE_OUTER_BOUND ( 'NONE', #222671, .T. ) ;
#238828 = CARTESIAN_POINT ( 'NONE',  ( 18.59999999999999787, 78.48087866980282001, -232.8271061603568910 ) ) ;
#238829 = SPHERICAL_SURFACE ( 'NONE', #223307, 0.1000000000000000056 ) ;
#238830 = DIRECTION ( 'NONE',  ( 0.000000000000000000, 0.2617529984165031243, 0.9651348961777157509 ) ) ;
#238831 = EDGE_LOOP ( 'NONE', ( #32897, #19051, #109461, #251441, #233087 ) ) ;
#238832 = DIRECTION ( 'NONE',  ( 1.000000000000000000, 7.304098846218133681E-16, -4.607487905232622991E-31 ) ) ;
#238833 = DIRECTION ( 'NONE',  ( 2.952720810173289112E-16, -1.000000000000000000, -0.000000000000000000 ) ) ;
#238834 = FACE_OUTER_BOUND ( 'NONE', #168133, .T. ) ;
#238836 = DIRECTION ( 'NONE',  ( 0.000000000000000000, 0.1298341882519953583, 0.9915357197604861561 ) ) ;
#238835 = CARTESIAN_POINT ( 'NONE',  ( -20.64999999999999858, 68.76258920191057200, -222.5680764032308048 ) ) ;
#238838 = EDGE_CURVE ( 'NONE', #52970, #176730, #138173, .T. ) ;
#238837 = CARTESIAN_POINT ( 'NONE',  ( 20.94999999999999574, -11.48912529306490349, -170.3999999999999773 ) ) ;
#238839 = DIRECTION ( 'NONE',  ( 0.000000000000000000, -0.8814952561688431665, 0.4721928772777345129 ) ) ;
#238840 = PLANE ( 'NONE',  #184678 ) ;
#238841 = CARTESIAN_POINT ( 'NONE',  ( -21.45000000000000284, 29.50054346320101928, -236.9717244483098568 ) ) ;
#238842 = AXIS2_PLACEMENT_3D ( 'NONE', #170092, #50087, #230014 ) ;
#238843 = VERTEX_POINT ( 'NONE', #34002 ) ;
#238844 = AXIS2_PLACEMENT_3D ( 'NONE', #216470, #233498, #134354 ) ;
#238845 = CIRCLE ( 'NONE', #172252, 2.000000000000002665 ) ;
#238846 = ORIENTED_EDGE ( 'NONE', *, *, #251487, .T. ) ;
#238847 = VERTEX_POINT ( 'NONE', #76933 ) ;
#238848 = ADVANCED_FACE ( 'NONE', ( #116078 ), #73754, .F. ) ;
#238849 = DIRECTION ( 'NONE',  ( -0.000000000000000000, -0.000000000000000000, -1.000000000000000000 ) ) ;
#238850 = SURFACE_STYLE_USAGE ( .BOTH. , #180177 ) ;
#238851 = EDGE_CURVE ( 'NONE', #205417, #81104, #123807, .T. ) ;
#238853 = CYLINDRICAL_SURFACE ( 'NONE', #204605, 0.09999999999999156786 ) ;
#238852 = AXIS2_PLACEMENT_3D ( 'NONE', #187032, #3208, #166194 ) ;
#238854 = CARTESIAN_POINT ( 'NONE',  ( -11.59999999999994458, 66.35000000001119247, -21.02310748452479316 ) ) ;
#238855 = ORIENTED_EDGE ( 'NONE', *, *, #3042, .F. ) ;
#238856 = VECTOR ( 'NONE', #21552, 1000.000000000000000 ) ;
#238857 = FACE_OUTER_BOUND ( 'NONE', #125939, .T. ) ;
#238858 = AXIS2_PLACEMENT_3D ( 'NONE', #120215, #41945, #201001 ) ;
#238859 = DIRECTION ( 'NONE',  ( 0.000000000000000000, -6.982962677686266711E-15, 1.000000000000000000 ) ) ;
#238860 = DIRECTION ( 'NONE',  ( 3.469446951953635015E-14, 6.982962677686266711E-15, -1.000000000000000000 ) ) ;
#238861 = CIRCLE ( 'NONE', #209636, 0.09999999999999982514 ) ;
#238862 = ADVANCED_FACE ( 'NONE', ( #233470 ), #165304, .F. ) ;
#238863 = ADVANCED_FACE ( 'NONE', ( #118659 ), #198165, .F. ) ;
#238864 = DIRECTION ( 'NONE',  ( 1.000000000000000000, -0.000000000000000000, -0.000000000000000000 ) ) ;
#238866 = ORIENTED_EDGE ( 'NONE', *, *, #238624, .T. ) ;
#238865 = LINE ( 'NONE', #137188, #254901 ) ;
#238867 = DIRECTION ( 'NONE',  ( -0.7071067811865127117, -0.7071067811865821007, 0.000000000000000000 ) ) ;
#238868 = DIRECTION ( 'NONE',  ( 1.000000000000000000, 0.000000000000000000, 0.000000000000000000 ) ) ;
#238869 = EDGE_CURVE ( 'NONE', #165014, #106096, #36334, .T. ) ;
#238870 = DIRECTION ( 'NONE',  ( 1.000000000000000000, -0.000000000000000000, 0.000000000000000000 ) ) ;
#238871 = ORIENTED_EDGE ( 'NONE', *, *, #194495, .T. ) ;
#238872 = CIRCLE ( 'NONE', #26498, 0.1000000000000028644 ) ;
#238873 = DIRECTION ( 'NONE',  ( 1.000000000000000000, 0.000000000000000000, 0.000000000000000000 ) ) ;
#238875 = CARTESIAN_POINT ( 'NONE',  ( -22.57320508075687115, 11.75000000001115552, -134.0000000000000000 ) ) ;
#238874 = CIRCLE ( 'NONE', #92929, 0.09999999999999939493 ) ;
#238877 = AXIS2_PLACEMENT_3D ( 'NONE', #146543, #129582, #27942 ) ;
#238876 = LINE ( 'NONE', #104467, #181570 ) ;
#238878 = EDGE_CURVE ( 'NONE', #141594, #143109, #97755, .T. ) ;
#238879 = ORIENTED_EDGE ( 'NONE', *, *, #190744, .T. ) ;
#238880 = DIRECTION ( 'NONE',  ( -1.000000000000000000, 0.000000000000000000, 0.000000000000000000 ) ) ;
#238881 = CARTESIAN_POINT ( 'NONE',  ( -22.50000000000000000, 64.18196446391819165, -247.0985338183330668 ) ) ;
#238882 = ORIENTED_EDGE ( 'NONE', *, *, #188464, .T. ) ;
#238883 = DIRECTION ( 'NONE',  ( 1.000000000000000000, -2.952720810173289112E-16, -2.061873921506763405E-30 ) ) ;
#238884 = EDGE_CURVE ( 'NONE', #34079, #194066, #153962, .T. ) ;
#238885 = AXIS2_PLACEMENT_3D ( 'NONE', #160907, #37115, #137455 ) ;
#238886 = CARTESIAN_POINT ( 'NONE',  ( -23.15000000000000213, 54.34471204062663219, -239.4366250215122420 ) ) ;
#238887 = CARTESIAN_POINT ( 'NONE',  ( 21.14999999999999858, 8.786607556600111835, -12.25000000000000000 ) ) ;
#238888 = ORIENTED_EDGE ( 'NONE', *, *, #106782, .T. ) ;
#238889 = VERTEX_POINT ( 'NONE', #54792 ) ;
#238890 = AXIS2_PLACEMENT_3D ( 'NONE', #195637, #22134, #142049 ) ;
#238891 = VECTOR ( 'NONE', #180023, 1000.000000000000114 ) ;
#238892 = TOROIDAL_SURFACE ( 'NONE', #113976, 11.65000000000000036, 0.1000000000000000056 ) ;
#238893 = EDGE_CURVE ( 'NONE', #29024, #178529, #57130, .T. ) ;
#238894 = AXIS2_PLACEMENT_3D ( 'NONE', #162917, #28570, #66360 ) ;
#238895 = CARTESIAN_POINT ( 'NONE',  ( -21.05000000000000071, 70.44746257310249860, -228.4383880063670347 ) ) ;
#238896 = FACE_OUTER_BOUND ( 'NONE', #103961, .T. ) ;
#238897 = CARTESIAN_POINT ( 'NONE',  ( 21.14999999999999858, 11.75000000001116263, -122.2500000000000284 ) ) ;
#238898 = CARTESIAN_POINT ( 'NONE',  ( 18.69999999999999929, 11.75000000000000000, -7.800000000000000711 ) ) ;
#238900 = FACE_OUTER_BOUND ( 'NONE', #55481, .T. ) ;
#238899 = FACE_OUTER_BOUND ( 'NONE', #211184, .T. ) ;
#238901 = LINE ( 'NONE', #40732, #81672 ) ;
#238902 = CARTESIAN_POINT ( 'NONE',  ( -16.81930730667006557, 66.06300193113754915, -56.79633975398618873 ) ) ;
#238903 = CARTESIAN_POINT ( 'NONE',  ( -22.50000000000000000, 64.35042919246734527, -136.6231074845243825 ) ) ;
#238904 = ORIENTED_EDGE ( 'NONE', *, *, #224159, .F. ) ;
#238905 = DIRECTION ( 'NONE',  ( 0.000000000000000000, 0.9126074666063751506, 0.4088369013363318816 ) ) ;
#238907 = EDGE_LOOP ( 'NONE', ( #31688, #103391, #85386, #15840 ) ) ;
#238906 = FACE_OUTER_BOUND ( 'NONE', #195654, .T. ) ;
#238908 = CARTESIAN_POINT ( 'NONE',  ( 22.59999985501178799, 11.74986979300298806, 0.06559866979947076571 ) ) ;
#238909 = CARTESIAN_POINT ( 'NONE',  ( 23.15000000000000213, 69.56804783242856161, -248.4091712263733882 ) ) ;
#238911 = CARTESIAN_POINT ( 'NONE',  ( 18.59999999999998366, 7.128833340094563376, -233.7327013124401276 ) ) ;
#238910 = CARTESIAN_POINT ( 'NONE',  ( -23.15000000000000213, 64.25000000001222134, -148.6731074845244507 ) ) ;
#238912 = ORIENTED_EDGE ( 'NONE', *, *, #67476, .F. ) ;
#238914 = CYLINDRICAL_SURFACE ( 'NONE', #59223, 0.5000000000000014433 ) ;
#238913 = CYLINDRICAL_SURFACE ( 'NONE', #222439, 0.09999999999999939493 ) ;
#238915 = DIRECTION ( 'NONE',  ( 0.000000000000000000, 0.000000000000000000, 1.000000000000000000 ) ) ;
#238916 = FACE_OUTER_BOUND ( 'NONE', #174202, .T. ) ;
#238917 = CARTESIAN_POINT ( 'NONE',  ( -23.15000000000000213, -11.48912529306489994, -164.4000000000000057 ) ) ;
#238918 = CARTESIAN_POINT ( 'NONE',  ( -15.51798037960204546, 66.62334006147904120, -185.8949149363071456 ) ) ;
#238919 = ORIENTED_EDGE ( 'NONE', *, *, #113697, .T. ) ;
#238920 = CARTESIAN_POINT ( 'NONE',  ( -20.85000000000000142, 87.75000000001172396, -69.52310748452423184 ) ) ;
#238921 = VERTEX_POINT ( 'NONE', #117354 ) ;
#238922 = AXIS2_PLACEMENT_3D ( 'NONE', #223841, #166487, #45221 ) ;
#238923 = CIRCLE ( 'NONE', #68035, 0.3999999999999975797 ) ;
#238924 = DIRECTION ( 'NONE',  ( 0.000000000000000000, 0.000000000000000000, 1.000000000000000000 ) ) ;
#238925 = ORIENTED_EDGE ( 'NONE', *, *, #7982, .F. ) ;
#238926 = DIRECTION ( 'NONE',  ( 0.000000000000000000, 0.9651348961777157509, -0.2617529984165031243 ) ) ;
#238927 = AXIS2_PLACEMENT_3D ( 'NONE', #168123, #188923, #29876 ) ;
#238928 = ORIENTED_EDGE ( 'NONE', *, *, #160265, .T. ) ;
#238929 = EDGE_CURVE ( 'NONE', #186437, #67087, #140346, .T. ) ;
#238930 = DIRECTION ( 'NONE',  ( 0.000000000000000000, -1.000000000000000000, -6.860497997771532351E-15 ) ) ;
#238931 = AXIS2_PLACEMENT_3D ( 'NONE', #114818, #53566, #194385 ) ;
#238932 = AXIS2_PLACEMENT_3D ( 'NONE', #198061, #22011, #101485 ) ;
#238933 = DIRECTION ( 'NONE',  ( -0.000000000000000000, 6.982962677686266711E-15, -1.000000000000000000 ) ) ;
#238934 = ORIENTED_EDGE ( 'NONE', *, *, #204216, .F. ) ;
#238935 = ADVANCED_FACE ( 'NONE', ( #156516 ), #152658, .F. ) ;
#238936 = ADVANCED_FACE ( 'NONE', ( #53524 ), #157807, .F. ) ;
#238937 = AXIS2_PLACEMENT_3D ( 'NONE', #106416, #185980, #107723 ) ;
#238938 = FACE_OUTER_BOUND ( 'NONE', #190565, .T. ) ;
#238939 = CARTESIAN_POINT ( 'NONE',  ( 21.87500000000000355, 22.61918030723623119, -230.9697045991730988 ) ) ;
#238941 = AXIS2_PLACEMENT_3D ( 'NONE', #255981, #57816, #156964 ) ;
#238940 = DIRECTION ( 'NONE',  ( -0.000000000000000000, 0.4721928772777345684, 0.8814952561688429444 ) ) ;
#238942 = EDGE_CURVE ( 'NONE', #167224, #99338, #244404, .T. ) ;
#238943 = ADVANCED_FACE ( 'NONE', ( #36569 ), #82071, .F. ) ;
#238944 = AXIS2_PLACEMENT_3D ( 'NONE', #92341, #96179, #115762 ) ;
#238945 = DIRECTION ( 'NONE',  ( 1.000000000000000000, 0.000000000000000000, 0.000000000000000000 ) ) ;
#238946 = CIRCLE ( 'NONE', #201503, 0.09999999999999817368 ) ;
#238947 = CARTESIAN_POINT ( 'NONE',  ( 12.25000000000000178, 62.53182050776835865, -217.4622410876596064 ) ) ;
#238948 = ADVANCED_FACE ( 'NONE', ( #173528 ), #194349, .F. ) ;
#238949 = ORIENTED_EDGE ( 'NONE', *, *, #215239, .F. ) ;
#238951 = ADVANCED_FACE ( 'NONE', ( #202027 ), #23418, .T. ) ;
#238950 = DIRECTION ( 'NONE',  ( 0.000000000000000000, 0.000000000000000000, 1.000000000000000000 ) ) ;
#238952 = EDGE_LOOP ( 'NONE', ( #63894, #58958, #77469, #233106 ) ) ;
#238954 = VERTEX_POINT ( 'NONE', #219006 ) ;
#238953 = LINE ( 'NONE', #103256, #35790 ) ;
#238955 = CIRCLE ( 'NONE', #109932, 0.1000000000000020595 ) ;
#238956 = EDGE_LOOP ( 'NONE', ( #154091, #171393, #72849, #126957 ) ) ;
#238957 = CARTESIAN_POINT ( 'NONE',  ( 18.52130828395271678, -9.481395502625792560, -7.024506723883644277 ) ) ;
#238958 = CARTESIAN_POINT ( 'NONE',  ( -18.59999999999999787, 11.75000000000000000, 6.000000000000001776 ) ) ;
#238959 = CARTESIAN_POINT ( 'NONE',  ( 12.25000000000000000, 66.65000000001258229, -186.7731074845244166 ) ) ;
#238960 = CARTESIAN_POINT ( 'NONE',  ( 21.09551895715285852, 60.18325881433904101, -221.2644573946620596 ) ) ;
#238961 = EDGE_CURVE ( 'NONE', #104084, #256760, #42952, .T. ) ;
#238962 = DIRECTION ( 'NONE',  ( 0.000000000000000000, -6.982962677686266711E-15, 1.000000000000000000 ) ) ;
#238963 = ORIENTED_EDGE ( 'NONE', *, *, #257460, .F. ) ;
#238964 = CARTESIAN_POINT ( 'NONE',  ( -16.81744102076749314, 9.950000000011142376, -146.6500000000000341 ) ) ;
#238966 = CARTESIAN_POINT ( 'NONE',  ( -16.83199030136657726, 66.06935196689877898, -157.2507064618668835 ) ) ;
#238965 = CIRCLE ( 'NONE', #209728, 0.09999999999999939493 ) ;
#238968 = ORIENTED_EDGE ( 'NONE', *, *, #120426, .F. ) ;
#238967 = DIRECTION ( 'NONE',  ( 0.000000000000000000, 0.000000000000000000, 1.000000000000000000 ) ) ;
#238969 = CARTESIAN_POINT ( 'NONE',  ( -33.72168855820452649, 62.50563584222673796, -209.4474707446456421 ) ) ;
#238970 = AXIS2_PLACEMENT_3D ( 'NONE', #141880, #183589, #184856 ) ;
#238971 = CARTESIAN_POINT ( 'NONE',  ( -16.87998658237754768, 9.950000000011137047, -79.86363956773804773 ) ) ;
#238972 = EDGE_LOOP ( 'NONE', ( #62443, #15304, #208258, #154832 ) ) ;
#238973 = TOROIDAL_SURFACE ( 'NONE', #105655, 11.70000000000000107, 0.1000000000000000056 ) ;
#238974 = VECTOR ( 'NONE', #30579, 1000.000000000000000 ) ;
#238975 = EDGE_CURVE ( 'NONE', #91128, #50799, #131985, .T. ) ;
#238976 = AXIS2_PLACEMENT_3D ( 'NONE', #137541, #41053, #16351 ) ;
#238977 = CARTESIAN_POINT ( 'NONE',  ( -21.14999999999999858, 87.65000000001235492, -167.1231074845242688 ) ) ;
#238978 = ORIENTED_EDGE ( 'NONE', *, *, #52839, .T. ) ;
#238979 = CARTESIAN_POINT ( 'NONE',  ( -17.29158576265544056, 10.36474766602906783, -178.9172417552077832 ) ) ;
#238980 = EDGE_CURVE ( 'NONE', #189217, #197646, #183748, .T. ) ;
#238981 = CARTESIAN_POINT ( 'NONE',  ( 21.05000000000000426, 6.258817194692633201, -133.9663672646664168 ) ) ;
#238982 = CARTESIAN_POINT ( 'NONE',  ( 20.94999999999999929, 85.00000000001251976, -179.9170766071767389 ) ) ;
#238983 = EDGE_CURVE ( 'NONE', #226125, #196796, #24046, .T. ) ;
#238984 = DIRECTION ( 'NONE',  ( 1.000000000000000000, 0.000000000000000000, 0.000000000000000000 ) ) ;
#238985 = CIRCLE ( 'NONE', #150927, 0.09999999999999520384 ) ;
#238986 = VECTOR ( 'NONE', #61641, 1000.000000000000114 ) ;
#238987 = AXIS2_PLACEMENT_3D ( 'NONE', #102352, #138907, #197630 ) ;
#238988 = CIRCLE ( 'NONE', #126559, 0.09999999999999939493 ) ;
#238989 = VERTEX_POINT ( 'NONE', #104185 ) ;
#238990 = CARTESIAN_POINT ( 'NONE',  ( -23.15000000000000213, 64.35000000001222986, -148.2731074845243882 ) ) ;
#238991 = ORIENTED_EDGE ( 'NONE', *, *, #97066, .F. ) ;
#238992 = CARTESIAN_POINT ( 'NONE',  ( -17.05016517655587904, 9.950000000007385381, -188.3273020040059293 ) ) ;
#238993 = DIRECTION ( 'NONE',  ( 0.000000000000000000, -0.2617529984165031243, -0.9651348961777157509 ) ) ;
#238996 = ORIENTED_EDGE ( 'NONE', *, *, #95931, .T. ) ;
#238995 = CARTESIAN_POINT ( 'NONE',  ( 22.88900146558018989, 67.29609520889979990, -194.2731074845244166 ) ) ;
#238994 =( BOUNDED_CURVE ( )  B_SPLINE_CURVE ( 3, ( #28974, #188006, #198888, #20268 ),
 .UNSPECIFIED., .F., .F. ) 
 B_SPLINE_CURVE_WITH_KNOTS ( ( 4, 4 ),
 ( 4.712388980384689674, 5.672655318024644622 ),
 .UNSPECIFIED. ) 
 CURVE ( )  GEOMETRIC_REPRESENTATION_ITEM ( )  RATIONAL_B_SPLINE_CURVE ( ( 1.000000000000000000, 0.9246222802177426203, 0.9246222802177426203, 1.000000000000000000 ) ) 
 REPRESENTATION_ITEM ( '' )  );
#238997 = CARTESIAN_POINT ( 'NONE',  ( -16.94445028196807002, 9.992063609708893068, -54.39266982158155628 ) ) ;
#238998 = CARTESIAN_POINT ( 'NONE',  ( 20.94999999999999574, 40.74071615341952679, -237.9411309446948337 ) ) ;
#238999 = DIRECTION ( 'NONE',  ( 0.000000000000000000, 0.000000000000000000, -1.000000000000000000 ) ) ;
#239000 = CARTESIAN_POINT ( 'NONE',  ( -16.80100426158790583, 9.943150520407293413, -79.68294575283408676 ) ) ;
#239001 = LINE ( 'NONE', #210150, #184803 ) ;
#239002 = DIRECTION ( 'NONE',  ( 0.000000000000000000, -0.2617529984165031243, -0.9651348961777157509 ) ) ;
#239004 = VERTEX_POINT ( 'NONE', #100325 ) ;
#239003 = CYLINDRICAL_SURFACE ( 'NONE', #190378, 11.80000000000000426 ) ;
#239005 = CARTESIAN_POINT ( 'NONE',  ( -18.69999999999999929, 6.726092018229619995, 9.512212474619552438 ) ) ;
#239006 = ORIENTED_EDGE ( 'NONE', *, *, #137930, .T. ) ;
#239007 = VERTEX_POINT ( 'NONE', #62517 ) ;
#239008 = CARTESIAN_POINT ( 'NONE',  ( -18.33682934331525161, 85.51118559110511796, -62.61745271585106565 ) ) ;
#239009 = CARTESIAN_POINT ( 'NONE',  ( -18.50000000000000000, 85.32100840337396619, -196.2871692354464415 ) ) ;
#239010 = VERTEX_POINT ( 'NONE', #160361 ) ;
#239011 = CARTESIAN_POINT ( 'NONE',  ( 21.72449340488910252, 10.28395627750227703, -113.1500000000000483 ) ) ;
#239012 = EDGE_CURVE ( 'NONE', #120723, #208327, #123996, .T. ) ;
#239013 = ADVANCED_FACE ( 'NONE', ( #1229 ), #239877, .F. ) ;
#239014 = VERTEX_POINT ( 'NONE', #164191 ) ;
#239015 = CIRCLE ( 'NONE', #59927, 7.800000000000001599 ) ;
#239016 = FACE_OUTER_BOUND ( 'NONE', #117348, .T. ) ;
#239017 = CIRCLE ( 'NONE', #134928, 0.09999999999999724387 ) ;
#239018 = DIRECTION ( 'NONE',  ( 0.000000000000000000, 0.9616958981405249185, -0.2741185865637160157 ) ) ;
#239019 = EDGE_CURVE ( 'NONE', #252190, #239900, #57322, .T. ) ;
#239020 = EDGE_LOOP ( 'NONE', ( #129926, #31791, #224701, #10700, #251567 ) ) ;
#239021 = ORIENTED_EDGE ( 'NONE', *, *, #231527, .T. ) ;
#239023 = EDGE_CURVE ( 'NONE', #205142, #19663, #83322, .T. ) ;
#239022 = CARTESIAN_POINT ( 'NONE',  ( -21.05000000000000071, -1.261786168553869603, -75.08649896354552311 ) ) ;
#239024 = ORIENTED_EDGE ( 'NONE', *, *, #119685, .F. ) ;
#239025 = FACE_OUTER_BOUND ( 'NONE', #157251, .T. ) ;
#239027 = VERTEX_POINT ( 'NONE', #139465 ) ;
#239026 = DIRECTION ( 'NONE',  ( 1.000000000000000000, 0.000000000000000000, 0.000000000000000000 ) ) ;
#239028 = DIRECTION ( 'NONE',  ( 1.000000000000000000, 0.000000000000000000, 0.000000000000000000 ) ) ;
#239029 = EDGE_LOOP ( 'NONE', ( #88924, #11554, #250297, #171359 ) ) ;
#239030 = DIRECTION ( 'NONE',  ( 0.000000000000000000, 0.000000000000000000, 1.000000000000000000 ) ) ;
#239031 = EDGE_LOOP ( 'NONE', ( #110078, #11911, #191852, #60588, #132704 ) ) ;
#239033 = ORIENTED_EDGE ( 'NONE', *, *, #249269, .F. ) ;
#239032 = EDGE_LOOP ( 'NONE', ( #81849, #20381, #118017, #203051, #92895 ) ) ;
#239035 = CARTESIAN_POINT ( 'NONE',  ( -16.27683809663750480, 13.59402435063957348, -219.4804627094287639 ) ) ;
#239034 = VECTOR ( 'NONE', #41770, 1000.000000000000000 ) ;
#239036 = ORIENTED_EDGE ( 'NONE', *, *, #192947, .F. ) ;
#239037 = ORIENTED_EDGE ( 'NONE', *, *, #137848, .F. ) ;
#239038 = TOROIDAL_SURFACE ( 'NONE', #84872, 12.97499999999999787, 0.1000000000000000056 ) ;
#239039 = ADVANCED_FACE ( 'NONE', ( #161637 ), #140528, .T. ) ;
#239040 = ADVANCED_FACE ( 'NONE', ( #181197 ), #123776, .F. ) ;
#239041 = AXIS2_PLACEMENT_3D ( 'NONE', #84346, #144345, #205618 ) ;
#239042 = AXIS2_PLACEMENT_3D ( 'NONE', #44052, #21931, #183568 ) ;
#239043 = VERTEX_POINT ( 'NONE', #178639 ) ;
#239044 = FACE_OUTER_BOUND ( 'NONE', #212728, .T. ) ;
#239045 = DIRECTION ( 'NONE',  ( -0.000000000000000000, 1.000000000000000000, 6.982962677686266711E-15 ) ) ;
#239047 = VERTEX_POINT ( 'NONE', #144595 ) ;
#239046 = LINE ( 'NONE', #99502, #115748 ) ;
#239048 = DIRECTION ( 'NONE',  ( -1.000000000000000000, -0.000000000000000000, -0.000000000000000000 ) ) ;
#239049 = VERTEX_POINT ( 'NONE', #224141 ) ;
#239050 = DIRECTION ( 'NONE',  ( 0.000000000000000000, 0.008583690987127625890, 0.9999631594459055250 ) ) ;
#239051 = CARTESIAN_POINT ( 'NONE',  ( 21.14999999999999503, 1.148907358139439339E-11, -201.0000000000015064 ) ) ;
#239052 = LINE ( 'NONE', #421, #97998 ) ;
#239053 = AXIS2_PLACEMENT_3D ( 'NONE', #120807, #4660, #67220 ) ;
#239054 = ORIENTED_EDGE ( 'NONE', *, *, #99353, .T. ) ;
#239055 = CIRCLE ( 'NONE', #172463, 0.09999999999999939493 ) ;
#239056 = DIRECTION ( 'NONE',  ( 0.000000000000000000, -1.000000000000000000, 0.000000000000000000 ) ) ;
#239058 = ADVANCED_FACE ( 'NONE', ( #125064 ), #99040, .T. ) ;
#239057 = CARTESIAN_POINT ( 'NONE',  ( -18.59999999999999787, 11.65000000001115232, -40.51480577065400013 ) ) ;
#239059 = DIRECTION ( 'NONE',  ( 0.5932847527679310229, -0.8049926720990042694, -6.366092712777067056E-16 ) ) ;
#239060 = AXIS2_PLACEMENT_3D ( 'NONE', #82103, #162974, #122560 ) ;
#239061 = ORIENTED_EDGE ( 'NONE', *, *, #171857, .F. ) ;
#239062 = EDGE_CURVE ( 'NONE', #202553, #62001, #161411, .T. ) ;
#239063 = DIRECTION ( 'NONE',  ( 0.000000000000000000, 0.2617529984164915779, 0.9651348961777189706 ) ) ;
#239064 = ORIENTED_EDGE ( 'NONE', *, *, #67467, .F. ) ;
#239065 = VECTOR ( 'NONE', #230011, 1000.000000000000000 ) ;
#239066 = ORIENTED_EDGE ( 'NONE', *, *, #244459, .T. ) ;
#239067 = CARTESIAN_POINT ( 'NONE',  ( 20.94999999999999929, 77.83534155023599510, -57.96795619196132776 ) ) ;
#239069 = ORIENTED_EDGE ( 'NONE', *, *, #211038, .F. ) ;
#239068 = AXIS2_PLACEMENT_3D ( 'NONE', #103459, #83871, #163460 ) ;
#239070 = ORIENTED_EDGE ( 'NONE', *, *, #11715, .F. ) ;
#239071 = CARTESIAN_POINT ( 'NONE',  ( -21.05000000000000071, 0.09779029131994770863, -127.7421853895239252 ) ) ;
#239072 = DIRECTION ( 'NONE',  ( 1.000000000000000000, -0.000000000000000000, -0.000000000000000000 ) ) ;
#239073 = ORIENTED_EDGE ( 'NONE', *, *, #78700, .T. ) ;
#239074 = VERTEX_POINT ( 'NONE', #61226 ) ;
#239075 = EDGE_CURVE ( 'NONE', #58126, #7171, #190641, .T. ) ;
#239076 = DIRECTION ( 'NONE',  ( 0.000000000000000000, 0.000000000000000000, 1.000000000000000000 ) ) ;
#239077 = CIRCLE ( 'NONE', #168387, 0.1000000000000002554 ) ;
#239078 = AXIS2_PLACEMENT_3D ( 'NONE', #22503, #186702, #220686 ) ;
#239079 = DIRECTION ( 'NONE',  ( 0.000000000000000000, 0.9770955615653317272, 0.2128009952263598126 ) ) ;
#239080 = EDGE_CURVE ( 'NONE', #249430, #21586, #106757, .T. ) ;
#239081 = CIRCLE ( 'NONE', #43444, 11.70000000000000284 ) ;
#239082 = VERTEX_POINT ( 'NONE', #186318 ) ;
#239083 = ORIENTED_EDGE ( 'NONE', *, *, #186340, .F. ) ;
#239084 = ADVANCED_FACE ( 'NONE', ( #49370 ), #126330, .F. ) ;
#239085 = VERTEX_POINT ( 'NONE', #147178 ) ;
#239086 =( BOUNDED_SURFACE ( )  B_SPLINE_SURFACE ( 3, 2, ( 
 ( #223476, #205194, #102216 ),
 ( #81373, #85227, #83926 ),
 ( #201357, #25313, #82659 ),
 ( #26598, #185653, #47406 ),
 ( #44857, #104789, #181799 ),
 ( #3135, #103522, #124403 ) ),
 .UNSPECIFIED., .F., .F., .F. ) 
 B_SPLINE_SURFACE_WITH_KNOTS ( ( 4, 2, 4 ),
 ( 3, 3 ),
 ( 0.0001300404313046710908, 0.0003183318589266773265, 0.0005066232865486835352 ),
 ( 0.000000000000000000, 1.000000000000000000 ),
 .UNSPECIFIED. ) 
 GEOMETRIC_REPRESENTATION_ITEM ( )  RATIONAL_B_SPLINE_SURFACE ( (
 ( 1.000000000000000000, 0.7071067811865352493, 1.000000000000000000),
 ( 1.000000000000000000, 0.7625113560539796831, 1.000000000000000000),
 ( 1.000000000000000000, 0.8126073484689130266, 1.000000000000000000),
 ( 1.000000000000000000, 0.8923049332731979311, 1.000000000000000000),
 ( 1.000000000000000000, 0.9231914937769916119, 1.000000000000000000),
 ( 1.000000000000000000, 0.9238795325112915124, 1.000000000000000000) ) ) 
 REPRESENTATION_ITEM ( '' )  SURFACE ( )  );
#239087 = CARTESIAN_POINT ( 'NONE',  ( 21.04999999999999716, 69.70076908992579945, -203.6215449845244052 ) ) ;
#239088 = CARTESIAN_POINT ( 'NONE',  ( 18.39999999999999858, 85.50000000001263345, -196.4910380878246201 ) ) ;
#239089 = EDGE_CURVE ( 'NONE', #104599, #18238, #177978, .T. ) ;
#239090 = DIRECTION ( 'NONE',  ( 0.000000000000000000, 1.000000000000000000, 6.938893903907222067E-15 ) ) ;
#239091 = CARTESIAN_POINT ( 'NONE',  ( 20.94999999999999929, -8.999999999988844479, -143.8939691226524644 ) ) ;
#239092 = LINE ( 'NONE', #82542, #66001 ) ;
#239093 = DIRECTION ( 'NONE',  ( 0.000000000000000000, 0.000000000000000000, -1.000000000000000000 ) ) ;
#239094 = ADVANCED_FACE ( 'NONE', ( #188880 ), #91060, .F. ) ;
#239095 = AXIS2_PLACEMENT_3D ( 'NONE', #100376, #118705, #177406 ) ;
#239097 = CARTESIAN_POINT ( 'NONE',  ( -20.94999999999999929, -1.849153571964891274, -145.6059666197970728 ) ) ;
#239096 = DIRECTION ( 'NONE',  ( -1.000000000000000000, 0.000000000000000000, 0.000000000000000000 ) ) ;
#239098 = CARTESIAN_POINT ( 'NONE',  ( 21.05000000000000071, 65.40605961984560679, -236.6728003091511425 ) ) ;
#239099 = CARTESIAN_POINT ( 'NONE',  ( -16.80891096016313924, 22.96249777872389330, -230.9267231593373424 ) ) ;
#239100 = CIRCLE ( 'NONE', #93335, 0.5000000000000004441 ) ;
#239101 = DIRECTION ( 'NONE',  ( 0.000000000000000000, 0.000000000000000000, -1.000000000000000000 ) ) ;
#239103 = DIRECTION ( 'NONE',  ( 1.000000000000000000, 0.000000000000000000, -0.000000000000000000 ) ) ;
#239102 = AXIS2_PLACEMENT_3D ( 'NONE', #75420, #55785, #154955 ) ;
#239104 = VERTEX_POINT ( 'NONE', #226705 ) ;
#239105 = VECTOR ( 'NONE', #20935, 1000.000000000000000 ) ;
#239106 = VECTOR ( 'NONE', #57248, 1000.000000000000227 ) ;
#239108 = ORIENTED_EDGE ( 'NONE', *, *, #25915, .T. ) ;
#239107 = DIRECTION ( 'NONE',  ( 4.239556034732057360E-17, 0.1298341882519953860, 0.9915357197604862671 ) ) ;
#239109 = DIRECTION ( 'NONE',  ( -0.000000000000000000, 7.272083257015735086E-15, -1.000000000000000000 ) ) ;
#239110 = DIRECTION ( 'NONE',  ( 0.000000000000000000, -0.2128009952263650861, 0.9770955615653305060 ) ) ;
#239111 = AXIS2_PLACEMENT_3D ( 'NONE', #192122, #31776, #132128 ) ;
#239112 = VERTEX_POINT ( 'NONE', #205865 ) ;
#239113 = TOROIDAL_SURFACE ( 'NONE', #47546, 0.2000000000000000111, 0.1000000000000000056 ) ;
#239114 = CIRCLE ( 'NONE', #1593, 0.5000000000000004441 ) ;
#239115 = DIRECTION ( 'NONE',  ( 0.000000000000000000, 6.982962677686266711E-15, -1.000000000000000000 ) ) ;
#239116 = AXIS2_PLACEMENT_3D ( 'NONE', #191364, #68833, #212196 ) ;
#239117 = CARTESIAN_POINT ( 'NONE',  ( -23.39999999999994529, 83.90000000001120384, -37.27310748452479316 ) ) ;
#239118 = EDGE_LOOP ( 'NONE', ( #145077, #155061, #218233, #6612, #59836, #130284 ) ) ;
#239119 = VECTOR ( 'NONE', #201511, 1000.000000000000227 ) ;
#239120 = CARTESIAN_POINT ( 'NONE',  ( -20.95613430942402644, 11.75000000001115552, -140.8571626482203101 ) ) ;
#239121 = CARTESIAN_POINT ( 'NONE',  ( -5.900000000000003020, -11.25000000000000000, 10.10000000000000142 ) ) ;
#239122 = DIRECTION ( 'NONE',  ( 0.000000000000000000, -0.9968797965484669232, -0.07893460099023190402 ) ) ;
#239124 = ORIENTED_EDGE ( 'NONE', *, *, #177611, .F. ) ;
#239123 = CARTESIAN_POINT ( 'NONE',  ( -20.94999999999999929, 64.35000000001195986, -109.8069731475024753 ) ) ;
#239125 = AXIS2_PLACEMENT_3D ( 'NONE', #116679, #37170, #219625 ) ;
#239127 = ORIENTED_EDGE ( 'NONE', *, *, #156789, .F. ) ;
#239126 = LINE ( 'NONE', #116607, #81276 ) ;
#239128 = SPHERICAL_SURFACE ( 'NONE', #4262, 0.1000000000000000056 ) ;
#239129 = DIRECTION ( 'NONE',  ( -0.000000000000000000, -0.000000000000000000, -1.000000000000000000 ) ) ;
#239130 = DIRECTION ( 'NONE',  ( -0.000000000000000000, -0.000000000000000000, -1.000000000000000000 ) ) ;
#239131 = CARTESIAN_POINT ( 'NONE',  ( -20.54999999999999361, 64.35000000001150511, -48.17310748452440095 ) ) ;
#239132 = CIRCLE ( 'NONE', #209932, 0.2000000000000005107 ) ;
#239134 = DIRECTION ( 'NONE',  ( -0.9880948137434723000, -0.1538461538461483591, -1.074301950413233512E-15 ) ) ;
#239133 = DIRECTION ( 'NONE',  ( -1.000000000000000000, 0.000000000000000000, 0.000000000000000000 ) ) ;
#239136 = EDGE_CURVE ( 'NONE', #160189, #229726, #68459, .T. ) ;
#239135 = CARTESIAN_POINT ( 'NONE',  ( -16.94333152886235894, 66.00965798856212530, -190.9151390155788306 ) ) ;
#239137 = DIRECTION ( 'NONE',  ( -1.000000000000000000, 0.000000000000000000, 0.000000000000000000 ) ) ;
#239138 = CARTESIAN_POINT ( 'NONE',  ( -18.59999999999999787, 69.01799029515544248, -99.32695536626806643 ) ) ;
#239139 = CARTESIAN_POINT ( 'NONE',  ( 20.84999999999999432, 7.021664781900089913, -37.33356540189728889 ) ) ;
#239140 = B_SPLINE_CURVE_WITH_KNOTS ( 'NONE', 3,
 ( #28515, #108007, #229247, #227952 ),
 .UNSPECIFIED., .F., .F.,
 ( 4, 4 ),
 ( 0.000000000000000000, 0.0001048066582182473756 ),
 .UNSPECIFIED. ) ;
#239141 = FACE_OUTER_BOUND ( 'NONE', #76182, .T. ) ;
#239142 = AXIS2_PLACEMENT_3D ( 'NONE', #252207, #115276, #31917 ) ;
#239144 = VERTEX_POINT ( 'NONE', #170651 ) ;
#239143 = AXIS2_PLACEMENT_3D ( 'NONE', #232330, #77075, #193197 ) ;
#239145 = CARTESIAN_POINT ( 'NONE',  ( 21.05000000000000426, 0.09843750001147434647, -94.20076908990776587 ) ) ;
#239146 = CIRCLE ( 'NONE', #101736, 11.74999999999999645 ) ;
#239147 = ORIENTED_EDGE ( 'NONE', *, *, #223944, .T. ) ;
#239148 = ORIENTED_EDGE ( 'NONE', *, *, #67282, .F. ) ;
#239149 = CARTESIAN_POINT ( 'NONE',  ( 23.24999999999999645, 1.115600667400684642E-11, -33.50000000000000000 ) ) ;
#239150 = ADVANCED_FACE ( 'NONE', ( #108063 ), #190173, .F. ) ;
#239151 = DIRECTION ( 'NONE',  ( 0.000000000000000000, -0.2617529984165031243, -0.9651348961777157509 ) ) ;
#239152 = ORIENTED_EDGE ( 'NONE', *, *, #141267, .T. ) ;
#239153 = EDGE_CURVE ( 'NONE', #26218, #185478, #90637, .T. ) ;
#239154 = EDGE_CURVE ( 'NONE', #160549, #53673, #208465, .T. ) ;
#239155 = ORIENTED_EDGE ( 'NONE', *, *, #177503, .T. ) ;
#239156 = SURFACE_STYLE_FILL_AREA ( #80036 ) ;
#239157 = ORIENTED_EDGE ( 'NONE', *, *, #254404, .T. ) ;
#239158 = AXIS2_PLACEMENT_3D ( 'NONE', #35482, #173729, #57556 ) ;
#239159 = VERTEX_POINT ( 'NONE', #151043 ) ;
#239160 = CARTESIAN_POINT ( 'NONE',  ( -20.54999999999999716, 68.85000000001200249, -115.3731074845243540 ) ) ;
#239161 = DIRECTION ( 'NONE',  ( -2.940209281316621016E-16, -1.000000000000000000, -5.880418562633242623E-15 ) ) ;
#239162 = DIRECTION ( 'NONE',  ( 0.000000000000000000, 0.2128009952263603399, -0.9770955615653315052 ) ) ;
#239163 = DIRECTION ( 'NONE',  ( 1.000000000000000000, 0.000000000000000000, 0.000000000000000000 ) ) ;
#239164 = EDGE_CURVE ( 'NONE', #64377, #196043, #52724, .T. ) ;
#239165 = FACE_OUTER_BOUND ( 'NONE', #190240, .T. ) ;
#239166 = EDGE_CURVE ( 'NONE', #212495, #70426, #105449, .T. ) ;
#239167 = DIRECTION ( 'NONE',  ( -1.000000000000000000, 0.000000000000000000, 0.000000000000000000 ) ) ;
#239169 = ORIENTED_EDGE ( 'NONE', *, *, #31655, .T. ) ;
#239168 = FACE_OUTER_BOUND ( 'NONE', #117672, .T. ) ;
#239171 = DIRECTION ( 'NONE',  ( 1.000000000000000000, 0.000000000000000000, 0.000000000000000000 ) ) ;
#239170 = CARTESIAN_POINT ( 'NONE',  ( -16.86133551771148831, 66.05000000001224691, -149.2217640499777929 ) ) ;
#239172 = CARTESIAN_POINT ( 'NONE',  ( 20.99999999999997868, 76.00000000001213607, -136.5231074845242745 ) ) ;
#239173 = ORIENTED_EDGE ( 'NONE', *, *, #23579, .T. ) ;
#239174 = DIRECTION ( 'NONE',  ( -1.836970198721029934E-16, -1.000000000000000000, -6.982962677686266711E-15 ) ) ;
#239175 = CARTESIAN_POINT ( 'NONE',  ( -20.64999999999999858, 68.85000000001259934, -191.2731074845244166 ) ) ;
#239176 = VERTEX_POINT ( 'NONE', #88462 ) ;
#239178 = CARTESIAN_POINT ( 'NONE',  ( 23.15000000000000213, 82.09643798151613225, -215.4278993322501208 ) ) ;
#239177 = CARTESIAN_POINT ( 'NONE',  ( 21.05000000000000071, 85.00000000001159606, -59.62913836187181715 ) ) ;
#239179 = CARTESIAN_POINT ( 'NONE',  ( 18.49999999999999289, 10.49142135624846439, -58.35000000000000142 ) ) ;
#239180 = CARTESIAN_POINT ( 'NONE',  ( 22.49999999999999645, 64.35042919246686210, -69.62310748452439668 ) ) ;
#239181 = ORIENTED_EDGE ( 'NONE', *, *, #216524, .T. ) ;
#239182 = SURFACE_STYLE_FILL_AREA ( #100905 ) ;
#239183 = CARTESIAN_POINT ( 'NONE',  ( -20.54999999999999716, 76.00000000001190870, -103.0231074845243029 ) ) ;
#239184 = EDGE_CURVE ( 'NONE', #116019, #139309, #244994, .T. ) ;
#239185 = CARTESIAN_POINT ( 'NONE',  ( -22.60000000000080433, 0.04781698047652392647, -55.24997756884729938 ) ) ;
#239186 = DIRECTION ( 'NONE',  ( 0.000000000000000000, 0.9651348961777148627, -0.2617529984165062329 ) ) ;
#239187 = DIRECTION ( 'NONE',  ( -0.000000000000000000, 0.000000000000000000, -1.000000000000000000 ) ) ;
#239188 = ORIENTED_EDGE ( 'NONE', *, *, #142649, .F. ) ;
#239189 = DIRECTION ( 'NONE',  ( 0.000000000000000000, 0.000000000000000000, 1.000000000000000000 ) ) ;
#239190 = EDGE_CURVE ( 'NONE', #35121, #25637, #219643, .T. ) ;
#239191 = PLANE ( 'NONE',  #123434 ) ;
#239192 = DIRECTION ( 'NONE',  ( 5.603264701231745086E-32, 7.172728831056619538E-15, -1.000000000000000000 ) ) ;
#239193 = DIRECTION ( 'NONE',  ( 1.000000000000000000, 0.000000000000000000, 0.000000000000000000 ) ) ;
#239194 = AXIS2_PLACEMENT_3D ( 'NONE', #85690, #218811, #179715 ) ;
#239195 = DIRECTION ( 'NONE',  ( 0.000000000000000000, 0.2128009952263604232, -0.9770955615653316162 ) ) ;
#239196 = AXIS2_PLACEMENT_3D ( 'NONE', #148176, #223849, #165180 ) ;
#239197 = CARTESIAN_POINT ( 'NONE',  ( -23.15000000000000213, 27.82649702422227733, -239.8850763025288870 ) ) ;
#239198 = TOROIDAL_SURFACE ( 'NONE', #89339, 0.2000000000000000111, 0.1000000000000000056 ) ;
#239199 = VECTOR ( 'NONE', #204465, 1000.000000000000000 ) ;
#239201 = ORIENTED_EDGE ( 'NONE', *, *, #201735, .F. ) ;
#239200 = CARTESIAN_POINT ( 'NONE',  ( 23.15000000000000213, -11.64999999998883595, -130.9000000000000341 ) ) ;
#239202 = DIRECTION ( 'NONE',  ( -1.000000000000000000, 0.000000000000000000, 0.000000000000000000 ) ) ;
#239203 = DIRECTION ( 'NONE',  ( 0.000000000000000000, 0.000000000000000000, -1.000000000000000000 ) ) ;
#239204 = CARTESIAN_POINT ( 'NONE',  ( 18.47149038651510367, 77.27495776109610404, -241.9532892334652274 ) ) ;
#239205 = CARTESIAN_POINT ( 'NONE',  ( -5.899999999999938183, 64.65000000001120384, -22.02310748452479316 ) ) ;
#239206 = CARTESIAN_POINT ( 'NONE',  ( 21.05000000000000071, 85.50000000001207923, -126.6291383618717816 ) ) ;
#239208 = ORIENTED_EDGE ( 'NONE', *, *, #58431, .F. ) ;
#239207 = CARTESIAN_POINT ( 'NONE',  ( 21.06600267594171783, 67.22483393081165559, -57.31884470214964722 ) ) ;
#239209 = CARTESIAN_POINT ( 'NONE',  ( -17.11825945287482753, 65.95000000001230944, -157.2731074845244166 ) ) ;
#239210 = CARTESIAN_POINT ( 'NONE',  ( 21.05000000000000071, 77.36087058720467269, -195.4501095574333931 ) ) ;
#239211 = CARTESIAN_POINT ( 'NONE',  ( 18.49999999999999645, -1.299733671219632791, -57.02812952286944892 ) ) ;
#239212 = ORIENTED_EDGE ( 'NONE', *, *, #95844, .T. ) ;
#239213 = DIRECTION ( 'NONE',  ( 0.000000000000000000, 0.1180230956474139226, -0.9930108503404186937 ) ) ;
#239214 = DIRECTION ( 'NONE',  ( 0.000000000000000000, 1.000000000000000000, 7.272083257015735086E-15 ) ) ;
#239215 = ADVANCED_FACE ( 'NONE', ( #46778 ), #82252, .T. ) ;
#239216 = SPHERICAL_SURFACE ( 'NONE', #112738, 0.1000000000000000056 ) ;
#239217 = DIRECTION ( 'NONE',  ( 0.000000000000000000, 0.1298341882520022694, 0.9915357197604852679 ) ) ;
#239218 = CIRCLE ( 'NONE', #60141, 0.09999999999998898659 ) ;
#239219 = DIRECTION ( 'NONE',  ( 1.000000000000000000, 0.000000000000000000, 0.000000000000000000 ) ) ;
#239221 = ORIENTED_EDGE ( 'NONE', *, *, #209042, .F. ) ;
#239220 = TOROIDAL_SURFACE ( 'NONE', #218350, 0.6000000000000013101, 0.1000000000000000056 ) ;
#239222 = ORIENTED_EDGE ( 'NONE', *, *, #227686, .F. ) ;
#239223 = VECTOR ( 'NONE', #136386, 1000.000000000000000 ) ;
#239224 = ADVANCED_FACE ( 'NONE', ( #148474 ), #228035, .F. ) ;
#239225 = FACE_OUTER_BOUND ( 'NONE', #137558, .T. ) ;
#239227 = EDGE_CURVE ( 'NONE', #176943, #212760, #173218, .T. ) ;
#239226 = CARTESIAN_POINT ( 'NONE',  ( -20.54999999999999716, 66.26558728512915764, -222.7970849955717938 ) ) ;
#239228 = CARTESIAN_POINT ( 'NONE',  ( -12.25000000000000178, 66.65000000001258229, -186.7731074845244166 ) ) ;
#239229 = DIRECTION ( 'NONE',  ( 0.000000000000000000, 0.2128009952263601456, -0.9770955615653316162 ) ) ;
#239230 = VERTEX_POINT ( 'NONE', #134025 ) ;
#239231 = EDGE_CURVE ( 'NONE', #235594, #59416, #130303, .T. ) ;
#239232 = EDGE_CURVE ( 'NONE', #14142, #174088, #232147, .T. ) ;
#239233 = CARTESIAN_POINT ( 'NONE',  ( 20.95420533658165141, 10.54586447477073285, -175.0675060206932017 ) ) ;
#239234 = CIRCLE ( 'NONE', #255761, 0.09999999999998898659 ) ;
#239235 = VECTOR ( 'NONE', #42994, 1000.000000000000000 ) ;
#239236 = CARTESIAN_POINT ( 'NONE',  ( 20.77526135991748291, 10.52954618004883613, -207.3738603278011681 ) ) ;
#239237 = CIRCLE ( 'NONE', #251712, 0.1999999999999905742 ) ;
#239238 = EDGE_CURVE ( 'NONE', #14935, #105944, #17927, .T. ) ;
#239239 = CARTESIAN_POINT ( 'NONE',  ( 22.50000000000000000, 67.23127455305841238, -235.8551265064783991 ) ) ;
#239240 = CARTESIAN_POINT ( 'NONE',  ( 21.05000000000000071, 1.115600667400684642E-11, -67.00000000000000000 ) ) ;
#239241 = VECTOR ( 'NONE', #33684, 1000.000000000000227 ) ;
#239242 = FACE_OUTER_BOUND ( 'NONE', #151436, .T. ) ;
#239243 = EDGE_CURVE ( 'NONE', #11085, #256624, #186352, .T. ) ;
#239245 = EDGE_CURVE ( 'NONE', #121900, #41312, #256485, .T. ) ;
#239244 = ADVANCED_FACE ( 'NONE', ( #92338 ), #213563, .T. ) ;
#239246 = ORIENTED_EDGE ( 'NONE', *, *, #112527, .F. ) ;
#239248 = VERTEX_POINT ( 'NONE', #212309 ) ;
#239247 = DIRECTION ( 'NONE',  ( 1.000000000000000000, 3.265361837132813093E-16, -0.000000000000000000 ) ) ;
#239249 = TOROIDAL_SURFACE ( 'NONE', #176718, 0.4000000000000012990, 0.1000000000000000056 ) ;
#239250 = EDGE_LOOP ( 'NONE', ( #217993, #221715, #122920, #117451, #67422, #83950 ) ) ;
#239251 = CARTESIAN_POINT ( 'NONE',  ( 23.14999999999999858, 5.600000000011153389, -54.59473398108690390 ) ) ;
#239252 = EDGE_LOOP ( 'NONE', ( #65761, #217098, #234424, #230795 ) ) ;
#239253 = CARTESIAN_POINT ( 'NONE',  ( -21.05000000000000071, -0.01465611850188162056, -27.00331341423204279 ) ) ;
#239254 = CARTESIAN_POINT ( 'NONE',  ( 18.39999999999999858, -9.499999999988842703, -174.5320693966996259 ) ) ;
#239255 = DIRECTION ( 'NONE',  ( 0.000000000000000000, 0.8814952561688437216, -0.4721928772777334582 ) ) ;
#239256 = VERTEX_POINT ( 'NONE', #57032 ) ;
#239257 = TOROIDAL_SURFACE ( 'NONE', #126827, 0.2000000000000000111, 0.1000000000000000056 ) ;
#239258 = DIRECTION ( 'NONE',  ( 0.000000000000000000, -1.000000000000000000, 0.000000000000000000 ) ) ;
#239259 = AXIS2_PLACEMENT_3D ( 'NONE', #102971, #5137, #44312 ) ;
#239260 = EDGE_LOOP ( 'NONE', ( #63094, #51353, #40359, #199451 ) ) ;
#239261 = CARTESIAN_POINT ( 'NONE',  ( 22.59066674512249762, 11.75000000001115552, -100.4694958763694217 ) ) ;
#239262 = EDGE_CURVE ( 'NONE', #223255, #156135, #69829, .T. ) ;
#239264 = ORIENTED_EDGE ( 'NONE', *, *, #107403, .T. ) ;
#239263 = DIRECTION ( 'NONE',  ( 0.000000000000000000, -6.982962677686266711E-15, 1.000000000000000000 ) ) ;
#239265 = DIRECTION ( 'NONE',  ( 0.000000000000000000, 0.000000000000000000, 1.000000000000000000 ) ) ;
#239266 = CARTESIAN_POINT ( 'NONE',  ( 20.04142135623730070, 64.35000000001197407, -111.8731074845243825 ) ) ;
#239267 = ADVANCED_FACE ( 'NONE', ( #191478 ), #236404, .T. ) ;
#239268 = EDGE_CURVE ( 'NONE', #110564, #221229, #248890, .T. ) ;
#239269 = ORIENTED_EDGE ( 'NONE', *, *, #212642, .T. ) ;
#239270 = PLANE ( 'NONE',  #43573 ) ;
#239272 = EDGE_CURVE ( 'NONE', #246315, #163980, #178165, .T. ) ;
#239271 = CARTESIAN_POINT ( 'NONE',  ( 23.14999999999999503, 62.92003201576280702, -207.2439188921395612 ) ) ;
#239273 = FACE_OUTER_BOUND ( 'NONE', #7400, .T. ) ;
#239274 = EDGE_LOOP ( 'NONE', ( #188629, #178249, #187962, #104055 ) ) ;
#239275 = CARTESIAN_POINT ( 'NONE',  ( 22.50497660315937765, 76.07871793023797125, -181.7729029894197481 ) ) ;
#239276 = LINE ( 'NONE', #141447, #97405 ) ;
#239277 = DIRECTION ( 'NONE',  ( 1.000000000000000000, -1.836970198721029934E-16, -1.282749433769087582E-30 ) ) ;
#239278 = ADVANCED_FACE ( 'NONE', ( #53218 ), #114472, .T. ) ;
#239279 = AXIS2_PLACEMENT_3D ( 'NONE', #246337, #132819, #212361 ) ;
#239280 = ORIENTED_EDGE ( 'NONE', *, *, #150744, .F. ) ;
#239281 = VECTOR ( 'NONE', #147278, 1000.000000000000000 ) ;
#239282 = VECTOR ( 'NONE', #53934, 1000.000000000000000 ) ;
#239283 = ORIENTED_EDGE ( 'NONE', *, *, #41756, .F. ) ;
#239284 = CIRCLE ( 'NONE', #118499, 0.09999999999999982514 ) ;
#239285 = AXIS2_PLACEMENT_3D ( 'NONE', #245873, #106329, #146736 ) ;
#239286 = ORIENTED_EDGE ( 'NONE', *, *, #194858, .F. ) ;
#239287 = CARTESIAN_POINT ( 'NONE',  ( -16.87036670365548474, 9.989418819312801290, -87.97956011730209980 ) ) ;
#239288 = PLANE ( 'NONE',  #125366 ) ;
#239290 = VERTEX_POINT ( 'NONE', #94897 ) ;
#239289 = DIRECTION ( 'NONE',  ( 0.000000000000000000, 0.000000000000000000, -1.000000000000000000 ) ) ;
#239291 = DIRECTION ( 'NONE',  ( -1.000000000000000000, 0.000000000000000000, 0.000000000000000000 ) ) ;
#239292 = CARTESIAN_POINT ( 'NONE',  ( 23.15000000000000213, 87.75000000001205080, -124.2731074845242176 ) ) ;
#239293 = DIRECTION ( 'NONE',  ( -1.000000000000000000, 2.952720810173289112E-16, 2.061873921506763405E-30 ) ) ;
#239294 = LINE ( 'NONE', #60631, #135205 ) ;
#239295 = CARTESIAN_POINT ( 'NONE',  ( -21.05000000000000071, -11.64999999999999858, -30.59999999999999432 ) ) ;
#239296 = AXIS2_PLACEMENT_3D ( 'NONE', #4642, #248415, #208021 ) ;
#239297 = DIRECTION ( 'NONE',  ( -1.000000000000000000, -1.394253735153569469E-16, -2.602809386958778209E-16 ) ) ;
#239298 = TOROIDAL_SURFACE ( 'NONE', #214178, 12.97499999999999787, 0.1000000000000000056 ) ;
#239300 = ORIENTED_EDGE ( 'NONE', *, *, #167423, .T. ) ;
#239299 = CARTESIAN_POINT ( 'NONE',  ( -16.94107738177414291, 65.98576071487592287, -182.5731074845244279 ) ) ;
#239302 = ORIENTED_EDGE ( 'NONE', *, *, #245343, .F. ) ;
#239301 = DIRECTION ( 'NONE',  ( 1.000000000000000000, 0.000000000000000000, 0.000000000000000000 ) ) ;
#239303 = CYLINDRICAL_SURFACE ( 'NONE', #91346, 0.9000000000000014655 ) ;
#239304 = VECTOR ( 'NONE', #63055, 1000.000000000000000 ) ;
#239305 = ORIENTED_EDGE ( 'NONE', *, *, #173448, .T. ) ;
#239306 = ORIENTED_EDGE ( 'NONE', *, *, #80030, .T. ) ;
#239307 = DIRECTION ( 'NONE',  ( 1.000000000000000000, 0.000000000000000000, 0.000000000000000000 ) ) ;
#239308 = DIRECTION ( 'NONE',  ( -1.000000000000000000, -0.000000000000000000, -0.000000000000000000 ) ) ;
#239309 = B_SPLINE_CURVE_WITH_KNOTS ( 'NONE', 3,
 ( #257060, #160614, #101865, #78461, #61486, #220559 ),
 .UNSPECIFIED., .F., .F.,
 ( 4, 2, 4 ),
 ( 0.000000000000000000, 0.0001497467027049212147, 0.0002994934054098424294 ),
 .UNSPECIFIED. ) ;
#239310 = CARTESIAN_POINT ( 'NONE',  ( -22.49231231312463208, 64.35001509633467265, -103.0841603721257513 ) ) ;
#239311 = CARTESIAN_POINT ( 'NONE',  ( -21.44999999999999929, 68.65000000001261071, -191.1731074845243938 ) ) ;
#239312 = DIRECTION ( 'NONE',  ( -0.000000000000000000, -0.2128009952263607285, 0.9770955615653316162 ) ) ;
#239313 = VECTOR ( 'NONE', #227338, 1000.000000000000000 ) ;
#239314 = DIRECTION ( 'NONE',  ( -0.000000000000000000, 0.03181660087583042251, -0.9994937237965568766 ) ) ;
#239315 = DIRECTION ( 'NONE',  ( 2.952720810173289112E-16, 1.000000000000000000, 1.261617073437673512E-14 ) ) ;
#239317 = VERTEX_POINT ( 'NONE', #15391 ) ;
#239316 = ADVANCED_FACE ( 'NONE', ( #93628 ), #136410, .T. ) ;
#239318 = ORIENTED_EDGE ( 'NONE', *, *, #223158, .F. ) ;
#239319 = ADVANCED_FACE ( 'NONE', ( #100007 ), #103866, .F. ) ;
#239320 = ORIENTED_EDGE ( 'NONE', *, *, #7108, .T. ) ;
#239321 = DIRECTION ( 'NONE',  ( -3.440080580676165237E-14, 0.08413937888703756918, -0.9964539953858901900 ) ) ;
#239323 = CIRCLE ( 'NONE', #193541, 0.09999999999999990841 ) ;
#239322 = DIRECTION ( 'NONE',  ( -0.000000000000000000, 6.982962677686266711E-15, -1.000000000000000000 ) ) ;
#239324 = AXIS2_PLACEMENT_3D ( 'NONE', #79015, #157337, #59441 ) ;
#239325 = CARTESIAN_POINT ( 'NONE',  ( -14.56556274378147720, 66.55344247693902560, -54.43316553017852044 ) ) ;
#239326 = CIRCLE ( 'NONE', #231164, 0.1000000000000118433 ) ;
#239327 = FACE_OUTER_BOUND ( 'NONE', #195437, .T. ) ;
#239328 = EDGE_CURVE ( 'NONE', #150150, #90293, #40105, .T. ) ;
#239329 = EDGE_LOOP ( 'NONE', ( #195980, #250326, #162300, #90202 ) ) ;
#239331 = EDGE_CURVE ( 'NONE', #224326, #25296, #238260, .T. ) ;
#239330 = CARTESIAN_POINT ( 'NONE',  ( -16.93211319090181632, 66.00001321885476102, -149.1006019852513589 ) ) ;
#239332 = EDGE_LOOP ( 'NONE', ( #29265, #163119, #68465, #31245 ) ) ;
#239333 = FACE_OUTER_BOUND ( 'NONE', #159327, .T. ) ;
#239334 = VERTEX_POINT ( 'NONE', #19224 ) ;
#239335 = DIRECTION ( 'NONE',  ( -0.000000000000000000, 0.000000000000000000, 1.000000000000000000 ) ) ;
#239336 = CARTESIAN_POINT ( 'NONE',  ( 15.52844286134408236, 9.375669526436931633, -183.3677900093859989 ) ) ;
#239337 = ORIENTED_EDGE ( 'NONE', *, *, #101380, .T. ) ;
#239338 = DIRECTION ( 'NONE',  ( -0.000000000000000000, 0.9126074666063770380, 0.4088369013363281068 ) ) ;
#239340 = ORIENTED_EDGE ( 'NONE', *, *, #65461, .F. ) ;
#239339 = DIRECTION ( 'NONE',  ( 1.000000000000000000, 0.000000000000000000, 0.000000000000000000 ) ) ;
#239341 = DIRECTION ( 'NONE',  ( 1.000000000000000000, 0.000000000000000000, 0.000000000000000000 ) ) ;
#239342 = AXIS2_PLACEMENT_3D ( 'NONE', #241366, #80973, #178847 ) ;
#239343 = ORIENTED_EDGE ( 'NONE', *, *, #67009, .F. ) ;
#239344 = EDGE_CURVE ( 'NONE', #61020, #135788, #86534, .T. ) ;
#239345 = EDGE_CURVE ( 'NONE', #103624, #162117, #90134, .T. ) ;
#239346 = CIRCLE ( 'NONE', #60276, 0.09999999999999939493 ) ;
#239347 = DIRECTION ( 'NONE',  ( 0.000000000000000000, 0.000000000000000000, -1.000000000000000000 ) ) ;
#239348 = ORIENTED_EDGE ( 'NONE', *, *, #162189, .T. ) ;
#239349 = DIRECTION ( 'NONE',  ( 1.000000000000000000, 2.952720810173289112E-16, -0.000000000000000000 ) ) ;
#239350 = DIRECTION ( 'NONE',  ( 0.000000000000000000, 0.000000000000000000, 1.000000000000000000 ) ) ;
#239351 = CARTESIAN_POINT ( 'NONE',  ( 20.94999999999999929, 85.00000000001197975, -112.5170766071766764 ) ) ;
#239352 = CARTESIAN_POINT ( 'NONE',  ( -16.87036670365548474, 9.989418819312801290, -121.4795601173020856 ) ) ;
#239353 = CARTESIAN_POINT ( 'NONE',  ( 20.94999999999999929, 76.00000000001172396, -71.52310748452431710 ) ) ;
#239354 = ORIENTED_EDGE ( 'NONE', *, *, #104950, .T. ) ;
#239356 = ADVANCED_FACE ( 'NONE', ( #102576 ), #200429, .F. ) ;
#239355 = DIRECTION ( 'NONE',  ( -1.000000000000000000, 0.000000000000000000, 0.000000000000000000 ) ) ;
#239357 = CARTESIAN_POINT ( 'NONE',  ( -17.71734398241073905, 41.60308423793308918, -235.4556039006346850 ) ) ;
#239358 = FACE_OUTER_BOUND ( 'NONE', #214970, .T. ) ;
#239359 = EDGE_LOOP ( 'NONE', ( #139732, #200772, #234779, #128850 ) ) ;
#239360 = ADVANCED_FACE ( 'NONE', ( #60905 ), #219985, .F. ) ;
#239361 = CARTESIAN_POINT ( 'NONE',  ( 20.94999027547553894, 68.00519115550238780, -224.2294631537215821 ) ) ;
#239362 = ORIENTED_EDGE ( 'NONE', *, *, #101465, .F. ) ;
#239363 = CARTESIAN_POINT ( 'NONE',  ( 23.24999999999999289, 6.450000000000001066, -12.35000000000000320 ) ) ;
#239364 = ORIENTED_EDGE ( 'NONE', *, *, #24328, .T. ) ;
#239365 = AXIS2_PLACEMENT_3D ( 'NONE', #146977, #105261, #226506 ) ;
#239366 = CIRCLE ( 'NONE', #126941, 0.09999999999998898659 ) ;
#239367 = CARTESIAN_POINT ( 'NONE',  ( -21.17356465864818560, 69.57719687377097273, -203.6220187255382541 ) ) ;
#239368 = CARTESIAN_POINT ( 'NONE',  ( -16.94107738177413225, 65.98576071487593708, -182.5731074845244564 ) ) ;
#239369 = VERTEX_POINT ( 'NONE', #182157 ) ;
#239371 = ORIENTED_EDGE ( 'NONE', *, *, #132784, .T. ) ;
#239370 = DIRECTION ( 'NONE',  ( -1.000000000000000000, 0.000000000000000000, 0.000000000000000000 ) ) ;
#239372 = CARTESIAN_POINT ( 'NONE',  ( -21.14999999999994174, 83.80000000001119531, -51.02310748452479316 ) ) ;
#239373 = ORIENTED_EDGE ( 'NONE', *, *, #167040, .T. ) ;
#239374 = EDGE_CURVE ( 'NONE', #210631, #84318, #111683, .T. ) ;
#239375 = DIRECTION ( 'NONE',  ( -1.000000000000000000, 1.836970198721029934E-16, 1.601412966608202925E-30 ) ) ;
#239376 = DIRECTION ( 'NONE',  ( 0.000000000000000000, 0.3896596508880098009, 0.9209589331071361684 ) ) ;
#239377 = EDGE_CURVE ( 'NONE', #168523, #149398, #74128, .T. ) ;
#239378 = ORIENTED_EDGE ( 'NONE', *, *, #42080, .F. ) ;
#239379 = ORIENTED_EDGE ( 'NONE', *, *, #47004, .F. ) ;
#239380 = PLANE ( 'NONE',  #193261 ) ;
#239381 = CARTESIAN_POINT ( 'NONE',  ( 21.05000000000000071, 76.03753606329841830, -209.8553797584600602 ) ) ;
#239382 = VERTEX_POINT ( 'NONE', #158762 ) ;
#239384 = DIRECTION ( 'NONE',  ( -0.000000000000000000, 0.8660254037844411501, 0.4999999999999956701 ) ) ;
#239383 = CIRCLE ( 'NONE', #156207, 0.1000000000000028644 ) ;
#239385 = EDGE_CURVE ( 'NONE', #81676, #211434, #28337, .T. ) ;
#239386 = VECTOR ( 'NONE', #82421, 1000.000000000000000 ) ;
#239387 = VERTEX_POINT ( 'NONE', #62206 ) ;
#239388 = ORIENTED_EDGE ( 'NONE', *, *, #41505, .F. ) ;
#239389 = CIRCLE ( 'NONE', #143705, 0.1000000000000028644 ) ;
#239390 = CIRCLE ( 'NONE', #51923, 0.6000000000000033085 ) ;
#239391 = EDGE_CURVE ( 'NONE', #91171, #207624, #142992, .T. ) ;
#239392 = CARTESIAN_POINT ( 'NONE',  ( 21.14999999999999858, -0.09999999998884338825, -88.85042919245522341 ) ) ;
#239393 =( GEOMETRIC_REPRESENTATION_CONTEXT ( 3 ) GLOBAL_UNCERTAINTY_ASSIGNED_CONTEXT ( ( #193744 ) ) GLOBAL_UNIT_ASSIGNED_CONTEXT ( ( #47303, #246803, #29099 ) ) REPRESENTATION_CONTEXT ( 'NONE', 'WORKASPACE' ) );
#239394 = ADVANCED_FACE ( 'NONE', ( #4762 ), #253145, .F. ) ;
#239396 = ORIENTED_EDGE ( 'NONE', *, *, #75077, .F. ) ;
#239395 = DIRECTION ( 'NONE',  ( 1.000000000000000000, -0.000000000000000000, -0.000000000000000000 ) ) ;
#239397 = DIRECTION ( 'NONE',  ( -1.000000000000000000, 0.000000000000000000, 0.000000000000000000 ) ) ;
#239398 = DIRECTION ( 'NONE',  ( 1.000000000000000000, 0.000000000000000000, 0.000000000000000000 ) ) ;
#239399 = CARTESIAN_POINT ( 'NONE',  ( -16.77683809663752257, 63.08610022504904435, -213.1421742787362064 ) ) ;
#239400 = EDGE_CURVE ( 'NONE', #7699, #108752, #163876, .T. ) ;
#239402 = CARTESIAN_POINT ( 'NONE',  ( 21.05000000000000071, 1.115600667400684642E-11, -45.65000000000000568 ) ) ;
#239401 = FACE_OUTER_BOUND ( 'NONE', #86905, .T. ) ;
#239403 = CARTESIAN_POINT ( 'NONE',  ( -21.05000000000000071, 76.09999996531173849, -143.0006596670174019 ) ) ;
#239404 = LINE ( 'NONE', #156033, #69322 ) ;
#239405 = DIRECTION ( 'NONE',  ( 0.000000000000000000, -0.9126074666063769270, -0.4088369013363280513 ) ) ;
#239406 = DIRECTION ( 'NONE',  ( 1.000000000000000000, 0.000000000000000000, 0.000000000000000000 ) ) ;
#239407 = CIRCLE ( 'NONE', #51938, 1.749999999999999778 ) ;
#239408 = EDGE_LOOP ( 'NONE', ( #224105, #210206, #100551, #224461 ) ) ;
#239409 = AXIS2_PLACEMENT_3D ( 'NONE', #75827, #58800, #256974 ) ;
#239410 = AXIS2_PLACEMENT_3D ( 'NONE', #111946, #72831, #54513 ) ;
#239411 = ORIENTED_EDGE ( 'NONE', *, *, #3589, .T. ) ;
#239412 = VERTEX_POINT ( 'NONE', #94277 ) ;
#239413 = EDGE_CURVE ( 'NONE', #239014, #8107, #224110, .T. ) ;
#239414 = FACE_OUTER_BOUND ( 'NONE', #175900, .T. ) ;
#239415 = ORIENTED_EDGE ( 'NONE', *, *, #203386, .T. ) ;
#239416 = CARTESIAN_POINT ( 'NONE',  ( -21.14999999999994174, 65.15000000001120384, -3.023107484524792277 ) ) ;
#239417 = DIRECTION ( 'NONE',  ( -1.000000000000000000, -0.000000000000000000, -0.000000000000000000 ) ) ;
#239418 = AXIS2_PLACEMENT_3D ( 'NONE', #208485, #29855, #36267 ) ;
#239419 = CIRCLE ( 'NONE', #197706, 0.09999999999999939493 ) ;
#239420 = VERTEX_POINT ( 'NONE', #229943 ) ;
#239421 = VECTOR ( 'NONE', #231000, 1000.000000000000000 ) ;
#239422 = LINE ( 'NONE', #213420, #69903 ) ;
#239423 = VECTOR ( 'NONE', #257063, 1000.000000000000000 ) ;
#239425 = ORIENTED_EDGE ( 'NONE', *, *, #105400, .T. ) ;
#239424 = ORIENTED_EDGE ( 'NONE', *, *, #82500, .F. ) ;
#239426 = EDGE_LOOP ( 'NONE', ( #185507, #244540, #202170, #92169 ) ) ;
#239427 = VERTEX_POINT ( 'NONE', #212954 ) ;
#239429 = DIRECTION ( 'NONE',  ( -1.000000000000000000, 0.000000000000000000, 0.000000000000000000 ) ) ;
#239428 = AXIS2_PLACEMENT_3D ( 'NONE', #103661, #21601, #223613 ) ;
#239430 = CARTESIAN_POINT ( 'NONE',  ( -21.10320863425827298, 75.97497774878489452, -109.4233848709835542 ) ) ;
#239432 = EDGE_LOOP ( 'NONE', ( #239785, #150257, #203305, #105789, #97580 ) ) ;
#239431 = DIRECTION ( 'NONE',  ( 0.000000000000000000, 6.982962677686266711E-15, -1.000000000000000000 ) ) ;
#239433 = CIRCLE ( 'NONE', #226964, 0.1000000000000028644 ) ;
#239434 = DIRECTION ( 'NONE',  ( 0.000000000000000000, -1.000000000000000000, 0.000000000000000000 ) ) ;
#239435 = DIRECTION ( 'NONE',  ( 0.000000000000000000, 0.000000000000000000, -1.000000000000000000 ) ) ;
#239437 = ORIENTED_EDGE ( 'NONE', *, *, #99329, .F. ) ;
#239436 = CARTESIAN_POINT ( 'NONE',  ( -20.05000000000000426, 52.27009174976920747, -232.4217594817395138 ) ) ;
#239438 = CARTESIAN_POINT ( 'NONE',  ( 19.96984138294323685, 11.75000000001116263, -125.2245720712022461 ) ) ;
#239439 = EDGE_LOOP ( 'NONE', ( #225409, #74287, #135412, #92771 ) ) ;
#239440 = DIRECTION ( 'NONE',  ( -1.000000000000000000, -0.000000000000000000, -0.000000000000000000 ) ) ;
#239441 = CIRCLE ( 'NONE', #127014, 0.1000000000000028644 ) ;
#239443 = ORIENTED_EDGE ( 'NONE', *, *, #154282, .T. ) ;
#239442 = CARTESIAN_POINT ( 'NONE',  ( -23.15000000000000213, 67.23127455305841238, -235.8551265064783991 ) ) ;
#239444 = DIRECTION ( 'NONE',  ( 0.000000000000000000, 0.000000000000000000, 1.000000000000000000 ) ) ;
#239445 = DIRECTION ( 'NONE',  ( 0.000000000000000000, 0.1495327102803180597, 0.9887567792719412774 ) ) ;
#239446 = DIRECTION ( 'NONE',  ( -1.000000000000000000, -0.000000000000000000, -0.000000000000000000 ) ) ;
#239447 = ORIENTED_EDGE ( 'NONE', *, *, #50527, .F. ) ;
#239449 = CARTESIAN_POINT ( 'NONE',  ( 23.24999999999999289, 15.92646454033040371, -219.3818586450342423 ) ) ;
#239448 = DIRECTION ( 'NONE',  ( 0.000000000000000000, 0.000000000000000000, -1.000000000000000000 ) ) ;
#239450 = DIRECTION ( 'NONE',  ( 1.000000000000000000, -0.000000000000000000, -0.000000000000000000 ) ) ;
#239451 = CARTESIAN_POINT ( 'NONE',  ( -0.8999999999999993561, -11.75000000000000000, 23.30000000000000426 ) ) ;
#239452 = DIRECTION ( 'NONE',  ( -0.4999999999999797939, 0.7633972851576996677, -0.4089310272085914799 ) ) ;
#239453 = FACE_OUTER_BOUND ( 'NONE', #168009, .T. ) ;
#239454 = ORIENTED_EDGE ( 'NONE', *, *, #121864, .T. ) ;
#239455 = ORIENTED_EDGE ( 'NONE', *, *, #18355, .T. ) ;
#239456 = ORIENTED_EDGE ( 'NONE', *, *, #174564, .T. ) ;
#239457 = DIRECTION ( 'NONE',  ( 0.000000000000000000, -6.769652589177795712E-15, 1.000000000000000000 ) ) ;
#239458 = ORIENTED_EDGE ( 'NONE', *, *, #190965, .T. ) ;
#239459 = LINE ( 'NONE', #136474, #97602 ) ;
#239460 = ORIENTED_EDGE ( 'NONE', *, *, #226467, .T. ) ;
#239461 = DIRECTION ( 'NONE',  ( -1.000000000000000000, -0.000000000000000000, -0.000000000000000000 ) ) ;
#239462 = EDGE_CURVE ( 'NONE', #138871, #226022, #198983, .T. ) ;
#239463 = DIRECTION ( 'NONE',  ( 1.020425574104004196E-15, 1.210927747993693964E-31, 1.000000000000000000 ) ) ;
#239464 = CIRCLE ( 'NONE', #68767, 0.1000000000000002554 ) ;
#239465 = ADVANCED_FACE ( 'NONE', ( #252072 ), #70902, .F. ) ;
#239466 = EDGE_CURVE ( 'NONE', #17273, #88954, #204261, .T. ) ;
#239467 = AXIS2_PLACEMENT_3D ( 'NONE', #74205, #113288, #192840 ) ;
#239468 = EDGE_LOOP ( 'NONE', ( #41853, #217664, #97211, #77048 ) ) ;
#239469 = DIRECTION ( 'NONE',  ( 1.000000000000000000, 0.000000000000000000, 0.000000000000000000 ) ) ;
#239470 = CIRCLE ( 'NONE', #52189, 3.899999999999993694 ) ;
#239471 = VERTEX_POINT ( 'NONE', #244672 ) ;
#239472 = ORIENTED_EDGE ( 'NONE', *, *, #20438, .F. ) ;
#239473 = ORIENTED_EDGE ( 'NONE', *, *, #159806, .T. ) ;
#239474 = VECTOR ( 'NONE', #8117, 1000.000000000000000 ) ;
#239475 = FACE_OUTER_BOUND ( 'NONE', #181932, .T. ) ;
#239476 = DIRECTION ( 'NONE',  ( 0.000000000000000000, 0.01283462868040404978, 0.9999176327611370985 ) ) ;
#239477 = AXIS2_PLACEMENT_3D ( 'NONE', #69821, #91920, #176308 ) ;
#239478 = PLANE ( 'NONE',  #138412 ) ;
#239479 = CARTESIAN_POINT ( 'NONE',  ( -23.25000000000000000, 11.65000000000000036, -12.15000000000000036 ) ) ;
#239480 = CARTESIAN_POINT ( 'NONE',  ( -16.87036670365549895, 9.989418819312803066, -113.0204398826979855 ) ) ;
#239481 = DIRECTION ( 'NONE',  ( -0.000000000000000000, 1.000000000000000000, 1.734723475976807292E-15 ) ) ;
#239482 = EDGE_CURVE ( 'NONE', #89756, #46601, #14782, .T. ) ;
#239484 = CARTESIAN_POINT ( 'NONE',  ( 23.14999999999999503, 11.65000000000000746, -26.48519422934606027 ) ) ;
#239483 = CARTESIAN_POINT ( 'NONE',  ( -21.14999999999999858, -11.74999999998884448, -134.0000000000000000 ) ) ;
#239485 = FACE_OUTER_BOUND ( 'NONE', #158637, .T. ) ;
#239487 = ORIENTED_EDGE ( 'NONE', *, *, #131760, .T. ) ;
#239486 = DIRECTION ( 'NONE',  ( -0.000000000000000000, 1.000000000000000000, -0.000000000000000000 ) ) ;
#239488 = CARTESIAN_POINT ( 'NONE',  ( 22.39999999999999858, 76.00000000001165290, -69.52310748452431710 ) ) ;
#239489 = DIRECTION ( 'NONE',  ( 1.000000000000000000, -7.304098846218134667E-16, -4.639676173203993355E-30 ) ) ;
#239490 = ORIENTED_EDGE ( 'NONE', *, *, #80191, .F. ) ;
#239491 = VERTEX_POINT ( 'NONE', #171312 ) ;
#239492 = DIRECTION ( 'NONE',  ( 0.000000000000000000, 0.1575844902526835067, 0.9875055080513738259 ) ) ;
#239493 = CIRCLE ( 'NONE', #214352, 0.1000000000000060146 ) ;
#239494 = LINE ( 'NONE', #63397, #22744 ) ;
#239495 = FACE_OUTER_BOUND ( 'NONE', #6107, .T. ) ;
#239496 = VERTEX_POINT ( 'NONE', #130841 ) ;
#239497 = AXIS2_PLACEMENT_3D ( 'NONE', #173333, #130290, #48189 ) ;
#239498 = CARTESIAN_POINT ( 'NONE',  ( -21.05000000000000071, 1.115653327213047955E-11, -96.20000000000007390 ) ) ;
#239499 = VERTEX_POINT ( 'NONE', #31782 ) ;
#239500 = ORIENTED_EDGE ( 'NONE', *, *, #126743, .T. ) ;
#239501 = CARTESIAN_POINT ( 'NONE',  ( -16.87036670365549895, 9.989418819301645769, -12.52043988269794816 ) ) ;
#239503 = ORIENTED_EDGE ( 'NONE', *, *, #113180, .F. ) ;
#239502 = EDGE_CURVE ( 'NONE', #137759, #191212, #51272, .T. ) ;
#239504 = CARTESIAN_POINT ( 'NONE',  ( -16.94309007106720344, 60.88703202972964590, -221.0733422789901113 ) ) ;
#239505 = DIRECTION ( 'NONE',  ( 1.000000000000000000, 0.000000000000000000, 0.000000000000000000 ) ) ;
#239506 = EDGE_CURVE ( 'NONE', #256542, #106794, #170021, .T. ) ;
#239507 = DIRECTION ( 'NONE',  ( 0.000000000000000000, 0.6728971962617388280, 0.7397360091702248619 ) ) ;
#239508 = CIRCLE ( 'NONE', #202091, 0.5000000000000004441 ) ;
#239509 = CARTESIAN_POINT ( 'NONE',  ( 20.99999999999999645, 63.27875933230978234, -213.1799721866121047 ) ) ;
#239510 = CARTESIAN_POINT ( 'NONE',  ( 22.48660254037843842, 11.75000000001115730, -133.9500000000000171 ) ) ;
#239511 = VERTEX_POINT ( 'NONE', #210397 ) ;
#239512 = CARTESIAN_POINT ( 'NONE',  ( -23.15000000000000213, 76.00000000001244871, -170.0231074845243597 ) ) ;
#239513 = DIRECTION ( 'NONE',  ( 0.000000000000000000, 0.8814952561688430555, -0.4721928772777346239 ) ) ;
#239514 = ADVANCED_FACE ( 'NONE', ( #91720 ), #232543, .T. ) ;
#239515 = DIRECTION ( 'NONE',  ( -1.000000000000000000, -0.000000000000000000, -0.000000000000000000 ) ) ;
#239516 = AXIS2_PLACEMENT_3D ( 'NONE', #123318, #162454, #64608 ) ;
#239517 = VERTEX_POINT ( 'NONE', #184703 ) ;
#239518 = AXIS2_PLACEMENT_3D ( 'NONE', #81435, #619, #201409 ) ;
#239520 = ORIENTED_EDGE ( 'NONE', *, *, #19899, .F. ) ;
#239519 = DIRECTION ( 'NONE',  ( -1.000000000000000000, 0.000000000000000000, 0.000000000000000000 ) ) ;
#239521 = DIRECTION ( 'NONE',  ( -1.000000000000000000, 0.000000000000000000, 0.000000000000000000 ) ) ;
#239522 = LINE ( 'NONE', #219949, #190400 ) ;
#239523 = CARTESIAN_POINT ( 'NONE',  ( -22.50000000000000000, 12.54152817314149715, -223.4164406214577241 ) ) ;
#239524 = CARTESIAN_POINT ( 'NONE',  ( 21.05000000000000071, 74.16465844978715438, -57.96795619196134908 ) ) ;
#239525 = CARTESIAN_POINT ( 'NONE',  ( -16.90202395485760078, 9.965944544561997631, -46.09698627874021781 ) ) ;
#239526 = CARTESIAN_POINT ( 'NONE',  ( -16.87331047859651179, 66.05000000001207638, -123.8731074845243683 ) ) ;
#239527 = ORIENTED_EDGE ( 'NONE', *, *, #140878, .F. ) ;
#239528 = EDGE_CURVE ( 'NONE', #139486, #41986, #136613, .T. ) ;
#239529 = LINE ( 'NONE', #242078, #84292 ) ;
#239530 = LINE ( 'NONE', #98683, #52477 ) ;
#239531 = DIRECTION ( 'NONE',  ( 0.000000000000000000, 6.982962677686266711E-15, -1.000000000000000000 ) ) ;
#239532 = LINE ( 'NONE', #162576, #150723 ) ;
#239533 = AXIS2_PLACEMENT_3D ( 'NONE', #148039, #72368, #232722 ) ;
#239534 = CARTESIAN_POINT ( 'NONE',  ( -18.39999999999999858, -9.599999999988844124, -141.0320693966996828 ) ) ;
#239535 = VERTEX_POINT ( 'NONE', #249523 ) ;
#239536 = VERTEX_POINT ( 'NONE', #231253 ) ;
#239537 = CARTESIAN_POINT ( 'NONE',  ( -23.24999999999999645, 86.99291436658650412, -199.6658631664729739 ) ) ;
#239538 = DIRECTION ( 'NONE',  ( 0.000000000000000000, 0.4088369013363281068, -0.9126074666063770380 ) ) ;
#239539 = EDGE_CURVE ( 'NONE', #191527, #131402, #149130, .T. ) ;
#239541 = CARTESIAN_POINT ( 'NONE',  ( 27.30103769104855971, 12.20000000000000284, -347.0000000000001137 ) ) ;
#239540 = VECTOR ( 'NONE', #237312, 1000.000000000000000 ) ;
#239542 = CARTESIAN_POINT ( 'NONE',  ( 21.05000000000000071, 17.11694853917244075, -224.3781540347815735 ) ) ;
#239543 = ORIENTED_EDGE ( 'NONE', *, *, #81113, .T. ) ;
#239544 = PLANE ( 'NONE',  #97425 ) ;
#239545 = EDGE_CURVE ( 'NONE', #191355, #239696, #107410, .T. ) ;
#239546 = EDGE_CURVE ( 'NONE', #177351, #90545, #61621, .T. ) ;
#239547 = LINE ( 'NONE', #64748, #225915 ) ;
#239548 = DIRECTION ( 'NONE',  ( 0.000000000000000000, -6.982962677686266711E-15, 1.000000000000000000 ) ) ;
#239549 = EDGE_CURVE ( 'NONE', #20295, #245292, #207390, .T. ) ;
#239550 = AXIS2_PLACEMENT_3D ( 'NONE', #252198, #193538, #174010 ) ;
#239551 = VECTOR ( 'NONE', #225384, 1000.000000000000000 ) ;
#239552 = EDGE_CURVE ( 'NONE', #185125, #56614, #225097, .T. ) ;
#239553 = EDGE_LOOP ( 'NONE', ( #74237, #147159, #62936, #172044 ) ) ;
#239554 = DIRECTION ( 'NONE',  ( -1.000000000000000000, -3.265361837132813093E-16, 0.000000000000000000 ) ) ;
#239555 = ORIENTED_EDGE ( 'NONE', *, *, #195745, .T. ) ;
#239556 = DIRECTION ( 'NONE',  ( 0.000000000000000000, 0.000000000000000000, 1.000000000000000000 ) ) ;
#239557 = CARTESIAN_POINT ( 'NONE',  ( 21.05000000000000071, 69.65564095796925415, -170.0379631194183503 ) ) ;
#239559 = EDGE_CURVE ( 'NONE', #36418, #95156, #182445, .T. ) ;
#239558 = CARTESIAN_POINT ( 'NONE',  ( -22.59999999999999787, 0.1000000000111554016, -155.8504291924551808 ) ) ;
#239560 = DIRECTION ( 'NONE',  ( -1.000000000000000000, -0.000000000000000000, -0.000000000000000000 ) ) ;
#239561 = CARTESIAN_POINT ( 'NONE',  ( 18.70000000000000284, 1.350000000000000089, 22.00000000000000355 ) ) ;
#239562 = DIRECTION ( 'NONE',  ( 0.000000000000000000, 0.000000000000000000, 1.000000000000000000 ) ) ;
#239563 = CARTESIAN_POINT ( 'NONE',  ( 20.94999999999999929, 69.09936979046463534, -247.6075824278584889 ) ) ;
#239564 = LINE ( 'NONE', #2211, #168243 ) ;
#239565 = DIRECTION ( 'NONE',  ( 1.000000000000000000, -0.000000000000000000, -0.000000000000000000 ) ) ;
#239566 = ADVANCED_FACE ( 'NONE', ( #79831 ), #257153, .F. ) ;
#239567 = DIRECTION ( 'NONE',  ( 0.000000000000000000, -0.9770955615653313941, -0.2128009952263603677 ) ) ;
#239568 = DIRECTION ( 'NONE',  ( -1.000000000000000000, 0.000000000000000000, 0.000000000000000000 ) ) ;
#239569 = LINE ( 'NONE', #197860, #252089 ) ;
#239570 = AXIS2_PLACEMENT_3D ( 'NONE', #79645, #236170, #120117 ) ;
#239571 = AXIS2_PLACEMENT_3D ( 'NONE', #177430, #19619, #99117 ) ;
#239572 = ADVANCED_FACE ( 'NONE', ( #176413 ), #120314, .F. ) ;
#239573 = EDGE_CURVE ( 'NONE', #215272, #137086, #178350, .T. ) ;
#239574 = DIRECTION ( 'NONE',  ( -1.000000000000000000, 0.000000000000000000, -0.000000000000000000 ) ) ;
#239576 = CARTESIAN_POINT ( 'NONE',  ( 21.04999999999999716, 56.18374508921710486, -227.9290876000915489 ) ) ;
#239575 = AXIS2_PLACEMENT_3D ( 'NONE', #211611, #92923, #169957 ) ;
#239577 = VECTOR ( 'NONE', #130870, 1000.000000000000000 ) ;
#239578 = ORIENTED_EDGE ( 'NONE', *, *, #67547, .T. ) ;
#239579 = LINE ( 'NONE', #240863, #35626 ) ;
#239581 = ADVANCED_FACE ( 'NONE', ( #117695 ), #103289, .F. ) ;
#239580 = DIRECTION ( 'NONE',  ( 1.000000000000000000, 0.000000000000000000, 0.000000000000000000 ) ) ;
#239582 = DIRECTION ( 'NONE',  ( 0.000000000000000000, 0.000000000000000000, 1.000000000000000000 ) ) ;
#239583 = ORIENTED_EDGE ( 'NONE', *, *, #3965, .F. ) ;
#239584 = CARTESIAN_POINT ( 'NONE',  ( -22.43310005002225438, 0.005636942152031573783, -55.35033787286564433 ) ) ;
#239585 = EDGE_CURVE ( 'NONE', #156311, #68456, #40768, .T. ) ;
#239586 = EDGE_CURVE ( 'NONE', #154626, #60331, #170006, .T. ) ;
#239587 = CARTESIAN_POINT ( 'NONE',  ( 22.59999999999999432, -2.381330705637465961, -189.5959759702857923 ) ) ;
#239588 = ORIENTED_EDGE ( 'NONE', *, *, #250821, .T. ) ;
#239589 = DIRECTION ( 'NONE',  ( 0.000000000000000000, 6.938893903907222067E-15, -1.000000000000000000 ) ) ;
#239590 = CARTESIAN_POINT ( 'NONE',  ( 22.50000000000000000, 75.90000000001172964, -81.17267829206912211 ) ) ;
#239591 = EDGE_CURVE ( 'NONE', #34506, #203324, #35636, .T. ) ;
#239592 = ORIENTED_EDGE ( 'NONE', *, *, #63698, .F. ) ;
#239593 = VECTOR ( 'NONE', #95075, 1000.000000000000000 ) ;
#239594 = CIRCLE ( 'NONE', #118801, 0.09999999999998898659 ) ;
#239595 = ORIENTED_EDGE ( 'NONE', *, *, #93748, .T. ) ;
#239596 = CARTESIAN_POINT ( 'NONE',  ( -18.59999999999999787, 77.16412189325330928, -128.6082593989527254 ) ) ;
#239597 = ORIENTED_EDGE ( 'NONE', *, *, #86128, .F. ) ;
#239598 = ADVANCED_FACE ( 'NONE', ( #253353 ), #165702, .T. ) ;
#239599 = CARTESIAN_POINT ( 'NONE',  ( 21.07954640115340439, 0.06600770713963947933, 6.329287696024268328 ) ) ;
#239600 = DIRECTION ( 'NONE',  ( 0.000000000000000000, 0.2128009952263485993, -0.9770955615653341697 ) ) ;
#239602 = VECTOR ( 'NONE', #91743, 1000.000000000000000 ) ;
#239601 = FACE_OUTER_BOUND ( 'NONE', #129404, .T. ) ;
#239604 = DIRECTION ( 'NONE',  ( 0.000000000000000000, 1.000000000000000000, 0.000000000000000000 ) ) ;
#239603 = VECTOR ( 'NONE', #124783, 1000.000000000000000 ) ;
#239605 = AXIS2_PLACEMENT_3D ( 'NONE', #138649, #156990, #20042 ) ;
#239606 = DIRECTION ( 'NONE',  ( -1.000000000000000000, -0.000000000000000000, -0.000000000000000000 ) ) ;
#239607 = CARTESIAN_POINT ( 'NONE',  ( 23.14999999999999858, 80.00000000001244871, -170.0231074845243313 ) ) ;
#239608 = CYLINDRICAL_SURFACE ( 'NONE', #72029, 0.09999999999999560629 ) ;
#239609 = DIRECTION ( 'NONE',  ( -0.7071067811865389130, 0.000000000000000000, 0.7071067811865561215 ) ) ;
#239611 = EDGE_LOOP ( 'NONE', ( #164228, #177335, #251263, #75226 ) ) ;
#239610 = CARTESIAN_POINT ( 'NONE',  ( -18.59999999999999787, 11.65000000001115232, -45.75000000000000000 ) ) ;
#239612 = ORIENTED_EDGE ( 'NONE', *, *, #195787, .T. ) ;
#239614 = DIRECTION ( 'NONE',  ( 0.000000000000000000, 0.000000000000000000, 1.000000000000000000 ) ) ;
#239613 = CARTESIAN_POINT ( 'NONE',  ( 22.45463910399148233, -8.887310749685707770E-13, 11.64957081018417639 ) ) ;
#239616 = ORIENTED_EDGE ( 'NONE', *, *, #147256, .T. ) ;
#239615 = CARTESIAN_POINT ( 'NONE',  ( -33.80000000000000426, 3.175288713399618601, -347.0000000000001137 ) ) ;
#239617 = EDGE_LOOP ( 'NONE', ( #98506, #150451, #162238, #202247, #167347, #54727 ) ) ;
#239618 = DIRECTION ( 'NONE',  ( -0.7070776581708965169, 0.7071359030027827286, 4.937903618720407826E-15 ) ) ;
#239619 = CARTESIAN_POINT ( 'NONE',  ( 23.14999999999999858, 1.115625160336667635E-11, -165.5000000000000284 ) ) ;
#239620 = AXIS2_PLACEMENT_3D ( 'NONE', #127102, #90533, #9715 ) ;
#239621 = FACE_OUTER_BOUND ( 'NONE', #173514, .T. ) ;
#239622 = DIRECTION ( 'NONE',  ( 1.000000000000000000, 0.000000000000000000, 0.000000000000000000 ) ) ;
#239623 = CARTESIAN_POINT ( 'NONE',  ( -18.50000000000000000, 1.115600667400684642E-11, -67.00000000000000000 ) ) ;
#239624 = AXIS2_PLACEMENT_3D ( 'NONE', #249192, #170980, #126664 ) ;
#239625 = FACE_OUTER_BOUND ( 'NONE', #191766, .T. ) ;
#239626 = AXIS2_PLACEMENT_3D ( 'NONE', #140185, #218441, #239315 ) ;
#239627 = DIRECTION ( 'NONE',  ( -0.000000000000000000, -0.4721928772777346239, -0.8814952561688430555 ) ) ;
#239628 = CARTESIAN_POINT ( 'NONE',  ( 18.59999999999999076, 77.14957036958777792, -128.7071950000224092 ) ) ;
#239630 = ORIENTED_EDGE ( 'NONE', *, *, #10092, .F. ) ;
#239629 = EDGE_CURVE ( 'NONE', #93986, #81149, #65896, .T. ) ;
#239631 = ORIENTED_EDGE ( 'NONE', *, *, #126868, .F. ) ;
#239632 = CARTESIAN_POINT ( 'NONE',  ( 17.23472005113827166, 60.28074582209914212, -222.1029091445273593 ) ) ;
#239633 = ADVANCED_FACE ( 'NONE', ( #98102 ), #236362, .F. ) ;
#239634 = EDGE_LOOP ( 'NONE', ( #57331, #179954, #2640 ) ) ;
#239635 = DIRECTION ( 'NONE',  ( -1.000000000000000000, 0.000000000000000000, 0.000000000000000000 ) ) ;
#239636 = ORIENTED_EDGE ( 'NONE', *, *, #5572, .T. ) ;
#239637 = CARTESIAN_POINT ( 'NONE',  ( -18.39999999999999858, 40.47920047438133651, -235.2678785906695396 ) ) ;
#239638 = DIRECTION ( 'NONE',  ( 0.000000000000000000, 0.000000000000000000, 1.000000000000000000 ) ) ;
#239639 = DIRECTION ( 'NONE',  ( 1.000000000000000000, 0.000000000000000000, 0.000000000000000000 ) ) ;
#239640 = DIRECTION ( 'NONE',  ( -0.000000000000000000, 0.000000000000000000, 1.000000000000000000 ) ) ;
#239641 = ORIENTED_EDGE ( 'NONE', *, *, #257669, .F. ) ;
#239642 = DIRECTION ( 'NONE',  ( 0.000000000000000000, 0.000000000000000000, -1.000000000000000000 ) ) ;
#239643 = ORIENTED_EDGE ( 'NONE', *, *, #232215, .T. ) ;
#239644 = AXIS2_PLACEMENT_3D ( 'NONE', #211409, #31518, #151452 ) ;
#239645 = FACE_OUTER_BOUND ( 'NONE', #44780, .T. ) ;
#239646 = DIRECTION ( 'NONE',  ( 1.000000000000000000, 0.000000000000000000, 0.000000000000000000 ) ) ;
#239647 = TOROIDAL_SURFACE ( 'NONE', #43830, 0.2000000000000000111, 0.1000000000000000056 ) ;
#239648 = CARTESIAN_POINT ( 'NONE',  ( 21.15000000000005187, 76.00000000001119815, -36.02310748452479316 ) ) ;
#239649 = DIRECTION ( 'NONE',  ( 0.000000000000000000, 1.000000000000000000, 0.000000000000000000 ) ) ;
#239650 = EDGE_CURVE ( 'NONE', #185482, #44981, #154313, .T. ) ;
#239651 = AXIS2_PLACEMENT_3D ( 'NONE', #3263, #684, #121955 ) ;
#239652 = VERTEX_POINT ( 'NONE', #58977 ) ;
#239653 = DIRECTION ( 'NONE',  ( -0.000000000000000000, -0.1298341882520022694, -0.9915357197604853789 ) ) ;
#239654 = ORIENTED_EDGE ( 'NONE', *, *, #151681, .T. ) ;
#239657 = VERTEX_POINT ( 'NONE', #233810 ) ;
#239656 = DIRECTION ( 'NONE',  ( 0.000000000000000000, -0.000000000000000000, 1.000000000000000000 ) ) ;
#239655 = FACE_OUTER_BOUND ( 'NONE', #173176, .T. ) ;
#239658 = CARTESIAN_POINT ( 'NONE',  ( 22.39999999999999503, 31.76383008438224564, -238.8689086587541510 ) ) ;
#239659 = CIRCLE ( 'NONE', #127222, 0.1000000000000028644 ) ;
#239660 = CARTESIAN_POINT ( 'NONE',  ( 20.94999999999999574, -1.851028230129704522, -45.15391326942249606 ) ) ;
#239661 = ORIENTED_EDGE ( 'NONE', *, *, #215551, .F. ) ;
#239662 = FACE_OUTER_BOUND ( 'NONE', #240115, .T. ) ;
#239663 = CARTESIAN_POINT ( 'NONE',  ( -22.45372860728439690, -3.133362159202385921, -228.2185976283504374 ) ) ;
#239664 = AXIS2_PLACEMENT_3D ( 'NONE', #73626, #74910, #55277 ) ;
#239665 = UNCERTAINTY_MEASURE_WITH_UNIT (LENGTH_MEASURE( 1.000000000000000082E-05 ), #198158, 'distance_accuracy_value', 'NONE');
#239667 = ORIENTED_EDGE ( 'NONE', *, *, #24728, .F. ) ;
#239666 = CARTESIAN_POINT ( 'NONE',  ( -18.40000000000000213, 64.66825945288690036, -123.8731074845243683 ) ) ;
#239668 = AXIS2_PLACEMENT_3D ( 'NONE', #187538, #169274, #109245 ) ;
#239669 = CARTESIAN_POINT ( 'NONE',  ( -20.00857864376270001, 9.350000000011156942, -155.2500000000000284 ) ) ;
#239670 = CIRCLE ( 'NONE', #127245, 0.09999999999999939493 ) ;
#239671 = ORIENTED_EDGE ( 'NONE', *, *, #223124, .F. ) ;
#239672 = FACE_OUTER_BOUND ( 'NONE', #190332, .T. ) ;
#239673 = CARTESIAN_POINT ( 'NONE',  ( -16.93935632781549572, 9.984730499736244269, -188.3896607487102699 ) ) ;
#239674 = CARTESIAN_POINT ( 'NONE',  ( -18.58744394320938298, -9.566385154537240254, -140.8228480538762994 ) ) ;
#239675 = ORIENTED_EDGE ( 'NONE', *, *, #111053, .T. ) ;
#239676 = DIRECTION ( 'NONE',  ( -1.000000000000000000, 0.000000000000000000, 0.000000000000000000 ) ) ;
#239677 = EDGE_LOOP ( 'NONE', ( #172393, #62441, #65982, #25565 ) ) ;
#239678 = DIRECTION ( 'NONE',  ( 1.000000000000000000, 0.000000000000000000, 0.000000000000000000 ) ) ;
#239679 = DIRECTION ( 'NONE',  ( -1.000000000000000000, 0.000000000000000000, 0.000000000000000000 ) ) ;
#239680 = DIRECTION ( 'NONE',  ( -1.836970198721029934E-16, 1.000000000000000000, 0.000000000000000000 ) ) ;
#239681 = AXIS2_PLACEMENT_3D ( 'NONE', #173361, #114619, #57187 ) ;
#239682 = VERTEX_POINT ( 'NONE', #237652 ) ;
#239683 = DIRECTION ( 'NONE',  ( 4.239556034732056743E-17, 0.1298341882519953860, 0.9915357197604862671 ) ) ;
#239684 = EDGE_CURVE ( 'NONE', #79646, #101850, #157519, .T. ) ;
#239685 = CARTESIAN_POINT ( 'NONE',  ( -20.94999999999999929, 0.000000000000000000, -33.50000000000000000 ) ) ;
#239686 = CARTESIAN_POINT ( 'NONE',  ( -21.04386569057572132, 64.25000000001250555, -176.8802701327438456 ) ) ;
#239687 = ADVANCED_FACE ( 'NONE', ( #139818 ), #138514, .F. ) ;
#239688 = ORIENTED_EDGE ( 'NONE', *, *, #170055, .T. ) ;
#239689 = CARTESIAN_POINT ( 'NONE',  ( -21.05000000000000071, 35.94660524813657076, -234.4748257877825495 ) ) ;
#239690 = DIRECTION ( 'NONE',  ( 0.000000000000000000, 0.9998779222360102414, 0.01562499999996356907 ) ) ;
#239691 = VERTEX_POINT ( 'NONE', #197235 ) ;
#239692 = CARTESIAN_POINT ( 'NONE',  ( 22.39999999999999503, 75.90000000001170122, -77.31388708289770761 ) ) ;
#239693 = TOROIDAL_SURFACE ( 'NONE', #61193, 4.149999999999999467, 0.1000000000000000056 ) ;
#239694 = AXIS2_PLACEMENT_3D ( 'NONE', #133441, #78589, #218088 ) ;
#239695 = ORIENTED_EDGE ( 'NONE', *, *, #65173, .T. ) ;
#239696 = VERTEX_POINT ( 'NONE', #198518 ) ;
#239697 = EDGE_CURVE ( 'NONE', #160821, #235594, #244763, .T. ) ;
#239698 = CARTESIAN_POINT ( 'NONE',  ( -21.14999999999994174, 76.00000000001119815, -36.02310748452479316 ) ) ;
#239699 = ORIENTED_EDGE ( 'NONE', *, *, #31476, .T. ) ;
#239701 = EDGE_LOOP ( 'NONE', ( #134306, #146507, #237330, #102261, #87965, #210099, #244864, #155860, #202171, #189102, #88969, #207773 ) ) ;
#239700 = DIRECTION ( 'NONE',  ( 1.000000000000000000, -0.000000000000000000, -0.000000000000000000 ) ) ;
#239702 = EDGE_CURVE ( 'NONE', #109096, #228673, #99397, .T. ) ;
#239703 = EDGE_CURVE ( 'NONE', #82701, #169886, #5422, .T. ) ;
#239706 = ORIENTED_EDGE ( 'NONE', *, *, #217458, .F. ) ;
#239705 = ORIENTED_EDGE ( 'NONE', *, *, #192162, .T. ) ;
#239704 = CARTESIAN_POINT ( 'NONE',  ( 23.40000000000005187, 76.00000000001119815, -36.02310748452479316 ) ) ;
#239707 = CARTESIAN_POINT ( 'NONE',  ( 21.05000000000000071, 65.51540711881665402, -95.56639391393910898 ) ) ;
#239708 = CARTESIAN_POINT ( 'NONE',  ( -20.94999999999999929, 44.15969672213208952, -258.9565289832007693 ) ) ;
#239709 = CARTESIAN_POINT ( 'NONE',  ( -20.94999999999999929, 18.26942912180536638, -237.6183358664095238 ) ) ;
#239710 = ADVANCED_FACE ( 'NONE', ( #126687 ), #182635, .T. ) ;
#239711 = DIRECTION ( 'NONE',  ( -1.020425574104004196E-15, 0.000000000000000000, 1.000000000000000000 ) ) ;
#239712 = DIRECTION ( 'NONE',  ( 0.000000000000000000, 2.891205793294679805E-16, -1.000000000000000000 ) ) ;
#239713 = AXIS2_PLACEMENT_3D ( 'NONE', #31668, #189435, #90307 ) ;
#239714 = LINE ( 'NONE', #79326, #143066 ) ;
#239715 = FACE_OUTER_BOUND ( 'NONE', #153757, .T. ) ;
#239717 = CARTESIAN_POINT ( 'NONE',  ( 23.15000000000000213, 28.42524210734032408, -258.3567845160494585 ) ) ;
#239716 = CARTESIAN_POINT ( 'NONE',  ( -20.85000000000000142, 17.16609282392353819, -224.6038045889790453 ) ) ;
#239718 = ORIENTED_EDGE ( 'NONE', *, *, #196779, .F. ) ;
#239719 = ORIENTED_EDGE ( 'NONE', *, *, #69682, .T. ) ;
#239720 = DIRECTION ( 'NONE',  ( 1.000000000000000000, 0.000000000000000000, 0.000000000000000000 ) ) ;
#239721 = AXIS2_PLACEMENT_3D ( 'NONE', #103876, #183450, #4771 ) ;
#239723 = VERTEX_POINT ( 'NONE', #43307 ) ;
#239722 = DIRECTION ( 'NONE',  ( 0.000000000000000000, 0.000000000000000000, 1.000000000000000000 ) ) ;
#239724 = DIRECTION ( 'NONE',  ( -1.000000000000000000, 0.000000000000000000, -0.000000000000000000 ) ) ;
#239725 = ORIENTED_EDGE ( 'NONE', *, *, #77821, .T. ) ;
#239726 = EDGE_CURVE ( 'NONE', #63552, #182014, #185376, .T. ) ;
#239727 = CARTESIAN_POINT ( 'NONE',  ( -16.79814274880124358, 12.41384038458400063, -211.2454210646436650 ) ) ;
#239728 = ORIENTED_EDGE ( 'NONE', *, *, #79784, .T. ) ;
#239729 = DIRECTION ( 'NONE',  ( 0.000000000000000000, 0.000000000000000000, 1.000000000000000000 ) ) ;
#239730 = ORIENTED_EDGE ( 'NONE', *, *, #188393, .F. ) ;
#239731 = B_SPLINE_CURVE_WITH_KNOTS ( 'NONE', 3,
 ( #184858, #148314, #88302, #89604, #126161, #67482, #167907 ),
 .UNSPECIFIED., .F., .F.,
 ( 4, 3, 4 ),
 ( 0.000000000000000000, 1.860045280646151707E-05, 5.251155757304620461E-05 ),
 .UNSPECIFIED. ) ;
#239732 = CARTESIAN_POINT ( 'NONE',  ( -6.100000000000005862, -11.75000000000000000, 13.90000000000000213 ) ) ;
#239733 = DIRECTION ( 'NONE',  ( 0.000000000000000000, -1.000000000000000000, -6.982962677686265922E-15 ) ) ;
#239736 = ORIENTED_EDGE ( 'NONE', *, *, #48184, .T. ) ;
#239735 = ORIENTED_EDGE ( 'NONE', *, *, #238350, .F. ) ;
#239734 = CIRCLE ( 'NONE', #14897, 0.5000000000000004441 ) ;
#239737 = VECTOR ( 'NONE', #192704, 1000.000000000000000 ) ;
#239738 = ORIENTED_EDGE ( 'NONE', *, *, #96503, .T. ) ;
#239739 = FACE_OUTER_BOUND ( 'NONE', #118556, .T. ) ;
#239740 = ORIENTED_EDGE ( 'NONE', *, *, #169765, .F. ) ;
#239741 = VERTEX_POINT ( 'NONE', #104520 ) ;
#239742 = DIRECTION ( 'NONE',  ( 0.000000000000000000, 7.026728003956683390E-15, -1.000000000000000000 ) ) ;
#239744 = ORIENTED_EDGE ( 'NONE', *, *, #257486, .F. ) ;
#239743 = DIRECTION ( 'NONE',  ( 0.000000000000000000, -1.000000000000000000, 0.000000000000000000 ) ) ;
#239746 = DIRECTION ( 'NONE',  ( 0.000000000000000000, -0.4088369013363783999, 0.9126074666063545004 ) ) ;
#239745 = FACE_OUTER_BOUND ( 'NONE', #168676, .T. ) ;
#239747 = DIRECTION ( 'NONE',  ( -0.000000000000000000, 0.2128009952263603677, -0.9770955615653313941 ) ) ;
#239748 = DIRECTION ( 'NONE',  ( 1.000000000000000000, 0.000000000000000000, 0.000000000000000000 ) ) ;
#239749 = CARTESIAN_POINT ( 'NONE',  ( -21.07928932188134041, 6.328516656404449492, -66.90110485434564680 ) ) ;
#239750 = ORIENTED_EDGE ( 'NONE', *, *, #105516, .T. ) ;
#239751 = EDGE_LOOP ( 'NONE', ( #90901, #128891, #15192, #226293 ) ) ;
#239752 = DIRECTION ( 'NONE',  ( -1.000000000000000000, -0.000000000000000000, -0.000000000000000000 ) ) ;
#239753 = CARTESIAN_POINT ( 'NONE',  ( 16.27683809663750125, 19.69766786220171184, -229.8585047820796490 ) ) ;
#239754 = VERTEX_POINT ( 'NONE', #202374 ) ;
#239755 = DIRECTION ( 'NONE',  ( -1.000000000000000000, 3.265361837132813093E-16, 2.280189983783949500E-30 ) ) ;
#239756 = CIRCLE ( 'NONE', #147987, 2.699999999999999289 ) ;
#239757 = AXIS2_PLACEMENT_3D ( 'NONE', #50596, #170626, #31095 ) ;
#239758 = AXIS2_PLACEMENT_3D ( 'NONE', #203462, #225555, #182626 ) ;
#239759 = EDGE_CURVE ( 'NONE', #124485, #256436, #4161, .T. ) ;
#239760 = CYLINDRICAL_SURFACE ( 'NONE', #134609, 0.09999999999999854838 ) ;
#239761 = CARTESIAN_POINT ( 'NONE',  ( -13.12432614554023225, 12.45583213463953776, -213.8748143118951930 ) ) ;
#239762 = ORIENTED_EDGE ( 'NONE', *, *, #128126, .T. ) ;
#239763 = EDGE_LOOP ( 'NONE', ( #49844, #45140, #73693, #130944 ) ) ;
#239764 = STYLED_ITEM ( 'NONE', ( #165058 ), #42038 ) ;
#239765 = CARTESIAN_POINT ( 'NONE',  ( 23.14999999999999858, 74.00000000001213607, -136.5231074845243597 ) ) ;
#239766 = DIRECTION ( 'NONE',  ( 0.000000000000000000, 0.2128009952263603677, -0.9770955615653313941 ) ) ;
#239767 = VERTEX_POINT ( 'NONE', #206226 ) ;
#239768 = LINE ( 'NONE', #139353, #184937 ) ;
#239769 = ORIENTED_EDGE ( 'NONE', *, *, #239903, .F. ) ;
#239770 = CARTESIAN_POINT ( 'NONE',  ( -23.15000000000000213, 64.25000000001215028, -136.5231074845243597 ) ) ;
#239772 = EDGE_CURVE ( 'NONE', #100316, #255281, #191006, .T. ) ;
#239771 = LINE ( 'NONE', #61120, #62269 ) ;
#239773 = CARTESIAN_POINT ( 'NONE',  ( -20.00857864376270001, 30.14024212288317628, -235.5657495473015501 ) ) ;
#239774 = CARTESIAN_POINT ( 'NONE',  ( -21.04999999999994387, 74.16448838626247664, -47.52760213295649550 ) ) ;
#239775 = CARTESIAN_POINT ( 'NONE',  ( -16.88560720703333473, 66.04943515626217732, -90.37499556366066145 ) ) ;
#239776 = EDGE_CURVE ( 'NONE', #60057, #140162, #143673, .T. ) ;
#239777 = ADVANCED_FACE ( 'NONE', ( #184088 ), #244054, .T. ) ;
#239778 = ORIENTED_EDGE ( 'NONE', *, *, #158034, .T. ) ;
#239779 = CARTESIAN_POINT ( 'NONE',  ( -24.30000000000000071, 3.175288713399619933, 33.00000000000000000 ) ) ;
#239780 = VECTOR ( 'NONE', #2011, 1000.000000000000000 ) ;
#239782 = ORIENTED_EDGE ( 'NONE', *, *, #209906, .T. ) ;
#239781 = EDGE_LOOP ( 'NONE', ( #219421, #21582, #42160, #50787 ) ) ;
#239783 = VERTEX_POINT ( 'NONE', #181546 ) ;
#239784 = CIRCLE ( 'NONE', #173193, 0.3999999999999975797 ) ;
#239785 = ORIENTED_EDGE ( 'NONE', *, *, #239817, .T. ) ;
#239786 = CARTESIAN_POINT ( 'NONE',  ( 22.42357213249528769, 7.672932386371071445, -33.40091303599844252 ) ) ;
#239787 = CARTESIAN_POINT ( 'NONE',  ( -22.59999999999999787, 75.89914163091303578, -81.27267460801371612 ) ) ;
#239788 = LINE ( 'NONE', #212845, #167322 ) ;
#239789 = DIRECTION ( 'NONE',  ( 0.000000000000000000, 0.000000000000000000, 1.000000000000000000 ) ) ;
#239790 = TOROIDAL_SURFACE ( 'NONE', #169076, 11.65000000000000036, 0.1000000000000000056 ) ;
#239791 = FACE_OUTER_BOUND ( 'NONE', #65547, .T. ) ;
#239792 = ADVANCED_FACE ( 'NONE', ( #65423 ), #101955, .F. ) ;
#239793 =( BOUNDED_SURFACE ( )  B_SPLINE_SURFACE ( 3, 2, ( 
 ( #242110, #21802, #101267 ),
 ( #180872, #222533, #166467 ),
 ( #240844, #62205, #163875 ),
 ( #140437, #183438, #221252 ),
 ( #42632, #45199, #63469 ),
 ( #122183, #2205, #142991 ) ),
 .UNSPECIFIED., .F., .F., .T. ) 
 B_SPLINE_SURFACE_WITH_KNOTS ( ( 4, 2, 4 ),
 ( 3, 3 ),
 ( 0.0001300404313046688953, 0.0003183318589266743992, 0.0005066232865486798489 ),
 ( 0.000000000000000000, 1.000000000000000000 ),
 .UNSPECIFIED. ) 
 GEOMETRIC_REPRESENTATION_ITEM ( )  RATIONAL_B_SPLINE_SURFACE ( (
 ( 1.000000000000000000, 0.7071067811865352493, 1.000000000000000000),
 ( 1.000000000000000000, 0.7625113560533072210, 1.000000000000000000),
 ( 1.000000000000000000, 0.8126073484697884375, 1.000000000000000000),
 ( 1.000000000000000000, 0.8923049332722788884, 1.000000000000000000),
 ( 1.000000000000000000, 0.9231914937776775076, 1.000000000000000000),
 ( 1.000000000000000000, 0.9238795325113161594, 1.000000000000000000) ) ) 
 REPRESENTATION_ITEM ( '' )  SURFACE ( )  );
#239795 = DIRECTION ( 'NONE',  ( 1.000000000000000000, 0.000000000000000000, 0.000000000000000000 ) ) ;
#239794 = DIRECTION ( 'NONE',  ( 0.000000000000000000, 0.000000000000000000, -1.000000000000000000 ) ) ;
#239796 = ORIENTED_EDGE ( 'NONE', *, *, #204702, .F. ) ;
#239797 = PLANE ( 'NONE',  #112358 ) ;
#239798 = EDGE_LOOP ( 'NONE', ( #21436, #222741, #152959, #250574 ) ) ;
#239799 = TOROIDAL_SURFACE ( 'NONE', #14936, 11.65000000000000036, 0.1000000000000000056 ) ;
#239800 = EDGE_CURVE ( 'NONE', #139968, #234879, #125413, .T. ) ;
#239801 = CARTESIAN_POINT ( 'NONE',  ( -22.48660254037843487, 11.65000000001115588, -66.95000000000005969 ) ) ;
#239802 = AXIS2_PLACEMENT_3D ( 'NONE', #32798, #254349, #194423 ) ;
#239803 = VECTOR ( 'NONE', #129393, 1000.000000000000000 ) ;
#239804 = VERTEX_POINT ( 'NONE', #1590 ) ;
#239805 = EDGE_LOOP ( 'NONE', ( #58045, #118178, #69392, #180732, #151113 ) ) ;
#239806 = CARTESIAN_POINT ( 'NONE',  ( -18.50000000000000000, -9.399999999988850163, -207.8820418481726335 ) ) ;
#239807 = CYLINDRICAL_SURFACE ( 'NONE', #135125, 0.1000000000000055844 ) ;
#239808 = CARTESIAN_POINT ( 'NONE',  ( -18.40000000000000213, 64.52683809664981140, -157.3731074845244393 ) ) ;
#239809 = CARTESIAN_POINT ( 'NONE',  ( 20.94999999999999929, 15.00011753506359469, -219.4812630108571057 ) ) ;
#239810 = VECTOR ( 'NONE', #47245, 1000.000000000000000 ) ;
#239811 = ORIENTED_EDGE ( 'NONE', *, *, #123004, .F. ) ;
#239812 = ORIENTED_EDGE ( 'NONE', *, *, #118683, .T. ) ;
#239814 =( BOUNDED_SURFACE ( )  B_SPLINE_SURFACE ( 3, 2, ( 
 ( #119298, #237944, #59268 ),
 ( #99696, #241802, #219661 ),
 ( #222214, #120598, #163558 ),
 ( #183132, #21496, #83963 ),
 ( #180557, #181836, #143976 ),
 ( #160995, #240525, #43613 ),
 ( #220942, #22788, #103555 ),
 ( #244360, #246931, #70907 ),
 ( #245661, #107428, #65736 ),
 ( #166161, #167433, #30485 ) ),
 .UNSPECIFIED., .F., .F., .F. ) 
 B_SPLINE_SURFACE_WITH_KNOTS ( ( 4, 2, 2, 2, 4 ),
 ( 3, 3 ),
 ( 0.002161241639767248670, 0.002579950749615824400, 0.002789305304540112482, 0.002893982582002256523, 0.002998659859464400564 ),
 ( 0.000000000000000000, 1.000000000000000000 ),
 .UNSPECIFIED. ) 
 GEOMETRIC_REPRESENTATION_ITEM ( )  RATIONAL_B_SPLINE_SURFACE ( (
 ( 1.000000000000000000, 0.7071067811865475727, 1.000000000000000000),
 ( 1.000000000000000000, 0.7632447400667299320, 1.000000000000000000),
 ( 1.000000000000000000, 0.8158073005105956899, 1.000000000000000000),
 ( 1.000000000000000000, 0.8906973462397930197, 1.000000000000000000),
 ( 1.000000000000000000, 0.9149408947800677927, 1.000000000000000000),
 ( 1.000000000000000000, 0.9493368785275483335, 1.000000000000000000),
 ( 1.000000000000000000, 0.9605194247156682019, 1.000000000000000000),
 ( 1.000000000000000000, 0.9803630264781214576, 1.000000000000000000),
 ( 1.000000000000000000, 0.9900844824271117783, 1.000000000000000000),
 ( 1.000000000000000000, 0.9894588281429294030, 1.000000000000000000) ) ) 
 REPRESENTATION_ITEM ( '' )  SURFACE ( )  );
#239813 = AXIS2_PLACEMENT_3D ( 'NONE', #96783, #116394, #229911 ) ;
#239815 = EDGE_CURVE ( 'NONE', #22117, #190676, #257550, .T. ) ;
#239816 = CARTESIAN_POINT ( 'NONE',  ( -18.59999999999999787, 9.150000000011157653, -79.35000000000005116 ) ) ;
#239818 = ORIENTED_EDGE ( 'NONE', *, *, #116493, .T. ) ;
#239817 = EDGE_CURVE ( 'NONE', #60065, #217929, #103468, .T. ) ;
#239819 = CARTESIAN_POINT ( 'NONE',  ( -18.39999999999999858, 86.99291436658650412, -199.6658631664729739 ) ) ;
#239820 = CARTESIAN_POINT ( 'NONE',  ( -16.92132318717937522, 9.966070024017081863, -46.12240663035206722 ) ) ;
#239821 = EDGE_CURVE ( 'NONE', #9918, #81803, #78550, .T. ) ;
#239822 = AXIS2_PLACEMENT_3D ( 'NONE', #79768, #81059, #182765 ) ;
#239823 = DIRECTION ( 'NONE',  ( 0.000000000000000000, 0.000000000000000000, -1.000000000000000000 ) ) ;
#239824 = DIRECTION ( 'NONE',  ( 0.000000000000000000, 0.000000000000000000, -1.000000000000000000 ) ) ;
#239825 = DIRECTION ( 'NONE',  ( 0.000000000000000000, 1.000000000000000000, 0.000000000000000000 ) ) ;
#239826 = FACE_OUTER_BOUND ( 'NONE', #35724, .T. ) ;
#239827 = CARTESIAN_POINT ( 'NONE',  ( 23.14999999999999503, 10.92199707682457088, -220.3694341645321515 ) ) ;
#239828 = CARTESIAN_POINT ( 'NONE',  ( 18.59999999999999787, -1.835341550213255957, -179.0551512925629538 ) ) ;
#239829 = DIRECTION ( 'NONE',  ( 0.000000000000000000, 0.000000000000000000, 1.000000000000000000 ) ) ;
#239830 = DIRECTION ( 'NONE',  ( -1.000000000000000000, 1.836970198721029934E-16, 1.282749433769087582E-30 ) ) ;
#239831 =( BOUNDED_CURVE ( )  B_SPLINE_CURVE ( 3, ( #186813, #32902, #211499, #189374 ),
 .UNSPECIFIED., .F., .F. ) 
 B_SPLINE_CURVE_WITH_KNOTS ( ( 4, 4 ),
 ( -6.483702463810914196E-14, 1.570796326794903219 ),
 .UNSPECIFIED. ) 
 CURVE ( )  GEOMETRIC_REPRESENTATION_ITEM ( )  RATIONAL_B_SPLINE_CURVE ( ( 1.000000000000000000, 0.8047378541243480621, 0.8047378541243480621, 1.000000000000000000 ) ) 
 REPRESENTATION_ITEM ( '' )  );
#239832 = EDGE_LOOP ( 'NONE', ( #127724, #7254, #89314, #141871 ) ) ;
#239833 = CARTESIAN_POINT ( 'NONE',  ( -16.89146115310546037, 30.21126098987748065, -234.8080499024818266 ) ) ;
#239834 = ORIENTED_EDGE ( 'NONE', *, *, #150371, .T. ) ;
#239835 = CARTESIAN_POINT ( 'NONE',  ( 18.50000000000000000, 85.41920976342134963, -129.2753380217652648 ) ) ;
#239837 = AXIS2_PLACEMENT_3D ( 'NONE', #151139, #70343, #53314 ) ;
#239836 = CARTESIAN_POINT ( 'NONE',  ( 20.94999999999999574, -11.64999999998883595, -136.9000000000000341 ) ) ;
#239838 = CARTESIAN_POINT ( 'NONE',  ( 23.24999999999999645, 64.25000000001207923, -123.8731074845243683 ) ) ;
#239840 = ORIENTED_EDGE ( 'NONE', *, *, #180711, .T. ) ;
#239839 = VECTOR ( 'NONE', #47233, 1000.000000000000000 ) ;
#239841 = EDGE_CURVE ( 'NONE', #123700, #125534, #86387, .T. ) ;
#239842 = DIRECTION ( 'NONE',  ( 0.000000000000000000, 0.000000000000000000, -1.000000000000000000 ) ) ;
#239843 = AXIS2_PLACEMENT_3D ( 'NONE', #57246, #216337, #37736 ) ;
#239844 = AXIS2_PLACEMENT_3D ( 'NONE', #51359, #210484, #244454 ) ;
#239845 = DIRECTION ( 'NONE',  ( -0.000000000000000000, -0.000000000000000000, 1.000000000000000000 ) ) ;
#239846 = DIRECTION ( 'NONE',  ( -1.000000000000000000, 0.000000000000000000, 0.000000000000000000 ) ) ;
#239847 = DIRECTION ( 'NONE',  ( 1.000000000000000000, 0.000000000000000000, 0.000000000000000000 ) ) ;
#239848 = CARTESIAN_POINT ( 'NONE',  ( -16.93262454970419384, 10.00202046794151478, -121.4270762262373466 ) ) ;
#239849 = DIRECTION ( 'NONE',  ( 0.000000000000000000, 0.000000000000000000, 1.000000000000000000 ) ) ;
#239850 = CIRCLE ( 'NONE', #123315, 0.1000000000000001027 ) ;
#239851 = ORIENTED_EDGE ( 'NONE', *, *, #116711, .F. ) ;
#239852 = DIRECTION ( 'NONE',  ( -0.000000000000000000, 0.000000000000000000, -1.000000000000000000 ) ) ;
#239853 = ORIENTED_EDGE ( 'NONE', *, *, #139982, .F. ) ;
#239854 = FACE_OUTER_BOUND ( 'NONE', #195961, .T. ) ;
#239855 = EDGE_CURVE ( 'NONE', #62691, #150108, #209260, .T. ) ;
#239856 = DIRECTION ( 'NONE',  ( 0.000000000000000000, 0.9126074666063660468, 0.4088369013363524762 ) ) ;
#239857 = DIRECTION ( 'NONE',  ( 0.000000000000000000, 0.000000000000000000, 1.000000000000000000 ) ) ;
#239858 = AXIS2_PLACEMENT_3D ( 'NONE', #199688, #234944, #178853 ) ;
#239859 = ORIENTED_EDGE ( 'NONE', *, *, #203008, .F. ) ;
#239860 = CARTESIAN_POINT ( 'NONE',  ( -22.41119224318417125, 76.00000000001222134, -148.1726782920690937 ) ) ;
#239861 = EDGE_CURVE ( 'NONE', #20178, #11297, #208797, .T. ) ;
#239862 = APPLICATION_PROTOCOL_DEFINITION ( 'draft international standard', 'automotive_design', 1998, #127392 ) ;
#239863 = CARTESIAN_POINT ( 'NONE',  ( 18.39999999999999858, -9.499999999988842703, -174.1001893912220737 ) ) ;
#239864 = CIRCLE ( 'NONE', #256339, 12.77500000000000036 ) ;
#239865 = ORIENTED_EDGE ( 'NONE', *, *, #50584, .F. ) ;
#239867 = EDGE_CURVE ( 'NONE', #241241, #244854, #73989, .T. ) ;
#239866 = FACE_OUTER_BOUND ( 'NONE', #151989, .T. ) ;
#239868 = CARTESIAN_POINT ( 'NONE',  ( 15.73863059295127798, 9.351403174152808973, -184.4795304368384734 ) ) ;
#239869 = EDGE_CURVE ( 'NONE', #107188, #210551, #53435, .T. ) ;
#239870 = EDGE_CURVE ( 'NONE', #176862, #173164, #215896, .T. ) ;
#239871 = CARTESIAN_POINT ( 'NONE',  ( 20.94999999999999929, 1.115600667400684642E-11, -71.09999999999999432 ) ) ;
#239872 = VERTEX_POINT ( 'NONE', #229640 ) ;
#239873 = AXIS2_PLACEMENT_3D ( 'NONE', #246126, #88294, #164023 ) ;
#239874 = EDGE_LOOP ( 'NONE', ( #30671, #41863, #30114, #43554 ) ) ;
#239875 = DIRECTION ( 'NONE',  ( 0.000000000000000000, 0.000000000000000000, 1.000000000000000000 ) ) ;
#239876 = CARTESIAN_POINT ( 'NONE',  ( -23.15000000000000213, 67.23127455305835554, -235.8551265064784559 ) ) ;
#239877 = PLANE ( 'NONE',  #240503 ) ;
#239878 = DIRECTION ( 'NONE',  ( 0.000000000000000000, -1.000000000000000000, -6.352154140967427193E-15 ) ) ;
#239879 = CARTESIAN_POINT ( 'NONE',  ( 18.56308993302939925, 10.38069115533503961, -125.2392226389383012 ) ) ;
#239881 = DIRECTION ( 'NONE',  ( 0.000000000000000000, 0.9126074666063769270, 0.4088369013363280513 ) ) ;
#239880 = CARTESIAN_POINT ( 'NONE',  ( 21.93340585971863632, 7.324147022855297173, -1.277737337956073836E-15 ) ) ;
#239882 = CARTESIAN_POINT ( 'NONE',  ( 23.24999999999999645, 4.775700934590584090, -145.8487681040459734 ) ) ;
#239883 = CARTESIAN_POINT ( 'NONE',  ( 20.94999999999999929, 76.00000000001142553, -36.02310748452432421 ) ) ;
#239884 = DIRECTION ( 'NONE',  ( -1.000000000000000000, 0.000000000000000000, 0.000000000000000000 ) ) ;
#239885 = CYLINDRICAL_SURFACE ( 'NONE', #72311, 0.09999999999999939493 ) ;
#239886 = AXIS2_PLACEMENT_3D ( 'NONE', #90649, #170256, #249742 ) ;
#239887 = ORIENTED_EDGE ( 'NONE', *, *, #96387, .F. ) ;
#239888 = EDGE_CURVE ( 'NONE', #217291, #84692, #91419, .T. ) ;
#239889 = VERTEX_POINT ( 'NONE', #171000 ) ;
#239890 = AXIS2_PLACEMENT_3D ( 'NONE', #234800, #52284, #131842 ) ;
#239891 = AXIS2_PLACEMENT_3D ( 'NONE', #58910, #138452, #217990 ) ;
#239892 = ADVANCED_FACE ( 'NONE', ( #32761 ), #172277, .T. ) ;
#239893 = DIRECTION ( 'NONE',  ( 0.000000000000000000, -1.000000000000000000, -6.982962677686266711E-15 ) ) ;
#239895 = CARTESIAN_POINT ( 'NONE',  ( 21.05000000000000071, 76.00000000001126921, -203.5231074845248997 ) ) ;
#239894 = CARTESIAN_POINT ( 'NONE',  ( 21.14999999999999503, 12.62988036037871176, -223.4632815780722410 ) ) ;
#239896 = DIRECTION ( 'NONE',  ( 0.000000000000000000, -0.4088369013363276072, 0.9126074666063772600 ) ) ;
#239898 = ADVANCED_FACE ( 'NONE', ( #71865 ), #74317, .F. ) ;
#239897 = LINE ( 'NONE', #199498, #108132 ) ;
#239899 = DIRECTION ( 'NONE',  ( 1.000000000000000000, -0.000000000000000000, -0.000000000000000000 ) ) ;
#239900 = VERTEX_POINT ( 'NONE', #70597 ) ;
#239901 = DIRECTION ( 'NONE',  ( -3.265361837132813093E-16, 1.000000000000000000, 0.000000000000000000 ) ) ;
#239902 = ORIENTED_EDGE ( 'NONE', *, *, #68328, .T. ) ;
#239903 = EDGE_CURVE ( 'NONE', #175744, #142448, #230946, .T. ) ;
#239904 = DIRECTION ( 'NONE',  ( 0.000000000000000000, -1.000000000000000000, 0.000000000000000000 ) ) ;
#239905 = AXIS2_PLACEMENT_3D ( 'NONE', #182090, #157768, #35234 ) ;
#239906 = ORIENTED_EDGE ( 'NONE', *, *, #246009, .F. ) ;
#239907 = FACE_OUTER_BOUND ( 'NONE', #120396, .T. ) ;
#239908 = EDGE_CURVE ( 'NONE', #57514, #108723, #199173, .T. ) ;
#239909 = CIRCLE ( 'NONE', #77548, 0.1999999999999987899 ) ;
#239910 = B_SPLINE_CURVE_WITH_KNOTS ( 'NONE', 3,
 ( #145256, #142685, #87841, #188252, #46165, #167432 ),
 .UNSPECIFIED., .F., .F.,
 ( 4, 2, 4 ),
 ( 1.138412281109779656E-18, 0.0001569047307838639788, 0.0003138094615677267650 ),
 .UNSPECIFIED. ) ;
#239911 = DIRECTION ( 'NONE',  ( -1.652117596168391306E-15, -0.4721928772777346239, -0.8814952561688430555 ) ) ;
#239912 = EDGE_CURVE ( 'NONE', #206465, #7959, #3525, .T. ) ;
#239913 = VECTOR ( 'NONE', #178020, 1000.000000000000000 ) ;
#239914 = VERTEX_POINT ( 'NONE', #233508 ) ;
#239915 = PLANE ( 'NONE',  #85075 ) ;
#239916 = VERTEX_POINT ( 'NONE', #212654 ) ;
#239917 = DIRECTION ( 'NONE',  ( 2.952720810173289112E-16, 1.000000000000000000, 1.261617073437673512E-14 ) ) ;
#239918 = ADVANCED_FACE ( 'NONE', ( #96516 ), #120102, .T. ) ;
#239919 = DIRECTION ( 'NONE',  ( 1.000000000000000000, -0.000000000000000000, -0.000000000000000000 ) ) ;
#239920 = DIRECTION ( 'NONE',  ( 6.938893903907220489E-15, -0.9770955615653313941, -0.2128009952263603677 ) ) ;
#239921 = CARTESIAN_POINT ( 'NONE',  ( 18.59999999999999432, 77.16270174994990327, -94.92310748452430857 ) ) ;
#239922 = CARTESIAN_POINT ( 'NONE',  ( -20.54999999999999716, 1.115625160336667635E-11, -202.9999999999999716 ) ) ;
#239924 = CARTESIAN_POINT ( 'NONE',  ( 18.52643265882457868, 65.68026841930924320, -130.9725740131889893 ) ) ;
#239923 = DIRECTION ( 'NONE',  ( 1.000000000000000000, 7.136802563874199107E-16, 1.554319503706929991E-16 ) ) ;
#239925 = CARTESIAN_POINT ( 'NONE',  ( 18.59999999999999432, 1.261786168576181755, -108.5864989635455089 ) ) ;
#239927 = ORIENTED_EDGE ( 'NONE', *, *, #43147, .F. ) ;
#239926 = CARTESIAN_POINT ( 'NONE',  ( 20.87631937322877462, 65.52850496324631990, -128.9433616099437359 ) ) ;
#239929 = DIRECTION ( 'NONE',  ( -0.000000000000000000, 1.000000000000000000, 0.000000000000000000 ) ) ;
#239928 = CARTESIAN_POINT ( 'NONE',  ( -16.89081410710458542, 9.951318529858268036, -188.3544059198363527 ) ) ;
#239930 = EDGE_LOOP ( 'NONE', ( #28979, #11023, #92725, #156676, #95273, #65295, #105301, #141746, #76479, #249514, #100744, #32122, #59024, #54405, #170365, #141535, #150843, #22264 ) ) ;
#239932 = ORIENTED_EDGE ( 'NONE', *, *, #42350, .T. ) ;
#239931 = DIRECTION ( 'NONE',  ( 1.000000000000000000, 0.000000000000000000, 0.000000000000000000 ) ) ;
#239933 = VECTOR ( 'NONE', #193231, 1000.000000000000000 ) ;
#239934 = ORIENTED_EDGE ( 'NONE', *, *, #77872, .F. ) ;
#239935 = LINE ( 'NONE', #19602, #90724 ) ;
#239936 = DIRECTION ( 'NONE',  ( 0.000000000000000000, 0.000000000000000000, 1.000000000000000000 ) ) ;
#239937 = LINE ( 'NONE', #24760, #176535 ) ;
#239938 = ORIENTED_EDGE ( 'NONE', *, *, #250997, .T. ) ;
#239939 = LINE ( 'NONE', #116142, #254572 ) ;
#239940 = CARTESIAN_POINT ( 'NONE',  ( -23.25000000000000000, 47.66483718802935954, -241.7716698398223514 ) ) ;
#239941 = LINE ( 'NONE', #221621, #10659 ) ;
#239942 = CARTESIAN_POINT ( 'NONE',  ( -16.90202395485681919, 9.965944544562010066, -154.9030137212600096 ) ) ;
#239943 = CARTESIAN_POINT ( 'NONE',  ( -18.52643265882458579, 46.42459709376392851, -243.0752906381742662 ) ) ;
#239944 = B_SPLINE_CURVE_WITH_KNOTS ( 'NONE', 3,
 ( #149786, #91072, #92346, #109328 ),
 .UNSPECIFIED., .F., .F.,
 ( 4, 4 ),
 ( 0.000000000000000000, 7.713889350927600000E-05 ),
 .UNSPECIFIED. ) ;
#239946 = VECTOR ( 'NONE', #164506, 1000.000000000000000 ) ;
#239945 = SPHERICAL_SURFACE ( 'NONE', #185091, 0.1000000000000000056 ) ;
#239947 = EDGE_LOOP ( 'NONE', ( #86002, #161370, #239388, #101436 ) ) ;
#239948 = ORIENTED_EDGE ( 'NONE', *, *, #45645, .F. ) ;
#239949 = DIRECTION ( 'NONE',  ( 0.000000000000000000, 7.026728003956683390E-15, -1.000000000000000000 ) ) ;
#239950 = AXIS2_PLACEMENT_3D ( 'NONE', #58818, #61416, #123973 ) ;
#239951 = AXIS2_PLACEMENT_3D ( 'NONE', #136737, #18081, #118492 ) ;
#239952 = VERTEX_POINT ( 'NONE', #138209 ) ;
#239953 = FACE_OUTER_BOUND ( 'NONE', #174859, .T. ) ;
#239954 = ORIENTED_EDGE ( 'NONE', *, *, #9530, .F. ) ;
#239955 = SPHERICAL_SURFACE ( 'NONE', #1166, 0.1000000000000000056 ) ;
#239956 = EDGE_CURVE ( 'NONE', #101453, #38568, #20116, .T. ) ;
#239957 = DIRECTION ( 'NONE',  ( -1.000000000000000000, 0.000000000000000000, 0.000000000000000000 ) ) ;
#239958 = CARTESIAN_POINT ( 'NONE',  ( 20.94999999999999574, 10.47338541492405994, -175.0786544642485012 ) ) ;
#239959 = DIRECTION ( 'NONE',  ( 0.000000000000000000, 0.000000000000000000, -1.000000000000000000 ) ) ;
#239960 = DIRECTION ( 'NONE',  ( 0.000000000000000000, 0.000000000000000000, 1.000000000000000000 ) ) ;
#239961 = VERTEX_POINT ( 'NONE', #256843 ) ;
#239962 = DIRECTION ( 'NONE',  ( -1.000000000000000000, -0.000000000000000000, -0.000000000000000000 ) ) ;
#239963 = CARTESIAN_POINT ( 'NONE',  ( 23.15000000000000213, -11.64999999998883595, -97.50000000000004263 ) ) ;
#239965 = EDGE_CURVE ( 'NONE', #196244, #251858, #174850, .T. ) ;
#239964 = DIRECTION ( 'NONE',  ( -1.000000000000000000, 0.000000000000000000, 0.000000000000000000 ) ) ;
#239966 = ORIENTED_EDGE ( 'NONE', *, *, #4198, .F. ) ;
#239968 = CARTESIAN_POINT ( 'NONE',  ( 22.50000000000000000, 64.35042919246734527, -136.6231074845243825 ) ) ;
#239967 = FACE_OUTER_BOUND ( 'NONE', #213931, .T. ) ;
#239969 = VECTOR ( 'NONE', #50965, 1000.000000000000000 ) ;
#239970 = ORIENTED_EDGE ( 'NONE', *, *, #250118, .T. ) ;
#239973 = ORIENTED_EDGE ( 'NONE', *, *, #194158, .T. ) ;
#239972 = SPHERICAL_SURFACE ( 'NONE', #112793, 0.1000000000000000056 ) ;
#239971 = PLANE ( 'NONE',  #90650 ) ;
#239974 = EDGE_LOOP ( 'NONE', ( #244036, #127247, #114858, #116152, #9473 ) ) ;
#239975 = DIRECTION ( 'NONE',  ( 0.000000000000000000, 0.000000000000000000, -1.000000000000000000 ) ) ;
#239976 = AXIS2_PLACEMENT_3D ( 'NONE', #40181, #100091, #240920 ) ;
#239977 = DIRECTION ( 'NONE',  ( 0.000000000000000000, 0.000000000000000000, 1.000000000000000000 ) ) ;
#239978 = FACE_OUTER_BOUND ( 'NONE', #17300, .T. ) ;
#239979 = EDGE_LOOP ( 'NONE', ( #247503, #11268, #235100, #190585 ) ) ;
#239980 = CARTESIAN_POINT ( 'NONE',  ( 19.90621891164687440, 16.76439071345979315, -222.7593519876740231 ) ) ;
#239981 = CIRCLE ( 'NONE', #156622, 11.80000000000000071 ) ;
#239982 = DIRECTION ( 'NONE',  ( 1.000000000000000000, -0.000000000000000000, -0.000000000000000000 ) ) ;
#239983 = CIRCLE ( 'NONE', #244050, 0.1000000000000028644 ) ;
#239985 = DIRECTION ( 'NONE',  ( -1.000000000000000000, 1.335000415235278971E-16, -2.979993593738921214E-16 ) ) ;
#239984 = DIRECTION ( 'NONE',  ( 1.000000000000000000, 0.000000000000000000, 0.000000000000000000 ) ) ;
#239986 = AXIS2_PLACEMENT_3D ( 'NONE', #130355, #31308, #207354 ) ;
#239988 = ORIENTED_EDGE ( 'NONE', *, *, #251910, .T. ) ;
#239987 = DIRECTION ( 'NONE',  ( 0.000000000000000000, 7.086529944415894657E-15, -1.000000000000000000 ) ) ;
#239989 = ORIENTED_EDGE ( 'NONE', *, *, #103798, .F. ) ;
#239990 = VECTOR ( 'NONE', #247077, 1000.000000000000000 ) ;
#239991 = CARTESIAN_POINT ( 'NONE',  ( -16.89797118371642881, 44.04503171409839979, -235.3105451120472082 ) ) ;
#239992 = ORIENTED_EDGE ( 'NONE', *, *, #173006, .F. ) ;
#239994 = VECTOR ( 'NONE', #201606, 1000.000000000000000 ) ;
#239993 = DIRECTION ( 'NONE',  ( 0.000000000000000000, 0.9908441862701605762, 0.1350103645451835310 ) ) ;
#239995 = ORIENTED_EDGE ( 'NONE', *, *, #118147, .T. ) ;
#239996 = AXIS2_PLACEMENT_3D ( 'NONE', #148146, #50310, #126006 ) ;
#239997 = CARTESIAN_POINT ( 'NONE',  ( -21.59142135623730852, 68.15000000001155911, -57.27310748452437394 ) ) ;
#239998 = CARTESIAN_POINT ( 'NONE',  ( 22.45463910399147522, 76.00000000001291767, -114.6726782947074383 ) ) ;
#239999 = CARTESIAN_POINT ( 'NONE',  ( -18.40000000000000213, 31.01370428745238783, -233.5116043003366713 ) ) ;
#240001 = ORIENTED_EDGE ( 'NONE', *, *, #57912, .T. ) ;
#240000 = TOROIDAL_SURFACE ( 'NONE', #19223, 11.89999999999999858, 0.1000000000000000056 ) ;
#240002 = CARTESIAN_POINT ( 'NONE',  ( -21.05000000000000071, 76.00000000001237765, -170.0231074845243597 ) ) ;
#240003 = EDGE_CURVE ( 'NONE', #167398, #195967, #211839, .T. ) ;
#240004 = AXIS2_PLACEMENT_3D ( 'NONE', #117, #226530, #27110 ) ;
#240005 = CARTESIAN_POINT ( 'NONE',  ( -16.77683809663752257, 9.945835743215303282, -54.33605098089579855 ) ) ;
#240006 = ORIENTED_EDGE ( 'NONE', *, *, #213875, .T. ) ;
#240007 = EDGE_LOOP ( 'NONE', ( #197621, #244790, #160372, #159435, #8139 ) ) ;
#240008 = ORIENTED_EDGE ( 'NONE', *, *, #155862, .T. ) ;
#240009 = EDGE_CURVE ( 'NONE', #242569, #5530, #66073, .T. ) ;
#240010 = DIRECTION ( 'NONE',  ( 0.000000000000000000, 6.982962677686266711E-15, -1.000000000000000000 ) ) ;
#240011 = ORIENTED_EDGE ( 'NONE', *, *, #19629, .F. ) ;
#240013 = EDGE_LOOP ( 'NONE', ( #125742, #154588, #207583, #56890 ) ) ;
#240012 = CARTESIAN_POINT ( 'NONE',  ( 14.88075390448864077, 66.56831044948847875, -185.2438174522883685 ) ) ;
#240014 = EDGE_CURVE ( 'NONE', #5146, #192537, #117389, .T. ) ;
#240015 = ORIENTED_EDGE ( 'NONE', *, *, #27641, .T. ) ;
#240016 = AXIS2_PLACEMENT_3D ( 'NONE', #99791, #56810, #221040 ) ;
#240017 = VECTOR ( 'NONE', #67656, 999.9999999999998863 ) ;
#240020 = EDGE_LOOP ( 'NONE', ( #90389, #232331, #89861, #26158 ) ) ;
#240019 = ORIENTED_EDGE ( 'NONE', *, *, #196470, .F. ) ;
#240018 = CARTESIAN_POINT ( 'NONE',  ( -16.81095280782811230, 9.950000000011138823, -113.1499999999991672 ) ) ;
#240021 = CIRCLE ( 'NONE', #210782, 0.09999999999998898659 ) ;
#240022 = AXIS2_PLACEMENT_3D ( 'NONE', #44692, #87639, #223297 ) ;
#240024 = ADVANCED_FACE ( 'NONE', ( #195672 ), #56108, .T. ) ;
#240023 = ORIENTED_EDGE ( 'NONE', *, *, #45863, .T. ) ;
#240025 = DIRECTION ( 'NONE',  ( 1.000000000000000000, 0.000000000000000000, -0.000000000000000000 ) ) ;
#240026 = AXIS2_PLACEMENT_3D ( 'NONE', #123, #139624, #177536 ) ;
#240027 = CARTESIAN_POINT ( 'NONE',  ( -23.15000000000000213, 2.000000000011154189, -80.22462192276213955 ) ) ;
#240028 = ORIENTED_EDGE ( 'NONE', *, *, #42884, .F. ) ;
#240029 = DIRECTION ( 'NONE',  ( -0.000000000000000000, 1.000000000000000000, -0.000000000000000000 ) ) ;
#240031 = VERTEX_POINT ( 'NONE', #134364 ) ;
#240030 = CARTESIAN_POINT ( 'NONE',  ( -21.05000000000000071, 7.128833340093095217, -233.7327013124392749 ) ) ;
#240032 = CARTESIAN_POINT ( 'NONE',  ( 19.97071067811864609, 11.72071067812981404, -91.75000000000005684 ) ) ;
#240034 = ORIENTED_EDGE ( 'NONE', *, *, #95693, .T. ) ;
#240033 = CARTESIAN_POINT ( 'NONE',  ( -20.07928932188135107, 9.220710678129810489, -121.6500000000000341 ) ) ;
#240035 = EDGE_CURVE ( 'NONE', #19773, #91807, #18286, .T. ) ;
#240036 = AXIS2_PLACEMENT_3D ( 'NONE', #165033, #145456, #144163 ) ;
#240037 = ORIENTED_EDGE ( 'NONE', *, *, #105977, .F. ) ;
#240038 = CIRCLE ( 'NONE', #10909, 7.791421356237341556 ) ;
#240039 = DIRECTION ( 'NONE',  ( 1.000000000000000000, 3.190570557967288949E-16, 6.948722487160392945E-17 ) ) ;
#240040 = CARTESIAN_POINT ( 'NONE',  ( 18.46921299892755997, 85.50937817783569983, -96.03652877515386876 ) ) ;
#240041 = TOROIDAL_SURFACE ( 'NONE', #6803, 0.2000000000000000111, 0.1000000000000000056 ) ;
#240042 = VERTEX_POINT ( 'NONE', #19587 ) ;
#240043 = ORIENTED_EDGE ( 'NONE', *, *, #20376, .T. ) ;
#240044 = DIRECTION ( 'NONE',  ( 1.000000000000000000, 0.000000000000000000, -0.000000000000000000 ) ) ;
#240045 = CARTESIAN_POINT ( 'NONE',  ( 23.14999999999999503, 6.550000000011156231, -112.8500000000000369 ) ) ;
#240047 = ORIENTED_EDGE ( 'NONE', *, *, #160629, .T. ) ;
#240046 = ORIENTED_EDGE ( 'NONE', *, *, #37060, .F. ) ;
#240048 = ORIENTED_EDGE ( 'NONE', *, *, #144461, .T. ) ;
#240049 = CARTESIAN_POINT ( 'NONE',  ( -22.39999999999999858, 64.25313205997782973, -247.2214437328673853 ) ) ;
#240050 = ORIENTED_EDGE ( 'NONE', *, *, #14549, .F. ) ;
#240051 = VERTEX_POINT ( 'NONE', #97792 ) ;
#240052 = CARTESIAN_POINT ( 'NONE',  ( 23.14999999999999858, 10.74948822439028540, -222.3968794097801549 ) ) ;
#240053 = AXIS2_PLACEMENT_3D ( 'NONE', #205379, #5896, #188402 ) ;
#240054 = VERTEX_POINT ( 'NONE', #99082 ) ;
#240055 = DIRECTION ( 'NONE',  ( -1.000000000000000000, 0.000000000000000000, 0.000000000000000000 ) ) ;
#240056 = CARTESIAN_POINT ( 'NONE',  ( 18.46947024752531874, -9.509297157144976254, -107.4866894486978879 ) ) ;
#240057 = EDGE_CURVE ( 'NONE', #176291, #115527, #99383, .T. ) ;
#240058 = VERTEX_POINT ( 'NONE', #79523 ) ;
#240060 = ORIENTED_EDGE ( 'NONE', *, *, #10518, .F. ) ;
#240059 = VERTEX_POINT ( 'NONE', #75709 ) ;
#240061 = CARTESIAN_POINT ( 'NONE',  ( -20.54999999999999716, -9.399999999988846611, -57.10603087734755690 ) ) ;
#240062 = CARTESIAN_POINT ( 'NONE',  ( 20.46382478191415188, 10.59862044130854031, -175.1778144693454635 ) ) ;
#240063 = ORIENTED_EDGE ( 'NONE', *, *, #102294, .F. ) ;
#240064 = TOROIDAL_SURFACE ( 'NONE', #44439, 11.65000000000000036, 0.1000000000000000056 ) ;
#240065 = CIRCLE ( 'NONE', #111056, 12.87499999999999822 ) ;
#240066 = AXIS2_PLACEMENT_3D ( 'NONE', #9022, #105515, #110687 ) ;
#240067 = CIRCLE ( 'NONE', #69385, 11.80000000000000426 ) ;
#240068 = EDGE_CURVE ( 'NONE', #221119, #67538, #216589, .T. ) ;
#240069 = CARTESIAN_POINT ( 'NONE',  ( -0.8999999999999437339, 64.25000000001119815, -12.72310748452478890 ) ) ;
#240070 = ORIENTED_EDGE ( 'NONE', *, *, #186278, .F. ) ;
#240071 = ORIENTED_EDGE ( 'NONE', *, *, #31781, .F. ) ;
#240072 = CARTESIAN_POINT ( 'NONE',  ( -20.64999999999999858, 7.128833340094563376, -233.7327013124401276 ) ) ;
#240073 = ORIENTED_EDGE ( 'NONE', *, *, #51529, .F. ) ;
#240074 = FACE_OUTER_BOUND ( 'NONE', #196917, .T. ) ;
#240075 = DIRECTION ( 'NONE',  ( 0.000000000000000000, 0.000000000000000000, -1.000000000000000000 ) ) ;
#240076 = EDGE_LOOP ( 'NONE', ( #235113, #242586, #37380, #192710 ) ) ;
#240077 = DIRECTION ( 'NONE',  ( 1.000000000000000000, 0.000000000000000000, 0.000000000000000000 ) ) ;
#240079 = EDGE_CURVE ( 'NONE', #56972, #89706, #86714, .T. ) ;
#240078 = FACE_OUTER_BOUND ( 'NONE', #138046, .T. ) ;
#240081 = CARTESIAN_POINT ( 'NONE',  ( -16.80621392010910498, 9.942202577518919782, -121.3104080345830909 ) ) ;
#240080 = CARTESIAN_POINT ( 'NONE',  ( 20.98284271247461064, 6.322468214605803993, 12.11686199900910488 ) ) ;
#240082 = DIRECTION ( 'NONE',  ( 0.000000000000000000, 0.000000000000000000, -1.000000000000000000 ) ) ;
#240083 = LINE ( 'NONE', #39332, #94978 ) ;
#240084 = DIRECTION ( 'NONE',  ( 0.000000000000000000, 0.000000000000000000, 1.000000000000000000 ) ) ;
#240085 = CARTESIAN_POINT ( 'NONE',  ( 18.59999999999999076, 64.35000000001197407, -111.7731074845243739 ) ) ;
#240086 = DIRECTION ( 'NONE',  ( 1.000000000000000000, 0.000000000000000000, 0.000000000000000000 ) ) ;
#240087 = TOROIDAL_SURFACE ( 'NONE', #90207, 0.2000000000000000111, 0.1000000000000000056 ) ;
#240088 = EDGE_CURVE ( 'NONE', #32767, #70529, #178685, .T. ) ;
#240089 = AXIS2_PLACEMENT_3D ( 'NONE', #19486, #101541, #2461 ) ;
#240090 = ORIENTED_EDGE ( 'NONE', *, *, #28810, .T. ) ;
#240092 = ORIENTED_EDGE ( 'NONE', *, *, #49360, .T. ) ;
#240091 = EDGE_LOOP ( 'NONE', ( #216886, #80859, #208476, #168581 ) ) ;
#240093 = CIRCLE ( 'NONE', #40201, 11.79999999999999893 ) ;
#240094 = ORIENTED_EDGE ( 'NONE', *, *, #233302, .F. ) ;
#240095 = ORIENTED_EDGE ( 'NONE', *, *, #160438, .F. ) ;
#240096 = DIRECTION ( 'NONE',  ( 0.000000000000000000, 0.2617529984165031243, 0.9651348961777157509 ) ) ;
#240097 = EDGE_CURVE ( 'NONE', #111434, #52403, #148796, .T. ) ;
#240098 = FACE_OUTER_BOUND ( 'NONE', #117425, .T. ) ;
#240100 = DIRECTION ( 'NONE',  ( 0.000000000000000000, 0.2558827019434435912, -0.9667078373770033872 ) ) ;
#240099 = DIRECTION ( 'NONE',  ( -1.000000000000000000, 1.207181226542539700E-16, -2.694675058168174199E-16 ) ) ;
#240101 = CARTESIAN_POINT ( 'NONE',  ( -23.15000000000000213, 67.23127455305841238, -235.8551265064783991 ) ) ;
#240102 = VERTEX_POINT ( 'NONE', #114820 ) ;
#240103 = EDGE_CURVE ( 'NONE', #20419, #50994, #15757, .T. ) ;
#240104 = CARTESIAN_POINT ( 'NONE',  ( -20.91682497891422798, 10.32263460347359363, -106.0605957968672328 ) ) ;
#240105 = FILL_AREA_STYLE ('',( #200968 ) ) ;
#240106 = ADVANCED_FACE ( 'NONE', ( #202067 ), #138134, .F. ) ;
#240107 = CARTESIAN_POINT ( 'NONE',  ( -18.59999999999999787, 1.866714910068465239, -78.75267524628205251 ) ) ;
#240108 = DIRECTION ( 'NONE',  ( 0.000000000000000000, 6.938893903907222067E-15, -1.000000000000000000 ) ) ;
#240109 = DIRECTION ( 'NONE',  ( 0.000000000000000000, -0.8660254037844384856, 0.5000000000000002220 ) ) ;
#240110 = ORIENTED_EDGE ( 'NONE', *, *, #112399, .T. ) ;
#240111 = CIRCLE ( 'NONE', #190224, 0.3999999999999975797 ) ;
#240112 = DIRECTION ( 'NONE',  ( 1.000000000000000000, 0.000000000000000000, 0.000000000000000000 ) ) ;
#240113 = EDGE_CURVE ( 'NONE', #74012, #211698, #241206, .T. ) ;
#240114 = CARTESIAN_POINT ( 'NONE',  ( -20.54999999999999716, -9.400000000000002132, -23.60603087734756045 ) ) ;
#240115 = EDGE_LOOP ( 'NONE', ( #81361, #157089, #32005, #211086 ) ) ;
#240116 = CARTESIAN_POINT ( 'NONE',  ( -16.89268316805466341, 66.04827818676939444, -56.87885996306994230 ) ) ;
#240117 = CARTESIAN_POINT ( 'NONE',  ( -20.94999999999999929, 74.83729825007431202, -161.9231074845243654 ) ) ;
#240118 = EDGE_CURVE ( 'NONE', #63545, #170195, #111893, .T. ) ;
#240119 = LINE ( 'NONE', #101854, #160206 ) ;
#240120 = PLANE ( 'NONE',  #210853 ) ;
#240121 = EDGE_CURVE ( 'NONE', #234687, #48376, #236750, .T. ) ;
#240122 = DIRECTION ( 'NONE',  ( 0.000000000000000000, 1.776356839400250465E-15, -1.000000000000000000 ) ) ;
#240123 = ORIENTED_EDGE ( 'NONE', *, *, #96442, .F. ) ;
#240124 = CARTESIAN_POINT ( 'NONE',  ( -20.00857864376270001, 9.150000000011157653, -121.6500000000000341 ) ) ;
#240125 = FACE_OUTER_BOUND ( 'NONE', #121377, .T. ) ;
#240126 = CARTESIAN_POINT ( 'NONE',  ( -21.37071067811865532, 8.070710678129811910, -146.2500000000000284 ) ) ;
#240128 = DIRECTION ( 'NONE',  ( -1.000000000000000000, 0.000000000000000000, 0.000000000000000000 ) ) ;
#240127 = LINE ( 'NONE', #124034, #186706 ) ;
#240129 = CARTESIAN_POINT ( 'NONE',  ( -21.05000000000000071, 76.00000000001234923, -165.7231074845244052 ) ) ;
#240130 = VECTOR ( 'NONE', #196252, 1000.000000000000000 ) ;
#240131 = CARTESIAN_POINT ( 'NONE',  ( 23.14999999999999503, 6.649999999999999467, -12.25000000000000000 ) ) ;
#240132 = CARTESIAN_POINT ( 'NONE',  ( 18.49999999999998934, 6.550000000000000711, -21.25000000000000000 ) ) ;
#240133 = CARTESIAN_POINT ( 'NONE',  ( 23.14999999999999858, 65.07363471106805264, -222.4165545841253220 ) ) ;
#240134 = AXIS2_PLACEMENT_3D ( 'NONE', #245200, #104368, #84794 ) ;
#240136 = ORIENTED_EDGE ( 'NONE', *, *, #25859, .T. ) ;
#240135 = CARTESIAN_POINT ( 'NONE',  ( 18.59999999999999787, 4.288595810029049993, -211.9930862808554934 ) ) ;
#240137 = VECTOR ( 'NONE', #57862, 1000.000000000000000 ) ;
#240138 = EDGE_LOOP ( 'NONE', ( #83683, #24036, #243129, #83165 ) ) ;
#240139 = EDGE_CURVE ( 'NONE', #203538, #60331, #232527, .T. ) ;
#240140 = EDGE_CURVE ( 'NONE', #246415, #83828, #23459, .T. ) ;
#240141 = CARTESIAN_POINT ( 'NONE',  ( -20.94999999999999929, 56.28322105926037722, -227.9393116591656963 ) ) ;
#240142 = CARTESIAN_POINT ( 'NONE',  ( 20.73486653747088582, 18.70606281991848974, -231.7096448200341854 ) ) ;
#240143 = EDGE_CURVE ( 'NONE', #129914, #169303, #1335, .T. ) ;
#240144 = CARTESIAN_POINT ( 'NONE',  ( 22.01447462590973103, 65.23436900571785202, -242.8397503278283125 ) ) ;
#240145 = DIRECTION ( 'NONE',  ( 0.000000000000000000, 0.2128009952263403282, -0.9770955615653358350 ) ) ;
#240146 = AXIS2_PLACEMENT_3D ( 'NONE', #167387, #227327, #29175 ) ;
#240147 = ORIENTED_EDGE ( 'NONE', *, *, #52880, .T. ) ;
#240148 = CARTESIAN_POINT ( 'NONE',  ( 23.14999999999999858, 4.813084112160684214, -122.0584822434762060 ) ) ;
#240149 = CIRCLE ( 'NONE', #61062, 0.1000000000000028644 ) ;
#240150 = CARTESIAN_POINT ( 'NONE',  ( -21.44999999999999929, 7.250000000011155521, -155.1500000000000057 ) ) ;
#240151 = DIRECTION ( 'NONE',  ( 0.000000000000000000, 1.953992523340277404E-14, 1.000000000000000000 ) ) ;
#240152 = AXIS2_PLACEMENT_3D ( 'NONE', #228862, #249708, #211881 ) ;
#240153 = FACE_OUTER_BOUND ( 'NONE', #71837, .T. ) ;
#240156 = ORIENTED_EDGE ( 'NONE', *, *, #58020, .T. ) ;
#240155 = CARTESIAN_POINT ( 'NONE',  ( 20.73486653747088226, 68.75000000001203659, -123.8731074845243540 ) ) ;
#240154 = AXIS2_PLACEMENT_3D ( 'NONE', #63850, #208515, #207225 ) ;
#240158 = CYLINDRICAL_SURFACE ( 'NONE', #121121, 0.1000000000000052097 ) ;
#240157 = DIRECTION ( 'NONE',  ( 1.000000000000000000, 0.000000000000000000, 0.000000000000000000 ) ) ;
#240159 = CARTESIAN_POINT ( 'NONE',  ( 23.14999999999999858, 67.23127455305841238, -235.8551265064783991 ) ) ;
#240160 = AXIS2_PLACEMENT_3D ( 'NONE', #171668, #73847, #95926 ) ;
#240161 = CARTESIAN_POINT ( 'NONE',  ( -18.50000000000000000, 77.86671491006887891, -57.77043223824230722 ) ) ;
#240163 = ORIENTED_EDGE ( 'NONE', *, *, #56740, .F. ) ;
#240162 = AXIS2_PLACEMENT_3D ( 'NONE', #100829, #37085, #1760 ) ;
#240164 = ADVANCED_FACE ( 'NONE', ( #6420 ), #41726, .F. ) ;
#240165 = CARTESIAN_POINT ( 'NONE',  ( 0.000000000000000000, 0.000000000000000000, 0.000000000000000000 ) ) ;
#240166 = DIRECTION ( 'NONE',  ( 1.000000000000000000, 0.000000000000000000, 0.000000000000000000 ) ) ;
#240167 = CARTESIAN_POINT ( 'NONE',  ( 18.59999999999999076, 65.79142135624927334, -111.7731074845243739 ) ) ;
#240168 = ORIENTED_EDGE ( 'NONE', *, *, #11765, .F. ) ;
#240170 = EDGE_CURVE ( 'NONE', #178668, #204747, #153426, .T. ) ;
#240169 = LINE ( 'NONE', #181487, #71049 ) ;
#240171 = CARTESIAN_POINT ( 'NONE',  ( -16.88005004766534967, 66.04989949669150917, -182.6727713725756530 ) ) ;
#240172 = VERTEX_POINT ( 'NONE', #140808 ) ;
#240173 = AXIS2_PLACEMENT_3D ( 'NONE', #157005, #39638, #233949 ) ;
#240174 = DIRECTION ( 'NONE',  ( 0.000000000000000000, 1.000000000000000000, -5.551115123125777653E-14 ) ) ;
#240175 = AXIS2_PLACEMENT_3D ( 'NONE', #198732, #256076, #257359 ) ;
#240176 = AXIS2_PLACEMENT_3D ( 'NONE', #209400, #30795, #12514 ) ;
#240177 = DIRECTION ( 'NONE',  ( 0.000000000000000000, 0.000000000000000000, -1.000000000000000000 ) ) ;
#240178 = EDGE_CURVE ( 'NONE', #78259, #29887, #162957, .T. ) ;
#240179 = FACE_OUTER_BOUND ( 'NONE', #4035, .T. ) ;
#240180 = ORIENTED_EDGE ( 'NONE', *, *, #152785, .T. ) ;
#240181 = EDGE_LOOP ( 'NONE', ( #49833, #138323, #192849, #180801 ) ) ;
#240182 = EDGE_CURVE ( 'NONE', #105588, #54007, #45556, .T. ) ;
#240183 = CARTESIAN_POINT ( 'NONE',  ( -21.12642695952773764, 69.62434007797678248, -103.1220107677137179 ) ) ;
#240184 = CYLINDRICAL_SURFACE ( 'NONE', #110857, 4.000000000000003553 ) ;
#240185 = PLANE ( 'NONE',  #61913 ) ;
#240186 = FACE_OUTER_BOUND ( 'NONE', #198482, .T. ) ;
#240187 = EDGE_CURVE ( 'NONE', #186897, #128325, #253336, .T. ) ;
#240188 = AXIS2_PLACEMENT_3D ( 'NONE', #49203, #29675, #10079 ) ;
#240190 = CARTESIAN_POINT ( 'NONE',  ( 20.95512820512820440, 10.62384868371188062, -12.15000000000000036 ) ) ;
#240189 = DIRECTION ( 'NONE',  ( 0.000000000000000000, 0.4721928772777346239, 0.8814952561688430555 ) ) ;
#240191 = DIRECTION ( 'NONE',  ( 1.000000000000000000, 0.000000000000000000, 0.000000000000000000 ) ) ;
#240192 = DIRECTION ( 'NONE',  ( -0.000000000000000000, -1.000000000000000000, -0.000000000000000000 ) ) ;
#240193 = CARTESIAN_POINT ( 'NONE',  ( -17.11825945287481332, 65.95000000001201101, -115.6731074845243796 ) ) ;
#240194 = ORIENTED_EDGE ( 'NONE', *, *, #197493, .T. ) ;
#240195 = FACE_OUTER_BOUND ( 'NONE', #229765, .T. ) ;
#240196 = ADVANCED_FACE ( 'NONE', ( #199517 ), #219042, .T. ) ;
#240197 = EDGE_LOOP ( 'NONE', ( #244582, #132262, #44994, #146745 ) ) ;
#240198 = FACE_OUTER_BOUND ( 'NONE', #218023, .T. ) ;
#240200 = EDGE_CURVE ( 'NONE', #166243, #195496, #37073, .T. ) ;
#240199 = EDGE_CURVE ( 'NONE', #180506, #253291, #195100, .T. ) ;
#240201 = CARTESIAN_POINT ( 'NONE',  ( 22.50000000000000000, 11.36146383068193444, -198.4232501820394816 ) ) ;
#240203 = FACE_OUTER_BOUND ( 'NONE', #2254, .T. ) ;
#240202 = DIRECTION ( 'NONE',  ( 0.000000000000000000, -6.982962677686266711E-15, 1.000000000000000000 ) ) ;
#240204 = ORIENTED_EDGE ( 'NONE', *, *, #65192, .T. ) ;
#240206 = DIRECTION ( 'NONE',  ( 0.000000000000000000, 0.000000000000000000, -1.000000000000000000 ) ) ;
#240205 = CARTESIAN_POINT ( 'NONE',  ( -16.83233564386412340, 66.06977820342686414, -56.74762814800010347 ) ) ;
#240207 = FACE_OUTER_BOUND ( 'NONE', #158741, .T. ) ;
#240208 = CARTESIAN_POINT ( 'NONE',  ( -18.40000000000000213, 67.23581240663841641, -214.2531594801197627 ) ) ;
#240209 = CARTESIAN_POINT ( 'NONE',  ( -23.25000000000000000, 69.25640205380744874, -247.7135141964517402 ) ) ;
#240210 = CARTESIAN_POINT ( 'NONE',  ( -15.66061380678751647, 66.63927620602653690, -186.2091802899176969 ) ) ;
#240211 = ORIENTED_EDGE ( 'NONE', *, *, #248670, .F. ) ;
#240212 = DIRECTION ( 'NONE',  ( 0.000000000000000000, 0.000000000000000000, -1.000000000000000000 ) ) ;
#240213 = AXIS2_PLACEMENT_3D ( 'NONE', #98195, #18699, #136049 ) ;
#240214 = ORIENTED_EDGE ( 'NONE', *, *, #107499, .F. ) ;
#240215 = AXIS2_PLACEMENT_3D ( 'NONE', #175553, #254996, #78961 ) ;
#240216 = VECTOR ( 'NONE', #244242, 1000.000000000000000 ) ;
#240217 = CIRCLE ( 'NONE', #77867, 0.3999999999999952482 ) ;
#240218 = DIRECTION ( 'NONE',  ( 0.000000000000000000, 0.000000000000000000, 1.000000000000000000 ) ) ;
#240219 = ORIENTED_EDGE ( 'NONE', *, *, #241675, .F. ) ;
#240220 = DIRECTION ( 'NONE',  ( -3.265361837132813093E-16, -1.000000000000000000, 7.445645354460596589E-46 ) ) ;
#240221 = EDGE_CURVE ( 'NONE', #83713, #75451, #88501, .T. ) ;
#240222 = EDGE_CURVE ( 'NONE', #196293, #249408, #110662, .T. ) ;
#240223 = ORIENTED_EDGE ( 'NONE', *, *, #40307, .T. ) ;
#240224 = TOROIDAL_SURFACE ( 'NONE', #227708, 0.4000000000000012990, 0.1000000000000000056 ) ;
#240225 = LINE ( 'NONE', #143664, #64530 ) ;
#240226 = EDGE_CURVE ( 'NONE', #233724, #243788, #208503, .T. ) ;
#240227 = CARTESIAN_POINT ( 'NONE',  ( 20.85000000000000142, 77.16412189325286874, -61.60825939895269698 ) ) ;
#240228 = EDGE_LOOP ( 'NONE', ( #211104, #8826, #87010, #15629 ) ) ;
#240229 = EDGE_CURVE ( 'NONE', #119487, #64202, #149813, .T. ) ;
#240230 = CARTESIAN_POINT ( 'NONE',  ( -16.89268316805465986, 66.04827818676982076, -115.6673550059788340 ) ) ;
#240232 = AXIS2_PLACEMENT_3D ( 'NONE', #171285, #92970, #194679 ) ;
#240231 = DIRECTION ( 'NONE',  ( -1.000000000000000000, 0.000000000000000000, 0.000000000000000000 ) ) ;
#240233 = ADVANCED_FACE ( 'NONE', ( #205904 ), #89799, .F. ) ;
#240234 = CARTESIAN_POINT ( 'NONE',  ( 21.05000000000000071, 11.75000000001115907, -160.6583993101029364 ) ) ;
#240235 = VECTOR ( 'NONE', #252684, 1000.000000000000000 ) ;
#240236 = DIRECTION ( 'NONE',  ( -1.000000000000000000, -0.000000000000000000, -0.000000000000000000 ) ) ;
#240237 = DIRECTION ( 'NONE',  ( 0.000000000000000000, 0.8814952561688476074, -0.4721928772777262417 ) ) ;
#240238 = CARTESIAN_POINT ( 'NONE',  ( 13.22261339317536866, 62.09660346237240702, -218.7363060264990509 ) ) ;
#240239 = ORIENTED_EDGE ( 'NONE', *, *, #82692, .F. ) ;
#240240 = DIRECTION ( 'NONE',  ( 1.000000000000000000, -0.000000000000000000, -0.000000000000000000 ) ) ;
#240241 = VERTEX_POINT ( 'NONE', #8994 ) ;
#240243 = ORIENTED_EDGE ( 'NONE', *, *, #7344, .F. ) ;
#240242 = CARTESIAN_POINT ( 'NONE',  ( -18.59999999999999787, 31.36165455396662693, -233.4973802202241302 ) ) ;
#240244 = ORIENTED_EDGE ( 'NONE', *, *, #109488, .T. ) ;
#240245 = CARTESIAN_POINT ( 'NONE',  ( -18.59999999999999787, 11.75000000001115552, -54.75000000000000000 ) ) ;
#240246 = CARTESIAN_POINT ( 'NONE',  ( 23.14999999999998437, 76.00000000001165290, -69.52310748452431710 ) ) ;
#240247 = DIRECTION ( 'NONE',  ( -1.000000000000000000, 0.000000000000000000, 0.000000000000000000 ) ) ;
#240248 = CARTESIAN_POINT ( 'NONE',  ( -21.12642695952773764, 61.05201444521252796, -234.2817334149543456 ) ) ;
#240249 = ORIENTED_EDGE ( 'NONE', *, *, #169830, .T. ) ;
#240250 = EDGE_CURVE ( 'NONE', #235787, #192532, #171961, .T. ) ;
#240251 = ADVANCED_FACE ( 'NONE', ( #225452 ), #51945, .T. ) ;
#240252 = DIRECTION ( 'NONE',  ( -0.000000000000000000, 1.000000000000000000, 7.272083257015735086E-15 ) ) ;
#240253 = DIRECTION ( 'NONE',  ( 1.000000000000000000, 0.000000000000000000, 0.000000000000000000 ) ) ;
#240254 = ORIENTED_EDGE ( 'NONE', *, *, #159489, .F. ) ;
#240255 = LINE ( 'NONE', #238969, #60791 ) ;
#240256 = EDGE_CURVE ( 'NONE', #61925, #14880, #169791, .T. ) ;
#240257 = DIRECTION ( 'NONE',  ( -1.836970198721029934E-16, 1.000000000000000000, 0.000000000000000000 ) ) ;
#240258 = AXIS2_PLACEMENT_3D ( 'NONE', #107031, #184012, #24972 ) ;
#240259 = ORIENTED_EDGE ( 'NONE', *, *, #46193, .T. ) ;
#240260 = AXIS2_PLACEMENT_3D ( 'NONE', #23973, #44802, #124342 ) ;
#240261 = CARTESIAN_POINT ( 'NONE',  ( -23.25000000000000000, -11.64999999998884483, -197.8999999999999773 ) ) ;
#240262 = VECTOR ( 'NONE', #120658, 1000.000000000000000 ) ;
#240263 = AXIS2_PLACEMENT_3D ( 'NONE', #67905, #28837, #6641 ) ;
#240264 = CARTESIAN_POINT ( 'NONE',  ( -21.55000000000000426, 68.29142135624960019, -157.6731074845243938 ) ) ;
#240265 = EDGE_LOOP ( 'NONE', ( #66781, #251516, #247459, #218459, #147085, #91453, #69420, #252159, #27873, #132804, #166022 ) ) ;
#240266 = DIRECTION ( 'NONE',  ( 0.000000000000000000, 0.000000000000000000, 1.000000000000000000 ) ) ;
#240267 = ADVANCED_FACE ( 'NONE', ( #147219 ), #106798, .T. ) ;
#240268 = DIRECTION ( 'NONE',  ( 1.000000000000000000, 0.000000000000000000, -0.000000000000000000 ) ) ;
#240269 = DIRECTION ( 'NONE',  ( 1.000000000000000000, -3.265361837132813093E-16, -2.280189983783949500E-30 ) ) ;
#240270 = LINE ( 'NONE', #77315, #46990 ) ;
#240271 = CIRCLE ( 'NONE', #23811, 0.5000000000000008882 ) ;
#240272 = VECTOR ( 'NONE', #94840, 1000.000000000000000 ) ;
#240273 = TOROIDAL_SURFACE ( 'NONE', #215311, 0.2000000000000000111, 0.1000000000000000056 ) ;
#240274 = DIRECTION ( 'NONE',  ( 0.000000000000000000, 0.000000000000000000, 1.000000000000000000 ) ) ;
#240275 = EDGE_CURVE ( 'NONE', #219487, #157474, #87229, .T. ) ;
#240276 = ORIENTED_EDGE ( 'NONE', *, *, #127837, .T. ) ;
#240277 = CARTESIAN_POINT ( 'NONE',  ( -18.39999999999999858, 64.52132590001281187, -127.2484142681837227 ) ) ;
#240278 = AXIS2_PLACEMENT_3D ( 'NONE', #200175, #81466, #220999 ) ;
#240279 = ORIENTED_EDGE ( 'NONE', *, *, #68486, .T. ) ;
#240281 = B_SPLINE_CURVE_WITH_KNOTS ( 'NONE', 3,
 ( #252171, #73581, #153131, #14883, #96924, #94383, #134781, #232647, #176519, #76110 ),
 .UNSPECIFIED., .F., .F.,
 ( 4, 3, 3, 4 ),
 ( 0.000000000000000000, 0.0002000000000008536833, 0.001000000000082972495, 0.001967863649483319807 ),
 .UNSPECIFIED. ) ;
#240280 = CARTESIAN_POINT ( 'NONE',  ( 18.69999999999999574, 6.742993295648862961, 9.658650260582458458 ) ) ;
#240282 = CARTESIAN_POINT ( 'NONE',  ( -23.15000000000000213, 1.999999999999998224, -20.27537807723789953 ) ) ;
#240284 = ORIENTED_EDGE ( 'NONE', *, *, #195970, .F. ) ;
#240283 = CARTESIAN_POINT ( 'NONE',  ( 21.11344571971254069, 10.61787902352924817, -146.2460208924022425 ) ) ;
#240285 = CARTESIAN_POINT ( 'NONE',  ( 21.12400222705960928, 67.22148809293440763, -57.27310748452438105 ) ) ;
#240286 = DIRECTION ( 'NONE',  ( 0.000000000000000000, 0.9654727137038715545, -0.2605042016806676242 ) ) ;
#240287 = PLANE ( 'NONE',  #125618 ) ;
#240288 = CYLINDRICAL_SURFACE ( 'NONE', #14635, 0.09999999999999939493 ) ;
#240289 = CARTESIAN_POINT ( 'NONE',  ( 23.14999999999999503, 64.25000000001253397, -182.1731074845244507 ) ) ;
#240290 = DIRECTION ( 'NONE',  ( 0.000000000000000000, 0.9770955615653316162, 0.2128009952263604232 ) ) ;
#240292 = EDGE_LOOP ( 'NONE', ( #149842, #143740, #220665, #225260 ) ) ;
#240291 = DIRECTION ( 'NONE',  ( 0.000000000000000000, 0.000000000000000000, 1.000000000000000000 ) ) ;
#240293 = AXIS2_PLACEMENT_3D ( 'NONE', #25216, #86420, #126867 ) ;
#240294 = DIRECTION ( 'NONE',  ( 1.000000000000000000, 0.000000000000000000, -0.000000000000000000 ) ) ;
#240295 = EDGE_LOOP ( 'NONE', ( #153030, #193328, #164384, #76944 ) ) ;
#240296 = ORIENTED_EDGE ( 'NONE', *, *, #197316, .T. ) ;
#240297 = CARTESIAN_POINT ( 'NONE',  ( -18.40904629823846861, 85.50000000001168132, -62.92291792204296286 ) ) ;
#240298 = DIRECTION ( 'NONE',  ( 0.7071067811865474617, 0.7071067811865474617, 0.000000000000000000 ) ) ;
#240299 = CIRCLE ( 'NONE', #256798, 11.64999999999999325 ) ;
#240300 = ORIENTED_EDGE ( 'NONE', *, *, #5406, .T. ) ;
#240301 = CYLINDRICAL_SURFACE ( 'NONE', #170958, 0.1000000000000028644 ) ;
#240302 = EDGE_CURVE ( 'NONE', #59204, #41196, #3719, .T. ) ;
#240303 = FILL_AREA_STYLE ('',( #57781 ) ) ;
#240304 = CIRCLE ( 'NONE', #82040, 7.900000000000009237 ) ;
#240305 = ORIENTED_EDGE ( 'NONE', *, *, #171624, .F. ) ;
#240306 = AXIS2_PLACEMENT_3D ( 'NONE', #11280, #169107, #187360 ) ;
#240307 = AXIS2_PLACEMENT_3D ( 'NONE', #141273, #138666, #39640 ) ;
#240308 = DIRECTION ( 'NONE',  ( 0.000000000000000000, 0.000000000000000000, -1.000000000000000000 ) ) ;
#240309 = LINE ( 'NONE', #220737, #113858 ) ;
#240310 = DIRECTION ( 'NONE',  ( 0.000000000000000000, -6.454785026890406770E-15, 1.000000000000000000 ) ) ;
#240311 = ORIENTED_EDGE ( 'NONE', *, *, #132678, .F. ) ;
#240312 = ORIENTED_EDGE ( 'NONE', *, *, #161270, .F. ) ;
#240314 = CARTESIAN_POINT ( 'NONE',  ( -18.50000000000000000, 77.13501884592155022, -28.30613060109199353 ) ) ;
#240313 = CIRCLE ( 'NONE', #107021, 11.79999999999999361 ) ;
#240315 = EDGE_LOOP ( 'NONE', ( #86649, #49016, #200181, #87875 ) ) ;
#240316 = EDGE_CURVE ( 'NONE', #94099, #5925, #49408, .T. ) ;
#240317 = CARTESIAN_POINT ( 'NONE',  ( -20.94999999999999929, 70.47363787294415260, -228.3418745167492432 ) ) ;
#240318 = CIRCLE ( 'NONE', #244398, 0.1000000000000007133 ) ;
#240319 = ORIENTED_EDGE ( 'NONE', *, *, #231012, .F. ) ;
#240321 = ORIENTED_EDGE ( 'NONE', *, *, #30312, .T. ) ;
#240320 = CARTESIAN_POINT ( 'NONE',  ( -23.15000000000000213, 76.00000000001126921, -203.5231074845248997 ) ) ;
#240323 = ADVANCED_FACE ( 'NONE', ( #226750 ), #28615, .F. ) ;
#240322 = LINE ( 'NONE', #163352, #156847 ) ;
#240324 = ORIENTED_EDGE ( 'NONE', *, *, #244203, .T. ) ;
#240325 = CARTESIAN_POINT ( 'NONE',  ( -20.64999999999999858, 0.000000000000000000, -35.40000000000000568 ) ) ;
#240326 = VERTEX_POINT ( 'NONE', #250179 ) ;
#240328 = ORIENTED_EDGE ( 'NONE', *, *, #458, .T. ) ;
#240327 = ORIENTED_EDGE ( 'NONE', *, *, #51696, .T. ) ;
#240329 = DIRECTION ( 'NONE',  ( 0.000000000000000000, -0.1335171055202867274, 0.9910465087640866200 ) ) ;
#240330 = CARTESIAN_POINT ( 'NONE',  ( -20.85000000000000142, 56.23643450586806836, -227.9054833905874489 ) ) ;
#240333 = ADVANCED_FACE ( 'NONE', ( #48116 ), #50662, .F. ) ;
#240332 = ORIENTED_EDGE ( 'NONE', *, *, #13488, .F. ) ;
#240331 = AXIS2_PLACEMENT_3D ( 'NONE', #249170, #49671, #47081 ) ;
#240334 = CIRCLE ( 'NONE', #165309, 3.899999999999999467 ) ;
#240335 = EDGE_CURVE ( 'NONE', #138313, #217847, #31168, .T. ) ;
#240336 = VECTOR ( 'NONE', #221805, 1000.000000000000000 ) ;
#240337 = EDGE_CURVE ( 'NONE', #92883, #224679, #127668, .T. ) ;
#240338 = ORIENTED_EDGE ( 'NONE', *, *, #113195, .T. ) ;
#240339 = CIRCLE ( 'NONE', #227849, 11.80000000000000249 ) ;
#240340 = CARTESIAN_POINT ( 'NONE',  ( 13.99999999999999822, 9.849999999999981881, -16.74999999999999645 ) ) ;
#240341 = DIRECTION ( 'NONE',  ( -0.000000000000000000, 1.000000000000000000, 6.982962677686266711E-15 ) ) ;
#240343 = EDGE_LOOP ( 'NONE', ( #5520, #153223, #228934, #92073, #213363 ) ) ;
#240342 = DIRECTION ( 'NONE',  ( -2.940209281316621016E-16, 1.000000000000000000, -8.881784197001251337E-16 ) ) ;
#240344 = DIRECTION ( 'NONE',  ( 0.000000000000000000, 0.2617529984162567103, 0.9651348961777825863 ) ) ;
#240345 = ORIENTED_EDGE ( 'NONE', *, *, #95561, .F. ) ;
#240346 = VECTOR ( 'NONE', #10970, 1000.000000000000000 ) ;
#240347 = EDGE_CURVE ( 'NONE', #199876, #165019, #170364, .T. ) ;
#240348 = CARTESIAN_POINT ( 'NONE',  ( 20.85000000000000142, 76.00000000001244871, -170.0231074845243597 ) ) ;
#240349 = DIRECTION ( 'NONE',  ( -0.000000000000000000, -1.000000000000000000, -6.982962677686266711E-15 ) ) ;
#240350 = ORIENTED_EDGE ( 'NONE', *, *, #183969, .T. ) ;
#240351 = DIRECTION ( 'NONE',  ( -0.000000000000000000, 1.000000000000000000, 8.717686153663073805E-15 ) ) ;
#240352 = DIRECTION ( 'NONE',  ( 0.000000000000000000, 0.000000000000000000, -1.000000000000000000 ) ) ;
#240353 = DIRECTION ( 'NONE',  ( 0.000000000000000000, 0.000000000000000000, -1.000000000000000000 ) ) ;
#240354 = ADVANCED_FACE ( 'NONE', ( #134061 ), #163296, .F. ) ;
#240355 = ORIENTED_EDGE ( 'NONE', *, *, #36179, .F. ) ;
#240356 = FACE_OUTER_BOUND ( 'NONE', #184270, .T. ) ;
#240357 = ORIENTED_EDGE ( 'NONE', *, *, #224535, .T. ) ;
#240358 = ORIENTED_EDGE ( 'NONE', *, *, #214933, .T. ) ;
#240359 = CIRCLE ( 'NONE', #186177, 4.050000000000022915 ) ;
#240360 = VECTOR ( 'NONE', #186265, 1000.000000000000000 ) ;
#240361 = ORIENTED_EDGE ( 'NONE', *, *, #254041, .F. ) ;
#240362 = EDGE_LOOP ( 'NONE', ( #211483, #164354, #200608, #143680 ) ) ;
#240363 = VERTEX_POINT ( 'NONE', #217436 ) ;
#240364 = EDGE_LOOP ( 'NONE', ( #19468, #43028, #256704, #109229, #179629 ) ) ;
#240365 = DIRECTION ( 'NONE',  ( 1.224646799147353207E-16, 1.000000000000000000, 0.000000000000000000 ) ) ;
#240366 = CARTESIAN_POINT ( 'NONE',  ( 23.24999999999999289, 11.75000000000000711, -0.1000000000000028644 ) ) ;
#240367 = ADVANCED_FACE ( 'NONE', ( #174544 ), #154951, .T. ) ;
#240368 = ORIENTED_EDGE ( 'NONE', *, *, #139781, .F. ) ;
#240369 = CIRCLE ( 'NONE', #207045, 0.1000000000000028644 ) ;
#240370 = ORIENTED_EDGE ( 'NONE', *, *, #105663, .F. ) ;
#240371 = VERTEX_POINT ( 'NONE', #36282 ) ;
#240372 = VECTOR ( 'NONE', #93451, 1000.000000000000000 ) ;
#240373 = EDGE_CURVE ( 'NONE', #183417, #247150, #174475, .T. ) ;
#240374 = CARTESIAN_POINT ( 'NONE',  ( -18.59999999999999787, 77.16270174995034381, -161.9231074845243370 ) ) ;
#240375 = FACE_OUTER_BOUND ( 'NONE', #30820, .T. ) ;
#240376 = DIRECTION ( 'NONE',  ( -0.000000000000000000, -6.982962677686266711E-15, 1.000000000000000000 ) ) ;
#240377 = AXIS2_PLACEMENT_3D ( 'NONE', #54623, #224597, #233293 ) ;
#240378 = LINE ( 'NONE', #141271, #27808 ) ;
#240379 = AXIS2_PLACEMENT_3D ( 'NONE', #255992, #156975, #218179 ) ;
#240380 = CARTESIAN_POINT ( 'NONE',  ( -23.25000000000000000, 11.75000000001115552, -134.0000000000000000 ) ) ;
#240382 = LINE ( 'NONE', #199978, #161986 ) ;
#240381 = CARTESIAN_POINT ( 'NONE',  ( 21.05000000000000071, 1.115600667400684642E-11, -67.00000000000004263 ) ) ;
#240384 = AXIS2_PLACEMENT_3D ( 'NONE', #11800, #250379, #167029 ) ;
#240383 = CARTESIAN_POINT ( 'NONE',  ( -23.25000000000000355, 14.23543104469003673, -219.1360829004572395 ) ) ;
#240385 = AXIS2_PLACEMENT_3D ( 'NONE', #108933, #93221, #89363 ) ;
#240386 = CARTESIAN_POINT ( 'NONE',  ( 20.00894256274685645, 4.611773101055291590, 22.11686199560476140 ) ) ;
#240387 = FACE_OUTER_BOUND ( 'NONE', #59851, .T. ) ;
#240388 = DIRECTION ( 'NONE',  ( 0.000000000000000000, 0.2617529984165031243, 0.9651348961777157509 ) ) ;
#240390 = VERTEX_POINT ( 'NONE', #173256 ) ;
#240389 = AXIS2_PLACEMENT_3D ( 'NONE', #153514, #109181, #72665 ) ;
#240391 = EDGE_CURVE ( 'NONE', #71034, #200289, #120299, .T. ) ;
#240393 = ORIENTED_EDGE ( 'NONE', *, *, #191005, .T. ) ;
#240392 = CARTESIAN_POINT ( 'NONE',  ( 21.05000000000000071, 10.42338541492406279, -107.9920519238701218 ) ) ;
#240394 = CARTESIAN_POINT ( 'NONE',  ( 20.94999999999999929, 65.61821452928816711, -131.0152621206402443 ) ) ;
#240395 = EDGE_CURVE ( 'NONE', #14640, #222564, #213601, .T. ) ;
#240396 = DIRECTION ( 'NONE',  ( 1.000000000000000000, 0.000000000000000000, 0.000000000000000000 ) ) ;
#240397 = CIRCLE ( 'NONE', #211175, 0.09999999999999875655 ) ;
#240398 = CARTESIAN_POINT ( 'NONE',  ( -22.49510344025093644, 64.11707268185745079, -247.0813483233072532 ) ) ;
#240399 = ORIENTED_EDGE ( 'NONE', *, *, #161934, .T. ) ;
#240400 = AXIS2_PLACEMENT_3D ( 'NONE', #62207, #45201, #86870 ) ;
#240401 = EDGE_CURVE ( 'NONE', #214618, #65120, #136392, .T. ) ;
#240402 = EDGE_CURVE ( 'NONE', #205515, #102606, #182819, .T. ) ;
#240403 = CARTESIAN_POINT ( 'NONE',  ( 20.94999999999999929, 1.115600667400684642E-11, -100.5000000000000426 ) ) ;
#240404 = CARTESIAN_POINT ( 'NONE',  ( 21.05000000000000426, 65.55640845144084494, -241.8974783712178862 ) ) ;
#240405 = ADVANCED_FACE ( 'NONE', ( #136625 ), #233203, .T. ) ;
#240406 = ORIENTED_EDGE ( 'NONE', *, *, #152515, .T. ) ;
#240407 = CARTESIAN_POINT ( 'NONE',  ( -18.50000972452446035, 10.29326151435326508, -206.4592822510414578 ) ) ;
#240408 = CARTESIAN_POINT ( 'NONE',  ( -23.25000000000000355, 16.64129698264336099, -222.1941556740511032 ) ) ;
#240409 = ADVANCED_FACE ( 'NONE', ( #195359 ), #195294, .T. ) ;
#240410 = LINE ( 'NONE', #85141, #120415 ) ;
#240412 = ORIENTED_EDGE ( 'NONE', *, *, #156333, .F. ) ;
#240411 = CARTESIAN_POINT ( 'NONE',  ( -20.93302460841143287, 67.49317130920637453, -195.4795610751097286 ) ) ;
#240414 = ORIENTED_EDGE ( 'NONE', *, *, #36987, .T. ) ;
#240413 = DIRECTION ( 'NONE',  ( 1.000000000000000000, 0.000000000000000000, 0.000000000000000000 ) ) ;
#240415 = DIRECTION ( 'NONE',  ( 0.000000000000000000, -7.086529944415894657E-15, 1.000000000000000000 ) ) ;
#240416 = LINE ( 'NONE', #124323, #29180 ) ;
#240417 = FACE_OUTER_BOUND ( 'NONE', #9202, .T. ) ;
#240418 = CARTESIAN_POINT ( 'NONE',  ( -14.77738660682463667, 9.436552840015577814, -182.6779554727602886 ) ) ;
#240420 = DIRECTION ( 'NONE',  ( 0.000000000000000000, 0.9126074666063660468, 0.4088369013363524762 ) ) ;
#240419 = DIRECTION ( 'NONE',  ( 0.000000000000000000, -6.982962677686266711E-15, 1.000000000000000000 ) ) ;
#240421 = CARTESIAN_POINT ( 'NONE',  ( 20.85000000000000142, 87.65000000001244018, -170.0231074845242745 ) ) ;
#240422 = CARTESIAN_POINT ( 'NONE',  ( -18.50000972452446035, 10.29326151434210779, -38.95928225104149334 ) ) ;
#240423 = DIRECTION ( 'NONE',  ( 0.000000000000000000, 0.000000000000000000, -1.000000000000000000 ) ) ;
#240424 = CIRCLE ( 'NONE', #161329, 0.9000000000000014655 ) ;
#240425 = CARTESIAN_POINT ( 'NONE',  ( 21.13498764882293557, 10.19455785685945948, -228.0060625952886824 ) ) ;
#240426 = CIRCLE ( 'NONE', #152978, 0.09999999999998898659 ) ;
#240427 = CIRCLE ( 'NONE', #69751, 0.1000000000000013933 ) ;
#240428 = VERTEX_POINT ( 'NONE', #57076 ) ;
#240429 = EDGE_CURVE ( 'NONE', #209017, #252467, #216165, .T. ) ;
#240430 = FACE_OUTER_BOUND ( 'NONE', #85713, .T. ) ;
#240431 = VERTEX_POINT ( 'NONE', #38839 ) ;
#240432 = ORIENTED_EDGE ( 'NONE', *, *, #14198, .T. ) ;
#240433 = CARTESIAN_POINT ( 'NONE',  ( -21.05315837394252654, 11.74999999999999289, -26.65835600069834399 ) ) ;
#240434 = DIRECTION ( 'NONE',  ( -1.000000000000000000, 0.000000000000000000, 0.000000000000000000 ) ) ;
#240435 = EDGE_CURVE ( 'NONE', #11624, #75529, #82781, .T. ) ;
#240436 = EDGE_LOOP ( 'NONE', ( #248218, #149247, #59850, #130657, #190633, #203032, #108952 ) ) ;
#240437 = ADVANCED_FACE ( 'NONE', ( #197887 ), #19260, .T. ) ;
#240438 = ORIENTED_EDGE ( 'NONE', *, *, #160687, .F. ) ;
#240439 = VECTOR ( 'NONE', #234499, 1000.000000000000000 ) ;
#240440 = CIRCLE ( 'NONE', #165627, 0.1000000000000028644 ) ;
#240441 = ORIENTED_EDGE ( 'NONE', *, *, #75082, .T. ) ;
#240442 = DIRECTION ( 'NONE',  ( -0.000000000000000000, 0.4088369013363281623, -0.9126074666063771490 ) ) ;
#240443 = VERTEX_POINT ( 'NONE', #101306 ) ;
#240444 = CARTESIAN_POINT ( 'NONE',  ( -18.59999999999999787, -1.687074390080403941, -87.68542703345838163 ) ) ;
#240445 = DIRECTION ( 'NONE',  ( 1.000000000000000000, 0.000000000000000000, 0.000000000000000000 ) ) ;
#240446 = AXIS2_PLACEMENT_3D ( 'NONE', #19965, #179056, #156921 ) ;
#240447 = CARTESIAN_POINT ( 'NONE',  ( -16.77828822459933633, 66.05377062495534801, -82.18573573544333044 ) ) ;
#240448 = CARTESIAN_POINT ( 'NONE',  ( -21.05000000000000071, 6.176982137395727435, -199.7570632862319542 ) ) ;
#240449 = CARTESIAN_POINT ( 'NONE',  ( 21.05000000000000071, 20.61385802457731131, -234.8303051839938007 ) ) ;
#240450 = CARTESIAN_POINT ( 'NONE',  ( -20.54999999999999716, 76.00000000001212186, -134.6231074845243256 ) ) ;
#240452 = VERTEX_POINT ( 'NONE', #182197 ) ;
#240451 = DIRECTION ( 'NONE',  ( 0.000000000000000000, 5.880418562633242623E-15, -1.000000000000000000 ) ) ;
#240454 = CARTESIAN_POINT ( 'NONE',  ( 18.54286124688534798, 85.62391757880919840, -29.28190515266157234 ) ) ;
#240453 = CARTESIAN_POINT ( 'NONE',  ( -16.94107738177414291, 63.04990807712501777, -213.0142932718104021 ) ) ;
#240455 = DIRECTION ( 'NONE',  ( 1.000000000000000000, -0.000000000000000000, -0.000000000000000000 ) ) ;
#240456 = ORIENTED_EDGE ( 'NONE', *, *, #155252, .T. ) ;
#240457 = CARTESIAN_POINT ( 'NONE',  ( -18.50000000000000000, 9.070041386091544311, -245.4580372780381765 ) ) ;
#240458 = DIRECTION ( 'NONE',  ( 1.000000000000000000, 0.000000000000000000, 0.000000000000000000 ) ) ;
#240459 = EDGE_LOOP ( 'NONE', ( #165706, #251137, #248845, #121389 ) ) ;
#240460 = ADVANCED_FACE ( 'NONE', ( #238297, #83043 ), #220030, .T. ) ;
#240462 = DIRECTION ( 'NONE',  ( -1.000000000000000000, -0.000000000000000000, 0.000000000000000000 ) ) ;
#240461 = LINE ( 'NONE', #60522, #12283 ) ;
#240463 = EDGE_CURVE ( 'NONE', #126285, #199100, #191187, .T. ) ;
#240464 = CARTESIAN_POINT ( 'NONE',  ( -16.87683809663752044, 66.05000000001182059, -82.92547150272069700 ) ) ;
#240465 = ORIENTED_EDGE ( 'NONE', *, *, #11161, .T. ) ;
#240466 = CARTESIAN_POINT ( 'NONE',  ( 21.05000000000000071, 6.258847123090224507, -66.96824164694493220 ) ) ;
#240467 = DIRECTION ( 'NONE',  ( 0.000000000000000000, -1.000000000000000000, 0.000000000000000000 ) ) ;
#240468 = DIRECTION ( 'NONE',  ( 0.000000000000000000, 0.1298341882520022694, 0.9915357197604852679 ) ) ;
#240469 = ADVANCED_FACE ( 'NONE', ( #161356 ), #79212, .T. ) ;
#240470 = ORIENTED_EDGE ( 'NONE', *, *, #251102, .T. ) ;
#240471 = CIRCLE ( 'NONE', #140496, 0.09999999999999939493 ) ;
#240472 = EDGE_CURVE ( 'NONE', #80054, #168194, #36517, .T. ) ;
#240473 = VECTOR ( 'NONE', #165524, 1000.000000000000000 ) ;
#240474 = CARTESIAN_POINT ( 'NONE',  ( -17.11825945287481687, 66.05000000001255955, -182.7731074845244450 ) ) ;
#240475 = CARTESIAN_POINT ( 'NONE',  ( -18.50000000000000000, 8.882751598337863541, -187.0399955572217721 ) ) ;
#240476 = EDGE_CURVE ( 'NONE', #115854, #99277, #16221, .T. ) ;
#240477 = AXIS2_PLACEMENT_3D ( 'NONE', #123524, #203048, #24448 ) ;
#240479 = LINE ( 'NONE', #87798, #157640 ) ;
#240478 = AXIS2_PLACEMENT_3D ( 'NONE', #10129, #251286, #149658 ) ;
#240480 = CARTESIAN_POINT ( 'NONE',  ( -18.49499033040906681, 85.43814877175698541, -162.8249542586008545 ) ) ;
#240481 = VECTOR ( 'NONE', #152393, 999.9999999999998863 ) ;
#240482 = ADVANCED_FACE ( 'NONE', ( #203022 ), #4803, .F. ) ;
#240484 = ORIENTED_EDGE ( 'NONE', *, *, #138006, .F. ) ;
#240483 = CARTESIAN_POINT ( 'NONE',  ( -21.05000000000000071, 77.83534155023700407, -191.8679561919613832 ) ) ;
#240485 = CARTESIAN_POINT ( 'NONE',  ( 23.25000000000000000, -4.914013037343258894, -233.1828366659746905 ) ) ;
#240487 = EDGE_CURVE ( 'NONE', #14558, #67305, #139181, .T. ) ;
#240486 = AXIS2_PLACEMENT_3D ( 'NONE', #127485, #204437, #47932 ) ;
#240488 = CARTESIAN_POINT ( 'NONE',  ( 21.14999999999999858, 64.35000000001195986, -102.9231074845243938 ) ) ;
#240489 = CARTESIAN_POINT ( 'NONE',  ( -23.25000000000000000, 11.75000000001115552, -21.75000000000000355 ) ) ;
#240490 = CARTESIAN_POINT ( 'NONE',  ( 22.57320508075688537, 55.98745301258801987, -232.8057040749261262 ) ) ;
#240491 = AXIS2_PLACEMENT_3D ( 'NONE', #102499, #120851, #158692 ) ;
#240492 = DIRECTION ( 'NONE',  ( -1.000000000000000000, 0.000000000000000000, 0.000000000000000000 ) ) ;
#240494 = ORIENTED_EDGE ( 'NONE', *, *, #110016, .F. ) ;
#240493 = CARTESIAN_POINT ( 'NONE',  ( 21.10710606213542206, 67.22310597611837579, -57.28211095812496723 ) ) ;
#240495 = CARTESIAN_POINT ( 'NONE',  ( -23.15000000000000213, -4.914013037343267776, -233.1828366659746905 ) ) ;
#240496 = DIRECTION ( 'NONE',  ( 0.000000000000000000, -1.000000000000000000, 0.000000000000000000 ) ) ;
#240497 = DIRECTION ( 'NONE',  ( 0.000000000000000000, -7.487053152578127080E-15, 1.000000000000000000 ) ) ;
#240498 = EDGE_LOOP ( 'NONE', ( #253734, #105590, #96591, #108395 ) ) ;
#240499 = CARTESIAN_POINT ( 'NONE',  ( -23.25000000000000000, 78.50726470275243685, -228.6618886302502176 ) ) ;
#240500 = DIRECTION ( 'NONE',  ( -1.000000000000000000, -0.000000000000000000, -0.000000000000000000 ) ) ;
#240501 = DIRECTION ( 'NONE',  ( -4.408576920032448588E-17, 0.1350103645451876666, 0.9908441862701600211 ) ) ;
#240502 = DIRECTION ( 'NONE',  ( -0.000000000000000000, 0.8660254037844411501, 0.4999999999999956701 ) ) ;
#240503 = AXIS2_PLACEMENT_3D ( 'NONE', #241163, #238578, #84591 ) ;
#240504 = CARTESIAN_POINT ( 'NONE',  ( -16.87333278164152972, 9.882609784590000501, -87.36683219384656240 ) ) ;
#240505 = ADVANCED_FACE ( 'NONE', ( #2242 ), #160079, .T. ) ;
#240506 = EDGE_CURVE ( 'NONE', #134285, #145606, #74502, .T. ) ;
#240507 = EDGE_LOOP ( 'NONE', ( #215435, #136461, #172085, #233618 ) ) ;
#240508 = ORIENTED_EDGE ( 'NONE', *, *, #230286, .T. ) ;
#240509 = CIRCLE ( 'NONE', #248893, 0.1000000000000008937 ) ;
#240510 = CARTESIAN_POINT ( 'NONE',  ( 23.24999999999999289, 8.882751598337874199, -187.0399955572217721 ) ) ;
#240512 = DIRECTION ( 'NONE',  ( 1.000000000000000000, 0.000000000000000000, -0.000000000000000000 ) ) ;
#240511 = MECHANICAL_DESIGN_GEOMETRIC_PRESENTATION_REPRESENTATION (  '', ( #15689 ), #74130 ) ;
#240513 = AXIS2_PLACEMENT_3D ( 'NONE', #121337, #242522, #120043 ) ;
#240514 =( BOUNDED_SURFACE ( )  B_SPLINE_SURFACE ( 3, 2, ( 
 ( #183792, #242467, #219049 ),
 ( #41734, #221606, #1282 ),
 ( #204621, #5115, #243764 ),
 ( #199525, #62566, #144648 ),
 ( #181245, #20896, #95588 ),
 ( #82091, #6, #43005 ),
 ( #175183, #79532, #159121 ),
 ( #238631, #140817, #59967 ),
 ( #100372, #161683, #80815 ),
 ( #142086, #121292, #160407 ),
 ( #239926, #61277, #220362 ),
 ( #128960, #187665, #88514 ) ),
 .UNSPECIFIED., .F., .F., .F. ) 
 B_SPLINE_SURFACE_WITH_KNOTS ( ( 4, 2, 2, 2, 2, 4 ),
 ( 3, 3 ),
 ( 3.174653483277205090, 3.943930578431714018, 4.713207673586222946, 5.482484768740731873, 5.867123316317986337, 6.251761863895240801 ),
 ( 0.000000000000000000, 1.000000000000000000 ),
 .UNSPECIFIED. ) 
 GEOMETRIC_REPRESENTATION_ITEM ( )  RATIONAL_B_SPLINE_SURFACE ( (
 ( 1.000000000000000000, 0.8659465255642114778, 1.000000000000000000),
 ( 1.000000000000000000, 0.8648614068487411322, 1.000000000000000000),
 ( 1.000000000000000000, 0.8489031841324523597, 1.000000000000000000),
 ( 1.000000000000000000, 0.7927507630160768315, 1.000000000000000000),
 ( 1.000000000000000000, 0.7523013859006951742, 1.000000000000000000),
 ( 1.000000000000000000, 0.6616226951198839190, 1.000000000000000000),
 ( 1.000000000000000000, 0.6112214368721479163, 1.000000000000000000),
 ( 1.000000000000000000, 0.5507684314500016498, 1.000000000000000000),
 ( 1.000000000000000000, 0.5333267243152196579, 1.000000000000000000),
 ( 1.000000000000000000, 0.5084565446481067452, 1.000000000000000000),
 ( 1.000000000000000000, 0.5010722703450574134, 1.000000000000000000),
 ( 1.000000000000000000, 0.5001234037138888588, 1.000000000000000000) ) ) 
 REPRESENTATION_ITEM ( '' )  SURFACE ( )  );
#240515 = LINE ( 'NONE', #61882, #162168 ) ;
#240516 = SPHERICAL_SURFACE ( 'NONE', #47372, 0.1000000000000000056 ) ;
#240517 = ORIENTED_EDGE ( 'NONE', *, *, #118609, .T. ) ;
#240518 = AXIS2_PLACEMENT_3D ( 'NONE', #188987, #89869, #149880 ) ;
#240519 = DIRECTION ( 'NONE',  ( 0.000000000000000000, 0.000000000000000000, 1.000000000000000000 ) ) ;
#240520 = DIRECTION ( 'NONE',  ( 1.000000000000000000, 0.000000000000000000, 0.000000000000000000 ) ) ;
#240521 = EDGE_CURVE ( 'NONE', #10221, #32161, #107768, .T. ) ;
#240522 = CARTESIAN_POINT ( 'NONE',  ( -16.80438519320023616, 9.949779096468343909, -12.65073828092127250 ) ) ;
#240523 = EDGE_CURVE ( 'NONE', #190309, #53632, #140714, .T. ) ;
#240524 = CARTESIAN_POINT ( 'NONE',  ( 20.95520789717937404, 10.57693059939611224, -108.0802329738748853 ) ) ;
#240525 = CARTESIAN_POINT ( 'NONE',  ( -16.85722902420155123, 9.949999999999985079, -20.73445252622950719 ) ) ;
#240526 = CIRCLE ( 'NONE', #140556, 0.1000000000000028644 ) ;
#240527 = AXIS2_PLACEMENT_3D ( 'NONE', #227622, #107681, #183383 ) ;
#240528 = ORIENTED_EDGE ( 'NONE', *, *, #257436, .F. ) ;
#240530 = VERTEX_POINT ( 'NONE', #223858 ) ;
#240529 = CARTESIAN_POINT ( 'NONE',  ( 21.05000000000000071, 28.32080209959243788, -238.8452605374484676 ) ) ;
#240531 = ORIENTED_EDGE ( 'NONE', *, *, #59714, .F. ) ;
#240532 = CARTESIAN_POINT ( 'NONE',  ( 21.05000000000000071, 56.16603649944111254, -228.1013850343386480 ) ) ;
#240533 = ORIENTED_EDGE ( 'NONE', *, *, #34489, .F. ) ;
#240534 = CYLINDRICAL_SURFACE ( 'NONE', #46566, 0.1000000000000028644 ) ;
#240535 = CARTESIAN_POINT ( 'NONE',  ( -20.85000000000000142, 77.73670573947892137, -24.50568489690058627 ) ) ;
#240536 = CARTESIAN_POINT ( 'NONE',  ( -23.25000000000000000, 43.00579525902548994, -254.2551217332645876 ) ) ;
#240537 = ORIENTED_EDGE ( 'NONE', *, *, #65002, .F. ) ;
#240538 = ADVANCED_FACE ( 'NONE', ( #60943 ), #70000, .T. ) ;
#240539 = CARTESIAN_POINT ( 'NONE',  ( 18.59999999999999432, 77.16270174994961906, -61.42310748452431568 ) ) ;
#240540 = DIRECTION ( 'NONE',  ( 1.000000000000000000, 0.000000000000000000, -0.000000000000000000 ) ) ;
#240541 = ORIENTED_EDGE ( 'NONE', *, *, #139749, .F. ) ;
#240542 = CARTESIAN_POINT ( 'NONE',  ( -16.86578989773640913, 9.984809801269950214, -54.46466488662223782 ) ) ;
#240543 = AXIS2_PLACEMENT_3D ( 'NONE', #123693, #203215, #184936 ) ;
#240545 = ORIENTED_EDGE ( 'NONE', *, *, #195768, .F. ) ;
#240544 = CARTESIAN_POINT ( 'NONE',  ( -16.94107738177415712, 10.01423928513662176, -12.55000000000000249 ) ) ;
#240546 = CARTESIAN_POINT ( 'NONE',  ( -20.00857864376270001, 30.09302283515540211, -235.6538990729184491 ) ) ;
#240547 = AXIS2_PLACEMENT_3D ( 'NONE', #46987, #126552, #246492 ) ;
#240548 = CYLINDRICAL_SURFACE ( 'NONE', #18920, 2.000000000000001776 ) ;
#240549 = EDGE_CURVE ( 'NONE', #167845, #13346, #198964, .T. ) ;
#240550 = CIRCLE ( 'NONE', #203121, 2.000000000000013323 ) ;
#240551 = EDGE_LOOP ( 'NONE', ( #148330, #89317, #17977, #37429, #66359 ) ) ;
#240552 = VECTOR ( 'NONE', #155737, 1000.000000000000000 ) ;
#240553 = CARTESIAN_POINT ( 'NONE',  ( -18.59999999999999787, 69.15387683765909799, -65.78538121767449809 ) ) ;
#240554 = CARTESIAN_POINT ( 'NONE',  ( -15.70407651835960650, 66.64419340838190919, -120.2320049529781727 ) ) ;
#240555 = CARTESIAN_POINT ( 'NONE',  ( -21.05000000000000071, 46.45388641681647357, -243.1520440498138385 ) ) ;
#240556 = EDGE_LOOP ( 'NONE', ( #158142, #58370, #140248, #73919, #240345, #25532, #145053, #143103 ) ) ;
#240557 = DIRECTION ( 'NONE',  ( -0.000000000000000000, 0.4721928772777345684, 0.8814952561688429444 ) ) ;
#240558 = ADVANCED_FACE ( 'NONE', ( #163912 ), #124789, .F. ) ;
#240559 = CARTESIAN_POINT ( 'NONE',  ( 15.39170923737819763, 49.08016403251641435, -233.6979168753148883 ) ) ;
#240560 = CARTESIAN_POINT ( 'NONE',  ( -21.70464131381649509, 7.095358018979010417, -100.5000000000000284 ) ) ;
#240561 = CIRCLE ( 'NONE', #132414, 12.97499999999999964 ) ;
#240562 = VERTEX_POINT ( 'NONE', #64796 ) ;
#240563 = VECTOR ( 'NONE', #217314, 1000.000000000000227 ) ;
#240564 = AXIS2_PLACEMENT_3D ( 'NONE', #64508, #185741, #183183 ) ;
#240565 = AXIS2_PLACEMENT_3D ( 'NONE', #88013, #71068, #151896 ) ;
#240566 = EDGE_LOOP ( 'NONE', ( #226718, #199073, #9942, #65171 ) ) ;
#240567 = ORIENTED_EDGE ( 'NONE', *, *, #111949, .F. ) ;
#240568 = DIRECTION ( 'NONE',  ( 0.000000000000000000, 6.982962677686266711E-15, -1.000000000000000000 ) ) ;
#240569 = LINE ( 'NONE', #61936, #121117 ) ;
#240571 = VERTEX_POINT ( 'NONE', #143037 ) ;
#240570 = DIRECTION ( 'NONE',  ( -0.000000000000000000, 0.1350103645451904977, 0.9908441862701597991 ) ) ;
#240572 = CARTESIAN_POINT ( 'NONE',  ( 18.59999999999999432, 46.55954744353147134, -243.3218549665227783 ) ) ;
#240573 = CARTESIAN_POINT ( 'NONE',  ( 21.05000000000000071, -9.500000000000001776, -9.893969122652443104 ) ) ;
#240574 = FACE_BOUND ( 'NONE', #112181, .T. ) ;
#240575 = CARTESIAN_POINT ( 'NONE',  ( 18.39999999999999858, 85.60000000001232934, -162.9910380878246201 ) ) ;
#240576 = DIRECTION ( 'NONE',  ( 0.2834754621636439431, -0.2834754621636535465, -0.9161240771326838450 ) ) ;
#240577 = AXIS2_PLACEMENT_3D ( 'NONE', #211999, #50315, #209406 ) ;
#240578 = CARTESIAN_POINT ( 'NONE',  ( -23.15000000000000213, 76.00000000001149658, -48.89810748452431710 ) ) ;
#240580 = VERTEX_POINT ( 'NONE', #100049 ) ;
#240579 = DIRECTION ( 'NONE',  ( 0.000000000000000000, 0.000000000000000000, 1.000000000000000000 ) ) ;
#240582 = ORIENTED_EDGE ( 'NONE', *, *, #51425, .F. ) ;
#240581 = DIRECTION ( 'NONE',  ( -0.000000000000000000, 0.9910827722268049644, -0.1332476588733589318 ) ) ;
#240583 = CARTESIAN_POINT ( 'NONE',  ( -18.59999999999999787, 11.65000000001115232, -167.5000000000000284 ) ) ;
#240584 = ORIENTED_EDGE ( 'NONE', *, *, #249062, .T. ) ;
#240585 = ORIENTED_EDGE ( 'NONE', *, *, #7527, .F. ) ;
#240586 = CARTESIAN_POINT ( 'NONE',  ( 18.49999999999999645, 1.736257131597397585, -11.56865232901749962 ) ) ;
#240587 = CARTESIAN_POINT ( 'NONE',  ( 21.05000000000000071, -11.64999999998883595, -33.50000000000000000 ) ) ;
#240588 = VECTOR ( 'NONE', #223218, 1000.000000000000000 ) ;
#240589 = CARTESIAN_POINT ( 'NONE',  ( 21.15000000000005542, 89.48413628383013929, -38.12477508515532065 ) ) ;
#240590 = DIRECTION ( 'NONE',  ( -0.000000000000000000, 1.000000000000000000, 0.000000000000000000 ) ) ;
#240591 = DIRECTION ( 'NONE',  ( 0.000000000000000000, 0.000000000000000000, -1.000000000000000000 ) ) ;
#240592 = CARTESIAN_POINT ( 'NONE',  ( 18.49999999999999645, 70.05000000001236060, -159.7174051794895320 ) ) ;
#240593 = CARTESIAN_POINT ( 'NONE',  ( -20.85000000000000142, 6.846123162363745074, -137.7377262668498759 ) ) ;
#240594 = ORIENTED_EDGE ( 'NONE', *, *, #256061, .T. ) ;
#240595 = ORIENTED_EDGE ( 'NONE', *, *, #88616, .T. ) ;
#240596 = EDGE_CURVE ( 'NONE', #19071, #51100, #203256, .T. ) ;
#240597 = SURFACE_STYLE_FILL_AREA ( #257528 ) ;
#240598 = AXIS2_PLACEMENT_3D ( 'NONE', #94873, #251386, #12806 ) ;
#240599 = CIRCLE ( 'NONE', #211578, 0.1000000000000054040 ) ;
#240600 = EDGE_LOOP ( 'NONE', ( #1076, #150268, #33907, #87064, #239973, #90114, #85812, #231367, #181878, #31815, #118199, #50094, #226358, #114951, #141518, #250572, #76778, #45845, #9781, #7165, #184753, #33696, #189379, #4852, #100433 ) ) ;
#240602 = CARTESIAN_POINT ( 'NONE',  ( 23.50000000000005684, 74.16448838626247664, -47.52760213295649550 ) ) ;
#240601 = CIRCLE ( 'NONE', #153165, 2.100000000000004530 ) ;
#240603 = SPHERICAL_SURFACE ( 'NONE', #210014, 0.1000000000000000056 ) ;
#240604 = CARTESIAN_POINT ( 'NONE',  ( -14.77738660682463845, 66.56344716000714357, -54.34515201176409249 ) ) ;
#240605 =( BOUNDED_SURFACE ( )  B_SPLINE_SURFACE ( 3, 2, ( 
 ( #30192, #189253, #31487 ),
 ( #110993, #165849, #171018 ),
 ( #146252, #185394, #250490 ),
 ( #71880, #151420, #230964 ),
 ( #52278, #131834, #245379 ),
 ( #54847, #116139, #17042 ) ),
 .UNSPECIFIED., .F., .F., .F. ) 
 B_SPLINE_SURFACE_WITH_KNOTS ( ( 4, 2, 4 ),
 ( 3, 3 ),
 ( 3.141592653589783346, 3.926990816987233845, 4.712388980384684345 ),
 ( 0.000000000000000000, 1.000000000000000000 ),
 .UNSPECIFIED. ) 
 GEOMETRIC_REPRESENTATION_ITEM ( )  RATIONAL_B_SPLINE_SURFACE ( (
 ( 1.000000000000000000, 0.9238795325112774126, 1.000000000000000000),
 ( 1.000000000000000000, 0.9240297172247110558, 1.000000000000000000),
 ( 1.000000000000000000, 0.9038128468034775098, 1.000000000000000000),
 ( 1.000000000000000000, 0.8282379607654114517, 1.000000000000000000),
 ( 1.000000000000000000, 0.7727932973487930957, 1.000000000000000000),
 ( 1.000000000000000000, 0.7071067811865352493, 1.000000000000000000) ) ) 
 REPRESENTATION_ITEM ( '' )  SURFACE ( )  );
#240606 = DIRECTION ( 'NONE',  ( 2.694716079187276397E-16, -0.4721928772777353456, -0.8814952561688426114 ) ) ;
#240607 = ORIENTED_EDGE ( 'NONE', *, *, #217599, .F. ) ;
#240608 = DIRECTION ( 'NONE',  ( 2.694716079187273439E-16, 0.9651348961777159730, -0.2617529984165023471 ) ) ;
#240609 = ORIENTED_EDGE ( 'NONE', *, *, #39372, .T. ) ;
#240610 = CARTESIAN_POINT ( 'NONE',  ( -13.40000000000000213, -11.75000000000000000, 17.70000000000000284 ) ) ;
#240611 = EDGE_LOOP ( 'NONE', ( #23587, #98146 ) ) ;
#240612 = ADVANCED_FACE ( 'NONE', ( #225137 ), #229026, .F. ) ;
#240613 = LINE ( 'NONE', #119390, #114935 ) ;
#240614 = DIRECTION ( 'NONE',  ( -0.000000000000000000, -0.000000000000000000, -1.000000000000000000 ) ) ;
#240615 = AXIS2_PLACEMENT_3D ( 'NONE', #2292, #139229, #60996 ) ;
#240616 = ORIENTED_EDGE ( 'NONE', *, *, #213226, .F. ) ;
#240617 = CARTESIAN_POINT ( 'NONE',  ( -21.05000000000000071, 76.00000000001237765, -170.0231074845243597 ) ) ;
#240619 = ORIENTED_EDGE ( 'NONE', *, *, #205139, .F. ) ;
#240618 = CARTESIAN_POINT ( 'NONE',  ( 18.59999999999999076, 10.80300742114540391, -220.2930047078982625 ) ) ;
#240620 = CARTESIAN_POINT ( 'NONE',  ( 23.15000000000000213, 85.00000000001159606, -59.62913836187181715 ) ) ;
#240621 = ORIENTED_EDGE ( 'NONE', *, *, #70303, .F. ) ;
#240622 = AXIS2_PLACEMENT_3D ( 'NONE', #89953, #209927, #52099 ) ;
#240623 = ADVANCED_FACE ( 'NONE', ( #131187 ), #74113, .F. ) ;
#240624 = CYLINDRICAL_SURFACE ( 'NONE', #240690, 12.87499999999999822 ) ;
#240625 = ADVANCED_FACE ( 'NONE', ( #170378 ), #50348, .T. ) ;
#240626 = ORIENTED_EDGE ( 'NONE', *, *, #187650, .F. ) ;
#240627 = CYLINDRICAL_SURFACE ( 'NONE', #249324, 12.87500000000000178 ) ;
#240628 = CARTESIAN_POINT ( 'NONE',  ( 18.79999999999999716, 0.000000000000000000, 32.89999999999999858 ) ) ;
#240629 = CARTESIAN_POINT ( 'NONE',  ( 18.52928932188133970, 10.27928932189250411, -158.7500000000000284 ) ) ;
#240630 = CARTESIAN_POINT ( 'NONE',  ( 18.55121869061587958, 67.49249915771264341, -195.4369143829851510 ) ) ;
#240631 = EDGE_CURVE ( 'NONE', #57292, #44391, #98990, .T. ) ;
#240632 = CARTESIAN_POINT ( 'NONE',  ( -22.59999999999999787, 0.1008583691098682150, -155.7504328765105868 ) ) ;
#240633 = ORIENTED_EDGE ( 'NONE', *, *, #110319, .T. ) ;
#240634 = DIRECTION ( 'NONE',  ( 0.000000000000000000, -1.000000000000000000, -6.982962677686265922E-15 ) ) ;
#240635 = EDGE_CURVE ( 'NONE', #155898, #54081, #132329, .T. ) ;
#240636 = CARTESIAN_POINT ( 'NONE',  ( 21.78635804494511419, 0.9736806036678684606, -230.3232395766309537 ) ) ;
#240637 = TOROIDAL_SURFACE ( 'NONE', #128226, 7.800000000000000711, 0.1000000000000000056 ) ;
#240638 = EDGE_LOOP ( 'NONE', ( #108425, #85511, #135641, #88499 ) ) ;
#240639 = CARTESIAN_POINT ( 'NONE',  ( 18.50000324121758055, 10.29307482169091870, -105.9586421466940038 ) ) ;
#240640 = ORIENTED_EDGE ( 'NONE', *, *, #199886, .T. ) ;
#240641 = CARTESIAN_POINT ( 'NONE',  ( 20.94999999999999929, 7.128833340094563376, -233.7327013124401276 ) ) ;
#240642 = AXIS2_PLACEMENT_3D ( 'NONE', #184191, #128090, #145067 ) ;
#240643 = VERTEX_POINT ( 'NONE', #209443 ) ;
#240644 = EDGE_CURVE ( 'NONE', #236424, #211247, #244709, .T. ) ;
#240645 = DIRECTION ( 'NONE',  ( 0.000000000000000000, -0.9770955615653316162, -0.2128009952263604232 ) ) ;
#240646 = LINE ( 'NONE', #41190, #64580 ) ;
#240647 = ORIENTED_EDGE ( 'NONE', *, *, #11976, .T. ) ;
#240649 = ORIENTED_EDGE ( 'NONE', *, *, #43838, .T. ) ;
#240648 = FACE_OUTER_BOUND ( 'NONE', #123606, .T. ) ;
#240650 = DIRECTION ( 'NONE',  ( 0.7071067811865388020, -0.7071067811865561215, 0.000000000000000000 ) ) ;
#240651 = ORIENTED_EDGE ( 'NONE', *, *, #104557, .T. ) ;
#240652 = CIRCLE ( 'NONE', #15839, 0.1000000000000055844 ) ;
#240653 = LINE ( 'NONE', #101088, #144103 ) ;
#240654 = DIRECTION ( 'NONE',  ( -1.000000000000000000, 0.000000000000000000, 0.000000000000000000 ) ) ;
#240656 = EDGE_CURVE ( 'NONE', #59365, #82535, #228210, .T. ) ;
#240655 = ORIENTED_EDGE ( 'NONE', *, *, #115170, .T. ) ;
#240657 = ORIENTED_EDGE ( 'NONE', *, *, #14471, .T. ) ;
#240658 = CARTESIAN_POINT ( 'NONE',  ( -21.14999999999999858, 11.75000000001115552, -174.2838656629781156 ) ) ;
#240659 = LINE ( 'NONE', #221083, #44399 ) ;
#240660 = CARTESIAN_POINT ( 'NONE',  ( 20.94999999999999574, 0.7653315920341953182, -212.6731560895497353 ) ) ;
#240661 = CIRCLE ( 'NONE', #48934, 0.1000000000000028644 ) ;
#240662 = CIRCLE ( 'NONE', #186514, 0.1000000000000068751 ) ;
#240664 = ORIENTED_EDGE ( 'NONE', *, *, #131739, .T. ) ;
#240663 = AXIS2_PLACEMENT_3D ( 'NONE', #247278, #90769, #166503 ) ;
#240665 = EDGE_LOOP ( 'NONE', ( #140508, #177153, #205963, #218588 ) ) ;
#240667 = LINE ( 'NONE', #137692, #14127 ) ;
#240666 = CIRCLE ( 'NONE', #15849, 0.09999999999999520384 ) ;
#240669 = ORIENTED_EDGE ( 'NONE', *, *, #141896, .F. ) ;
#240668 = CARTESIAN_POINT ( 'NONE',  ( -16.87683809663753109, 9.864913778549569301, -46.77571563563853374 ) ) ;
#240670 = CARTESIAN_POINT ( 'NONE',  ( 16.87683809663750267, 9.950000000011138823, -46.15000000000000568 ) ) ;
#240671 = DIRECTION ( 'NONE',  ( -1.000000000000000000, 0.000000000000000000, -0.000000000000000000 ) ) ;
#240672 = CARTESIAN_POINT ( 'NONE',  ( 23.15000000000000213, -8.596261682242991142, -9.450127517150276546 ) ) ;
#240674 = CARTESIAN_POINT ( 'NONE',  ( -23.25000000000000000, 23.40438595358395091, -253.3416554127419431 ) ) ;
#240673 = CYLINDRICAL_SURFACE ( 'NONE', #6880, 0.09999999999999939493 ) ;
#240675 = FACE_OUTER_BOUND ( 'NONE', #192582, .T. ) ;
#240676 = DIRECTION ( 'NONE',  ( -1.000000000000000000, 8.673617379884087537E-15, 0.000000000000000000 ) ) ;
#240677 = VECTOR ( 'NONE', #52579, 1000.000000000000000 ) ;
#240678 = DIRECTION ( 'NONE',  ( -1.000000000000000000, 0.000000000000000000, 0.000000000000000000 ) ) ;
#240679 = CARTESIAN_POINT ( 'NONE',  ( 22.45463910399148588, -3.140208065486764344, -228.2318569525289718 ) ) ;
#240680 = AXIS2_PLACEMENT_3D ( 'NONE', #206365, #105946, #245495 ) ;
#240681 = ORIENTED_EDGE ( 'NONE', *, *, #66758, .F. ) ;
#240682 = EDGE_CURVE ( 'NONE', #9026, #91403, #111490, .T. ) ;
#240683 = AXIS2_PLACEMENT_3D ( 'NONE', #6243, #181068, #121108 ) ;
#240685 = ADVANCED_FACE ( 'NONE', ( #11256 ), #126043, .F. ) ;
#240684 = TOROIDAL_SURFACE ( 'NONE', #220020, 4.149999999999999467, 0.1000000000000000056 ) ;
#240686 = AXIS2_PLACEMENT_3D ( 'NONE', #199251, #179688, #20621 ) ;
#240687 = ORIENTED_EDGE ( 'NONE', *, *, #21113, .F. ) ;
#240688 = DIRECTION ( 'NONE',  ( -0.000000000000000000, -0.000000000000000000, -1.000000000000000000 ) ) ;
#240689 = ORIENTED_EDGE ( 'NONE', *, *, #169192, .F. ) ;
#240690 = AXIS2_PLACEMENT_3D ( 'NONE', #159821, #698, #140215 ) ;
#240691 = EDGE_CURVE ( 'NONE', #196126, #149025, #165190, .T. ) ;
#240692 = ADVANCED_FACE ( 'NONE', ( #149504 ), #189890, .T. ) ;
#240693 = CYLINDRICAL_SURFACE ( 'NONE', #89930, 0.5000000000000004441 ) ;
#240694 = ORIENTED_EDGE ( 'NONE', *, *, #175041, .T. ) ;
#240695 = EDGE_CURVE ( 'NONE', #239961, #153115, #68665, .T. ) ;
#240696 = FILL_AREA_STYLE ('',( #42485 ) ) ;
#240697 = CARTESIAN_POINT ( 'NONE',  ( 20.84999999999998721, 65.66751761918692409, -130.9282609406112670 ) ) ;
#240698 = ADVANCED_FACE ( 'NONE', ( #230289 ), #71246, .F. ) ;
#240700 = EDGE_LOOP ( 'NONE', ( #43768, #90442, #209606, #43146 ) ) ;
#240699 = ORIENTED_EDGE ( 'NONE', *, *, #246469, .T. ) ;
#240701 = ORIENTED_EDGE ( 'NONE', *, *, #219299, .F. ) ;
#240704 = EDGE_CURVE ( 'NONE', #246187, #140884, #182431, .T. ) ;
#240703 = EDGE_CURVE ( 'NONE', #133767, #36158, #144788, .T. ) ;
#240702 = CIRCLE ( 'NONE', #49164, 0.1000000000000028644 ) ;
#240705 = VECTOR ( 'NONE', #1835, 1000.000000000000000 ) ;
#240706 = ORIENTED_EDGE ( 'NONE', *, *, #174223, .T. ) ;
#240707 = FACE_OUTER_BOUND ( 'NONE', #123067, .T. ) ;
#240708 = DIRECTION ( 'NONE',  ( -1.186688945009010077E-16, 1.000000000000000000, 0.000000000000000000 ) ) ;
#240710 = VERTEX_POINT ( 'NONE', #106466 ) ;
#240709 = DIRECTION ( 'NONE',  ( 1.000000000000000000, 0.000000000000000000, 0.000000000000000000 ) ) ;
#240711 = EDGE_CURVE ( 'NONE', #106308, #213820, #178148, .T. ) ;
#240712 = CARTESIAN_POINT ( 'NONE',  ( 21.05000000000000071, 70.50000000001223555, -148.9283735034374843 ) ) ;
#240713 = FACE_OUTER_BOUND ( 'NONE', #137987, .T. ) ;
#240715 = ORIENTED_EDGE ( 'NONE', *, *, #34870, .T. ) ;
#240714 = CARTESIAN_POINT ( 'NONE',  ( 20.94999999999999929, 69.55000000001207638, -126.5060803140843291 ) ) ;
#240716 = FACE_OUTER_BOUND ( 'NONE', #55334, .T. ) ;
#240717 = EDGE_LOOP ( 'NONE', ( #198347, #147405, #170982, #12868 ) ) ;
#240718 = CARTESIAN_POINT ( 'NONE',  ( -23.25000000000000000, 85.68240343348806221, -62.86626410711144786 ) ) ;
#240720 = ORIENTED_EDGE ( 'NONE', *, *, #224295, .F. ) ;
#240719 = DIRECTION ( 'NONE',  ( 0.000000000000000000, 0.2128009952263485993, -0.9770955615653341697 ) ) ;
#240721 = STYLED_ITEM ( 'NONE', ( #124663 ), #18376 ) ;
#240722 = CARTESIAN_POINT ( 'NONE',  ( -18.50000000000000000, 11.65000000001115232, -122.2500000000000284 ) ) ;
#240724 = ADVANCED_FACE ( 'NONE', ( #35964 ), #212037, .T. ) ;
#240723 = CARTESIAN_POINT ( 'NONE',  ( -15.73854595235691889, 26.51259657475388920, -233.5074718021644173 ) ) ;
#240725 = CIRCLE ( 'NONE', #111546, 0.1000000000000000472 ) ;
#240726 = DIRECTION ( 'NONE',  ( 0.000000000000000000, 0.9229812358756199764, -0.3848449534832346086 ) ) ;
#240727 = EDGE_LOOP ( 'NONE', ( #103035, #854, #217640, #58186 ) ) ;
#240729 = CARTESIAN_POINT ( 'NONE',  ( 20.97217846901852312, 8.875441724720827708, -109.0012276839372447 ) ) ;
#240728 = CARTESIAN_POINT ( 'NONE',  ( -21.52071067811865746, 52.87137254617348958, -233.7639410278083005 ) ) ;
#240730 = CARTESIAN_POINT ( 'NONE',  ( -15.57281606413133979, 66.62934494888835957, -85.49728422854349219 ) ) ;
#240731 = AXIS2_PLACEMENT_3D ( 'NONE', #161956, #164516, #244025 ) ;
#240732 = EDGE_CURVE ( 'NONE', #187769, #66771, #153219, .T. ) ;
#240733 = EDGE_CURVE ( 'NONE', #21708, #214842, #135021, .T. ) ;
#240734 = CARTESIAN_POINT ( 'NONE',  ( 18.58725287972269058, 85.56662691070425808, -163.2006026787589974 ) ) ;
#240735 = DIRECTION ( 'NONE',  ( 1.000000000000000000, 0.000000000000000000, 0.000000000000000000 ) ) ;
#240736 = DIRECTION ( 'NONE',  ( 0.000000000000000000, -0.1350103645451807555, -0.9908441862701610203 ) ) ;
#240737 = EDGE_LOOP ( 'NONE', ( #237135, #117114, #216760, #45095 ) ) ;
#240738 = ORIENTED_EDGE ( 'NONE', *, *, #46602, .T. ) ;
#240740 = ORIENTED_EDGE ( 'NONE', *, *, #48499, .F. ) ;
#240739 = AXIS2_PLACEMENT_3D ( 'NONE', #214092, #36779, #178858 ) ;
#240741 = EDGE_CURVE ( 'NONE', #24156, #21614, #153376, .T. ) ;
#240742 = CARTESIAN_POINT ( 'NONE',  ( -21.13422380239033771, 1.115470038567900342E-11, -127.5066734851939003 ) ) ;
#240743 = ORIENTED_EDGE ( 'NONE', *, *, #77821, .F. ) ;
#240744 = DIRECTION ( 'NONE',  ( 1.000000000000000000, 0.000000000000000000, -0.000000000000000000 ) ) ;
#240745 = VERTEX_POINT ( 'NONE', #34687 ) ;
#240746 = LINE ( 'NONE', #222423, #98350 ) ;
#240747 = DIRECTION ( 'NONE',  ( 0.000000000000000000, 0.000000000000000000, 1.000000000000000000 ) ) ;
#240748 = EDGE_CURVE ( 'NONE', #238413, #20839, #58056, .T. ) ;
#240749 = ADVANCED_FACE ( 'NONE', ( #254931 ), #253124, .F. ) ;
#240750 = AXIS2_PLACEMENT_3D ( 'NONE', #105819, #224504, #165843 ) ;
#240751 = CIRCLE ( 'NONE', #236455, 0.09999999999999485689 ) ;
#240752 = AXIS2_PLACEMENT_3D ( 'NONE', #245590, #183054, #46084 ) ;
#240753 = ORIENTED_EDGE ( 'NONE', *, *, #155652, .F. ) ;
#240754 = TOROIDAL_SURFACE ( 'NONE', #15927, 4.149999999999999467, 0.1000000000000000056 ) ;
#240755 = DIRECTION ( 'NONE',  ( 0.9880948137434723000, 0.1538461538461484146, -0.000000000000000000 ) ) ;
#240756 =( LENGTH_UNIT ( ) NAMED_UNIT ( * ) SI_UNIT ( .MILLI., .METRE. ) );
#240757 = TOROIDAL_SURFACE ( 'NONE', #153499, 0.6000000000000006439, 0.1000000000000000056 ) ;
#240758 = ORIENTED_EDGE ( 'NONE', *, *, #219431, .T. ) ;
#240759 = EDGE_LOOP ( 'NONE', ( #32140, #15152, #121473, #232662 ) ) ;
#240760 = ORIENTED_EDGE ( 'NONE', *, *, #245725, .F. ) ;
#240761 = LINE ( 'NONE', #178240, #187878 ) ;
#240762 = DIRECTION ( 'NONE',  ( 1.000000000000000000, 0.000000000000000000, 0.000000000000000000 ) ) ;
#240763 = CARTESIAN_POINT ( 'NONE',  ( 21.14999999999999858, 67.21339244341217523, -157.6731074845244223 ) ) ;
#240764 = CARTESIAN_POINT ( 'NONE',  ( -20.54999999999999716, 48.50000630096246823, -244.2465039064066161 ) ) ;
#240765 = LINE ( 'NONE', #85487, #64889 ) ;
#240766 = CARTESIAN_POINT ( 'NONE',  ( 16.27683809663750125, 66.65000000001161595, -60.27310748452439526 ) ) ;
#240768 = DIRECTION ( 'NONE',  ( 0.000000000000000000, 1.000000000000000000, 0.000000000000000000 ) ) ;
#240767 = CARTESIAN_POINT ( 'NONE',  ( -23.25000000000000000, 27.82020797438361370, -240.1085946414904413 ) ) ;
#240769 = CARTESIAN_POINT ( 'NONE',  ( -20.94999999999999929, 64.40000000001161595, -62.59490425424885274 ) ) ;
#240771 = ORIENTED_EDGE ( 'NONE', *, *, #251889, .T. ) ;
#240770 = CARTESIAN_POINT ( 'NONE',  ( 22.14074124539698829, 68.60992214896820940, -103.1221603803684417 ) ) ;
#240772 = DIRECTION ( 'NONE',  ( 0.000000000000000000, -1.000000000000000000, 0.000000000000000000 ) ) ;
#240773 = CARTESIAN_POINT ( 'NONE',  ( -18.59999996769639097, -9.363273769819199899, -141.1814939154657793 ) ) ;
#240774 = ORIENTED_EDGE ( 'NONE', *, *, #136034, .F. ) ;
#240775 = DIRECTION ( 'NONE',  ( 0.000000000000000000, 1.000000000000000000, 0.000000000000000000 ) ) ;
#240776 = CARTESIAN_POINT ( 'NONE',  ( -20.85000000000000142, 79.11538813396778380, -196.3722783875038544 ) ) ;
#240777 = DIRECTION ( 'NONE',  ( 1.000000000000000000, 0.000000000000000000, 0.000000000000000000 ) ) ;
#240778 = VERTEX_POINT ( 'NONE', #235416 ) ;
#240779 = AXIS2_PLACEMENT_3D ( 'NONE', #181253, #161692, #15 ) ;
#240780 = DIRECTION ( 'NONE',  ( -1.000000000000000000, -9.012599976027990443E-15, -6.882867235861669241E-14 ) ) ;
#240781 = ORIENTED_EDGE ( 'NONE', *, *, #206946, .T. ) ;
#240782 = ORIENTED_EDGE ( 'NONE', *, *, #113053, .F. ) ;
#240783 = DIRECTION ( 'NONE',  ( 0.000000000000000000, -0.9651348961777379554, 0.2617529984164210233 ) ) ;
#240784 = VERTEX_POINT ( 'NONE', #12558 ) ;
#240785 = DIRECTION ( 'NONE',  ( 0.000000000000000000, 0.000000000000000000, -1.000000000000000000 ) ) ;
#240786 = LINE ( 'NONE', #142936, #165611 ) ;
#240787 = CARTESIAN_POINT ( 'NONE',  ( -16.77683809663752257, 9.945835743215303282, -121.3360509808958341 ) ) ;
#240788 = DIRECTION ( 'NONE',  ( -1.000000000000000000, -0.000000000000000000, 0.000000000000000000 ) ) ;
#240789 = EDGE_LOOP ( 'NONE', ( #175565, #212517, #68758, #69732 ) ) ;
#240790 = DIRECTION ( 'NONE',  ( 0.000000000000000000, 0.000000000000000000, -1.000000000000000000 ) ) ;
#240791 = ADVANCED_FACE ( 'NONE', ( #16407 ), #174076, .F. ) ;
#240792 = LINE ( 'NONE', #26906, #91703 ) ;
#240793 = FACE_OUTER_BOUND ( 'NONE', #162661, .T. ) ;
#240794 = AXIS2_PLACEMENT_3D ( 'NONE', #247888, #227036, #245332 ) ;
#240795 = CIRCLE ( 'NONE', #2881, 12.77499999999999503 ) ;
#240796 = AXIS2_PLACEMENT_3D ( 'NONE', #88292, #195157, #193853 ) ;
#240797 = ADVANCED_FACE ( 'NONE', ( #192459 ), #94910, .F. ) ;
#240798 = AXIS2_PLACEMENT_3D ( 'NONE', #188514, #89404, #168995 ) ;
#240799 = ORIENTED_EDGE ( 'NONE', *, *, #209469, .T. ) ;
#240800 = EDGE_CURVE ( 'NONE', #135854, #86031, #11556, .T. ) ;
#240802 = VERTEX_POINT ( 'NONE', #114199 ) ;
#240801 = DIRECTION ( 'NONE',  ( -1.000000000000000000, 0.000000000000000000, -0.000000000000000000 ) ) ;
#240803 = EDGE_CURVE ( 'NONE', #12339, #152450, #193743, .T. ) ;
#240804 = LINE ( 'NONE', #156156, #180591 ) ;
#240805 = CARTESIAN_POINT ( 'NONE',  ( 18.43473516226063325, 78.23945979424732400, -231.5402134245487105 ) ) ;
#240806 = DIRECTION ( 'NONE',  ( 1.000000000000000000, 0.000000000000000000, 0.000000000000000000 ) ) ;
#240807 = CYLINDRICAL_SURFACE ( 'NONE', #208766, 0.09999999999999939493 ) ;
#240808 = DIRECTION ( 'NONE',  ( -1.000000000000000000, -0.000000000000000000, -0.000000000000000000 ) ) ;
#240809 = DIRECTION ( 'NONE',  ( 1.000000000000000000, 0.000000000000000000, 0.000000000000000000 ) ) ;
#240810 = ORIENTED_EDGE ( 'NONE', *, *, #23083, .T. ) ;
#240811 = CARTESIAN_POINT ( 'NONE',  ( -16.94107738177414291, 63.04990807712501777, -213.0142932718103737 ) ) ;
#240812 = LINE ( 'NONE', #82976, #48209 ) ;
#240813 = AXIS2_PLACEMENT_3D ( 'NONE', #169980, #30439, #171270 ) ;
#240814 = CARTESIAN_POINT ( 'NONE',  ( -22.39999999999999858, -1.124330358361676913E-15, 11.75043289245860834 ) ) ;
#240815 = CYLINDRICAL_SURFACE ( 'NONE', #195969, 0.1000000000000028644 ) ;
#240816 = B_SPLINE_CURVE_WITH_KNOTS ( 'NONE', 3,
 ( #118968, #99364, #178969, #133391, #212922, #34313, #14750, #219327, #184056, #82359, #143644, #44561, #65395, #223176, #199799, #180227, #124105, #1558, #139780, #40739, #120278, #203624 ),
 .UNSPECIFIED., .F., .F.,
 ( 4, 3, 3, 3, 3, 3, 3, 4 ),
 ( 0.000000000000000000, 7.307836821087015899E-06, 4.161455748548358328E-05, 7.576591810647013904E-05, 0.0001098090429817646371, 0.0001438003617351047054, 0.0001777914035423768207, 0.0002117966137402968007 ),
 .UNSPECIFIED. ) ;
#240817 = CARTESIAN_POINT ( 'NONE',  ( 22.57320508075688181, 11.48087284840413780, -198.4995883060917947 ) ) ;
#240818 = CARTESIAN_POINT ( 'NONE',  ( 20.87631937322884212, 65.52850496324762730, -61.94336160994270557 ) ) ;
#240819 = ADVANCED_FACE ( 'NONE', ( #136300 ), #157211, .F. ) ;
#240820 = CIRCLE ( 'NONE', #128388, 4.049999999999994493 ) ;
#240821 = EDGE_CURVE ( 'NONE', #185020, #113811, #136597, .T. ) ;
#240822 = ORIENTED_EDGE ( 'NONE', *, *, #179235, .F. ) ;
#240823 = ORIENTED_EDGE ( 'NONE', *, *, #87605, .T. ) ;
#240824 = CARTESIAN_POINT ( 'NONE',  ( 23.24999999999999645, 76.00000000001213607, -136.5231074845242745 ) ) ;
#240825 = CARTESIAN_POINT ( 'NONE',  ( 20.94999999999999574, 74.73821383144687047, -94.93660852097883662 ) ) ;
#240826 = DIRECTION ( 'NONE',  ( 1.000000000000000000, -0.000000000000000000, -0.000000000000000000 ) ) ;
#240827 = CARTESIAN_POINT ( 'NONE',  ( -16.97048326478265423, 23.41097584464640136, -231.1669605819007813 ) ) ;
#240828 = ORIENTED_EDGE ( 'NONE', *, *, #178575, .F. ) ;
#240829 = CARTESIAN_POINT ( 'NONE',  ( -16.87036670365548474, 66.01058118071060221, -149.0435473672224020 ) ) ;
#240830 = CARTESIAN_POINT ( 'NONE',  ( -16.94445028196808778, 9.992063609708889516, -113.1073301784184792 ) ) ;
#240831 = FACE_OUTER_BOUND ( 'NONE', #37864, .T. ) ;
#240832 = ADVANCED_FACE ( 'NONE', ( #253698 ), #176761, .F. ) ;
#240833 = CARTESIAN_POINT ( 'NONE',  ( -20.64999999999999858, 71.75000000001151079, -48.37310748452435405 ) ) ;
#240834 = AXIS2_PLACEMENT_3D ( 'NONE', #16901, #177277, #235923 ) ;
#240835 = EDGE_CURVE ( 'NONE', #121457, #189217, #251121, .T. ) ;
#240836 = VECTOR ( 'NONE', #63956, 1000.000000000000114 ) ;
#240837 = VECTOR ( 'NONE', #40102, 1000.000000000000000 ) ;
#240838 = EDGE_LOOP ( 'NONE', ( #132763, #201505, #92470, #124200, #46595, #31205, #100422 ) ) ;
#240839 = DIRECTION ( 'NONE',  ( -1.000000000000000000, 0.000000000000000000, 0.000000000000000000 ) ) ;
#240840 = ORIENTED_EDGE ( 'NONE', *, *, #32541, .T. ) ;
#240841 = DIRECTION ( 'NONE',  ( 0.000000000000000000, 1.000000000000000000, 0.000000000000000000 ) ) ;
#240842 = DIRECTION ( 'NONE',  ( -1.000000000000000000, 0.000000000000000000, 0.000000000000000000 ) ) ;
#240843 = CIRCLE ( 'NONE', #36868, 11.64999999999999325 ) ;
#240844 = CARTESIAN_POINT ( 'NONE',  ( -21.11825140030083858, 10.16595892622148511, -228.0477036210933477 ) ) ;
#240845 = EDGE_CURVE ( 'NONE', #20729, #59138, #203060, .T. ) ;
#240846 = DIRECTION ( 'NONE',  ( 1.000000000000000000, 0.000000000000000000, 0.000000000000000000 ) ) ;
#240847 = CARTESIAN_POINT ( 'NONE',  ( -20.94999999999999929, 77.83534155023627932, -91.46795619196130644 ) ) ;
#240848 = CARTESIAN_POINT ( 'NONE',  ( -22.50000000000000000, 7.790779598384560245, -100.4000000000000341 ) ) ;
#240849 = CARTESIAN_POINT ( 'NONE',  ( 22.47071067811865319, 76.00000000001195133, -103.0231074845243171 ) ) ;
#240850 = DIRECTION ( 'NONE',  ( 0.000000000000000000, 0.000000000000000000, -1.000000000000000000 ) ) ;
#240851 = EDGE_CURVE ( 'NONE', #240710, #9426, #123977, .T. ) ;
#240852 = CARTESIAN_POINT ( 'NONE',  ( -20.94999999999999929, -11.48912529306489994, -64.10000000000000853 ) ) ;
#240853 = DIRECTION ( 'NONE',  ( 1.652117596168391700E-15, 1.000000000000000000, -0.000000000000000000 ) ) ;
#240854 = DIRECTION ( 'NONE',  ( -1.020425574104004196E-15, -1.210927747993693964E-31, -1.000000000000000000 ) ) ;
#240855 = EDGE_CURVE ( 'NONE', #71546, #245454, #158495, .T. ) ;
#240856 = CIRCLE ( 'NONE', #3312, 6.329289321881358177 ) ;
#240857 = VECTOR ( 'NONE', #113742, 1000.000000000000000 ) ;
#240858 = AXIS2_PLACEMENT_3D ( 'NONE', #76056, #173929, #53930 ) ;
#240859 = DIRECTION ( 'NONE',  ( 0.000000000000000000, 0.000000000000000000, 1.000000000000000000 ) ) ;
#240860 = CARTESIAN_POINT ( 'NONE',  ( 21.05315837706675453, 56.18370558019869776, -227.9291052909716200 ) ) ;
#240861 = CIRCLE ( 'NONE', #182433, 0.1000000000000054040 ) ;
#240862 = ORIENTED_EDGE ( 'NONE', *, *, #244775, .F. ) ;
#240863 = CARTESIAN_POINT ( 'NONE',  ( 18.54999999999999716, 67.25000000001222134, -149.1731074845244223 ) ) ;
#240864 = CARTESIAN_POINT ( 'NONE',  ( 13.99999999999999822, 9.850000000011137402, -150.7500000000000284 ) ) ;
#240865 = EDGE_CURVE ( 'NONE', #191917, #108350, #161044, .T. ) ;
#240866 = ORIENTED_EDGE ( 'NONE', *, *, #161398, .F. ) ;
#240867 = SPHERICAL_SURFACE ( 'NONE', #39019, 0.1000000000000000056 ) ;
#240868 = AXIS2_PLACEMENT_3D ( 'NONE', #22435, #103206, #39439 ) ;
#240869 = LINE ( 'NONE', #80458, #247243 ) ;
#240870 = EDGE_CURVE ( 'NONE', #192641, #53900, #65691, .T. ) ;
#240871 = EDGE_LOOP ( 'NONE', ( #153160, #54373, #160829, #228249 ) ) ;
#240872 = CARTESIAN_POINT ( 'NONE',  ( -23.15000000000000213, 76.00000000001165290, -69.52310748452431710 ) ) ;
#240873 = LINE ( 'NONE', #162624, #172622 ) ;
#240874 = VECTOR ( 'NONE', #217748, 1000.000000000000000 ) ;
#240875 = ORIENTED_EDGE ( 'NONE', *, *, #213214, .F. ) ;
#240876 = AXIS2_PLACEMENT_3D ( 'NONE', #180743, #30348, #81594 ) ;
#240877 = AXIS2_PLACEMENT_3D ( 'NONE', #50093, #72244, #35706 ) ;
#240879 = EDGE_LOOP ( 'NONE', ( #62381, #160515, #251251, #30300 ) ) ;
#240878 = VECTOR ( 'NONE', #186096, 1000.000000000000000 ) ;
#240880 = CARTESIAN_POINT ( 'NONE',  ( -21.05000000000000071, 76.00000000001213607, -136.5231074845242745 ) ) ;
#240881 = ORIENTED_EDGE ( 'NONE', *, *, #188144, .T. ) ;
#240882 = CIRCLE ( 'NONE', #65908, 0.09999999999999834022 ) ;
#240883 = FACE_OUTER_BOUND ( 'NONE', #96992, .T. ) ;
#240884 = DIRECTION ( 'NONE',  ( -1.000000000000000000, 0.000000000000000000, 0.000000000000000000 ) ) ;
#240886 = DIRECTION ( 'NONE',  ( 0.000000000000000000, 0.2128009952263598958, -0.9770955615653316162 ) ) ;
#240885 = PRODUCT_DEFINITION_CONTEXT ( 'detailed design', #255667, 'design' ) ;
#240887 = DIRECTION ( 'NONE',  ( 0.000000000000000000, -0.9126074666063770380, -0.4088369013363281068 ) ) ;
#240888 = DIRECTION ( 'NONE',  ( 1.000000000000000000, 0.000000000000000000, 0.000000000000000000 ) ) ;
#240889 = CARTESIAN_POINT ( 'NONE',  ( -17.04761207306817639, 10.02645087340892438, -87.85000000000002274 ) ) ;
#240890 = CARTESIAN_POINT ( 'NONE',  ( 21.05000000000000071, -11.64999999998883595, -167.4999999999999432 ) ) ;
#240891 = CARTESIAN_POINT ( 'NONE',  ( -23.15000000000000213, 85.00000000001159606, -59.62913836187181715 ) ) ;
#240893 = ORIENTED_EDGE ( 'NONE', *, *, #107567, .F. ) ;
#240892 = LINE ( 'NONE', #158810, #173506 ) ;
#240894 = VERTEX_POINT ( 'NONE', #241849 ) ;
#240896 = DIRECTION ( 'NONE',  ( 0.000000000000000000, 0.000000000000000000, -1.000000000000000000 ) ) ;
#240895 = DIRECTION ( 'NONE',  ( 0.000000000000000000, 0.000000000000000000, 1.000000000000000000 ) ) ;
#240898 = ORIENTED_EDGE ( 'NONE', *, *, #127030, .F. ) ;
#240897 = CARTESIAN_POINT ( 'NONE',  ( 21.14999999999999858, 10.71339244341104013, -146.2500000000000284 ) ) ;
#240899 = ORIENTED_EDGE ( 'NONE', *, *, #160358, .T. ) ;
#240900 = DIRECTION ( 'NONE',  ( 0.7071359030027593029, 0.7070776581709197206, 0.000000000000000000 ) ) ;
#240901 = VECTOR ( 'NONE', #55078, 1000.000000000000000 ) ;
#240902 = LINE ( 'NONE', #89505, #242756 ) ;
#240903 = DIRECTION ( 'NONE',  ( -0.000000000000000000, -0.000000000000000000, 1.000000000000000000 ) ) ;
#240904 = CYLINDRICAL_SURFACE ( 'NONE', #135721, 0.1000000000000028644 ) ;
#240905 = CYLINDRICAL_SURFACE ( 'NONE', #258090, 3.999999999999996447 ) ;
#240906 = DIRECTION ( 'NONE',  ( 0.000000000000000000, -7.272083257015735086E-15, 1.000000000000000000 ) ) ;
#240907 = VECTOR ( 'NONE', #228895, 1000.000000000000000 ) ;
#240908 = AXIS2_PLACEMENT_3D ( 'NONE', #102154, #143872, #146432 ) ;
#240909 = LINE ( 'NONE', #242178, #139464 ) ;
#240910 = ORIENTED_EDGE ( 'NONE', *, *, #49995, .F. ) ;
#240911 = ORIENTED_EDGE ( 'NONE', *, *, #120704, .F. ) ;
#240912 = DIRECTION ( 'NONE',  ( -1.000000000000000000, -0.000000000000000000, -0.000000000000000000 ) ) ;
#240913 = VERTEX_POINT ( 'NONE', #119346 ) ;
#240914 = CARTESIAN_POINT ( 'NONE',  ( 20.94999999999999929, 8.776282895303628706, -142.5586289951409640 ) ) ;
#240915 = EDGE_LOOP ( 'NONE', ( #152246, #123830, #121511, #248226 ) ) ;
#240916 = CARTESIAN_POINT ( 'NONE',  ( -16.90138253750127362, 14.12954199452179616, -219.1198060924749029 ) ) ;
#240917 = CONICAL_SURFACE ( 'NONE', #116040, 4.299999999999964295, 0.7853981633974466137 ) ;
#240918 = CARTESIAN_POINT ( 'NONE',  ( -12.26136940704871670, 48.33137198101100296, -234.0751437313343502 ) ) ;
#240919 = EDGE_CURVE ( 'NONE', #47980, #239317, #111503, .T. ) ;
#240920 = DIRECTION ( 'NONE',  ( 0.7071067811865708874, -0.3338907855511046296, -0.6233112732207185536 ) ) ;
#240921 = CARTESIAN_POINT ( 'NONE',  ( -21.07928932188134041, 75.90110485435833709, -209.8516241409176644 ) ) ;
#240922 = ORIENTED_EDGE ( 'NONE', *, *, #24211, .F. ) ;
#240923 = AXIS2_PLACEMENT_3D ( 'NONE', #164550, #47130, #48431 ) ;
#240924 = DIRECTION ( 'NONE',  ( 1.000000000000000000, 0.000000000000000000, 0.000000000000000000 ) ) ;
#240925 = ORIENTED_EDGE ( 'NONE', *, *, #16628, .T. ) ;
#240926 = ADVANCED_FACE ( 'NONE', ( #642 ), #103601, .F. ) ;
#240927 = CARTESIAN_POINT ( 'NONE',  ( 22.40736611211992368, 1.115600667400684642E-11, -122.3504291924552234 ) ) ;
#240929 = EDGE_CURVE ( 'NONE', #182355, #219709, #91013, .T. ) ;
#240928 = AXIS2_PLACEMENT_3D ( 'NONE', #1833, #78799, #158399 ) ;
#240931 = CARTESIAN_POINT ( 'NONE',  ( 18.39999999999999503, 65.08943781962308606, -222.1672656287770451 ) ) ;
#240930 = CIRCLE ( 'NONE', #78424, 0.1000000000000028644 ) ;
#240932 = PLANE ( 'NONE',  #4958 ) ;
#240933 = AXIS2_PLACEMENT_3D ( 'NONE', #239836, #56021, #256765 ) ;
#240934 = DIRECTION ( 'NONE',  ( 1.000000000000000000, 0.000000000000000000, 0.000000000000000000 ) ) ;
#240935 = ORIENTED_EDGE ( 'NONE', *, *, #122078, .T. ) ;
#240936 = DIRECTION ( 'NONE',  ( 1.000000000000000000, 0.000000000000000000, 0.000000000000000000 ) ) ;
#240937 = VERTEX_POINT ( 'NONE', #217124 ) ;
#240940 = ORIENTED_EDGE ( 'NONE', *, *, #202364, .F. ) ;
#240939 = CARTESIAN_POINT ( 'NONE',  ( -23.25000000000000000, 1.115600667400684642E-11, -200.9999999999999432 ) ) ;
#240938 = CARTESIAN_POINT ( 'NONE',  ( 18.47073956224761204, 47.01875662081600638, -255.2888406289864918 ) ) ;
#240941 = CARTESIAN_POINT ( 'NONE',  ( 23.25000000000000000, -5.011722593499792211, -233.2041167654973322 ) ) ;
#240942 = ORIENTED_EDGE ( 'NONE', *, *, #122702, .F. ) ;
#240943 = DIRECTION ( 'NONE',  ( 0.000000000000000000, 0.000000000000000000, -1.000000000000000000 ) ) ;
#240944 = ORIENTED_EDGE ( 'NONE', *, *, #57085, .F. ) ;
#240945 = LINE ( 'NONE', #180975, #222011 ) ;
#240946 = ADVANCED_FACE ( 'NONE', ( #219710 ), #121921, .F. ) ;
#240947 = CARTESIAN_POINT ( 'NONE',  ( -16.94107738177414291, 10.01423928514777373, -54.44999999999999574 ) ) ;
#240948 = CARTESIAN_POINT ( 'NONE',  ( -22.44366136229477249, -3.135927281448380732, -228.2235526381227260 ) ) ;
#240950 = ORIENTED_EDGE ( 'NONE', *, *, #87684, .F. ) ;
#240949 = LINE ( 'NONE', #199261, #251722 ) ;
#240951 = CARTESIAN_POINT ( 'NONE',  ( -18.50000000000000000, 68.87972903831453664, -132.8635444426850825 ) ) ;
#240952 = ORIENTED_EDGE ( 'NONE', *, *, #183341, .F. ) ;
#240953 = DIRECTION ( 'NONE',  ( 0.000000000000000000, -0.9126074666063769270, -0.4088369013363280513 ) ) ;
#240954 = CARTESIAN_POINT ( 'NONE',  ( 18.59999999999999076, 66.47189219944506533, -213.6315278230738102 ) ) ;
#240955 = CARTESIAN_POINT ( 'NONE',  ( -18.50000000000000000, -9.399999999988850163, -140.8820418481727188 ) ) ;
#240956 = ORIENTED_EDGE ( 'NONE', *, *, #132687, .T. ) ;
#240957 = DIRECTION ( 'NONE',  ( 0.000000000000000000, 0.2128009952263403282, -0.9770955615653358350 ) ) ;
#240958 = ORIENTED_EDGE ( 'NONE', *, *, #189412, .T. ) ;
#240959 = DIRECTION ( 'NONE',  ( 0.000000000000000000, 0.8814952561688430555, -0.4721928772777346239 ) ) ;
#240960 = EDGE_CURVE ( 'NONE', #17763, #12698, #178336, .T. ) ;
#240961 = CARTESIAN_POINT ( 'NONE',  ( -20.94999999999999929, 76.00000000001139711, -31.92310748452432279 ) ) ;
#240962 = CARTESIAN_POINT ( 'NONE',  ( -18.59999999999999787, -9.849999999999994316, 30.09999999999999787 ) ) ;
#240963 = EDGE_CURVE ( 'NONE', #172274, #133, #120085, .T. ) ;
#240965 = ORIENTED_EDGE ( 'NONE', *, *, #11236, .F. ) ;
#240964 = DIRECTION ( 'NONE',  ( 0.000000000000000000, 6.982962677686266711E-15, -1.000000000000000000 ) ) ;
#240966 = CARTESIAN_POINT ( 'NONE',  ( -18.34374000495059676, 64.52683809664929981, -78.77310748452438816 ) ) ;
#240967 = CARTESIAN_POINT ( 'NONE',  ( -23.15000000000000213, 1.115600667400684642E-11, -130.0000000000000284 ) ) ;
#240968 = CARTESIAN_POINT ( 'NONE',  ( 21.05000000000000071, 77.36087058720393372, -94.95010955743333625 ) ) ;
#240970 = ADVANCED_FACE ( 'NONE', ( #102302 ), #174260, .F. ) ;
#240969 = VERTEX_POINT ( 'NONE', #22835 ) ;
#240971 = AXIS2_PLACEMENT_3D ( 'NONE', #15732, #232201, #73141 ) ;
#240973 = AXIS2_PLACEMENT_3D ( 'NONE', #228827, #224942, #108864 ) ;
#240972 = DIRECTION ( 'NONE',  ( 0.000000000000000000, 0.8814952561688428334, -0.4721928772777348460 ) ) ;
#240974 = DIRECTION ( 'NONE',  ( 0.000000000000000000, -7.026728003956695223E-15, 1.000000000000000000 ) ) ;
#240975 = ORIENTED_EDGE ( 'NONE', *, *, #68251, .T. ) ;
#240976 = VECTOR ( 'NONE', #199786, 1000.000000000000000 ) ;
#240977 = CARTESIAN_POINT ( 'NONE',  ( -22.47071067811865319, 65.11488425470511743, -243.2801022963548689 ) ) ;
#240978 = ORIENTED_EDGE ( 'NONE', *, *, #8314, .F. ) ;
#240979 = DIRECTION ( 'NONE',  ( -1.000000000000000000, 0.000000000000000000, -0.000000000000000000 ) ) ;
#240980 = CIRCLE ( 'NONE', #157826, 2.000000000000001776 ) ;
#240981 = ORIENTED_EDGE ( 'NONE', *, *, #220135, .T. ) ;
#240983 = ORIENTED_EDGE ( 'NONE', *, *, #49033, .F. ) ;
#240982 = CARTESIAN_POINT ( 'NONE',  ( -18.79999999999999716, 11.49641995933507843, -1.885425182446134107 ) ) ;
#240987 = ADVANCED_FACE ( 'NONE', ( #43662 ), #82740, .T. ) ;
#240986 = EDGE_LOOP ( 'NONE', ( #68478, #196931, #219426, #254363 ) ) ;
#240985 = VERTEX_POINT ( 'NONE', #179336 ) ;
#240984 = DIRECTION ( 'NONE',  ( 1.000000000000000000, -0.000000000000000000, -0.000000000000000000 ) ) ;
#240989 = CIRCLE ( 'NONE', #103765, 0.6000000000000033085 ) ;
#240988 = CARTESIAN_POINT ( 'NONE',  ( 20.95262331984812221, 65.49584273722207683, -95.46221915493103438 ) ) ;
#240990 = AXIS2_PLACEMENT_3D ( 'NONE', #250362, #230821, #192965 ) ;
#240991 = CARTESIAN_POINT ( 'NONE',  ( 13.99999999999999822, 9.850000000011137402, -50.24999999999999289 ) ) ;
#240992 = CARTESIAN_POINT ( 'NONE',  ( 21.97500000000000497, 9.750000000011153745, -88.25000000000005684 ) ) ;
#240993 = CIRCLE ( 'NONE', #57807, 0.1000000000000028644 ) ;
#240995 = DIRECTION ( 'NONE',  ( -0.000000000000000000, -2.891205793294679805E-16, 1.000000000000000000 ) ) ;
#240994 = CARTESIAN_POINT ( 'NONE',  ( 20.94999999999999929, 46.32970330538243786, -243.0551226933711746 ) ) ;
#240996 = CARTESIAN_POINT ( 'NONE',  ( -16.87331047859649757, 9.950000000011138823, -87.85000000000005116 ) ) ;
#240997 = CARTESIAN_POINT ( 'NONE',  ( -17.78241384941187420, 65.14442424719499058, -59.27406981206009817 ) ) ;
#240998 = DIRECTION ( 'NONE',  ( 2.952720810173289112E-16, -1.000000000000000000, 0.000000000000000000 ) ) ;
#240999 = AXIS2_PLACEMENT_3D ( 'NONE', #123336, #184578, #226249 ) ;
#241001 = CARTESIAN_POINT ( 'NONE',  ( -22.50000000000088463, 75.95463834342453424, -148.1736163187296995 ) ) ;
#241000 = CYLINDRICAL_SURFACE ( 'NONE', #251195, 0.09999999999999939493 ) ;
#241002 = ORIENTED_EDGE ( 'NONE', *, *, #212339, .F. ) ;
#241003 = ORIENTED_EDGE ( 'NONE', *, *, #19152, .T. ) ;
#241004 = EDGE_CURVE ( 'NONE', #120848, #151382, #21537, .T. ) ;
#241005 = DIRECTION ( 'NONE',  ( 0.000000000000000000, 0.000000000000000000, 1.000000000000000000 ) ) ;
#241006 = ADVANCED_FACE ( 'NONE', ( #84009 ), #11250, .T. ) ;
#241008 = VERTEX_POINT ( 'NONE', #144025 ) ;
#241007 = LINE ( 'NONE', #41542, #228554 ) ;
#241009 = VERTEX_POINT ( 'NONE', #50073 ) ;
#241010 = CARTESIAN_POINT ( 'NONE',  ( -21.46681500593124170, 6.857511159386057820, -9.855405879761855605E-16 ) ) ;
#241011 = VERTEX_POINT ( 'NONE', #129620 ) ;
#241012 = DIRECTION ( 'NONE',  ( 0.000000000000000000, 1.000000000000000000, 0.000000000000000000 ) ) ;
#241013 = ADVANCED_FACE ( 'NONE', ( #46213 ), #20104, .F. ) ;
#241014 = ADVANCED_FACE ( 'NONE', ( #125748 ), #226114, .T. ) ;
#241015 = ORIENTED_EDGE ( 'NONE', *, *, #22818, .T. ) ;
#241016 = CYLINDRICAL_SURFACE ( 'NONE', #118799, 0.09999999999999939493 ) ;
#241017 = DIRECTION ( 'NONE',  ( 0.000000000000000000, 0.000000000000000000, 1.000000000000000000 ) ) ;
#241018 = AXIS2_PLACEMENT_3D ( 'NONE', #127231, #168968, #170258 ) ;
#241019 = VECTOR ( 'NONE', #106597, 1000.000000000000227 ) ;
#241020 = AXIS2_PLACEMENT_3D ( 'NONE', #55436, #175446, #201083 ) ;
#241021 = EDGE_CURVE ( 'NONE', #126194, #111115, #61787, .T. ) ;
#241023 = ORIENTED_EDGE ( 'NONE', *, *, #172568, .F. ) ;
#241022 = ORIENTED_EDGE ( 'NONE', *, *, #151680, .T. ) ;
#241024 = ORIENTED_EDGE ( 'NONE', *, *, #231509, .T. ) ;
#241026 = EDGE_CURVE ( 'NONE', #114442, #216036, #147907, .T. ) ;
#241025 = DIRECTION ( 'NONE',  ( 0.000000000000000000, -0.6324589521315897578, 0.7745938767306462802 ) ) ;
#241027 = VERTEX_POINT ( 'NONE', #7087 ) ;
#241028 = VERTEX_POINT ( 'NONE', #89194 ) ;
#241029 = FACE_OUTER_BOUND ( 'NONE', #15888, .T. ) ;
#241031 = EDGE_LOOP ( 'NONE', ( #218713, #2808, #88539, #12096 ) ) ;
#241030 = DIRECTION ( 'NONE',  ( 1.000000000000000000, -3.265361837132813093E-16, -2.280189983783949500E-30 ) ) ;
#241032 = AXIS2_PLACEMENT_3D ( 'NONE', #50952, #69277, #151386 ) ;
#241033 = EDGE_CURVE ( 'NONE', #122253, #48993, #65878, .T. ) ;
#241035 = DIRECTION ( 'NONE',  ( 0.000000000000000000, 1.000000000000000000, -0.000000000000000000 ) ) ;
#241034 = DIRECTION ( 'NONE',  ( -0.000000000000000000, 1.000000000000000000, 6.982962677686267499E-15 ) ) ;
#241036 = DIRECTION ( 'NONE',  ( 1.000000000000000000, 0.000000000000000000, 0.000000000000000000 ) ) ;
#241037 = CARTESIAN_POINT ( 'NONE',  ( 23.24999999999999289, 64.25000000001220712, -148.2731074845243882 ) ) ;
#241038 = DIRECTION ( 'NONE',  ( 0.000000000000000000, 0.000000000000000000, 1.000000000000000000 ) ) ;
#241039 = ORIENTED_EDGE ( 'NONE', *, *, #243929, .T. ) ;
#241040 = EDGE_LOOP ( 'NONE', ( #243563, #202368, #58194, #5012 ) ) ;
#241041 = LINE ( 'NONE', #238461, #257997 ) ;
#241042 = CARTESIAN_POINT ( 'NONE',  ( -20.94999999999999929, 0.000000000000000000, -21.70000000000000284 ) ) ;
#241044 = EDGE_CURVE ( 'NONE', #11322, #26951, #170075, .T. ) ;
#241043 = CARTESIAN_POINT ( 'NONE',  ( -20.64999999999999858, 84.66355140188093742, -79.04720860259155302 ) ) ;
#241045 = ORIENTED_EDGE ( 'NONE', *, *, #108656, .T. ) ;
#241046 = AXIS2_PLACEMENT_3D ( 'NONE', #226836, #5196, #207298 ) ;
#241048 = CARTESIAN_POINT ( 'NONE',  ( -21.65000000000000213, 7.250000000011138646, -121.3500000000000369 ) ) ;
#241047 = AXIS2_PLACEMENT_3D ( 'NONE', #130436, #146144, #10508 ) ;
#241049 = EDGE_CURVE ( 'NONE', #256858, #89873, #30537, .T. ) ;
#241050 = ADVANCED_FACE ( 'NONE', ( #248280, #168795 ), #48786, .T. ) ;
#241051 = VECTOR ( 'NONE', #49453, 1000.000000000000000 ) ;
#241052 = DIRECTION ( 'NONE',  ( 0.7071359030027296599, 0.1850796971394779999, 0.6824253222084255555 ) ) ;
#241053 = DIRECTION ( 'NONE',  ( -1.020425574104004394E-15, -0.9126074666063769270, -0.4088369013363280513 ) ) ;
#241054 = AXIS2_PLACEMENT_3D ( 'NONE', #226711, #149780, #31133 ) ;
#241055 = EDGE_LOOP ( 'NONE', ( #207743, #210917, #203213, #118868, #18687 ) ) ;
#241056 = EDGE_LOOP ( 'NONE', ( #215572, #98311, #147619, #155824 ) ) ;
#241057 = EDGE_CURVE ( 'NONE', #230071, #99483, #219997, .T. ) ;
#241058 = LINE ( 'NONE', #221449, #13555 ) ;
#241059 = CARTESIAN_POINT ( 'NONE',  ( -20.64999999999999858, 4.350000000011156054, -188.6499999999999488 ) ) ;
#241060 = ORIENTED_EDGE ( 'NONE', *, *, #11089, .F. ) ;
#241061 = DIRECTION ( 'NONE',  ( 0.000000000000000000, -0.4088369013363205573, 0.9126074666063803686 ) ) ;
#241062 = ORIENTED_EDGE ( 'NONE', *, *, #112348, .F. ) ;
#241063 = CARTESIAN_POINT ( 'NONE',  ( -22.39999999999999858, 1.115486826172573664E-11, -55.35042919245524473 ) ) ;
#241064 = CARTESIAN_POINT ( 'NONE',  ( -18.59999999999999787, -1.164121893230052995, -74.71484808557160306 ) ) ;
#241066 = CARTESIAN_POINT ( 'NONE',  ( -20.85882249326303040, 68.11287320386161070, -224.1382462126928488 ) ) ;
#241065 = CARTESIAN_POINT ( 'NONE',  ( -18.59999999999999787, 18.86061765788380740, -226.6874733728449485 ) ) ;
#241067 = EDGE_CURVE ( 'NONE', #74558, #142715, #65785, .T. ) ;
#241068 = AXIS2_PLACEMENT_3D ( 'NONE', #235267, #133603, #137444 ) ;
#241069 = AXIS2_PLACEMENT_3D ( 'NONE', #187615, #45517, #149778 ) ;
#241070 = DIRECTION ( 'NONE',  ( -3.265361837132813093E-16, 1.000000000000000000, 0.000000000000000000 ) ) ;
#241071 = CARTESIAN_POINT ( 'NONE',  ( -16.89268316805466341, 66.04827818676967865, -90.37885996306994230 ) ) ;
#241072 = EDGE_CURVE ( 'NONE', #148316, #177021, #207554, .T. ) ;
#241073 = ORIENTED_EDGE ( 'NONE', *, *, #123838, .F. ) ;
#241074 = AXIS2_PLACEMENT_3D ( 'NONE', #43956, #120956, #222570 ) ;
#241075 = LINE ( 'NONE', #156422, #164872 ) ;
#241078 = ORIENTED_EDGE ( 'NONE', *, *, #154731, .T. ) ;
#241077 = VERTEX_POINT ( 'NONE', #29280 ) ;
#241076 = AXIS2_PLACEMENT_3D ( 'NONE', #35207, #254193, #233393 ) ;
#241079 = ORIENTED_EDGE ( 'NONE', *, *, #49607, .T. ) ;
#241080 = AXIS2_PLACEMENT_3D ( 'NONE', #58935, #199791, #198477 ) ;
#241081 = AXIS2_PLACEMENT_3D ( 'NONE', #30047, #226933, #207389 ) ;
#241082 = ORIENTED_EDGE ( 'NONE', *, *, #256839, .T. ) ;
#241083 = VECTOR ( 'NONE', #7884, 1000.000000000000000 ) ;
#241084 = DIRECTION ( 'NONE',  ( 0.000000000000000000, -7.304098846218085561E-15, 1.000000000000000000 ) ) ;
#241085 = CARTESIAN_POINT ( 'NONE',  ( -23.25000000000000000, 87.75000000001173817, -72.62310748452422615 ) ) ;
#241086 = CARTESIAN_POINT ( 'NONE',  ( 21.05000000000000071, 76.52350599684427834, -201.5928376921694678 ) ) ;
#241087 = LINE ( 'NONE', #62436, #48647 ) ;
#241088 = DIRECTION ( 'NONE',  ( 0.000000000000000000, -1.000000000000000000, 6.308085367188393199E-16 ) ) ;
#241089 = EDGE_CURVE ( 'NONE', #195545, #104039, #8396, .T. ) ;
#241090 = AXIS2_PLACEMENT_3D ( 'NONE', #17470, #18753, #94435 ) ;
#241092 = CARTESIAN_POINT ( 'NONE',  ( -20.54999999999999716, 71.65000000001222702, -148.7731074845243882 ) ) ;
#241091 = CYLINDRICAL_SURFACE ( 'NONE', #16397, 0.1000000000000070832 ) ;
#241094 = VERTEX_POINT ( 'NONE', #5785 ) ;
#241093 = DIRECTION ( 'NONE',  ( 0.000000000000000000, 6.982962677686266711E-15, -1.000000000000000000 ) ) ;
#241095 = ORIENTED_EDGE ( 'NONE', *, *, #84302, .F. ) ;
#241096 = PLANE ( 'NONE',  #71690 ) ;
#241097 = ORIENTED_EDGE ( 'NONE', *, *, #49394, .T. ) ;
#241098 = ORIENTED_EDGE ( 'NONE', *, *, #226791, .F. ) ;
#241099 = DIRECTION ( 'NONE',  ( -1.000000000000000000, -2.952720810173289112E-16, 0.000000000000000000 ) ) ;
#241100 = CARTESIAN_POINT ( 'NONE',  ( -16.87683809663752399, 66.05000000001261640, -190.8731074845244393 ) ) ;
#241101 = CARTESIAN_POINT ( 'NONE',  ( -16.79270642812312531, 66.05375578307346984, -48.68417420596193779 ) ) ;
#241102 = CARTESIAN_POINT ( 'NONE',  ( 21.05000000000000071, 65.51556651037091683, -196.0663016830324636 ) ) ;
#241103 = ADVANCED_BREP_SHAPE_REPRESENTATION ( '', ( #22252, #2425 ), #52661 ) ;
#241104 = AXIS2_PLACEMENT_3D ( 'NONE', #32193, #153450, #135099 ) ;
#241105 = AXIS2_PLACEMENT_3D ( 'NONE', #244988, #3815, #123769 ) ;
#241106 = CYLINDRICAL_SURFACE ( 'NONE', #21781, 11.75000000000000000 ) ;
#241107 = VERTEX_POINT ( 'NONE', #223555 ) ;
#241108 = ORIENTED_EDGE ( 'NONE', *, *, #225795, .T. ) ;
#241109 = CARTESIAN_POINT ( 'NONE',  ( -20.94999999999999929, 1.115600667400684642E-11, -167.4999999999999716 ) ) ;
#241110 = ORIENTED_EDGE ( 'NONE', *, *, #82390, .T. ) ;
#241111 = DIRECTION ( 'NONE',  ( -0.000000000000000000, -6.982962677686266711E-15, 1.000000000000000000 ) ) ;
#241112 = LINE ( 'NONE', #62461, #248450 ) ;
#241113 = CARTESIAN_POINT ( 'NONE',  ( -23.15000000000000213, 76.00000000001170974, -69.52310748452431710 ) ) ;
#241114 = CYLINDRICAL_SURFACE ( 'NONE', #111353, 0.09999999999999939493 ) ;
#241115 = DIRECTION ( 'NONE',  ( 1.000000000000000000, 0.000000000000000000, 0.000000000000000000 ) ) ;
#241116 = DIRECTION ( 'NONE',  ( 0.000000000000000000, 0.2128009952263601456, -0.9770955615653316162 ) ) ;
#241117 = AXIS2_PLACEMENT_3D ( 'NONE', #217663, #63748, #183710 ) ;
#241118 = DIRECTION ( 'NONE',  ( -2.915501640297152804E-16, -1.000000000000000000, -6.997203936713167125E-15 ) ) ;
#241119 = CYLINDRICAL_SURFACE ( 'NONE', #108381, 0.1000000000000028644 ) ;
#241120 = AXIS2_PLACEMENT_3D ( 'NONE', #47163, #186717, #167175 ) ;
#241121 = CARTESIAN_POINT ( 'NONE',  ( 18.49999999999999289, 65.79142135624982757, -178.8731074845244109 ) ) ;
#241122 = ADVANCED_FACE ( 'NONE', ( #90476 ), #124490, .F. ) ;
#241123 = FACE_OUTER_BOUND ( 'NONE', #115584, .T. ) ;
#241124 = DIRECTION ( 'NONE',  ( 0.000000000000000000, -1.000000000000000000, 0.000000000000000000 ) ) ;
#241125 = ADVANCED_FACE ( 'NONE', ( #196025 ), #151774, .F. ) ;
#241126 = VECTOR ( 'NONE', #35819, 1000.000000000000000 ) ;
#241127 = ORIENTED_EDGE ( 'NONE', *, *, #4360, .F. ) ;
#241128 = EDGE_CURVE ( 'NONE', #43598, #212847, #56474, .T. ) ;
#241129 = DIRECTION ( 'NONE',  ( 0.000000000000000000, 0.2818822000685679008, -0.9594490217226259166 ) ) ;
#241130 = EDGE_CURVE ( 'NONE', #11112, #138031, #28523, .T. ) ;
#241131 = VERTEX_POINT ( 'NONE', #133469 ) ;
#241132 = DIRECTION ( 'NONE',  ( -1.000000000000000000, -0.000000000000000000, 0.000000000000000000 ) ) ;
#241133 = CARTESIAN_POINT ( 'NONE',  ( -21.05000000000000071, -11.39257802169451672, -170.5739495798319183 ) ) ;
#241134 = DIRECTION ( 'NONE',  ( 1.000000000000000000, -0.000000000000000000, -0.000000000000000000 ) ) ;
#241135 = AXIS2_PLACEMENT_3D ( 'NONE', #255503, #19530, #238556 ) ;
#241136 = VERTEX_POINT ( 'NONE', #252122 ) ;
#241137 = CYLINDRICAL_SURFACE ( 'NONE', #138142, 0.09999999999998898659 ) ;
#241138 = AXIS2_PLACEMENT_3D ( 'NONE', #175259, #253455, #213049 ) ;
#241139 = LINE ( 'NONE', #138140, #218679 ) ;
#241140 = LINE ( 'NONE', #85861, #212903 ) ;
#241141 = CARTESIAN_POINT ( 'NONE',  ( -16.77683809663752257, 14.15196434607590348, -219.2423291894720307 ) ) ;
#241142 = CARTESIAN_POINT ( 'NONE',  ( -16.93521499325732549, 9.994786119814678571, -121.4071085410935780 ) ) ;
#241143 = LINE ( 'NONE', #117325, #223645 ) ;
#241144 = VERTEX_POINT ( 'NONE', #153077 ) ;
#241145 = DIRECTION ( 'NONE',  ( 0.000000000000000000, 0.000000000000000000, -1.000000000000000000 ) ) ;
#241147 = EDGE_LOOP ( 'NONE', ( #115725, #39369, #46770, #135208 ) ) ;
#241146 = FACE_OUTER_BOUND ( 'NONE', #141189, .T. ) ;
#241148 = CARTESIAN_POINT ( 'NONE',  ( 21.05000000000000071, 53.86595165227826243, -236.3638196928718855 ) ) ;
#241149 = DIRECTION ( 'NONE',  ( 0.000000000000000000, 0.4088369013363281623, -0.9126074666063771490 ) ) ;
#241150 = CARTESIAN_POINT ( 'NONE',  ( 21.05000000000000071, 65.27628289530434813, -90.87310748452438247 ) ) ;
#241151 = ORIENTED_EDGE ( 'NONE', *, *, #239888, .F. ) ;
#241152 = B_SPLINE_CURVE_WITH_KNOTS ( 'NONE', 3,
 ( #77154, #38060, #216672, #175033, #74637, #115001, #154178, #155459, #73342, #18474, #15936, #55001, #97980, #212832, #197096, #234960, #135833, #215378, #117569 ),
 .UNSPECIFIED., .F., .F.,
 ( 4, 3, 3, 3, 3, 3, 4 ),
 ( 0.000000000000000000, 1.655171619026035414E-05, 2.773500582848695921E-05, 5.941817267378285075E-05, 0.0001114174635873568916, 0.0001914169455916313886, 0.0002627181070750597572 ),
 .UNSPECIFIED. ) ;
#241153 = DIRECTION ( 'NONE',  ( 0.000000000000000000, -6.982962677686266711E-15, 1.000000000000000000 ) ) ;
#241154 = EDGE_LOOP ( 'NONE', ( #108972, #48660, #107814, #2069 ) ) ;
#241155 = CYLINDRICAL_SURFACE ( 'NONE', #29549, 0.9000000000000014655 ) ;
#241156 = EDGE_CURVE ( 'NONE', #79153, #14935, #95616, .T. ) ;
#241157 = CARTESIAN_POINT ( 'NONE',  ( -18.59999999999999787, 77.16412189325286874, -61.60825939895269698 ) ) ;
#241158 = ORIENTED_EDGE ( 'NONE', *, *, #231116, .T. ) ;
#241159 = EDGE_LOOP ( 'NONE', ( #98495, #189387, #166407, #247259 ) ) ;
#241160 = CARTESIAN_POINT ( 'NONE',  ( 20.94999999999999929, 5.500000000011153745, -155.0947339810869323 ) ) ;
#241161 = FACE_OUTER_BOUND ( 'NONE', #228549, .T. ) ;
#241162 = EDGE_CURVE ( 'NONE', #237270, #112967, #70198, .T. ) ;
#241163 = CARTESIAN_POINT ( 'NONE',  ( -21.05000000000000071, 74.75000000001207923, -128.5231074845243029 ) ) ;
#241164 = CARTESIAN_POINT ( 'NONE',  ( 22.49231231312462853, 64.35001509633539740, -203.5841603721258082 ) ) ;
#241165 = CARTESIAN_POINT ( 'NONE',  ( 18.49999999999999289, 10.49142135624846617, -125.2500000000000426 ) ) ;
#241166 = DIRECTION ( 'NONE',  ( -0.000000000000000000, 1.000000000000000000, 7.172728831056617961E-15 ) ) ;
#241167 = ADVANCED_FACE ( 'NONE', ( #176468 ), #36884, .T. ) ;
#241169 = CARTESIAN_POINT ( 'NONE',  ( -18.79999999999999716, -1.800000000000000044, -11.61130914238355771 ) ) ;
#241168 = CARTESIAN_POINT ( 'NONE',  ( 21.05000000000000071, -1.362597741190629819, -194.8440013506711068 ) ) ;
#241170 = CIRCLE ( 'NONE', #24704, 0.09999999999998898659 ) ;
#241172 = CARTESIAN_POINT ( 'NONE',  ( -23.15000000000000213, 85.50000000001222134, -146.4170766071767389 ) ) ;
#241171 = AXIS2_PLACEMENT_3D ( 'NONE', #46012, #125556, #206386 ) ;
#241173 = CARTESIAN_POINT ( 'NONE',  ( -20.54999999999999716, 7.150000000011155876, -146.3500000000000227 ) ) ;
#241174 = AXIS2_PLACEMENT_3D ( 'NONE', #214840, #16665, #15383 ) ;
#241176 = CARTESIAN_POINT ( 'NONE',  ( -20.94999999999999929, -11.29603075032412995, -70.04789915966391334 ) ) ;
#241175 = VECTOR ( 'NONE', #33256, 1000.000000000000114 ) ;
#241177 = ORIENTED_EDGE ( 'NONE', *, *, #168710, .F. ) ;
#241178 = ORIENTED_EDGE ( 'NONE', *, *, #44395, .T. ) ;
#241179 = DIRECTION ( 'NONE',  ( 0.000000000000000000, -6.938893903907222067E-15, 1.000000000000000000 ) ) ;
#241180 = CARTESIAN_POINT ( 'NONE',  ( -23.25000000000000000, 36.65892442174935439, -249.5511627012433848 ) ) ;
#241182 = CARTESIAN_POINT ( 'NONE',  ( 21.87500000000000355, 14.02742277431099893, -219.5907614236512870 ) ) ;
#241181 = CARTESIAN_POINT ( 'NONE',  ( -20.64999999999999858, 1.115600667400684642E-11, -100.5000000000000426 ) ) ;
#241183 = EDGE_CURVE ( 'NONE', #147515, #80105, #215878, .T. ) ;
#241184 = AXIS2_PLACEMENT_3D ( 'NONE', #117628, #115063, #237583 ) ;
#241185 = CARTESIAN_POINT ( 'NONE',  ( 23.24999999999999645, 8.822561741677553471, -146.6500000000000341 ) ) ;
#241186 = DIRECTION ( 'NONE',  ( 1.000000000000000000, 0.000000000000000000, 0.000000000000000000 ) ) ;
#241187 = DIRECTION ( 'NONE',  ( 0.000000000000000000, -0.9651348961777157509, 0.2617529984165031243 ) ) ;
#241188 = EDGE_CURVE ( 'NONE', #47601, #56965, #103457, .T. ) ;
#241189 = VERTEX_POINT ( 'NONE', #52635 ) ;
#241190 = EDGE_CURVE ( 'NONE', #134468, #188219, #214293, .T. ) ;
#241191 = DIRECTION ( 'NONE',  ( -0.000000000000000000, -6.982962677686266711E-15, 1.000000000000000000 ) ) ;
#241192 = VERTEX_POINT ( 'NONE', #233856 ) ;
#241193 = VECTOR ( 'NONE', #59747, 1000.000000000000000 ) ;
#241195 = CIRCLE ( 'NONE', #45546, 0.2000000000000057288 ) ;
#241194 = CARTESIAN_POINT ( 'NONE',  ( -16.92973740335347443, 51.65264569848611842, -231.8847607149625958 ) ) ;
#241196 = EDGE_CURVE ( 'NONE', #153115, #199045, #134729, .T. ) ;
#241197 = ORIENTED_EDGE ( 'NONE', *, *, #14804, .T. ) ;
#241198 = CARTESIAN_POINT ( 'NONE',  ( -20.85000000000000142, 80.80934863333322937, -192.8037999715871535 ) ) ;
#241199 = VECTOR ( 'NONE', #102140, 1000.000000000000000 ) ;
#241200 = CARTESIAN_POINT ( 'NONE',  ( -20.90000000000000213, 11.49641995933507843, 1.885425182446133885 ) ) ;
#241201 = EDGE_LOOP ( 'NONE', ( #224252, #113654, #3039, #189070, #109419, #186056 ) ) ;
#241202 = CARTESIAN_POINT ( 'NONE',  ( -17.11825945287482753, 65.95000000001262208, -190.8731074845244109 ) ) ;
#241203 = EDGE_CURVE ( 'NONE', #175862, #253099, #190820, .T. ) ;
#241204 = VERTEX_POINT ( 'NONE', #213000 ) ;
#241205 = CARTESIAN_POINT ( 'NONE',  ( -21.05000000000000071, 6.400000000011158541, -43.43042463006157305 ) ) ;
#241206 = LINE ( 'NONE', #221595, #203460 ) ;
#241207 = CARTESIAN_POINT ( 'NONE',  ( -23.25000000000000000, 87.75000000001190870, -103.0231074845242176 ) ) ;
#241208 = LINE ( 'NONE', #101642, #170922 ) ;
#241209 = CARTESIAN_POINT ( 'NONE',  ( -21.56666275994539816, 1.115600667400684642E-11, -93.54263159310670517 ) ) ;
#241211 = FACE_OUTER_BOUND ( 'NONE', #86022, .T. ) ;
#241210 = CARTESIAN_POINT ( 'NONE',  ( -16.94226253665224391, 66.05000000001254534, -182.9698420801401539 ) ) ;
#241212 = CARTESIAN_POINT ( 'NONE',  ( -20.94999999999999929, -1.261786168553869603, -41.58649896354548048 ) ) ;
#241214 = VERTEX_POINT ( 'NONE', #34395 ) ;
#241213 = CARTESIAN_POINT ( 'NONE',  ( 21.14261333020286671, 65.28430735075768609, -191.2731074845242176 ) ) ;
#241216 = CARTESIAN_POINT ( 'NONE',  ( -18.59999999999999787, -9.399999999999943512, -7.297259759663287326 ) ) ;
#241215 = DIRECTION ( 'NONE',  ( -0.5932847527679299127, 0.8049926720990051576, 6.366092712777055223E-16 ) ) ;
#241217 = ORIENTED_EDGE ( 'NONE', *, *, #220299, .T. ) ;
#241219 = EDGE_LOOP ( 'NONE', ( #111606, #170200, #43064, #15979 ) ) ;
#241218 = FACE_OUTER_BOUND ( 'NONE', #232928, .T. ) ;
#241220 = AXIS2_PLACEMENT_3D ( 'NONE', #48421, #28920, #203655 ) ;
#241221 = ORIENTED_EDGE ( 'NONE', *, *, #26455, .T. ) ;
#241222 = CARTESIAN_POINT ( 'NONE',  ( -23.49999999999994316, 76.00000000001119815, -31.97310748452479601 ) ) ;
#241223 = FACE_OUTER_BOUND ( 'NONE', #224278, .T. ) ;
#241224 = LINE ( 'NONE', #100383, #55861 ) ;
#241225 = VERTEX_POINT ( 'NONE', #17379 ) ;
#241226 = CARTESIAN_POINT ( 'NONE',  ( 21.13435531349810859, 1.115406763810579610E-11, -127.5062789364073694 ) ) ;
#241227 = DIRECTION ( 'NONE',  ( 1.000000000000000000, 0.000000000000000000, 0.000000000000000000 ) ) ;
#241228 = CIRCLE ( 'NONE', #24764, 0.2000000000000057288 ) ;
#241229 = FACE_BOUND ( 'NONE', #167524, .T. ) ;
#241230 = ORIENTED_EDGE ( 'NONE', *, *, #208411, .T. ) ;
#241231 = DIRECTION ( 'NONE',  ( 0.000000000000000000, 0.000000000000000000, -1.000000000000000000 ) ) ;
#241232 = FACE_OUTER_BOUND ( 'NONE', #16961, .T. ) ;
#241233 = ORIENTED_EDGE ( 'NONE', *, *, #243441, .T. ) ;
#241234 = ORIENTED_EDGE ( 'NONE', *, *, #144619, .T. ) ;
#241235 = AXIS2_PLACEMENT_3D ( 'NONE', #68560, #108949, #73713 ) ;
#241236 = DIRECTION ( 'NONE',  ( -1.000000000000000000, 0.000000000000000000, 0.000000000000000000 ) ) ;
#241237 = AXIS2_PLACEMENT_3D ( 'NONE', #247192, #129816, #29480 ) ;
#241238 = ADVANCED_FACE ( 'NONE', ( #12260 ), #113903, .T. ) ;
#241239 = ORIENTED_EDGE ( 'NONE', *, *, #214991, .T. ) ;
#241241 = VERTEX_POINT ( 'NONE', #96867 ) ;
#241240 = VECTOR ( 'NONE', #194704, 1000.000000000000000 ) ;
#241242 = DIRECTION ( 'NONE',  ( 0.000000000000000000, 1.776356839400244943E-15, -1.000000000000000000 ) ) ;
#241243 = CARTESIAN_POINT ( 'NONE',  ( -18.59999999999999787, 1.340746217944851715, -90.22713749457885513 ) ) ;
#241244 = ADVANCED_FACE ( 'NONE', ( #155637 ), #236557, .F. ) ;
#241245 = CYLINDRICAL_SURFACE ( 'NONE', #156429, 7.900000000000003908 ) ;
#241246 = DIRECTION ( 'NONE',  ( -0.000000000000000000, -0.1298341882520022694, -0.9915357197604853789 ) ) ;
#241247 = VERTEX_POINT ( 'NONE', #231301 ) ;
#241248 = AXIS2_PLACEMENT_3D ( 'NONE', #139713, #200997, #43209 ) ;
#241249 = VECTOR ( 'NONE', #172906, 1000.000000000000000 ) ;
#241250 = CARTESIAN_POINT ( 'NONE',  ( -23.15000000000000213, 4.350000000011156054, -79.35000000000005116 ) ) ;
#241251 = ADVANCED_FACE ( 'NONE', ( #211738 ), #132185, .T. ) ;
#241252 = EDGE_CURVE ( 'NONE', #257242, #234655, #93051, .T. ) ;
#241253 = DIRECTION ( 'NONE',  ( 0.7071067811865388020, -0.7071067811865561215, 0.000000000000000000 ) ) ;
#241254 = CARTESIAN_POINT ( 'NONE',  ( -22.50000000000094147, 0.1000000000110504439, -88.85042919245520920 ) ) ;
#241255 = CARTESIAN_POINT ( 'NONE',  ( 20.94999999999999929, 74.16465844978745281, -91.46795619196133487 ) ) ;
#241256 = EDGE_LOOP ( 'NONE', ( #77067, #10215, #36264, #113068 ) ) ;
#241258 = CARTESIAN_POINT ( 'NONE',  ( 18.39999999999999503, 64.25000000001151079, -45.27310748452440237 ) ) ;
#241257 = CARTESIAN_POINT ( 'NONE',  ( 23.14999999999999503, 69.45000000001181206, -81.87310748452435405 ) ) ;
#241259 = ORIENTED_EDGE ( 'NONE', *, *, #54244, .T. ) ;
#241262 = VERTEX_POINT ( 'NONE', #145972 ) ;
#241261 = DIRECTION ( 'NONE',  ( 0.000000000000000000, 0.9770955615653316162, 0.2128009952263597848 ) ) ;
#241260 = CARTESIAN_POINT ( 'NONE',  ( 23.15000000000000213, 84.59626168225506149, -127.0729799673739677 ) ) ;
#241263 = TOROIDAL_SURFACE ( 'NONE', #166256, 1.900000000000002576, 0.1000000000000000056 ) ;
#241264 = EDGE_LOOP ( 'NONE', ( #56892, #97423, #89921, #1511 ) ) ;
#241265 = CARTESIAN_POINT ( 'NONE',  ( 20.94999999999999929, 5.000000000011153745, -55.09473398108690390 ) ) ;
#241266 = AXIS2_PLACEMENT_3D ( 'NONE', #131476, #32411, #53224 ) ;
#241267 = VECTOR ( 'NONE', #72072, 1000.000000000000000 ) ;
#241268 = TOROIDAL_SURFACE ( 'NONE', #37246, 0.4000000000000010214, 0.1000000000000000056 ) ;
#241269 = CARTESIAN_POINT ( 'NONE',  ( -21.29999999999995808, 0.8618440306782485516, -204.9572370243411115 ) ) ;
#241270 = ORIENTED_EDGE ( 'NONE', *, *, #205993, .T. ) ;
#241271 = CARTESIAN_POINT ( 'NONE',  ( 21.05000000000000071, 76.00000000001267608, -203.5231074845243597 ) ) ;
#241272 = EDGE_CURVE ( 'NONE', #38568, #134779, #62604, .T. ) ;
#241273 = AXIS2_PLACEMENT_3D ( 'NONE', #39331, #67526, #99258 ) ;
#241274 = DIRECTION ( 'NONE',  ( -1.000000000000000000, 0.000000000000000000, 0.000000000000000000 ) ) ;
#241275 = EDGE_CURVE ( 'NONE', #163726, #25563, #104267, .T. ) ;
#241277 = FACE_OUTER_BOUND ( 'NONE', #174724, .T. ) ;
#241276 = FACE_OUTER_BOUND ( 'NONE', #79579, .T. ) ;
#241279 = EDGE_LOOP ( 'NONE', ( #131442, #121644, #21934, #148827 ) ) ;
#241278 = DIRECTION ( 'NONE',  ( 0.2834754621636358940, -0.2834754621636437211, 0.9161240771326893961 ) ) ;
#241280 = PRODUCT_RELATED_PRODUCT_CATEGORY ( 'part', '', ( #30667 ) ) ;
#241281 = VERTEX_POINT ( 'NONE', #126414 ) ;
#241282 = VECTOR ( 'NONE', #196242, 1000.000000000000000 ) ;
#241283 = LINE ( 'NONE', #104297, #23035 ) ;
#241284 = LINE ( 'NONE', #87310, #226382 ) ;
#241285 = ORIENTED_EDGE ( 'NONE', *, *, #16669, .T. ) ;
#241286 = CARTESIAN_POINT ( 'NONE',  ( 18.39999999999999858, 85.50000000001185185, -96.10844914155455854 ) ) ;
#241287 = EDGE_LOOP ( 'NONE', ( #121518, #91824, #204186 ) ) ;
#241288 = EDGE_CURVE ( 'NONE', #149370, #142179, #144978, .T. ) ;
#241289 = DIRECTION ( 'NONE',  ( 0.000000000000000000, 0.8034013718071717491, -0.5954378521544919645 ) ) ;
#241291 = ADVANCED_FACE ( 'NONE', ( #46864 ), #74487, .T. ) ;
#241290 = CARTESIAN_POINT ( 'NONE',  ( 18.49999999999999645, 1.115600667400684642E-11, -100.5000000000000284 ) ) ;
#241292 = CARTESIAN_POINT ( 'NONE',  ( -21.44999999999999929, 7.350000000011155166, -45.75000000000000000 ) ) ;
#241293 = EDGE_CURVE ( 'NONE', #185168, #82597, #225492, .T. ) ;
#241294 = ORIENTED_EDGE ( 'NONE', *, *, #197839, .T. ) ;
#241295 = LINE ( 'NONE', #61352, #121048 ) ;
#241296 = AXIS2_PLACEMENT_3D ( 'NONE', #79565, #20929, #22202 ) ;
#241297 = AXIS2_PLACEMENT_3D ( 'NONE', #109863, #49899, #31662 ) ;
#241298 = EDGE_CURVE ( 'NONE', #95630, #4734, #199358, .T. ) ;
#241299 = AXIS2_PLACEMENT_3D ( 'NONE', #81022, #158064, #139714 ) ;
#241300 = ORIENTED_EDGE ( 'NONE', *, *, #187229, .T. ) ;
#241301 = ORIENTED_EDGE ( 'NONE', *, *, #60544, .T. ) ;
#241302 = ORIENTED_EDGE ( 'NONE', *, *, #22695, .F. ) ;
#241303 = CARTESIAN_POINT ( 'NONE',  ( 23.24999999999999645, 11.75000000001113953, -188.3499999999999659 ) ) ;
#241304 = VERTEX_POINT ( 'NONE', #205953 ) ;
#241306 = VERTEX_POINT ( 'NONE', #185111 ) ;
#241305 = CARTESIAN_POINT ( 'NONE',  ( 13.54577453029516398, 66.54939790392401733, -185.0792115214277658 ) ) ;
#241307 = ORIENTED_EDGE ( 'NONE', *, *, #174319, .F. ) ;
#241308 = CIRCLE ( 'NONE', #120517, 0.1000000000000028644 ) ;
#241311 = EDGE_CURVE ( 'NONE', #224095, #45297, #78525, .T. ) ;
#241310 = ORIENTED_EDGE ( 'NONE', *, *, #29746, .F. ) ;
#241309 = ORIENTED_EDGE ( 'NONE', *, *, #183556, .F. ) ;
#241312 = ORIENTED_EDGE ( 'NONE', *, *, #54045, .T. ) ;
#241313 = PLANE ( 'NONE',  #85584 ) ;
#241314 = AXIS2_PLACEMENT_3D ( 'NONE', #130585, #224549, #9352 ) ;
#241315 = CARTESIAN_POINT ( 'NONE',  ( 21.05000000000000071, 67.22371735104150048, -195.0355151060044534 ) ) ;
#241316 = CARTESIAN_POINT ( 'NONE',  ( -16.88705144915432044, 14.09920906346404124, -218.9805296183471341 ) ) ;
#241317 = EDGE_LOOP ( 'NONE', ( #233039, #15727, #133409, #46146 ) ) ;
#241318 = ADVANCED_FACE ( 'NONE', ( #84683 ), #106842, .F. ) ;
#241319 = CARTESIAN_POINT ( 'NONE',  ( -20.94999999999999929, -1.135018845899022466, -141.7169768834323520 ) ) ;
#241321 = ORIENTED_EDGE ( 'NONE', *, *, #246893, .F. ) ;
#241320 = CARTESIAN_POINT ( 'NONE',  ( 22.37643362114956247, 7.625789993969535274, -167.4009186263185995 ) ) ;
#241322 = CARTESIAN_POINT ( 'NONE',  ( 19.99999999999998934, 11.75000000001115552, -188.8499999999999659 ) ) ;
#241324 = ORIENTED_EDGE ( 'NONE', *, *, #235735, .T. ) ;
#241323 = DIRECTION ( 'NONE',  ( -0.000000000000000000, 0.9651348961777157509, -0.2617529984165031243 ) ) ;
#241325 =( BOUNDED_SURFACE ( )  B_SPLINE_SURFACE ( 3, 2, ( 
 ( #53094, #192619, #28447 ),
 ( #252570, #227889, #71405 ),
 ( #50507, #109210, #29723 ),
 ( #188755, #229183, #209610 ) ),
 .UNSPECIFIED., .F., .F., .F. ) 
 B_SPLINE_SURFACE_WITH_KNOTS ( ( 4, 4 ),
 ( 3, 3 ),
 ( -1.908195823574487804E-17, 0.001979672783031562362 ),
 ( 0.000000000000000000, 1.000000000000000000 ),
 .UNSPECIFIED. ) 
 GEOMETRIC_REPRESENTATION_ITEM ( )  RATIONAL_B_SPLINE_SURFACE ( (
 ( 1.000000000000000000, 0.7103081912008383236, 1.000000000000000000),
 ( 1.000000000000000000, 0.7104998333557640544, 1.000000000000000000),
 ( 1.000000000000000000, 0.7107238315756078118, 1.000000000000000000),
 ( 1.000000000000000000, 0.7110073749539294052, 1.000000000000000000) ) ) 
 REPRESENTATION_ITEM ( '' )  SURFACE ( )  );
#241326 = EDGE_LOOP ( 'NONE', ( #37760, #76421, #107065, #217615 ) ) ;
#241327 = EDGE_CURVE ( 'NONE', #254141, #244837, #3699, .T. ) ;
#241328 = CARTESIAN_POINT ( 'NONE',  ( -20.15000000000000568, 66.70857864377468616, -115.3731074845243683 ) ) ;
#241329 = EDGE_LOOP ( 'NONE', ( #180567, #64130, #61343, #40266 ) ) ;
#241330 = VERTEX_POINT ( 'NONE', #45606 ) ;
#241331 = VECTOR ( 'NONE', #205589, 1000.000000000000000 ) ;
#241332 = DIRECTION ( 'NONE',  ( 0.000000000000000000, 0.8777080977375072424, -0.4791956752371691608 ) ) ;
#241333 = DIRECTION ( 'NONE',  ( -0.000000000000000000, 0.000000000000000000, 1.000000000000000000 ) ) ;
#241334 = EDGE_CURVE ( 'NONE', #116437, #40625, #236938, .T. ) ;
#241336 = ORIENTED_EDGE ( 'NONE', *, *, #43760, .F. ) ;
#241335 = ORIENTED_EDGE ( 'NONE', *, *, #220529, .F. ) ;
#241337 = ORIENTED_EDGE ( 'NONE', *, *, #110132, .T. ) ;
#241339 = ADVANCED_FACE ( 'NONE', ( #6464 ), #85976, .T. ) ;
#241338 = DIRECTION ( 'NONE',  ( 1.000000000000000000, 0.000000000000000000, 0.000000000000000000 ) ) ;
#241340 = ORIENTED_EDGE ( 'NONE', *, *, #35575, .T. ) ;
#241341 = VERTEX_POINT ( 'NONE', #224225 ) ;
#241342 = SPHERICAL_SURFACE ( 'NONE', #117584, 0.1000000000000000056 ) ;
#241344 = ORIENTED_EDGE ( 'NONE', *, *, #34671, .F. ) ;
#241343 = PLANE ( 'NONE',  #193370 ) ;
#241345 = DIRECTION ( 'NONE',  ( 0.000000000000000000, 1.000000000000000000, 0.000000000000000000 ) ) ;
#241347 = CARTESIAN_POINT ( 'NONE',  ( 18.41789779300684060, -9.499999999988844479, -107.5320696663599307 ) ) ;
#241346 = DIRECTION ( 'NONE',  ( 1.000000000000000000, 0.000000000000000000, 0.000000000000000000 ) ) ;
#241348 = ORIENTED_EDGE ( 'NONE', *, *, #172509, .F. ) ;
#241350 = VERTEX_POINT ( 'NONE', #221648 ) ;
#241349 = ORIENTED_EDGE ( 'NONE', *, *, #194981, .F. ) ;
#241352 = AXIS2_PLACEMENT_3D ( 'NONE', #181849, #241812, #146544 ) ;
#241351 = CARTESIAN_POINT ( 'NONE',  ( 20.85000000000000142, 69.01799029515598249, -166.3269553662681233 ) ) ;
#241353 = CARTESIAN_POINT ( 'NONE',  ( -20.64999999999999858, 7.150000000011155876, -112.8500000000000369 ) ) ;
#241354 = AXIS2_PLACEMENT_3D ( 'NONE', #130384, #153865, #233378 ) ;
#241355 = VERTEX_POINT ( 'NONE', #23508 ) ;
#241356 = EDGE_CURVE ( 'NONE', #117855, #84837, #57765, .T. ) ;
#241357 =( BOUNDED_CURVE ( )  B_SPLINE_CURVE ( 3, ( #217811, #234834, #176166, #135716 ),
 .UNSPECIFIED., .F., .F. ) 
 B_SPLINE_CURVE_WITH_KNOTS ( ( 4, 4 ),
 ( 3.141592653589793116, 4.712388980384689674 ),
 .UNSPECIFIED. ) 
 CURVE ( )  GEOMETRIC_REPRESENTATION_ITEM ( )  RATIONAL_B_SPLINE_CURVE ( ( 1.000000000000000000, 0.8047378541243649375, 0.8047378541243649375, 1.000000000000000000 ) ) 
 REPRESENTATION_ITEM ( '' )  );
#241358 = TOROIDAL_SURFACE ( 'NONE', #62276, 11.65000000000000036, 0.1000000000000000056 ) ;
#241359 = LINE ( 'NONE', #197067, #143045 ) ;
#241360 = VERTEX_POINT ( 'NONE', #182563 ) ;
#241361 = ORIENTED_EDGE ( 'NONE', *, *, #211364, .F. ) ;
#241362 = EDGE_CURVE ( 'NONE', #44452, #28264, #178525, .T. ) ;
#241363 = CARTESIAN_POINT ( 'NONE',  ( -22.94999999999999929, 6.783826713665066954, 9.593862367105558064 ) ) ;
#241364 = EDGE_LOOP ( 'NONE', ( #176118, #173355, #147115, #78655, #71139, #106526 ) ) ;
#241365 = DIRECTION ( 'NONE',  ( 0.000000000000000000, 0.000000000000000000, 1.000000000000000000 ) ) ;
#241366 = CARTESIAN_POINT ( 'NONE',  ( -20.00857864376270001, 44.18876898710608003, -236.1516686502934590 ) ) ;
#241367 = ORIENTED_EDGE ( 'NONE', *, *, #235803, .T. ) ;
#241368 = CARTESIAN_POINT ( 'NONE',  ( 20.85000000000000142, 76.00000000001207923, -128.6231074845243540 ) ) ;
#241370 = SPHERICAL_SURFACE ( 'NONE', #203832, 0.1000000000000000056 ) ;
#241369 = DIRECTION ( 'NONE',  ( 1.000000000000000000, -1.772924042024179943E-16, 4.808324575169860901E-17 ) ) ;
#241371 = DIRECTION ( 'NONE',  ( -1.000000000000000000, -0.000000000000000000, -0.000000000000000000 ) ) ;
#241373 = DIRECTION ( 'NONE',  ( -1.000000000000000000, 0.000000000000000000, -0.000000000000000000 ) ) ;
#241372 = AXIS2_PLACEMENT_3D ( 'NONE', #60852, #38746, #37470 ) ;
#241375 = EDGE_CURVE ( 'NONE', #17722, #25020, #141088, .T. ) ;
#241374 = CARTESIAN_POINT ( 'NONE',  ( 21.05000000000000071, -8.663551401857999323, -90.97589888193273566 ) ) ;
#241376 = VECTOR ( 'NONE', #222946, 1000.000000000000000 ) ;
#241377 = DIRECTION ( 'NONE',  ( -1.000000000000000000, 0.000000000000000000, 0.000000000000000000 ) ) ;
#241378 = DIRECTION ( 'NONE',  ( 1.000000000000000000, 0.000000000000000000, 0.000000000000000000 ) ) ;
#241379 = ADVANCED_FACE ( 'NONE', ( #3909 ), #166053, .T. ) ;
#241380 = EDGE_LOOP ( 'NONE', ( #31644, #119693, #195008, #167187 ) ) ;
#241381 = CIRCLE ( 'NONE', #83099, 4.049999999999998046 ) ;
#241383 = EDGE_LOOP ( 'NONE', ( #30271, #183332, #29231, #10796, #130220 ) ) ;
#241382 = VERTEX_POINT ( 'NONE', #163002 ) ;
#241384 = ORIENTED_EDGE ( 'NONE', *, *, #33245, .F. ) ;
#241385 = DIRECTION ( 'NONE',  ( 0.000000000000000000, 0.9968797965484755830, 0.07893460099012303277 ) ) ;
#241386 = CARTESIAN_POINT ( 'NONE',  ( -18.59999999999999787, 1.162701749949165642, -75.10000000000003695 ) ) ;
#241387 = ADVANCED_FACE ( 'NONE', ( #29914 ), #95290, .T. ) ;
#241389 = CARTESIAN_POINT ( 'NONE',  ( 20.94999999999999929, 11.65000000001115943, -194.2161343370218560 ) ) ;
#241388 = DIRECTION ( 'NONE',  ( 0.000000000000000000, 0.2128009952263605620, -0.9770955615653313941 ) ) ;
#241390 = ADVANCED_FACE ( 'NONE', ( #207261 ), #186411, .F. ) ;
#241391 = CARTESIAN_POINT ( 'NONE',  ( 21.05000000000000071, -8.999999999988842703, -124.5060308773475839 ) ) ;
#241392 = VERTEX_POINT ( 'NONE', #208544 ) ;
#241393 = CARTESIAN_POINT ( 'NONE',  ( 21.05000000000000071, 6.257814610487280937, -66.90220970869124528 ) ) ;
#241394 =( NAMED_UNIT ( * ) SI_UNIT ( $, .STERADIAN. ) SOLID_ANGLE_UNIT ( ) );
#241395 = DIRECTION ( 'NONE',  ( -0.000000000000000000, -0.1298341882519953583, -0.9915357197604862671 ) ) ;
#241396 = CARTESIAN_POINT ( 'NONE',  ( -20.00857864376270001, 63.93636616954134411, -213.0474835168086827 ) ) ;
#241397 = CARTESIAN_POINT ( 'NONE',  ( -17.11825945287482753, 65.95000000001232365, -157.3731074845244393 ) ) ;
#241398 = VERTEX_POINT ( 'NONE', #148561 ) ;
#241399 = AXIS2_PLACEMENT_3D ( 'NONE', #209767, #11582, #212350 ) ;
#241400 = CARTESIAN_POINT ( 'NONE',  ( -21.00857864376268935, 64.40000000001161595, -62.59490425424883853 ) ) ;
#241401 = PLANE ( 'NONE',  #38540 ) ;
#241402 = EDGE_LOOP ( 'NONE', ( #60074, #53088, #83745 ) ) ;
#241403 = CARTESIAN_POINT ( 'NONE',  ( -21.14999999999999858, 64.25000000001195133, -103.0231074845244024 ) ) ;
#241404 = AXIS2_PLACEMENT_3D ( 'NONE', #253228, #99282, #57591 ) ;
#241405 = CARTESIAN_POINT ( 'NONE',  ( -21.05000000000000071, 64.35000000001238618, -169.9231074845244507 ) ) ;
#241406 = DIRECTION ( 'NONE',  ( 1.000000000000000000, 0.000000000000000000, 0.000000000000000000 ) ) ;
#241407 = CARTESIAN_POINT ( 'NONE',  ( -20.64999999999999858, 1.115600667400684642E-11, -100.5000000000000426 ) ) ;
#241408 = DIRECTION ( 'NONE',  ( 0.000000000000000000, -2.139158043593750707E-15, 1.000000000000000000 ) ) ;
#241409 = ORIENTED_EDGE ( 'NONE', *, *, #74992, .T. ) ;
#241410 = CARTESIAN_POINT ( 'NONE',  ( 21.15000000000005187, 64.25000000001119815, -51.02310748452479316 ) ) ;
#241411 = DIRECTION ( 'NONE',  ( 0.000000000000000000, 0.000000000000000000, 1.000000000000000000 ) ) ;
#241412 = CARTESIAN_POINT ( 'NONE',  ( -21.05000000000000071, -0.08579911626297563598, -60.58602111851162419 ) ) ;
#241414 = CARTESIAN_POINT ( 'NONE',  ( -23.15000000000000213, 71.85000000001198828, -115.3731074845243256 ) ) ;
#241413 = CARTESIAN_POINT ( 'NONE',  ( -23.25000000000000000, 64.35000000001214460, -136.5231074845243597 ) ) ;
#241415 = CARTESIAN_POINT ( 'NONE',  ( 20.12500000000000000, 66.25000000001155342, -48.37310748452438958 ) ) ;
#241416 =( LENGTH_UNIT ( ) NAMED_UNIT ( * ) SI_UNIT ( .MILLI., .METRE. ) );
#241417 = LINE ( 'NONE', #178904, #60349 ) ;
#241418 = FACE_OUTER_BOUND ( 'NONE', #55217, .T. ) ;
#241419 = CIRCLE ( 'NONE', #75019, 0.2000000000000057288 ) ;
#241421 = EDGE_LOOP ( 'NONE', ( #115651, #63941, #18951 ) ) ;
#241420 = DIRECTION ( 'NONE',  ( 1.000000000000000000, 0.000000000000000000, 0.000000000000000000 ) ) ;
#241422 = EDGE_CURVE ( 'NONE', #253318, #207476, #91141, .T. ) ;
#241423 = VECTOR ( 'NONE', #87542, 1000.000000000000000 ) ;
#241424 = VERTEX_POINT ( 'NONE', #230669 ) ;
#241425 = CIRCLE ( 'NONE', #108138, 0.09999999999999939493 ) ;
#241426 = CIRCLE ( 'NONE', #12297, 0.4000000000000114575 ) ;
#241427 = AXIS2_PLACEMENT_3D ( 'NONE', #98407, #37217, #5425 ) ;
#241428 = LINE ( 'NONE', #164458, #113033 ) ;
#241429 = EDGE_CURVE ( 'NONE', #215387, #217189, #7817, .T. ) ;
#241430 = CARTESIAN_POINT ( 'NONE',  ( 13.22261339317536866, 9.436552840015581367, -149.1779554727603454 ) ) ;
#241431 = ORIENTED_EDGE ( 'NONE', *, *, #75022, .F. ) ;
#241432 = CIRCLE ( 'NONE', #45785, 0.09999999999999691080 ) ;
#241433 = LINE ( 'NONE', #22396, #217889 ) ;
#241434 = CIRCLE ( 'NONE', #83160, 0.09999999999999867328 ) ;
#241435 = CIRCLE ( 'NONE', #191574, 0.5000000000000004441 ) ;
#241436 = DIRECTION ( 'NONE',  ( 1.000000000000000000, -0.000000000000000000, 0.000000000000000000 ) ) ;
#241437 = CARTESIAN_POINT ( 'NONE',  ( -22.47007471830799119, 76.00000000001200817, -110.7438181364507983 ) ) ;
#241438 = AXIS2_PLACEMENT_3D ( 'NONE', #71086, #11098, #170222 ) ;
#241439 = CIRCLE ( 'NONE', #249807, 7.791421356237310469 ) ;
#241440 = ORIENTED_EDGE ( 'NONE', *, *, #110285, .F. ) ;
#241441 = DIRECTION ( 'NONE',  ( 0.000000000000000000, -2.775557561562888827E-14, 1.000000000000000000 ) ) ;
#241442 = ORIENTED_EDGE ( 'NONE', *, *, #168992, .T. ) ;
#241444 = CARTESIAN_POINT ( 'NONE',  ( -17.29838795458566025, 10.37154985795929818, -156.1047412826179368 ) ) ;
#241443 = DIRECTION ( 'NONE',  ( -1.000000000000000000, 0.000000000000000000, 0.000000000000000000 ) ) ;
#241445 = CIRCLE ( 'NONE', #33369, 0.09999999999999939493 ) ;
#241446 = CARTESIAN_POINT ( 'NONE',  ( 20.44999100639871514, 65.56028929680051931, -162.2640317585554044 ) ) ;
#241447 = CARTESIAN_POINT ( 'NONE',  ( 23.24999999999999645, 78.10000000001171827, -69.52310748452430289 ) ) ;
#241448 = ORIENTED_EDGE ( 'NONE', *, *, #245502, .F. ) ;
#241449 = DIRECTION ( 'NONE',  ( 0.000000000000000000, 0.000000000000000000, 1.000000000000000000 ) ) ;
#241450 = CARTESIAN_POINT ( 'NONE',  ( 21.05000000000000071, 4.999999999999997335, -12.40526601891309788 ) ) ;
#241451 = PLANE ( 'NONE',  #239822 ) ;
#241452 = ORIENTED_EDGE ( 'NONE', *, *, #111010, .F. ) ;
#241453 = LINE ( 'NONE', #61528, #150163 ) ;
#241454 = DIRECTION ( 'NONE',  ( 0.000000000000000000, 0.000000000000000000, 1.000000000000000000 ) ) ;
#241455 = DIRECTION ( 'NONE',  ( 0.000000000000000000, -0.9371753822965315228, 0.3488585713686134238 ) ) ;
#241456 = FACE_OUTER_BOUND ( 'NONE', #251978, .T. ) ;
#241457 = ORIENTED_EDGE ( 'NONE', *, *, #92942, .F. ) ;
#241458 = ORIENTED_EDGE ( 'NONE', *, *, #8801, .T. ) ;
#241459 = CIRCLE ( 'NONE', #16622, 0.1999999999999987899 ) ;
#241460 = CARTESIAN_POINT ( 'NONE',  ( -21.59780538579341069, 69.15290947006869260, -103.1220861541223428 ) ) ;
#241461 = DIRECTION ( 'NONE',  ( 0.000000000000000000, -6.938893903907222067E-15, 1.000000000000000000 ) ) ;
#241462 = FACE_OUTER_BOUND ( 'NONE', #243809, .T. ) ;
#241463 = DIRECTION ( 'NONE',  ( -1.000000000000000000, 0.000000000000000000, -0.000000000000000000 ) ) ;
#241464 = AXIS2_PLACEMENT_3D ( 'NONE', #183880, #49506, #27415 ) ;
#241465 = EDGE_CURVE ( 'NONE', #194645, #193988, #12923, .T. ) ;
#241466 = CARTESIAN_POINT ( 'NONE',  ( -16.77683809663752257, 12.41293291551535916, -211.2574046339461233 ) ) ;
#241467 = CARTESIAN_POINT ( 'NONE',  ( 18.59999999999999076, 74.75000000001260503, -195.5231074845243597 ) ) ;
#241468 = CARTESIAN_POINT ( 'NONE',  ( 20.94999999999999574, 74.75000000001261924, -195.6231074845243540 ) ) ;
#241469 = CARTESIAN_POINT ( 'NONE',  ( -20.94999999999999929, 1.115600667400684642E-11, -100.5000000000000284 ) ) ;
#241470 = ORIENTED_EDGE ( 'NONE', *, *, #171852, .F. ) ;
#241471 = CARTESIAN_POINT ( 'NONE',  ( 21.15000000000005187, 64.25000000001119815, -5.923107484524795296 ) ) ;
#241472 = AXIS2_PLACEMENT_3D ( 'NONE', #249127, #209992, #151312 ) ;
#241474 = EDGE_LOOP ( 'NONE', ( #172860, #92499, #155302 ) ) ;
#241473 = FACE_OUTER_BOUND ( 'NONE', #119481, .T. ) ;
#241475 = CARTESIAN_POINT ( 'NONE',  ( -20.85000000000000142, 7.021664781911246322, -171.3335654018973173 ) ) ;
#241477 = DIRECTION ( 'NONE',  ( -1.000000000000000000, -8.034189347746079853E-16, 2.566115377699053192E-16 ) ) ;
#241476 = CARTESIAN_POINT ( 'NONE',  ( -18.59999999999999787, 0.7653315920341953182, -212.6731560895497353 ) ) ;
#241478 = EDGE_CURVE ( 'NONE', #178965, #117385, #124337, .T. ) ;
#241479 = EDGE_LOOP ( 'NONE', ( #250595, #145987, #64400, #214050 ) ) ;
#241481 = DIRECTION ( 'NONE',  ( 0.000000000000000000, 0.000000000000000000, -1.000000000000000000 ) ) ;
#241480 = DIRECTION ( 'NONE',  ( 0.000000000000000000, 0.8814952561688722543, -0.4721928772776801675 ) ) ;
#241482 = DIRECTION ( 'NONE',  ( 1.000000000000000000, 0.000000000000000000, 0.000000000000000000 ) ) ;
#241483 = CARTESIAN_POINT ( 'NONE',  ( 20.97224591636398472, 65.37484658384840941, -124.2731815798607897 ) ) ;
#241484 = CARTESIAN_POINT ( 'NONE',  ( 21.15000000000005542, 74.73834681386826162, -44.00978271863746016 ) ) ;
#241485 = DIRECTION ( 'NONE',  ( 1.000000000000000000, -7.304098846218134667E-16, -5.100424963727255829E-30 ) ) ;
#241486 = EDGE_CURVE ( 'NONE', #149669, #239387, #186896, .T. ) ;
#241487 = VERTEX_POINT ( 'NONE', #228102 ) ;
#241489 = ORIENTED_EDGE ( 'NONE', *, *, #83812, .F. ) ;
#241488 = AXIS2_PLACEMENT_3D ( 'NONE', #138798, #240512, #202664 ) ;
#241490 = AXIS2_PLACEMENT_3D ( 'NONE', #165637, #88622, #10408 ) ;
#241491 = DIRECTION ( 'NONE',  ( -1.000000000000000000, 0.000000000000000000, 0.000000000000000000 ) ) ;
#241492 = ADVANCED_FACE ( 'NONE', ( #7767 ), #11928, .F. ) ;
#241493 = EDGE_LOOP ( 'NONE', ( #146356, #226203, #121147, #29783 ) ) ;
#241494 = VECTOR ( 'NONE', #214402, 1000.000000000000000 ) ;
#241495 = ORIENTED_EDGE ( 'NONE', *, *, #139344, .F. ) ;
#241496 = DIRECTION ( 'NONE',  ( 0.000000000000000000, 0.000000000000000000, -1.000000000000000000 ) ) ;
#241497 = DIRECTION ( 'NONE',  ( 1.000000000000000000, 0.000000000000000000, 0.000000000000000000 ) ) ;
#241498 = ORIENTED_EDGE ( 'NONE', *, *, #152205, .T. ) ;
#241499 = EDGE_CURVE ( 'NONE', #213752, #16468, #188964, .T. ) ;
#241500 = CARTESIAN_POINT ( 'NONE',  ( -16.78493211734303969, 9.945835743215329927, -87.83605098089604724 ) ) ;
#241501 = CARTESIAN_POINT ( 'NONE',  ( -21.05000000000000071, 65.63520407022599557, -242.0679395242962357 ) ) ;
#241502 = CARTESIAN_POINT ( 'NONE',  ( 20.85000000000000142, 11.75000000001115907, -160.7161343370219129 ) ) ;
#241503 = DIRECTION ( 'NONE',  ( 1.000000000000000000, 0.000000000000000000, -0.000000000000000000 ) ) ;
#241504 = DIRECTION ( 'NONE',  ( 0.000000000000000000, -0.7071067811865479058, 0.7071067811865472397 ) ) ;
#241505 = DIRECTION ( 'NONE',  ( 0.000000000000000000, 0.008583690987128059571, -0.9999631594459056361 ) ) ;
#241506 = CARTESIAN_POINT ( 'NONE',  ( 14.45204356427543146, 62.05093865251256346, -218.8507522889722168 ) ) ;
#241507 = ORIENTED_EDGE ( 'NONE', *, *, #62102, .T. ) ;
#241509 = CARTESIAN_POINT ( 'NONE',  ( -23.25000000000000000, 1.115626384983466744E-11, -131.9000000000000341 ) ) ;
#241508 = CARTESIAN_POINT ( 'NONE',  ( 18.59999999999999076, 46.59314322379660922, -243.1831726892433210 ) ) ;
#241510 = EDGE_LOOP ( 'NONE', ( #149954, #192015, #244174, #124784 ) ) ;
#241512 = VERTEX_POINT ( 'NONE', #89847 ) ;
#241511 = FACE_OUTER_BOUND ( 'NONE', #210070, .T. ) ;
#241513 = VERTEX_POINT ( 'NONE', #51995 ) ;
#241514 = DIRECTION ( 'NONE',  ( 0.000000000000000000, 1.000000000000000000, 0.000000000000000000 ) ) ;
#241515 = DIRECTION ( 'NONE',  ( 0.000000000000000000, 0.000000000000000000, 1.000000000000000000 ) ) ;
#241516 = FACE_OUTER_BOUND ( 'NONE', #88730, .T. ) ;
#241517 = CARTESIAN_POINT ( 'NONE',  ( -22.59999999999999787, 64.35042919246788529, -203.6231074845244393 ) ) ;
#241518 = ORIENTED_EDGE ( 'NONE', *, *, #191870, .F. ) ;
#241519 = CYLINDRICAL_SURFACE ( 'NONE', #84656, 0.09999999999999781286 ) ;
#241520 = LINE ( 'NONE', #242792, #193813 ) ;
#241521 = EDGE_LOOP ( 'NONE', ( #81054, #155511, #4147 ) ) ;
#241522 = DIRECTION ( 'NONE',  ( 0.000000000000000000, 7.026728003956695223E-15, -1.000000000000000000 ) ) ;
#241523 = TOROIDAL_SURFACE ( 'NONE', #183260, 0.4000000000000017431, 0.1000000000000000056 ) ;
#241524 = CIRCLE ( 'NONE', #37525, 0.09999999999998898659 ) ;
#241525 = VECTOR ( 'NONE', #243263, 1000.000000000000227 ) ;
#241527 = AXIS2_PLACEMENT_3D ( 'NONE', #136501, #54417, #195246 ) ;
#241526 = CYLINDRICAL_SURFACE ( 'NONE', #159992, 0.09999999999998898659 ) ;
#241528 = ORIENTED_EDGE ( 'NONE', *, *, #62578, .T. ) ;
#241529 = CARTESIAN_POINT ( 'NONE',  ( -21.14999999999994174, 77.83551161375991967, -47.52760213295649550 ) ) ;
#241530 = EDGE_CURVE ( 'NONE', #119503, #241591, #220197, .T. ) ;
#241531 = AXIS2_PLACEMENT_3D ( 'NONE', #110595, #151020, #229276 ) ;
#241532 = CARTESIAN_POINT ( 'NONE',  ( -23.25000000000000000, 7.788796164756791818, -245.4641525896719543 ) ) ;
#241533 = EDGE_LOOP ( 'NONE', ( #242566, #199794, #54664, #179821 ) ) ;
#241534 = DIRECTION ( 'NONE',  ( 0.000000000000000000, -7.124650136758317602E-15, 1.000000000000000000 ) ) ;
#241535 = DIRECTION ( 'NONE',  ( 1.000000000000000000, 0.000000000000000000, 0.000000000000000000 ) ) ;
#241536 = DIRECTION ( 'NONE',  ( 0.000000000000000000, 0.4088369013363306603, -0.9126074666063758167 ) ) ;
#241537 = EDGE_CURVE ( 'NONE', #180046, #90818, #70334, .T. ) ;
#241538 = FACE_OUTER_BOUND ( 'NONE', #157143, .T. ) ;
#241539 = CIRCLE ( 'NONE', #141569, 4.099999999999992539 ) ;
#241540 = AXIS2_PLACEMENT_3D ( 'NONE', #178199, #93494, #16548 ) ;
#241541 = EDGE_CURVE ( 'NONE', #159851, #208846, #103632, .T. ) ;
#241542 = DIRECTION ( 'NONE',  ( 0.000000000000000000, 0.9126074666063660468, 0.4088369013363524762 ) ) ;
#241543 = CARTESIAN_POINT ( 'NONE',  ( 18.79999999999999716, 1.212568896937007645, -7.800000000000000711 ) ) ;
#241544 = LINE ( 'NONE', #214587, #197930 ) ;
#241545 = ORIENTED_EDGE ( 'NONE', *, *, #37480, .F. ) ;
#241547 = DIRECTION ( 'NONE',  ( 1.000000000000000000, 0.000000000000000000, -0.000000000000000000 ) ) ;
#241546 = CARTESIAN_POINT ( 'NONE',  ( 16.87683809663749557, 9.949999999999976197, -20.85000000000000142 ) ) ;
#241548 = EDGE_LOOP ( 'NONE', ( #137669, #257509, #176632, #4238 ) ) ;
#241549 = CARTESIAN_POINT ( 'NONE',  ( 23.24999999999999289, 10.94327717634720543, -220.4671437206886822 ) ) ;
#241550 = CARTESIAN_POINT ( 'NONE',  ( -21.14999999999999858, -1.331831764083658554, -194.8847705854734045 ) ) ;
#241553 = EDGE_CURVE ( 'NONE', #87352, #127248, #136981, .T. ) ;
#241552 = EDGE_LOOP ( 'NONE', ( #238785, #198028, #87644, #171528 ) ) ;
#241551 = DIRECTION ( 'NONE',  ( -1.000000000000000000, -0.000000000000000000, 0.000000000000000000 ) ) ;
#241555 = ORIENTED_EDGE ( 'NONE', *, *, #31823, .F. ) ;
#241554 = CARTESIAN_POINT ( 'NONE',  ( -16.98495255085918032, 10.00556436600592569, -54.36538279377951000 ) ) ;
#241556 = CARTESIAN_POINT ( 'NONE',  ( 20.94999999999999574, 46.45388641681647357, -243.1520440498138385 ) ) ;
#241557 = CARTESIAN_POINT ( 'NONE',  ( 18.59999999999999076, 13.20456090973765662, -206.4140623547709765 ) ) ;
#241558 = DIRECTION ( 'NONE',  ( 1.000000000000000000, 0.000000000000000000, 0.000000000000000000 ) ) ;
#241559 = EDGE_CURVE ( 'NONE', #200926, #63948, #41144, .T. ) ;
#241560 = DIRECTION ( 'NONE',  ( -1.000000000000000000, 0.000000000000000000, 0.000000000000000000 ) ) ;
#241562 = ORIENTED_EDGE ( 'NONE', *, *, #78955, .T. ) ;
#241561 = CARTESIAN_POINT ( 'NONE',  ( 21.04105312098497649, 67.12466737696867369, -157.6946007373123564 ) ) ;
#241563 = VECTOR ( 'NONE', #93345, 1000.000000000000000 ) ;
#241565 = ADVANCED_FACE ( 'NONE', ( #26908 ), #182109, .T. ) ;
#241564 = CARTESIAN_POINT ( 'NONE',  ( 21.05000000000000071, -11.64999999998883595, -64.10000000000000853 ) ) ;
#241566 = VERTEX_POINT ( 'NONE', #165104 ) ;
#241567 = EDGE_LOOP ( 'NONE', ( #153654, #14768, #72427, #118728 ) ) ;
#241568 = CIRCLE ( 'NONE', #245674, 11.65000000000000391 ) ;
#241570 = EDGE_CURVE ( 'NONE', #86629, #91289, #63421, .T. ) ;
#241569 = CARTESIAN_POINT ( 'NONE',  ( -17.01825945287482966, 10.05000000001113847, -46.15000000000000568 ) ) ;
#241571 = DIRECTION ( 'NONE',  ( 0.000000000000000000, 0.000000000000000000, 1.000000000000000000 ) ) ;
#241572 = ADVANCED_FACE ( 'NONE', ( #240793 ), #101561, .T. ) ;
#241573 = ORIENTED_EDGE ( 'NONE', *, *, #206634, .F. ) ;
#241574 = CARTESIAN_POINT ( 'NONE',  ( -18.59999999999999787, 69.06610602788607878, -166.2374616501508342 ) ) ;
#241575 = CARTESIAN_POINT ( 'NONE',  ( -18.59999999999999787, 11.65000000001115232, -74.01480577065404987 ) ) ;
#241576 = EDGE_LOOP ( 'NONE', ( #83874, #228502 ) ) ;
#241577 = VECTOR ( 'NONE', #241186, 1000.000000000000000 ) ;
#241578 = CARTESIAN_POINT ( 'NONE',  ( 21.09316766718127667, 6.215893237032393159, -199.6060609392288256 ) ) ;
#241579 = AXIS2_PLACEMENT_3D ( 'NONE', #139511, #75714, #217753 ) ;
#241580 = DIRECTION ( 'NONE',  ( -0.000000000000000000, 0.000000000000000000, -1.000000000000000000 ) ) ;
#241581 = ORIENTED_EDGE ( 'NONE', *, *, #137171, .T. ) ;
#241582 = ORIENTED_EDGE ( 'NONE', *, *, #107064, .T. ) ;
#241583 = CARTESIAN_POINT ( 'NONE',  ( -18.44085059012131822, 64.48598750652770661, -45.28280216540286318 ) ) ;
#241584 = EDGE_CURVE ( 'NONE', #186519, #10339, #119911, .T. ) ;
#241585 = AXIS2_PLACEMENT_3D ( 'NONE', #137196, #94211, #36852 ) ;
#241586 = ORIENTED_EDGE ( 'NONE', *, *, #149560, .F. ) ;
#241587 = EDGE_CURVE ( 'NONE', #113100, #16494, #146799, .T. ) ;
#241588 = CARTESIAN_POINT ( 'NONE',  ( -16.78493832629887805, 22.98839712131284685, -230.9453208111997071 ) ) ;
#241589 = ORIENTED_EDGE ( 'NONE', *, *, #248653, .F. ) ;
#241591 = VERTEX_POINT ( 'NONE', #201658 ) ;
#241590 = DIRECTION ( 'NONE',  ( 0.000000000000000000, 0.2617529984164856383, 0.9651348961777204138 ) ) ;
#241592 = CIRCLE ( 'NONE', #187438, 11.90000000000000746 ) ;
#241593 = AXIS2_PLACEMENT_3D ( 'NONE', #142079, #118697, #99085 ) ;
#241594 = DIRECTION ( 'NONE',  ( 1.000000000000000000, 0.000000000000000000, 0.000000000000000000 ) ) ;
#241595 = ORIENTED_EDGE ( 'NONE', *, *, #38795, .T. ) ;
#241596 = CARTESIAN_POINT ( 'NONE',  ( 22.49999999999999645, 0.1000000000111554016, -88.85042919245522341 ) ) ;
#241597 = ORIENTED_EDGE ( 'NONE', *, *, #256856, .F. ) ;
#241600 = ADVANCED_FACE ( 'NONE', ( #3445 ), #23052, .F. ) ;
#241599 = VERTEX_POINT ( 'NONE', #46425 ) ;
#241598 = EDGE_LOOP ( 'NONE', ( #243023, #86279, #43687 ) ) ;
#241601 = CARTESIAN_POINT ( 'NONE',  ( 21.11833042828134310, 69.55435530615692130, -136.5302079935837867 ) ) ;
#241602 = CARTESIAN_POINT ( 'NONE',  ( -16.89268316805465986, 14.16190809729244648, -219.2603268738197073 ) ) ;
#241603 = VERTEX_POINT ( 'NONE', #226329 ) ;
#241604 = TOROIDAL_SURFACE ( 'NONE', #212406, 12.97499999999999609, 0.1000000000000000056 ) ;
#241605 = VECTOR ( 'NONE', #196268, 1000.000000000000000 ) ;
#241606 = CIRCLE ( 'NONE', #204170, 0.5000000000000004441 ) ;
#241607 = AXIS2_PLACEMENT_3D ( 'NONE', #132018, #12100, #138106 ) ;
#241608 = VECTOR ( 'NONE', #134269, 1000.000000000000000 ) ;
#241609 = ORIENTED_EDGE ( 'NONE', *, *, #254431, .T. ) ;
#241610 = CYLINDRICAL_SURFACE ( 'NONE', #236814, 0.1000000000000118433 ) ;
#241611 = LINE ( 'NONE', #237757, #80482 ) ;
#241613 = ORIENTED_EDGE ( 'NONE', *, *, #231876, .T. ) ;
#241612 = DIRECTION ( 'NONE',  ( -0.000000000000000000, 0.2128009952263604232, -0.9770955615653316162 ) ) ;
#241614 = DIRECTION ( 'NONE',  ( -1.000000000000000000, -0.000000000000000000, 0.000000000000000000 ) ) ;
#241615 = ORIENTED_EDGE ( 'NONE', *, *, #64894, .T. ) ;
#241616 = FACE_OUTER_BOUND ( 'NONE', #219497, .T. ) ;
#241617 = DIRECTION ( 'NONE',  ( 1.000000000000000000, -0.000000000000000000, -0.000000000000000000 ) ) ;
#241619 = VERTEX_POINT ( 'NONE', #183391 ) ;
#241618 = EDGE_CURVE ( 'NONE', #123059, #13549, #224275, .T. ) ;
#241620 = FACE_OUTER_BOUND ( 'NONE', #1562, .T. ) ;
#241621 = DIRECTION ( 'NONE',  ( -1.000000000000000000, -2.952720810173289112E-16, 0.000000000000000000 ) ) ;
#241622 = EDGE_CURVE ( 'NONE', #243446, #11085, #174454, .T. ) ;
#241623 = ORIENTED_EDGE ( 'NONE', *, *, #120739, .F. ) ;
#241624 = CARTESIAN_POINT ( 'NONE',  ( 20.94999999999999929, 77.16412189325286874, -61.60825939895269698 ) ) ;
#241625 = ORIENTED_EDGE ( 'NONE', *, *, #194967, .T. ) ;
#241626 = EDGE_CURVE ( 'NONE', #22494, #154603, #86882, .T. ) ;
#241628 = ORIENTED_EDGE ( 'NONE', *, *, #255740, .F. ) ;
#241627 = ORIENTED_EDGE ( 'NONE', *, *, #246787, .F. ) ;
#241629 = ORIENTED_EDGE ( 'NONE', *, *, #80195, .T. ) ;
#241631 = EDGE_CURVE ( 'NONE', #131489, #233299, #161949, .T. ) ;
#241630 = DIRECTION ( 'NONE',  ( 0.000000000000000000, -0.8660254037844383745, 0.5000000000000003331 ) ) ;
#241632 = ORIENTED_EDGE ( 'NONE', *, *, #51951, .F. ) ;
#241633 = DIRECTION ( 'NONE',  ( 0.000000000000000000, -0.2617529984165152257, -0.9651348961777124202 ) ) ;
#241634 = ORIENTED_EDGE ( 'NONE', *, *, #83809, .F. ) ;
#241635 = DIRECTION ( 'NONE',  ( -1.000000000000000000, 0.000000000000000000, -0.000000000000000000 ) ) ;
#241636 = EDGE_CURVE ( 'NONE', #126382, #107706, #257533, .T. ) ;
#241637 = DIRECTION ( 'NONE',  ( 0.000000000000000000, 0.000000000000000000, -1.000000000000000000 ) ) ;
#241638 = AXIS2_PLACEMENT_3D ( 'NONE', #48506, #185460, #204990 ) ;
#241639 = EDGE_LOOP ( 'NONE', ( #150634, #83933, #16027, #93418, #181149, #147782, #56696, #40608, #111828, #128779, #206095, #128067 ) ) ;
#241640 = AXIS2_PLACEMENT_3D ( 'NONE', #156339, #136725, #216261 ) ;
#241641 = VERTEX_POINT ( 'NONE', #187251 ) ;
#241642 = ORIENTED_EDGE ( 'NONE', *, *, #71251, .F. ) ;
#241643 = AXIS2_PLACEMENT_3D ( 'NONE', #10204, #131410, #91005 ) ;
#241644 = ADVANCED_FACE ( 'NONE', ( #8600 ), #128543, .T. ) ;
#241645 = ADVANCED_FACE ( 'NONE', ( #213197 ), #193656, .F. ) ;
#241646 = CARTESIAN_POINT ( 'NONE',  ( -16.85718274719363308, 66.02385768539012645, -82.08645381670704921 ) ) ;
#241647 = ORIENTED_EDGE ( 'NONE', *, *, #9159, .T. ) ;
#241648 = ADVANCED_FACE ( 'NONE', ( #9873 ), #166235, .T. ) ;
#241649 = CARTESIAN_POINT ( 'NONE',  ( 20.95512820512820795, 12.97672201526442137, -210.6599585865309052 ) ) ;
#241650 = CARTESIAN_POINT ( 'NONE',  ( -20.94560253601877164, 11.75000000001115197, -127.0100835125151093 ) ) ;
#241651 = CARTESIAN_POINT ( 'NONE',  ( -23.15000000000000213, 1.115600667400684642E-11, -169.6000000000000227 ) ) ;
#241652 = CIRCLE ( 'NONE', #233303, 0.1000000000000027117 ) ;
#241653 = DIRECTION ( 'NONE',  ( -1.000000000000000000, 0.000000000000000000, 0.000000000000000000 ) ) ;
#241654 = DIRECTION ( 'NONE',  ( -0.000000000000000000, 6.982962677686266711E-15, -1.000000000000000000 ) ) ;
#241655 = CIRCLE ( 'NONE', #129244, 0.09999999999999939493 ) ;
#241657 = CARTESIAN_POINT ( 'NONE',  ( 21.05000000000000071, 34.10192277420338058, -243.5988165382224508 ) ) ;
#241656 = CYLINDRICAL_SURFACE ( 'NONE', #111121, 0.09999999999998898659 ) ;
#241658 = DIRECTION ( 'NONE',  ( 1.836970198721029934E-16, -1.000000000000000000, -0.000000000000000000 ) ) ;
#241659 = DIRECTION ( 'NONE',  ( -0.000000000000000000, -6.982962677686266711E-15, 1.000000000000000000 ) ) ;
#241660 = DIRECTION ( 'NONE',  ( 1.000000000000000000, 0.000000000000000000, 0.000000000000000000 ) ) ;
#241661 = CYLINDRICAL_SURFACE ( 'NONE', #184324, 4.000000000000000000 ) ;
#241662 = EDGE_CURVE ( 'NONE', #22978, #100496, #21632, .T. ) ;
#241663 = CIRCLE ( 'NONE', #208371, 0.09999999999999638345 ) ;
#241664 =( BOUNDED_SURFACE ( )  B_SPLINE_SURFACE ( 3, 2, ( 
 ( #224813, #166175, #7056 ),
 ( #158783, #79197, #125720 ),
 ( #218706, #65752, #245678 ),
 ( #40123, #238277, #205245 ),
 ( #59617, #26650, #44913 ),
 ( #196587, #38818, #178343 ),
 ( #226080, #220005, #185708 ),
 ( #19239, #177060, #119642 ),
 ( #199165, #118358, #20548 ),
 ( #25368, #86569, #67041 ),
 ( #257797, #164863, #179619 ),
 ( #146549, #17948, #124455 ) ),
 .UNSPECIFIED., .F., .F., .T. ) 
 B_SPLINE_SURFACE_WITH_KNOTS ( ( 4, 2, 2, 2, 2, 4 ),
 ( 3, 3 ),
 ( 3.174653483277205090, 3.943930578431714018, 4.713207673586222946, 5.482484768740731873, 5.867123316317986337, 6.251761863895240801 ),
 ( 0.000000000000000000, 1.000000000000000000 ),
 .UNSPECIFIED. ) 
 GEOMETRIC_REPRESENTATION_ITEM ( )  RATIONAL_B_SPLINE_SURFACE ( (
 ( 1.000000000000000000, 0.8659465255642401216, 1.000000000000000000),
 ( 1.000000000000000000, 0.8648614068488893469, 1.000000000000000000),
 ( 1.000000000000000000, 0.8489031841323232408, 1.000000000000000000),
 ( 1.000000000000000000, 0.7927507630162343721, 1.000000000000000000),
 ( 1.000000000000000000, 0.7523013859014273663, 1.000000000000000000),
 ( 1.000000000000000000, 0.6616226951191639394, 1.000000000000000000),
 ( 1.000000000000000000, 0.6112214368725455982, 1.000000000000000000),
 ( 1.000000000000000000, 0.5507684314497544031, 1.000000000000000000),
 ( 1.000000000000000000, 0.5333267243152143289, 1.000000000000000000),
 ( 1.000000000000000000, 0.5084565446480221462, 1.000000000000000000),
 ( 1.000000000000000000, 0.5010722703450330995, 1.000000000000000000),
 ( 1.000000000000000000, 0.5001234037138393429, 1.000000000000000000) ) ) 
 REPRESENTATION_ITEM ( '' )  SURFACE ( )  );
#241665 = ORIENTED_EDGE ( 'NONE', *, *, #157087, .F. ) ;
#241666 = AXIS2_PLACEMENT_3D ( 'NONE', #82307, #161904, #62781 ) ;
#241667 = EDGE_CURVE ( 'NONE', #254695, #100941, #210372, .T. ) ;
#241669 = ORIENTED_EDGE ( 'NONE', *, *, #75383, .F. ) ;
#241668 = DIRECTION ( 'NONE',  ( 1.000000000000000000, -0.000000000000000000, -0.000000000000000000 ) ) ;
#241670 = ORIENTED_EDGE ( 'NONE', *, *, #133617, .F. ) ;
#241671 = DIRECTION ( 'NONE',  ( 0.000000000000000000, 0.2617529984165031243, 0.9651348961777157509 ) ) ;
#241672 = EDGE_CURVE ( 'NONE', #186227, #210448, #53779, .T. ) ;
#241673 = CARTESIAN_POINT ( 'NONE',  ( 20.59588692710267921, 10.36872342118052259, -141.6390810945103169 ) ) ;
#241674 = CARTESIAN_POINT ( 'NONE',  ( 22.88900146558018989, 8.703904791112817563, -9.250000000000001776 ) ) ;
#241675 = EDGE_CURVE ( 'NONE', #145730, #3674, #253670, .T. ) ;
#241676 = ORIENTED_EDGE ( 'NONE', *, *, #61860, .F. ) ;
#241677 = SURFACE_STYLE_USAGE ( .BOTH. , #4332 ) ;
#241679 = AXIS2_PLACEMENT_3D ( 'NONE', #20394, #81591, #103728 ) ;
#241678 = DIRECTION ( 'NONE',  ( 0.000000000000000000, 0.000000000000000000, 1.000000000000000000 ) ) ;
#241680 = AXIS2_PLACEMENT_3D ( 'NONE', #164294, #185128, #41793 ) ;
#241681 = FACE_OUTER_BOUND ( 'NONE', #95480, .T. ) ;
#241682 = ORIENTED_EDGE ( 'NONE', *, *, #230704, .F. ) ;
#241683 = DIRECTION ( 'NONE',  ( 0.000000000000000000, -0.3738317757009345654, 0.9274965247785492695 ) ) ;
#241684 = LINE ( 'NONE', #139990, #71469 ) ;
#241685 = LINE ( 'NONE', #202558, #117907 ) ;
#241686 = ADVANCED_FACE ( 'NONE', ( #51532 ), #11164, .F. ) ;
#241687 = CARTESIAN_POINT ( 'NONE',  ( 21.05000000000000071, 40.84268664891381917, -237.9560832633917187 ) ) ;
#241689 = ORIENTED_EDGE ( 'NONE', *, *, #173941, .T. ) ;
#241688 = CARTESIAN_POINT ( 'NONE',  ( -20.94983749550516450, 67.49429988484537546, -195.5441618131978601 ) ) ;
#241690 = DIRECTION ( 'NONE',  ( -0.000000000000000000, 1.000000000000000000, 1.734723475976807292E-15 ) ) ;
#241692 = ORIENTED_EDGE ( 'NONE', *, *, #182700, .F. ) ;
#241691 = DIRECTION ( 'NONE',  ( -2.840903330521632269E-16, -0.8700118002898356018, 0.4930308989875170078 ) ) ;
#241693 = DIRECTION ( 'NONE',  ( -0.000000000000000000, 0.4721928772777345684, 0.8814952561688429444 ) ) ;
#241694 = CYLINDRICAL_SURFACE ( 'NONE', #129102, 0.09999999999999939493 ) ;
#241695 = DIRECTION ( 'NONE',  ( 0.000000000000000000, 0.000000000000000000, -1.000000000000000000 ) ) ;
#241696 = CARTESIAN_POINT ( 'NONE',  ( -12.25000000000000178, 9.350000000011139178, -184.2499999999999716 ) ) ;
#241697 = ADVANCED_FACE ( 'NONE', ( #249773 ), #58029, .F. ) ;
#241698 = AXIS2_PLACEMENT_3D ( 'NONE', #48443, #107132, #208812 ) ;
#241701 = CARTESIAN_POINT ( 'NONE',  ( -23.25000000000000355, 12.53302308287915245, -211.3193184079345883 ) ) ;
#241700 = AXIS2_PLACEMENT_3D ( 'NONE', #175053, #212851, #74661 ) ;
#241699 = DIRECTION ( 'NONE',  ( 0.000000000000000000, 6.997203936713167125E-15, -1.000000000000000000 ) ) ;
#241702 = CARTESIAN_POINT ( 'NONE',  ( -16.90257928357874206, 66.04589317890723521, -190.8868220544107430 ) ) ;
#241703 = DIRECTION ( 'NONE',  ( 1.000000000000000000, 0.000000000000000000, 0.000000000000000000 ) ) ;
#241704 = CIRCLE ( 'NONE', #254160, 0.1000000000000028644 ) ;
#241705 = CARTESIAN_POINT ( 'NONE',  ( -18.50016250449483479, 10.29766095124169922, -38.97436639332758546 ) ) ;
#241706 = CARTESIAN_POINT ( 'NONE',  ( -21.44999999999999929, 63.37018259659601682, -222.0118260003222872 ) ) ;
#241707 = CARTESIAN_POINT ( 'NONE',  ( 21.11927991906887669, 10.16575863945443459, -228.0440959703046246 ) ) ;
#241708 = ORIENTED_EDGE ( 'NONE', *, *, #230905, .F. ) ;
#241709 = DIRECTION ( 'NONE',  ( 0.000000000000000000, 0.000000000000000000, -1.000000000000000000 ) ) ;
#241710 = AXIS2_PLACEMENT_3D ( 'NONE', #11177, #90696, #211956 ) ;
#241711 = EDGE_LOOP ( 'NONE', ( #180973, #11642, #177597, #73058, #220681 ) ) ;
#241712 = ORIENTED_EDGE ( 'NONE', *, *, #23162, .T. ) ;
#241713 = EDGE_CURVE ( 'NONE', #25616, #6721, #74673, .T. ) ;
#241714 = CARTESIAN_POINT ( 'NONE',  ( -20.94999999999999929, 11.63687328910415886, -26.67824078667520382 ) ) ;
#241715 = DIRECTION ( 'NONE',  ( 0.000000000000000000, 1.000000000000000000, 0.000000000000000000 ) ) ;
#241716 = ORIENTED_EDGE ( 'NONE', *, *, #145660, .F. ) ;
#241717 = SHAPE_REPRESENTATION ( 'Injection Molded Chain Links 10', ( #2425 ), #89914 ) ;
#241718 = AXIS2_PLACEMENT_3D ( 'NONE', #88765, #126630, #11849 ) ;
#241719 = EDGE_LOOP ( 'NONE', ( #249961, #112080, #70606, #60413 ) ) ;
#241720 =( NAMED_UNIT ( * ) SI_UNIT ( $, .STERADIAN. ) SOLID_ANGLE_UNIT ( ) );
#241721 = EDGE_CURVE ( 'NONE', #152244, #20407, #170282, .T. ) ;
#241722 = ORIENTED_EDGE ( 'NONE', *, *, #58431, .T. ) ;
#241723 = CARTESIAN_POINT ( 'NONE',  ( -18.40000000000000213, 14.17280543801757986, -210.8598471598932349 ) ) ;
#241724 = VERTEX_POINT ( 'NONE', #13727 ) ;
#241725 = LINE ( 'NONE', #177916, #75637 ) ;
#241726 = CARTESIAN_POINT ( 'NONE',  ( -18.59999999999999787, 76.00000000001126921, -203.5231074845248997 ) ) ;
#241727 = DIRECTION ( 'NONE',  ( 0.000000000000000000, -6.982962677686266711E-15, 1.000000000000000000 ) ) ;
#241728 = CARTESIAN_POINT ( 'NONE',  ( 11.60000000000006004, 66.35000000001119247, -21.02310748452479316 ) ) ;
#241729 = DIRECTION ( 'NONE',  ( 0.000000000000000000, 0.8814952561688430555, -0.4721928772777346239 ) ) ;
#241730 = CARTESIAN_POINT ( 'NONE',  ( -21.14999999999999858, 11.65000000001115232, -100.5000000000000284 ) ) ;
#241731 = CARTESIAN_POINT ( 'NONE',  ( -21.65000000000000213, 10.05000000001113847, -54.35000000000000142 ) ) ;
#241733 = ORIENTED_EDGE ( 'NONE', *, *, #37667, .T. ) ;
#241732 = DIRECTION ( 'NONE',  ( 1.000000000000000000, 0.000000000000000000, 0.000000000000000000 ) ) ;
#241735 = DIRECTION ( 'NONE',  ( 0.000000000000000000, 0.000000000000000000, -1.000000000000000000 ) ) ;
#241734 = CARTESIAN_POINT ( 'NONE',  ( -18.44085059012131822, 62.46367190038257178, -209.4461346550174312 ) ) ;
#241736 = CARTESIAN_POINT ( 'NONE',  ( -21.07094088545368749, 75.90110629745947790, -75.84327470644144853 ) ) ;
#241737 = ORIENTED_EDGE ( 'NONE', *, *, #112146, .F. ) ;
#241738 = DIRECTION ( 'NONE',  ( 0.000000000000000000, 0.9553114395363127009, 0.2956011730204364252 ) ) ;
#241739 =( NAMED_UNIT ( * ) PLANE_ANGLE_UNIT ( ) SI_UNIT ( $, .RADIAN. ) );
#241740 = EDGE_LOOP ( 'NONE', ( #42047, #122316, #199404, #65597 ) ) ;
#241742 = FACE_OUTER_BOUND ( 'NONE', #153959, .T. ) ;
#241741 = FACE_OUTER_BOUND ( 'NONE', #73176, .T. ) ;
#241743 = CIRCLE ( 'NONE', #16911, 0.09999999999999938105 ) ;
#241744 = DIRECTION ( 'NONE',  ( -0.7071067811865303643, 0.3338907855507385891, 0.6233112732209604712 ) ) ;
#241745 = EDGE_LOOP ( 'NONE', ( #147726, #23862, #215354, #84485 ) ) ;
#241746 = DIRECTION ( 'NONE',  ( 1.000000000000000000, 0.000000000000000000, 0.000000000000000000 ) ) ;
#241748 = DIRECTION ( 'NONE',  ( 1.000000000000000000, 0.000000000000000000, 0.000000000000000000 ) ) ;
#241747 = AXIS2_PLACEMENT_3D ( 'NONE', #251334, #175679, #173148 ) ;
#241749 = DIRECTION ( 'NONE',  ( 0.000000000000000000, 0.000000000000000000, -1.000000000000000000 ) ) ;
#241750 = ORIENTED_EDGE ( 'NONE', *, *, #246397, .F. ) ;
#241751 = EDGE_CURVE ( 'NONE', #76466, #82405, #154937, .T. ) ;
#241752 = CARTESIAN_POINT ( 'NONE',  ( 21.05000000000000071, 67.22371711014413620, -90.84689234345620434 ) ) ;
#241753 = CARTESIAN_POINT ( 'NONE',  ( -23.25000000000000000, 10.33248238082518711, -39.09484654391314962 ) ) ;
#241754 = CARTESIAN_POINT ( 'NONE',  ( -16.87786941232800686, 30.23414331161600899, -234.8126936039916473 ) ) ;
#241755 = AXIS2_PLACEMENT_3D ( 'NONE', #205559, #123476, #103884 ) ;
#241756 = FACE_OUTER_BOUND ( 'NONE', #172766, .T. ) ;
#241758 = DIRECTION ( 'NONE',  ( 0.000000000000000000, 0.000000000000000000, -1.000000000000000000 ) ) ;
#241757 = CIRCLE ( 'NONE', #83514, 0.1000000000000013933 ) ;
#241760 = EDGE_LOOP ( 'NONE', ( #123104, #31066, #222675, #249474 ) ) ;
#241759 = DIRECTION ( 'NONE',  ( 1.000000000000000000, 0.000000000000000000, 0.000000000000000000 ) ) ;
#241761 = CARTESIAN_POINT ( 'NONE',  ( 20.94999999999999929, -4.714262876194486473, -233.3440214805475819 ) ) ;
#241762 = CARTESIAN_POINT ( 'NONE',  ( -16.80891096016328135, 66.05000000001187743, -90.39077029179252065 ) ) ;
#241763 = CARTESIAN_POINT ( 'NONE',  ( -21.08621493067320429, 75.94380516053566055, -75.87240177569626098 ) ) ;
#241764 = CIRCLE ( 'NONE', #237687, 0.09999999999999939493 ) ;
#241765 = CARTESIAN_POINT ( 'NONE',  ( -20.94999999999999929, 76.00000000001193712, -107.1231074845243114 ) ) ;
#241766 = EDGE_CURVE ( 'NONE', #13152, #105430, #178719, .T. ) ;
#241767 = CARTESIAN_POINT ( 'NONE',  ( -22.94999999999999929, 6.783826713665066954, 9.593862367105558064 ) ) ;
#241769 = EDGE_LOOP ( 'NONE', ( #20696, #101704 ) ) ;
#241768 = CARTESIAN_POINT ( 'NONE',  ( -22.50000000000000000, 36.65892442174472876, -249.5511627012454596 ) ) ;
#241770 = CARTESIAN_POINT ( 'NONE',  ( -20.64999999999999858, 6.268811756569107274, -220.3853799378769622 ) ) ;
#241771 = AXIS2_PLACEMENT_3D ( 'NONE', #75953, #56361, #158101 ) ;
#241772 = CARTESIAN_POINT ( 'NONE',  ( -16.95709691156337229, 63.08309975593071783, -213.1373284914761825 ) ) ;
#241773 = CARTESIAN_POINT ( 'NONE',  ( 20.92356734117541706, 67.49293571122092317, -195.4648732548341741 ) ) ;
#241774 = AXIS2_PLACEMENT_3D ( 'NONE', #135024, #193746, #72529 ) ;
#241775 = ADVANCED_FACE ( 'NONE', ( #32035 ), #114099, .T. ) ;
#241776 = ORIENTED_EDGE ( 'NONE', *, *, #113169, .F. ) ;
#241777 = CARTESIAN_POINT ( 'NONE',  ( -12.25000000000000178, 66.65000000001228386, -153.2731074845244166 ) ) ;
#241778 = DIRECTION ( 'NONE',  ( 1.000000000000000000, -2.952720810173289112E-16, -2.061873921506763405E-30 ) ) ;
#241779 = DIRECTION ( 'NONE',  ( 1.000000000000000000, 0.000000000000000000, 0.000000000000000000 ) ) ;
#241780 = DIRECTION ( 'NONE',  ( 0.000000000000000000, 0.000000000000000000, -1.000000000000000000 ) ) ;
#241781 = EDGE_CURVE ( 'NONE', #251301, #100316, #70564, .T. ) ;
#241782 = ORIENTED_EDGE ( 'NONE', *, *, #209530, .T. ) ;
#241784 = DIRECTION ( 'NONE',  ( 0.000000000000000000, 0.2617529984165031243, 0.9651348961777157509 ) ) ;
#241783 = CIRCLE ( 'NONE', #225005, 0.09999999999999963085 ) ;
#241785 = CIRCLE ( 'NONE', #62734, 0.09999999999998898659 ) ;
#241786 = CIRCLE ( 'NONE', #91935, 0.1000000000000075273 ) ;
#241787 = VERTEX_POINT ( 'NONE', #26607 ) ;
#241788 = TOROIDAL_SURFACE ( 'NONE', #12862, 11.70000000000000462, 0.1000000000000000056 ) ;
#241789 = AXIS2_PLACEMENT_3D ( 'NONE', #149725, #68896, #207114 ) ;
#241790 = ADVANCED_FACE ( 'NONE', ( #206504 ), #126970, .F. ) ;
#241791 = DIRECTION ( 'NONE',  ( -1.000000000000000000, 0.000000000000000000, 0.000000000000000000 ) ) ;
#241792 = CARTESIAN_POINT ( 'NONE',  ( 20.94999999999999929, 62.08148826970417389, -247.6553521922769221 ) ) ;
#241793 = ADVANCED_FACE ( 'NONE', ( #9581 ), #244336, .F. ) ;
#241794 = SURFACE_STYLE_FILL_AREA ( #162280 ) ;
#241795 = LINE ( 'NONE', #215794, #251762 ) ;
#241796 = ORIENTED_EDGE ( 'NONE', *, *, #154483, .T. ) ;
#241797 = EDGE_CURVE ( 'NONE', #218429, #30910, #138720, .T. ) ;
#241798 = CARTESIAN_POINT ( 'NONE',  ( 20.95462737510932882, 10.55678195165489441, -175.0699500565622486 ) ) ;
#241799 = DIRECTION ( 'NONE',  ( 1.000000000000000000, 0.000000000000000000, 0.000000000000000000 ) ) ;
#241800 = EDGE_CURVE ( 'NONE', #17324, #152778, #89124, .T. ) ;
#241801 = DIRECTION ( 'NONE',  ( 0.000000000000000000, 0.2128009952263403282, -0.9770955615653358350 ) ) ;
#241802 = CARTESIAN_POINT ( 'NONE',  ( -16.89155683852570888, 9.949999999999981526, -20.22262815045992923 ) ) ;
#241803 = DIRECTION ( 'NONE',  ( 1.000000000000000000, 0.000000000000000000, 0.000000000000000000 ) ) ;
#241804 = ORIENTED_EDGE ( 'NONE', *, *, #167585, .F. ) ;
#241806 = ORIENTED_EDGE ( 'NONE', *, *, #108045, .T. ) ;
#241805 = CARTESIAN_POINT ( 'NONE',  ( 20.04142135623730070, 61.47936603916258491, -212.1738987416902376 ) ) ;
#241807 = ORIENTED_EDGE ( 'NONE', *, *, #86351, .F. ) ;
#241808 = DIRECTION ( 'NONE',  ( 0.000000000000000000, 0.000000000000000000, 1.000000000000000000 ) ) ;
#241809 = ORIENTED_EDGE ( 'NONE', *, *, #158484, .F. ) ;
#241810 = CARTESIAN_POINT ( 'NONE',  ( 21.05000000000000071, 61.06337788713324244, -234.0934405812916168 ) ) ;
#241811 = DIRECTION ( 'NONE',  ( 0.000000000000000000, 0.000000000000000000, -1.000000000000000000 ) ) ;
#241812 = DIRECTION ( 'NONE',  ( -1.000000000000000000, -3.265361837132813093E-16, 0.000000000000000000 ) ) ;
#241813 = ORIENTED_EDGE ( 'NONE', *, *, #175453, .F. ) ;
#241814 = CARTESIAN_POINT ( 'NONE',  ( -16.91256925476571737, 66.01426884188337851, -56.99074997352966676 ) ) ;
#241815 = B_SPLINE_CURVE_WITH_KNOTS ( 'NONE', 3,
 ( #208556, #29925, #91154, #170750, #131567, #109418, #229397, #50714, #190271, #11641 ),
 .UNSPECIFIED., .F., .F.,
 ( 4, 3, 3, 4 ),
 ( 0.000000000000000000, 3.394313611811463347E-05, 6.779740500699467213E-05, 0.0001049857339142579784 ),
 .UNSPECIFIED. ) ;
#241817 = VERTEX_POINT ( 'NONE', #85236 ) ;
#241816 = CIRCLE ( 'NONE', #83573, 0.09999999999998898659 ) ;
#241818 = EDGE_CURVE ( 'NONE', #36019, #219709, #216341, .T. ) ;
#241819 = CARTESIAN_POINT ( 'NONE',  ( -14.77538296656415362, 9.436662931810241517, -152.3230367322949235 ) ) ;
#241821 = ORIENTED_EDGE ( 'NONE', *, *, #84902, .F. ) ;
#241820 = DIRECTION ( 'NONE',  ( -1.000000000000000000, 3.265361837132813093E-16, 2.280189983783949500E-30 ) ) ;
#241822 = DIRECTION ( 'NONE',  ( 1.000000000000000000, 0.000000000000000000, 0.000000000000000000 ) ) ;
#241823 = DIRECTION ( 'NONE',  ( 0.000000000000000000, -0.4721928772777347350, -0.8814952561688431665 ) ) ;
#241824 = AXIS2_PLACEMENT_3D ( 'NONE', #233915, #55242, #165557 ) ;
#241825 = ORIENTED_EDGE ( 'NONE', *, *, #94119, .F. ) ;
#241826 = DIRECTION ( 'NONE',  ( -1.000000000000000000, -0.000000000000000000, -0.000000000000000000 ) ) ;
#241828 = ADVANCED_FACE ( 'NONE', ( #205203 ), #4439, .F. ) ;
#241827 = CARTESIAN_POINT ( 'NONE',  ( 21.14261333020286671, 10.71569264926606202, -79.25000000000027001 ) ) ;
#241829 = CIRCLE ( 'NONE', #150266, 0.09999999999999761857 ) ;
#241830 = CARTESIAN_POINT ( 'NONE',  ( 18.49999999999999645, -1.162701749926855266, -41.60000000000000142 ) ) ;
#241831 = EDGE_LOOP ( 'NONE', ( #6674, #173273, #94121, #247753 ) ) ;
#241832 = DIRECTION ( 'NONE',  ( 1.000000000000000000, 0.000000000000000000, 0.000000000000000000 ) ) ;
#241833 = DIRECTION ( 'NONE',  ( -0.000000000000000000, 1.000000000000000000, -0.000000000000000000 ) ) ;
#241834 = AXIS2_PLACEMENT_3D ( 'NONE', #227216, #66865, #48578 ) ;
#241835 = ORIENTED_EDGE ( 'NONE', *, *, #35771, .T. ) ;
#241836 = EDGE_CURVE ( 'NONE', #218126, #10704, #107941, .T. ) ;
#241837 = B_SPLINE_CURVE_WITH_KNOTS ( 'NONE', 3,
 ( #222733, #204454, #148347, #10126, #143201, #207042, #167942, #227885, #105326, #169231 ),
 .UNSPECIFIED., .F., .F.,
 ( 4, 3, 3, 4 ),
 ( 0.000000000000000000, 0.0002000000000002908468, 0.001000000000045115191, 0.001967863649472108723 ),
 .UNSPECIFIED. ) ;
#241838 = AXIS2_PLACEMENT_3D ( 'NONE', #204802, #220541, #60160 ) ;
#241839 = EDGE_CURVE ( 'NONE', #115598, #32552, #145342, .T. ) ;
#241840 = CIRCLE ( 'NONE', #83592, 0.1000000000000013933 ) ;
#241842 = VERTEX_POINT ( 'NONE', #73448 ) ;
#241841 = CIRCLE ( 'NONE', #79332, 0.2000000000000002054 ) ;
#241843 = ORIENTED_EDGE ( 'NONE', *, *, #14102, .F. ) ;
#241844 = CARTESIAN_POINT ( 'NONE',  ( 22.39999999999999503, 11.65000000001116298, -33.50000000000000000 ) ) ;
#241845 = CARTESIAN_POINT ( 'NONE',  ( -16.82542659449977762, 66.06550010858508415, -182.7677430845504318 ) ) ;
#241848 = EDGE_CURVE ( 'NONE', #78009, #66095, #157884, .T. ) ;
#241847 = ORIENTED_EDGE ( 'NONE', *, *, #134256, .F. ) ;
#241846 = CARTESIAN_POINT ( 'NONE',  ( -22.50000000000000000, 0.000000000000000000, 0.1000000000000028644 ) ) ;
#241849 = CARTESIAN_POINT ( 'NONE',  ( 21.05000000000000071, -8.663551401858002876, -76.52410111806734960 ) ) ;
#241850 = DIRECTION ( 'NONE',  ( 0.000000000000000000, 0.000000000000000000, -1.000000000000000000 ) ) ;
#241851 = CARTESIAN_POINT ( 'NONE',  ( -22.39999999999999858, 59.68594599439717285, -233.9123800762197902 ) ) ;
#241852 = DIRECTION ( 'NONE',  ( 0.000000000000000000, 6.982962677686266711E-15, -1.000000000000000000 ) ) ;
#241853 = DIRECTION ( 'NONE',  ( 0.000000000000000000, 0.000000000000000000, 1.000000000000000000 ) ) ;
#241854 = EDGE_CURVE ( 'NONE', #144388, #197466, #252050, .T. ) ;
#241855 = DIRECTION ( 'NONE',  ( -2.940209281316620523E-16, 0.9770955615653310611, 0.2128009952263628657 ) ) ;
#241856 = EDGE_CURVE ( 'NONE', #23447, #156427, #170542, .T. ) ;
#241858 = ORIENTED_EDGE ( 'NONE', *, *, #208611, .F. ) ;
#241857 = DIRECTION ( 'NONE',  ( -1.000000000000000000, -2.952720810173289112E-16, 0.000000000000000000 ) ) ;
#241860 = ORIENTED_EDGE ( 'NONE', *, *, #236501, .T. ) ;
#241859 = DIRECTION ( 'NONE',  ( 0.7071067811865475727, 0.7071067811865475727, 4.937700262164531476E-15 ) ) ;
#241861 = CARTESIAN_POINT ( 'NONE',  ( -20.54999999999999716, 47.91013932883114990, -242.3192343197862044 ) ) ;
#241862 = CIRCLE ( 'NONE', #116976, 0.09999999999999530098 ) ;
#241863 = ORIENTED_EDGE ( 'NONE', *, *, #87036, .F. ) ;
#241864 = DIRECTION ( 'NONE',  ( 1.000000000000000000, 0.000000000000000000, 0.000000000000000000 ) ) ;
#241866 = EDGE_CURVE ( 'NONE', #201957, #51518, #63939, .T. ) ;
#241865 = CARTESIAN_POINT ( 'NONE',  ( -20.94999999999994600, 64.35000000001120668, -29.92310748452479174 ) ) ;
#241867 = CARTESIAN_POINT ( 'NONE',  ( 21.05000000000000071, 0.4597584103430730762, -208.9850561804005906 ) ) ;
#241868 = CYLINDRICAL_SURFACE ( 'NONE', #63796, 12.87500000000000000 ) ;
#241869 = DIRECTION ( 'NONE',  ( 1.000000000000000000, 0.000000000000000000, -0.000000000000000000 ) ) ;
#241870 = VERTEX_POINT ( 'NONE', #190834 ) ;
#241871 = CARTESIAN_POINT ( 'NONE',  ( 21.05000000000000071, 71.18691588786226987, -81.46462524104816794 ) ) ;
#241872 = AXIS2_PLACEMENT_3D ( 'NONE', #30838, #253695, #212034 ) ;
#241873 = ORIENTED_EDGE ( 'NONE', *, *, #7003, .F. ) ;
#241874 = VERTEX_POINT ( 'NONE', #129548 ) ;
#241875 = AXIS2_PLACEMENT_3D ( 'NONE', #57295, #155172, #56003 ) ;
#241876 =( NAMED_UNIT ( * ) SI_UNIT ( $, .STERADIAN. ) SOLID_ANGLE_UNIT ( ) );
#241877 = VECTOR ( 'NONE', #45797, 1000.000000000000000 ) ;
#241878 = VERTEX_POINT ( 'NONE', #12186 ) ;
#241879 = FACE_OUTER_BOUND ( 'NONE', #62988, .T. ) ;
#241880 = AXIS2_PLACEMENT_3D ( 'NONE', #99367, #155551, #139784 ) ;
#241881 = CARTESIAN_POINT ( 'NONE',  ( -18.40000000000000213, 11.75000000001113953, -91.25000000000005684 ) ) ;
#241882 = ORIENTED_EDGE ( 'NONE', *, *, #108554, .T. ) ;
#241883 = EDGE_CURVE ( 'NONE', #199092, #135643, #91384, .T. ) ;
#241884 = ORIENTED_EDGE ( 'NONE', *, *, #71196, .F. ) ;
#241885 = ADVANCED_FACE ( 'NONE', ( #172574 ), #109965, .F. ) ;
#241886 = DIRECTION ( 'NONE',  ( 0.000000000000000000, 1.000000000000000000, 0.000000000000000000 ) ) ;
#241887 = ORIENTED_EDGE ( 'NONE', *, *, #218461, .F. ) ;
#241888 = DIRECTION ( 'NONE',  ( -1.073024830501117725E-15, -0.000000000000000000, -1.000000000000000000 ) ) ;
#241889 = SPHERICAL_SURFACE ( 'NONE', #163771, 0.1000000000000000056 ) ;
#241890 = VERTEX_POINT ( 'NONE', #171288 ) ;
#241891 = ADVANCED_FACE ( 'NONE', ( #151706 ), #50000, .T. ) ;
#241892 = CARTESIAN_POINT ( 'NONE',  ( -18.59999999999999787, 11.65000000001115232, -55.25000000000004974 ) ) ;
#241894 = ORIENTED_EDGE ( 'NONE', *, *, #88223, .T. ) ;
#241893 = DIRECTION ( 'NONE',  ( -1.000000000000000000, 0.000000000000000000, 0.000000000000000000 ) ) ;
#241895 = FACE_OUTER_BOUND ( 'NONE', #67715, .T. ) ;
#241896 = EDGE_LOOP ( 'NONE', ( #81819, #207695, #31874 ) ) ;
#241897 = CARTESIAN_POINT ( 'NONE',  ( -16.94225986326249611, 66.05000000001261640, -190.5763881089164897 ) ) ;
#241898 = ORIENTED_EDGE ( 'NONE', *, *, #223931, .T. ) ;
#241899 = DIRECTION ( 'NONE',  ( -1.000000000000000000, 3.265361837132813093E-16, 2.280189983783949500E-30 ) ) ;
#241901 = CARTESIAN_POINT ( 'NONE',  ( 19.75857864376269291, 64.35000000001251408, -178.7731074845244450 ) ) ;
#241900 = AXIS2_PLACEMENT_3D ( 'NONE', #4446, #3152, #82673 ) ;
#241902 = FACE_OUTER_BOUND ( 'NONE', #172417, .T. ) ;
#241903 = DIRECTION ( 'NONE',  ( 1.000000000000000000, -0.000000000000000000, 0.000000000000000000 ) ) ;
#241904 = LINE ( 'NONE', #84069, #73063 ) ;
#241905 = DIRECTION ( 'NONE',  ( -0.000000000000000000, 0.000000000000000000, 1.000000000000000000 ) ) ;
#241906 = TOROIDAL_SURFACE ( 'NONE', #129507, 0.2000000000000000111, 0.1000000000000000056 ) ;
#241907 = ORIENTED_EDGE ( 'NONE', *, *, #186406, .F. ) ;
#241908 = CARTESIAN_POINT ( 'NONE',  ( -21.05000000000000071, 1.115600667400684642E-11, -141.9000000000000341 ) ) ;
#241909 = DIRECTION ( 'NONE',  ( 1.186688945009010077E-16, 0.9651348961777157509, -0.2617529984165031243 ) ) ;
#241910 = DIRECTION ( 'NONE',  ( 1.073024830501117725E-15, -0.000000000000000000, -1.000000000000000000 ) ) ;
#241911 = CARTESIAN_POINT ( 'NONE',  ( 21.59780538579342135, 1.139892542176100809, -230.4123047064117316 ) ) ;
#241912 = CIRCLE ( 'NONE', #146057, 0.5000000000000004441 ) ;
#241913 = EDGE_CURVE ( 'NONE', #4010, #94457, #189525, .T. ) ;
#241914 = VERTEX_POINT ( 'NONE', #72153 ) ;
#241915 = CARTESIAN_POINT ( 'NONE',  ( -18.59999999999999787, 69.06610602788553877, -99.23746165015076315 ) ) ;
#241916 = ORIENTED_EDGE ( 'NONE', *, *, #141713, .F. ) ;
#241917 = CARTESIAN_POINT ( 'NONE',  ( 18.59999999999999787, -9.849999999999996092, 31.39999999999999858 ) ) ;
#241918 = ORIENTED_EDGE ( 'NONE', *, *, #178455, .F. ) ;
#241919 = CARTESIAN_POINT ( 'NONE',  ( 18.49999999999999645, -1.835859311432484375, -212.5044391687984842 ) ) ;
#241920 = CARTESIAN_POINT ( 'NONE',  ( -20.85000000000000142, 10.33248238083634440, -72.59484654391314962 ) ) ;
#241921 = ORIENTED_EDGE ( 'NONE', *, *, #105959, .F. ) ;
#241922 = AXIS2_PLACEMENT_3D ( 'NONE', #70823, #29146, #111206 ) ;
#241925 = VERTEX_POINT ( 'NONE', #150405 ) ;
#241924 = ADVANCED_FACE ( 'NONE', ( #10886 ), #132112, .T. ) ;
#241923 = CARTESIAN_POINT ( 'NONE',  ( 18.49999999999999645, 7.675662554762638479, -241.7139905447625381 ) ) ;
#241926 = CARTESIAN_POINT ( 'NONE',  ( -18.39999999999999858, 64.52683809664941350, -93.69716141771641560 ) ) ;
#241927 = EDGE_LOOP ( 'NONE', ( #255147, #255576, #34184, #212866 ) ) ;
#241928 = CARTESIAN_POINT ( 'NONE',  ( -22.45372860728439690, 0.01492061955964464615, -21.85020286529612576 ) ) ;
#241929 = ADVANCED_FACE ( 'NONE', ( #92973 ), #211663, .T. ) ;
#241930 = CYLINDRICAL_SURFACE ( 'NONE', #235435, 0.09999999999999939493 ) ;
#241931 = ORIENTED_EDGE ( 'NONE', *, *, #72732, .F. ) ;
#241932 = VERTEX_POINT ( 'NONE', #34319 ) ;
#241933 = DIRECTION ( 'NONE',  ( -1.000000000000000000, 0.000000000000000000, 0.000000000000000000 ) ) ;
#241935 = EDGE_CURVE ( 'NONE', #252199, #140280, #95470, .T. ) ;
#241934 = DIRECTION ( 'NONE',  ( 1.000000000000000000, 0.000000000000000000, 0.000000000000000000 ) ) ;
#241936 = CARTESIAN_POINT ( 'NONE',  ( 20.95512820512820440, 22.03025613173517883, -231.6455594930189648 ) ) ;
#241937 = AXIS2_PLACEMENT_3D ( 'NONE', #220971, #144005, #183159 ) ;
#241938 = VECTOR ( 'NONE', #131862, 1000.000000000000000 ) ;
#241939 = ORIENTED_EDGE ( 'NONE', *, *, #86941, .T. ) ;
#241940 = ORIENTED_EDGE ( 'NONE', *, *, #53180, .F. ) ;
#241941 = ADVANCED_FACE ( 'NONE', ( #35610 ), #14759, .F. ) ;
#241942 = VECTOR ( 'NONE', #49749, 1000.000000000000000 ) ;
#241945 = EDGE_CURVE ( 'NONE', #16903, #247452, #195453, .T. ) ;
#241944 = EDGE_CURVE ( 'NONE', #89497, #205134, #55102, .T. ) ;
#241943 = CARTESIAN_POINT ( 'NONE',  ( -21.05000000000000071, 1.115600667400684642E-11, -100.5000000000000426 ) ) ;
#241946 = CIRCLE ( 'NONE', #104556, 2.100000000000002309 ) ;
#241947 = CIRCLE ( 'NONE', #46142, 0.09999999999999911737 ) ;
#241948 = AXIS2_PLACEMENT_3D ( 'NONE', #13533, #193461, #14838 ) ;
#241950 = VERTEX_POINT ( 'NONE', #38159 ) ;
#241949 = CARTESIAN_POINT ( 'NONE',  ( 18.59999999999999787, -9.749999999999994671, 30.09999999999999076 ) ) ;
#241951 = CARTESIAN_POINT ( 'NONE',  ( -16.77683809663752257, 52.34166666667822199, -52.77310748452448763 ) ) ;
#241952 = CARTESIAN_POINT ( 'NONE',  ( -22.47886152344871036, 75.96249906115004080, -81.17309612757226489 ) ) ;
#241953 = DIRECTION ( 'NONE',  ( 0.000000000000000000, -1.000000000000000000, -7.272083257015735086E-15 ) ) ;
#241955 = DIRECTION ( 'NONE',  ( 1.000000000000000000, 0.000000000000000000, 0.000000000000000000 ) ) ;
#241954 = CARTESIAN_POINT ( 'NONE',  ( -18.59999999999999787, 66.85000000001275566, -215.2731074845244166 ) ) ;
#241956 = CARTESIAN_POINT ( 'NONE',  ( 21.05000000000036309, 10.60832956796502025, -108.0916850132954607 ) ) ;
#241957 = DIRECTION ( 'NONE',  ( 0.000000000000000000, -0.9126074666063770380, -0.4088369013363281068 ) ) ;
#241958 = CARTESIAN_POINT ( 'NONE',  ( -16.88495309932520883, 60.93084759950085783, -221.0554292032533112 ) ) ;
#241959 = AXIS2_PLACEMENT_3D ( 'NONE', #57978, #234062, #119275 ) ;
#241960 = CARTESIAN_POINT ( 'NONE',  ( 20.94999999999999929, 66.37537870982728805, -213.6053525232321704 ) ) ;
#241961 = EDGE_CURVE ( 'NONE', #189338, #225448, #18585, .T. ) ;
#241963 = EDGE_CURVE ( 'NONE', #87080, #236598, #138493, .T. ) ;
#241962 = VECTOR ( 'NONE', #250526, 1000.000000000000227 ) ;
#241964 = TOROIDAL_SURFACE ( 'NONE', #137330, 0.2000000000000000111, 0.1000000000000000056 ) ;
#241966 = ORIENTED_EDGE ( 'NONE', *, *, #167142, .T. ) ;
#241965 = AXIS2_PLACEMENT_3D ( 'NONE', #226164, #123256, #224902 ) ;
#241967 = ORIENTED_EDGE ( 'NONE', *, *, #171910, .T. ) ;
#241968 = ADVANCED_FACE ( 'NONE', ( #155558 ), #149660, .T. ) ;
#241969 = DIRECTION ( 'NONE',  ( -1.000000000000000000, 0.000000000000000000, 0.000000000000000000 ) ) ;
#241970 = EDGE_LOOP ( 'NONE', ( #141558, #179903, #77056, #99241 ) ) ;
#241971 = CARTESIAN_POINT ( 'NONE',  ( -16.87036670365549895, 65.91505003675678154, -123.9731074845243626 ) ) ;
#241972 = EDGE_CURVE ( 'NONE', #31606, #111418, #178978, .T. ) ;
#241973 = AXIS2_PLACEMENT_3D ( 'NONE', #182331, #223993, #28416 ) ;
#241974 = EDGE_LOOP ( 'NONE', ( #238118, #109208, #65595 ) ) ;
#241975 = SURFACE_STYLE_USAGE ( .BOTH. , #103719 ) ;
#241976 = CARTESIAN_POINT ( 'NONE',  ( -18.34374000495059676, 11.47316190337362940, -91.25000000000005684 ) ) ;
#241977 = EDGE_CURVE ( 'NONE', #137749, #224282, #219334, .T. ) ;
#241979 = VERTEX_POINT ( 'NONE', #98078 ) ;
#241978 = VERTEX_POINT ( 'NONE', #77253 ) ;
#241980 = ORIENTED_EDGE ( 'NONE', *, *, #199612, .F. ) ;
#241981 = ORIENTED_EDGE ( 'NONE', *, *, #125705, .T. ) ;
#241982 = CARTESIAN_POINT ( 'NONE',  ( -20.00857864376270001, 66.65000000001222702, -148.8731074845244393 ) ) ;
#241983 = CARTESIAN_POINT ( 'NONE',  ( 13.99999999999999822, 66.15000000001228386, -153.2731074845244450 ) ) ;
#241985 = VERTEX_POINT ( 'NONE', #116406 ) ;
#241984 = DIRECTION ( 'NONE',  ( 0.000000000000000000, 0.000000000000000000, -1.000000000000000000 ) ) ;
#241986 = ADVANCED_FACE ( 'NONE', ( #100646 ), #237633, .T. ) ;
#241987 = CARTESIAN_POINT ( 'NONE',  ( 19.86930884467607328, 11.68691006698174739, -158.7392226389382870 ) ) ;
#241989 = VERTEX_POINT ( 'NONE', #40747 ) ;
#241988 = LINE ( 'NONE', #62077, #93548 ) ;
#241990 = FACE_OUTER_BOUND ( 'NONE', #154983, .T. ) ;
#241991 = ORIENTED_EDGE ( 'NONE', *, *, #92792, .F. ) ;
#241992 = CARTESIAN_POINT ( 'NONE',  ( -18.59999999999999787, 6.933893972126341509, -37.28564583437357527 ) ) ;
#241993 = VECTOR ( 'NONE', #122301, 1000.000000000000000 ) ;
#241995 = ORIENTED_EDGE ( 'NONE', *, *, #189710, .F. ) ;
#241994 = CARTESIAN_POINT ( 'NONE',  ( 21.05000000000000071, -8.999999999988842703, -191.6060308773475072 ) ) ;
#241996 = DIRECTION ( 'NONE',  ( 1.000000000000000000, 0.000000000000000000, 0.000000000000000000 ) ) ;
#241997 = CARTESIAN_POINT ( 'NONE',  ( -14.22969084473441725, 27.89153536508384335, -234.1274767587460133 ) ) ;
#241998 = CARTESIAN_POINT ( 'NONE',  ( -23.15000000000000213, 87.75000000001202238, -114.7731074845242318 ) ) ;
#242000 = ADVANCED_FACE ( 'NONE', ( #288 ), #216770, .T. ) ;
#241999 = ORIENTED_EDGE ( 'NONE', *, *, #213710, .T. ) ;
#242002 = CARTESIAN_POINT ( 'NONE',  ( -16.87435696428308063, 44.13547318391088936, -235.2989327256209151 ) ) ;
#242001 = DIRECTION ( 'NONE',  ( -1.000000000000000000, -0.000000000000000000, -0.000000000000000000 ) ) ;
#242003 = DIRECTION ( 'NONE',  ( 0.000000000000000000, 0.000000000000000000, -1.000000000000000000 ) ) ;
#242004 = CARTESIAN_POINT ( 'NONE',  ( -23.15000000000000213, 11.65000000001115588, -88.75000000000004263 ) ) ;
#242005 = DIRECTION ( 'NONE',  ( -1.000000000000000000, 0.000000000000000000, 0.000000000000000000 ) ) ;
#242006 = CARTESIAN_POINT ( 'NONE',  ( -20.85000000000000142, 67.75954444190071513, -227.8703747234148693 ) ) ;
#242007 = VERTEX_POINT ( 'NONE', #39463 ) ;
#242008 = VERTEX_POINT ( 'NONE', #198494 ) ;
#242009 = ORIENTED_EDGE ( 'NONE', *, *, #151039, .F. ) ;
#242011 = VECTOR ( 'NONE', #166384, 1000.000000000000000 ) ;
#242010 = LINE ( 'NONE', #43821, #63919 ) ;
#242012 = ORIENTED_EDGE ( 'NONE', *, *, #236028, .T. ) ;
#242013 = DIRECTION ( 'NONE',  ( -3.265361837132813093E-16, -1.000000000000000000, -6.982962677686266711E-15 ) ) ;
#242014 = VERTEX_POINT ( 'NONE', #78539 ) ;
#242015 = EDGE_CURVE ( 'NONE', #166805, #247452, #156837, .T. ) ;
#242016 = DIRECTION ( 'NONE',  ( 0.000000000000000000, 0.000000000000000000, 1.000000000000000000 ) ) ;
#242017 = CARTESIAN_POINT ( 'NONE',  ( -17.22767730082070869, 14.82413144765285651, -220.4329393275840516 ) ) ;
#242018 = ORIENTED_EDGE ( 'NONE', *, *, #71953, .T. ) ;
#242019 = DIRECTION ( 'NONE',  ( -1.000000000000000000, 0.000000000000000000, -0.000000000000000000 ) ) ;
#242020 =( NAMED_UNIT ( * ) PLANE_ANGLE_UNIT ( ) SI_UNIT ( $, .RADIAN. ) );
#242021 = CIRCLE ( 'NONE', #58663, 0.1000000000000013933 ) ;
#242023 = ORIENTED_EDGE ( 'NONE', *, *, #160082, .T. ) ;
#242022 = AXIS2_PLACEMENT_3D ( 'NONE', #86741, #47613, #124614 ) ;
#242024 = VERTEX_POINT ( 'NONE', #1565 ) ;
#242025 = ORIENTED_EDGE ( 'NONE', *, *, #139640, .T. ) ;
#242026 = VECTOR ( 'NONE', #119737, 999.9999999999998863 ) ;
#242027 = DIRECTION ( 'NONE',  ( 0.000000000000000000, -0.9209589331071864615, 0.3896596508878908960 ) ) ;
#242028 = FILL_AREA_STYLE_COLOUR ( '', #153275 ) ;
#242029 = DIRECTION ( 'NONE',  ( 1.000000000000000000, 0.000000000000000000, 0.000000000000000000 ) ) ;
#242030 = DIRECTION ( 'NONE',  ( 0.000000000000000000, 0.4721928772777331806, 0.8814952561688438326 ) ) ;
#242031 = CYLINDRICAL_SURFACE ( 'NONE', #172076, 0.1000000000000028644 ) ;
#242032 =( BOUNDED_SURFACE ( )  B_SPLINE_SURFACE ( 3, 2, ( 
 ( #42299, #124413, #166136 ),
 ( #201365, #241772, #1858 ),
 ( #245636, #24039, #102225 ),
 ( #140089, #160976, #145233 ) ),
 .UNSPECIFIED., .F., .F., .F. ) 
 B_SPLINE_SURFACE_WITH_KNOTS ( ( 4, 4 ),
 ( 3, 3 ),
 ( 3.658908243880901523, 4.712388980384689674 ),
 ( 0.000000000000000000, 1.000000000000000000 ),
 .UNSPECIFIED. ) 
 GEOMETRIC_REPRESENTATION_ITEM ( )  RATIONAL_B_SPLINE_SURFACE ( (
 ( 1.000000000000000000, 0.8984936768950856356, 1.000000000000000000),
 ( 1.000000000000000000, 0.8646876308616651130, 1.000000000000000000),
 ( 1.000000000000000000, 0.7953136715911847121, 1.000000000000000000),
 ( 1.000000000000000000, 0.7071067811866510455, 1.000000000000000000) ) ) 
 REPRESENTATION_ITEM ( '' )  SURFACE ( )  );
#242034 = DIRECTION ( 'NONE',  ( -0.000000000000000000, -0.07893460099012017395, 0.9968797965484759160 ) ) ;
#242033 = DIRECTION ( 'NONE',  ( -3.265361837132813586E-16, -0.4088369013363280513, 0.9126074666063769270 ) ) ;
#242035 = DIRECTION ( 'NONE',  ( -1.000000000000000000, -0.000000000000000000, -0.000000000000000000 ) ) ;
#242037 = EDGE_LOOP ( 'NONE', ( #207005, #68143, #9734, #229788 ) ) ;
#242036 = LINE ( 'NONE', #2132, #210623 ) ;
#242038 = CARTESIAN_POINT ( 'NONE',  ( 21.14999999999999858, 76.10000000001272724, -210.0637644362255969 ) ) ;
#242039 = CARTESIAN_POINT ( 'NONE',  ( 23.15000000000000213, -8.999999999988842703, -57.60603087734755690 ) ) ;
#242040 = ORIENTED_EDGE ( 'NONE', *, *, #239075, .T. ) ;
#242041 = DIRECTION ( 'NONE',  ( 0.000000000000000000, -1.734723475976757554E-14, 1.000000000000000000 ) ) ;
#242042 = CYLINDRICAL_SURFACE ( 'NONE', #93642, 2.000000000000001776 ) ;
#242043 = CYLINDRICAL_SURFACE ( 'NONE', #162318, 0.1000000000000012546 ) ;
#242044 = EDGE_LOOP ( 'NONE', ( #48473, #74014, #70812, #94413, #20747, #136035, #30702, #207891, #256702 ) ) ;
#242045 = VECTOR ( 'NONE', #70687, 1000.000000000000000 ) ;
#242046 = B_SPLINE_CURVE_WITH_KNOTS ( 'NONE', 3,
 ( #162399, #24173, #247040, #7146, #187107, #8454, #26750, #164950, #106237, #167547, #82804, #245777, #103664 ),
 .UNSPECIFIED., .F., .F.,
 ( 4, 3, 3, 3, 4 ),
 ( -3.224855718275878119E-06, -4.235164736271501695E-22, 6.199515528669195097E-06, 4.034952380127538728E-05, 7.452715123699865944E-05 ),
 .UNSPECIFIED. ) ;
#242047 = CARTESIAN_POINT ( 'NONE',  ( 21.11101077988997332, 69.57631526528663812, -203.5383927534386999 ) ) ;
#242048 = DIRECTION ( 'NONE',  ( -1.000000000000000000, -0.000000000000000000, -0.000000000000000000 ) ) ;
#242049 = VERTEX_POINT ( 'NONE', #137236 ) ;
#242050 = VERTEX_POINT ( 'NONE', #56401 ) ;
#242051 = CARTESIAN_POINT ( 'NONE',  ( -23.15000000000000213, -8.596261682231830292, -124.5498724828497501 ) ) ;
#242052 = ORIENTED_EDGE ( 'NONE', *, *, #223346, .T. ) ;
#242053 = CARTESIAN_POINT ( 'NONE',  ( 21.53752568617671415, 6.786807874515035977, -66.90102553872934266 ) ) ;
#242054 = CARTESIAN_POINT ( 'NONE',  ( -18.39999999999999503, -9.499999999988851584, -174.1001893912220737 ) ) ;
#242055 = DIRECTION ( 'NONE',  ( -0.000000000000000000, -6.982962677686266711E-15, 1.000000000000000000 ) ) ;
#242056 = DIRECTION ( 'NONE',  ( 0.000000000000000000, -0.1480365673253065117, 0.9889818879709273425 ) ) ;
#242057 = ORIENTED_EDGE ( 'NONE', *, *, #127501, .F. ) ;
#242058 = VECTOR ( 'NONE', #192683, 1000.000000000000000 ) ;
#242061 = EDGE_CURVE ( 'NONE', #88568, #91302, #37409, .T. ) ;
#242060 = DIRECTION ( 'NONE',  ( 0.000000000000000000, 0.000000000000000000, 1.000000000000000000 ) ) ;
#242059 = VECTOR ( 'NONE', #6088, 1000.000000000000000 ) ;
#242062 = AXIS2_PLACEMENT_3D ( 'NONE', #17887, #234370, #213522 ) ;
#242063 = CARTESIAN_POINT ( 'NONE',  ( 23.15000000000000213, -11.64999999998883595, -164.4000000000000057 ) ) ;
#242064 = FACE_OUTER_BOUND ( 'NONE', #251574, .T. ) ;
#242065 = VERTEX_POINT ( 'NONE', #58953 ) ;
#242067 = ORIENTED_EDGE ( 'NONE', *, *, #71845, .T. ) ;
#242066 = LINE ( 'NONE', #218647, #229461 ) ;
#242068 = CARTESIAN_POINT ( 'NONE',  ( 18.49999999999998934, 10.90071697730193456, -220.2717246083756208 ) ) ;
#242069 = DIRECTION ( 'NONE',  ( 0.000000000000000000, 0.000000000000000000, -1.000000000000000000 ) ) ;
#242070 = ADVANCED_FACE ( 'NONE', ( #240207 ), #208101, .T. ) ;
#242071 = CARTESIAN_POINT ( 'NONE',  ( -20.85000000000000142, 11.64999999999999680, -33.50000000000000000 ) ) ;
#242072 = DIRECTION ( 'NONE',  ( 0.000000000000000000, -0.8660254037844411501, -0.4999999999999956146 ) ) ;
#242073 = DIRECTION ( 'NONE',  ( -1.000000000000000000, -0.000000000000000000, -0.000000000000000000 ) ) ;
#242074 = CARTESIAN_POINT ( 'NONE',  ( -23.25000000000000000, 1.115600667400684642E-11, -67.00000000000000000 ) ) ;
#242075 = AXIS2_PLACEMENT_3D ( 'NONE', #113179, #234397, #14097 ) ;
#242076 = EDGE_CURVE ( 'NONE', #238821, #11972, #36896, .T. ) ;
#242077 = ORIENTED_EDGE ( 'NONE', *, *, #179326, .T. ) ;
#242078 = CARTESIAN_POINT ( 'NONE',  ( -21.65000000000000213, 9.052352027203962592, -208.4953267290897543 ) ) ;
#242079 = LINE ( 'NONE', #63439, #35765 ) ;
#242080 = DIRECTION ( 'NONE',  ( 1.000000000000000000, 0.000000000000000000, 0.000000000000000000 ) ) ;
#242081 = CARTESIAN_POINT ( 'NONE',  ( 22.47071067811865319, 7.720074744509197728, -133.9009075452974002 ) ) ;
#242082 = DIRECTION ( 'NONE',  ( 0.000000000000000000, 0.000000000000000000, -1.000000000000000000 ) ) ;
#242083 = DIRECTION ( 'NONE',  ( -0.000000000000000000, 0.000000000000000000, 1.000000000000000000 ) ) ;
#242084 = ORIENTED_EDGE ( 'NONE', *, *, #32952, .T. ) ;
#242085 = ORIENTED_EDGE ( 'NONE', *, *, #144860, .F. ) ;
#242086 = FACE_OUTER_BOUND ( 'NONE', #114558, .T. ) ;
#242087 = DIRECTION ( 'NONE',  ( 1.000000000000000000, 0.000000000000000000, 0.000000000000000000 ) ) ;
#242088 = EDGE_CURVE ( 'NONE', #71592, #104858, #19879, .T. ) ;
#242089 = CARTESIAN_POINT ( 'NONE',  ( 21.46681500597193093, 1.115539681028482333E-11, -127.1424888405652212 ) ) ;
#242090 = DIRECTION ( 'NONE',  ( 0.000000000000000000, -6.517943393102681197E-15, 1.000000000000000000 ) ) ;
#242091 = EDGE_CURVE ( 'NONE', #199740, #187756, #101934, .T. ) ;
#242092 = AXIS2_PLACEMENT_3D ( 'NONE', #250147, #10260, #29843 ) ;
#242093 = VERTEX_POINT ( 'NONE', #197209 ) ;
#242094 = DIRECTION ( 'NONE',  ( 1.000000000000000000, 0.000000000000000000, 0.000000000000000000 ) ) ;
#242095 = EDGE_CURVE ( 'NONE', #238428, #48720, #236339, .T. ) ;
#242096 = SPHERICAL_SURFACE ( 'NONE', #59312, 0.1000000000000000056 ) ;
#242097 = TOROIDAL_SURFACE ( 'NONE', #100434, 0.2000000000000000111, 0.1000000000000000056 ) ;
#242098 = DIRECTION ( 'NONE',  ( -1.000000000000000000, -2.885090398161910739E-16, -6.283419270304611573E-17 ) ) ;
#242099 = EDGE_CURVE ( 'NONE', #195218, #30065, #195638, .T. ) ;
#242100 = DIRECTION ( 'NONE',  ( 0.000000000000000000, 1.000000000000000000, 0.000000000000000000 ) ) ;
#242101 = VECTOR ( 'NONE', #27040, 1000.000000000000000 ) ;
#242102 = CIRCLE ( 'NONE', #200420, 4.049999999999999822 ) ;
#242103 = EDGE_CURVE ( 'NONE', #72605, #156710, #212195, .T. ) ;
#242104 = VERTEX_POINT ( 'NONE', #105783 ) ;
#242105 = DIRECTION ( 'NONE',  ( 0.000000000000000000, -1.000000000000000000, 0.000000000000000000 ) ) ;
#242106 = VECTOR ( 'NONE', #225385, 1000.000000000000000 ) ;
#242107 = ORIENTED_EDGE ( 'NONE', *, *, #47782, .T. ) ;
#242108 = DIRECTION ( 'NONE',  ( 0.000000000000000000, 0.8814952561688430555, -0.4721928772777346239 ) ) ;
#242109 = CARTESIAN_POINT ( 'NONE',  ( 21.05000000000000071, 0.06570161032208717000, 6.258316057332036664 ) ) ;
#242110 = CARTESIAN_POINT ( 'NONE',  ( -21.15000000000000213, 10.21728496540352360, -227.9671432372868765 ) ) ;
#242111 = CARTESIAN_POINT ( 'NONE',  ( -23.15000000000000213, 64.35000000001228670, -157.8731074845244393 ) ) ;
#242112 = CARTESIAN_POINT ( 'NONE',  ( 18.52928932188133970, 65.72071067813043044, -78.37310748452438247 ) ) ;
#242113 = DIRECTION ( 'NONE',  ( -2.978066053179067751E-16, 1.000000000000000000, 0.000000000000000000 ) ) ;
#242114 = AXIS2_PLACEMENT_3D ( 'NONE', #13650, #112752, #237832 ) ;
#242115 = DIRECTION ( 'NONE',  ( 1.000000000000000000, 0.000000000000000000, 0.000000000000000000 ) ) ;
#242116 = EDGE_CURVE ( 'NONE', #172693, #104276, #221884, .T. ) ;
#242117 = CARTESIAN_POINT ( 'NONE',  ( -20.85000000000000142, 56.18374508921710486, -227.9290876000915489 ) ) ;
#242118 = FACE_OUTER_BOUND ( 'NONE', #219883, .T. ) ;
#242119 = LINE ( 'NONE', #143005, #14879 ) ;
#242120 = DIRECTION ( 'NONE',  ( 1.000000000000000000, 0.000000000000000000, 0.000000000000000000 ) ) ;
#242121 = AXIS2_PLACEMENT_3D ( 'NONE', #177418, #176128, #135673 ) ;
#242122 = CIRCLE ( 'NONE', #92288, 0.09999999999999641120 ) ;
#242123 = CYLINDRICAL_SURFACE ( 'NONE', #128676, 0.1000000000000028644 ) ;
#242124 = CARTESIAN_POINT ( 'NONE',  ( -21.14999999999999858, 64.25000000001161027, -62.79697684846522066 ) ) ;
#242125 = ORIENTED_EDGE ( 'NONE', *, *, #236515, .F. ) ;
#242127 =( BOUNDED_SURFACE ( )  B_SPLINE_SURFACE ( 3, 2, ( 
 ( #199763, #161919, #79759 ),
 ( #241444, #198449, #121513 ),
 ( #1522, #120241, #98033 ),
 ( #219292, #159348, #180190 ) ),
 .UNSPECIFIED., .F., .F., .F. ) 
 B_SPLINE_SURFACE_WITH_KNOTS ( ( 4, 4 ),
 ( 3, 3 ),
 ( 0.3000847527772392276, 0.5552748953338751958 ),
 ( 0.000000000000000000, 1.000000000000000000 ),
 .UNSPECIFIED. ) 
 GEOMETRIC_REPRESENTATION_ITEM ( )  RATIONAL_B_SPLINE_SURFACE ( (
 ( 1.000000000000000000, 0.9152888060719425178, 1.000000000000000000),
 ( 1.000000000000000000, 0.9104333467450189676, 1.000000000000000000),
 ( 1.000000000000000000, 0.9035312726220716684, 1.000000000000000000),
 ( 1.000000000000000000, 0.8946697475932030574, 1.000000000000000000) ) ) 
 REPRESENTATION_ITEM ( '' )  SURFACE ( )  );
#242126 = VECTOR ( 'NONE', #190688, 1000.000000000000000 ) ;
#242128 = CARTESIAN_POINT ( 'NONE',  ( 21.14999999999999858, 11.65000000001115943, -179.6499999999999773 ) ) ;
#242129 = FACE_OUTER_BOUND ( 'NONE', #18700, .T. ) ;
#242130 = AXIS2_PLACEMENT_3D ( 'NONE', #35064, #154997, #177128 ) ;
#242131 = ORIENTED_EDGE ( 'NONE', *, *, #14686, .T. ) ;
#242132 = CARTESIAN_POINT ( 'NONE',  ( -22.45372860728439690, 0.01492061955964465135, -55.35020286529617550 ) ) ;
#242133 = CARTESIAN_POINT ( 'NONE',  ( 21.07964655665547227, 67.22511038503374436, -157.8011909015603749 ) ) ;
#242134 = CARTESIAN_POINT ( 'NONE',  ( -16.94107738177413580, 10.01423928514777195, -188.4499999999999602 ) ) ;
#242135 = ORIENTED_EDGE ( 'NONE', *, *, #246273, .F. ) ;
#242136 = DIRECTION ( 'NONE',  ( -1.000000000000000000, 0.000000000000000000, 0.000000000000000000 ) ) ;
#242137 = DIRECTION ( 'NONE',  ( -1.000000000000000000, 7.304098846218134667E-16, -4.217023435051678980E-16 ) ) ;
#242138 = CIRCLE ( 'NONE', #34090, 0.09999999999999990841 ) ;
#242139 = VERTEX_POINT ( 'NONE', #225737 ) ;
#242140 = CIRCLE ( 'NONE', #154698, 0.09999999999999939493 ) ;
#242141 = AXIS2_PLACEMENT_3D ( 'NONE', #174795, #155215, #156504 ) ;
#242142 = AXIS2_PLACEMENT_3D ( 'NONE', #49054, #9936, #245986 ) ;
#242143 = EDGE_CURVE ( 'NONE', #136469, #184662, #166421, .T. ) ;
#242144 = VERTEX_POINT ( 'NONE', #164522 ) ;
#242145 = CARTESIAN_POINT ( 'NONE',  ( -20.85000000000000142, 36.65892442174935439, -249.5511627012433848 ) ) ;
#242146 = ORIENTED_EDGE ( 'NONE', *, *, #168383, .F. ) ;
#242147 = DIRECTION ( 'NONE',  ( 1.000000000000000000, 0.000000000000000000, 0.000000000000000000 ) ) ;
#242148 = EDGE_CURVE ( 'NONE', #196258, #108824, #43283, .T. ) ;
#242150 = ADVANCED_FACE ( 'NONE', ( #65401 ), #53949, .T. ) ;
#242149 = CARTESIAN_POINT ( 'NONE',  ( 18.59999999999999432, 13.71992543034163958, -238.5823796952984992 ) ) ;
#242151 = DIRECTION ( 'NONE',  ( 0.000000000000000000, 0.000000000000000000, 1.000000000000000000 ) ) ;
#242152 = CARTESIAN_POINT ( 'NONE',  ( 21.14999999999999858, 76.00000000001246292, -181.6726782920691505 ) ) ;
#242153 = DIRECTION ( 'NONE',  ( 1.000000000000000000, -0.000000000000000000, -0.000000000000000000 ) ) ;
#242154 = DIRECTION ( 'NONE',  ( 1.000000000000000000, 0.000000000000000000, 0.000000000000000000 ) ) ;
#242155 = PLANE ( 'NONE',  #108328 ) ;
#242156 = EDGE_CURVE ( 'NONE', #139686, #161202, #74840, .T. ) ;
#242157 = CARTESIAN_POINT ( 'NONE',  ( 18.49999999999999645, 13.71992543034163781, -238.5823796952984992 ) ) ;
#242158 = CARTESIAN_POINT ( 'NONE',  ( -23.15000000000000213, 76.00000000001170974, -69.52310748452431710 ) ) ;
#242159 = EDGE_CURVE ( 'NONE', #122938, #180099, #116505, .T. ) ;
#242161 = VERTEX_POINT ( 'NONE', #125389 ) ;
#242160 = CARTESIAN_POINT ( 'NONE',  ( -18.50000000000001066, -9.421308209728413985, -40.74236321405096106 ) ) ;
#242162 = ORIENTED_EDGE ( 'NONE', *, *, #233906, .T. ) ;
#242164 = CYLINDRICAL_SURFACE ( 'NONE', #18875, 0.1000000000000024342 ) ;
#242163 = DIRECTION ( 'NONE',  ( -1.000000000000000000, 7.492892343619937423E-30, -1.073024830501117725E-15 ) ) ;
#242166 = VERTEX_POINT ( 'NONE', #202349 ) ;
#242165 = CARTESIAN_POINT ( 'NONE',  ( -16.84981964351505113, 61.02838145972558692, -220.8383371048568904 ) ) ;
#242167 = EDGE_CURVE ( 'NONE', #180924, #78889, #226462, .T. ) ;
#242168 = B_SPLINE_CURVE_WITH_KNOTS ( 'NONE', 3,
 ( #192966, #151278, #134246, #52143, #213801, #131698, #15637, #191707, #13061, #53448, #132998, #212539, #33937, #113420 ),
 .UNSPECIFIED., .F., .F.,
 ( 4, 2, 2, 2, 2, 2, 4 ),
 ( 0.000000000000000000, 0.0003823333598417659224, 0.0005735000397626485854, 0.0006690833797230926003, 0.0007168750497033104336, 0.0007407708846934199466, 0.0007646667196835293511 ),
 .UNSPECIFIED. ) ;
#242169 = VERTEX_POINT ( 'NONE', #143653 ) ;
#242170 = DIRECTION ( 'NONE',  ( -0.000000000000000000, 0.9126074666063771490, 0.4088369013363281623 ) ) ;
#242171 = ADVANCED_FACE ( 'NONE', ( #82367 ), #204900, .T. ) ;
#242172 = FACE_OUTER_BOUND ( 'NONE', #214968, .T. ) ;
#242174 = EDGE_CURVE ( 'NONE', #13858, #94366, #48399, .T. ) ;
#242173 = DIRECTION ( 'NONE',  ( 1.000000000000000000, 0.000000000000000000, 0.000000000000000000 ) ) ;
#242175 = DIRECTION ( 'NONE',  ( 0.000000000000000000, 0.000000000000000000, -1.000000000000000000 ) ) ;
#242176 = LINE ( 'NONE', #257840, #199898 ) ;
#242177 = CARTESIAN_POINT ( 'NONE',  ( 20.94999999999999929, 0.6656436123793473270, -212.6810495496487476 ) ) ;
#242178 = CARTESIAN_POINT ( 'NONE',  ( -15.55912972643741199, 8.490870273562562076, -12.65000000000000213 ) ) ;
#242179 = ORIENTED_EDGE ( 'NONE', *, *, #241130, .T. ) ;
#242180 = ORIENTED_EDGE ( 'NONE', *, *, #3809, .F. ) ;
#242181 = LINE ( 'NONE', #161385, #164743 ) ;
#242182 = VERTEX_POINT ( 'NONE', #146214 ) ;
#242183 = CARTESIAN_POINT ( 'NONE',  ( 23.15000000000000213, 87.65000000001215597, -139.5231074845243029 ) ) ;
#242184 = ORIENTED_EDGE ( 'NONE', *, *, #200877, .F. ) ;
#242185 = DIRECTION ( 'NONE',  ( -3.265361837132813093E-16, -1.000000000000000000, 7.445645354460596589E-46 ) ) ;
#242186 = ADVANCED_FACE ( 'NONE', ( #186654 ), #8014, .F. ) ;
#242187 = AXIS2_PLACEMENT_3D ( 'NONE', #240444, #222128, #138728 ) ;
#242188 = FACE_OUTER_BOUND ( 'NONE', #39286, .T. ) ;
#242189 = CARTESIAN_POINT ( 'NONE',  ( 18.50000000000009948, 65.71984138295431421, -44.79853541332369105 ) ) ;
#242190 = EDGE_CURVE ( 'NONE', #16840, #17539, #83644, .T. ) ;
#242191 = CARTESIAN_POINT ( 'NONE',  ( -16.92778301347256331, 22.93290994670652694, -230.8530800172858619 ) ) ;
#242192 = ORIENTED_EDGE ( 'NONE', *, *, #140996, .F. ) ;
#242193 = EDGE_CURVE ( 'NONE', #195524, #141132, #79053, .T. ) ;
#242194 = DIRECTION ( 'NONE',  ( 0.000000000000000000, 0.000000000000000000, -1.000000000000000000 ) ) ;
#242195 = ORIENTED_EDGE ( 'NONE', *, *, #67340, .F. ) ;
#242196 = CARTESIAN_POINT ( 'NONE',  ( -20.64999999999999858, 0.000000000000000000, -33.50000000000000000 ) ) ;
#242197 = CARTESIAN_POINT ( 'NONE',  ( 23.14999999999998792, 11.65000000001115588, -167.4999999999999716 ) ) ;
#242198 = DIRECTION ( 'NONE',  ( 0.000000000000000000, 6.608470384673536035E-15, -1.000000000000000000 ) ) ;
#242199 = CARTESIAN_POINT ( 'NONE',  ( -23.15000000000000213, 87.65000000001246860, -173.1231074845242688 ) ) ;
#242200 = ORIENTED_EDGE ( 'NONE', *, *, #174786, .T. ) ;
#242202 = DIRECTION ( 'NONE',  ( -0.000000000000000000, -1.000000000000000000, -0.000000000000000000 ) ) ;
#242201 = AXIS2_PLACEMENT_3D ( 'NONE', #124677, #84193, #165078 ) ;
#242203 = ORIENTED_EDGE ( 'NONE', *, *, #253753, .F. ) ;
#242206 = ORIENTED_EDGE ( 'NONE', *, *, #50092, .T. ) ;
#242205 = CARTESIAN_POINT ( 'NONE',  ( -18.50000000000000000, 9.250000000011157297, -155.1500000000000057 ) ) ;
#242204 = CARTESIAN_POINT ( 'NONE',  ( -22.49999999999999645, 64.25043287652330548, -203.6239658536231900 ) ) ;
#242207 = AXIS2_PLACEMENT_3D ( 'NONE', #257331, #157031, #81289 ) ;
#242208 = CARTESIAN_POINT ( 'NONE',  ( -16.77683809663752257, 9.945835743215303282, -154.8360509808958057 ) ) ;
#242209 = ORIENTED_EDGE ( 'NONE', *, *, #95989, .T. ) ;
#242210 = CIRCLE ( 'NONE', #188060, 1.899999999999999023 ) ;
#242211 = DIRECTION ( 'NONE',  ( 0.000000000000000000, 0.000000000000000000, -1.000000000000000000 ) ) ;
#242212 = ORIENTED_EDGE ( 'NONE', *, *, #254212, .T. ) ;
#242213 = FACE_OUTER_BOUND ( 'NONE', #251177, .T. ) ;
#242214 = CARTESIAN_POINT ( 'NONE',  ( 21.05000000000000071, -9.000000000000000000, -23.60603087734755690 ) ) ;
#242215 = CARTESIAN_POINT ( 'NONE',  ( -18.46902351632713035, -9.509470118669714367, -73.98645393425734085 ) ) ;
#242216 = DIRECTION ( 'NONE',  ( -0.000000000000000000, 0.4721928772777346239, 0.8814952561688430555 ) ) ;
#242217 = CIRCLE ( 'NONE', #33994, 0.09999999999999939493 ) ;
#242218 = ORIENTED_EDGE ( 'NONE', *, *, #182721, .T. ) ;
#242219 = DIRECTION ( 'NONE',  ( -1.000000000000000000, -1.927470528863115795E-15, 0.000000000000000000 ) ) ;
#242220 = DIRECTION ( 'NONE',  ( 1.000000000000000000, -0.000000000000000000, -0.000000000000000000 ) ) ;
#242221 = DIRECTION ( 'NONE',  ( 0.000000000000000000, 0.000000000000000000, -1.000000000000000000 ) ) ;
#242222 = ORIENTED_EDGE ( 'NONE', *, *, #56088, .F. ) ;
#242223 = CARTESIAN_POINT ( 'NONE',  ( -20.94999999999999929, -1.164121893230052995, -108.4148480855716485 ) ) ;
#242224 = ORIENTED_EDGE ( 'NONE', *, *, #52700, .F. ) ;
#242225 = CARTESIAN_POINT ( 'NONE',  ( -20.94999999999999929, 76.00000000001213607, -136.5231074845243313 ) ) ;
#242226 = FACE_OUTER_BOUND ( 'NONE', #212666, .T. ) ;
#242227 = DIRECTION ( 'NONE',  ( -0.000000000000000000, -1.000000000000000000, 0.000000000000000000 ) ) ;
#242229 = ORIENTED_EDGE ( 'NONE', *, *, #43022, .F. ) ;
#242228 = CARTESIAN_POINT ( 'NONE',  ( -20.94999999999999929, 28.63831050940605394, -258.0693639473472558 ) ) ;
#242230 = DIRECTION ( 'NONE',  ( 0.000000000000000000, 0.000000000000000000, -1.000000000000000000 ) ) ;
#242231 = DIRECTION ( 'NONE',  ( 0.000000000000000000, 0.000000000000000000, 1.000000000000000000 ) ) ;
#242232 = ADVANCED_FACE ( 'NONE', ( #64126 ), #28900, .F. ) ;
#242233 = CIRCLE ( 'NONE', #13307, 0.1000000000000028644 ) ;
#242234 = AXIS2_PLACEMENT_3D ( 'NONE', #7333, #243370, #242082 ) ;
#242235 = CARTESIAN_POINT ( 'NONE',  ( -18.59999999999999787, -1.835859311432481045, -112.0044391687985694 ) ) ;
#242236 = VERTEX_POINT ( 'NONE', #211341 ) ;
#242237 = AXIS2_PLACEMENT_3D ( 'NONE', #228946, #131115, #69888 ) ;
#242238 = DIRECTION ( 'NONE',  ( -0.000000000000000000, -1.000000000000000000, 0.000000000000000000 ) ) ;
#242240 = EDGE_CURVE ( 'NONE', #135464, #2493, #30153, .T. ) ;
#242239 = DIRECTION ( 'NONE',  ( 1.000000000000000000, 0.000000000000000000, 0.000000000000000000 ) ) ;
#242241 = ORIENTED_EDGE ( 'NONE', *, *, #238557, .T. ) ;
#242242 = CARTESIAN_POINT ( 'NONE',  ( -21.00023020733502932, 65.55844536562159419, -242.0231774319958049 ) ) ;
#242243 = ORIENTED_EDGE ( 'NONE', *, *, #229146, .T. ) ;
#242244 = ADVANCED_FACE ( 'NONE', ( #50950 ), #3318, .T. ) ;
#242245 = FACE_OUTER_BOUND ( 'NONE', #246123, .T. ) ;
#242246 = ORIENTED_EDGE ( 'NONE', *, *, #100150, .T. ) ;
#242249 = ADVANCED_FACE ( 'NONE', ( #32742 ), #203981, .F. ) ;
#242248 = VERTEX_POINT ( 'NONE', #210067 ) ;
#242247 = PLANE ( 'NONE',  #68081 ) ;
#242250 = CIRCLE ( 'NONE', #25782, 0.5000000000000004441 ) ;
#242253 = EDGE_LOOP ( 'NONE', ( #83717, #132020, #28238, #202804 ) ) ;
#242252 = EDGE_LOOP ( 'NONE', ( #230879, #204329, #210305, #194457 ) ) ;
#242251 = CARTESIAN_POINT ( 'NONE',  ( -18.59999999999999787, -11.65000000000000036, 5.900000000000001243 ) ) ;
#242254 = DIRECTION ( 'NONE',  ( -1.000000000000000000, 0.000000000000000000, 0.000000000000000000 ) ) ;
#242255 = CARTESIAN_POINT ( 'NONE',  ( -2.995603634470891112E-16, 87.75000000001253397, -182.2731074845242745 ) ) ;
#242256 = LINE ( 'NONE', #63627, #223276 ) ;
#242258 = CARTESIAN_POINT ( 'NONE',  ( -18.34374000495059676, 62.50563584222673796, -209.4474707446456421 ) ) ;
#242257 = DIRECTION ( 'NONE',  ( 0.000000000000000000, -1.000000000000000000, -6.982962677686266711E-15 ) ) ;
#242259 = CARTESIAN_POINT ( 'NONE',  ( -18.37013991200266005, 64.50025238379961934, -60.31613049504152002 ) ) ;
#242260 = LINE ( 'NONE', #23258, #101316 ) ;
#242261 = EDGE_CURVE ( 'NONE', #223637, #189423, #90087, .T. ) ;
#242262 = CARTESIAN_POINT ( 'NONE',  ( 21.14999999999999858, 6.650000000011155876, -179.7499999999999716 ) ) ;
#242263 = EDGE_CURVE ( 'NONE', #104351, #176509, #172259, .T. ) ;
#242264 = ORIENTED_EDGE ( 'NONE', *, *, #228405, .F. ) ;
#242265 = EDGE_LOOP ( 'NONE', ( #107436, #94286, #129764, #11473, #21038, #76867, #194311, #242909, #46918, #50173, #122147, #16089, #244618, #165531, #34443, #224381, #163930, #240043, #205857, #159500, #185362, #240034, #241507, #204790, #49465, #102906, #221817 ) ) ;
#242266 = DIRECTION ( 'NONE',  ( -1.000000000000000000, -0.000000000000000000, -0.000000000000000000 ) ) ;
#242268 = ORIENTED_EDGE ( 'NONE', *, *, #44073, .F. ) ;
#242267 = DIRECTION ( 'NONE',  ( 0.000000000000000000, -0.3848449534832867891, -0.9229812358755983270 ) ) ;
#242269 = ORIENTED_EDGE ( 'NONE', *, *, #220751, .F. ) ;
#242271 = DIRECTION ( 'NONE',  ( 0.000000000000000000, 0.9908441862701605762, -0.1350103645451835310 ) ) ;
#242270 = AXIS2_PLACEMENT_3D ( 'NONE', #216605, #217865, #116245 ) ;
#242272 = ORIENTED_EDGE ( 'NONE', *, *, #3065, .F. ) ;
#242273 = LINE ( 'NONE', #105302, #129568 ) ;
#242274 = CIRCLE ( 'NONE', #79764, 0.5000000000000004441 ) ;
#242275 = EDGE_CURVE ( 'NONE', #22326, #90118, #220564, .T. ) ;
#242276 = ORIENTED_EDGE ( 'NONE', *, *, #253187, .F. ) ;
#242278 = TOROIDAL_SURFACE ( 'NONE', #100606, 1.900000000000002576, 0.1000000000000000056 ) ;
#242277 = DIRECTION ( 'NONE',  ( 1.000000000000000000, -0.000000000000000000, 0.000000000000000000 ) ) ;
#242279 = PLANE ( 'NONE',  #136294 ) ;
#242280 = EDGE_CURVE ( 'NONE', #11922, #136223, #245505, .T. ) ;
#242282 = ORIENTED_EDGE ( 'NONE', *, *, #198683, .F. ) ;
#242281 = ORIENTED_EDGE ( 'NONE', *, *, #153106, .T. ) ;
#242283 = VERTEX_POINT ( 'NONE', #53548 ) ;
#242285 = CARTESIAN_POINT ( 'NONE',  ( 21.08750232978087524, 10.72486338602132250, -45.72885817299957267 ) ) ;
#242284 = AXIS2_PLACEMENT_3D ( 'NONE', #93908, #232158, #155206 ) ;
#242286 = ORIENTED_EDGE ( 'NONE', *, *, #86418, .T. ) ;
#242287 = VERTEX_POINT ( 'NONE', #212634 ) ;
#242288 = DIRECTION ( 'NONE',  ( 0.000000000000000000, 0.000000000000000000, -1.000000000000000000 ) ) ;
#242289 = DIRECTION ( 'NONE',  ( 0.000000000000000000, 0.6728971962616412394, -0.7397360091703134577 ) ) ;
#242290 = CIRCLE ( 'NONE', #225135, 0.1000000000000124678 ) ;
#242292 = ORIENTED_EDGE ( 'NONE', *, *, #56481, .T. ) ;
#242291 = FACE_OUTER_BOUND ( 'NONE', #139674, .T. ) ;
#242294 = CARTESIAN_POINT ( 'NONE',  ( -16.89060415895971090, 60.93711167174846111, -221.0453457311873819 ) ) ;
#242293 = LINE ( 'NONE', #66240, #15866 ) ;
#242295 = EDGE_CURVE ( 'NONE', #29148, #9105, #99718, .T. ) ;
#242296 = CARTESIAN_POINT ( 'NONE',  ( 21.08479644141222309, 0.05855444257529583002, -60.65496134226815172 ) ) ;
#242297 = DIRECTION ( 'NONE',  ( 1.000000000000000000, 0.000000000000000000, 0.000000000000000000 ) ) ;
#242298 = CARTESIAN_POINT ( 'NONE',  ( -21.22070241538126112, 6.469946272880768845, -66.90108096946502769 ) ) ;
#242299 = ORIENTED_EDGE ( 'NONE', *, *, #135283, .T. ) ;
#242300 = DIRECTION ( 'NONE',  ( -0.000000000000000000, -1.000000000000000000, -5.421010862427649374E-16 ) ) ;
#242301 = AXIS2_PLACEMENT_3D ( 'NONE', #144510, #67557, #42866 ) ;
#242302 = EDGE_CURVE ( 'NONE', #168923, #122992, #113520, .T. ) ;
#242303 = ORIENTED_EDGE ( 'NONE', *, *, #215428, .F. ) ;
#242304 = CIRCLE ( 'NONE', #129867, 11.65000000000000746 ) ;
#242305 = CARTESIAN_POINT ( 'NONE',  ( -16.87304349924914604, 66.03825492205506009, -149.1340408094791599 ) ) ;
#242306 = DIRECTION ( 'NONE',  ( 0.7071067811864931718, -0.2890913453341744099, 0.6453109281989217738 ) ) ;
#242309 = EDGE_CURVE ( 'NONE', #144623, #219396, #257909, .T. ) ;
#242308 = VERTEX_POINT ( 'NONE', #213900 ) ;
#242307 = CIRCLE ( 'NONE', #88345, 0.1000000000000028644 ) ;
#242310 = CIRCLE ( 'NONE', #196522, 0.1000000000000055844 ) ;
#242311 = DIRECTION ( 'NONE',  ( 1.000000000000000000, -0.000000000000000000, -0.000000000000000000 ) ) ;
#242312 = CARTESIAN_POINT ( 'NONE',  ( 21.05000000000000071, 18.65264709638147878, -228.0117735144100379 ) ) ;
#242313 = ORIENTED_EDGE ( 'NONE', *, *, #166781, .T. ) ;
#242314 = EDGE_LOOP ( 'NONE', ( #25894, #151427 ) ) ;
#242315 = AXIS2_PLACEMENT_3D ( 'NONE', #216090, #37483, #218654 ) ;
#242316 = CARTESIAN_POINT ( 'NONE',  ( -21.14999999999999858, 76.10085836911147794, -215.2726746080137445 ) ) ;
#242317 = CARTESIAN_POINT ( 'NONE',  ( 22.84999999999999787, 4.898587196589412829E-16, -4.000000000000000000 ) ) ;
#242318 = ORIENTED_EDGE ( 'NONE', *, *, #6697, .T. ) ;
#242319 = DIRECTION ( 'NONE',  ( -0.000000000000000000, -0.8660254037844459241, -0.4999999999999873990 ) ) ;
#242320 = VERTEX_POINT ( 'NONE', #114806 ) ;
#242321 = EDGE_CURVE ( 'NONE', #207108, #142401, #124879, .T. ) ;
#242322 = DIRECTION ( 'NONE',  ( 7.304098846218134667E-16, -1.000000000000000000, 0.000000000000000000 ) ) ;
#242323 = CARTESIAN_POINT ( 'NONE',  ( 20.94999999999999929, 64.36312671090810511, -143.3448666978490849 ) ) ;
#242325 = FACE_OUTER_BOUND ( 'NONE', #41469, .T. ) ;
#242324 = FACE_OUTER_BOUND ( 'NONE', #248939, .T. ) ;
#242326 = DIRECTION ( 'NONE',  ( 0.000000000000000000, 7.109473446599835262E-15, -1.000000000000000000 ) ) ;
#242328 = EDGE_CURVE ( 'NONE', #206025, #177843, #49693, .T. ) ;
#242327 = DIRECTION ( 'NONE',  ( 0.000000000000000000, 0.6728971962616697722, 0.7397360091702875895 ) ) ;
#242329 = ORIENTED_EDGE ( 'NONE', *, *, #140464, .T. ) ;
#242330 = CARTESIAN_POINT ( 'NONE',  ( 18.41832399655381280, -9.682403266662619856, -207.6568436200278143 ) ) ;
#242331 = CIRCLE ( 'NONE', #167348, 0.09999999999999939493 ) ;
#242332 = AXIS2_PLACEMENT_3D ( 'NONE', #152337, #256469, #94885 ) ;
#242333 = AXIS2_PLACEMENT_3D ( 'NONE', #143994, #613, #102273 ) ;
#242335 = ORIENTED_EDGE ( 'NONE', *, *, #8448, .T. ) ;
#242334 = ORIENTED_EDGE ( 'NONE', *, *, #247944, .F. ) ;
#242337 = ORIENTED_EDGE ( 'NONE', *, *, #108829, .F. ) ;
#242336 = AXIS2_PLACEMENT_3D ( 'NONE', #152277, #94834, #36173 ) ;
#242338 = ORIENTED_EDGE ( 'NONE', *, *, #42281, .T. ) ;
#242339 = CARTESIAN_POINT ( 'NONE',  ( 23.14999999999999858, 64.35000000001176090, -76.53791325517833855 ) ) ;
#242340 = DIRECTION ( 'NONE',  ( 0.000000000000000000, -1.000000000000000000, 0.000000000000000000 ) ) ;
#242341 = CARTESIAN_POINT ( 'NONE',  ( 18.49999999999999289, 30.76917518201224055, -234.8152055956155380 ) ) ;
#242342 = CARTESIAN_POINT ( 'NONE',  ( -23.15000000000000213, 1.115600667400684642E-11, -134.0000000000000284 ) ) ;
#242343 = CARTESIAN_POINT ( 'NONE',  ( -21.14999999999999858, 11.65000000001115232, -167.4999999999999716 ) ) ;
#242345 = CARTESIAN_POINT ( 'NONE',  ( 20.85000000000000142, 1.115600667400684642E-11, -67.00000000000000000 ) ) ;
#242344 = FACE_OUTER_BOUND ( 'NONE', #206062, .T. ) ;
#242347 = ORIENTED_EDGE ( 'NONE', *, *, #115513, .F. ) ;
#242346 = CARTESIAN_POINT ( 'NONE',  ( 20.94999999999999574, 10.47338541492405994, -41.07865446424855094 ) ) ;
#242348 = CARTESIAN_POINT ( 'NONE',  ( 23.24999999999999645, 8.822561741677553471, -180.1499999999999773 ) ) ;
#242349 = EDGE_LOOP ( 'NONE', ( #25392, #23147, #171777, #124001 ) ) ;
#242350 = LINE ( 'NONE', #162842, #13422 ) ;
#242351 = ORIENTED_EDGE ( 'NONE', *, *, #183439, .T. ) ;
#242352 = ORIENTED_EDGE ( 'NONE', *, *, #163545, .T. ) ;
#242353 = SPHERICAL_SURFACE ( 'NONE', #50292, 0.1000000000000000056 ) ;
#242354 = CARTESIAN_POINT ( 'NONE',  ( 23.14999999999999858, 11.65000000000000746, -26.48519422934606027 ) ) ;
#242355 = DIRECTION ( 'NONE',  ( 1.000000000000000000, 0.000000000000000000, 0.000000000000000000 ) ) ;
#242356 = DIRECTION ( 'NONE',  ( 0.000000000000000000, 0.9126074666063545004, 0.4088369013363783999 ) ) ;
#242357 = CIRCLE ( 'NONE', #159009, 0.09999999999999939493 ) ;
#242358 = CARTESIAN_POINT ( 'NONE',  ( -21.65000000000000213, 68.75000000001263345, -194.2731074845244166 ) ) ;
#242359 = EDGE_LOOP ( 'NONE', ( #44019, #202982, #131599, #219179, #149581 ) ) ;
#242360 = VERTEX_POINT ( 'NONE', #169689 ) ;
#242361 = CARTESIAN_POINT ( 'NONE',  ( -18.59999999999999787, -1.851617760457748618, -212.6031897196036198 ) ) ;
#242362 = VERTEX_POINT ( 'NONE', #249190 ) ;
#242363 = CARTESIAN_POINT ( 'NONE',  ( 12.25000000000000000, 48.12247445990688277, -234.1702647910923361 ) ) ;
#242364 = DIRECTION ( 'NONE',  ( -0.000000000000000000, -0.000000000000000000, -1.000000000000000000 ) ) ;
#242365 = DIRECTION ( 'NONE',  ( 0.000000000000000000, 6.982962677686266711E-15, -1.000000000000000000 ) ) ;
#242366 = DIRECTION ( 'NONE',  ( 0.000000000000000000, -0.9770955615653315052, -0.2128009952263603954 ) ) ;
#242367 = DIRECTION ( 'NONE',  ( 1.000000000000000000, -0.000000000000000000, 0.000000000000000000 ) ) ;
#242368 = CYLINDRICAL_SURFACE ( 'NONE', #162694, 0.09999999999999939493 ) ;
#242369 = DIRECTION ( 'NONE',  ( 0.000000000000000000, 0.000000000000000000, 1.000000000000000000 ) ) ;
#242370 = DIRECTION ( 'NONE',  ( -1.000000000000000000, 0.000000000000000000, 0.000000000000000000 ) ) ;
#242371 = CARTESIAN_POINT ( 'NONE',  ( 18.49999999999716849, 65.55993210786937198, -178.7559897356427712 ) ) ;
#242373 = EDGE_CURVE ( 'NONE', #19158, #45529, #199736, .T. ) ;
#242372 = CARTESIAN_POINT ( 'NONE',  ( 18.79999999999999716, 11.75000000000000000, 16.39999999999999858 ) ) ;
#242374 = CARTESIAN_POINT ( 'NONE',  ( -17.80356949363865837, 10.87673139701229630, -56.71307302422879815 ) ) ;
#242376 = VERTEX_POINT ( 'NONE', #176091 ) ;
#242375 = AXIS2_PLACEMENT_3D ( 'NONE', #147773, #227292, #128206 ) ;
#242377 = FACE_OUTER_BOUND ( 'NONE', #6618, .T. ) ;
#242378 = EDGE_CURVE ( 'NONE', #144454, #155114, #12466, .T. ) ;
#242379 = VERTEX_POINT ( 'NONE', #255541 ) ;
#242380 = APPLICATION_CONTEXT ( 'automotive_design' ) ;
#242381 = CARTESIAN_POINT ( 'NONE',  ( -20.64999999999999858, 1.115600667400684642E-11, -154.6250000000000284 ) ) ;
#242382 = CARTESIAN_POINT ( 'NONE',  ( -22.50000000000000000, 26.02743912001966464, -254.3139371321002216 ) ) ;
#242384 = EDGE_CURVE ( 'NONE', #239387, #253858, #178906, .T. ) ;
#242383 = LINE ( 'NONE', #127585, #52275 ) ;
#242385 = EDGE_CURVE ( 'NONE', #176891, #125880, #79506, .T. ) ;
#242386 = ORIENTED_EDGE ( 'NONE', *, *, #157124, .T. ) ;
#242387 = CARTESIAN_POINT ( 'NONE',  ( 22.48970261584622321, 11.65000000001115588, -100.4446305117826199 ) ) ;
#242388 = CARTESIAN_POINT ( 'NONE',  ( 23.15000000000000213, -9.000000000000001776, -9.893969122652443104 ) ) ;
#242389 = DIRECTION ( 'NONE',  ( 1.000000000000000000, 0.000000000000000000, 0.000000000000000000 ) ) ;
#242390 = PLANE ( 'NONE',  #179595 ) ;
#242391 = VECTOR ( 'NONE', #243681, 1000.000000000000000 ) ;
#242392 = DIRECTION ( 'NONE',  ( -0.000000000000000000, 6.982962677686266711E-15, -1.000000000000000000 ) ) ;
#242394 = CARTESIAN_POINT ( 'NONE',  ( 13.99999999999999822, 9.850000000011137402, -83.75000000000004263 ) ) ;
#242393 = AXIS2_PLACEMENT_3D ( 'NONE', #168757, #94289, #173888 ) ;
#242395 = ORIENTED_EDGE ( 'NONE', *, *, #7344, .T. ) ;
#242396 = CARTESIAN_POINT ( 'NONE',  ( 22.39999999999999503, 68.20922040163875977, -136.5231074845243313 ) ) ;
#242398 = ORIENTED_EDGE ( 'NONE', *, *, #168060, .F. ) ;
#242397 = DIRECTION ( 'NONE',  ( 0.000000000000000000, 0.8660254037844384856, -0.5000000000000003331 ) ) ;
#242399 = CARTESIAN_POINT ( 'NONE',  ( 22.50927854361889402, -0.1008580735143376206, -122.2504328739731108 ) ) ;
#242400 = EDGE_CURVE ( 'NONE', #151632, #47244, #160378, .T. ) ;
#242401 = DIRECTION ( 'NONE',  ( 0.000000000000000000, 0.000000000000000000, -1.000000000000000000 ) ) ;
#242402 = SURFACE_STYLE_USAGE ( .BOTH. , #162906 ) ;
#242403 = ORIENTED_EDGE ( 'NONE', *, *, #99950, .T. ) ;
#242404 = CARTESIAN_POINT ( 'NONE',  ( -21.45000000000000284, 7.708578643773852157, -54.75000000000000000 ) ) ;
#242405 = CONTEXT_DEPENDENT_SHAPE_REPRESENTATION ( #90813, #116200 ) ;
#242406 = CARTESIAN_POINT ( 'NONE',  ( 20.94999999999999929, 7.120270961697594103, -37.15956304183931991 ) ) ;
#242407 = VECTOR ( 'NONE', #231715, 1000.000000000000000 ) ;
#242408 = ORIENTED_EDGE ( 'NONE', *, *, #15294, .F. ) ;
#242409 = DIRECTION ( 'NONE',  ( 1.000000000000000000, -0.000000000000000000, -0.000000000000000000 ) ) ;
#242410 = LINE ( 'NONE', #221546, #146670 ) ;
#242411 =( NAMED_UNIT ( * ) SI_UNIT ( $, .STERADIAN. ) SOLID_ANGLE_UNIT ( ) );
#242412 = ADVANCED_FACE ( 'NONE', ( #56084 ), #29058, .T. ) ;
#242413 = EDGE_LOOP ( 'NONE', ( #84386, #255398, #137551, #111198 ) ) ;
#242414 = EDGE_LOOP ( 'NONE', ( #99868, #240358, #93706, #241825 ) ) ;
#242415 = CARTESIAN_POINT ( 'NONE',  ( -18.79999999999999716, -1.467286812112899463, 28.00000000000000000 ) ) ;
#242416 = DIRECTION ( 'NONE',  ( -1.000000000000000000, 0.000000000000000000, -0.000000000000000000 ) ) ;
#242417 = DIRECTION ( 'NONE',  ( 0.000000000000000000, -6.938893903907222067E-15, 1.000000000000000000 ) ) ;
#242418 = CARTESIAN_POINT ( 'NONE',  ( -16.87331047859649757, 9.950000000011138823, -154.8500000000000227 ) ) ;
#242420 = FACE_OUTER_BOUND ( 'NONE', #37388, .T. ) ;
#242419 = AXIS2_PLACEMENT_3D ( 'NONE', #29905, #246362, #32483 ) ;
#242421 = CIRCLE ( 'NONE', #84151, 0.09999999999998898659 ) ;
#242422 = CARTESIAN_POINT ( 'NONE',  ( -20.94999999999999929, 47.92640890138473253, -246.4059919526569900 ) ) ;
#242423 = EDGE_CURVE ( 'NONE', #242248, #39025, #239897, .T. ) ;
#242426 = DIRECTION ( 'NONE',  ( 0.000000000000000000, -1.000000000000000000, -6.982962677686265922E-15 ) ) ;
#242425 = AXIS2_PLACEMENT_3D ( 'NONE', #121565, #143652, #1564 ) ;
#242424 = DIRECTION ( 'NONE',  ( 2.827886303505249259E-16, -0.8660254037844411501, -0.4999999999999956701 ) ) ;
#242427 = CARTESIAN_POINT ( 'NONE',  ( 20.12500000000000000, 40.07562767317620711, -237.3368484665046765 ) ) ;
#242428 = CARTESIAN_POINT ( 'NONE',  ( -20.64999999999999858, 5.159242054424403534, -213.4109969955686665 ) ) ;
#242429 = DIRECTION ( 'NONE',  ( 0.000000000000000000, 0.000000000000000000, -1.000000000000000000 ) ) ;
#242430 = CARTESIAN_POINT ( 'NONE',  ( 20.95265033839679347, 18.76182816757560445, -228.0387018287258911 ) ) ;
#242431 = VERTEX_POINT ( 'NONE', #99060 ) ;
#242432 = ORIENTED_EDGE ( 'NONE', *, *, #142084, .F. ) ;
#242433 = DIRECTION ( 'NONE',  ( 0.000000000000000000, -1.000000000000000000, 0.000000000000000000 ) ) ;
#242434 = DIRECTION ( 'NONE',  ( -0.000000000000000000, 0.2617529984165031243, 0.9651348961777157509 ) ) ;
#242436 = DIRECTION ( 'NONE',  ( 0.000000000000000000, 0.2128009952263596460, -0.9770955615653317272 ) ) ;
#242435 = CARTESIAN_POINT ( 'NONE',  ( -18.50000000000000000, 68.97833521811159585, -65.88954208262707368 ) ) ;
#242437 = CARTESIAN_POINT ( 'NONE',  ( -23.25000000000000000, 67.85909929089923764, -227.8797997985275856 ) ) ;
#242438 = FACE_OUTER_BOUND ( 'NONE', #129044, .T. ) ;
#242439 = CARTESIAN_POINT ( 'NONE',  ( -18.40000000000000213, 11.47316190337364183, -91.17405393319209850 ) ) ;
#242440 = CARTESIAN_POINT ( 'NONE',  ( -21.05000000000000071, 69.09936979046463534, -247.6075824278584889 ) ) ;
#242442 = ORIENTED_EDGE ( 'NONE', *, *, #61257, .F. ) ;
#242441 = CIRCLE ( 'NONE', #221583, 0.09999999999999939493 ) ;
#242443 = CARTESIAN_POINT ( 'NONE',  ( -23.25000000000000355, 5.650000000011139001, -42.75000000000000000 ) ) ;
#242444 = EDGE_LOOP ( 'NONE', ( #248868, #174771, #147479, #76688 ) ) ;
#242445 = DIRECTION ( 'NONE',  ( -0.000000000000000000, 1.000000000000000000, -0.000000000000000000 ) ) ;
#242446 = AXIS2_PLACEMENT_3D ( 'NONE', #178840, #79680, #159259 ) ;
#242447 = CARTESIAN_POINT ( 'NONE',  ( 18.50000000000000355, 85.42107434499949647, -29.19863542509363441 ) ) ;
#242448 = EDGE_CURVE ( 'NONE', #166449, #15753, #126238, .T. ) ;
#242449 = EDGE_CURVE ( 'NONE', #129511, #33930, #18271, .T. ) ;
#242450 = ORIENTED_EDGE ( 'NONE', *, *, #154914, .F. ) ;
#242451 = FACE_OUTER_BOUND ( 'NONE', #131574, .T. ) ;
#242452 = AXIS2_PLACEMENT_3D ( 'NONE', #75530, #41544, #204097 ) ;
#242453 = ORIENTED_EDGE ( 'NONE', *, *, #99344, .F. ) ;
#242454 = EDGE_CURVE ( 'NONE', #138601, #106738, #62340, .T. ) ;
#242456 = EDGE_CURVE ( 'NONE', #53585, #3049, #241419, .T. ) ;
#242455 = CARTESIAN_POINT ( 'NONE',  ( 22.39999999999999503, 0.2612980822699583205, -230.0539506776466681 ) ) ;
#242457 = CARTESIAN_POINT ( 'NONE',  ( -22.47071067811865319, 68.27992525551358938, -69.62219993922697370 ) ) ;
#242459 = VECTOR ( 'NONE', #53160, 1000.000000000000000 ) ;
#242458 = DIRECTION ( 'NONE',  ( -2.252264143451594314E-15, -0.1298341882520124002, -0.9915357197604841577 ) ) ;
#242460 = PLANE ( 'NONE',  #241593 ) ;
#242461 = CARTESIAN_POINT ( 'NONE',  ( -23.15000000000000213, 64.35000000001218723, -143.5379132551784096 ) ) ;
#242462 = CARTESIAN_POINT ( 'NONE',  ( -16.84419801905646352, 66.05000000001257376, -182.6925973307465085 ) ) ;
#242463 = CIRCLE ( 'NONE', #46632, 0.09999999999999939493 ) ;
#242464 = EDGE_CURVE ( 'NONE', #64483, #45900, #125074, .T. ) ;
#242465 = FACE_OUTER_BOUND ( 'NONE', #85642, .T. ) ;
#242466 = TOROIDAL_SURFACE ( 'NONE', #104884, 0.2000000000000000111, 0.1000000000000000056 ) ;
#242468 = EDGE_LOOP ( 'NONE', ( #94268, #105309 ) ) ;
#242467 = CARTESIAN_POINT ( 'NONE',  ( 20.97217846901852312, 67.12455827530239105, -128.0218798005871577 ) ) ;
#242470 = CARTESIAN_POINT ( 'NONE',  ( 18.59999999999999076, 10.92199707682457088, -220.3694341645321515 ) ) ;
#242469 = PLANE ( 'NONE',  #66204 ) ;
#242471 = ORIENTED_EDGE ( 'NONE', *, *, #181547, .T. ) ;
#242473 = ORIENTED_EDGE ( 'NONE', *, *, #27708, .T. ) ;
#242472 = FACE_OUTER_BOUND ( 'NONE', #223583, .T. ) ;
#242474 = EDGE_CURVE ( 'NONE', #121863, #138951, #20856, .T. ) ;
#242475 = ORIENTED_EDGE ( 'NONE', *, *, #5209, .T. ) ;
#242476 = CARTESIAN_POINT ( 'NONE',  ( -20.94999999999999929, 7.783179459866052419, -245.3643104511423303 ) ) ;
#242479 = ADVANCED_FACE ( 'NONE', ( #254293 ), #245686, .F. ) ;
#242478 = EDGE_CURVE ( 'NONE', #23626, #88201, #135637, .T. ) ;
#242477 = AXIS2_PLACEMENT_3D ( 'NONE', #161619, #220298, #157791 ) ;
#242480 = CARTESIAN_POINT ( 'NONE',  ( 20.94999999999999574, 1.849084418638171856, -112.1560105214471577 ) ) ;
#242481 = DIRECTION ( 'NONE',  ( 1.000000000000000000, 0.000000000000000000, 0.000000000000000000 ) ) ;
#242482 = ORIENTED_EDGE ( 'NONE', *, *, #29356, .T. ) ;
#242483 = FACE_OUTER_BOUND ( 'NONE', #227758, .T. ) ;
#242484 = CARTESIAN_POINT ( 'NONE',  ( -20.94999999999999929, -11.48912529306489994, -97.40000000000004832 ) ) ;
#242485 = CARTESIAN_POINT ( 'NONE',  ( 22.50000000000000000, 1.115600667400684642E-11, -67.00000000000004263 ) ) ;
#242486 = ORIENTED_EDGE ( 'NONE', *, *, #85271, .F. ) ;
#242487 = CIRCLE ( 'NONE', #59284, 0.09999999999999543976 ) ;
#242488 = CARTESIAN_POINT ( 'NONE',  ( -20.64999999999999858, 76.00000000001195133, -103.0231074845243171 ) ) ;
#242489 = VECTOR ( 'NONE', #126617, 1000.000000000000000 ) ;
#242490 = EDGE_CURVE ( 'NONE', #99842, #90507, #174828, .T. ) ;
#242491 = CARTESIAN_POINT ( 'NONE',  ( 21.12757541349815682, 69.52661942876069645, -136.5282687003340811 ) ) ;
#242492 = CIRCLE ( 'NONE', #125962, 0.09999999999999939493 ) ;
#242493 = AXIS2_PLACEMENT_3D ( 'NONE', #161524, #97653, #101482 ) ;
#242494 = VERTEX_POINT ( 'NONE', #140786 ) ;
#242495 = ORIENTED_EDGE ( 'NONE', *, *, #153670, .F. ) ;
#242496 = FACE_OUTER_BOUND ( 'NONE', #103336, .T. ) ;
#242497 = ADVANCED_FACE ( 'NONE', ( #234750 ), #183325, .F. ) ;
#242499 = ADVANCED_FACE ( 'NONE', ( #157829 ), #96498, .F. ) ;
#242498 = TOROIDAL_SURFACE ( 'NONE', #46667, 0.2000000000000000111, 0.1000000000000000056 ) ;
#242500 = ORIENTED_EDGE ( 'NONE', *, *, #45244, .T. ) ;
#242501 = DIRECTION ( 'NONE',  ( 1.000000000000000000, 0.000000000000000000, 0.000000000000000000 ) ) ;
#242502 = ORIENTED_EDGE ( 'NONE', *, *, #80957, .T. ) ;
#242503 = DIRECTION ( 'NONE',  ( 0.000000000000000000, 0.9126074666063769270, 0.4088369013363283844 ) ) ;
#242504 = AXIS2_PLACEMENT_3D ( 'NONE', #225063, #46439, #7322 ) ;
#242505 = EDGE_CURVE ( 'NONE', #215603, #175396, #122520, .T. ) ;
#242506 = DIRECTION ( 'NONE',  ( 0.000000000000000000, 0.000000000000000000, -1.000000000000000000 ) ) ;
#242507 = DIRECTION ( 'NONE',  ( -1.000000000000000000, 0.000000000000000000, 0.000000000000000000 ) ) ;
#242508 = AXIS2_PLACEMENT_3D ( 'NONE', #41252, #141597, #42494 ) ;
#242509 = CARTESIAN_POINT ( 'NONE',  ( -21.08884785362073089, 30.83694912164556357, -252.1047855145109224 ) ) ;
#242510 = CARTESIAN_POINT ( 'NONE',  ( 23.14999999999999503, 66.44571689960341132, -213.7280413126916017 ) ) ;
#242511 = ORIENTED_EDGE ( 'NONE', *, *, #178167, .T. ) ;
#242512 = EDGE_CURVE ( 'NONE', #239334, #61048, #203331, .T. ) ;
#242513 = DIRECTION ( 'NONE',  ( -1.000000000000000000, -0.000000000000000000, -0.000000000000000000 ) ) ;
#242514 = EDGE_CURVE ( 'NONE', #84354, #67400, #66627, .T. ) ;
#242515 = CARTESIAN_POINT ( 'NONE',  ( -20.15000000000000568, 9.291421356248463326, -179.8499999999999943 ) ) ;
#242516 = CARTESIAN_POINT ( 'NONE',  ( -18.59999999999999787, 6.846123162363745074, -70.73772626684986164 ) ) ;
#242517 = ORIENTED_EDGE ( 'NONE', *, *, #25139, .F. ) ;
#242519 = DIRECTION ( 'NONE',  ( 0.000000000000000000, -0.9875055080513754913, 0.1575844902526733482 ) ) ;
#242518 = DIRECTION ( 'NONE',  ( -0.000000000000000000, 0.2617529984165031243, 0.9651348961777157509 ) ) ;
#242520 = CIRCLE ( 'NONE', #130080, 12.97499999999999964 ) ;
#242521 = VERTEX_POINT ( 'NONE', #183767 ) ;
#242523 = VERTEX_POINT ( 'NONE', #62536 ) ;
#242522 = DIRECTION ( 'NONE',  ( -0.000000000000000000, -0.000000000000000000, -1.000000000000000000 ) ) ;
#242524 = AXIS2_PLACEMENT_3D ( 'NONE', #216813, #38207, #117721 ) ;
#242525 = ORIENTED_EDGE ( 'NONE', *, *, #106905, .T. ) ;
#242526 = CARTESIAN_POINT ( 'NONE',  ( -17.11825945287481332, 66.05000000001182059, -82.27310748452437394 ) ) ;
#242527 = CIRCLE ( 'NONE', #109422, 4.900000000000000355 ) ;
#242528 = CARTESIAN_POINT ( 'NONE',  ( 20.94999999999999929, 72.02722222756959525, -225.1832529173024398 ) ) ;
#242529 = LINE ( 'NONE', #172025, #70 ) ;
#242530 = ORIENTED_EDGE ( 'NONE', *, *, #252434, .T. ) ;
#242531 = CARTESIAN_POINT ( 'NONE',  ( -18.50000000000000000, 85.40000000001167280, -62.60844914155458696 ) ) ;
#242532 = FACE_OUTER_BOUND ( 'NONE', #253174, .T. ) ;
#242534 = CARTESIAN_POINT ( 'NONE',  ( 20.94999999999999929, 88.41227409416113403, -39.02310748452423894 ) ) ;
#242533 = CARTESIAN_POINT ( 'NONE',  ( -21.33487959338958362, 6.725558151922345296, -167.4999999999999716 ) ) ;
#242536 = VERTEX_POINT ( 'NONE', #25983 ) ;
#242535 = DIRECTION ( 'NONE',  ( -1.000000000000000000, -2.885090398161910739E-16, -6.283419270304611573E-17 ) ) ;
#242537 = ORIENTED_EDGE ( 'NONE', *, *, #61753, .T. ) ;
#242538 = CARTESIAN_POINT ( 'NONE',  ( -20.94999999999999929, 1.115600667400684642E-11, -200.9999999999999432 ) ) ;
#242539 = AXIS2_PLACEMENT_3D ( 'NONE', #169279, #87117, #208386 ) ;
#242540 = DIRECTION ( 'NONE',  ( 0.000000000000000000, 0.9770955615653312831, 0.2128009952263620053 ) ) ;
#242541 = FACE_OUTER_BOUND ( 'NONE', #79840, .T. ) ;
#242542 = ORIENTED_EDGE ( 'NONE', *, *, #254801, .T. ) ;
#242543 = CARTESIAN_POINT ( 'NONE',  ( 23.14999999999999858, 6.703231349641842307, -231.7785101893094577 ) ) ;
#242544 = VERTEX_POINT ( 'NONE', #102917 ) ;
#242545 = DIRECTION ( 'NONE',  ( -1.000000000000000000, 0.000000000000000000, 0.000000000000000000 ) ) ;
#242546 = CIRCLE ( 'NONE', #188555, 11.70000000000000284 ) ;
#242547 = CARTESIAN_POINT ( 'NONE',  ( -22.49806830649814415, 64.35011034517329165, -170.1005718008499343 ) ) ;
#242548 = CARTESIAN_POINT ( 'NONE',  ( 20.84999999999999787, 64.25000000001219291, -143.4422547304831710 ) ) ;
#242549 = ORIENTED_EDGE ( 'NONE', *, *, #169552, .T. ) ;
#242550 = FACE_OUTER_BOUND ( 'NONE', #190428, .T. ) ;
#242551 = ADVANCED_FACE ( 'NONE', ( #145905 ), #144618, .F. ) ;
#242553 = ADVANCED_FACE ( 'NONE', ( #105471 ), #63822, .F. ) ;
#242552 = CARTESIAN_POINT ( 'NONE',  ( 21.00000000000000000, 66.25000000001260503, -191.2731074845244166 ) ) ;
#242555 = VERTEX_POINT ( 'NONE', #222877 ) ;
#242554 = VECTOR ( 'NONE', #101588, 1000.000000000000000 ) ;
#242556 = ORIENTED_EDGE ( 'NONE', *, *, #22333, .F. ) ;
#242557 = ORIENTED_EDGE ( 'NONE', *, *, #131343, .T. ) ;
#242558 = EDGE_CURVE ( 'NONE', #165690, #201109, #174995, .T. ) ;
#242559 = LINE ( 'NONE', #221696, #129039 ) ;
#242560 = ORIENTED_EDGE ( 'NONE', *, *, #202681, .F. ) ;
#242563 = EDGE_CURVE ( 'NONE', #201392, #192753, #108325, .T. ) ;
#242562 = ORIENTED_EDGE ( 'NONE', *, *, #139344, .T. ) ;
#242561 = DIRECTION ( 'NONE',  ( 1.000000000000000000, -0.000000000000000000, 0.000000000000000000 ) ) ;
#242564 = EDGE_LOOP ( 'NONE', ( #160115, #120987 ) ) ;
#242567 = EDGE_LOOP ( 'NONE', ( #19144, #196523, #161544, #165820 ) ) ;
#242566 = ORIENTED_EDGE ( 'NONE', *, *, #52196, .T. ) ;
#242565 = CARTESIAN_POINT ( 'NONE',  ( -23.25000000000000000, -9.000000000000003553, -9.893969122652444881 ) ) ;
#242568 = AXIS2_PLACEMENT_3D ( 'NONE', #88426, #109287, #188839 ) ;
#242569 = VERTEX_POINT ( 'NONE', #104207 ) ;
#242570 = DIRECTION ( 'NONE',  ( -1.000000000000000000, 0.000000000000000000, 0.000000000000000000 ) ) ;
#242571 = VECTOR ( 'NONE', #147550, 1000.000000000000000 ) ;
#242572 = EDGE_CURVE ( 'NONE', #232077, #248304, #220732, .T. ) ;
#242573 = CARTESIAN_POINT ( 'NONE',  ( 21.05000000000000071, 87.65000000001192859, -106.0231074845242176 ) ) ;
#242574 = ORIENTED_EDGE ( 'NONE', *, *, #187468, .T. ) ;
#242575 = VECTOR ( 'NONE', #175660, 1000.000000000000000 ) ;
#242576 = CARTESIAN_POINT ( 'NONE',  ( 21.05000000000000071, 1.115623935689868526E-11, -165.6000000000000227 ) ) ;
#242578 = ORIENTED_EDGE ( 'NONE', *, *, #222460, .T. ) ;
#242577 = CARTESIAN_POINT ( 'NONE',  ( 20.94999999999999929, 71.00000000001253397, -182.4283735034374843 ) ) ;
#242579 = FACE_OUTER_BOUND ( 'NONE', #59745, .T. ) ;
#242581 = VERTEX_POINT ( 'NONE', #164214 ) ;
#242580 = CARTESIAN_POINT ( 'NONE',  ( -21.64999999999999858, 9.350000000011133849, -180.1499999999999773 ) ) ;
#242582 = ORIENTED_EDGE ( 'NONE', *, *, #412, .F. ) ;
#242583 = VECTOR ( 'NONE', #167592, 1000.000000000000000 ) ;
#242584 = AXIS2_PLACEMENT_3D ( 'NONE', #69067, #88587, #191595 ) ;
#242585 = VERTEX_POINT ( 'NONE', #106780 ) ;
#242586 = ORIENTED_EDGE ( 'NONE', *, *, #178084, .F. ) ;
#242587 = FACE_OUTER_BOUND ( 'NONE', #136367, .T. ) ;
#242588 = CARTESIAN_POINT ( 'NONE',  ( -21.05000000000000071, -0.08579911626282435422, -161.0860211185119795 ) ) ;
#242589 = EDGE_CURVE ( 'NONE', #12028, #2285, #16743, .T. ) ;
#242591 = ORIENTED_EDGE ( 'NONE', *, *, #136590, .F. ) ;
#242590 = ORIENTED_EDGE ( 'NONE', *, *, #217706, .T. ) ;
#242592 = VERTEX_POINT ( 'NONE', #5087 ) ;
#242593 = FACE_OUTER_BOUND ( 'NONE', #100632, .T. ) ;
#242594 = ORIENTED_EDGE ( 'NONE', *, *, #102799, .F. ) ;
#242595 = ORIENTED_EDGE ( 'NONE', *, *, #13110, .F. ) ;
#242597 = DIRECTION ( 'NONE',  ( 4.026293107431335996E-15, -0.8700118002898359348, 0.4930308989875165082 ) ) ;
#242596 = VECTOR ( 'NONE', #27359, 1000.000000000000000 ) ;
#242599 = VERTEX_POINT ( 'NONE', #125086 ) ;
#242598 = CARTESIAN_POINT ( 'NONE',  ( -22.57320508075687115, 55.89093952297024970, -232.7795287750844579 ) ) ;
#242600 = CARTESIAN_POINT ( 'NONE',  ( -20.54999999999999716, 6.353932154659650777, -220.7762181625030848 ) ) ;
#242602 = SPHERICAL_SURFACE ( 'NONE', #106812, 0.1000000000000000056 ) ;
#242601 = CARTESIAN_POINT ( 'NONE',  ( -21.44999999999999929, 7.150000000011155876, -146.2500000000000284 ) ) ;
#242603 = ADVANCED_FACE ( 'NONE', ( #84614 ), #46799, .F. ) ;
#242604 = ORIENTED_EDGE ( 'NONE', *, *, #65571, .F. ) ;
#242605 = CIRCLE ( 'NONE', #126068, 0.09999999999999158173 ) ;
#242606 = CIRCLE ( 'NONE', #113623, 0.1999999999999945155 ) ;
#242607 = VECTOR ( 'NONE', #88802, 1000.000000000000114 ) ;
#242608 = ADVANCED_FACE ( 'NONE', ( #242438 ), #87208, .T. ) ;
#242610 = ORIENTED_EDGE ( 'NONE', *, *, #110961, .T. ) ;
#242609 = VERTEX_POINT ( 'NONE', #143346 ) ;
#242611 = VECTOR ( 'NONE', #75562, 1000.000000000000000 ) ;
#242612 = DIRECTION ( 'NONE',  ( 1.000000000000000000, 0.000000000000000000, 0.000000000000000000 ) ) ;
#242613 = DIRECTION ( 'NONE',  ( -1.000000000000000000, -0.000000000000000000, -0.000000000000000000 ) ) ;
#242614 = ORIENTED_EDGE ( 'NONE', *, *, #93950, .T. ) ;
#242615 = EDGE_CURVE ( 'NONE', #73178, #136488, #158409, .T. ) ;
#242616 = DIRECTION ( 'NONE',  ( -1.020425574104004196E-15, 6.982962677686266711E-15, -1.000000000000000000 ) ) ;
#242617 = EDGE_LOOP ( 'NONE', ( #247670, #104827, #2136 ) ) ;
#242618 = ORIENTED_EDGE ( 'NONE', *, *, #205128, .T. ) ;
#242619 = DIRECTION ( 'NONE',  ( 0.5932847527679309119, -0.7865547670005531566, -0.1713032417725958989 ) ) ;
#242621 = ADVANCED_FACE ( 'NONE', ( #200760 ), #233235, .F. ) ;
#242620 = ORIENTED_EDGE ( 'NONE', *, *, #193395, .F. ) ;
#242622 = DIRECTION ( 'NONE',  ( 5.421010862427554711E-16, -1.000000000000000000, -3.252606517456533024E-15 ) ) ;
#242623 = CARTESIAN_POINT ( 'NONE',  ( 20.94999999999999929, -1.362429037193307435, -41.38888124792119783 ) ) ;
#242624 = ORIENTED_EDGE ( 'NONE', *, *, #59276, .F. ) ;
#242625 = ADVANCED_FACE ( 'NONE', ( #161658 ), #62526, .F. ) ;
#242626 = CARTESIAN_POINT ( 'NONE',  ( 20.00000000000000355, 64.25000000001220712, -145.3731074845244393 ) ) ;
#242627 = SPHERICAL_SURFACE ( 'NONE', #103746, 0.1000000000000000056 ) ;
#242629 = DIRECTION ( 'NONE',  ( -1.000000000000000000, 0.000000000000000000, 0.000000000000000000 ) ) ;
#242628 = CARTESIAN_POINT ( 'NONE',  ( 20.95000000000000284, 64.40000000001175806, -76.45131071479988805 ) ) ;
#242630 = DIRECTION ( 'NONE',  ( 0.000000000000000000, -0.9915357197604971473, 0.1298341882519111479 ) ) ;
#242631 = CARTESIAN_POINT ( 'NONE',  ( 21.12769345151713196, 65.28071232307172522, -157.7756271383269393 ) ) ;
#242632 = DIRECTION ( 'NONE',  ( 0.000000000000000000, 0.000000000000000000, -1.000000000000000000 ) ) ;
#242634 = ADVANCED_FACE ( 'NONE', ( #152366 ), #71544, .F. ) ;
#242633 = DIRECTION ( 'NONE',  ( 0.000000000000000000, -0.9126074666063770380, -0.4088369013363281068 ) ) ;
#242635 = CARTESIAN_POINT ( 'NONE',  ( -20.94999999999999929, 0.3882413827466408840, -209.1776850584169551 ) ) ;
#242636 = AXIS2_PLACEMENT_3D ( 'NONE', #16101, #173913, #249564 ) ;
#242637 = ORIENTED_EDGE ( 'NONE', *, *, #203043, .T. ) ;
#242638 = TOROIDAL_SURFACE ( 'NONE', #159278, 11.65000000000000036, 0.1000000000000000056 ) ;
#242640 = ORIENTED_EDGE ( 'NONE', *, *, #100367, .T. ) ;
#242639 = ORIENTED_EDGE ( 'NONE', *, *, #245461, .T. ) ;
#242641 = ORIENTED_EDGE ( 'NONE', *, *, #47843, .F. ) ;
#242643 = ADVANCED_FACE ( 'NONE', ( #32427 ), #29250, .F. ) ;
#242642 = CARTESIAN_POINT ( 'NONE',  ( -21.05000000000000071, 4.252251777740764460, -211.8999245327126744 ) ) ;
#242644 = CIRCLE ( 'NONE', #130203, 0.09999999999999996392 ) ;
#242645 = LINE ( 'NONE', #64021, #128567 ) ;
#242647 = CARTESIAN_POINT ( 'NONE',  ( -17.05016517655648656, 9.950000000011138823, -146.6726979959938433 ) ) ;
#242646 = CARTESIAN_POINT ( 'NONE',  ( -20.00857864376270001, 9.150000000000002132, -21.15000000000000213 ) ) ;
#242648 = DIRECTION ( 'NONE',  ( -1.000000000000000000, -0.000000000000000000, -0.000000000000000000 ) ) ;
#242649 = ORIENTED_EDGE ( 'NONE', *, *, #187026, .T. ) ;
#242650 = AXIS2_PLACEMENT_3D ( 'NONE', #18849, #239187, #157102 ) ;
#242651 = DIRECTION ( 'NONE',  ( 0.000000000000000000, 0.000000000000000000, 1.000000000000000000 ) ) ;
#242652 = FACE_OUTER_BOUND ( 'NONE', #206277, .T. ) ;
#242653 = CIRCLE ( 'NONE', #255057, 0.09999999999999939493 ) ;
#242654 = CARTESIAN_POINT ( 'NONE',  ( -16.97048326478264713, 66.05000000001187743, -89.88200060439721994 ) ) ;
#242655 = CIRCLE ( 'NONE', #167675, 4.299999999999957190 ) ;
#242656 = CIRCLE ( 'NONE', #42746, 0.09999999999999939493 ) ;
#242657 = CARTESIAN_POINT ( 'NONE',  ( -16.94445028196807002, 9.992063609708893068, -87.89266982158160602 ) ) ;
#242658 = ORIENTED_EDGE ( 'NONE', *, *, #122314, .F. ) ;
#242659 = AXIS2_PLACEMENT_3D ( 'NONE', #219966, #20507, #17905 ) ;
#242660 = CARTESIAN_POINT ( 'NONE',  ( 18.41356215285960829, -9.500000000000023093, -7.032069396699602848 ) ) ;
#242661 = AXIS2_PLACEMENT_3D ( 'NONE', #69028, #208537, #205947 ) ;
#242662 = CARTESIAN_POINT ( 'NONE',  ( 13.99999999999999822, 66.15000000001204228, -119.7731074845243739 ) ) ;
#242663 = ORIENTED_EDGE ( 'NONE', *, *, #81671, .F. ) ;
#242664 = LINE ( 'NONE', #203549, #120583 ) ;
#242665 = CARTESIAN_POINT ( 'NONE',  ( 23.14999999999999858, -11.74999999998883560, -122.2500000000000284 ) ) ;
#242666 = DIRECTION ( 'NONE',  ( 0.000000000000000000, 0.000000000000000000, -1.000000000000000000 ) ) ;
#242667 = CARTESIAN_POINT ( 'NONE',  ( 18.59999999999999076, 62.49201502323811752, -208.8221019049098857 ) ) ;
#242668 = DIRECTION ( 'NONE',  ( 1.000000000000000000, 0.000000000000000000, 0.000000000000000000 ) ) ;
#242670 = VECTOR ( 'NONE', #6963, 1000.000000000000227 ) ;
#242669 = FACE_OUTER_BOUND ( 'NONE', #240566, .T. ) ;
#242671 = ORIENTED_EDGE ( 'NONE', *, *, #244249, .F. ) ;
#242672 = DIRECTION ( 'NONE',  ( 0.000000000000000000, 0.000000000000000000, -1.000000000000000000 ) ) ;
#242673 = DIRECTION ( 'NONE',  ( 1.000000000000000000, 0.000000000000000000, 0.000000000000000000 ) ) ;
#242674 = CARTESIAN_POINT ( 'NONE',  ( 20.94999999999999929, 71.14953271029267512, -157.9888400755227167 ) ) ;
#242675 = CIRCLE ( 'NONE', #196879, 0.1000000000000024342 ) ;
#242676 = CYLINDRICAL_SURFACE ( 'NONE', #257737, 0.1000000000000064587 ) ;
#242677 =( NAMED_UNIT ( * ) SI_UNIT ( $, .STERADIAN. ) SOLID_ANGLE_UNIT ( ) );
#242678 = AXIS2_PLACEMENT_3D ( 'NONE', #224909, #188370, #7149 ) ;
#242679 = DIRECTION ( 'NONE',  ( -1.000000000000000000, -0.000000000000000000, -0.000000000000000000 ) ) ;
#242680 = CARTESIAN_POINT ( 'NONE',  ( -21.29999999999995808, 76.00000000001213607, -136.5231074845242745 ) ) ;
#242682 = EDGE_LOOP ( 'NONE', ( #158818, #9195, #198387 ) ) ;
#242681 = DIRECTION ( 'NONE',  ( -0.7071067811865214825, -0.7071067811865735520, 0.000000000000000000 ) ) ;
#242683 = VECTOR ( 'NONE', #219134, 1000.000000000000000 ) ;
#242684 = VECTOR ( 'NONE', #175140, 1000.000000000000000 ) ;
#242685 = AXIS2_PLACEMENT_3D ( 'NONE', #99152, #79591, #58736 ) ;
#242686 = AXIS2_PLACEMENT_3D ( 'NONE', #163499, #222158, #243025 ) ;
#242687 = EDGE_CURVE ( 'NONE', #82068, #243292, #237495, .T. ) ;
#242688 = FACE_OUTER_BOUND ( 'NONE', #156744, .T. ) ;
#242689 = EDGE_CURVE ( 'NONE', #194615, #247013, #120805, .T. ) ;
#242690 = EDGE_CURVE ( 'NONE', #162856, #243905, #187429, .T. ) ;
#242691 = CARTESIAN_POINT ( 'NONE',  ( -18.50596464788227635, 65.69367753730607262, -30.51892380663480964 ) ) ;
#242692 = CARTESIAN_POINT ( 'NONE',  ( -23.15000000000000213, 8.751106741858205140, -220.7398867978735950 ) ) ;
#242693 = CIRCLE ( 'NONE', #180351, 0.09999999999999939493 ) ;
#242694 = ORIENTED_EDGE ( 'NONE', *, *, #95376, .T. ) ;
#242695 = AXIS2_PLACEMENT_3D ( 'NONE', #76664, #175796, #213609 ) ;
#242697 = CARTESIAN_POINT ( 'NONE',  ( -21.05000000000000071, 6.257814610487270279, -133.9022097086912311 ) ) ;
#242696 = AXIS2_PLACEMENT_3D ( 'NONE', #98864, #136729, #181021 ) ;
#242698 = DIRECTION ( 'NONE',  ( 0.000000000000000000, -0.1335171055202867274, -0.9910465087640865089 ) ) ;
#242699 = CARTESIAN_POINT ( 'NONE',  ( -18.56579813702275672, 65.66974365629666011, -97.43601455626047425 ) ) ;
#242700 = ORIENTED_EDGE ( 'NONE', *, *, #122832, .F. ) ;
#242701 = DIRECTION ( 'NONE',  ( 0.000000000000000000, 0.000000000000000000, -1.000000000000000000 ) ) ;
#242703 = ORIENTED_EDGE ( 'NONE', *, *, #163634, .F. ) ;
#242702 = CARTESIAN_POINT ( 'NONE',  ( -16.80621392010912629, 9.942202577518866491, -188.3104080345828208 ) ) ;
#242705 = CARTESIAN_POINT ( 'NONE',  ( 21.09610168723073187, 0.03358950689149224622, 6.378955715224786438 ) ) ;
#242704 = CARTESIAN_POINT ( 'NONE',  ( 22.88900146558018989, 8.703904791123973084, -79.65000000000004832 ) ) ;
#242706 = EDGE_CURVE ( 'NONE', #166959, #11590, #216634, .T. ) ;
#242707 = FILL_AREA_STYLE_COLOUR ( '', #79246 ) ;
#242708 = EDGE_LOOP ( 'NONE', ( #52978, #253630, #52961, #29036 ) ) ;
#242709 = DIRECTION ( 'NONE',  ( 1.000000000000000000, 0.000000000000000000, 0.000000000000000000 ) ) ;
#242710 = CARTESIAN_POINT ( 'NONE',  ( 20.09999999999999787, 9.750000000011137757, -143.2500000000000284 ) ) ;
#242711 = CARTESIAN_POINT ( 'NONE',  ( -21.05000000000000071, 1.162701749938009677, -8.000000000000000000 ) ) ;
#242712 = ORIENTED_EDGE ( 'NONE', *, *, #118881, .F. ) ;
#242713 = CARTESIAN_POINT ( 'NONE',  ( 21.07928932188134397, 36.65892442174472876, -249.5511627012454596 ) ) ;
#242714 = VECTOR ( 'NONE', #232738, 1000.000000000000000 ) ;
#242715 = CARTESIAN_POINT ( 'NONE',  ( -23.15000000000000213, 85.00000000001251976, -179.9170766071767389 ) ) ;
#242716 = AXIS2_PLACEMENT_3D ( 'NONE', #185350, #27599, #6707 ) ;
#242717 = FACE_OUTER_BOUND ( 'NONE', #50064, .T. ) ;
#242718 = DIRECTION ( 'NONE',  ( 0.000000000000000000, 0.000000000000000000, -1.000000000000000000 ) ) ;
#242719 = ADVANCED_FACE ( 'NONE', ( #153682 ), #70267, .T. ) ;
#242720 = ORIENTED_EDGE ( 'NONE', *, *, #136992, .T. ) ;
#242721 = EDGE_CURVE ( 'NONE', #250417, #4697, #33722, .T. ) ;
#242722 = ORIENTED_EDGE ( 'NONE', *, *, #89125, .T. ) ;
#242723 = DIRECTION ( 'NONE',  ( 0.000000000000000000, 0.000000000000000000, 1.000000000000000000 ) ) ;
#242724 = LINE ( 'NONE', #238895, #23688 ) ;
#242725 = DIRECTION ( 'NONE',  ( -1.000000000000000000, 0.000000000000000000, 0.000000000000000000 ) ) ;
#242726 = CARTESIAN_POINT ( 'NONE',  ( 21.05000000000000071, 10.62872031401550288, -141.6649135690876449 ) ) ;
#242727 = EDGE_CURVE ( 'NONE', #234718, #250549, #208277, .T. ) ;
#242729 = FACE_OUTER_BOUND ( 'NONE', #68988, .T. ) ;
#242728 = CARTESIAN_POINT ( 'NONE',  ( 18.59999999999999432, 74.26374286841466699, -124.9544551555068068 ) ) ;
#242730 = LINE ( 'NONE', #27591, #239946 ) ;
#242731 = CARTESIAN_POINT ( 'NONE',  ( -16.79139129368504513, 66.05505583754988663, -56.85286285169858189 ) ) ;
#242732 = CARTESIAN_POINT ( 'NONE',  ( -22.59999985501179154, 64.25013020700916400, -136.5887061543240009 ) ) ;
#242733 = DIRECTION ( 'NONE',  ( 2.952720810173289112E-16, 1.000000000000000000, 6.467318590049456648E-15 ) ) ;
#242734 = AXIS2_PLACEMENT_3D ( 'NONE', #52566, #10897, #228671 ) ;
#242736 = VERTEX_POINT ( 'NONE', #51927 ) ;
#242735 = DIRECTION ( 'NONE',  ( 1.000000000000000000, -0.000000000000000000, -0.000000000000000000 ) ) ;
#242737 = CARTESIAN_POINT ( 'NONE',  ( -21.00250684356850073, 64.25000000001209344, -129.5083017157663789 ) ) ;
#242738 = CARTESIAN_POINT ( 'NONE',  ( -18.59999999999999787, 77.83534155023646406, -124.9679561919613064 ) ) ;
#242740 = LINE ( 'NONE', #199801, #15970 ) ;
#242739 = FACE_OUTER_BOUND ( 'NONE', #51065, .T. ) ;
#242741 = VERTEX_POINT ( 'NONE', #130189 ) ;
#242743 = DIRECTION ( 'NONE',  ( 0.000000000000000000, -1.000000000000000000, -6.982962677686266711E-15 ) ) ;
#242742 = DIRECTION ( 'NONE',  ( 0.000000000000000000, -0.7397890806274287634, -0.6728388485992942147 ) ) ;
#242744 = CARTESIAN_POINT ( 'NONE',  ( -18.50000000000000000, 72.08710075277861051, -125.0412845115133678 ) ) ;
#242745 = DIRECTION ( 'NONE',  ( 1.186688945009009831E-16, 1.000000000000000000, 6.982962677686266711E-15 ) ) ;
#242746 = CARTESIAN_POINT ( 'NONE',  ( -14.00000000000000178, 9.849999999999978328, -16.75000000000000355 ) ) ;
#242747 = FACE_OUTER_BOUND ( 'NONE', #71632, .T. ) ;
#242748 = ORIENTED_EDGE ( 'NONE', *, *, #240656, .F. ) ;
#242749 = ORIENTED_EDGE ( 'NONE', *, *, #128649, .T. ) ;
#242750 = ADVANCED_FACE ( 'NONE', ( #171944 ), #53239, .F. ) ;
#242752 = VECTOR ( 'NONE', #29209, 1000.000000000000000 ) ;
#242751 = CARTESIAN_POINT ( 'NONE',  ( -18.59999999999999787, 68.97833521811233481, -166.1895420826271277 ) ) ;
#242753 = ORIENTED_EDGE ( 'NONE', *, *, #196250, .T. ) ;
#242754 = CARTESIAN_POINT ( 'NONE',  ( 21.00000000000000000, 9.750000000011153745, -88.25000000000005684 ) ) ;
#242755 = ORIENTED_EDGE ( 'NONE', *, *, #151864, .T. ) ;
#242756 = VECTOR ( 'NONE', #169099, 1000.000000000000000 ) ;
#242757 = CYLINDRICAL_SURFACE ( 'NONE', #106025, 0.09999999999999939493 ) ;
#242758 = DIRECTION ( 'NONE',  ( 1.000000000000000000, -0.000000000000000000, -0.000000000000000000 ) ) ;
#242759 = TOROIDAL_SURFACE ( 'NONE', #46931, 11.70000000000000639, 0.1000000000000000056 ) ;
#242760 = EDGE_CURVE ( 'NONE', #198122, #23723, #87454, .T. ) ;
#242761 =( BOUNDED_SURFACE ( )  B_SPLINE_SURFACE ( 3, 2, ( 
 ( #19578, #79517, #57390 ),
 ( #119986, #159100, #238616 ),
 ( #76963, #100358, #136942 ),
 ( #37870, #179937, #117384 ),
 ( #1266, #18280, #196913 ),
 ( #200771, #22158, #181228 ),
 ( #63834, #162950, #102930 ),
 ( #182515, #24735, #221589 ),
 ( #242447, #143358, #145917 ),
 ( #105485, #187646, #164225 ) ),
 .UNSPECIFIED., .F., .F., .F. ) 
 B_SPLINE_SURFACE_WITH_KNOTS ( ( 4, 2, 2, 2, 4 ),
 ( 3, 3 ),
 ( 0.0001701955120502367854, 0.0002247052511886119680, 0.0002792149903269871506, 0.0003882344686037374616, 0.0006062734251572381378 ),
 ( 0.000000000000000000, 1.000000000000000000 ),
 .UNSPECIFIED. ) 
 GEOMETRIC_REPRESENTATION_ITEM ( )  RATIONAL_B_SPLINE_SURFACE ( (
 ( 1.000000000000000000, 0.2966190024560742544, 1.000000000000000000),
 ( 1.000000000000000000, 0.2964522492714360968, 1.000000000000000000),
 ( 1.000000000000000000, 0.3059923531879654712, 1.000000000000000000),
 ( 1.000000000000000000, 0.3355751146950147756, 1.000000000000000000),
 ( 1.000000000000000000, 0.3550672384961490180, 1.000000000000000000),
 ( 1.000000000000000000, 0.4157034672184696245, 1.000000000000000000),
 ( 1.000000000000000000, 0.4588031877653353519, 1.000000000000000000),
 ( 1.000000000000000000, 0.5771441759663189508, 1.000000000000000000),
 ( 1.000000000000000000, 0.6469377121770625294, 1.000000000000000000),
 ( 1.000000000000000000, 0.7071067811865402453, 1.000000000000000000) ) ) 
 REPRESENTATION_ITEM ( '' )  SURFACE ( )  );
#242762 = CARTESIAN_POINT ( 'NONE',  ( -20.96428641294356510, 62.87317279473557363, -207.0346585172401603 ) ) ;
#242763 = ORIENTED_EDGE ( 'NONE', *, *, #119112, .T. ) ;
#242764 = EDGE_CURVE ( 'NONE', #107904, #62992, #37591, .T. ) ;
#242766 = ADVANCED_FACE ( 'NONE', ( #111947 ), #99894, .F. ) ;
#242765 = FACE_OUTER_BOUND ( 'NONE', #15671, .T. ) ;
#242767 = CARTESIAN_POINT ( 'NONE',  ( 23.40000000000005542, 83.80000000001119531, -51.02310748452479316 ) ) ;
#242768 = CARTESIAN_POINT ( 'NONE',  ( 18.49999999999999645, -1.299733671219632791, -23.52812952286940273 ) ) ;
#242769 = CIRCLE ( 'NONE', #163672, 4.300000000000039790 ) ;
#242771 = DIRECTION ( 'NONE',  ( 1.000000000000000000, 0.000000000000000000, 0.000000000000000000 ) ) ;
#242770 = VECTOR ( 'NONE', #165264, 1000.000000000000000 ) ;
#242772 = FACE_OUTER_BOUND ( 'NONE', #94492, .T. ) ;
#242774 = CIRCLE ( 'NONE', #172091, 4.149999999999987033 ) ;
#242773 = DIRECTION ( 'NONE',  ( 1.000000000000000000, 0.000000000000000000, 0.000000000000000000 ) ) ;
#242775 = CARTESIAN_POINT ( 'NONE',  ( -23.15000000000000213, 74.07476635515273244, -182.7533510176504876 ) ) ;
#242776 = ORIENTED_EDGE ( 'NONE', *, *, #24863, .F. ) ;
#242778 = CARTESIAN_POINT ( 'NONE',  ( -22.45372860728439690, 75.98507938046427057, -215.1729046192282340 ) ) ;
#242777 = CARTESIAN_POINT ( 'NONE',  ( -18.59999999999999787, -9.849999999999942801, -15.00000000000002309 ) ) ;
#242779 = EDGE_LOOP ( 'NONE', ( #9136, #81885, #5444 ) ) ;
#242781 = ORIENTED_EDGE ( 'NONE', *, *, #27279, .F. ) ;
#242780 = DIRECTION ( 'NONE',  ( 1.000000000000000000, -0.000000000000000000, 0.000000000000000000 ) ) ;
#242782 = ADVANCED_FACE ( 'NONE', ( #132795 ), #162490, .T. ) ;
#242783 = ORIENTED_EDGE ( 'NONE', *, *, #6458, .T. ) ;
#242784 = DIRECTION ( 'NONE',  ( -0.7071067811865475727, 0.2890913453342130457, -0.6453109281988448354 ) ) ;
#242785 = ADVANCED_FACE ( 'NONE', ( #168099 ), #209750, .T. ) ;
#242786 = FACE_OUTER_BOUND ( 'NONE', #67804, .T. ) ;
#242787 = FACE_OUTER_BOUND ( 'NONE', #140187, .T. ) ;
#242788 = CIRCLE ( 'NONE', #138690, 0.09999999999999939493 ) ;
#242789 = CARTESIAN_POINT ( 'NONE',  ( -21.05000000000000071, -11.39257802169451672, -103.5739495798319751 ) ) ;
#242790 = EDGE_LOOP ( 'NONE', ( #94101, #106219, #205057, #245854 ) ) ;
#242791 = DIRECTION ( 'NONE',  ( 0.7071067811865493491, 0.7071067811865456854, 0.000000000000000000 ) ) ;
#242793 = EDGE_CURVE ( 'NONE', #31458, #82011, #50646, .T. ) ;
#242792 = CARTESIAN_POINT ( 'NONE',  ( 20.27550659511088682, 61.64772458173430181, -221.2338429919259966 ) ) ;
#242794 = CIRCLE ( 'NONE', #201275, 5.000000000000003553 ) ;
#242795 = ORIENTED_EDGE ( 'NONE', *, *, #64697, .T. ) ;
#242796 = AXIS2_PLACEMENT_3D ( 'NONE', #114900, #31548, #169776 ) ;
#242797 = AXIS2_PLACEMENT_3D ( 'NONE', #149803, #126360, #127651 ) ;
#242798 = CARTESIAN_POINT ( 'NONE',  ( -2.995603634470884209E-16, 6.650000000011155876, -54.65000000000000568 ) ) ;
#242799 = AXIS2_PLACEMENT_3D ( 'NONE', #81376, #572, #159679 ) ;
#242800 = EDGE_CURVE ( 'NONE', #100635, #168456, #114496, .T. ) ;
#242801 = DIRECTION ( 'NONE',  ( -1.000000000000000000, 0.000000000000000000, 0.000000000000000000 ) ) ;
#242802 = ORIENTED_EDGE ( 'NONE', *, *, #109384, .T. ) ;
#242803 = CARTESIAN_POINT ( 'NONE',  ( -16.77308656112214180, 9.950000000011137047, -146.6501931917023001 ) ) ;
#242804 = ADVANCED_FACE ( 'NONE', ( #157511 ), #136603, .F. ) ;
#242805 = EDGE_CURVE ( 'NONE', #5347, #37627, #250149, .T. ) ;
#242806 = EDGE_LOOP ( 'NONE', ( #2380, #195780, #42112, #233199 ) ) ;
#242807 = CARTESIAN_POINT ( 'NONE',  ( -21.64999999999999858, 68.65000000001261071, -191.2731074845244166 ) ) ;
#242808 = EDGE_LOOP ( 'NONE', ( #11396, #48237, #145024, #186361, #39344, #107200 ) ) ;
#242809 = CARTESIAN_POINT ( 'NONE',  ( -21.14999999999999858, 56.01362831242966678, -232.7091905853083347 ) ) ;
#242810 = EDGE_CURVE ( 'NONE', #99187, #171946, #135323, .T. ) ;
#242811 = FACE_OUTER_BOUND ( 'NONE', #100176, .T. ) ;
#242812 = CARTESIAN_POINT ( 'NONE',  ( 18.59999999999997655, 76.00000000001213607, -136.5231074845243313 ) ) ;
#242813 = EDGE_CURVE ( 'NONE', #235463, #245346, #158585, .T. ) ;
#242814 = EDGE_CURVE ( 'NONE', #11624, #219843, #40122, .T. ) ;
#242815 = AXIS2_PLACEMENT_3D ( 'NONE', #73467, #232538, #180247 ) ;
#242816 = EDGE_CURVE ( 'NONE', #186991, #113855, #233423, .T. ) ;
#242817 = AXIS2_PLACEMENT_3D ( 'NONE', #99574, #138689, #257333 ) ;
#242818 = CARTESIAN_POINT ( 'NONE',  ( 18.49999999999998934, 43.16354019706792400, -239.5695141926698284 ) ) ;
#242819 = CARTESIAN_POINT ( 'NONE',  ( 20.95000000000005258, 65.19115966511134275, -29.92310748452479174 ) ) ;
#242820 = CARTESIAN_POINT ( 'NONE',  ( -21.05000000000000071, 74.83729825007408465, -128.5231074845243029 ) ) ;
#242821 = VERTEX_POINT ( 'NONE', #36265 ) ;
#242823 = CARTESIAN_POINT ( 'NONE',  ( -20.85000000000000142, 72.03510814376021187, -246.5782642391033903 ) ) ;
#242822 = CARTESIAN_POINT ( 'NONE',  ( -21.05000000000000071, 69.45934304831114048, -170.0231074845243882 ) ) ;
#242824 = ORIENTED_EDGE ( 'NONE', *, *, #33100, .F. ) ;
#242825 = CIRCLE ( 'NONE', #176214, 0.1000000000000028644 ) ;
#242826 = CARTESIAN_POINT ( 'NONE',  ( -16.90202395485563613, 12.41833139826750454, -211.1876964646075976 ) ) ;
#242827 = LINE ( 'NONE', #244108, #120720 ) ;
#242828 = CIRCLE ( 'NONE', #138915, 0.09999999999999939493 ) ;
#242830 = EDGE_LOOP ( 'NONE', ( #53888, #185200, #160940 ) ) ;
#242829 = FACE_OUTER_BOUND ( 'NONE', #73051, .T. ) ;
#242832 = ORIENTED_EDGE ( 'NONE', *, *, #219682, .T. ) ;
#242831 = LINE ( 'NONE', #218117, #212091 ) ;
#242833 = EDGE_CURVE ( 'NONE', #1674, #237441, #212569, .T. ) ;
#242834 = DIRECTION ( 'NONE',  ( -1.000000000000000000, 0.000000000000000000, 0.000000000000000000 ) ) ;
#242836 = CARTESIAN_POINT ( 'NONE',  ( -20.09999999999999787, 5.552655413246003313, 16.61686199900910310 ) ) ;
#242835 =( BOUNDED_CURVE ( )  B_SPLINE_CURVE ( 3, ( #13043, #155131, #172134, #73030 ),
 .UNSPECIFIED., .F., .F. ) 
 B_SPLINE_CURVE_WITH_KNOTS ( ( 4, 4 ),
 ( 0.3000847527772381729, 0.5497968875596822569 ),
 .UNSPECIFIED. ) 
 CURVE ( )  GEOMETRIC_REPRESENTATION_ITEM ( )  RATIONAL_B_SPLINE_CURVE ( ( 1.000000000000000000, 0.9948104011409419911, 0.9948104011409419911, 1.000000000000000000 ) ) 
 REPRESENTATION_ITEM ( '' )  );
#242837 = DIRECTION ( 'NONE',  ( -0.000000000000000000, 0.6132151058540549204, -0.7899159663865520375 ) ) ;
#242838 = EDGE_CURVE ( 'NONE', #146605, #256668, #95998, .T. ) ;
#242839 = CIRCLE ( 'NONE', #130408, 0.1000000000000052097 ) ;
#242840 = CARTESIAN_POINT ( 'NONE',  ( 21.14999999999999858, 67.21339244341145047, -57.17310748452437963 ) ) ;
#242842 = VERTEX_POINT ( 'NONE', #919 ) ;
#242841 = DIRECTION ( 'NONE',  ( -1.000000000000000000, 0.000000000000000000, 0.000000000000000000 ) ) ;
#242843 = AXIS2_PLACEMENT_3D ( 'NONE', #148256, #227787, #49154 ) ;
#242844 = CIRCLE ( 'NONE', #59643, 12.77499999999999503 ) ;
#242845 = AXIS2_PLACEMENT_3D ( 'NONE', #87050, #84457, #208329 ) ;
#242846 = PRODUCT_DEFINITION_SHAPE ( 'NONE', 'NONE',  #148835 ) ;
#242847 = AXIS2_PLACEMENT_3D ( 'NONE', #198905, #99780, #195087 ) ;
#242848 = CARTESIAN_POINT ( 'NONE',  ( 21.08489834409762054, 10.62232389474667293, -179.8499999999999943 ) ) ;
#242849 = ORIENTED_EDGE ( 'NONE', *, *, #183941, .T. ) ;
#242850 = ORIENTED_EDGE ( 'NONE', *, *, #52577, .T. ) ;
#242851 = DIRECTION ( 'NONE',  ( 0.000000000000000000, -7.304098846218139203E-15, 1.000000000000000000 ) ) ;
#242852 = CARTESIAN_POINT ( 'NONE',  ( -21.44999999999999929, 44.91518204311810081, -238.0177672736398620 ) ) ;
#242853 = AXIS2_PLACEMENT_3D ( 'NONE', #109904, #12132, #132053 ) ;
#242854 = ORIENTED_EDGE ( 'NONE', *, *, #125698, .T. ) ;
#242855 = DIRECTION ( 'NONE',  ( 0.000000000000000000, 0.000000000000000000, -1.000000000000000000 ) ) ;
#242856 = VECTOR ( 'NONE', #132509, 999.9999999999998863 ) ;
#242857 = DIRECTION ( 'NONE',  ( 0.000000000000000000, 0.9856811345164832039, 0.1686199900910280158 ) ) ;
#242858 = AXIS2_PLACEMENT_3D ( 'NONE', #63950, #204723, #182627 ) ;
#242859 = EDGE_CURVE ( 'NONE', #98576, #245959, #48287, .T. ) ;
#242860 = ORIENTED_EDGE ( 'NONE', *, *, #224218, .T. ) ;
#242862 = EDGE_CURVE ( 'NONE', #174523, #181466, #175771, .T. ) ;
#242861 = CARTESIAN_POINT ( 'NONE',  ( 12.25000000000000000, 9.349999999999983658, -16.74999999999999645 ) ) ;
#242864 =( BOUNDED_SURFACE ( )  B_SPLINE_SURFACE ( 3, 2, ( 
 ( #79150, #180847, #257747 ),
 ( #140412, #158739, #99982 ),
 ( #58300, #41354, #238235 ),
 ( #236962, #117016, #235662 ),
 ( #60878, #120896, #200405 ),
 ( #884, #136557, #101246 ),
 ( #57007, #59567, #139102 ),
 ( #218663, #2180, #81693 ),
 ( #196541, #161295, #179574 ),
 ( #216099, #36217, #137840 ),
 ( #240818, #62182, #141701 ),
 ( #115733, #256451, #156168 ) ),
 .UNSPECIFIED., .F., .F., .F. ) 
 B_SPLINE_SURFACE_WITH_KNOTS ( ( 4, 2, 2, 2, 2, 4 ),
 ( 3, 3 ),
 ( 3.174653483277205090, 3.943930578431714018, 4.713207673586222946, 5.482484768740731873, 5.867123316317986337, 6.251761863895240801 ),
 ( 0.000000000000000000, 1.000000000000000000 ),
 .UNSPECIFIED. ) 
 GEOMETRIC_REPRESENTATION_ITEM ( )  RATIONAL_B_SPLINE_SURFACE ( (
 ( 1.000000000000000000, 0.8659465255642289083, 1.000000000000000000),
 ( 1.000000000000000000, 0.8648614068487556761, 1.000000000000000000),
 ( 1.000000000000000000, 0.8489031841324650163, 1.000000000000000000),
 ( 1.000000000000000000, 0.7927507630160894880, 1.000000000000000000),
 ( 1.000000000000000000, 0.7523013859007079418, 1.000000000000000000),
 ( 1.000000000000000000, 0.6616226951198711514, 1.000000000000000000),
 ( 1.000000000000000000, 0.6112214368721650137, 1.000000000000000000),
 ( 1.000000000000000000, 0.5507684314500187472, 1.000000000000000000),
 ( 1.000000000000000000, 0.5333267243151817993, 1.000000000000000000),
 ( 1.000000000000000000, 0.5084565446480915352, 1.000000000000000000),
 ( 1.000000000000000000, 0.5010722703450180004, 1.000000000000000000),
 ( 1.000000000000000000, 0.5001234037138587718, 1.000000000000000000) ) ) 
 REPRESENTATION_ITEM ( '' )  SURFACE ( )  );
#242863 = AXIS2_PLACEMENT_3D ( 'NONE', #28901, #69276, #74102 ) ;
#242866 = VECTOR ( 'NONE', #44352, 1000.000000000000000 ) ;
#242865 = DIRECTION ( 'NONE',  ( 0.000000000000000000, 0.000000000000000000, -1.000000000000000000 ) ) ;
#242867 = VERTEX_POINT ( 'NONE', #218704 ) ;
#242868 = VECTOR ( 'NONE', #210340, 1000.000000000000000 ) ;
#242869 = ORIENTED_EDGE ( 'NONE', *, *, #122890, .F. ) ;
#242870 = CARTESIAN_POINT ( 'NONE',  ( 18.49999999999999645, 77.86671491006917734, -91.27043223824227880 ) ) ;
#242871 = ORIENTED_EDGE ( 'NONE', *, *, #272, .T. ) ;
#242872 = CARTESIAN_POINT ( 'NONE',  ( 17.23472005113828232, 10.30788195451192379, -178.9534231399312887 ) ) ;
#242873 = ORIENTED_EDGE ( 'NONE', *, *, #248641, .F. ) ;
#242875 = VERTEX_POINT ( 'NONE', #80453 ) ;
#242874 = CARTESIAN_POINT ( 'NONE',  ( -18.59999999999999787, 11.65000000001115232, -141.0148057706540214 ) ) ;
#242876 = DIRECTION ( 'NONE',  ( 1.186688945009010077E-16, 1.000000000000000000, 6.982962677686266711E-15 ) ) ;
#242877 = ORIENTED_EDGE ( 'NONE', *, *, #51968, .T. ) ;
#242878 = DIRECTION ( 'NONE',  ( -1.000000000000000000, -0.000000000000000000, -0.000000000000000000 ) ) ;
#242879 = VERTEX_POINT ( 'NONE', #216146 ) ;
#242881 = ORIENTED_EDGE ( 'NONE', *, *, #48330, .T. ) ;
#242880 = ORIENTED_EDGE ( 'NONE', *, *, #126665, .T. ) ;
#242882 = CARTESIAN_POINT ( 'NONE',  ( 21.07954763557393818, 69.67070900997488536, -136.5889834031427768 ) ) ;
#242883 = EDGE_CURVE ( 'NONE', #205599, #29656, #97463, .T. ) ;
#242884 = CARTESIAN_POINT ( 'NONE',  ( 23.24999999999999645, 11.74999999999998224, -9.250000000000001776 ) ) ;
#242886 = ORIENTED_EDGE ( 'NONE', *, *, #38695, .F. ) ;
#242885 = CIRCLE ( 'NONE', #188909, 0.1000000000000024342 ) ;
#242887 = AXIS2_PLACEMENT_3D ( 'NONE', #166215, #67081, #224854 ) ;
#242888 = AXIS2_PLACEMENT_3D ( 'NONE', #8740, #149558, #229079 ) ;
#242889 = VECTOR ( 'NONE', #209557, 1000.000000000000000 ) ;
#242890 = ORIENTED_EDGE ( 'NONE', *, *, #166865, .T. ) ;
#242891 = DIRECTION ( 'NONE',  ( -0.000000000000000000, 0.2128009952263603677, -0.9770955615653313941 ) ) ;
#242892 = DIRECTION ( 'NONE',  ( 0.000000000000000000, -0.9908441862701605762, 0.1350103645451835310 ) ) ;
#242893 = ORIENTED_EDGE ( 'NONE', *, *, #142432, .F. ) ;
#242894 = CARTESIAN_POINT ( 'NONE',  ( -23.15000000000000213, 1.115650265596050101E-11, -62.95000000000004547 ) ) ;
#242895 = EDGE_LOOP ( 'NONE', ( #106215, #237521, #5208 ) ) ;
#242896 = CARTESIAN_POINT ( 'NONE',  ( 23.14999999999999858, 0.000000000000000000, -33.50000000000000000 ) ) ;
#242897 = CARTESIAN_POINT ( 'NONE',  ( 18.52928932188133970, 65.72071067813061518, -111.8731074845243683 ) ) ;
#242898 = EDGE_LOOP ( 'NONE', ( #21627, #219129, #78225, #142168 ) ) ;
#242899 = LINE ( 'NONE', #5553, #248762 ) ;
#242900 = DIRECTION ( 'NONE',  ( -1.000000000000000000, 0.000000000000000000, 0.000000000000000000 ) ) ;
#242901 = EDGE_LOOP ( 'NONE', ( #255644, #55526, #172672, #154254, #26814, #52902 ) ) ;
#242902 = DIRECTION ( 'NONE',  ( -0.000000000000000000, -0.000000000000000000, -1.000000000000000000 ) ) ;
#242903 = ORIENTED_EDGE ( 'NONE', *, *, #40593, .F. ) ;
#242905 = ORIENTED_EDGE ( 'NONE', *, *, #241252, .T. ) ;
#242904 = ORIENTED_EDGE ( 'NONE', *, *, #16380, .T. ) ;
#242906 = CIRCLE ( 'NONE', #151357, 2.100000000000004974 ) ;
#242907 = ORIENTED_EDGE ( 'NONE', *, *, #249965, .F. ) ;
#242908 = SPHERICAL_SURFACE ( 'NONE', #149133, 0.1000000000000000056 ) ;
#242909 = ORIENTED_EDGE ( 'NONE', *, *, #86709, .T. ) ;
#242910 = CARTESIAN_POINT ( 'NONE',  ( -16.87242674293849376, 66.05000000001153637, -48.67201723815204417 ) ) ;
#242911 = VERTEX_POINT ( 'NONE', #197869 ) ;
#242912 = CARTESIAN_POINT ( 'NONE',  ( -21.14999999999999858, 64.35000000001195986, -102.9231074845243938 ) ) ;
#242913 = EDGE_CURVE ( 'NONE', #176547, #218877, #338, .T. ) ;
#242914 = ORIENTED_EDGE ( 'NONE', *, *, #164177, .T. ) ;
#242915 = EDGE_CURVE ( 'NONE', #60211, #150205, #162664, .T. ) ;
#242916 = ORIENTED_EDGE ( 'NONE', *, *, #171175, .F. ) ;
#242917 = VECTOR ( 'NONE', #45599, 1000.000000000000000 ) ;
#242918 = ORIENTED_EDGE ( 'NONE', *, *, #42561, .F. ) ;
#242919 = CIRCLE ( 'NONE', #134580, 0.1000000000000028644 ) ;
#242920 = AXIS2_PLACEMENT_3D ( 'NONE', #28443, #104059, #203180 ) ;
#242921 = EDGE_CURVE ( 'NONE', #238186, #13565, #125249, .T. ) ;
#242922 = CARTESIAN_POINT ( 'NONE',  ( -16.94878442675511465, 66.00827089702079320, -82.13488790888651181 ) ) ;
#242923 = EDGE_LOOP ( 'NONE', ( #16836, #126968, #39134, #53440 ) ) ;
#242924 = FACE_OUTER_BOUND ( 'NONE', #99603, .T. ) ;
#242926 = EDGE_CURVE ( 'NONE', #96700, #156221, #137686, .T. ) ;
#242925 = DIRECTION ( 'NONE',  ( 1.836970198721029934E-16, 1.000000000000000000, 6.982962677686266711E-15 ) ) ;
#242927 = DIRECTION ( 'NONE',  ( 2.952720810173289112E-16, -1.000000000000000000, 0.000000000000000000 ) ) ;
#242928 = CARTESIAN_POINT ( 'NONE',  ( -20.87155475150660777, 11.75000000001115197, -127.0955865291576714 ) ) ;
#242929 = DIRECTION ( 'NONE',  ( 0.000000000000000000, 1.000000000000000000, 0.000000000000000000 ) ) ;
#242930 = CARTESIAN_POINT ( 'NONE',  ( -20.15000000000000568, 66.70857864377474300, -124.2731074845243597 ) ) ;
#242931 = DIRECTION ( 'NONE',  ( 1.000000000000000000, 0.000000000000000000, 0.000000000000000000 ) ) ;
#242933 = FACE_OUTER_BOUND ( 'NONE', #38243, .T. ) ;
#242932 = DIRECTION ( 'NONE',  ( -1.000000000000000000, -0.000000000000000000, 0.000000000000000000 ) ) ;
#242934 = SPHERICAL_SURFACE ( 'NONE', #132401, 0.1000000000000000056 ) ;
#242935 = DIRECTION ( 'NONE',  ( 0.000000000000000000, -1.000000000000000000, -6.837150591533219968E-15 ) ) ;
#242936 = AXIS2_PLACEMENT_3D ( 'NONE', #39468, #293, #240212 ) ;
#242937 = EDGE_CURVE ( 'NONE', #13140, #238715, #50207, .T. ) ;
#242938 = CYLINDRICAL_SURFACE ( 'NONE', #251790, 0.1000000000000002554 ) ;
#242939 = AXIS2_PLACEMENT_3D ( 'NONE', #171666, #148208, #67392 ) ;
#242940 = ORIENTED_EDGE ( 'NONE', *, *, #159230, .T. ) ;
#242941 = AXIS2_PLACEMENT_3D ( 'NONE', #61029, #197976, #117173 ) ;
#242943 = ORIENTED_EDGE ( 'NONE', *, *, #41362, .F. ) ;
#242942 = CARTESIAN_POINT ( 'NONE',  ( -33.72168855820452649, 23.65833333334447985, -50.25000000000000000 ) ) ;
#242944 = EDGE_LOOP ( 'NONE', ( #162988, #186073, #186126, #162805 ) ) ;
#242946 = ADVANCED_FACE ( 'NONE', ( #81741 ), #64777, .T. ) ;
#242945 = DIRECTION ( 'NONE',  ( -1.000000000000000000, 0.000000000000000000, -0.000000000000000000 ) ) ;
#242947 = DIRECTION ( 'NONE',  ( -1.000000000000000000, 0.000000000000000000, -0.000000000000000000 ) ) ;
#242948 = CARTESIAN_POINT ( 'NONE',  ( 20.84999999999999432, 43.35377423437995503, -245.1717807829448930 ) ) ;
#242949 = VERTEX_POINT ( 'NONE', #42652 ) ;
#242950 = VECTOR ( 'NONE', #34856, 1000.000000000000000 ) ;
#242951 = VECTOR ( 'NONE', #159535, 1000.000000000000000 ) ;
#242953 = VECTOR ( 'NONE', #122866, 999.9999999999998863 ) ;
#242952 = DIRECTION ( 'NONE',  ( -0.8660254037843277963, 0.000000000000000000, 0.5000000000001921796 ) ) ;
#242954 = DIRECTION ( 'NONE',  ( -1.000000000000000000, -0.000000000000000000, -0.000000000000000000 ) ) ;
#242955 = ORIENTED_EDGE ( 'NONE', *, *, #245356, .F. ) ;
#242956 = SPHERICAL_SURFACE ( 'NONE', #59014, 0.1000000000000000056 ) ;
#242957 = DIRECTION ( 'NONE',  ( 0.000000000000000000, -0.9651348961777157509, 0.2617529984165031243 ) ) ;
#242958 = DIRECTION ( 'NONE',  ( -0.000000000000000000, 0.1686199900910313187, -0.9856811345164828708 ) ) ;
#242959 = AXIS2_PLACEMENT_3D ( 'NONE', #110194, #154505, #73681 ) ;
#242960 = DIRECTION ( 'NONE',  ( 0.000000000000000000, 0.000000000000000000, -1.000000000000000000 ) ) ;
#242962 = EDGE_LOOP ( 'NONE', ( #215052, #165991, #236145, #18091 ) ) ;
#242961 = CARTESIAN_POINT ( 'NONE',  ( -20.64999999999999858, 4.349999999999999645, -12.35000000000000142 ) ) ;
#242963 = DIRECTION ( 'NONE',  ( 1.000000000000000000, 0.000000000000000000, 0.000000000000000000 ) ) ;
#242965 = VERTEX_POINT ( 'NONE', #141745 ) ;
#242964 = PLANE ( 'NONE',  #6469 ) ;
#242966 = CARTESIAN_POINT ( 'NONE',  ( -22.48660254037843487, 11.65000000001115588, -167.4499999999999886 ) ) ;
#242968 = DIRECTION ( 'NONE',  ( -1.000000000000000000, 0.000000000000000000, 0.000000000000000000 ) ) ;
#242967 = AXIS2_PLACEMENT_3D ( 'NONE', #28688, #7802, #62637 ) ;
#242970 = VERTEX_POINT ( 'NONE', #60920 ) ;
#242969 = VECTOR ( 'NONE', #99427, 1000.000000000000227 ) ;
#242971 = CARTESIAN_POINT ( 'NONE',  ( 23.14999999999999503, 61.90000000001145963, -41.62340509566378444 ) ) ;
#242972 = CARTESIAN_POINT ( 'NONE',  ( 18.49999999999999645, 1.115600667400684642E-11, -67.00000000000004263 ) ) ;
#242973 = CIRCLE ( 'NONE', #172310, 0.1000000000000124678 ) ;
#242975 = CARTESIAN_POINT ( 'NONE',  ( 20.94999999999999574, 74.75000000001207923, -128.6231074845242972 ) ) ;
#242974 = CARTESIAN_POINT ( 'NONE',  ( -16.93353400591626112, 63.05466693176257564, -213.0335249609126151 ) ) ;
#242976 = CARTESIAN_POINT ( 'NONE',  ( -18.59999999999999787, 77.85102823015292017, -124.8691942151017855 ) ) ;
#242977 = CARTESIAN_POINT ( 'NONE',  ( -20.94999999999999929, 14.76289716703256083, -235.7888246855571026 ) ) ;
#242978 = FILL_AREA_STYLE ('',( #224694 ) ) ;
#242979 = CARTESIAN_POINT ( 'NONE',  ( -23.25000000000000000, 4.150000000000001243, -21.25000000000000000 ) ) ;
#242980 = LINE ( 'NONE', #186893, #10096 ) ;
#242981 = ORIENTED_EDGE ( 'NONE', *, *, #224798, .F. ) ;
#242982 = ADVANCED_FACE ( 'NONE', ( #242129 ), #165169, .T. ) ;
#242983 = CARTESIAN_POINT ( 'NONE',  ( -21.05000000000000071, 87.65000000001246860, -172.9231074845242802 ) ) ;
#242984 = EDGE_LOOP ( 'NONE', ( #133241, #196621, #185248, #224669 ) ) ;
#242985 = ORIENTED_EDGE ( 'NONE', *, *, #75002, .T. ) ;
#242986 = FACE_OUTER_BOUND ( 'NONE', #16631, .T. ) ;
#242987 = CARTESIAN_POINT ( 'NONE',  ( -22.39999999999999858, 64.35000000001238618, -170.0231074845244166 ) ) ;
#242988 = ORIENTED_EDGE ( 'NONE', *, *, #205662, .F. ) ;
#242989 = EDGE_CURVE ( 'NONE', #223292, #4792, #91910, .T. ) ;
#242990 = VERTEX_POINT ( 'NONE', #101285 ) ;
#242991 = AXIS2_PLACEMENT_3D ( 'NONE', #47115, #87533, #186671 ) ;
#242992 = EDGE_CURVE ( 'NONE', #115244, #221121, #221271, .T. ) ;
#242993 = EDGE_CURVE ( 'NONE', #110754, #50587, #145894, .T. ) ;
#242994 = TOROIDAL_SURFACE ( 'NONE', #51436, 11.65000000000000036, 0.1000000000000000056 ) ;
#242995 = VERTEX_POINT ( 'NONE', #66061 ) ;
#242996 = AXIS2_PLACEMENT_3D ( 'NONE', #187954, #229643, #191829 ) ;
#242997 = CARTESIAN_POINT ( 'NONE',  ( -23.15000000000000213, 85.60000000001208775, -126.6291383618717816 ) ) ;
#242998 = EDGE_LOOP ( 'NONE', ( #228018, #235742, #123855, #229703 ) ) ;
#242999 = DIRECTION ( 'NONE',  ( -1.000000000000000000, 0.000000000000000000, 0.000000000000000000 ) ) ;
#243000 = DIRECTION ( 'NONE',  ( 0.000000000000000000, 0.000000000000000000, 1.000000000000000000 ) ) ;
#243001 = DIRECTION ( 'NONE',  ( 1.000000000000000000, 0.000000000000000000, 0.000000000000000000 ) ) ;
#243002 = DIRECTION ( 'NONE',  ( -0.000000000000000000, -0.9770955615653316162, -0.2128009952263597848 ) ) ;
#243003 = FACE_OUTER_BOUND ( 'NONE', #224404, .T. ) ;
#243004 = CARTESIAN_POINT ( 'NONE',  ( 21.07928932188134397, 65.47931918658503037, -241.9371126717015841 ) ) ;
#243005 = CARTESIAN_POINT ( 'NONE',  ( 23.24999999999999645, 70.40000000001222702, -148.2731074845243313 ) ) ;
#243007 = ORIENTED_EDGE ( 'NONE', *, *, #135744, .F. ) ;
#243006 = CYLINDRICAL_SURFACE ( 'NONE', #221437, 0.1000000000000024342 ) ;
#243009 = CARTESIAN_POINT ( 'NONE',  ( -18.59999999999999787, -1.263275465206102233, -208.9018646667463770 ) ) ;
#243008 = CARTESIAN_POINT ( 'NONE',  ( 20.95520789717937404, 65.42306940062664466, -61.94287451064954553 ) ) ;
#243010 = EDGE_CURVE ( 'NONE', #221695, #56583, #220004, .T. ) ;
#243011 = DIRECTION ( 'NONE',  ( 1.000000000000000000, 0.000000000000000000, 0.000000000000000000 ) ) ;
#243012 = VERTEX_POINT ( 'NONE', #26973 ) ;
#243013 = AXIS2_PLACEMENT_3D ( 'NONE', #204567, #28557, #25946 ) ;
#243014 = DIRECTION ( 'NONE',  ( 0.000000000000000000, -0.2617529984165152257, -0.9651348961777124202 ) ) ;
#243016 = EDGE_CURVE ( 'NONE', #7336, #71686, #216818, .T. ) ;
#243015 = LINE ( 'NONE', #64394, #183336 ) ;
#243017 = VERTEX_POINT ( 'NONE', #243417 ) ;
#243018 = TOROIDAL_SURFACE ( 'NONE', #30660, 0.9750000000000019762, 0.1000000000000000056 ) ;
#243020 = CARTESIAN_POINT ( 'NONE',  ( -21.07946286933445279, 6.329037319018855356, -33.42331615674359568 ) ) ;
#243019 = CARTESIAN_POINT ( 'NONE',  ( 19.97071067811864609, 31.48319315813861863, -233.4822683806297903 ) ) ;
#243021 = CIRCLE ( 'NONE', #251404, 0.09999999999999976963 ) ;
#243022 = CARTESIAN_POINT ( 'NONE',  ( -21.45000000000000284, 68.29142135624881860, -48.27310748452437394 ) ) ;
#243023 = ORIENTED_EDGE ( 'NONE', *, *, #110386, .F. ) ;
#243024 = CIRCLE ( 'NONE', #76424, 0.09999999999998898659 ) ;
#243025 = DIRECTION ( 'NONE',  ( 0.000000000000000000, -8.881784197001263367E-15, -1.000000000000000000 ) ) ;
#243026 = DIRECTION ( 'NONE',  ( 2.915501640297156255E-16, 1.000000000000000000, 6.997203936713175802E-15 ) ) ;
#243027 = EDGE_CURVE ( 'NONE', #12745, #34181, #237680, .T. ) ;
#243028 = CARTESIAN_POINT ( 'NONE',  ( -21.14999999999994174, 76.00000000001119815, -31.87310748452479459 ) ) ;
#243029 = DIRECTION ( 'NONE',  ( 1.000000000000000000, -0.000000000000000000, -0.000000000000000000 ) ) ;
#243030 = EDGE_CURVE ( 'NONE', #147164, #7536, #120990, .T. ) ;
#243031 = ORIENTED_EDGE ( 'NONE', *, *, #30866, .F. ) ;
#243032 = ADVANCED_FACE ( 'NONE', ( #106445 ), #162614, .F. ) ;
#243033 = AXIS2_PLACEMENT_3D ( 'NONE', #249148, #107028, #69231 ) ;
#243034 = ORIENTED_EDGE ( 'NONE', *, *, #45419, .F. ) ;
#243035 = CARTESIAN_POINT ( 'NONE',  ( 23.14999999999999858, 70.50000000001230660, -157.6178414656113205 ) ) ;
#243037 = AXIS2_PLACEMENT_3D ( 'NONE', #90896, #89603, #229134 ) ;
#243036 = DIRECTION ( 'NONE',  ( 0.000000000000000000, 6.982962677686266711E-15, -1.000000000000000000 ) ) ;
#243038 = DIRECTION ( 'NONE',  ( 1.000000000000000000, -0.000000000000000000, -0.000000000000000000 ) ) ;
#243039 = CARTESIAN_POINT ( 'NONE',  ( 17.23472005113827166, 65.69211804551122214, -114.4765306244556768 ) ) ;
#243040 = CARTESIAN_POINT ( 'NONE',  ( 18.39999999999999503, 64.25000000001159606, -56.87310748452440379 ) ) ;
#243041 = DIRECTION ( 'NONE',  ( -1.000000000000000000, -0.000000000000000000, -0.000000000000000000 ) ) ;
#243042 = CIRCLE ( 'NONE', #251431, 0.09999999999999939493 ) ;
#243043 = CIRCLE ( 'NONE', #180704, 0.5000000000000004441 ) ;
#243045 = VERTEX_POINT ( 'NONE', #3513 ) ;
#243044 = CARTESIAN_POINT ( 'NONE',  ( 21.13920837816993270, 8.783247050131068434, -179.7499999999999716 ) ) ;
#243046 = CIRCLE ( 'NONE', #47216, 0.1000000000000026007 ) ;
#243047 = LINE ( 'NONE', #126962, #10198 ) ;
#243049 = EDGE_CURVE ( 'NONE', #196167, #37642, #100082, .T. ) ;
#243048 = DIRECTION ( 'NONE',  ( 0.000000000000000000, 0.000000000000000000, -1.000000000000000000 ) ) ;
#243050 = CARTESIAN_POINT ( 'NONE',  ( -23.25000000000000000, 1.115600667400684642E-11, -67.00000000000004263 ) ) ;
#243051 = DIRECTION ( 'NONE',  ( -1.000000000000000000, -3.265361837132813093E-16, 0.000000000000000000 ) ) ;
#243052 = DIRECTION ( 'NONE',  ( 0.000000000000000000, -1.000000000000000000, 0.000000000000000000 ) ) ;
#243054 = EDGE_LOOP ( 'NONE', ( #252184, #172371, #92663, #86675 ) ) ;
#243053 = DIRECTION ( 'NONE',  ( 0.000000000000000000, 0.000000000000000000, -1.000000000000000000 ) ) ;
#243055 = CARTESIAN_POINT ( 'NONE',  ( -22.10000000000000497, 10.88519226655716565, -15.14794223642649840 ) ) ;
#243056 = CARTESIAN_POINT ( 'NONE',  ( 21.05193202509564898, 10.72393601970834354, -179.6725346033257154 ) ) ;
#243057 = CARTESIAN_POINT ( 'NONE',  ( -20.94999999999999929, 16.52766025697963315, -240.8672687545768270 ) ) ;
#243058 = DIRECTION ( 'NONE',  ( 0.000000000000000000, -1.000000000000000000, -1.734723475976807292E-15 ) ) ;
#243059 = VERTEX_POINT ( 'NONE', #83026 ) ;
#243060 = CARTESIAN_POINT ( 'NONE',  ( -15.51798037960204546, 66.62334006147872856, -152.3949149363072024 ) ) ;
#243061 = DIRECTION ( 'NONE',  ( 0.000000000000000000, 0.1298341882520022972, 0.9915357197604853789 ) ) ;
#243062 = DIRECTION ( 'NONE',  ( 0.000000000000000000, -1.000000000000000000, -6.982962677686265922E-15 ) ) ;
#243063 = ADVANCED_FACE ( 'NONE', ( #63484 ), #203004, .T. ) ;
#243064 = CARTESIAN_POINT ( 'NONE',  ( -18.58693740092205005, 78.17469254045161620, -231.4408793351767315 ) ) ;
#243065 = AXIS2_PLACEMENT_3D ( 'NONE', #104610, #160803, #19995 ) ;
#243067 = ORIENTED_EDGE ( 'NONE', *, *, #51746, .F. ) ;
#243066 = AXIS2_PLACEMENT_3D ( 'NONE', #190914, #72233, #136014 ) ;
#243068 = DIRECTION ( 'NONE',  ( -0.000000000000000000, 0.2617529984165031243, 0.9651348961777157509 ) ) ;
#243069 = AXIS2_PLACEMENT_3D ( 'NONE', #102629, #218737, #119673 ) ;
#243070 = CIRCLE ( 'NONE', #68302, 11.80000000000000426 ) ;
#243071 = ORIENTED_EDGE ( 'NONE', *, *, #216633, .T. ) ;
#243072 = DIRECTION ( 'NONE',  ( 1.000000000000000000, 0.000000000000000000, 0.000000000000000000 ) ) ;
#243073 = CARTESIAN_POINT ( 'NONE',  ( -18.39999999999999858, -9.499999999988849808, -140.9992856778388841 ) ) ;
#243074 = EDGE_CURVE ( 'NONE', #199629, #1028, #150201, .T. ) ;
#243075 = PLANE ( 'NONE',  #249648 ) ;
#243076 = DIRECTION ( 'NONE',  ( 0.000000000000000000, 2.664535259100375697E-15, -1.000000000000000000 ) ) ;
#243077 = ORIENTED_EDGE ( 'NONE', *, *, #238577, .T. ) ;
#243078 = EDGE_CURVE ( 'NONE', #207248, #127786, #223838, .T. ) ;
#243079 = CARTESIAN_POINT ( 'NONE',  ( 21.05000000000000071, 0.000000000000000000, -30.59999999999999432 ) ) ;
#243080 = DIRECTION ( 'NONE',  ( -1.000000000000000000, 9.012599976028471648E-15, 6.882867235861662930E-14 ) ) ;
#243081 = ADVANCED_FACE ( 'NONE', ( #204279 ), #112901, .F. ) ;
#243082 = DIRECTION ( 'NONE',  ( 6.484947573744954877E-15, 0.9274965247785529332, -0.3738317757009255171 ) ) ;
#243083 = DIRECTION ( 'NONE',  ( 0.000000000000000000, 0.000000000000000000, 1.000000000000000000 ) ) ;
#243084 = CARTESIAN_POINT ( 'NONE',  ( 18.53317502108576420, 10.32263460347359718, -206.5605957968671760 ) ) ;
#243085 = EDGE_LOOP ( 'NONE', ( #135628, #229142, #239069, #215357 ) ) ;
#243087 = ORIENTED_EDGE ( 'NONE', *, *, #144061, .T. ) ;
#243086 = FACE_OUTER_BOUND ( 'NONE', #73733, .T. ) ;
#243088 = EDGE_CURVE ( 'NONE', #140889, #61685, #188575, .T. ) ;
#243089 = ORIENTED_EDGE ( 'NONE', *, *, #158525, .T. ) ;
#243090 = AXIS2_PLACEMENT_3D ( 'NONE', #194409, #15780, #116144 ) ;
#243091 = LINE ( 'NONE', #100963, #36421 ) ;
#243092 = ADVANCED_FACE ( 'NONE', ( #128618 ), #167764, .F. ) ;
#243093 = ORIENTED_EDGE ( 'NONE', *, *, #156202, .T. ) ;
#243094 = CARTESIAN_POINT ( 'NONE',  ( 21.05563370358598263, 65.27576964416554972, -124.3400166685613044 ) ) ;
#243095 = CARTESIAN_POINT ( 'NONE',  ( -21.05000000000000071, 6.299230910103437608, -100.4015624999997414 ) ) ;
#243096 = CARTESIAN_POINT ( 'NONE',  ( 21.05000000000000071, 71.00000000001199396, -114.9283735034374274 ) ) ;
#243097 = ORIENTED_EDGE ( 'NONE', *, *, #158867, .T. ) ;
#243098 = CARTESIAN_POINT ( 'NONE',  ( -16.94107738177415712, 65.98576071487495653, -56.97310748452439810 ) ) ;
#243099 = CARTESIAN_POINT ( 'NONE',  ( -20.85000000000000142, 11.64999999999999680, -26.71613433702190576 ) ) ;
#243100 = VERTEX_POINT ( 'NONE', #110325 ) ;
#243101 = CARTESIAN_POINT ( 'NONE',  ( -23.25000000000000000, 76.00000000001162448, -65.37310748452432563 ) ) ;
#243103 = VERTEX_POINT ( 'NONE', #231572 ) ;
#243102 = DIRECTION ( 'NONE',  ( 1.000000000000000000, 0.000000000000000000, 0.000000000000000000 ) ) ;
#243104 = CARTESIAN_POINT ( 'NONE',  ( -21.05000000000000071, 74.26374286841520700, -191.9544551555068779 ) ) ;
#243105 = CARTESIAN_POINT ( 'NONE',  ( -23.25000000000000000, 64.35000000001198828, -115.2731074845243739 ) ) ;
#243106 = CIRCLE ( 'NONE', #205501, 12.97499999999999964 ) ;
#243107 = ADVANCED_FACE ( 'NONE', ( #212014 ), #225166, .F. ) ;
#243108 = VECTOR ( 'NONE', #46806, 1000.000000000000000 ) ;
#243109 = EDGE_CURVE ( 'NONE', #110910, #74710, #111617, .T. ) ;
#243110 = VERTEX_POINT ( 'NONE', #129877 ) ;
#243111 = AXIS2_PLACEMENT_3D ( 'NONE', #223700, #45083, #124626 ) ;
#243112 = DIRECTION ( 'NONE',  ( 0.000000000000000000, -1.000000000000000000, -6.982962677686265922E-15 ) ) ;
#243113 = DIRECTION ( 'NONE',  ( -1.000000000000000000, 0.000000000000000000, 0.000000000000000000 ) ) ;
#243114 = CARTESIAN_POINT ( 'NONE',  ( -20.54999999999999716, 46.15118611352045974, -240.5321844900040844 ) ) ;
#243115 = ORIENTED_EDGE ( 'NONE', *, *, #49272, .T. ) ;
#243116 = DIRECTION ( 'NONE',  ( 0.000000000000000000, 1.000000000000000000, 0.000000000000000000 ) ) ;
#243117 = EDGE_CURVE ( 'NONE', #92109, #153564, #166484, .T. ) ;
#243118 = CARTESIAN_POINT ( 'NONE',  ( 20.94999999999999574, 10.62357026049396680, -40.99194520323055713 ) ) ;
#243119 = ORIENTED_EDGE ( 'NONE', *, *, #241935, .F. ) ;
#243120 = EDGE_CURVE ( 'NONE', #103596, #45717, #244753, .T. ) ;
#243121 = VECTOR ( 'NONE', #90459, 1000.000000000000000 ) ;
#243122 = EDGE_CURVE ( 'NONE', #217224, #152168, #154340, .T. ) ;
#243123 = VECTOR ( 'NONE', #234830, 1000.000000000000000 ) ;
#243124 = CIRCLE ( 'NONE', #176515, 0.09999999999998898659 ) ;
#243125 = ORIENTED_EDGE ( 'NONE', *, *, #223004, .F. ) ;
#243126 = CYLINDRICAL_SURFACE ( 'NONE', #244216, 0.09999999999999939493 ) ;
#243127 = AXIS2_PLACEMENT_3D ( 'NONE', #75503, #16806, #233292 ) ;
#243128 = ADVANCED_FACE ( 'NONE', ( #208164 ), #249842, .F. ) ;
#243129 = ORIENTED_EDGE ( 'NONE', *, *, #123212, .T. ) ;
#243130 = CARTESIAN_POINT ( 'NONE',  ( 18.59999999999999432, 77.13501884592155022, -28.30613060109199353 ) ) ;
#243131 = CARTESIAN_POINT ( 'NONE',  ( -16.77180007708462028, 66.05000000001255955, -182.6587216034792505 ) ) ;
#243133 = EDGE_LOOP ( 'NONE', ( #45098, #124894, #178628, #248250 ) ) ;
#243132 = DIRECTION ( 'NONE',  ( 0.000000000000000000, 0.9908441862701600211, -0.1350103645451876666 ) ) ;
#243134 = CARTESIAN_POINT ( 'NONE',  ( 21.14999999999999858, 87.75000000001156764, -57.27310748452423894 ) ) ;
#243135 = CARTESIAN_POINT ( 'NONE',  ( 21.13461538461538325, 10.61458296203669249, -112.8500000000000369 ) ) ;
#243136 = CARTESIAN_POINT ( 'NONE',  ( 21.07928932188134397, 75.90110485435729970, -75.85162414091763594 ) ) ;
#243137 = DIRECTION ( 'NONE',  ( -1.000000000000000000, 2.952720810173289112E-16, 2.061873921506763405E-30 ) ) ;
#243138 = EDGE_CURVE ( 'NONE', #166912, #150964, #75195, .T. ) ;
#243139 = CARTESIAN_POINT ( 'NONE',  ( -18.41353343127310538, 85.50000000001207923, -129.4910380878245064 ) ) ;
#243140 = AXIS2_PLACEMENT_3D ( 'NONE', #210587, #233992, #252265 ) ;
#243141 = CARTESIAN_POINT ( 'NONE',  ( 11.60000000000000142, -8.250000000000003553, 17.60000000000000497 ) ) ;
#243142 = CIRCLE ( 'NONE', #55670, 0.09999999999999741040 ) ;
#243144 = VERTEX_POINT ( 'NONE', #68645 ) ;
#243143 = DIRECTION ( 'NONE',  ( 0.000000000000000000, 1.000000000000000000, 6.938893903907222067E-15 ) ) ;
#243146 = VERTEX_POINT ( 'NONE', #209420 ) ;
#243145 = CARTESIAN_POINT ( 'NONE',  ( -23.15000000000000213, 64.25000000001219291, -143.3647081744214802 ) ) ;
#243148 = DIRECTION ( 'NONE',  ( 0.000000000000000000, 0.000000000000000000, -1.000000000000000000 ) ) ;
#243147 = CIRCLE ( 'NONE', #230889, 4.000000000000003553 ) ;
#243149 = EDGE_LOOP ( 'NONE', ( #136578, #217893, #43219, #189676 ) ) ;
#243150 = DIRECTION ( 'NONE',  ( 1.000000000000000000, 0.000000000000000000, 0.000000000000000000 ) ) ;
#243151 = TOROIDAL_SURFACE ( 'NONE', #147482, 6.258578643762700899, 0.1000000000000000056 ) ;
#243152 = DIRECTION ( 'NONE',  ( 0.000000000000000000, 0.000000000000000000, 1.000000000000000000 ) ) ;
#243153 = TOROIDAL_SURFACE ( 'NONE', #76560, 0.4000000000000012990, 0.1000000000000000056 ) ;
#243154 = DIRECTION ( 'NONE',  ( 0.000000000000000000, 0.1495327102803792052, -0.9887567792719320625 ) ) ;
#243155 = DIRECTION ( 'NONE',  ( -1.000000000000000000, 0.000000000000000000, -0.000000000000000000 ) ) ;
#243156 = CIRCLE ( 'NONE', #130731, 0.09999999999999939493 ) ;
#243158 = ORIENTED_EDGE ( 'NONE', *, *, #254971, .F. ) ;
#243157 = AXIS2_PLACEMENT_3D ( 'NONE', #232255, #128004, #9327 ) ;
#243160 = TOROIDAL_SURFACE ( 'NONE', #143396, 0.2000000000000000111, 0.1000000000000000056 ) ;
#243159 = CARTESIAN_POINT ( 'NONE',  ( -20.85000000000000142, 87.75000000001190870, -103.0231074845242176 ) ) ;
#243161 = LINE ( 'NONE', #80201, #131596 ) ;
#243162 = EDGE_LOOP ( 'NONE', ( #193263, #88826, #206931, #60774 ) ) ;
#243163 = PLANE ( 'NONE',  #14461 ) ;
#243164 = CARTESIAN_POINT ( 'NONE',  ( 20.94999999999999929, 87.29603075034673054, -39.07100664418810965 ) ) ;
#243165 = ORIENTED_EDGE ( 'NONE', *, *, #246410, .F. ) ;
#243166 = EDGE_CURVE ( 'NONE', #226840, #5761, #4600, .T. ) ;
#243167 = DIRECTION ( 'NONE',  ( 0.000000000000000000, -6.938893903907222067E-15, 1.000000000000000000 ) ) ;
#243168 = EDGE_LOOP ( 'NONE', ( #215990, #24714, #165943, #95539 ) ) ;
#243169 = DIRECTION ( 'NONE',  ( 1.000000000000000000, 0.000000000000000000, -0.000000000000000000 ) ) ;
#243170 = VERTEX_POINT ( 'NONE', #107756 ) ;
#243171 = FACE_OUTER_BOUND ( 'NONE', #27333, .T. ) ;
#243172 = FACE_OUTER_BOUND ( 'NONE', #94151, .T. ) ;
#243173 = ORIENTED_EDGE ( 'NONE', *, *, #137075, .F. ) ;
#243174 = AXIS2_PLACEMENT_3D ( 'NONE', #4529, #10650, #121933 ) ;
#243175 = CARTESIAN_POINT ( 'NONE',  ( -21.44999999999999929, 7.250000000011155521, -155.2500000000000284 ) ) ;
#243177 = ORIENTED_EDGE ( 'NONE', *, *, #71146, .T. ) ;
#243176 = CARTESIAN_POINT ( 'NONE',  ( -21.78635804494510708, 7.035661485164336426, -100.4009949344923456 ) ) ;
#243178 = EDGE_CURVE ( 'NONE', #90063, #199384, #79614, .T. ) ;
#243179 = AXIS2_PLACEMENT_3D ( 'NONE', #162960, #63842, #139510 ) ;
#243180 = CARTESIAN_POINT ( 'NONE',  ( 20.94999999999999929, 40.68212387350988735, -238.0221676322813096 ) ) ;
#243181 = ORIENTED_EDGE ( 'NONE', *, *, #44341, .T. ) ;
#243182 = AXIS2_PLACEMENT_3D ( 'NONE', #82132, #106845, #239964 ) ;
#243183 = VECTOR ( 'NONE', #132659, 1000.000000000000227 ) ;
#243184 = ORIENTED_EDGE ( 'NONE', *, *, #152466, .F. ) ;
#243185 = LINE ( 'NONE', #223607, #111748 ) ;
#243186 = CARTESIAN_POINT ( 'NONE',  ( 19.75857864376269291, 64.25000000001250555, -178.6731074845244507 ) ) ;
#243187 = LINE ( 'NONE', #24169, #169775 ) ;
#243188 = VECTOR ( 'NONE', #68610, 1000.000000000000000 ) ;
#243189 = CYLINDRICAL_SURFACE ( 'NONE', #85438, 0.09999999999999939493 ) ;
#243190 = DIRECTION ( 'NONE',  ( 0.000000000000000000, 0.000000000000000000, -1.000000000000000000 ) ) ;
#243191 = VERTEX_POINT ( 'NONE', #11234 ) ;
#243192 = DIRECTION ( 'NONE',  ( 1.000000000000000000, -7.304098846218134667E-16, -5.100424963727256530E-30 ) ) ;
#243193 = VECTOR ( 'NONE', #190176, 1000.000000000000000 ) ;
#243194 = DIRECTION ( 'NONE',  ( -1.000000000000000000, 0.000000000000000000, 0.000000000000000000 ) ) ;
#243195 = DIRECTION ( 'NONE',  ( 0.000000000000000000, 0.000000000000000000, 1.000000000000000000 ) ) ;
#243196 = DIRECTION ( 'NONE',  ( -0.7071067811865487940, -0.7071067811865463515, -4.937700262164522799E-15 ) ) ;
#243197 = ORIENTED_EDGE ( 'NONE', *, *, #252434, .F. ) ;
#243198 = ORIENTED_EDGE ( 'NONE', *, *, #20655, .F. ) ;
#243199 = CARTESIAN_POINT ( 'NONE',  ( 14.45204356427541548, 9.450668889178684751, -115.5555464902073766 ) ) ;
#243201 = ORIENTED_EDGE ( 'NONE', *, *, #149391, .F. ) ;
#243200 = CIRCLE ( 'NONE', #189052, 0.09999999999999939493 ) ;
#243202 = CARTESIAN_POINT ( 'NONE',  ( -15.75000000000000711, 26.10747769360538229, -233.2920644364424732 ) ) ;
#243203 = CARTESIAN_POINT ( 'NONE',  ( -20.85882249326303040, 10.33248238083634796, -72.59484654391314962 ) ) ;
#243204 = ORIENTED_EDGE ( 'NONE', *, *, #253283, .F. ) ;
#243206 = ORIENTED_EDGE ( 'NONE', *, *, #210402, .F. ) ;
#243205 = DIRECTION ( 'NONE',  ( 0.000000000000000000, 0.000000000000000000, -1.000000000000000000 ) ) ;
#243207 = SPHERICAL_SURFACE ( 'NONE', #54744, 0.1000000000000000056 ) ;
#243208 = ORIENTED_EDGE ( 'NONE', *, *, #249338, .F. ) ;
#243209 = CIRCLE ( 'NONE', #89273, 0.1999999999999996503 ) ;
#243210 = CARTESIAN_POINT ( 'NONE',  ( 20.95000000000005258, 64.25000000001119815, -30.12310748452479103 ) ) ;
#243211 = EDGE_CURVE ( 'NONE', #187354, #61933, #54503, .T. ) ;
#243212 = DIRECTION ( 'NONE',  ( -1.836970198721029934E-16, 1.000000000000000000, 0.000000000000000000 ) ) ;
#243213 = EDGE_LOOP ( 'NONE', ( #146152, #137622, #104641, #240327 ) ) ;
#243214 = VECTOR ( 'NONE', #132286, 1000.000000000000000 ) ;
#243215 = EDGE_CURVE ( 'NONE', #104618, #154183, #150743, .T. ) ;
#243216 = CARTESIAN_POINT ( 'NONE',  ( -16.87036670365549895, 66.01058118071041747, -124.0026676018264169 ) ) ;
#243218 = ORIENTED_EDGE ( 'NONE', *, *, #249071, .F. ) ;
#243217 = AXIS2_PLACEMENT_3D ( 'NONE', #149953, #226895, #110797 ) ;
#243219 = VERTEX_POINT ( 'NONE', #148167 ) ;
#243220 = TOROIDAL_SURFACE ( 'NONE', #218268, 0.2000000000000000111, 0.1000000000000000056 ) ;
#243221 = TOROIDAL_SURFACE ( 'NONE', #147380, 0.6000000000000009770, 0.1000000000000000056 ) ;
#243222 = FACE_OUTER_BOUND ( 'NONE', #148263, .T. ) ;
#243223 = EDGE_CURVE ( 'NONE', #182849, #119449, #150384, .T. ) ;
#243224 =( BOUNDED_CURVE ( )  B_SPLINE_CURVE ( 3, ( #53867, #113831, #12195, #87824 ),
 .UNSPECIFIED., .F., .F. ) 
 B_SPLINE_CURVE_WITH_KNOTS ( ( 4, 4 ),
 ( 1.570796326794908992, 2.617993877991549034 ),
 .UNSPECIFIED. ) 
 CURVE ( )  GEOMETRIC_REPRESENTATION_ITEM ( )  RATIONAL_B_SPLINE_CURVE ( ( 1.000000000000000000, 0.9106836025229521070, 0.9106836025229521070, 1.000000000000000000 ) ) 
 REPRESENTATION_ITEM ( '' )  );
#243225 = EDGE_CURVE ( 'NONE', #113073, #6953, #49063, .T. ) ;
#243227 = ORIENTED_EDGE ( 'NONE', *, *, #201265, .F. ) ;
#243226 = DIRECTION ( 'NONE',  ( 1.000000000000000000, 0.000000000000000000, 0.000000000000000000 ) ) ;
#243228 = DIRECTION ( 'NONE',  ( 0.000000000000000000, -0.8814952561688430555, 0.4721928772777346239 ) ) ;
#243229 = CYLINDRICAL_SURFACE ( 'NONE', #240053, 0.1000000000000008937 ) ;
#243231 = DIRECTION ( 'NONE',  ( -0.8191520442889921316, -0.5735764363510457153, 0.000000000000000000 ) ) ;
#243230 = CARTESIAN_POINT ( 'NONE',  ( -23.15000000000000213, 64.25000000001205080, -124.3731074845243825 ) ) ;
#243232 = CARTESIAN_POINT ( 'NONE',  ( 21.05000000000000071, 10.62872031401550288, -108.1649135690876449 ) ) ;
#243233 = CARTESIAN_POINT ( 'NONE',  ( -18.59999999999999787, 61.53642629385834795, -221.5144953033309321 ) ) ;
#243234 = B_SPLINE_CURVE_WITH_KNOTS ( 'NONE', 3,
 ( #65383, #144902, #204880, #146195, #105768, #66677, #225716, #47083, #206183, #180214, #1546, #81078, #233158, #75367, #36237, #87497 ),
 .UNSPECIFIED., .F., .F.,
 ( 4, 3, 3, 3, 3, 4 ),
 ( 0.000000000000000000, 3.357088238234077717E-05, 6.714213034887153676E-05, 0.0001007408646120950283, 0.0001343627955914246212, 0.0001573956632896022318 ),
 .UNSPECIFIED. ) ;
#243235 = EDGE_CURVE ( 'NONE', #166959, #16861, #175338, .T. ) ;
#243236 = CARTESIAN_POINT ( 'NONE',  ( -20.94999999999999929, -11.48912529306490349, -103.5000000000000426 ) ) ;
#243237 = CIRCLE ( 'NONE', #84413, 11.65000000000000036 ) ;
#243238 = PLANE ( 'NONE',  #38409 ) ;
#243239 = CIRCLE ( 'NONE', #201549, 0.09999999999998898659 ) ;
#243240 = CIRCLE ( 'NONE', #130832, 0.09999999999999939493 ) ;
#243241 = ORIENTED_EDGE ( 'NONE', *, *, #241662, .F. ) ;
#243242 = ORIENTED_EDGE ( 'NONE', *, *, #139149, .F. ) ;
#243243 = CYLINDRICAL_SURFACE ( 'NONE', #122820, 4.000000000000003553 ) ;
#243244 = VERTEX_POINT ( 'NONE', #175463 ) ;
#243245 = EDGE_CURVE ( 'NONE', #32089, #18615, #137874, .T. ) ;
#243246 = CARTESIAN_POINT ( 'NONE',  ( -16.87331047859651179, 9.950000000011142376, -146.6500000000000341 ) ) ;
#243247 = EDGE_LOOP ( 'NONE', ( #28445, #47611, #154910, #3159 ) ) ;
#243248 = DIRECTION ( 'NONE',  ( 0.000000000000000000, 0.000000000000000000, 1.000000000000000000 ) ) ;
#243249 = ORIENTED_EDGE ( 'NONE', *, *, #180106, .T. ) ;
#243250 = CARTESIAN_POINT ( 'NONE',  ( -21.07946286933443503, 6.167755875232504792, -199.5782471168023449 ) ) ;
#243251 = EDGE_LOOP ( 'NONE', ( #16573, #77950, #30523, #150493 ) ) ;
#243252 = ORIENTED_EDGE ( 'NONE', *, *, #211451, .T. ) ;
#243253 = CARTESIAN_POINT ( 'NONE',  ( -16.86422026484316916, 9.970447360871808939, -46.08221322567300149 ) ) ;
#243254 = AXIS2_PLACEMENT_3D ( 'NONE', #179967, #241227, #144662 ) ;
#243255 = CARTESIAN_POINT ( 'NONE',  ( -21.14999999999999858, 76.00000000001200817, -109.5637644362255543 ) ) ;
#243257 = ORIENTED_EDGE ( 'NONE', *, *, #108035, .T. ) ;
#243256 = DIRECTION ( 'NONE',  ( -1.000000000000000000, -0.000000000000000000, -0.000000000000000000 ) ) ;
#243258 = CARTESIAN_POINT ( 'NONE',  ( 20.94999675878240808, 65.70692517833232671, -97.56446533783034170 ) ) ;
#243260 = VERTEX_POINT ( 'NONE', #153356 ) ;
#243259 = CARTESIAN_POINT ( 'NONE',  ( -23.25000000000000000, 4.350000000011156054, -179.6499999999999773 ) ) ;
#243261 = CARTESIAN_POINT ( 'NONE',  ( 20.04142135391667168, 11.75000000001116263, -125.2025068656295588 ) ) ;
#243262 = EDGE_LOOP ( 'NONE', ( #87718, #78784, #244120, #125734, #200333 ) ) ;
#243263 = DIRECTION ( 'NONE',  ( -0.000000000000000000, -0.2128009952263603677, 0.9770955615653313941 ) ) ;
#243266 = ADVANCED_FACE ( 'NONE', ( #237968 ), #193725, .F. ) ;
#243265 = ORIENTED_EDGE ( 'NONE', *, *, #106361, .F. ) ;
#243264 = DIRECTION ( 'NONE',  ( 1.734723475976823250E-13, 0.7899159663865635839, 0.6132151058540398214 ) ) ;
#243267 = CARTESIAN_POINT ( 'NONE',  ( 18.52643265882457868, 10.31973158071402885, -173.0505334713354841 ) ) ;
#243268 = CARTESIAN_POINT ( 'NONE',  ( -12.42749937872396693, 27.00310224281248495, -233.7483545961832476 ) ) ;
#243269 = CARTESIAN_POINT ( 'NONE',  ( 23.25000000000000000, 85.00000000001261924, -193.6291383618718385 ) ) ;
#243270 = ORIENTED_EDGE ( 'NONE', *, *, #36871, .F. ) ;
#243272 = CARTESIAN_POINT ( 'NONE',  ( 20.52683494730037239, 8.980530818312608687, -109.0052527225372359 ) ) ;
#243271 = DIRECTION ( 'NONE',  ( 0.000000000000000000, -0.9126074666063770380, -0.4088369013363281068 ) ) ;
#243273 = DIRECTION ( 'NONE',  ( 1.000000000000000000, 0.000000000000000000, -0.000000000000000000 ) ) ;
#243274 = AXIS2_PLACEMENT_3D ( 'NONE', #30249, #34125, #210165 ) ;
#243275 = CARTESIAN_POINT ( 'NONE',  ( -20.54999999999999716, 67.23127455305835554, -235.8551265064784559 ) ) ;
#243276 = AXIS2_PLACEMENT_3D ( 'NONE', #170363, #226408, #47774 ) ;
#243277 = DIRECTION ( 'NONE',  ( 0.7071067811865474617, 0.7071067811865474617, 2.044391222244499837E-16 ) ) ;
#243278 = CARTESIAN_POINT ( 'NONE',  ( -16.92209698673566010, 44.19081817725273709, -235.2741415492630495 ) ) ;
#243279 = ORIENTED_EDGE ( 'NONE', *, *, #167054, .F. ) ;
#243281 = ORIENTED_EDGE ( 'NONE', *, *, #138533, .T. ) ;
#243280 = CIRCLE ( 'NONE', #243473, 4.100000000000009415 ) ;
#243282 = ORIENTED_EDGE ( 'NONE', *, *, #144941, .T. ) ;
#243283 = VECTOR ( 'NONE', #80335, 1000.000000000000000 ) ;
#243284 = EDGE_CURVE ( 'NONE', #161574, #249634, #108672, .T. ) ;
#243285 = FACE_OUTER_BOUND ( 'NONE', #179331, .T. ) ;
#243286 = EDGE_LOOP ( 'NONE', ( #194160, #191065 ) ) ;
#243287 = DIRECTION ( 'NONE',  ( -0.000000000000000000, -0.000000000000000000, 1.000000000000000000 ) ) ;
#243288 = ORIENTED_EDGE ( 'NONE', *, *, #30228, .F. ) ;
#243289 = DIRECTION ( 'NONE',  ( 0.000000000000000000, 0.000000000000000000, -1.000000000000000000 ) ) ;
#243290 = CARTESIAN_POINT ( 'NONE',  ( -18.50000000000000000, 1.115600667400684642E-11, -67.00000000000004263 ) ) ;
#243291 = EDGE_CURVE ( 'NONE', #80949, #255841, #221085, .T. ) ;
#243292 = VERTEX_POINT ( 'NONE', #119324 ) ;
#243293 = AXIS2_PLACEMENT_3D ( 'NONE', #39205, #194424, #56153 ) ;
#243294 = CARTESIAN_POINT ( 'NONE',  ( 15.75000000000000000, 9.350000000011135626, -150.8657431672739619 ) ) ;
#243295 = FILL_AREA_STYLE ('',( #180778 ) ) ;
#243296 = EDGE_CURVE ( 'NONE', #235293, #1901, #254389, .T. ) ;
#243297 = CIRCLE ( 'NONE', #126793, 0.09999999999998898659 ) ;
#243298 = ORIENTED_EDGE ( 'NONE', *, *, #92982, .T. ) ;
#243299 = ORIENTED_EDGE ( 'NONE', *, *, #125992, .T. ) ;
#243300 = ORIENTED_EDGE ( 'NONE', *, *, #100042, .T. ) ;
#243301 = AXIS2_PLACEMENT_3D ( 'NONE', #253783, #73917, #214667 ) ;
#243302 = LINE ( 'NONE', #167653, #242011 ) ;
#243303 = DIRECTION ( 'NONE',  ( 0.000000000000000000, 0.2128009952263618110, -0.9770955615653312831 ) ) ;
#243304 = DIRECTION ( 'NONE',  ( -1.000000000000000000, 2.952720810173289112E-16, 2.061873921506763405E-30 ) ) ;
#243305 = CIRCLE ( 'NONE', #14402, 0.1000000000000096922 ) ;
#243306 = CARTESIAN_POINT ( 'NONE',  ( 15.31784899511109899, 27.35084141791447010, -233.9052011656356171 ) ) ;
#243307 = DIRECTION ( 'NONE',  ( 0.000000000000000000, 0.000000000000000000, -1.000000000000000000 ) ) ;
#243308 = DIRECTION ( 'NONE',  ( -1.000000000000000000, 7.492892343619937423E-30, -1.073024830501117725E-15 ) ) ;
#243309 = EDGE_CURVE ( 'NONE', #192117, #189211, #158774, .T. ) ;
#243311 = CARTESIAN_POINT ( 'NONE',  ( 20.94999999999999574, 0.3882413827466408840, -209.1776850584169551 ) ) ;
#243310 = FACE_OUTER_BOUND ( 'NONE', #115831, .T. ) ;
#243312 = CARTESIAN_POINT ( 'NONE',  ( 21.05000000000000071, 60.92723693130623985, -225.4208407479578113 ) ) ;
#243314 = ORIENTED_EDGE ( 'NONE', *, *, #127937, .F. ) ;
#243313 = CARTESIAN_POINT ( 'NONE',  ( -5.900000000000002132, -11.34999999999999964, 13.90000000000000213 ) ) ;
#243316 = CARTESIAN_POINT ( 'NONE',  ( -16.93658623642908267, 12.43561208657240513, -211.1991990270598478 ) ) ;
#243315 = CARTESIAN_POINT ( 'NONE',  ( 23.24999999999999645, 5.000000000011153745, -146.4052660189131245 ) ) ;
#243317 = DIRECTION ( 'NONE',  ( 1.000000000000000000, 0.000000000000000000, 0.000000000000000000 ) ) ;
#243318 = ORIENTED_EDGE ( 'NONE', *, *, #224744, .T. ) ;
#243319 = CARTESIAN_POINT ( 'NONE',  ( 20.95575313997065336, 10.61455330328599089, -74.62129070194487213 ) ) ;
#243321 = VECTOR ( 'NONE', #49923, 1000.000000000000000 ) ;
#243320 = CARTESIAN_POINT ( 'NONE',  ( 22.50014994444006788, 64.25028026811989434, -103.1061876412436504 ) ) ;
#243323 = EDGE_CURVE ( 'NONE', #129511, #204776, #118030, .T. ) ;
#243322 = LINE ( 'NONE', #84196, #91564 ) ;
#243324 = AXIS2_PLACEMENT_3D ( 'NONE', #176741, #18924, #42354 ) ;
#243326 = ADVANCED_FACE ( 'NONE', ( #13798 ), #172919, .T. ) ;
#243325 = VERTEX_POINT ( 'NONE', #98421 ) ;
#243327 = CARTESIAN_POINT ( 'NONE',  ( -21.14999999999999858, 38.04609728753136011, -236.0545303518866547 ) ) ;
#243328 = AXIS2_PLACEMENT_3D ( 'NONE', #214006, #109300, #248842 ) ;
#243329 = CARTESIAN_POINT ( 'NONE',  ( 21.07971444708685738, 69.67020791838612581, -203.6109309208423213 ) ) ;
#243330 = DIRECTION ( 'NONE',  ( 1.000000000000000000, 0.000000000000000000, 0.000000000000000000 ) ) ;
#243331 = VERTEX_POINT ( 'NONE', #176740 ) ;
#243332 = ORIENTED_EDGE ( 'NONE', *, *, #203063, .T. ) ;
#243333 = ADVANCED_FACE ( 'NONE', ( #236681 ), #116746, .T. ) ;
#243334 = AXIS2_PLACEMENT_3D ( 'NONE', #234523, #175860, #97551 ) ;
#243335 = LINE ( 'NONE', #42571, #144869 ) ;
#243336 = ORIENTED_EDGE ( 'NONE', *, *, #80845, .F. ) ;
#243337 = CARTESIAN_POINT ( 'NONE',  ( 11.60000000000006004, 64.25000000001119815, -18.32310748452479388 ) ) ;
#243338 = DIRECTION ( 'NONE',  ( -0.000000000000000000, -0.000000000000000000, -1.000000000000000000 ) ) ;
#243339 = DIRECTION ( 'NONE',  ( 1.000000000000000000, 0.000000000000000000, 0.000000000000000000 ) ) ;
#243341 = ADVANCED_FACE ( 'NONE', ( #232867 ), #55451, .T. ) ;
#243340 = FACE_OUTER_BOUND ( 'NONE', #218392, .T. ) ;
#243342 = ORIENTED_EDGE ( 'NONE', *, *, #198935, .F. ) ;
#243343 = EDGE_CURVE ( 'NONE', #161815, #169411, #187976, .T. ) ;
#243344 = CIRCLE ( 'NONE', #222476, 0.1000000000000124678 ) ;
#243345 = AXIS2_PLACEMENT_3D ( 'NONE', #250202, #187684, #9024 ) ;
#243346 = AXIS2_PLACEMENT_3D ( 'NONE', #235691, #117043, #136582 ) ;
#243347 = CARTESIAN_POINT ( 'NONE',  ( 18.59999999999999787, -8.350000000000004974, 33.00000000000000000 ) ) ;
#243348 = CARTESIAN_POINT ( 'NONE',  ( 21.00000000000000000, 66.25000000001223555, -148.8731074845244393 ) ) ;
#243349 = CARTESIAN_POINT ( 'NONE',  ( 18.39999999999999503, 64.25000000001188027, -90.37310748452439668 ) ) ;
#243350 = CARTESIAN_POINT ( 'NONE',  ( 21.10000000000000142, -11.65000000000000036, 11.99999999999999645 ) ) ;
#243351 = EDGE_LOOP ( 'NONE', ( #59558, #104032, #224896, #186591 ) ) ;
#243353 = ORIENTED_EDGE ( 'NONE', *, *, #124260, .F. ) ;
#243352 = DIRECTION ( 'NONE',  ( -1.000000000000000000, 0.000000000000000000, 0.000000000000000000 ) ) ;
#243354 = EDGE_CURVE ( 'NONE', #23723, #120532, #133606, .T. ) ;
#243355 = DIRECTION ( 'NONE',  ( 0.000000000000000000, -0.9651348961777428404, 0.2617529984164035373 ) ) ;
#243356 = DIRECTION ( 'NONE',  ( -0.000000000000000000, 1.000000000000000000, 0.000000000000000000 ) ) ;
#243357 = EDGE_CURVE ( 'NONE', #26265, #110056, #200145, .T. ) ;
#243358 = CARTESIAN_POINT ( 'NONE',  ( 22.50000000000000000, 68.20922040163827660, -69.62310748452438247 ) ) ;
#243359 = DIRECTION ( 'NONE',  ( 0.000000000000000000, 0.000000000000000000, -1.000000000000000000 ) ) ;
#243360 = CARTESIAN_POINT ( 'NONE',  ( -21.05000000000000071, 1.115600667400684642E-11, -134.0000000000000284 ) ) ;
#243361 = FACE_OUTER_BOUND ( 'NONE', #128696, .T. ) ;
#243362 = VERTEX_POINT ( 'NONE', #1915 ) ;
#243363 = DIRECTION ( 'NONE',  ( 0.000000000000000000, 0.000000000000000000, -1.000000000000000000 ) ) ;
#243364 = VECTOR ( 'NONE', #237354, 1000.000000000000000 ) ;
#243365 = DIRECTION ( 'NONE',  ( -1.000000000000000000, 0.000000000000000000, 0.000000000000000000 ) ) ;
#243367 = AXIS2_PLACEMENT_3D ( 'NONE', #163014, #177454, #237400 ) ;
#243366 = CARTESIAN_POINT ( 'NONE',  ( -21.55000000000000071, 68.65000000001187175, -90.67310748452436542 ) ) ;
#243368 = ADVANCED_FACE ( 'NONE', ( #142718 ), #21521, .T. ) ;
#243369 = AXIS2_PLACEMENT_3D ( 'NONE', #136303, #213292, #152074 ) ;
#243370 = DIRECTION ( 'NONE',  ( 1.000000000000000000, 0.000000000000000000, 0.000000000000000000 ) ) ;
#243371 = DIRECTION ( 'NONE',  ( -1.000000000000000000, -0.000000000000000000, -0.000000000000000000 ) ) ;
#243372 = ORIENTED_EDGE ( 'NONE', *, *, #60851, .F. ) ;
#243373 = ORIENTED_EDGE ( 'NONE', *, *, #55814, .T. ) ;
#243374 = DIRECTION ( 'NONE',  ( -0.000000000000000000, 1.000000000000000000, -0.000000000000000000 ) ) ;
#243375 = AXIS2_PLACEMENT_3D ( 'NONE', #127075, #224872, #48814 ) ;
#243376 = DIRECTION ( 'NONE',  ( 1.000000000000000000, -2.952720810173289112E-16, -2.061873921506763405E-30 ) ) ;
#243377 = CARTESIAN_POINT ( 'NONE',  ( 22.48970261584622321, 11.65000000000000036, 0.05536948821740608068 ) ) ;
#243378 = TOROIDAL_SURFACE ( 'NONE', #72726, 7.791421356237335338, 0.1000000000000000056 ) ;
#243379 = DIRECTION ( 'NONE',  ( 1.000000000000000000, 0.000000000000000000, -0.000000000000000000 ) ) ;
#243380 = CARTESIAN_POINT ( 'NONE',  ( -20.94999999999999929, -1.164121893230052995, -175.4148480855716059 ) ) ;
#243381 = CIRCLE ( 'NONE', #235025, 0.09999999999999938105 ) ;
#243382 = DIRECTION ( 'NONE',  ( -1.000000000000000000, 0.000000000000000000, 0.000000000000000000 ) ) ;
#243383 = EDGE_CURVE ( 'NONE', #145844, #85966, #103580, .T. ) ;
#243384 = DIRECTION ( 'NONE',  ( 0.000000000000000000, 0.9126074666063844765, 0.4088369013363113980 ) ) ;
#243385 = CIRCLE ( 'NONE', #97614, 0.1000000000000000472 ) ;
#243386 = AXIS2_PLACEMENT_3D ( 'NONE', #85460, #142879, #64649 ) ;
#243387 = CARTESIAN_POINT ( 'NONE',  ( -16.90257928357874917, 9.954106821105362712, -12.63628543011369842 ) ) ;
#243388 = ADVANCED_FACE ( 'NONE', ( #80151 ), #83990, .F. ) ;
#243389 = EDGE_LOOP ( 'NONE', ( #212182, #185509, #139436, #220783, #28726, #126457, #208359, #213559, #240194, #75461, #24162, #96046, #109694, #22704, #12054, #224422, #254186, #143349, #204424, #71258, #200791, #186501, #69882 ) ) ;
#243390 = LINE ( 'NONE', #200422, #69313 ) ;
#243391 = EDGE_CURVE ( 'NONE', #206683, #166202, #228635, .T. ) ;
#243392 = ORIENTED_EDGE ( 'NONE', *, *, #130877, .T. ) ;
#243393 = CARTESIAN_POINT ( 'NONE',  ( -21.05000000000000071, 76.00000000001170974, -76.06376443622555428 ) ) ;
#243394 = CARTESIAN_POINT ( 'NONE',  ( 21.05000000000000071, 5.850000000011156942, -90.36750277572211587 ) ) ;
#243396 = VECTOR ( 'NONE', #72142, 1000.000000000000000 ) ;
#243395 = CARTESIAN_POINT ( 'NONE',  ( 22.50000000000000000, 1.115600667400684642E-11, -33.50000000000000000 ) ) ;
#243397 = CARTESIAN_POINT ( 'NONE',  ( -21.14999999999994174, 76.00000000001119815, -3.023107484524792277 ) ) ;
#243398 = DIRECTION ( 'NONE',  ( 1.000000000000000000, 0.000000000000000000, 0.000000000000000000 ) ) ;
#243400 = ADVANCED_FACE ( 'NONE', ( #184422 ), #219689, .T. ) ;
#243399 = LINE ( 'NONE', #225099, #51970 ) ;
#243401 = LINE ( 'NONE', #225100, #245519 ) ;
#243402 = CYLINDRICAL_SURFACE ( 'NONE', #168440, 0.09999999999999939493 ) ;
#243403 = DIRECTION ( 'NONE',  ( -1.000000000000000000, 0.000000000000000000, 0.000000000000000000 ) ) ;
#243404 = FACE_OUTER_BOUND ( 'NONE', #212643, .T. ) ;
#243405 = EDGE_CURVE ( 'NONE', #91407, #116470, #29593, .T. ) ;
#243406 = DIRECTION ( 'NONE',  ( 0.000000000000000000, 0.000000000000000000, -1.000000000000000000 ) ) ;
#243407 = CARTESIAN_POINT ( 'NONE',  ( -20.64999999999999858, 71.65000000001222702, -148.7731074845243882 ) ) ;
#243408 = AXIS2_PLACEMENT_3D ( 'NONE', #156383, #132949, #138049 ) ;
#243409 = CARTESIAN_POINT ( 'NONE',  ( -18.59999999999999787, 66.65000000001187175, -90.67310748452437963 ) ) ;
#243410 = VECTOR ( 'NONE', #132615, 1000.000000000000000 ) ;
#243411 = EDGE_CURVE ( 'NONE', #151569, #654, #129526, .T. ) ;
#243412 = AXIS2_PLACEMENT_3D ( 'NONE', #98092, #177702, #57701 ) ;
#243414 = EDGE_CURVE ( 'NONE', #6865, #143962, #253536, .T. ) ;
#243413 = EDGE_CURVE ( 'NONE', #20391, #95961, #71279, .T. ) ;
#243415 = EDGE_LOOP ( 'NONE', ( #26986, #216159, #1571, #33175 ) ) ;
#243416 = DIRECTION ( 'NONE',  ( 1.000000000000000000, -0.000000000000000000, -0.000000000000000000 ) ) ;
#243417 = CARTESIAN_POINT ( 'NONE',  ( -22.39999999999999858, 64.25000000001195133, -102.9231074845243938 ) ) ;
#243418 = ORIENTED_EDGE ( 'NONE', *, *, #189132, .F. ) ;
#243419 = DIRECTION ( 'NONE',  ( 0.000000000000000000, -1.000000000000000000, -6.982962677686265922E-15 ) ) ;
#243420 = FACE_OUTER_BOUND ( 'NONE', #155074, .T. ) ;
#243421 = CARTESIAN_POINT ( 'NONE',  ( -21.05000000000000071, 76.00000000001170974, -69.52310748452431710 ) ) ;
#243422 = ORIENTED_EDGE ( 'NONE', *, *, #154409, .T. ) ;
#243423 = LINE ( 'NONE', #225127, #242059 ) ;
#243424 = CARTESIAN_POINT ( 'NONE',  ( 22.49533356619865643, 31.83654316555196928, -238.9459102234743284 ) ) ;
#243425 = ORIENTED_EDGE ( 'NONE', *, *, #56105, .F. ) ;
#243426 = EDGE_CURVE ( 'NONE', #101165, #113973, #216983, .T. ) ;
#243427 = AXIS2_PLACEMENT_3D ( 'NONE', #239091, #182979, #65578 ) ;
#243428 = EDGE_CURVE ( 'NONE', #7048, #23903, #50379, .T. ) ;
#243429 = CARTESIAN_POINT ( 'NONE',  ( -18.59999999999999787, -9.849999999999990763, 31.50000000000000000 ) ) ;
#243430 = EDGE_CURVE ( 'NONE', #10416, #240802, #128864, .T. ) ;
#243431 = AXIS2_PLACEMENT_3D ( 'NONE', #163221, #143637, #101919 ) ;
#243432 = ORIENTED_EDGE ( 'NONE', *, *, #85939, .F. ) ;
#243433 = DIRECTION ( 'NONE',  ( -0.000000000000000000, 1.000000000000000000, -0.000000000000000000 ) ) ;
#243434 = CARTESIAN_POINT ( 'NONE',  ( 22.45380639572303494, 1.426796658862355976E-07, -21.74956710889332356 ) ) ;
#243435 = EDGE_CURVE ( 'NONE', #25677, #115688, #166979, .T. ) ;
#243436 = DIRECTION ( 'NONE',  ( 1.000000000000000000, -0.000000000000000000, -0.000000000000000000 ) ) ;
#243438 = FACE_OUTER_BOUND ( 'NONE', #134349, .T. ) ;
#243437 = PRODUCT_DEFINITION_CONTEXT ( 'detailed design', #69159, 'design' ) ;
#243439 = CARTESIAN_POINT ( 'NONE',  ( -18.50000000000000000, 11.65000000001115232, -67.10000000000005116 ) ) ;
#243440 = CARTESIAN_POINT ( 'NONE',  ( 20.94999999999999574, 1.835341550235567887, -45.15515129256298366 ) ) ;
#243441 = EDGE_CURVE ( 'NONE', #156778, #20503, #127024, .T. ) ;
#243442 = CARTESIAN_POINT ( 'NONE',  ( -16.98495255085916966, 10.00556436600592214, -87.86538279377954552 ) ) ;
#243443 = DIRECTION ( 'NONE',  ( 1.000000000000000000, 0.000000000000000000, 0.000000000000000000 ) ) ;
#243444 = CARTESIAN_POINT ( 'NONE',  ( -18.50000000000000000, 9.350000000011156942, -88.35000000000003695 ) ) ;
#243446 = VERTEX_POINT ( 'NONE', #128323 ) ;
#243445 = CARTESIAN_POINT ( 'NONE',  ( 18.39999999999999858, 86.89640087696871262, -199.6396878666313341 ) ) ;
#243447 = EDGE_LOOP ( 'NONE', ( #46896, #17662, #124085, #211145 ) ) ;
#243449 = CARTESIAN_POINT ( 'NONE',  ( 18.49999999999998934, 69.35000000001259934, -191.1731074845243938 ) ) ;
#243448 = CARTESIAN_POINT ( 'NONE',  ( 23.25000000000000000, -9.599999999988845900, -143.8939691226524644 ) ) ;
#243451 = ORIENTED_EDGE ( 'NONE', *, *, #11570, .F. ) ;
#243450 = DIRECTION ( 'NONE',  ( -1.000000000000000000, 0.000000000000000000, 0.000000000000000000 ) ) ;
#243452 = ORIENTED_EDGE ( 'NONE', *, *, #52489, .F. ) ;
#243453 = DIRECTION ( 'NONE',  ( 0.000000000000000000, -7.124650136758317602E-15, 1.000000000000000000 ) ) ;
#243454 = DIRECTION ( 'NONE',  ( 1.000000000000000000, 0.000000000000000000, -0.000000000000000000 ) ) ;
#243455 = CIRCLE ( 'NONE', #131022, 0.5000000000000051070 ) ;
#243456 = AXIS2_PLACEMENT_3D ( 'NONE', #197909, #104871, #20585 ) ;
#243457 = LINE ( 'NONE', #3557, #4954 ) ;
#243458 = DIRECTION ( 'NONE',  ( 0.000000000000000000, 1.897661533703519897E-16, -1.000000000000000000 ) ) ;
#243459 = EDGE_CURVE ( 'NONE', #57195, #104231, #125441, .T. ) ;
#243460 = CARTESIAN_POINT ( 'NONE',  ( 21.05000000000000071, 69.74218538953583391, -103.1208977758331571 ) ) ;
#243461 = DIRECTION ( 'NONE',  ( 0.000000000000000000, -0.4088369013363283289, 0.9126074666063768159 ) ) ;
#243462 = DIRECTION ( 'NONE',  ( 1.000000000000000000, -3.448943450116727512E-16, -6.438528483529605672E-16 ) ) ;
#243463 = ADVANCED_FACE ( 'NONE', ( #187025 ), #111322, .F. ) ;
#243464 = ORIENTED_EDGE ( 'NONE', *, *, #215397, .T. ) ;
#243465 = VERTEX_POINT ( 'NONE', #50051 ) ;
#243466 = CARTESIAN_POINT ( 'NONE',  ( -18.59999999999999787, 76.00000000001126921, -203.5231074845248997 ) ) ;
#243467 = AXIS2_PLACEMENT_3D ( 'NONE', #230376, #127429, #68746 ) ;
#243468 = AXIS2_PLACEMENT_3D ( 'NONE', #113569, #50995, #30201 ) ;
#243469 = ORIENTED_EDGE ( 'NONE', *, *, #115650, .F. ) ;
#243470 = DIRECTION ( 'NONE',  ( 0.000000000000000000, 6.938893903907030216E-14, -1.000000000000000000 ) ) ;
#243471 = ORIENTED_EDGE ( 'NONE', *, *, #55181, .F. ) ;
#243472 = CARTESIAN_POINT ( 'NONE',  ( -16.80100914604134132, 9.943149094114721365, -154.8170441272876587 ) ) ;
#243473 = AXIS2_PLACEMENT_3D ( 'NONE', #116014, #255451, #156446 ) ;
#243474 = AXIS2_PLACEMENT_3D ( 'NONE', #240553, #118029, #237967 ) ;
#243475 = CARTESIAN_POINT ( 'NONE',  ( -20.94999999999999929, 77.25000000001189449, -95.02310748452430289 ) ) ;
#243476 = EDGE_CURVE ( 'NONE', #93920, #20493, #117057, .T. ) ;
#243477 = FACE_OUTER_BOUND ( 'NONE', #234912, .T. ) ;
#243478 = CARTESIAN_POINT ( 'NONE',  ( -21.08078803292166725, 75.92081401285503262, -209.8561204489615193 ) ) ;
#243479 = ORIENTED_EDGE ( 'NONE', *, *, #178633, .T. ) ;
#243480 = DIRECTION ( 'NONE',  ( 0.000000000000000000, 1.000000000000000000, 0.000000000000000000 ) ) ;
#243481 = EDGE_LOOP ( 'NONE', ( #105674, #253737, #41577, #10467 ) ) ;
#243482 = CARTESIAN_POINT ( 'NONE',  ( -18.40000000000000213, 11.75000000001113953, -121.3500000000000369 ) ) ;
#243483 = CARTESIAN_POINT ( 'NONE',  ( -22.00411653889226571, 29.99888786984131173, -252.4262548924342013 ) ) ;
#243484 = CARTESIAN_POINT ( 'NONE',  ( 21.05000000000000071, 1.115600667400684642E-11, -33.50000000000000000 ) ) ;
#243485 = DIRECTION ( 'NONE',  ( 1.000000000000000000, 0.000000000000000000, 0.000000000000000000 ) ) ;
#243486 = EDGE_LOOP ( 'NONE', ( #74944, #227796, #45369, #81881 ) ) ;
#243487 = FACE_OUTER_BOUND ( 'NONE', #40561, .T. ) ;
#243489 = ORIENTED_EDGE ( 'NONE', *, *, #5843, .F. ) ;
#243488 = AXIS2_PLACEMENT_3D ( 'NONE', #6251, #7550, #124942 ) ;
#243492 = VERTEX_POINT ( 'NONE', #188278 ) ;
#243491 = CARTESIAN_POINT ( 'NONE',  ( 18.54286124688533732, -9.623917578786661764, -107.2412023318627377 ) ) ;
#243490 = DIRECTION ( 'NONE',  ( 1.000000000000000000, 1.186688945009010077E-16, 0.000000000000000000 ) ) ;
#243493 = ADVANCED_FACE ( 'NONE', ( #108744 ), #64549, .T. ) ;
#243494 = DIRECTION ( 'NONE',  ( 0.000000000000000000, -7.086529944415886769E-15, 1.000000000000000000 ) ) ;
#243496 = ORIENTED_EDGE ( 'NONE', *, *, #120686, .F. ) ;
#243495 = AXIS2_PLACEMENT_3D ( 'NONE', #1352, #43073, #78326 ) ;
#243497 = VECTOR ( 'NONE', #125837, 1000.000000000000000 ) ;
#243498 = DIRECTION ( 'NONE',  ( -1.000000000000000000, -0.000000000000000000, -0.000000000000000000 ) ) ;
#243499 = ORIENTED_EDGE ( 'NONE', *, *, #20235, .T. ) ;
#243501 = CARTESIAN_POINT ( 'NONE',  ( -17.78043020864321022, 65.14640788800663529, -159.6861566502446124 ) ) ;
#243500 = CIRCLE ( 'NONE', #239410, 0.09999999999999799327 ) ;
#243502 = CARTESIAN_POINT ( 'NONE',  ( 18.59999999999999076, 66.56840568906282840, -213.6577031229154500 ) ) ;
#243503 = CARTESIAN_POINT ( 'NONE',  ( 20.94999999999999929, 76.00000000001260503, -190.6481074845243597 ) ) ;
#243504 = CARTESIAN_POINT ( 'NONE',  ( 23.40000000000005187, 76.00000000001119815, -36.02310748452479316 ) ) ;
#243505 = AXIS2_PLACEMENT_3D ( 'NONE', #140459, #184407, #58340 ) ;
#243506 = CARTESIAN_POINT ( 'NONE',  ( -20.64999999999999858, 53.08776555244186568, -234.2469744149522626 ) ) ;
#243507 = CIRCLE ( 'NONE', #210216, 1.500000000000001332 ) ;
#243508 = ORIENTED_EDGE ( 'NONE', *, *, #252643, .F. ) ;
#243509 = CARTESIAN_POINT ( 'NONE',  ( 20.27550659511089037, 66.78395627750272467, -56.87310748452438247 ) ) ;
#243510 = CARTESIAN_POINT ( 'NONE',  ( 20.94999999999999929, 84.73084112150691283, -59.92503276553992464 ) ) ;
#243511 = AXIS2_PLACEMENT_3D ( 'NONE', #111905, #53193, #132755 ) ;
#243512 = CARTESIAN_POINT ( 'NONE',  ( -19.99999999999999645, 5.572646938319271825, 16.60000000000000142 ) ) ;
#243513 = ORIENTED_EDGE ( 'NONE', *, *, #7513, .F. ) ;
#243514 = CARTESIAN_POINT ( 'NONE',  ( -2.995603634470891112E-16, -11.74999999998884448, -188.7499999999999716 ) ) ;
#243515 = ORIENTED_EDGE ( 'NONE', *, *, #209631, .F. ) ;
#243516 = DIRECTION ( 'NONE',  ( 1.000000000000000000, -0.000000000000000000, -0.000000000000000000 ) ) ;
#243517 = AXIS2_PLACEMENT_3D ( 'NONE', #66158, #46574, #27063 ) ;
#243518 = AXIS2_PLACEMENT_3D ( 'NONE', #119625, #199149, #20531 ) ;
#243519 = CARTESIAN_POINT ( 'NONE',  ( 23.14999999999999858, 5.499999999999998224, -21.09473398108690390 ) ) ;
#243520 = CARTESIAN_POINT ( 'NONE',  ( 20.85000000106542117, 36.17380055357438096, -235.9616714914856459 ) ) ;
#243522 = ORIENTED_EDGE ( 'NONE', *, *, #225000, .F. ) ;
#243521 = CARTESIAN_POINT ( 'NONE',  ( 20.12500000000000355, 10.24195072709382970, -141.8602037270861445 ) ) ;
#243523 = CARTESIAN_POINT ( 'NONE',  ( -23.15000000000000213, 67.23127455305835554, -235.8551265064784559 ) ) ;
#243524 = VECTOR ( 'NONE', #35428, 1000.000000000000114 ) ;
#243525 = CIRCLE ( 'NONE', #255949, 0.09999999999999999167 ) ;
#243526 = DIRECTION ( 'NONE',  ( 1.000000000000000000, 3.265361837132813093E-16, -0.000000000000000000 ) ) ;
#243527 = ADVANCED_FACE ( 'NONE', ( #70937, #185723 ), #150460, .T. ) ;
#243528 = DIRECTION ( 'NONE',  ( 0.000000000000000000, -1.000000000000000000, -7.272083257015735086E-15 ) ) ;
#243529 = ORIENTED_EDGE ( 'NONE', *, *, #26385, .T. ) ;
#243530 = LINE ( 'NONE', #100140, #230685 ) ;
#243531 = CARTESIAN_POINT ( 'NONE',  ( -18.40000000000000213, 54.09347887257330711, -229.1540424707546322 ) ) ;
#243532 = VERTEX_POINT ( 'NONE', #146563 ) ;
#243533 = CARTESIAN_POINT ( 'NONE',  ( -16.94180778212363592, 9.992443055743303049, -146.6041835705332517 ) ) ;
#243534 = VERTEX_POINT ( 'NONE', #118716 ) ;
#243535 = CARTESIAN_POINT ( 'NONE',  ( -20.64999999999999858, 27.77927773649450316, -239.9732258281457860 ) ) ;
#243536 = EDGE_LOOP ( 'NONE', ( #48034, #153359, #225572, #118021 ) ) ;
#243537 = EDGE_CURVE ( 'NONE', #218463, #38071, #46298, .T. ) ;
#243538 = EDGE_CURVE ( 'NONE', #50660, #151483, #17046, .T. ) ;
#243541 = ORIENTED_EDGE ( 'NONE', *, *, #249005, .T. ) ;
#243540 = ORIENTED_EDGE ( 'NONE', *, *, #8141, .F. ) ;
#243539 = DIRECTION ( 'NONE',  ( 0.000000000000000000, 6.982962677686266711E-15, -1.000000000000000000 ) ) ;
#243542 = CIRCLE ( 'NONE', #118485, 0.09999999999999892308 ) ;
#243543 = FACE_OUTER_BOUND ( 'NONE', #147276, .T. ) ;
#243544 = CARTESIAN_POINT ( 'NONE',  ( -21.14999999999999858, 76.10000000001272724, -210.0637644362255969 ) ) ;
#243545 = CIRCLE ( 'NONE', #239467, 0.1000000000000043771 ) ;
#243546 = DIRECTION ( 'NONE',  ( 0.5932847527679299127, 0.8049926720990051576, 4.984624513800587583E-15 ) ) ;
#243548 = CARTESIAN_POINT ( 'NONE',  ( -16.91256925476569606, 9.985731158128174911, -20.96764248900527505 ) ) ;
#243547 = DIRECTION ( 'NONE',  ( 1.000000000000000000, 0.000000000000000000, 0.000000000000000000 ) ) ;
#243549 = FACE_OUTER_BOUND ( 'NONE', #56607, .T. ) ;
#243550 = AXIS2_PLACEMENT_3D ( 'NONE', #30543, #8400, #125752 ) ;
#243551 = EDGE_CURVE ( 'NONE', #217224, #189431, #179611, .T. ) ;
#243552 = CARTESIAN_POINT ( 'NONE',  ( -17.80356949363740782, 65.12326860301170939, -59.23618050875686691 ) ) ;
#243553 = DIRECTION ( 'NONE',  ( 0.000000000000000000, 0.8814952561688429444, -0.4721928772777345684 ) ) ;
#243554 = PLANE ( 'NONE',  #251518 ) ;
#243555 = ORIENTED_EDGE ( 'NONE', *, *, #8537, .T. ) ;
#243557 = ORIENTED_EDGE ( 'NONE', *, *, #120311, .F. ) ;
#243556 = VECTOR ( 'NONE', #7111, 1000.000000000000000 ) ;
#243558 = EDGE_CURVE ( 'NONE', #84528, #148169, #237364, .T. ) ;
#243559 = DIRECTION ( 'NONE',  ( 1.000000000000000000, 0.000000000000000000, 0.000000000000000000 ) ) ;
#243560 = AXIS2_PLACEMENT_3D ( 'NONE', #242667, #202272, #23663 ) ;
#243563 = ORIENTED_EDGE ( 'NONE', *, *, #108228, .T. ) ;
#243562 = EDGE_CURVE ( 'NONE', #98192, #186539, #217771, .T. ) ;
#243561 = CARTESIAN_POINT ( 'NONE',  ( -20.94999999999999929, 64.23744694032048130, -224.5446448091673233 ) ) ;
#243564 = ORIENTED_EDGE ( 'NONE', *, *, #103050, .T. ) ;
#243565 = CARTESIAN_POINT ( 'NONE',  ( 18.59999999999999432, -1.135018845899022466, -208.7169768834322952 ) ) ;
#243566 =( BOUNDED_CURVE ( )  B_SPLINE_CURVE ( 3, ( #5014, #84529, #183693, #207106 ),
 .UNSPECIFIED., .F., .F. ) 
 B_SPLINE_CURVE_WITH_KNOTS ( ( 4, 4 ),
 ( 3.141592653589791784, 4.712388980384688786 ),
 .UNSPECIFIED. ) 
 CURVE ( )  GEOMETRIC_REPRESENTATION_ITEM ( )  RATIONAL_B_SPLINE_CURVE ( ( 1.000000000000000000, 0.8047378541243649375, 0.8047378541243649375, 1.000000000000000000 ) ) 
 REPRESENTATION_ITEM ( '' )  );
#243567 = ORIENTED_EDGE ( 'NONE', *, *, #247298, .F. ) ;
#243568 = FACE_OUTER_BOUND ( 'NONE', #141365, .T. ) ;
#243569 = EDGE_CURVE ( 'NONE', #154034, #20400, #20, .T. ) ;
#243570 = CIRCLE ( 'NONE', #47923, 0.09999999999999939493 ) ;
#243571 = VERTEX_POINT ( 'NONE', #121303 ) ;
#243572 = EDGE_CURVE ( 'NONE', #120661, #65772, #34073, .T. ) ;
#243573 = VECTOR ( 'NONE', #222111, 1000.000000000000000 ) ;
#243574 = CARTESIAN_POINT ( 'NONE',  ( 21.14999999999999858, 9.104497675943859392, -211.5542940109215522 ) ) ;
#243575 = CARTESIAN_POINT ( 'NONE',  ( -18.47140463609785854, -9.671474685209730637, -174.1727604582741833 ) ) ;
#243577 = VERTEX_POINT ( 'NONE', #61291 ) ;
#243576 = ORIENTED_EDGE ( 'NONE', *, *, #30, .T. ) ;
#243578 = ORIENTED_EDGE ( 'NONE', *, *, #99185, .F. ) ;
#243579 = CARTESIAN_POINT ( 'NONE',  ( 21.10642757222115407, 10.72315628916975250, -45.74069752378520093 ) ) ;
#243580 = VERTEX_POINT ( 'NONE', #216506 ) ;
#243581 = ORIENTED_EDGE ( 'NONE', *, *, #15436, .F. ) ;
#243582 = CARTESIAN_POINT ( 'NONE',  ( 20.04142135623730070, 64.35000000001180354, -81.67310748452439384 ) ) ;
#243584 = ORIENTED_EDGE ( 'NONE', *, *, #180388, .F. ) ;
#243583 = CARTESIAN_POINT ( 'NONE',  ( -21.55000000000000071, 7.349999999999998757, -21.15000000000000213 ) ) ;
#243585 = EDGE_CURVE ( 'NONE', #216520, #145447, #104719, .T. ) ;
#243586 = AXIS2_PLACEMENT_3D ( 'NONE', #56079, #75689, #135631 ) ;
#243587 = CARTESIAN_POINT ( 'NONE',  ( -20.94999999999999929, 1.115649653272650466E-11, -71.00000000000001421 ) ) ;
#243588 = CARTESIAN_POINT ( 'NONE',  ( -21.04999999999994387, 67.75000000001118394, -3.123107484524795474 ) ) ;
#243590 = ORIENTED_EDGE ( 'NONE', *, *, #197371, .F. ) ;
#243589 = FACE_OUTER_BOUND ( 'NONE', #249357, .T. ) ;
#243591 = SPHERICAL_SURFACE ( 'NONE', #196827, 0.1000000000000000056 ) ;
#243592 = ORIENTED_EDGE ( 'NONE', *, *, #2341, .F. ) ;
#243593 = DIRECTION ( 'NONE',  ( -1.000000000000000000, 0.000000000000000000, 0.000000000000000000 ) ) ;
#243595 = EDGE_CURVE ( 'NONE', #10681, #51363, #239939, .T. ) ;
#243594 = ORIENTED_EDGE ( 'NONE', *, *, #48001, .T. ) ;
#243596 = SPHERICAL_SURFACE ( 'NONE', #243488, 0.1000000000000000056 ) ;
#243597 = DIRECTION ( 'NONE',  ( 0.000000000000000000, 0.9876197685951252359, -0.1568667991644863424 ) ) ;
#243598 = ORIENTED_EDGE ( 'NONE', *, *, #87563, .F. ) ;
#243599 = DIRECTION ( 'NONE',  ( -1.000000000000000000, 0.000000000000000000, 0.000000000000000000 ) ) ;
#243600 = CIRCLE ( 'NONE', #172915, 0.1000000000000028644 ) ;
#243601 = DIRECTION ( 'NONE',  ( 0.000000000000000000, 0.4930308989874980785, 0.8700118002898462599 ) ) ;
#243602 = AXIS2_PLACEMENT_3D ( 'NONE', #27614, #31463, #107108 ) ;
#243603 = CARTESIAN_POINT ( 'NONE',  ( -16.27683809663750480, 9.350000000011133849, -109.7500000000000426 ) ) ;
#243604 = ORIENTED_EDGE ( 'NONE', *, *, #45296, .T. ) ;
#243605 = EDGE_LOOP ( 'NONE', ( #44111, #141244, #169648, #195963, #181231 ) ) ;
#243606 = ADVANCED_FACE ( 'NONE', ( #80830 ), #156577, .F. ) ;
#243607 = DIRECTION ( 'NONE',  ( 0.000000000000000000, 0.000000000000000000, 1.000000000000000000 ) ) ;
#243608 = CARTESIAN_POINT ( 'NONE',  ( -20.07928932188135107, 66.77928932189357170, -148.8731074845244393 ) ) ;
#243609 = ORIENTED_EDGE ( 'NONE', *, *, #184834, .T. ) ;
#243610 = EDGE_LOOP ( 'NONE', ( #186712, #103493, #120490, #48692 ) ) ;
#243611 = CARTESIAN_POINT ( 'NONE',  ( 23.14999999999999858, 3.900000000011155432, -100.5000000000000426 ) ) ;
#243612 =( NAMED_UNIT ( * ) SI_UNIT ( $, .STERADIAN. ) SOLID_ANGLE_UNIT ( ) );
#243613 = CARTESIAN_POINT ( 'NONE',  ( 22.46250603428203618, 0.02114417614996233138, -55.35013690265996189 ) ) ;
#243614 = DIRECTION ( 'NONE',  ( 1.000000000000000000, 0.000000000000000000, 0.000000000000000000 ) ) ;
#243615 = ORIENTED_EDGE ( 'NONE', *, *, #19359, .F. ) ;
#243616 = DIRECTION ( 'NONE',  ( 0.000000000000000000, 6.982962677686266711E-15, -1.000000000000000000 ) ) ;
#243617 = AXIS2_PLACEMENT_3D ( 'NONE', #784, #255085, #56907 ) ;
#243618 = EDGE_CURVE ( 'NONE', #1657, #131459, #229671, .T. ) ;
#243620 = ORIENTED_EDGE ( 'NONE', *, *, #146470, .F. ) ;
#243619 = VERTEX_POINT ( 'NONE', #79545 ) ;
#243621 = EDGE_LOOP ( 'NONE', ( #67405, #248132, #113396 ) ) ;
#243622 = ORIENTED_EDGE ( 'NONE', *, *, #8766, .T. ) ;
#243623 = DIRECTION ( 'NONE',  ( -1.000000000000000000, 0.000000000000000000, -0.000000000000000000 ) ) ;
#243624 = DIRECTION ( 'NONE',  ( -1.000000000000000000, 0.000000000000000000, 0.000000000000000000 ) ) ;
#243625 = AXIS2_PLACEMENT_3D ( 'NONE', #24707, #3830, #82043 ) ;
#243626 = CARTESIAN_POINT ( 'NONE',  ( -20.85000000000000142, -1.164121893230052995, -141.9148480855716343 ) ) ;
#243627 = CARTESIAN_POINT ( 'NONE',  ( 18.59999999999999076, -1.164121893230052995, -175.4148480855716059 ) ) ;
#243628 = CYLINDRICAL_SURFACE ( 'NONE', #51017, 0.09999999999999939493 ) ;
#243629 = EDGE_CURVE ( 'NONE', #86852, #38092, #129703, .T. ) ;
#243631 = CARTESIAN_POINT ( 'NONE',  ( 18.39999999999999858, -9.519327731081283162, -140.9729763765593589 ) ) ;
#243630 = FACE_OUTER_BOUND ( 'NONE', #181486, .T. ) ;
#243633 = ORIENTED_EDGE ( 'NONE', *, *, #116442, .F. ) ;
#243632 = CARTESIAN_POINT ( 'NONE',  ( 18.33996824403515191, 77.36682667616904041, -241.8005656296788572 ) ) ;
#243634 = DIRECTION ( 'NONE',  ( 1.000000000000000000, -3.265361837132813093E-16, -2.280189983783949500E-30 ) ) ;
#243635 = EDGE_LOOP ( 'NONE', ( #50512, #250938, #18214, #21332 ) ) ;
#243636 = CARTESIAN_POINT ( 'NONE',  ( 23.14999999999999503, 11.65000000001116298, -88.25000000000005684 ) ) ;
#243637 = ORIENTED_EDGE ( 'NONE', *, *, #69359, .F. ) ;
#243638 = EDGE_LOOP ( 'NONE', ( #99940, #30350, #159698, #212377 ) ) ;
#243639 = DIRECTION ( 'NONE',  ( -1.000000000000000000, 0.000000000000000000, -0.000000000000000000 ) ) ;
#243640 = CARTESIAN_POINT ( 'NONE',  ( -21.05000000000000071, 64.40000000001219860, -143.4513107147999449 ) ) ;
#243642 = EDGE_CURVE ( 'NONE', #134983, #203694, #200803, .T. ) ;
#243641 = FACE_OUTER_BOUND ( 'NONE', #174887, .T. ) ;
#243643 = EDGE_CURVE ( 'NONE', #111004, #43473, #67344, .T. ) ;
#243644 = CARTESIAN_POINT ( 'NONE',  ( -23.15000000000000213, 11.75000000001115552, -112.7500000000000284 ) ) ;
#243645 = EDGE_CURVE ( 'NONE', #47981, #127870, #58695, .T. ) ;
#243646 = AXIS2_PLACEMENT_3D ( 'NONE', #216846, #17380, #194756 ) ;
#243647 = DIRECTION ( 'NONE',  ( 1.000000000000000000, 2.952720810173289112E-16, -0.000000000000000000 ) ) ;
#243648 = ORIENTED_EDGE ( 'NONE', *, *, #73860, .F. ) ;
#243649 = ORIENTED_EDGE ( 'NONE', *, *, #257768, .T. ) ;
#243650 = EDGE_CURVE ( 'NONE', #132129, #44449, #56133, .T. ) ;
#243651 = CARTESIAN_POINT ( 'NONE',  ( 21.05000000000000071, -0.09999999998884338825, -122.3504291924552234 ) ) ;
#243652 = ORIENTED_EDGE ( 'NONE', *, *, #91435, .F. ) ;
#243653 = DIRECTION ( 'NONE',  ( -1.000000000000000000, -0.000000000000000000, -0.000000000000000000 ) ) ;
#243654 = CARTESIAN_POINT ( 'NONE',  ( 21.30000000000002558, 1.115650265596050101E-11, -104.5500000000000256 ) ) ;
#243655 = DIRECTION ( 'NONE',  ( 0.000000000000000000, 0.000000000000000000, 1.000000000000000000 ) ) ;
#243656 = DIRECTION ( 'NONE',  ( 0.000000000000000000, 0.000000000000000000, 1.000000000000000000 ) ) ;
#243657 = DIRECTION ( 'NONE',  ( 0.000000000000000000, 0.000000000000000000, -1.000000000000000000 ) ) ;
#243658 = ORIENTED_EDGE ( 'NONE', *, *, #85522, .T. ) ;
#243659 = DIRECTION ( 'NONE',  ( 0.000000000000000000, -6.982962677686266711E-15, 1.000000000000000000 ) ) ;
#243660 = CARTESIAN_POINT ( 'NONE',  ( 20.94999999999999929, 85.50000000001197975, -112.9170766071766820 ) ) ;
#243661 = DIRECTION ( 'NONE',  ( -0.7071067811865474617, 0.7071067811865474617, 4.937700262164531476E-15 ) ) ;
#243662 = LINE ( 'NONE', #61173, #195846 ) ;
#243663 = DIRECTION ( 'NONE',  ( -0.000000000000000000, 6.982962677686266711E-15, -1.000000000000000000 ) ) ;
#243664 = VECTOR ( 'NONE', #115558, 1000.000000000000000 ) ;
#243665 = CARTESIAN_POINT ( 'NONE',  ( 18.50000000000000000, 77.31518212004206703, -241.6587219750726092 ) ) ;
#243666 = CIRCLE ( 'NONE', #160488, 0.6000000000000139666 ) ;
#243667 = CIRCLE ( 'NONE', #131229, 0.1000000000000124678 ) ;
#243668 = TOROIDAL_SURFACE ( 'NONE', #18799, 3.899999999999999467, 0.1000000000000000056 ) ;
#243669 = EDGE_CURVE ( 'NONE', #72339, #18553, #63053, .T. ) ;
#243670 = ORIENTED_EDGE ( 'NONE', *, *, #109112, .T. ) ;
#243671 =( BOUNDED_SURFACE ( )  B_SPLINE_SURFACE ( 3, 2, ( 
 ( #111706, #215917, #133831 ),
 ( #252484, #76416, #115548 ),
 ( #173012, #17718, #251198 ),
 ( #112996, #171715, #37321 ),
 ( #92140, #72601, #195121 ),
 ( #73897, #213358, #116841 ) ),
 .UNSPECIFIED., .F., .F., .T. ) 
 B_SPLINE_SURFACE_WITH_KNOTS ( ( 4, 2, 4 ),
 ( 3, 3 ),
 ( 1.570796326794897668, 2.356194490192346169, 3.141592653589794448 ),
 ( 0.000000000000000000, 1.000000000000000000 ),
 .UNSPECIFIED. ) 
 GEOMETRIC_REPRESENTATION_ITEM ( )  RATIONAL_B_SPLINE_SURFACE ( (
 ( 1.000000000000000000, 0.7071067811865597852, 1.000000000000000000),
 ( 1.000000000000000000, 0.6611148371798263312, 1.000000000000000000),
 ( 1.000000000000000000, 0.6092287576670563087, 1.000000000000000000),
 ( 1.000000000000000000, 0.5278258667083555178, 1.000000000000000000),
 ( 1.000000000000000000, 0.4993418825314846488, 1.000000000000000000),
 ( 1.000000000000000000, 0.5000000000000154321, 1.000000000000000000) ) ) 
 REPRESENTATION_ITEM ( '' )  SURFACE ( )  );
#243672 = STYLED_ITEM ( 'NONE', ( #251949 ), #26624 ) ;
#243673 = CARTESIAN_POINT ( 'NONE',  ( -22.39999999999999503, 68.20922040163873135, -136.5231074845243597 ) ) ;
#243674 = EDGE_LOOP ( 'NONE', ( #221181, #129040, #197194 ) ) ;
#243675 = EDGE_CURVE ( 'NONE', #97342, #1847, #125602, .T. ) ;
#243676 = EDGE_CURVE ( 'NONE', #214793, #189932, #121373, .T. ) ;
#243677 = CARTESIAN_POINT ( 'NONE',  ( 20.94999999999999929, 71.00000000001230660, -157.6178414656113205 ) ) ;
#243678 = CARTESIAN_POINT ( 'NONE',  ( -6.000000000000003553, -11.65000000000000036, 10.00000000000000178 ) ) ;
#243679 = CARTESIAN_POINT ( 'NONE',  ( 21.06086055316007943, 61.95649253837676440, -221.7814335778687962 ) ) ;
#243680 = ORIENTED_EDGE ( 'NONE', *, *, #26708, .T. ) ;
#243681 = DIRECTION ( 'NONE',  ( 1.652117596168391700E-15, -0.9651348961777157509, 0.2617529984165031243 ) ) ;
#243682 = FACE_OUTER_BOUND ( 'NONE', #69208, .T. ) ;
#243683 = B_SPLINE_CURVE_WITH_KNOTS ( 'NONE', 3,
 ( #23017, #80360, #179516, #821, #221171, #17837, #157404, #102486, #235603, #62123, #119539, #19133, #59510, #159955, #182069, #216040 ),
 .UNSPECIFIED., .F., .F.,
 ( 4, 3, 3, 3, 3, 4 ),
 ( 0.000000000000000000, 2.209833635978099498E-05, 5.595056164119025226E-05, 8.979992002654954499E-05, 0.0001236482757198867745, 0.0001574984039362969023 ),
 .UNSPECIFIED. ) ;
#243684 = FACE_OUTER_BOUND ( 'NONE', #71896, .T. ) ;
#243685 = EDGE_CURVE ( 'NONE', #205324, #212994, #17292, .T. ) ;
#243686 = CARTESIAN_POINT ( 'NONE',  ( 18.59999999999999076, 74.16465844978819177, -191.9679561919613775 ) ) ;
#243687 = CIRCLE ( 'NONE', #193800, 0.09999999999999939493 ) ;
#243688 = CARTESIAN_POINT ( 'NONE',  ( 21.05000000000000071, 11.60000000001116227, -60.07179676972450011 ) ) ;
#243689 = AXIS2_PLACEMENT_3D ( 'NONE', #165326, #242277, #44092 ) ;
#243690 = ORIENTED_EDGE ( 'NONE', *, *, #85585, .F. ) ;
#243691 = CARTESIAN_POINT ( 'NONE',  ( -18.59999999999999787, 1.736257131608553550, -45.06865232901750318 ) ) ;
#243693 = ORIENTED_EDGE ( 'NONE', *, *, #154890, .F. ) ;
#243692 = CARTESIAN_POINT ( 'NONE',  ( 23.14999999999999858, 76.00000000001126921, -203.5231074845248997 ) ) ;
#243694 = CARTESIAN_POINT ( 'NONE',  ( -21.05000000000000071, -1.261786168553869603, -75.08649896354552311 ) ) ;
#243695 = CARTESIAN_POINT ( 'NONE',  ( -21.14999999999999858, 1.115600667400684642E-11, -161.2414213562372538 ) ) ;
#243696 = ORIENTED_EDGE ( 'NONE', *, *, #125291, .F. ) ;
#243697 = CARTESIAN_POINT ( 'NONE',  ( -23.25000000000000000, -11.64999999998884483, -134.0000000000000000 ) ) ;
#243698 = TOROIDAL_SURFACE ( 'NONE', #106291, 0.9750000000000019762, 0.1000000000000000056 ) ;
#243699 = AXIS2_PLACEMENT_3D ( 'NONE', #238291, #103900, #123493 ) ;
#243700 = CIRCLE ( 'NONE', #127171, 0.1000000000000002554 ) ;
#243701 = ADVANCED_FACE ( 'NONE', ( #182541 ), #106816, .F. ) ;
#243702 = CARTESIAN_POINT ( 'NONE',  ( 11.60000000000006182, 64.35000000001120668, -23.72310748452479601 ) ) ;
#243703 = ORIENTED_EDGE ( 'NONE', *, *, #140214, .F. ) ;
#243704 = CARTESIAN_POINT ( 'NONE',  ( -20.94999999999999929, 1.115600667400684642E-11, -134.0000000000000284 ) ) ;
#243705 = CARTESIAN_POINT ( 'NONE',  ( 15.74999999999999645, 9.350000000011139178, -184.3657431672739051 ) ) ;
#243706 = CIRCLE ( 'NONE', #52332, 0.1000000000000001860 ) ;
#243707 = FACE_OUTER_BOUND ( 'NONE', #218271, .T. ) ;
#243709 = ORIENTED_EDGE ( 'NONE', *, *, #25985, .F. ) ;
#243708 = AXIS2_PLACEMENT_3D ( 'NONE', #49829, #125519, #205027 ) ;
#243710 = ORIENTED_EDGE ( 'NONE', *, *, #216677, .F. ) ;
#243711 = CARTESIAN_POINT ( 'NONE',  ( -21.05000000000000071, 64.35000000001176090, -76.53791325517833855 ) ) ;
#243712 = CIRCLE ( 'NONE', #214661, 0.5999999999999894307 ) ;
#243713 = FACE_OUTER_BOUND ( 'NONE', #17790, .T. ) ;
#243714 = LINE ( 'NONE', #202025, #257330 ) ;
#243715 = AXIS2_PLACEMENT_3D ( 'NONE', #26712, #25416, #185758 ) ;
#243716 = CARTESIAN_POINT ( 'NONE',  ( 22.50000000000000000, 76.00000000001195133, -103.0231074845243171 ) ) ;
#243717 = LINE ( 'NONE', #126332, #19471 ) ;
#243718 = EDGE_CURVE ( 'NONE', #212748, #177537, #204699, .T. ) ;
#243719 = DIRECTION ( 'NONE',  ( 0.000000000000000000, -0.4999999999999799605, 0.8660254037844502539 ) ) ;
#243720 = DIRECTION ( 'NONE',  ( -1.000000000000000000, 0.000000000000000000, 0.000000000000000000 ) ) ;
#243722 = CARTESIAN_POINT ( 'NONE',  ( -18.46856557590792391, -9.474215907775336731, -74.10198624088232577 ) ) ;
#243721 = CARTESIAN_POINT ( 'NONE',  ( 21.04999999999999716, -1.244299762474901705, -194.8241018385075733 ) ) ;
#243723 = DIRECTION ( 'NONE',  ( -0.000000000000000000, -0.8660254037844468122, -0.4999999999999860112 ) ) ;
#243724 = EDGE_CURVE ( 'NONE', #69280, #20464, #133790, .T. ) ;
#243725 = CARTESIAN_POINT ( 'NONE',  ( -18.40000000000000213, 70.35000000001254250, -179.2731074845243882 ) ) ;
#243726 = CARTESIAN_POINT ( 'NONE',  ( 22.39999999999999503, 1.115600667400684642E-11, -155.8504291924551808 ) ) ;
#243727 = FACE_OUTER_BOUND ( 'NONE', #164443, .T. ) ;
#243728 = ORIENTED_EDGE ( 'NONE', *, *, #50610, .T. ) ;
#243729 = ORIENTED_EDGE ( 'NONE', *, *, #14375, .T. ) ;
#243730 = DIRECTION ( 'NONE',  ( -0.000000000000000000, 6.982962677686266711E-15, -1.000000000000000000 ) ) ;
#243731 = CYLINDRICAL_SURFACE ( 'NONE', #145217, 7.899999999999994138 ) ;
#243733 = FACE_OUTER_BOUND ( 'NONE', #107496, .T. ) ;
#243732 = DIRECTION ( 'NONE',  ( 0.000000000000000000, 0.000000000000000000, -1.000000000000000000 ) ) ;
#243734 = ADVANCED_FACE ( 'NONE', ( #3881 ), #164821, .T. ) ;
#243735 = ADVANCED_FACE ( 'NONE', ( #242483 ), #143388, .F. ) ;
#243736 = PLANE ( 'NONE',  #89361 ) ;
#243737 = DIRECTION ( 'NONE',  ( 3.469446951953728416E-14, -0.8660254037844309360, 0.5000000000000134337 ) ) ;
#243738 = ORIENTED_EDGE ( 'NONE', *, *, #169031, .T. ) ;
#243739 = CIRCLE ( 'NONE', #214505, 0.09999999999999939493 ) ;
#243740 = AXIS2_PLACEMENT_3D ( 'NONE', #3598, #66146, #145670 ) ;
#243741 = CARTESIAN_POINT ( 'NONE',  ( -16.92778301347303582, 51.66969098184829079, -231.8678752041996347 ) ) ;
#243742 = ORIENTED_EDGE ( 'NONE', *, *, #161821, .F. ) ;
#243743 = DIRECTION ( 'NONE',  ( 0.000000000000000000, 1.000000000000000000, 6.938893903907222067E-15 ) ) ;
#243744 = AXIS2_PLACEMENT_3D ( 'NONE', #25108, #129000, #29915 ) ;
#243745 = EDGE_CURVE ( 'NONE', #46173, #133581, #238022, .T. ) ;
#243746 = EDGE_CURVE ( 'NONE', #74755, #141820, #163049, .T. ) ;
#243747 = CARTESIAN_POINT ( 'NONE',  ( -16.94445028196808778, 12.44605341304038859, -211.1922452800140775 ) ) ;
#243748 = ORIENTED_EDGE ( 'NONE', *, *, #82690, .F. ) ;
#243749 = DIRECTION ( 'NONE',  ( 1.000000000000000000, 0.000000000000000000, 0.000000000000000000 ) ) ;
#243750 = ORIENTED_EDGE ( 'NONE', *, *, #104662, .T. ) ;
#243752 = CIRCLE ( 'NONE', #6419, 0.09999999999998898659 ) ;
#243751 = CARTESIAN_POINT ( 'NONE',  ( -20.85000000000000497, 64.25000000001250555, -176.9422547304831426 ) ) ;
#243754 = CIRCLE ( 'NONE', #239668, 0.09999999999998898659 ) ;
#243753 = CARTESIAN_POINT ( 'NONE',  ( 20.94999999999999929, 69.35000000001259934, -191.3731074845244109 ) ) ;
#243755 = DIRECTION ( 'NONE',  ( 0.000000000000000000, 0.000000000000000000, -1.000000000000000000 ) ) ;
#243756 = CARTESIAN_POINT ( 'NONE',  ( 18.45036689428330590, -9.490184143317831555, -141.0126958274863682 ) ) ;
#243757 = CARTESIAN_POINT ( 'NONE',  ( -18.50000000000000000, -9.399999999988850163, -107.4146583429697017 ) ) ;
#243758 = EDGE_CURVE ( 'NONE', #57243, #22952, #96364, .T. ) ;
#243759 = B_SPLINE_CURVE_WITH_KNOTS ( 'NONE', 3,
 ( #31825, #168787, #111334, #248272, #231292, #210445, #190899, #147897 ),
 .UNSPECIFIED., .F., .F.,
 ( 4, 2, 2, 4 ),
 ( 0.000000000000000000, 0.0001306511400391185051, 0.0001959767100586981136, 0.0002613022800782777220 ),
 .UNSPECIFIED. ) ;
#243760 = CARTESIAN_POINT ( 'NONE',  ( 20.94999999999999574, 74.73821383144760944, -195.4366085209788935 ) ) ;
#243761 = VECTOR ( 'NONE', #93590, 1000.000000000000227 ) ;
#243762 = CARTESIAN_POINT ( 'NONE',  ( -18.50000000000000000, 64.25000000001173817, -81.27310748452440237 ) ) ;
#243763 = CYLINDRICAL_SURFACE ( 'NONE', #244734, 11.80000000000000426 ) ;
#243766 = ORIENTED_EDGE ( 'NONE', *, *, #48190, .T. ) ;
#243765 = EDGE_CURVE ( 'NONE', #92704, #97681, #57228, .T. ) ;
#243764 = CARTESIAN_POINT ( 'NONE',  ( 20.52683494730046476, 67.01946918171073264, -128.0178547619901508 ) ) ;
#243768 = CARTESIAN_POINT ( 'NONE',  ( 18.59999999999999432, 77.63717271298244782, -124.9409541190522788 ) ) ;
#243767 = DIRECTION ( 'NONE',  ( 0.000000000000000000, 0.000000000000000000, 1.000000000000000000 ) ) ;
#243769 = ORIENTED_EDGE ( 'NONE', *, *, #246900, .T. ) ;
#243771 = VERTEX_POINT ( 'NONE', #105510 ) ;
#243770 = DIRECTION ( 'NONE',  ( 0.000000000000000000, -1.000000000000000000, -6.982962677686265922E-15 ) ) ;
#243772 = ORIENTED_EDGE ( 'NONE', *, *, #27924, .T. ) ;
#243773 = CARTESIAN_POINT ( 'NONE',  ( 20.94999999999999929, 24.17260720300848575, -252.6908294531417027 ) ) ;
#243774 = CARTESIAN_POINT ( 'NONE',  ( -22.47071067811865319, 29.57301391503006016, -252.6169816238249552 ) ) ;
#243775 = VERTEX_POINT ( 'NONE', #147237 ) ;
#243776 = DIRECTION ( 'NONE',  ( 0.000000000000000000, 0.8814952561688438326, -0.4721928772777332362 ) ) ;
#243777 = CARTESIAN_POINT ( 'NONE',  ( -22.57320508075687115, 11.75000000000000000, 0.000000000000000000 ) ) ;
#243779 = DIRECTION ( 'NONE',  ( 0.000000000000000000, -0.4721928772777242433, -0.8814952561688484955 ) ) ;
#243778 = AXIS2_PLACEMENT_3D ( 'NONE', #166930, #209883, #31275 ) ;
#243780 = ADVANCED_FACE ( 'NONE', ( #28634 ), #9015, .T. ) ;
#243781 = CARTESIAN_POINT ( 'NONE',  ( 23.24999999999999289, 66.40155400966892785, -213.5088390336144073 ) ) ;
#243782 = CARTESIAN_POINT ( 'NONE',  ( -21.14999999999999858, 69.45934304831143891, -203.5231074845243882 ) ) ;
#243783 = CYLINDRICAL_SURFACE ( 'NONE', #122568, 0.09999999999999939493 ) ;
#243784 = EDGE_CURVE ( 'NONE', #88943, #211780, #250501, .T. ) ;
#243785 = ORIENTED_EDGE ( 'NONE', *, *, #198967, .T. ) ;
#243786 = VERTEX_POINT ( 'NONE', #221619 ) ;
#243787 = AXIS2_PLACEMENT_3D ( 'NONE', #206084, #23630, #103103 ) ;
#243788 = VERTEX_POINT ( 'NONE', #43019 ) ;
#243789 = CIRCLE ( 'NONE', #239518, 0.1000000000000070832 ) ;
#243790 = DIRECTION ( 'NONE',  ( -0.000000000000000000, -0.000000000000000000, -1.000000000000000000 ) ) ;
#243791 = ORIENTED_EDGE ( 'NONE', *, *, #18524, .T. ) ;
#243792 = CARTESIAN_POINT ( 'NONE',  ( 18.59999999999999076, 77.83585931145546510, -91.41866831572575336 ) ) ;
#243793 = CARTESIAN_POINT ( 'NONE',  ( -17.11825945287483108, 9.950000000011112178, -180.1499999999999488 ) ) ;
#243794 = CARTESIAN_POINT ( 'NONE',  ( -22.47007471830798409, 68.27928934808545591, -103.0231074845243597 ) ) ;
#243795 = EDGE_CURVE ( 'NONE', #246161, #196907, #211070, .T. ) ;
#243796 = CARTESIAN_POINT ( 'NONE',  ( 21.05000000000000071, 67.92720994251783395, -214.1870976236629929 ) ) ;
#243797 = CARTESIAN_POINT ( 'NONE',  ( 21.04116576186311605, 10.62466307876251292, -179.8285817686277426 ) ) ;
#243798 = ORIENTED_EDGE ( 'NONE', *, *, #124110, .F. ) ;
#243799 = DIRECTION ( 'NONE',  ( -0.8660254037843878594, 0.4407476280845205041, -0.2360964386388684777 ) ) ;
#243800 = CARTESIAN_POINT ( 'NONE',  ( 18.39999999999999858, 85.51932773110506503, -196.5501311079649724 ) ) ;
#243801 = DIRECTION ( 'NONE',  ( 1.000000000000000000, 0.000000000000000000, 0.000000000000000000 ) ) ;
#243802 = DIRECTION ( 'NONE',  ( 1.000000000000000000, 0.000000000000000000, 0.000000000000000000 ) ) ;
#243803 = ORIENTED_EDGE ( 'NONE', *, *, #76738, .F. ) ;
#243804 = CIRCLE ( 'NONE', #239533, 0.09999999999999711897 ) ;
#243805 = CARTESIAN_POINT ( 'NONE',  ( -22.47007471830799830, 7.720710651937627844, -134.0000000000000000 ) ) ;
#243806 = ORIENTED_EDGE ( 'NONE', *, *, #27008, .T. ) ;
#243809 = EDGE_LOOP ( 'NONE', ( #181912, #202360, #205274 ) ) ;
#243808 = CARTESIAN_POINT ( 'NONE',  ( 18.59999999999999432, 77.16270174995010223, -128.4231074845242802 ) ) ;
#243807 = CYLINDRICAL_SURFACE ( 'NONE', #119931, 0.1000000000000122874 ) ;
#243810 = ORIENTED_EDGE ( 'NONE', *, *, #135117, .F. ) ;
#243811 = CARTESIAN_POINT ( 'NONE',  ( -21.05000000000000071, 88.41227409416160299, -105.9231074845242091 ) ) ;
#243812 = DIRECTION ( 'NONE',  ( 0.000000000000000000, 0.9770955615653315052, 0.2128009952263603954 ) ) ;
#243813 = AXIS2_PLACEMENT_3D ( 'NONE', #107747, #184713, #244679 ) ;
#243814 = VERTEX_POINT ( 'NONE', #35037 ) ;
#243815 = CARTESIAN_POINT ( 'NONE',  ( 20.94999999999999929, 68.19849547655701372, -211.6586561550524834 ) ) ;
#243816 = DIRECTION ( 'NONE',  ( 4.026293107431335996E-15, -0.8700118002898359348, 0.4930308989875165082 ) ) ;
#243818 = CARTESIAN_POINT ( 'NONE',  ( -20.64999999999999858, -9.499999999988846255, -157.6060308773475924 ) ) ;
#243817 = FACE_OUTER_BOUND ( 'NONE', #72980, .T. ) ;
#243820 = ORIENTED_EDGE ( 'NONE', *, *, #59576, .T. ) ;
#243819 = CARTESIAN_POINT ( 'NONE',  ( 18.39999999999999503, 11.75000000001113953, -180.1499999999999773 ) ) ;
#243821 = VERTEX_POINT ( 'NONE', #149830 ) ;
#243822 = CARTESIAN_POINT ( 'NONE',  ( 19.96984138294275013, 64.25000000001176659, -78.29853541332350630 ) ) ;
#243823 = LINE ( 'NONE', #246403, #251951 ) ;
#243824 = VECTOR ( 'NONE', #143289, 1000.000000000000114 ) ;
#243825 = DIRECTION ( 'NONE',  ( 1.000000000000000000, 0.000000000000000000, 0.000000000000000000 ) ) ;
#243826 = ORIENTED_EDGE ( 'NONE', *, *, #95349, .T. ) ;
#243827 = CARTESIAN_POINT ( 'NONE',  ( -20.85000000000000142, 74.93036000061670165, -233.6816308724374949 ) ) ;
#243828 = EDGE_LOOP ( 'NONE', ( #189793, #225602, #22116, #206988 ) ) ;
#243829 = CARTESIAN_POINT ( 'NONE',  ( 20.95429402530531959, 18.83316948772580091, -229.9329191065959037 ) ) ;
#243830 = LINE ( 'NONE', #103025, #115964 ) ;
#243831 = DIRECTION ( 'NONE',  ( 0.000000000000000000, -1.000000000000000000, 0.000000000000000000 ) ) ;
#243832 = VERTEX_POINT ( 'NONE', #191535 ) ;
#243833 = CYLINDRICAL_SURFACE ( 'NONE', #100135, 0.09999999999999939493 ) ;
#243834 = EDGE_CURVE ( 'NONE', #66095, #164666, #117241, .T. ) ;
#243835 = AXIS2_PLACEMENT_3D ( 'NONE', #198323, #19708, #99206 ) ;
#243836 = PLANE ( 'NONE',  #214694 ) ;
#243838 = AXIS2_PLACEMENT_3D ( 'NONE', #19292, #36309, #196637 ) ;
#243837 = B_SPLINE_CURVE_WITH_KNOTS ( 'NONE', 3,
 ( #150865, #173046, #110451, #251234, #229127, #174334, #73931, #111745, #109156, #188706, #53045, #10072, #152181, #191315, #34804, #75209 ),
 .UNSPECIFIED., .F., .F.,
 ( 4, 3, 3, 3, 3, 4 ),
 ( 0.000000000000000000, 2.209075297430758666E-05, 5.594258369009633163E-05, 8.979524372342017908E-05, 0.0001236472815274585488, 0.0001574990747609553653 ),
 .UNSPECIFIED. ) ;
#243839 = CIRCLE ( 'NONE', #181326, 2.100000000000004530 ) ;
#243840 = CONICAL_SURFACE ( 'NONE', #164747, 6.250000000000005329, 0.7853981633974431720 ) ;
#243841 = ORIENTED_EDGE ( 'NONE', *, *, #65839, .T. ) ;
#243842 = ORIENTED_EDGE ( 'NONE', *, *, #69742, .F. ) ;
#243843 = EDGE_LOOP ( 'NONE', ( #225882, #201261, #85867, #40100 ) ) ;
#243844 = CARTESIAN_POINT ( 'NONE',  ( 22.39999999999999503, 1.115600667400684642E-11, -25.70922040162662370 ) ) ;
#243846 = EDGE_CURVE ( 'NONE', #211228, #139671, #49426, .T. ) ;
#243845 = ORIENTED_EDGE ( 'NONE', *, *, #88504, .T. ) ;
#243848 = ORIENTED_EDGE ( 'NONE', *, *, #65909, .T. ) ;
#243847 = CARTESIAN_POINT ( 'NONE',  ( -21.40925344232282512, 6.658518859390450295, 0.09895018861964700874 ) ) ;
#243849 = ORIENTED_EDGE ( 'NONE', *, *, #224870, .T. ) ;
#243850 = EDGE_CURVE ( 'NONE', #70242, #188351, #196327, .T. ) ;
#243853 = ORIENTED_EDGE ( 'NONE', *, *, #230336, .T. ) ;
#243852 = VERTEX_POINT ( 'NONE', #113248 ) ;
#243851 = FACE_OUTER_BOUND ( 'NONE', #251911, .T. ) ;
#243854 = LINE ( 'NONE', #245150, #252135 ) ;
#243855 = ORIENTED_EDGE ( 'NONE', *, *, #234639, .T. ) ;
#243856 = CARTESIAN_POINT ( 'NONE',  ( 20.94999999999999929, 1.115600667400684642E-11, -134.0000000000000284 ) ) ;
#243857 = AXIS2_PLACEMENT_3D ( 'NONE', #158565, #95980, #238065 ) ;
#243858 = FACE_OUTER_BOUND ( 'NONE', #22203, .T. ) ;
#243859 = CARTESIAN_POINT ( 'NONE',  ( -18.54260524012582323, 87.05308753821724110, -199.5365204736072258 ) ) ;
#243860 = ORIENTED_EDGE ( 'NONE', *, *, #153874, .T. ) ;
#243861 = EDGE_CURVE ( 'NONE', #226915, #137139, #134081, .T. ) ;
#243862 = DIRECTION ( 'NONE',  ( 0.000000000000000000, 0.01562500000001045344, 0.9998779222360096863 ) ) ;
#243865 = ORIENTED_EDGE ( 'NONE', *, *, #30710, .T. ) ;
#243864 = ADVANCED_FACE ( 'NONE', ( #229360 ), #183873, .T. ) ;
#243863 = CARTESIAN_POINT ( 'NONE',  ( 23.14999999999999503, 31.40887384169439756, -233.4092306946072313 ) ) ;
#243866 = CARTESIAN_POINT ( 'NONE',  ( 21.13461538461538325, 67.11458296203710461, -57.17310748452437963 ) ) ;
#243868 = ORIENTED_EDGE ( 'NONE', *, *, #68976, .F. ) ;
#243867 = DIRECTION ( 'NONE',  ( -0.000000000000000000, 6.982962677686266711E-15, -1.000000000000000000 ) ) ;
#243869 = ORIENTED_EDGE ( 'NONE', *, *, #136835, .F. ) ;
#243870 = DIRECTION ( 'NONE',  ( 0.000000000000000000, 0.000000000000000000, -1.000000000000000000 ) ) ;
#243871 = TOROIDAL_SURFACE ( 'NONE', #131452, 12.97499999999999787, 0.1000000000000000056 ) ;
#243872 = EDGE_CURVE ( 'NONE', #224664, #187777, #114537, .T. ) ;
#243873 = CIRCLE ( 'NONE', #189711, 0.5000000000000004441 ) ;
#243874 = ORIENTED_EDGE ( 'NONE', *, *, #155762, .F. ) ;
#243875 = EDGE_LOOP ( 'NONE', ( #99246, #5164, #189218, #116893 ) ) ;
#243876 = CARTESIAN_POINT ( 'NONE',  ( -22.94999999999999929, 11.49641995933507843, 1.885425182446134107 ) ) ;
#243877 = CARTESIAN_POINT ( 'NONE',  ( -20.94999999999999929, -1.835859311432479268, -179.0044391687985410 ) ) ;
#243880 = ORIENTED_EDGE ( 'NONE', *, *, #106259, .F. ) ;
#243879 = VERTEX_POINT ( 'NONE', #132827 ) ;
#243878 = AXIS2_PLACEMENT_3D ( 'NONE', #148957, #88945, #10716 ) ;
#243881 = ORIENTED_EDGE ( 'NONE', *, *, #62410, .F. ) ;
#243882 = CARTESIAN_POINT ( 'NONE',  ( -23.15000000000000213, 73.50000000001151079, -49.24772940728643533 ) ) ;
#243884 = ORIENTED_EDGE ( 'NONE', *, *, #104406, .F. ) ;
#243883 = EDGE_CURVE ( 'NONE', #239889, #20419, #108849, .T. ) ;
#243885 = VERTEX_POINT ( 'NONE', #170711 ) ;
#243886 = CARTESIAN_POINT ( 'NONE',  ( 18.46905048506371472, 85.47374425739481296, -163.3471211922688724 ) ) ;
#243888 = VERTEX_POINT ( 'NONE', #168138 ) ;
#243887 = DIRECTION ( 'NONE',  ( 0.000000000000000000, -0.2128009952263485993, 0.9770955615653341697 ) ) ;
#243889 = LINE ( 'NONE', #104361, #206643 ) ;
#243890 = AXIS2_PLACEMENT_3D ( 'NONE', #59940, #157830, #161205 ) ;
#243891 = CIRCLE ( 'NONE', #89950, 7.791421356237335338 ) ;
#243893 = DIRECTION ( 'NONE',  ( 1.000000000000000000, 0.000000000000000000, 0.000000000000000000 ) ) ;
#243892 = DIRECTION ( 'NONE',  ( -0.000000000000000000, 0.4721928772777345684, 0.8814952561688429444 ) ) ;
#243894 = DIRECTION ( 'NONE',  ( 0.000000000000000000, -5.551115123125777653E-14, 1.000000000000000000 ) ) ;
#243895 = ORIENTED_EDGE ( 'NONE', *, *, #209519, .T. ) ;
#243897 = EDGE_CURVE ( 'NONE', #201700, #102074, #4117, .T. ) ;
#243896 = EDGE_LOOP ( 'NONE', ( #155720, #194904, #79886, #35829 ) ) ;
#243898 = LINE ( 'NONE', #24886, #206981 ) ;
#243899 = DIRECTION ( 'NONE',  ( 0.000000000000000000, 0.000000000000000000, -1.000000000000000000 ) ) ;
#243900 = ORIENTED_EDGE ( 'NONE', *, *, #57051, .F. ) ;
#243901 = LINE ( 'NONE', #127828, #67673 ) ;
#243902 = ORIENTED_EDGE ( 'NONE', *, *, #160376, .T. ) ;
#243903 = VERTEX_POINT ( 'NONE', #173278 ) ;
#243904 = DIRECTION ( 'NONE',  ( -1.000000000000000000, -0.000000000000000000, 0.000000000000000000 ) ) ;
#243905 = VERTEX_POINT ( 'NONE', #53283 ) ;
#243906 = CARTESIAN_POINT ( 'NONE',  ( -21.05000000000000426, 11.63687328911556662, -107.3217592133250520 ) ) ;
#243907 = DIRECTION ( 'NONE',  ( 0.000000000000000000, 0.2128009952263603677, -0.9770955615653313941 ) ) ;
#243909 = ORIENTED_EDGE ( 'NONE', *, *, #23802, .T. ) ;
#243908 = APPLICATION_CONTEXT ( 'automotive_design' ) ;
#243910 = CARTESIAN_POINT ( 'NONE',  ( 18.54999999999999716, 51.61886293219128419, -231.9464690156495408 ) ) ;
#243911 = CARTESIAN_POINT ( 'NONE',  ( -20.94999999999999929, 6.846123162352588665, -37.23772626684986164 ) ) ;
#243912 = DIRECTION ( 'NONE',  ( -0.000000000000000000, -1.000000000000000000, -0.000000000000000000 ) ) ;
#243913 = CARTESIAN_POINT ( 'NONE',  ( -23.15000000000000213, 1.999999999999998224, -12.72462192276209869 ) ) ;
#243914 = VECTOR ( 'NONE', #104275, 1000.000000000000000 ) ;
#243915 = CARTESIAN_POINT ( 'NONE',  ( -21.14999999999999858, 26.06832281015329755, -254.4051978787608732 ) ) ;
#243916 = CARTESIAN_POINT ( 'NONE',  ( 20.95512820512820440, 8.876151316299271343, -142.5586289951409640 ) ) ;
#243917 = CIRCLE ( 'NONE', #214876, 0.09999999999999080458 ) ;
#243918 = CYLINDRICAL_SURFACE ( 'NONE', #28546, 0.09999999999999939493 ) ;
#243919 = AXIS2_PLACEMENT_3D ( 'NONE', #10014, #27043, #167835 ) ;
#243920 = ORIENTED_EDGE ( 'NONE', *, *, #129233, .T. ) ;
#243921 = AXIS2_PLACEMENT_3D ( 'NONE', #72946, #110746, #232004 ) ;
#243922 = ADVANCED_FACE ( 'NONE', ( #14178 ), #234880, .T. ) ;
#243924 = EDGE_LOOP ( 'NONE', ( #122984, #66258, #249877, #127097 ) ) ;
#243923 = ORIENTED_EDGE ( 'NONE', *, *, #118530, .F. ) ;
#243925 = ORIENTED_EDGE ( 'NONE', *, *, #252435, .F. ) ;
#243926 = ADVANCED_FACE ( 'NONE', ( #254029 ), #138063, .T. ) ;
#243927 = DIRECTION ( 'NONE',  ( 0.000000000000000000, -0.2617529984165031243, -0.9651348961777157509 ) ) ;
#243928 = DIRECTION ( 'NONE',  ( -1.000000000000000000, 1.836970198721029934E-16, 1.282749433769087757E-30 ) ) ;
#243929 = EDGE_CURVE ( 'NONE', #7208, #191970, #199212, .T. ) ;
#243931 = EDGE_CURVE ( 'NONE', #155591, #92348, #67163, .T. ) ;
#243930 = AXIS2_PLACEMENT_3D ( 'NONE', #2727, #203520, #181408 ) ;
#243933 = CARTESIAN_POINT ( 'NONE',  ( -13.22483237240078324, 9.436674251842845251, -15.17686193099921255 ) ) ;
#243932 = DIRECTION ( 'NONE',  ( -1.000000000000000000, 0.000000000000000000, 0.000000000000000000 ) ) ;
#243934 = DIRECTION ( 'NONE',  ( 1.000000000000000000, 0.000000000000000000, -0.000000000000000000 ) ) ;
#243936 = EDGE_LOOP ( 'NONE', ( #53395, #66434, #170971, #173768 ) ) ;
#243935 = CIRCLE ( 'NONE', #139872, 0.09999999999999939493 ) ;
#243937 = CARTESIAN_POINT ( 'NONE',  ( 23.14999999999999503, 11.65000000001116298, -88.35000000000003695 ) ) ;
#243938 = DIRECTION ( 'NONE',  ( 0.000000000000000000, 0.000000000000000000, 1.000000000000000000 ) ) ;
#243939 = AXIS2_PLACEMENT_3D ( 'NONE', #163511, #98674, #195284 ) ;
#243940 = DIRECTION ( 'NONE',  ( -0.000000000000000000, -6.982962677686266711E-15, 1.000000000000000000 ) ) ;
#243941 = ADVANCED_FACE ( 'NONE', ( #119680 ), #97500, .T. ) ;
#243942 = CARTESIAN_POINT ( 'NONE',  ( -20.85000000000000142, -1.164121893230052995, -208.8148480855715832 ) ) ;
#243943 = ORIENTED_EDGE ( 'NONE', *, *, #165335, .T. ) ;
#243944 = ADVANCED_FACE ( 'NONE', ( #136646 ), #58936, .T. ) ;
#243946 = ADVANCED_FACE ( 'NONE', ( #217460 ), #88157, .F. ) ;
#243945 = ADVANCED_FACE ( 'NONE', ( #16733 ), #204884, .F. ) ;
#243947 = CARTESIAN_POINT ( 'NONE',  ( 21.51976009735019346, 6.910458441670357388, -134.0000000000000000 ) ) ;
#243948 = DIRECTION ( 'NONE',  ( 1.000000000000000000, 0.000000000000000000, 0.000000000000000000 ) ) ;
#243949 = ORIENTED_EDGE ( 'NONE', *, *, #46474, .T. ) ;
#243950 = ORIENTED_EDGE ( 'NONE', *, *, #38387, .F. ) ;
#243951 = CARTESIAN_POINT ( 'NONE',  ( -16.87435696428308063, 66.04999753707934929, -56.87311571935783405 ) ) ;
#243952 = PLANE ( 'NONE',  #14747 ) ;
#243953 = AXIS2_PLACEMENT_3D ( 'NONE', #105285, #244822, #4909 ) ;
#243954 = DIRECTION ( 'NONE',  ( 1.000000000000000000, -0.000000000000000000, -0.000000000000000000 ) ) ;
#243955 = DIRECTION ( 'NONE',  ( 1.000000000000000000, 0.000000000000000000, 0.000000000000000000 ) ) ;
#243956 = CARTESIAN_POINT ( 'NONE',  ( -17.11825945287482753, 12.51174298335651791, -211.2216088517780292 ) ) ;
#243957 = LINE ( 'NONE', #10503, #16867 ) ;
#243958 = ORIENTED_EDGE ( 'NONE', *, *, #166601, .F. ) ;
#243959 = DIRECTION ( 'NONE',  ( 0.000000000000000000, -0.1350103645451945777, 0.9908441862701590219 ) ) ;
#243960 = DIRECTION ( 'NONE',  ( 0.000000000000000000, 0.000000000000000000, 1.000000000000000000 ) ) ;
#243961 = CARTESIAN_POINT ( 'NONE',  ( -21.05000000000000071, 0.03175835306654922752, -60.74115287691999754 ) ) ;
#243962 = EDGE_CURVE ( 'NONE', #29621, #66961, #96238, .T. ) ;
#243964 = DIRECTION ( 'NONE',  ( -1.000000000000000000, 0.000000000000000000, 0.000000000000000000 ) ) ;
#243963 = CARTESIAN_POINT ( 'NONE',  ( -18.59999999999999787, 0.000000000000000000, 0.000000000000000000 ) ) ;
#243965 = CYLINDRICAL_SURFACE ( 'NONE', #108198, 0.09999999999999789613 ) ;
#243966 = CARTESIAN_POINT ( 'NONE',  ( -18.59999999999999787, 51.33926024308902925, -230.0993571250899379 ) ) ;
#243967 = FACE_OUTER_BOUND ( 'NONE', #128589, .T. ) ;
#243968 = DIRECTION ( 'NONE',  ( 1.000000000000000000, 0.000000000000000000, 0.000000000000000000 ) ) ;
#243969 = ADVANCED_FACE ( 'NONE', ( #55803 ), #121547, .T. ) ;
#243970 = ADVANCED_FACE ( 'NONE', ( #239621 ), #38319, .T. ) ;
#243972 = ORIENTED_EDGE ( 'NONE', *, *, #1108, .T. ) ;
#243971 = DIRECTION ( 'NONE',  ( 0.000000000000000000, -0.9915357197604792727, 0.1298341882520475943 ) ) ;
#243973 = TOROIDAL_SURFACE ( 'NONE', #144001, 11.70000000000000107, 0.1000000000000000056 ) ;
#243974 = ADVANCED_FACE ( 'NONE', ( #135363 ), #17987, .T. ) ;
#243975 = EDGE_CURVE ( 'NONE', #146245, #16782, #71644, .T. ) ;
#243976 = CARTESIAN_POINT ( 'NONE',  ( 20.94999999999999929, -11.29603075032412995, -137.0478991596638991 ) ) ;
#243977 = CARTESIAN_POINT ( 'NONE',  ( -23.15000000000000213, 64.40000000001219860, -143.4513107147999449 ) ) ;
#243978 = CARTESIAN_POINT ( 'NONE',  ( -2.995603634470829482E-16, -6.214048216528735402, -227.6835268426532082 ) ) ;
#243979 = CIRCLE ( 'NONE', #89854, 0.1000000000000070832 ) ;
#243980 = ORIENTED_EDGE ( 'NONE', *, *, #204758, .T. ) ;
#243981 = CARTESIAN_POINT ( 'NONE',  ( 21.05000000000000071, 6.540656951712400691, -100.6000000000000369 ) ) ;
#243982 = CARTESIAN_POINT ( 'NONE',  ( 18.49999999999996803, 7.070967871809997973, -171.2465642218683115 ) ) ;
#243983 = FACE_OUTER_BOUND ( 'NONE', #12890, .T. ) ;
#243984 = VECTOR ( 'NONE', #153345, 1000.000000000000000 ) ;
#243985 = VERTEX_POINT ( 'NONE', #118395 ) ;
#243986 = DIRECTION ( 'NONE',  ( -1.000000000000000000, -0.000000000000000000, -0.000000000000000000 ) ) ;
#243988 = ORIENTED_EDGE ( 'NONE', *, *, #44649, .F. ) ;
#243987 = FACE_OUTER_BOUND ( 'NONE', #204443, .T. ) ;
#243990 = DIRECTION ( 'NONE',  ( 0.000000000000000000, 0.4930308989874729320, 0.8700118002898605818 ) ) ;
#243989 = FACE_OUTER_BOUND ( 'NONE', #137253, .T. ) ;
#243991 = CARTESIAN_POINT ( 'NONE',  ( 20.94999999999999574, 79.10508929521364507, -235.9670348125907537 ) ) ;
#243992 = ORIENTED_EDGE ( 'NONE', *, *, #117599, .F. ) ;
#243993 = FACE_OUTER_BOUND ( 'NONE', #117943, .T. ) ;
#243994 = CARTESIAN_POINT ( 'NONE',  ( 0.000000000000000000, 0.000000000000000000, 0.000000000000000000 ) ) ;
#243995 = CARTESIAN_POINT ( 'NONE',  ( 21.05000000000000071, 67.07338541492498507, -128.0514244653012383 ) ) ;
#243996 = DIRECTION ( 'NONE',  ( 0.000000000000000000, -0.8814952561688476074, 0.4721928772777262417 ) ) ;
#243997 = ORIENTED_EDGE ( 'NONE', *, *, #251396, .F. ) ;
#243998 = DIRECTION ( 'NONE',  ( -1.000000000000000000, -0.000000000000000000, -0.000000000000000000 ) ) ;
#243999 = AXIS2_PLACEMENT_3D ( 'NONE', #138650, #239079, #214371 ) ;
#244000 = DIRECTION ( 'NONE',  ( -1.000000000000000000, 0.000000000000000000, 0.000000000000000000 ) ) ;
#244001 = B_SPLINE_CURVE_WITH_KNOTS ( 'NONE', 3,
 ( #205721, #141899, #243575, #27132, #24551, #221417, #106605, #166643 ),
 .UNSPECIFIED., .F., .F.,
 ( 4, 2, 2, 4 ),
 ( 0.000000000000000000, 0.0001094981963948554304, 0.0002189963927897108607, 0.0004379927855794217215 ),
 .UNSPECIFIED. ) ;
#244002 = FACE_OUTER_BOUND ( 'NONE', #211463, .T. ) ;
#244003 = VERTEX_POINT ( 'NONE', #117107 ) ;
#244004 = ORIENTED_EDGE ( 'NONE', *, *, #90004, .T. ) ;
#244005 = CARTESIAN_POINT ( 'NONE',  ( 21.13461538461538680, 65.38541703798651383, -124.1731074845243654 ) ) ;
#244006 = CYLINDRICAL_SURFACE ( 'NONE', #161216, 12.87499999999999822 ) ;
#244007 = DIRECTION ( 'NONE',  ( 0.000000000000000000, -8.717686153663073805E-15, 1.000000000000000000 ) ) ;
#244008 = EDGE_CURVE ( 'NONE', #31617, #8702, #196520, .T. ) ;
#244009 = CARTESIAN_POINT ( 'NONE',  ( 20.94999999999999929, 10.47338541492405106, -141.5786544642485580 ) ) ;
#244010 = DIRECTION ( 'NONE',  ( -0.000000000000000000, 0.8660254037844383745, -0.5000000000000003331 ) ) ;
#244013 = DIRECTION ( 'NONE',  ( 1.000000000000000000, 0.000000000000000000, 0.000000000000000000 ) ) ;
#244012 = AXIS2_PLACEMENT_3D ( 'NONE', #191644, #189042, #10413 ) ;
#244011 = CARTESIAN_POINT ( 'NONE',  ( 20.85000000000000142, 70.29876110920605470, -198.0544810472949564 ) ) ;
#244014 = CARTESIAN_POINT ( 'NONE',  ( -18.59999999999999787, 57.82359945636609666, -226.0354702357591350 ) ) ;
#244015 = ADVANCED_FACE ( 'NONE', ( #246038 ), #67393, .T. ) ;
#244016 = AXIS2_PLACEMENT_3D ( 'NONE', #214604, #236728, #213317 ) ;
#244017 = CARTESIAN_POINT ( 'NONE',  ( 23.14999999999998437, 64.25000000001215028, -136.5231074845243597 ) ) ;
#244018 = LINE ( 'NONE', #225724, #88839 ) ;
#244019 = TOROIDAL_SURFACE ( 'NONE', #135685, 0.2000000000000000111, 0.1000000000000000056 ) ;
#244020 = CYLINDRICAL_SURFACE ( 'NONE', #81536, 0.09999999999999939493 ) ;
#244021 = AXIS2_PLACEMENT_3D ( 'NONE', #187447, #231708, #28398 ) ;
#244023 = ORIENTED_EDGE ( 'NONE', *, *, #157121, .T. ) ;
#244022 = FACE_OUTER_BOUND ( 'NONE', #181481, .T. ) ;
#244024 = CARTESIAN_POINT ( 'NONE',  ( -20.94684162521793525, 64.25000000001209344, -129.6814634907268271 ) ) ;
#244025 = DIRECTION ( 'NONE',  ( 0.000000000000000000, 0.000000000000000000, 1.000000000000000000 ) ) ;
#244027 = CYLINDRICAL_SURFACE ( 'NONE', #207667, 0.5000000000000004441 ) ;
#244026 = DIRECTION ( 'NONE',  ( -0.000000000000000000, 0.4088369013363281623, -0.9126074666063771490 ) ) ;
#244028 = EDGE_CURVE ( 'NONE', #153561, #171180, #223878, .T. ) ;
#244029 = ADVANCED_FACE ( 'NONE', ( #123518 ), #146905, .T. ) ;
#244030 = ORIENTED_EDGE ( 'NONE', *, *, #219530, .T. ) ;
#244031 = CARTESIAN_POINT ( 'NONE',  ( -16.89208623190940273, 66.04842205103652475, -115.6678352813060968 ) ) ;
#244032 = DIRECTION ( 'NONE',  ( 1.000000000000000000, -0.000000000000000000, -0.000000000000000000 ) ) ;
#244033 = FACE_OUTER_BOUND ( 'NONE', #98225, .T. ) ;
#244034 = DIRECTION ( 'NONE',  ( 0.000000000000000000, 0.000000000000000000, -1.000000000000000000 ) ) ;
#244035 = CARTESIAN_POINT ( 'NONE',  ( -13.11924609551134857, 66.56831044948847875, -185.2438174522883685 ) ) ;
#244036 = ORIENTED_EDGE ( 'NONE', *, *, #243391, .F. ) ;
#244037 = ORIENTED_EDGE ( 'NONE', *, *, #45863, .F. ) ;
#244038 = DIRECTION ( 'NONE',  ( 0.000000000000000000, 1.000000000000000000, 2.891205793294679805E-16 ) ) ;
#244039 = EDGE_LOOP ( 'NONE', ( #194802, #102484, #193795, #247995 ) ) ;
#244040 = DIRECTION ( 'NONE',  ( -1.000000000000000000, -0.000000000000000000, 0.000000000000000000 ) ) ;
#244041 = AXIS2_PLACEMENT_3D ( 'NONE', #232661, #73597, #34472 ) ;
#244042 = EDGE_LOOP ( 'NONE', ( #49986, #56140, #49934, #254609, #83600, #212742, #243750, #183621, #158389, #162916, #31907 ) ) ;
#244043 = EDGE_CURVE ( 'NONE', #170331, #194531, #34249, .T. ) ;
#244044 = DIRECTION ( 'NONE',  ( 0.000000000000000000, -0.2617529984165031243, -0.9651348961777157509 ) ) ;
#244045 = EDGE_CURVE ( 'NONE', #242569, #141218, #59115, .T. ) ;
#244046 = CARTESIAN_POINT ( 'NONE',  ( 23.14999999999999503, 6.650000000011155876, -88.35000000000003695 ) ) ;
#244047 = CARTESIAN_POINT ( 'NONE',  ( -21.05000000000000071, 62.82351852614505106, -207.2177435922979498 ) ) ;
#244049 = ORIENTED_EDGE ( 'NONE', *, *, #201092, .T. ) ;
#244048 = CIRCLE ( 'NONE', #194194, 12.87499999999999822 ) ;
#244050 = AXIS2_PLACEMENT_3D ( 'NONE', #12897, #92392, #234469 ) ;
#244051 = FACE_OUTER_BOUND ( 'NONE', #28928, .T. ) ;
#244053 = CARTESIAN_POINT ( 'NONE',  ( -20.54999999999999716, 74.07476635515205032, -90.29286395139820343 ) ) ;
#244052 = CIRCLE ( 'NONE', #31719, 0.09999999999999939493 ) ;
#244054 = CYLINDRICAL_SURFACE ( 'NONE', #161786, 0.09999999999999939493 ) ;
#244055 = CARTESIAN_POINT ( 'NONE',  ( -23.25000000000000000, -9.599999999988845900, -124.1060308773475924 ) ) ;
#244056 = CARTESIAN_POINT ( 'NONE',  ( -16.97048326478265423, 44.58366951172476433, -235.0981489915114082 ) ) ;
#244057 = EDGE_CURVE ( 'NONE', #185124, #220406, #238210, .T. ) ;
#244058 = CARTESIAN_POINT ( 'NONE',  ( 18.59999999999999076, 69.55000000001159322, -59.50608031408435039 ) ) ;
#244059 = CARTESIAN_POINT ( 'NONE',  ( -23.25000000000000000, 1.115600667400684642E-11, -171.4000000000000341 ) ) ;
#244061 = ORIENTED_EDGE ( 'NONE', *, *, #114701, .F. ) ;
#244060 = EDGE_CURVE ( 'NONE', #187820, #31603, #84329, .T. ) ;
#244063 = FACE_OUTER_BOUND ( 'NONE', #160264, .T. ) ;
#244062 = CARTESIAN_POINT ( 'NONE',  ( -21.05000000000000071, 87.65000000001163016, -66.52310748452423184 ) ) ;
#244064 = EDGE_LOOP ( 'NONE', ( #87528, #20691, #235690, #80789 ) ) ;
#244066 = ORIENTED_EDGE ( 'NONE', *, *, #68852, .F. ) ;
#244065 = DIRECTION ( 'NONE',  ( 1.000000000000000000, 0.000000000000000000, -0.000000000000000000 ) ) ;
#244067 = VECTOR ( 'NONE', #178159, 1000.000000000000000 ) ;
#244068 = ORIENTED_EDGE ( 'NONE', *, *, #228875, .T. ) ;
#244069 = CARTESIAN_POINT ( 'NONE',  ( -23.25000000000000000, 8.793666940903476004, -220.9353059101866847 ) ) ;
#244070 = CIRCLE ( 'NONE', #206658, 0.3999999999999975797 ) ;
#244071 = CARTESIAN_POINT ( 'NONE',  ( -20.94999999999999929, 77.36242903720540198, -128.6342262366031548 ) ) ;
#244072 = VECTOR ( 'NONE', #6701, 1000.000000000000227 ) ;
#244073 = DIRECTION ( 'NONE',  ( 0.000000000000000000, 0.000000000000000000, -1.000000000000000000 ) ) ;
#244074 = DIRECTION ( 'NONE',  ( 0.000000000000000000, 0.000000000000000000, 1.000000000000000000 ) ) ;
#244075 = EDGE_LOOP ( 'NONE', ( #70832, #178123, #164168, #197898 ) ) ;
#244076 = CARTESIAN_POINT ( 'NONE',  ( 20.94999999999999929, 85.50000000001207923, -126.6291383618717816 ) ) ;
#244077 = LINE ( 'NONE', #159432, #60515 ) ;
#244078 = AXIS2_PLACEMENT_3D ( 'NONE', #13914, #111723, #93428 ) ;
#244079 = EDGE_CURVE ( 'NONE', #76552, #117708, #126063, .T. ) ;
#244080 = ORIENTED_EDGE ( 'NONE', *, *, #32032, .F. ) ;
#244081 = ADVANCED_FACE ( 'NONE', ( #163933 ), #244728, .T. ) ;
#244082 = CARTESIAN_POINT ( 'NONE',  ( -20.93975676684922504, 10.31104185822947450, -39.02045169831057336 ) ) ;
#244083 = AXIS2_PLACEMENT_3D ( 'NONE', #77101, #74579, #154122 ) ;
#244084 = EDGE_CURVE ( 'NONE', #89005, #48580, #66107, .T. ) ;
#244085 = ORIENTED_EDGE ( 'NONE', *, *, #218245, .F. ) ;
#244086 = CARTESIAN_POINT ( 'NONE',  ( -16.84981964351498007, 9.917318234109995245, -146.8696016140195013 ) ) ;
#244087 = ORIENTED_EDGE ( 'NONE', *, *, #177607, .F. ) ;
#244088 = DIRECTION ( 'NONE',  ( 1.000000000000000000, 0.000000000000000000, 0.000000000000000000 ) ) ;
#244089 = ORIENTED_EDGE ( 'NONE', *, *, #249628, .T. ) ;
#244090 = FACE_OUTER_BOUND ( 'NONE', #113266, .T. ) ;
#244091 = B_SPLINE_CURVE_WITH_KNOTS ( 'NONE', 3,
 ( #57900, #98289, #192305, #235262, #137437, #55315, #216975, #78749, #56598, #38365, #214416, #35814, #117885, #197422, #18784, #158342 ),
 .UNSPECIFIED., .F., .F.,
 ( 4, 3, 3, 3, 3, 4 ),
 ( 0.000000000000000000, 3.357088238233517998E-05, 6.714213034887110308E-05, 0.0001007408646120942151, 0.0001343627955914231033, 0.0001573956632896011476 ),
 .UNSPECIFIED. ) ;
#244092 = LINE ( 'NONE', #184119, #143351 ) ;
#244093 = EDGE_CURVE ( 'NONE', #255703, #105984, #180928, .T. ) ;
#244094 = CARTESIAN_POINT ( 'NONE',  ( -20.64999999999999858, 76.00000000001170974, -69.52310748452431710 ) ) ;
#244095 = AXIS2_PLACEMENT_3D ( 'NONE', #251498, #9047, #250226 ) ;
#244096 = AXIS2_PLACEMENT_3D ( 'NONE', #204375, #221360, #24492 ) ;
#244097 = ADVANCED_FACE ( 'NONE', ( #184765 ), #171616, .T. ) ;
#244098 = VECTOR ( 'NONE', #132657, 1000.000000000000000 ) ;
#244099 = CIRCLE ( 'NONE', #131687, 0.1000000000000017958 ) ;
#244100 = LINE ( 'NONE', #185423, #90577 ) ;
#244101 = CARTESIAN_POINT ( 'NONE',  ( -20.09999999999999787, 4.645987002755569861, 21.91686199900910736 ) ) ;
#244102 = DIRECTION ( 'NONE',  ( 0.000000000000000000, 0.2617529984165026802, 0.9651348961777159730 ) ) ;
#244103 = ORIENTED_EDGE ( 'NONE', *, *, #197470, .T. ) ;
#244105 = CARTESIAN_POINT ( 'NONE',  ( 23.14999999999999503, 11.65000000001116298, -126.9851942293460922 ) ) ;
#244104 = DIRECTION ( 'NONE',  ( 0.000000000000000000, 6.982962677686266711E-15, -1.000000000000000000 ) ) ;
#244106 = AXIS2_PLACEMENT_3D ( 'NONE', #204391, #6196, #240974 ) ;
#244107 = CARTESIAN_POINT ( 'NONE',  ( -23.15000000000000213, 76.00000000001246292, -172.1231074845243540 ) ) ;
#244108 = CARTESIAN_POINT ( 'NONE',  ( -21.05000000000000071, -1.835341550213255957, -45.15515129256298366 ) ) ;
#244110 = ORIENTED_EDGE ( 'NONE', *, *, #19680, .T. ) ;
#244109 = CARTESIAN_POINT ( 'NONE',  ( -18.50000000000000000, -9.480686695267820596, -207.9411151687577899 ) ) ;
#244112 = ORIENTED_EDGE ( 'NONE', *, *, #125210, .T. ) ;
#244111 = CARTESIAN_POINT ( 'NONE',  ( 18.59999999999999076, 10.20857864377385127, -88.35000000000003695 ) ) ;
#244113 = CARTESIAN_POINT ( 'NONE',  ( -23.25000000000000000, -0.1008583690875562017, -88.75043287651064361 ) ) ;
#244115 = DIRECTION ( 'NONE',  ( 1.000000000000000000, 0.000000000000000000, 0.000000000000000000 ) ) ;
#244114 = AXIS2_PLACEMENT_3D ( 'NONE', #142873, #222403, #205426 ) ;
#244116 = DIRECTION ( 'NONE',  ( 3.469446951953498700E-14, -0.7899159663865300551, -0.6132151058540831201 ) ) ;
#244117 = LINE ( 'NONE', #65483, #192816 ) ;
#244118 = TOROIDAL_SURFACE ( 'NONE', #131703, 0.4000000000000012990, 0.1000000000000000056 ) ;
#244120 = ORIENTED_EDGE ( 'NONE', *, *, #161502, .F. ) ;
#244119 = CARTESIAN_POINT ( 'NONE',  ( 21.14999999999999858, 67.21339244341217523, -157.7731074845244166 ) ) ;
#244121 = AXIS2_PLACEMENT_3D ( 'NONE', #110930, #254272, #173529 ) ;
#244122 = DIRECTION ( 'NONE',  ( -0.000000000000000000, 0.9126074666063771490, 0.4088369013363281623 ) ) ;
#244123 = ORIENTED_EDGE ( 'NONE', *, *, #162823, .F. ) ;
#244124 = ORIENTED_EDGE ( 'NONE', *, *, #196871, .T. ) ;
#244125 = AXIS2_PLACEMENT_3D ( 'NONE', #148001, #244516, #8497 ) ;
#244126 = DIRECTION ( 'NONE',  ( 1.000000000000000000, 0.000000000000000000, 0.000000000000000000 ) ) ;
#244127 = CARTESIAN_POINT ( 'NONE',  ( -20.64999999999999858, -9.499999999988846255, -157.6060308773475924 ) ) ;
#244128 = ORIENTED_EDGE ( 'NONE', *, *, #213971, .T. ) ;
#244129 = CARTESIAN_POINT ( 'NONE',  ( -16.97683809663752186, 62.88879881541066652, -213.8537543555185607 ) ) ;
#244130 = CARTESIAN_POINT ( 'NONE',  ( 18.49999999999998934, 69.35000000001156195, -57.17310748452436542 ) ) ;
#244131 = VERTEX_POINT ( 'NONE', #127371 ) ;
#244132 = AXIS2_PLACEMENT_3D ( 'NONE', #184610, #120819, #103762 ) ;
#244133 = CARTESIAN_POINT ( 'NONE',  ( -16.89208623190940273, 66.04842205103602737, -48.66783528130612524 ) ) ;
#244134 = AXIS2_PLACEMENT_3D ( 'NONE', #118721, #198228, #27346 ) ;
#244135 = CIRCLE ( 'NONE', #60978, 0.09999999999999939493 ) ;
#244136 = ORIENTED_EDGE ( 'NONE', *, *, #176981, .F. ) ;
#244137 = ORIENTED_EDGE ( 'NONE', *, *, #223023, .T. ) ;
#244138 = CARTESIAN_POINT ( 'NONE',  ( -18.33981767444254984, -9.569575789793166365, -73.81916184372514067 ) ) ;
#244139 = EDGE_LOOP ( 'NONE', ( #116488, #223423, #94486, #209627 ) ) ;
#244140 = CARTESIAN_POINT ( 'NONE',  ( 18.52351027002947603, -0.8635125639127735342, -242.3458057457398809 ) ) ;
#244142 = EDGE_CURVE ( 'NONE', #4508, #19453, #243457, .T. ) ;
#244141 = ORIENTED_EDGE ( 'NONE', *, *, #67489, .F. ) ;
#244144 = ORIENTED_EDGE ( 'NONE', *, *, #74431, .F. ) ;
#244143 = DIRECTION ( 'NONE',  ( -1.000000000000000000, -2.952720810173289112E-16, 0.000000000000000000 ) ) ;
#244145 = CARTESIAN_POINT ( 'NONE',  ( -18.59999999999999787, 66.65000000001157332, -57.27310748452438816 ) ) ;
#244146 = EDGE_LOOP ( 'NONE', ( #181809, #127991, #64947, #200052 ) ) ;
#244147 = EDGE_CURVE ( 'NONE', #95143, #96628, #63230, .T. ) ;
#244148 = DIRECTION ( 'NONE',  ( 0.000000000000000000, -1.000000000000000000, 0.000000000000000000 ) ) ;
#244149 = ADVANCED_FACE ( 'NONE', ( #85631 ), #161374, .T. ) ;
#244150 = EDGE_LOOP ( 'NONE', ( #140789, #191625, #191468 ) ) ;
#244152 = ORIENTED_EDGE ( 'NONE', *, *, #173557, .T. ) ;
#244151 = ORIENTED_EDGE ( 'NONE', *, *, #24910, .T. ) ;
#244153 = DIRECTION ( 'NONE',  ( -0.000000000000000000, 0.9910465087640861759, 0.1335171055202901691 ) ) ;
#244154 = CIRCLE ( 'NONE', #131740, 4.299999999999956302 ) ;
#244155 = CARTESIAN_POINT ( 'NONE',  ( -20.94999999999999929, 86.25530027761219287, -209.3091956463349277 ) ) ;
#244156 = CIRCLE ( 'NONE', #131744, 0.3999999999999975797 ) ;
#244157 = ORIENTED_EDGE ( 'NONE', *, *, #135523, .T. ) ;
#244158 = AXIS2_PLACEMENT_3D ( 'NONE', #12882, #140483, #178371 ) ;
#244159 = ORIENTED_EDGE ( 'NONE', *, *, #58847, .T. ) ;
#244160 = EDGE_CURVE ( 'NONE', #73041, #9423, #63527, .T. ) ;
#244161 = DIRECTION ( 'NONE',  ( -0.000000000000000000, 0.4721928772777345684, 0.8814952561688429444 ) ) ;
#244162 = DIRECTION ( 'NONE',  ( 1.000000000000000000, 0.000000000000000000, 0.000000000000000000 ) ) ;
#244164 = EDGE_LOOP ( 'NONE', ( #122607, #18651, #112304, #26769 ) ) ;
#244163 = DIRECTION ( 'NONE',  ( 1.000000000000000000, 0.000000000000000000, 0.000000000000000000 ) ) ;
#244165 = DIRECTION ( 'NONE',  ( 0.000000000000000000, 0.000000000000000000, -1.000000000000000000 ) ) ;
#244166 = ORIENTED_EDGE ( 'NONE', *, *, #216867, .F. ) ;
#244167 = CARTESIAN_POINT ( 'NONE',  ( 20.85000000000000142, 75.77017861926654518, -203.7552340087416951 ) ) ;
#244168 = DIRECTION ( 'NONE',  ( 0.7071067811865456854, -0.7071067811865493491, -0.000000000000000000 ) ) ;
#244169 = ORIENTED_EDGE ( 'NONE', *, *, #154720, .T. ) ;
#244170 = DIRECTION ( 'NONE',  ( -0.000000000000000000, 1.000000000000000000, 6.982962677686266711E-15 ) ) ;
#244171 = PLANE ( 'NONE',  #153241 ) ;
#244172 = ORIENTED_EDGE ( 'NONE', *, *, #153689, .T. ) ;
#244173 = CARTESIAN_POINT ( 'NONE',  ( -18.69999999999999929, 0.000000000000000000, 0.000000000000000000 ) ) ;
#244174 = ORIENTED_EDGE ( 'NONE', *, *, #201994, .F. ) ;
#244175 = VECTOR ( 'NONE', #187795, 1000.000000000000000 ) ;
#244177 = EDGE_LOOP ( 'NONE', ( #63934, #146733, #195985, #104295 ) ) ;
#244176 = ORIENTED_EDGE ( 'NONE', *, *, #213862, .T. ) ;
#244178 = VERTEX_POINT ( 'NONE', #143060 ) ;
#244179 = EDGE_CURVE ( 'NONE', #72990, #115688, #86928, .T. ) ;
#244180 = ORIENTED_EDGE ( 'NONE', *, *, #231876, .F. ) ;
#244181 = EDGE_CURVE ( 'NONE', #13038, #137086, #229846, .T. ) ;
#244182 = CARTESIAN_POINT ( 'NONE',  ( 22.50497660315936344, 25.96815610755211523, -254.4267512576819286 ) ) ;
#244183 = ORIENTED_EDGE ( 'NONE', *, *, #252346, .T. ) ;
#244184 = CARTESIAN_POINT ( 'NONE',  ( -18.59999999999999787, 68.97833521811233481, -166.1895420826271277 ) ) ;
#244185 = VECTOR ( 'NONE', #17537, 1000.000000000000000 ) ;
#244186 = FACE_OUTER_BOUND ( 'NONE', #145349, .T. ) ;
#244187 = ORIENTED_EDGE ( 'NONE', *, *, #228184, .T. ) ;
#244189 = EDGE_CURVE ( 'NONE', #43410, #3957, #107800, .T. ) ;
#244188 = EDGE_LOOP ( 'NONE', ( #118004, #53423, #60288, #204064, #182268 ) ) ;
#244190 = AXIS2_PLACEMENT_3D ( 'NONE', #66682, #163220, #146200 ) ;
#244191 = ORIENTED_EDGE ( 'NONE', *, *, #249823, .F. ) ;
#244192 = AXIS2_PLACEMENT_3D ( 'NONE', #181811, #60565, #196228 ) ;
#244193 = AXIS2_PLACEMENT_3D ( 'NONE', #167586, #191002, #90576 ) ;
#244194 = DIRECTION ( 'NONE',  ( 0.000000000000000000, 0.000000000000000000, -1.000000000000000000 ) ) ;
#244195 = ORIENTED_EDGE ( 'NONE', *, *, #86783, .T. ) ;
#244196 = CARTESIAN_POINT ( 'NONE',  ( 21.14999999999999858, 76.00000000001219291, -143.0637644362255401 ) ) ;
#244198 = EDGE_LOOP ( 'NONE', ( #6147, #241440, #150884, #15499, #64334 ) ) ;
#244197 = CARTESIAN_POINT ( 'NONE',  ( -18.59999999999999787, 44.01574086017817677, -236.0100308471058099 ) ) ;
#244199 = CARTESIAN_POINT ( 'NONE',  ( -22.59999999999999787, 76.00000000001195133, -103.0231074845243171 ) ) ;
#244200 = FACE_OUTER_BOUND ( 'NONE', #32158, .T. ) ;
#244201 = CARTESIAN_POINT ( 'NONE',  ( -18.59999999999999787, 11.75000000001115552, -134.0000000000000284 ) ) ;
#244203 = EDGE_CURVE ( 'NONE', #137582, #99703, #32145, .T. ) ;
#244202 = DIRECTION ( 'NONE',  ( 2.978066053179067751E-16, -1.000000000000000000, 0.000000000000000000 ) ) ;
#244205 = CARTESIAN_POINT ( 'NONE',  ( -23.15000000000000213, 2.600000000011156054, -55.25000000000004974 ) ) ;
#244204 = CARTESIAN_POINT ( 'NONE',  ( -23.25000000000000355, 70.35000000001153353, -48.67310748452436542 ) ) ;
#244206 = DIRECTION ( 'NONE',  ( 1.000000000000000000, 0.000000000000000000, 0.000000000000000000 ) ) ;
#244207 = CARTESIAN_POINT ( 'NONE',  ( 23.24999999999999645, 76.00000000001126921, -203.5231074845248997 ) ) ;
#244208 = CARTESIAN_POINT ( 'NONE',  ( 23.14999999999999858, 45.93587830916155212, -239.9163948487882863 ) ) ;
#244209 = CARTESIAN_POINT ( 'NONE',  ( -23.25000000000000000, 4.554494125284476169, -212.9355439031026265 ) ) ;
#244210 = AXIS2_PLACEMENT_3D ( 'NONE', #224448, #164500, #221860 ) ;
#244211 = ORIENTED_EDGE ( 'NONE', *, *, #14198, .F. ) ;
#244212 = AXIS2_PLACEMENT_3D ( 'NONE', #84045, #144053, #223587 ) ;
#244213 = EDGE_CURVE ( 'NONE', #62686, #142859, #117424, .T. ) ;
#244215 = ORIENTED_EDGE ( 'NONE', *, *, #114081, .F. ) ;
#244214 = DIRECTION ( 'NONE',  ( 1.000000000000000000, -0.000000000000000000, -0.000000000000000000 ) ) ;
#244216 = AXIS2_PLACEMENT_3D ( 'NONE', #164885, #238313, #235745 ) ;
#244217 = EDGE_LOOP ( 'NONE', ( #157863, #185630, #156319, #13002 ) ) ;
#244218 = CARTESIAN_POINT ( 'NONE',  ( 21.14999999999999858, 12.37888392014804495, -249.8746333190754569 ) ) ;
#244219 = SPHERICAL_SURFACE ( 'NONE', #44530, 0.1000000000000000056 ) ;
#244220 = CIRCLE ( 'NONE', #119348, 0.1999999999999996503 ) ;
#244221 = ADVANCED_FACE ( 'NONE', ( #112945 ), #52954, .T. ) ;
#244222 = EDGE_CURVE ( 'NONE', #35875, #103565, #192433, .T. ) ;
#244223 = AXIS2_PLACEMENT_3D ( 'NONE', #123323, #89307, #69779 ) ;
#244224 = FACE_OUTER_BOUND ( 'NONE', #19698, .T. ) ;
#244225 = ORIENTED_EDGE ( 'NONE', *, *, #33597, .F. ) ;
#244226 = SURFACE_STYLE_FILL_AREA ( #141296 ) ;
#244227 = CARTESIAN_POINT ( 'NONE',  ( 20.94999999999999929, 42.96960653111219131, -254.4772109693542745 ) ) ;
#244228 = LINE ( 'NONE', #3048, #112046 ) ;
#244229 = ORIENTED_EDGE ( 'NONE', *, *, #136652, .F. ) ;
#244230 = EDGE_CURVE ( 'NONE', #217355, #188830, #146610, .T. ) ;
#244232 = CARTESIAN_POINT ( 'NONE',  ( -18.59999999999999787, 77.83585931145600512, -158.4186683157258244 ) ) ;
#244231 = CIRCLE ( 'NONE', #86005, 0.09999999999999939493 ) ;
#244233 = LINE ( 'NONE', #20082, #167157 ) ;
#244234 = EDGE_CURVE ( 'NONE', #188456, #253877, #67523, .T. ) ;
#244235 = CIRCLE ( 'NONE', #190103, 11.90000000000000746 ) ;
#244236 = DIRECTION ( 'NONE',  ( 0.000000000000000000, -0.9126074666063770380, -0.4088369013363281068 ) ) ;
#244237 = CIRCLE ( 'NONE', #223388, 0.09999999999999939493 ) ;
#244238 = CARTESIAN_POINT ( 'NONE',  ( 18.52928932188133970, 15.28939250479744949, -222.8979625946709007 ) ) ;
#244240 = ORIENTED_EDGE ( 'NONE', *, *, #87893, .F. ) ;
#244239 = DIRECTION ( 'NONE',  ( 0.000000000000000000, -1.000000000000000000, 0.000000000000000000 ) ) ;
#244241 = EDGE_CURVE ( 'NONE', #53873, #144717, #208997, .T. ) ;
#244242 = DIRECTION ( 'NONE',  ( 1.000000000000000000, -0.000000000000000000, -0.000000000000000000 ) ) ;
#244243 = FACE_OUTER_BOUND ( 'NONE', #36703, .T. ) ;
#244244 = CYLINDRICAL_SURFACE ( 'NONE', #12680, 0.09999999999998898659 ) ;
#244245 = FACE_OUTER_BOUND ( 'NONE', #221846, .T. ) ;
#244246 = ORIENTED_EDGE ( 'NONE', *, *, #86688, .T. ) ;
#244247 = CARTESIAN_POINT ( 'NONE',  ( -16.94107738177415712, 10.01423928514777728, -79.55000000000005400 ) ) ;
#244248 = CARTESIAN_POINT ( 'NONE',  ( 18.39999999999999503, 64.52683809664974035, -149.1731074845244507 ) ) ;
#244249 = EDGE_CURVE ( 'NONE', #56290, #196101, #167332, .T. ) ;
#244251 = DIRECTION ( 'NONE',  ( -1.000000000000000000, 1.207181226542539700E-16, -2.694675058168174199E-16 ) ) ;
#244250 = CARTESIAN_POINT ( 'NONE',  ( -20.94999999999999929, 64.40000000001177227, -76.45131071479988805 ) ) ;
#244252 = CARTESIAN_POINT ( 'NONE',  ( -5.899999999999938183, 64.75000000001119815, -22.12310748452479103 ) ) ;
#244253 = CARTESIAN_POINT ( 'NONE',  ( -21.00219873199078435, 64.39461131213575129, -163.1104600562298401 ) ) ;
#244254 = DIRECTION ( 'NONE',  ( -7.304098846218443309E-16, -0.4088369013363783999, 0.9126074666063545004 ) ) ;
#244255 = CARTESIAN_POINT ( 'NONE',  ( 18.54116936837188589, 85.46356419838456020, -129.4745649936359939 ) ) ;
#244256 = CARTESIAN_POINT ( 'NONE',  ( -16.78805706634180339, 9.948252493082335945, -87.84415320803191207 ) ) ;
#244257 = EDGE_CURVE ( 'NONE', #14889, #31859, #233937, .T. ) ;
#244258 = EDGE_CURVE ( 'NONE', #186437, #162457, #254738, .T. ) ;
#244259 = ORIENTED_EDGE ( 'NONE', *, *, #147446, .F. ) ;
#244260 = DIRECTION ( 'NONE',  ( -0.000000000000000000, -6.982962677686266711E-15, 1.000000000000000000 ) ) ;
#244261 = VERTEX_POINT ( 'NONE', #11277 ) ;
#244262 = ORIENTED_EDGE ( 'NONE', *, *, #143391, .F. ) ;
#244263 = EDGE_CURVE ( 'NONE', #159227, #235467, #242307, .T. ) ;
#244264 = FACE_OUTER_BOUND ( 'NONE', #136827, .T. ) ;
#244265 = CARTESIAN_POINT ( 'NONE',  ( -22.50000000000000000, 11.75000000001115552, -67.00000000000004263 ) ) ;
#244266 = ORIENTED_EDGE ( 'NONE', *, *, #16713, .F. ) ;
#244267 = EDGE_CURVE ( 'NONE', #86390, #67836, #191224, .T. ) ;
#244268 = VECTOR ( 'NONE', #251172, 1000.000000000000000 ) ;
#244269 = EDGE_CURVE ( 'NONE', #26849, #55598, #242492, .T. ) ;
#244270 = CIRCLE ( 'NONE', #127772, 0.1000000000000002554 ) ;
#244271 = ORIENTED_EDGE ( 'NONE', *, *, #45667, .T. ) ;
#244272 = CIRCLE ( 'NONE', #169328, 11.74999999999999645 ) ;
#244273 = CIRCLE ( 'NONE', #90146, 0.1000000000000028644 ) ;
#244274 = ADVANCED_FACE ( 'NONE', ( #229046 ), #150782, .T. ) ;
#244275 = EDGE_LOOP ( 'NONE', ( #47617, #111264, #31861, #60360 ) ) ;
#244276 = SPHERICAL_SURFACE ( 'NONE', #220889, 0.1000000000000000056 ) ;
#244277 = ORIENTED_EDGE ( 'NONE', *, *, #92879, .T. ) ;
#244278 = CIRCLE ( 'NONE', #227534, 0.1000000000000028644 ) ;
#244279 = FACE_OUTER_BOUND ( 'NONE', #250728, .T. ) ;
#244280 = CYLINDRICAL_SURFACE ( 'NONE', #170221, 0.1000000000000000472 ) ;
#244281 = CARTESIAN_POINT ( 'NONE',  ( -21.05000000000000071, 18.26942912180536638, -237.6183358664095238 ) ) ;
#244282 = CARTESIAN_POINT ( 'NONE',  ( -20.94999999999999929, 1.115649653272650466E-11, -104.5000000000000568 ) ) ;
#244283 = CARTESIAN_POINT ( 'NONE',  ( 23.24999999999999645, 0.000000000000000000, 0.000000000000000000 ) ) ;
#244284 =( BOUNDED_CURVE ( )  B_SPLINE_CURVE ( 3, ( #139418, #122459, #218966, #20800 ),
 .UNSPECIFIED., .F., .F. ) 
 B_SPLINE_CURVE_WITH_KNOTS ( ( 4, 4 ),
 ( 4.712388980384689674, 6.283185307179586232 ),
 .UNSPECIFIED. ) 
 CURVE ( )  GEOMETRIC_REPRESENTATION_ITEM ( )  RATIONAL_B_SPLINE_CURVE ( ( 1.000000000000000000, 0.8047378541243649375, 0.8047378541243649375, 1.000000000000000000 ) ) 
 REPRESENTATION_ITEM ( '' )  );
#244285 = DIRECTION ( 'NONE',  ( 0.000000000000000000, 0.4721928772777346239, 0.8814952561688430555 ) ) ;
#244286 = CARTESIAN_POINT ( 'NONE',  ( -21.64999999999999858, 29.33122518167236237, -237.2878098217501588 ) ) ;
#244288 = ORIENTED_EDGE ( 'NONE', *, *, #104793, .F. ) ;
#244287 = CARTESIAN_POINT ( 'NONE',  ( 21.04999999999999716, 44.12019864330184049, -236.4877982702160182 ) ) ;
#244290 = CARTESIAN_POINT ( 'NONE',  ( 18.39999999999999858, -9.599999999988845900, -174.2001893912220680 ) ) ;
#244289 = DIRECTION ( 'NONE',  ( 0.000000000000000000, 0.000000000000000000, -1.000000000000000000 ) ) ;
#244291 = ADVANCED_FACE ( 'NONE', ( #93367 ), #1037, .T. ) ;
#244292 = LINE ( 'NONE', #47368, #107394 ) ;
#244293 = ORIENTED_EDGE ( 'NONE', *, *, #134961, .F. ) ;
#244294 = DIRECTION ( 'NONE',  ( 0.7071067811865474617, 0.7071067811865474617, -0.000000000000000000 ) ) ;
#244295 = CARTESIAN_POINT ( 'NONE',  ( -21.00000000000000000, 0.000000000000000000, 4.100000000000000533 ) ) ;
#244296 = CARTESIAN_POINT ( 'NONE',  ( -20.64999999999999858, 9.614325556249161409, -211.5456030694648746 ) ) ;
#244298 = EDGE_LOOP ( 'NONE', ( #72242, #220160, #233729, #103562 ) ) ;
#244297 = CIRCLE ( 'NONE', #131887, 0.3999999999999975797 ) ;
#244299 = VECTOR ( 'NONE', #225415, 1000.000000000000000 ) ;
#244301 = CARTESIAN_POINT ( 'NONE',  ( -20.54999999999999716, -11.74999999998884626, -179.8499999999999943 ) ) ;
#244300 = DIRECTION ( 'NONE',  ( 0.000000000000000000, 0.000000000000000000, 1.000000000000000000 ) ) ;
#244302 = CYLINDRICAL_SURFACE ( 'NONE', #14854, 0.09999999999998898659 ) ;
#244303 = ORIENTED_EDGE ( 'NONE', *, *, #203332, .F. ) ;
#244304 = CARTESIAN_POINT ( 'NONE',  ( 21.07928932188134397, 6.328516656404468144, -66.90110485434564680 ) ) ;
#244305 = CARTESIAN_POINT ( 'NONE',  ( 18.59999999999999787, -9.749999999999996447, 31.39999999999999858 ) ) ;
#244306 = CARTESIAN_POINT ( 'NONE',  ( -18.39999999999999858, -0.7490476236415797295, -242.2033265267442061 ) ) ;
#244307 = AXIS2_PLACEMENT_3D ( 'NONE', #180715, #218516, #21638 ) ;
#244308 = LINE ( 'NONE', #46113, #165906 ) ;
#244309 = VERTEX_POINT ( 'NONE', #152091 ) ;
#244310 = ORIENTED_EDGE ( 'NONE', *, *, #241977, .F. ) ;
#244311 = CARTESIAN_POINT ( 'NONE',  ( -16.95709691156737620, 66.05000000001255955, -182.6831650470390969 ) ) ;
#244312 = DIRECTION ( 'NONE',  ( 0.000000000000000000, -0.9770955615653259541, -0.2128009952263860971 ) ) ;
#244313 = EDGE_CURVE ( 'NONE', #238489, #115296, #196695, .T. ) ;
#244314 = DIRECTION ( 'NONE',  ( 1.000000000000000000, 1.541880601228652843E-16, 2.878400969107353907E-16 ) ) ;
#244315 = CARTESIAN_POINT ( 'NONE',  ( -18.59999999999999787, 51.38014393322265505, -230.1906178717505611 ) ) ;
#244316 = CIRCLE ( 'NONE', #106951, 11.65000000000000036 ) ;
#244317 = CIRCLE ( 'NONE', #44619, 0.1000000000000000472 ) ;
#244318 = CARTESIAN_POINT ( 'NONE',  ( 18.79999999999999716, 11.61130914238355771, -1.800000000000000044 ) ) ;
#244319 = ADVANCED_FACE ( 'NONE', ( #247302 ), #49103, .F. ) ;
#244320 = CIRCLE ( 'NONE', #119446, 0.09999999999999939493 ) ;
#244321 = AXIS2_PLACEMENT_3D ( 'NONE', #29437, #231467, #69828 ) ;
#244322 = DIRECTION ( 'NONE',  ( 1.000000000000000000, 0.000000000000000000, 0.000000000000000000 ) ) ;
#244323 = ORIENTED_EDGE ( 'NONE', *, *, #64134, .F. ) ;
#244324 = CARTESIAN_POINT ( 'NONE',  ( 21.05000000000000071, 70.88170441948386724, -234.2197789011331679 ) ) ;
#244326 = EDGE_LOOP ( 'NONE', ( #90642, #8642, #157471, #123274 ) ) ;
#244325 = DIRECTION ( 'NONE',  ( 0.000000000000000000, -4.163336342344333240E-14, -1.000000000000000000 ) ) ;
#244327 = CARTESIAN_POINT ( 'NONE',  ( 23.14999999999999503, 10.99842653345846699, -220.2504445088529792 ) ) ;
#244328 = CARTESIAN_POINT ( 'NONE',  ( 22.39999999999999503, 7.790779598384535376, -66.90000000000004832 ) ) ;
#244329 = CARTESIAN_POINT ( 'NONE',  ( -21.14999999999999858, 76.00000000001169553, -76.06376443622556849 ) ) ;
#244330 = CARTESIAN_POINT ( 'NONE',  ( 11.60000000000000320, -12.24999999999999822, 15.00000000000000355 ) ) ;
#244331 = EDGE_CURVE ( 'NONE', #239085, #231547, #254950, .T. ) ;
#244332 = CYLINDRICAL_SURFACE ( 'NONE', #100471, 0.09999999999999939493 ) ;
#244334 = ORIENTED_EDGE ( 'NONE', *, *, #35591, .F. ) ;
#244333 = CARTESIAN_POINT ( 'NONE',  ( 12.25000000000000000, 66.15000000001204228, -119.7731074845243739 ) ) ;
#244335 = DIRECTION ( 'NONE',  ( 0.000000000000000000, -0.1568667991644714932, 0.9876197685951274563 ) ) ;
#244336 = PLANE ( 'NONE',  #249601 ) ;
#244337 = CARTESIAN_POINT ( 'NONE',  ( -22.39999999999999858, 76.00000000001273293, -211.3138870828977645 ) ) ;
#244338 = DIRECTION ( 'NONE',  ( 0.000000000000000000, -0.5859227990963362664, -0.8103668758649469339 ) ) ;
#244339 = VERTEX_POINT ( 'NONE', #257519 ) ;
#244340 = FACE_OUTER_BOUND ( 'NONE', #174211, .T. ) ;
#244341 = CARTESIAN_POINT ( 'NONE',  ( -16.84981964351502270, 66.08268176591298015, -115.8927090985433352 ) ) ;
#244342 = CARTESIAN_POINT ( 'NONE',  ( -18.54270223418605923, 87.05302002691458085, -199.5363343069655571 ) ) ;
#244343 = AXIS2_PLACEMENT_3D ( 'NONE', #136190, #32020, #114084 ) ;
#244345 = TOROIDAL_SURFACE ( 'NONE', #19518, 11.65000000000000036, 0.1000000000000000056 ) ;
#244344 = CARTESIAN_POINT ( 'NONE',  ( -18.50000000000000711, 78.21981816082171690, -231.3313247107103052 ) ) ;
#244346 = VERTEX_POINT ( 'NONE', #56780 ) ;
#244347 = CARTESIAN_POINT ( 'NONE',  ( -16.80070461187905551, 9.950000000011138823, -87.85303617083869199 ) ) ;
#244348 = ORIENTED_EDGE ( 'NONE', *, *, #159099, .F. ) ;
#244350 = DIRECTION ( 'NONE',  ( 0.000000000000000000, -0.9126074666063770380, -0.4088369013363281068 ) ) ;
#244349 = CIRCLE ( 'NONE', #19323, 0.1000000000000028644 ) ;
#244351 = CARTESIAN_POINT ( 'NONE',  ( -20.54999999999999716, 1.115600667400684642E-11, -67.00000000000004263 ) ) ;
#244352 = CARTESIAN_POINT ( 'NONE',  ( -23.25000000000000000, 4.349999999999999645, -21.34999999999999787 ) ) ;
#244353 = CARTESIAN_POINT ( 'NONE',  ( 18.46921299892753510, -9.509378177812612520, -174.4865787093704341 ) ) ;
#244354 = ORIENTED_EDGE ( 'NONE', *, *, #17346, .F. ) ;
#244355 =( BOUNDED_SURFACE ( )  B_SPLINE_SURFACE ( 3, 2, ( 
 ( #234229, #116861, #156012 ),
 ( #235514, #238080, #175571 ),
 ( #55564, #253785, #73918 ),
 ( #157299, #17740, #15209 ),
 ( #137683, #56849, #115572 ),
 ( #59415, #255022, #196389 ) ),
 .UNSPECIFIED., .F., .F., .F. ) 
 B_SPLINE_SURFACE_WITH_KNOTS ( ( 4, 2, 4 ),
 ( 3, 3 ),
 ( 1.570796326794897668, 2.356194490192346169, 3.141592653589794448 ),
 ( 0.000000000000000000, 1.000000000000000000 ),
 .UNSPECIFIED. ) 
 GEOMETRIC_REPRESENTATION_ITEM ( )  RATIONAL_B_SPLINE_SURFACE ( (
 ( 1.000000000000000000, 0.7071067811865475727, 1.000000000000000000),
 ( 1.000000000000000000, 0.6611148371756124797, 1.000000000000000000),
 ( 1.000000000000000000, 0.6092287576726203024, 1.000000000000000000),
 ( 1.000000000000000000, 0.5278258667029250839, 1.000000000000000000),
 ( 1.000000000000000000, 0.4993418825354254964, 1.000000000000000000),
 ( 1.000000000000000000, 0.5000000000000260902, 1.000000000000000000) ) ) 
 REPRESENTATION_ITEM ( '' )  SURFACE ( )  );
#244356 = B_SPLINE_CURVE_WITH_KNOTS ( 'NONE', 3,
 ( #156733, #112452, #236231, #57579, #133288, #53743, #191998, #13340 ),
 .UNSPECIFIED., .F., .F.,
 ( 4, 2, 2, 4 ),
 ( 0.000000000000000000, 0.0001306511400391301332, 0.0001959767100586967854, 0.0002613022800782634106 ),
 .UNSPECIFIED. ) ;
#244357 = DIRECTION ( 'NONE',  ( 1.000000000000000000, 0.000000000000000000, 0.000000000000000000 ) ) ;
#244358 = DIRECTION ( 'NONE',  ( 0.000000000000000000, 0.2617529984165021806, 0.9651348961777159730 ) ) ;
#244359 = LINE ( 'NONE', #246930, #53781 ) ;
#244360 = CARTESIAN_POINT ( 'NONE',  ( -16.80621392010911563, 9.942202577507737615, -20.81040803458294164 ) ) ;
#244361 = VECTOR ( 'NONE', #172761, 1000.000000000000000 ) ;
#244362 = EDGE_CURVE ( 'NONE', #196464, #92669, #59294, .T. ) ;
#244363 = DIRECTION ( 'NONE',  ( 1.000000000000000000, -7.304098846218134667E-16, -4.639676173203993355E-30 ) ) ;
#244364 = EDGE_LOOP ( 'NONE', ( #239169, #61795, #105542, #127542, #245841, #224345, #102286, #207558, #83460, #141834, #103296, #228632 ) ) ;
#244366 = ORIENTED_EDGE ( 'NONE', *, *, #24922, .F. ) ;
#244365 = CARTESIAN_POINT ( 'NONE',  ( 20.86777300164945004, 10.33200063080771969, -106.0931674956643320 ) ) ;
#244367 = EDGE_LOOP ( 'NONE', ( #6585, #134050, #226371, #246447, #230306, #202178, #197605, #166196, #128219, #250192, #8042, #181678, #59334, #54302, #122359, #71455 ) ) ;
#244368 = DIRECTION ( 'NONE',  ( 0.000000000000000000, -6.938893903907233900E-15, 1.000000000000000000 ) ) ;
#244369 = ORIENTED_EDGE ( 'NONE', *, *, #27133, .T. ) ;
#244370 = DIRECTION ( 'NONE',  ( 1.000000000000000000, 0.000000000000000000, 0.000000000000000000 ) ) ;
#244371 = CARTESIAN_POINT ( 'NONE',  ( 18.59999999999999076, 74.16465844978787914, -158.3679561919613832 ) ) ;
#244372 = CARTESIAN_POINT ( 'NONE',  ( -20.54999999999999716, 87.75000000001223555, -148.8731074845242972 ) ) ;
#244373 = ORIENTED_EDGE ( 'NONE', *, *, #23057, .T. ) ;
#244374 = FACE_OUTER_BOUND ( 'NONE', #130084, .T. ) ;
#244375 = CARTESIAN_POINT ( 'NONE',  ( -21.05000000000000071, -1.835341550213255957, -112.0551512925630107 ) ) ;
#244376 = CIRCLE ( 'NONE', #131955, 0.09999999999999939493 ) ;
#244377 = LINE ( 'NONE', #217420, #197705 ) ;
#244378 = EDGE_CURVE ( 'NONE', #151955, #228147, #254905, .T. ) ;
#244379 = ORIENTED_EDGE ( 'NONE', *, *, #171973, .T. ) ;
#244380 = CARTESIAN_POINT ( 'NONE',  ( 22.49544290803769897, 11.74987023786852802, -100.4346880407425573 ) ) ;
#244382 = ORIENTED_EDGE ( 'NONE', *, *, #202883, .T. ) ;
#244381 = DIRECTION ( 'NONE',  ( 1.000000000000000000, 0.000000000000000000, 0.000000000000000000 ) ) ;
#244384 = EDGE_CURVE ( 'NONE', #186223, #238367, #155046, .T. ) ;
#244383 = CARTESIAN_POINT ( 'NONE',  ( -23.15000000000000213, 4.349999999999999645, -21.14999999999999858 ) ) ;
#244385 = CIRCLE ( 'NONE', #231941, 0.09999999999999993616 ) ;
#244386 = VECTOR ( 'NONE', #79674, 1000.000000000000000 ) ;
#244387 = CIRCLE ( 'NONE', #227818, 0.4000000000000114575 ) ;
#244388 = ORIENTED_EDGE ( 'NONE', *, *, #185596, .F. ) ;
#244389 =( BOUNDED_SURFACE ( )  B_SPLINE_SURFACE ( 3, 2, ( 
 ( #45966, #121679, #240330 ),
 ( #223306, #43404, #125505 ),
 ( #201189, #22568, #162088 ),
 ( #205017, #23870, #103356 ),
 ( #4258, #83767, #163361 ),
 ( #6843, #64252, #143775 ) ),
 .UNSPECIFIED., .F., .F., .F. ) 
 B_SPLINE_SURFACE_WITH_KNOTS ( ( 4, 2, 4 ),
 ( 3, 3 ),
 ( 1.570796326794897668, 2.356194490192346169, 3.141592653589794448 ),
 ( 0.000000000000000000, 1.000000000000000000 ),
 .UNSPECIFIED. ) 
 GEOMETRIC_REPRESENTATION_ITEM ( )  RATIONAL_B_SPLINE_SURFACE ( (
 ( 1.000000000000000000, 0.7071067811864701902, 1.000000000000000000),
 ( 1.000000000000000000, 0.6611148371806441215, 1.000000000000000000),
 ( 1.000000000000000000, 0.6092287576661893356, 1.000000000000000000),
 ( 1.000000000000000000, 0.5278258667090959255, 1.000000000000000000),
 ( 1.000000000000000000, 0.4993418825306182307, 1.000000000000000000),
 ( 1.000000000000000000, 0.5000000000001614264, 1.000000000000000000) ) ) 
 REPRESENTATION_ITEM ( '' )  SURFACE ( )  );
#244391 = PLANE ( 'NONE',  #76885 ) ;
#244390 = AXIS2_PLACEMENT_3D ( 'NONE', #98039, #161924, #65364 ) ;
#244393 = EDGE_CURVE ( 'NONE', #79119, #193842, #134152, .T. ) ;
#244392 = CARTESIAN_POINT ( 'NONE',  ( -18.36973785203556275, 11.47550320048421924, -24.25000000000000000 ) ) ;
#244394 = LINE ( 'NONE', #43642, #14414 ) ;
#244396 = VERTEX_POINT ( 'NONE', #135043 ) ;
#244395 = AXIS2_PLACEMENT_3D ( 'NONE', #152527, #132944, #175935 ) ;
#244397 = DIRECTION ( 'NONE',  ( -1.000000000000000000, -7.304098846218164250E-16, 4.217023435051628197E-16 ) ) ;
#244398 = AXIS2_PLACEMENT_3D ( 'NONE', #230519, #253908, #152282 ) ;
#244399 = EDGE_CURVE ( 'NONE', #64013, #91812, #159320, .T. ) ;
#244400 = FACE_OUTER_BOUND ( 'NONE', #6265, .T. ) ;
#244401 = ADVANCED_FACE ( 'NONE', ( #94649 ), #136319, .T. ) ;
#244402 = ORIENTED_EDGE ( 'NONE', *, *, #7442, .T. ) ;
#244403 = EDGE_CURVE ( 'NONE', #47002, #1289, #215866, .T. ) ;
#244404 = CIRCLE ( 'NONE', #48775, 0.1000000000000032391 ) ;
#244405 = AXIS2_PLACEMENT_3D ( 'NONE', #207615, #6827, #88914 ) ;
#244406 = ORIENTED_EDGE ( 'NONE', *, *, #246762, .F. ) ;
#244407 = CARTESIAN_POINT ( 'NONE',  ( 21.09793522318408066, 65.27537548979982773, -191.2838166135473728 ) ) ;
#244408 = VECTOR ( 'NONE', #164444, 1000.000000000000000 ) ;
#244409 = VERTEX_POINT ( 'NONE', #198890 ) ;
#244410 = CIRCLE ( 'NONE', #198622, 0.1999999999999987899 ) ;
#244411 = DIRECTION ( 'NONE',  ( 1.000000000000000000, 0.000000000000000000, 0.000000000000000000 ) ) ;
#244413 = EDGE_CURVE ( 'NONE', #236044, #225653, #197599, .T. ) ;
#244412 = CARTESIAN_POINT ( 'NONE',  ( 21.15000000000005187, 76.00000000001119815, -36.02310748452479316 ) ) ;
#244415 = ORIENTED_EDGE ( 'NONE', *, *, #159403, .F. ) ;
#244414 = CARTESIAN_POINT ( 'NONE',  ( -16.81453046979149235, 9.939102281452070642, -146.7117265236030619 ) ) ;
#244417 = DIRECTION ( 'NONE',  ( -1.000000000000000000, 0.000000000000000000, -0.000000000000000000 ) ) ;
#244416 = B_SPLINE_CURVE_WITH_KNOTS ( 'NONE', 3,
 ( #218046, #155568, #39470, #96803, #197218, #177697, #115124, #257143, #35620, #215498 ),
 .UNSPECIFIED., .F., .F.,
 ( 4, 2, 2, 2, 4 ),
 ( 0.000000000000000000, 4.221631689686865393E-05, 8.443263379373730786E-05, 0.0001688652675874746157, 0.0003377305351749315589 ),
 .UNSPECIFIED. ) ;
#244419 = AXIS2_PLACEMENT_3D ( 'NONE', #145330, #125768, #26705 ) ;
#244418 = DIRECTION ( 'NONE',  ( -1.000000000000000000, 0.000000000000000000, -0.000000000000000000 ) ) ;
#244420 = DIRECTION ( 'NONE',  ( 0.000000000000000000, -0.9126074666063774821, -0.4088369013363273297 ) ) ;
#244421 = CARTESIAN_POINT ( 'NONE',  ( 21.12230431290518951, 75.99479014832267865, -75.98067413781733137 ) ) ;
#244422 = AXIS2_PLACEMENT_3D ( 'NONE', #151593, #72038, #154180 ) ;
#244423 = SPHERICAL_SURFACE ( 'NONE', #60202, 0.1000000000000000056 ) ;
#244424 = CARTESIAN_POINT ( 'NONE',  ( -20.64999999999999858, 4.350000000011156054, -45.85000000000000142 ) ) ;
#244425 = FACE_OUTER_BOUND ( 'NONE', #8427, .T. ) ;
#244426 = CARTESIAN_POINT ( 'NONE',  ( 18.59999999999999076, 33.98796489282361932, -236.2185561567993091 ) ) ;
#244428 = ORIENTED_EDGE ( 'NONE', *, *, #12273, .F. ) ;
#244427 = FACE_OUTER_BOUND ( 'NONE', #227716, .T. ) ;
#244429 = DIRECTION ( 'NONE',  ( 1.000000000000000000, 0.000000000000000000, -0.000000000000000000 ) ) ;
#244430 = ORIENTED_EDGE ( 'NONE', *, *, #131007, .T. ) ;
#244431 = DIRECTION ( 'NONE',  ( -0.000000000000000000, -6.982962677686266711E-15, 1.000000000000000000 ) ) ;
#244432 = VECTOR ( 'NONE', #103105, 1000.000000000000000 ) ;
#244433 = AXIS2_PLACEMENT_3D ( 'NONE', #48639, #53784, #107333 ) ;
#244434 = DIRECTION ( 'NONE',  ( 0.000000000000000000, -1.000000000000000000, 0.000000000000000000 ) ) ;
#244435 = CARTESIAN_POINT ( 'NONE',  ( -21.14999999999999858, 75.90220970870291239, -75.78092209500043452 ) ) ;
#244436 = CARTESIAN_POINT ( 'NONE',  ( 20.12481660106788439, 66.47365600773768790, -195.2969658154282229 ) ) ;
#244437 = DIRECTION ( 'NONE',  ( 0.000000000000000000, 0.000000000000000000, -1.000000000000000000 ) ) ;
#244438 = ORIENTED_EDGE ( 'NONE', *, *, #209753, .T. ) ;
#244439 = CARTESIAN_POINT ( 'NONE',  ( -16.97683809663752186, 9.950000000011138823, -147.4023640181965220 ) ) ;
#244440 = DIRECTION ( 'NONE',  ( 0.000000000000000000, 1.000000000000000000, 0.000000000000000000 ) ) ;
#244441 = CIRCLE ( 'NONE', #56985, 0.1000000000000001721 ) ;
#244442 = ORIENTED_EDGE ( 'NONE', *, *, #173080, .F. ) ;
#244444 = ADVANCED_FACE ( 'NONE', ( #34709 ), #18961, .T. ) ;
#244443 = CARTESIAN_POINT ( 'NONE',  ( 20.94999999999999929, 69.28189128378591022, -247.5258150475912089 ) ) ;
#244446 = CARTESIAN_POINT ( 'NONE',  ( -18.50000000000000000, 86.87843599112028414, -199.3967987332378584 ) ) ;
#244445 = CIRCLE ( 'NONE', #11431, 0.09999999999999939493 ) ;
#244447 = ORIENTED_EDGE ( 'NONE', *, *, #232919, .F. ) ;
#244448 = CARTESIAN_POINT ( 'NONE',  ( -21.05000000000000071, 6.413662734880551497, -67.08559286336239325 ) ) ;
#244449 = ORIENTED_EDGE ( 'NONE', *, *, #116198, .T. ) ;
#244451 = EDGE_CURVE ( 'NONE', #99123, #241925, #80190, .T. ) ;
#244450 = CARTESIAN_POINT ( 'NONE',  ( -18.40000000000000213, 64.52683809664949877, -112.3490535513323323 ) ) ;
#244452 = ORIENTED_EDGE ( 'NONE', *, *, #110945, .T. ) ;
#244453 = TOROIDAL_SURFACE ( 'NONE', #140401, 0.6000000000000009770, 0.1000000000000000056 ) ;
#244454 = DIRECTION ( 'NONE',  ( 1.000000000000000000, 0.000000000000000000, 0.000000000000000000 ) ) ;
#244455 = CIRCLE ( 'NONE', #132043, 0.09999999999999108213 ) ;
#244456 = EDGE_CURVE ( 'NONE', #125186, #129332, #17674, .T. ) ;
#244457 = CARTESIAN_POINT ( 'NONE',  ( 14.11444803880197441, 9.457431528860068326, -182.4999169378996555 ) ) ;
#244459 = EDGE_CURVE ( 'NONE', #239804, #7829, #158511, .T. ) ;
#244458 = CIRCLE ( 'NONE', #165374, 0.1000000000000013933 ) ;
#244460 = CIRCLE ( 'NONE', #206875, 0.09999999999999997780 ) ;
#244461 = EDGE_LOOP ( 'NONE', ( #202503, #32529, #124130, #91981 ) ) ;
#244462 = CARTESIAN_POINT ( 'NONE',  ( 23.14999999999999858, 5.950000000011160139, -123.6942976949652149 ) ) ;
#244464 = ORIENTED_EDGE ( 'NONE', *, *, #249621, .F. ) ;
#244463 = CARTESIAN_POINT ( 'NONE',  ( -20.94999999999999929, -1.249999999988843369, -41.50000000000000000 ) ) ;
#244465 = CARTESIAN_POINT ( 'NONE',  ( 21.11345278033224560, 67.11787792664171093, -191.2770853137656104 ) ) ;
#244466 = VERTEX_POINT ( 'NONE', #114222 ) ;
#244467 = AXIS2_PLACEMENT_3D ( 'NONE', #160527, #38013, #77106 ) ;
#244468 = VERTEX_POINT ( 'NONE', #59343 ) ;
#244469 = ADVANCED_FACE ( 'NONE', ( #196317 ), #176784, .T. ) ;
#244470 = CARTESIAN_POINT ( 'NONE',  ( 18.59999999999999076, 76.00000000001190870, -103.0231074845243029 ) ) ;
#244471 = DIRECTION ( 'NONE',  ( -0.000000000000000000, 6.982962677686266711E-15, -1.000000000000000000 ) ) ;
#244472 = CARTESIAN_POINT ( 'NONE',  ( -18.50000000000000000, 9.250000000011157297, -188.8499999999999659 ) ) ;
#244473 = EDGE_CURVE ( 'NONE', #92498, #128191, #62760, .T. ) ;
#244474 = CARTESIAN_POINT ( 'NONE',  ( -22.39999999999999858, 11.75000000001115552, -133.9000000000000057 ) ) ;
#244475 = VECTOR ( 'NONE', #69155, 1000.000000000000000 ) ;
#244476 = DIRECTION ( 'NONE',  ( -2.812466655313719426E-14, 0.1350103645451904977, 0.9908441862701596881 ) ) ;
#244477 = CARTESIAN_POINT ( 'NONE',  ( 13.40000000000005898, 64.25000000001119815, -21.02310748452479316 ) ) ;
#244478 = TOROIDAL_SURFACE ( 'NONE', #161308, 0.9750000000000019762, 0.1000000000000000056 ) ;
#244479 = ORIENTED_EDGE ( 'NONE', *, *, #130505, .T. ) ;
#244480 = DIRECTION ( 'NONE',  ( 0.000000000000000000, 0.000000000000000000, 1.000000000000000000 ) ) ;
#244481 = DIRECTION ( 'NONE',  ( 0.000000000000000000, -0.8777080977375132376, 0.4791956752371582251 ) ) ;
#244483 = LINE ( 'NONE', #86667, #195315 ) ;
#244482 = PRODUCT_RELATED_PRODUCT_CATEGORY ( 'part', '', ( #151478 ) ) ;
#244484 = CARTESIAN_POINT ( 'NONE',  ( 21.12642695952774119, 1.555420789734674569, -230.6349773343582115 ) ) ;
#244485 = ORIENTED_EDGE ( 'NONE', *, *, #148858, .F. ) ;
#244486 = CARTESIAN_POINT ( 'NONE',  ( -23.15000000000000213, 74.08971962618026907, -123.8917396293253717 ) ) ;
#244487 = EDGE_LOOP ( 'NONE', ( #93912, #48567, #223960, #93856, #71721 ) ) ;
#244488 = CARTESIAN_POINT ( 'NONE',  ( 13.43443725621853169, 9.446557523083692232, -115.5899419543459459 ) ) ;
#244490 = ORIENTED_EDGE ( 'NONE', *, *, #82356, .T. ) ;
#244489 = TOROIDAL_SURFACE ( 'NONE', #152962, 0.2000000000000000111, 0.1000000000000000056 ) ;
#244491 = DIRECTION ( 'NONE',  ( -1.000000000000000000, 0.000000000000000000, 0.000000000000000000 ) ) ;
#244492 = DIRECTION ( 'NONE',  ( -1.000000000000000000, -0.000000000000000000, -0.000000000000000000 ) ) ;
#244493 = ADVANCED_FACE ( 'NONE', ( #253716 ), #104887, .T. ) ;
#244494 = ORIENTED_EDGE ( 'NONE', *, *, #30355, .F. ) ;
#244495 = ORIENTED_EDGE ( 'NONE', *, *, #9093, .F. ) ;
#244497 = ORIENTED_EDGE ( 'NONE', *, *, #166969, .F. ) ;
#244496 = DIRECTION ( 'NONE',  ( 0.000000000000000000, -6.982962677686266711E-15, 1.000000000000000000 ) ) ;
#244498 = EDGE_CURVE ( 'NONE', #98456, #66524, #21755, .T. ) ;
#244499 = CARTESIAN_POINT ( 'NONE',  ( -21.05000000000000071, 77.26178616857691850, -94.93660852097882241 ) ) ;
#244500 = ORIENTED_EDGE ( 'NONE', *, *, #101106, .F. ) ;
#244501 = EDGE_CURVE ( 'NONE', #190938, #173155, #150918, .T. ) ;
#244502 = DIRECTION ( 'NONE',  ( -1.000000000000000000, 0.000000000000000000, 0.000000000000000000 ) ) ;
#244503 = FACE_OUTER_BOUND ( 'NONE', #46391, .T. ) ;
#244504 = ORIENTED_EDGE ( 'NONE', *, *, #107906, .F. ) ;
#244505 = DIRECTION ( 'NONE',  ( 0.000000000000000000, 0.4999999999999689138, -0.8660254037844565822 ) ) ;
#244506 = CARTESIAN_POINT ( 'NONE',  ( 18.49999999999998934, 33.78581792236875003, -236.3841486493325874 ) ) ;
#244507 = AXIS2_PLACEMENT_3D ( 'NONE', #86307, #169771, #165902 ) ;
#244508 = CIRCLE ( 'NONE', #219560, 3.999999999999999112 ) ;
#244509 = VERTEX_POINT ( 'NONE', #5804 ) ;
#244510 = CARTESIAN_POINT ( 'NONE',  ( -20.64999999999999858, 6.300962096140152013, -220.8843452229073705 ) ) ;
#244511 = CARTESIAN_POINT ( 'NONE',  ( 20.85000000000000142, 1.115600667400684642E-11, -134.0000000000000284 ) ) ;
#244513 = ORIENTED_EDGE ( 'NONE', *, *, #245838, .F. ) ;
#244512 = CYLINDRICAL_SURFACE ( 'NONE', #151521, 0.5000000000000004441 ) ;
#244514 = DIRECTION ( 'NONE',  ( -0.8660254037843505559, 0.1064004976132069402, -0.4885477807828162988 ) ) ;
#244515 = CARTESIAN_POINT ( 'NONE',  ( -21.65000000000000213, 9.950000000011140600, -79.75000000000004263 ) ) ;
#244517 = EDGE_CURVE ( 'NONE', #154893, #81857, #218102, .T. ) ;
#244516 = DIRECTION ( 'NONE',  ( 1.000000000000000000, 0.000000000000000000, 0.000000000000000000 ) ) ;
#244520 = DIRECTION ( 'NONE',  ( -1.000000000000000000, -0.000000000000000000, -0.000000000000000000 ) ) ;
#244519 = CIRCLE ( 'NONE', #132118, 0.1000000000000002831 ) ;
#244518 = DIRECTION ( 'NONE',  ( 0.000000000000000000, 0.000000000000000000, 1.000000000000000000 ) ) ;
#244521 = CARTESIAN_POINT ( 'NONE',  ( -20.94788355080264353, 65.69792220476374212, -164.5335554128461979 ) ) ;
#244522 = DIRECTION ( 'NONE',  ( 0.000000000000000000, -0.2128009952263485993, 0.9770955615653341697 ) ) ;
#244523 = CIRCLE ( 'NONE', #198736, 0.5000000000000004441 ) ;
#244524 = DIRECTION ( 'NONE',  ( 0.000000000000000000, 2.891205793294679805E-16, -1.000000000000000000 ) ) ;
#244525 = DIRECTION ( 'NONE',  ( 0.000000000000000000, 0.000000000000000000, -1.000000000000000000 ) ) ;
#244526 = VERTEX_POINT ( 'NONE', #163627 ) ;
#244527 = AXIS2_PLACEMENT_3D ( 'NONE', #56767, #192467, #210743 ) ;
#244528 = VERTEX_POINT ( 'NONE', #185754 ) ;
#244529 = EDGE_CURVE ( 'NONE', #140683, #34419, #26032, .T. ) ;
#244530 = DIRECTION ( 'NONE',  ( 1.000000000000000000, -0.000000000000000000, 0.000000000000000000 ) ) ;
#244531 = ORIENTED_EDGE ( 'NONE', *, *, #251254, .T. ) ;
#244532 = EDGE_CURVE ( 'NONE', #206526, #138829, #163399, .T. ) ;
#244533 = ORIENTED_EDGE ( 'NONE', *, *, #238293, .F. ) ;
#244534 = SURFACE_STYLE_FILL_AREA ( #85432 ) ;
#244536 = ADVANCED_FACE ( 'NONE', ( #201451 ), #188327, .F. ) ;
#244535 = CARTESIAN_POINT ( 'NONE',  ( 20.94999999999999929, -8.999999999988842703, -90.60603087734760663 ) ) ;
#244538 = ORIENTED_EDGE ( 'NONE', *, *, #186509, .F. ) ;
#244537 = COLOUR_RGB ( '', 0.66274510, 0.83137255, 0.94901961) ;
#244539 = CARTESIAN_POINT ( 'NONE',  ( 21.05000000000000071, 55.49311008795314137, -234.6486875357297492 ) ) ;
#244540 = ORIENTED_EDGE ( 'NONE', *, *, #172767, .T. ) ;
#244541 = ORIENTED_EDGE ( 'NONE', *, *, #206427, .T. ) ;
#244542 = ADVANCED_FACE ( 'NONE', ( #205295 ), #221628, .F. ) ;
#244543 = DIRECTION ( 'NONE',  ( 0.000000000000000000, 0.2128009952263606730, -0.9770955615653315052 ) ) ;
#244544 = DIRECTION ( 'NONE',  ( 1.000000000000000000, 0.000000000000000000, 0.000000000000000000 ) ) ;
#244547 = EDGE_CURVE ( 'NONE', #7750, #202760, #184227, .T. ) ;
#244546 = ORIENTED_EDGE ( 'NONE', *, *, #167076, .T. ) ;
#244545 = CARTESIAN_POINT ( 'NONE',  ( -23.15000000000000213, 49.36776662947724503, -253.7196102226803021 ) ) ;
#244548 = DIRECTION ( 'NONE',  ( -1.000000000000000000, 0.000000000000000000, 0.000000000000000000 ) ) ;
#244550 = ORIENTED_EDGE ( 'NONE', *, *, #189576, .T. ) ;
#244549 = LINE ( 'NONE', #104999, #193340 ) ;
#244551 = FACE_BOUND ( 'NONE', #139722, .T. ) ;
#244553 = CARTESIAN_POINT ( 'NONE',  ( -16.87331047859649757, 9.950000000011138823, -121.3500000000000369 ) ) ;
#244552 = CIRCLE ( 'NONE', #248662, 0.09999999999999939493 ) ;
#244554 = B_SPLINE_CURVE_WITH_KNOTS ( 'NONE', 3,
 ( #220043, #21850, #101323, #2257, #161368, #225150, #124802, #89500, #169095, #145624 ),
 .UNSPECIFIED., .F., .F.,
 ( 4, 3, 3, 4 ),
 ( 0.000000000000000000, 3.394313611811197040E-05, 6.779740500700327799E-05, 0.0001049857339142765996 ),
 .UNSPECIFIED. ) ;
#244556 = ORIENTED_EDGE ( 'NONE', *, *, #182156, .F. ) ;
#244555 = CYLINDRICAL_SURFACE ( 'NONE', #218662, 0.1000000000000028644 ) ;
#244557 = CARTESIAN_POINT ( 'NONE',  ( 18.53317502108576775, 10.32263460347359896, -173.0605957968672328 ) ) ;
#244558 = FACE_OUTER_BOUND ( 'NONE', #249787, .T. ) ;
#244559 = DIRECTION ( 'NONE',  ( 0.000000000000000000, 0.4721928772777346239, 0.8814952561688430555 ) ) ;
#244560 = VECTOR ( 'NONE', #315, 1000.000000000000000 ) ;
#244562 = CARTESIAN_POINT ( 'NONE',  ( 21.14999999999999503, 30.73962027982165424, -265.0781340245722504 ) ) ;
#244561 = DIRECTION ( 'NONE',  ( 1.000000000000000000, 0.000000000000000000, -0.000000000000000000 ) ) ;
#244563 = CARTESIAN_POINT ( 'NONE',  ( 18.59999999999999432, 1.162701749949165642, -108.6000000000000227 ) ) ;
#244564 = CARTESIAN_POINT ( 'NONE',  ( 18.50000000000000355, 85.40000000001239755, -163.1410656363516125 ) ) ;
#244565 = VECTOR ( 'NONE', #144333, 1000.000000000000000 ) ;
#244566 = CIRCLE ( 'NONE', #128060, 0.1000000000000000472 ) ;
#244567 = ADVANCED_FACE ( 'NONE', ( #181905 ), #26703, .F. ) ;
#244568 = CARTESIAN_POINT ( 'NONE',  ( -22.59999999999999787, 75.90000000001202807, -114.6726782920691221 ) ) ;
#244569 = EDGE_CURVE ( 'NONE', #76314, #111495, #142526, .T. ) ;
#244570 = ORIENTED_EDGE ( 'NONE', *, *, #125653, .T. ) ;
#244571 = EDGE_LOOP ( 'NONE', ( #234064, #211568, #85032, #119269 ) ) ;
#244572 = EDGE_LOOP ( 'NONE', ( #205351, #80575, #170011, #135797, #59318, #29594, #193711, #210065, #90182, #196226, #184606, #90156, #159186, #134214, #245036, #74586 ) ) ;
#244573 = PRODUCT_DEFINITION_FORMATION_WITH_SPECIFIED_SOURCE ( 'ANY', '', #244984, .NOT_KNOWN. ) ;
#244574 = ORIENTED_EDGE ( 'NONE', *, *, #191744, .T. ) ;
#244575 = DIRECTION ( 'NONE',  ( 0.000000000000000000, 0.000000000000000000, -1.000000000000000000 ) ) ;
#244576 = ORIENTED_EDGE ( 'NONE', *, *, #176541, .T. ) ;
#244577 = ADVANCED_FACE ( 'NONE', ( #164906 ), #124503, .F. ) ;
#244579 = CARTESIAN_POINT ( 'NONE',  ( -21.07094088545303379, 6.320167221927637691, -100.4011062974478250 ) ) ;
#244578 = AXIS2_PLACEMENT_3D ( 'NONE', #93544, #235615, #72738 ) ;
#244580 = DIRECTION ( 'NONE',  ( 0.000000000000000000, -6.530723674265620862E-15, 1.000000000000000000 ) ) ;
#244581 = EDGE_CURVE ( 'NONE', #4597, #241985, #175881, .T. ) ;
#244582 = ORIENTED_EDGE ( 'NONE', *, *, #251257, .T. ) ;
#244583 = CARTESIAN_POINT ( 'NONE',  ( 20.94999999999999929, 10.71906255309368383, -222.4921384173655383 ) ) ;
#244584 = ADVANCED_FACE ( 'NONE', ( #142751 ), #63420, .F. ) ;
#244585 = AXIS2_PLACEMENT_3D ( 'NONE', #234406, #132776, #115757 ) ;
#244586 = ORIENTED_EDGE ( 'NONE', *, *, #162717, .F. ) ;
#244587 = ORIENTED_EDGE ( 'NONE', *, *, #201924, .F. ) ;
#244588 = EDGE_LOOP ( 'NONE', ( #223289, #214874, #255559, #30299 ) ) ;
#244589 = CARTESIAN_POINT ( 'NONE',  ( -23.15000000000000213, -9.499999999988846255, -124.1060308773475924 ) ) ;
#244590 = CARTESIAN_POINT ( 'NONE',  ( 20.94999999999999929, -11.64999999998883595, -134.0000000000000284 ) ) ;
#244591 = CARTESIAN_POINT ( 'NONE',  ( 23.24999999999999645, 36.65892442174935439, -249.5511627012433848 ) ) ;
#244592 = FACE_OUTER_BOUND ( 'NONE', #49082, .T. ) ;
#244593 = CARTESIAN_POINT ( 'NONE',  ( -20.12071067811865888, 66.67928932189394686, -191.1731074845244223 ) ) ;
#244594 = AXIS2_PLACEMENT_3D ( 'NONE', #176158, #154056, #117452 ) ;
#244595 = DIRECTION ( 'NONE',  ( 1.000000000000000000, 0.000000000000000000, 0.000000000000000000 ) ) ;
#244597 = DIRECTION ( 'NONE',  ( 0.000000000000000000, 0.000000000000000000, -1.000000000000000000 ) ) ;
#244596 = FACE_OUTER_BOUND ( 'NONE', #68802, .T. ) ;
#244598 = CARTESIAN_POINT ( 'NONE',  ( -21.65000000000000213, 7.708578643773852157, -45.85000000000000142 ) ) ;
#244600 = ORIENTED_EDGE ( 'NONE', *, *, #148405, .T. ) ;
#244599 = DIRECTION ( 'NONE',  ( 1.000000000000000000, -0.000000000000000000, 0.000000000000000000 ) ) ;
#244602 = CARTESIAN_POINT ( 'NONE',  ( 21.14250536705908345, 69.48182782313122630, -103.0231074845243597 ) ) ;
#244601 = DIRECTION ( 'NONE',  ( 1.000000000000000000, 0.000000000000000000, 0.000000000000000000 ) ) ;
#244603 = EDGE_CURVE ( 'NONE', #12754, #14945, #145329, .T. ) ;
#244604 = VECTOR ( 'NONE', #74210, 1000.000000000000000 ) ;
#244605 = CARTESIAN_POINT ( 'NONE',  ( 23.15000000000000213, -9.599999999988842347, -57.10603087734755690 ) ) ;
#244606 = EDGE_CURVE ( 'NONE', #130320, #39562, #101022, .T. ) ;
#244607 = EDGE_LOOP ( 'NONE', ( #257491, #205004, #86254, #238825 ) ) ;
#244608 = FACE_OUTER_BOUND ( 'NONE', #250078, .T. ) ;
#244609 = DIRECTION ( 'NONE',  ( 0.000000000000000000, -6.982962677686266711E-15, 1.000000000000000000 ) ) ;
#244610 = DIRECTION ( 'NONE',  ( 0.000000000000000000, 0.9994937237965558774, 0.03181660087586650476 ) ) ;
#244611 = ORIENTED_EDGE ( 'NONE', *, *, #128876, .F. ) ;
#244612 = CARTESIAN_POINT ( 'NONE',  ( -18.59999999999999787, 85.48068669529106955, -129.5819923157664562 ) ) ;
#244613 = CYLINDRICAL_SURFACE ( 'NONE', #56865, 0.1000000000000001443 ) ;
#244614 = DIRECTION ( 'NONE',  ( -0.000000000000000000, -0.1332476588733647882, -0.9910827722268041873 ) ) ;
#244616 = ORIENTED_EDGE ( 'NONE', *, *, #176764, .T. ) ;
#244615 = AXIS2_PLACEMENT_3D ( 'NONE', #169301, #248806, #70186 ) ;
#244617 = VERTEX_POINT ( 'NONE', #149214 ) ;
#244618 = ORIENTED_EDGE ( 'NONE', *, *, #28896, .T. ) ;
#244619 = LINE ( 'NONE', #183381, #198604 ) ;
#244620 = CARTESIAN_POINT ( 'NONE',  ( -18.58744394320951088, -9.566385154537224267, -174.3228480538763279 ) ) ;
#244621 = DIRECTION ( 'NONE',  ( 0.000000000000000000, 6.982962677686266711E-15, -1.000000000000000000 ) ) ;
#244622 = CARTESIAN_POINT ( 'NONE',  ( -20.94788355080263997, 10.30207779525983547, -206.4895520716781903 ) ) ;
#244623 = EDGE_LOOP ( 'NONE', ( #238031, #32267, #228384, #159094 ) ) ;
#244624 = CARTESIAN_POINT ( 'NONE',  ( -13.54036565897074773, 9.451541661396667848, -118.9538754988306266 ) ) ;
#244625 = AXIS2_PLACEMENT_3D ( 'NONE', #242642, #163137, #219228 ) ;
#244626 = DIRECTION ( 'NONE',  ( 1.000000000000000000, 0.000000000000000000, 0.000000000000000000 ) ) ;
#244627 = CIRCLE ( 'NONE', #169673, 0.1000000000000026007 ) ;
#244628 = CARTESIAN_POINT ( 'NONE',  ( -16.87331047859649757, 63.08573235307424198, -213.1276215869287967 ) ) ;
#244629 = DIRECTION ( 'NONE',  ( 0.000000000000000000, -7.429790795770647916E-15, 1.000000000000000000 ) ) ;
#244630 = ADVANCED_FACE ( 'NONE', ( #209156 ), #146599, .T. ) ;
#244631 = ORIENTED_EDGE ( 'NONE', *, *, #242721, .T. ) ;
#244632 = DIRECTION ( 'NONE',  ( 0.000000000000000000, -0.1686199900910312910, 0.9856811345164826488 ) ) ;
#244633 = CIRCLE ( 'NONE', #107263, 0.09999999999999938105 ) ;
#244635 = ORIENTED_EDGE ( 'NONE', *, *, #149185, .F. ) ;
#244634 = DIRECTION ( 'NONE',  ( 0.000000000000000000, -0.000000000000000000, 1.000000000000000000 ) ) ;
#244636 = DIRECTION ( 'NONE',  ( 1.000000000000000000, 0.000000000000000000, 0.000000000000000000 ) ) ;
#244637 = CARTESIAN_POINT ( 'NONE',  ( -21.07928932188134041, 33.98134083355181190, -243.8161431329798461 ) ) ;
#244638 = DIRECTION ( 'NONE',  ( -4.408576920032448588E-17, 0.1350103645451876944, 0.9908441862701601321 ) ) ;
#244639 = CARTESIAN_POINT ( 'NONE',  ( -20.54999999999999716, 85.00000000001179501, -79.41707660717668205 ) ) ;
#244640 = CIRCLE ( 'NONE', #132221, 0.1000000000000055844 ) ;
#244641 = DIRECTION ( 'NONE',  ( 0.000000000000000000, 0.8660254037844424824, 0.4999999999999934497 ) ) ;
#244642 = LINE ( 'NONE', #88111, #157106 ) ;
#244644 = EDGE_LOOP ( 'NONE', ( #138413, #25103, #144236, #129488 ) ) ;
#244643 = AXIS2_PLACEMENT_3D ( 'NONE', #186151, #60092, #101763 ) ;
#244645 = DIRECTION ( 'NONE',  ( 1.000000000000000000, 0.000000000000000000, 0.000000000000000000 ) ) ;
#244646 = DIRECTION ( 'NONE',  ( 0.000000000000000000, -0.000000000000000000, -1.000000000000000000 ) ) ;
#244647 = AXIS2_PLACEMENT_3D ( 'NONE', #177297, #57291, #37775 ) ;
#244648 = AXIS2_PLACEMENT_3D ( 'NONE', #250996, #114064, #249741 ) ;
#244649 = CARTESIAN_POINT ( 'NONE',  ( 20.94999999999999574, 68.48451787451661232, -224.2224406095231757 ) ) ;
#244650 = VECTOR ( 'NONE', #99749, 999.9999999999998863 ) ;
#244651 = EDGE_CURVE ( 'NONE', #30904, #114526, #238395, .T. ) ;
#244652 = CARTESIAN_POINT ( 'NONE',  ( 20.94999999999999929, 1.360870587203197646, -142.0729979270909951 ) ) ;
#244653 = DIRECTION ( 'NONE',  ( 0.000000000000000000, 0.2617529984165180013, 0.9651348961777117541 ) ) ;
#244654 = CIRCLE ( 'NONE', #240389, 0.1000000000000024342 ) ;
#244655 = ORIENTED_EDGE ( 'NONE', *, *, #221372, .T. ) ;
#244656 = ORIENTED_EDGE ( 'NONE', *, *, #75087, .F. ) ;
#244657 = DIRECTION ( 'NONE',  ( -1.000000000000000000, 0.000000000000000000, 0.000000000000000000 ) ) ;
#244658 = DIRECTION ( 'NONE',  ( 0.000000000000000000, 0.000000000000000000, -1.000000000000000000 ) ) ;
#244659 = DIRECTION ( 'NONE',  ( 0.000000000000000000, 0.000000000000000000, 1.000000000000000000 ) ) ;
#244660 = DIRECTION ( 'NONE',  ( 0.000000000000000000, 0.2128009952263603677, -0.9770955615653313941 ) ) ;
#244661 = DIRECTION ( 'NONE',  ( 0.000000000000000000, -1.000000000000000000, 0.000000000000000000 ) ) ;
#244662 = CIRCLE ( 'NONE', #65602, 0.1000000000000028644 ) ;
#244663 = DIRECTION ( 'NONE',  ( -1.000000000000000000, 0.000000000000000000, 0.000000000000000000 ) ) ;
#244664 = CARTESIAN_POINT ( 'NONE',  ( -21.04386569057698964, 17.15049515251747891, -224.5321864300226480 ) ) ;
#244665 = VECTOR ( 'NONE', #38197, 1000.000000000000000 ) ;
#244666 = ORIENTED_EDGE ( 'NONE', *, *, #64412, .T. ) ;
#244667 = DIRECTION ( 'NONE',  ( -1.073024830501117725E-15, 0.000000000000000000, 1.000000000000000000 ) ) ;
#244668 = VERTEX_POINT ( 'NONE', #187061 ) ;
#244669 = CARTESIAN_POINT ( 'NONE',  ( -21.05000000000000071, 76.02110330807039418, -75.82762381378833538 ) ) ;
#244670 = DIRECTION ( 'NONE',  ( 0.000000000000000000, 6.982962677686266711E-15, -1.000000000000000000 ) ) ;
#244671 = FACE_OUTER_BOUND ( 'NONE', #21749, .T. ) ;
#244672 = CARTESIAN_POINT ( 'NONE',  ( -23.25000000000000000, 85.60000000001252829, -179.9170766071767389 ) ) ;
#244673 = CARTESIAN_POINT ( 'NONE',  ( -16.77902162784673834, 9.946419257218996890, -46.16199124406934828 ) ) ;
#244674 = CARTESIAN_POINT ( 'NONE',  ( -18.40000000000000213, 64.52683809664901560, -45.34905355133235361 ) ) ;
#244675 = LINE ( 'NONE', #7359, #95478 ) ;
#244676 = CARTESIAN_POINT ( 'NONE',  ( -16.91049119928363709, 66.05000000001183480, -82.14138709133354155 ) ) ;
#244677 = CARTESIAN_POINT ( 'NONE',  ( 23.14999999999999503, 6.450000000011156587, -45.85000000000000142 ) ) ;
#244678 = CARTESIAN_POINT ( 'NONE',  ( -23.15000000000000213, 6.277629359189123015, -229.8243190661787878 ) ) ;
#244680 = EDGE_CURVE ( 'NONE', #34439, #135650, #90491, .T. ) ;
#244679 = DIRECTION ( 'NONE',  ( 0.000000000000000000, 6.938893903907030216E-14, 1.000000000000000000 ) ) ;
#244681 = DIRECTION ( 'NONE',  ( 1.000000000000000000, 0.000000000000000000, 0.000000000000000000 ) ) ;
#244682 = AXIS2_PLACEMENT_3D ( 'NONE', #190148, #154888, #132746 ) ;
#244683 = AXIS2_PLACEMENT_3D ( 'NONE', #23371, #221514, #83280 ) ;
#244684 = FACE_OUTER_BOUND ( 'NONE', #99223, .T. ) ;
#244685 = CARTESIAN_POINT ( 'NONE',  ( -20.64999999999999858, 6.857177884343597540, -212.0437362999421680 ) ) ;
#244686 = VERTEX_POINT ( 'NONE', #31844 ) ;
#244687 = CARTESIAN_POINT ( 'NONE',  ( 21.14999999999999503, -11.74999999999999112, -2.900000000000003464 ) ) ;
#244689 = EDGE_CURVE ( 'NONE', #45573, #228499, #64276, .T. ) ;
#244688 = DIRECTION ( 'NONE',  ( -1.000000000000000000, -0.000000000000000000, -0.000000000000000000 ) ) ;
#244690 = ORIENTED_EDGE ( 'NONE', *, *, #167428, .F. ) ;
#244692 = EDGE_CURVE ( 'NONE', #139739, #5736, #59971, .T. ) ;
#244691 = CARTESIAN_POINT ( 'NONE',  ( -21.29999999999995808, 76.00000000001210765, -132.4731074845242915 ) ) ;
#244693 = CARTESIAN_POINT ( 'NONE',  ( 21.11345278033298811, 11.28464776068242692, -211.0754094929459654 ) ) ;
#244694 = CARTESIAN_POINT ( 'NONE',  ( -23.25000000000000000, 77.85161776048073534, -91.41991776492061206 ) ) ;
#244695 = VERTEX_POINT ( 'NONE', #127063 ) ;
#244696 = VECTOR ( 'NONE', #233257, 1000.000000000000000 ) ;
#244697 = DIRECTION ( 'NONE',  ( 0.000000000000000000, 0.9856811345164827598, 0.1686199900910313187 ) ) ;
#244698 = CARTESIAN_POINT ( 'NONE',  ( 23.14999999999999858, 72.00000000001213607, -136.5231074845243597 ) ) ;
#244699 = VECTOR ( 'NONE', #106768, 1000.000000000000000 ) ;
#244700 = ADVANCED_FACE ( 'NONE', ( #226126 ), #87906, .F. ) ;
#244701 = ORIENTED_EDGE ( 'NONE', *, *, #118936, .T. ) ;
#244702 =( BOUNDED_CURVE ( )  B_SPLINE_CURVE ( 3, ( #221084, #42455, #180698, #82834 ),
 .UNSPECIFIED., .F., .T. ) 
 B_SPLINE_CURVE_WITH_KNOTS ( ( 4, 4 ),
 ( 0.000000000000000000, 1.570796326794908992 ),
 .UNSPECIFIED. ) 
 CURVE ( )  GEOMETRIC_REPRESENTATION_ITEM ( )  RATIONAL_B_SPLINE_CURVE ( ( 1.000000000000000000, 0.8047378541243619399, 0.8047378541243619399, 1.000000000000000000 ) ) 
 REPRESENTATION_ITEM ( '' )  );
#244703 = AXIS2_PLACEMENT_3D ( 'NONE', #233436, #255490, #133044 ) ;
#244704 = CARTESIAN_POINT ( 'NONE',  ( 20.94999999999999929, 1.360870587203197646, -41.57299792709095954 ) ) ;
#244705 = ORIENTED_EDGE ( 'NONE', *, *, #255489, .F. ) ;
#244707 = ADVANCED_FACE ( 'NONE', ( #107492 ), #130911, .T. ) ;
#244706 = DIRECTION ( 'NONE',  ( -1.000000000000000000, -0.000000000000000000, 0.000000000000000000 ) ) ;
#244708 = CARTESIAN_POINT ( 'NONE',  ( 22.40000000000010161, 1.020945264940608290E-11, -21.74956710754107547 ) ) ;
#244709 = LINE ( 'NONE', #9966, #194898 ) ;
#244710 = FACE_OUTER_BOUND ( 'NONE', #217536, .T. ) ;
#244711 = DIRECTION ( 'NONE',  ( 1.000000000000000000, -0.000000000000000000, -0.000000000000000000 ) ) ;
#244712 = CARTESIAN_POINT ( 'NONE',  ( -16.80070461187834496, 66.05000000001230376, -157.3761436553679118 ) ) ;
#244713 = FACE_OUTER_BOUND ( 'NONE', #30994, .T. ) ;
#244714 = DIRECTION ( 'NONE',  ( 1.000000000000000000, -0.000000000000000000, -0.000000000000000000 ) ) ;
#244715 = CARTESIAN_POINT ( 'NONE',  ( 23.14999999999999858, 16.98881331171930498, -224.4946931418895417 ) ) ;
#244717 = ORIENTED_EDGE ( 'NONE', *, *, #125358, .F. ) ;
#244716 = CARTESIAN_POINT ( 'NONE',  ( -22.47071067811865319, -1.546016791165058635, -193.4356622592196970 ) ) ;
#244718 = ORIENTED_EDGE ( 'NONE', *, *, #124772, .F. ) ;
#244720 = DIRECTION ( 'NONE',  ( 0.000000000000000000, 0.2128009952263603954, -0.9770955615653315052 ) ) ;
#244719 = CARTESIAN_POINT ( 'NONE',  ( -21.05000000000000071, 87.65000000001144542, -38.92310748452424463 ) ) ;
#244722 = EDGE_LOOP ( 'NONE', ( #63559, #57869, #125493, #70315 ) ) ;
#244721 = CARTESIAN_POINT ( 'NONE',  ( 18.59999999999999432, -1.261786168553869603, -175.5864989635454378 ) ) ;
#244723 = AXIS2_PLACEMENT_3D ( 'NONE', #36794, #158037, #219231 ) ;
#244724 = EDGE_LOOP ( 'NONE', ( #239362, #235725, #18060, #209869, #148784 ) ) ;
#244725 = CARTESIAN_POINT ( 'NONE',  ( -21.05000000000000071, 14.05000000001115623, -39.01369507076099552 ) ) ;
#244727 = CARTESIAN_POINT ( 'NONE',  ( 20.74897398619109268, 10.59569302167756888, -175.1793114562568974 ) ) ;
#244726 = CIRCLE ( 'NONE', #148899, 11.80000000000001137 ) ;
#244728 = CYLINDRICAL_SURFACE ( 'NONE', #159143, 0.09999999999999939493 ) ;
#244729 = CARTESIAN_POINT ( 'NONE',  ( -23.25000000000000000, -8.999999999988844479, -191.1060308773475356 ) ) ;
#244730 = DIRECTION ( 'NONE',  ( -1.000000000000000000, 0.000000000000000000, 0.000000000000000000 ) ) ;
#244731 = FACE_OUTER_BOUND ( 'NONE', #73341, .T. ) ;
#244732 = EDGE_CURVE ( 'NONE', #149809, #65489, #255767, .T. ) ;
#244734 = AXIS2_PLACEMENT_3D ( 'NONE', #245047, #108109, #65118 ) ;
#244733 = DIRECTION ( 'NONE',  ( 0.000000000000000000, 0.9126074666063660468, 0.4088369013363524762 ) ) ;
#244735 = ORIENTED_EDGE ( 'NONE', *, *, #17752, .T. ) ;
#244736 = ORIENTED_EDGE ( 'NONE', *, *, #180357, .F. ) ;
#244737 = CARTESIAN_POINT ( 'NONE',  ( -23.25000000000000000, 11.65000000001115588, -88.25000000000005684 ) ) ;
#244738 = AXIS2_PLACEMENT_3D ( 'NONE', #128358, #27999, #167501 ) ;
#244739 = AXIS2_PLACEMENT_3D ( 'NONE', #166354, #86758, #71089 ) ;
#244740 = ORIENTED_EDGE ( 'NONE', *, *, #63063, .T. ) ;
#244741 = CARTESIAN_POINT ( 'NONE',  ( -21.59142135623730852, 68.15000000001205649, -124.1731074845243512 ) ) ;
#244742 = VERTEX_POINT ( 'NONE', #246996 ) ;
#244744 = CARTESIAN_POINT ( 'NONE',  ( -16.80469485234342031, 9.942151663152193564, -154.8099668439312211 ) ) ;
#244743 = AXIS2_PLACEMENT_3D ( 'NONE', #66085, #206884, #89487 ) ;
#244745 = EDGE_CURVE ( 'NONE', #41329, #251252, #110058, .T. ) ;
#244746 = AXIS2_PLACEMENT_3D ( 'NONE', #49883, #87711, #146393 ) ;
#244747 = FACE_OUTER_BOUND ( 'NONE', #103631, .T. ) ;
#244748 = AXIS2_PLACEMENT_3D ( 'NONE', #239172, #197465, #215738 ) ;
#244750 = B_SPLINE_CURVE_WITH_KNOTS ( 'NONE', 3,
 ( #81818, #21890, #204357, #121016, #64850, #140531 ),
 .UNSPECIFIED., .F., .F.,
 ( 4, 2, 4 ),
 ( 0.000000000000000000, 0.0001895189928937424410, 0.0003790379857874848820 ),
 .UNSPECIFIED. ) ;
#244749 = DIRECTION ( 'NONE',  ( -1.000000000000000000, 2.849773892568378313E-16, -7.728835255496647986E-17 ) ) ;
#244751 = FACE_OUTER_BOUND ( 'NONE', #51162, .T. ) ;
#244752 = ORIENTED_EDGE ( 'NONE', *, *, #217294, .T. ) ;
#244754 = ADVANCED_FACE ( 'NONE', ( #51336 ), #248293, .F. ) ;
#244753 =( BOUNDED_CURVE ( )  B_SPLINE_CURVE ( 3, ( #192439, #149479, #67353, #229004 ),
 .UNSPECIFIED., .F., .F. ) 
 B_SPLINE_CURVE_WITH_KNOTS ( ( 4, 4 ),
 ( 0.000000000000000000, 1.570796326794896558 ),
 .UNSPECIFIED. ) 
 CURVE ( )  GEOMETRIC_REPRESENTATION_ITEM ( )  RATIONAL_B_SPLINE_CURVE ( ( 1.000000000000000000, 0.8047378541243649375, 0.8047378541243649375, 1.000000000000000000 ) ) 
 REPRESENTATION_ITEM ( '' )  );
#244755 = ORIENTED_EDGE ( 'NONE', *, *, #236469, .T. ) ;
#244756 = DIRECTION ( 'NONE',  ( 1.000000000000000000, -0.000000000000000000, -0.000000000000000000 ) ) ;
#244757 = CARTESIAN_POINT ( 'NONE',  ( -21.07094088545368038, 30.85066122990915716, -252.0448291528320510 ) ) ;
#244758 = CARTESIAN_POINT ( 'NONE',  ( -21.55000000000000426, 68.25000000001151079, -48.37310748452437537 ) ) ;
#244759 = DIRECTION ( 'NONE',  ( -1.000000000000000000, -0.000000000000000000, -0.000000000000000000 ) ) ;
#244760 = EDGE_CURVE ( 'NONE', #128659, #209214, #76732, .T. ) ;
#244761 = VERTEX_POINT ( 'NONE', #13545 ) ;
#244762 = CARTESIAN_POINT ( 'NONE',  ( -21.05000000000000071, 64.25000000001189449, -96.23924182154622997 ) ) ;
#244763 = CIRCLE ( 'NONE', #132342, 6.329289321881370611 ) ;
#244764 = EDGE_LOOP ( 'NONE', ( #185512, #182299, #54232 ) ) ;
#244767 = ORIENTED_EDGE ( 'NONE', *, *, #64260, .T. ) ;
#244766 = DIRECTION ( 'NONE',  ( 0.000000000000000000, -0.4099100576505548821, -0.9121259477928028714 ) ) ;
#244765 = LINE ( 'NONE', #169133, #240878 ) ;
#244768 = LINE ( 'NONE', #68718, #214333 ) ;
#244769 = VECTOR ( 'NONE', #73605, 1000.000000000000000 ) ;
#244770 = ORIENTED_EDGE ( 'NONE', *, *, #148106, .T. ) ;
#244771 = CARTESIAN_POINT ( 'NONE',  ( -23.25000000000000355, 5.650000000011139001, -188.3499999999999659 ) ) ;
#244772 = ORIENTED_EDGE ( 'NONE', *, *, #199864, .T. ) ;
#244773 = DIRECTION ( 'NONE',  ( 0.000000000000000000, 0.000000000000000000, -1.000000000000000000 ) ) ;
#244774 = AXIS2_PLACEMENT_3D ( 'NONE', #50713, #29924, #10353 ) ;
#244775 = EDGE_CURVE ( 'NONE', #150070, #244889, #91787, .T. ) ;
#244776 = VECTOR ( 'NONE', #174289, 1000.000000000000000 ) ;
#244777 = CARTESIAN_POINT ( 'NONE',  ( 21.05000000000000071, 1.316055977212909456, -230.7323992127457473 ) ) ;
#244778 = DIRECTION ( 'NONE',  ( -0.000000000000000000, -0.9876197685951290106, 0.1568667991644625281 ) ) ;
#244779 = ADVANCED_FACE ( 'NONE', ( #67088 ), #68379, .T. ) ;
#244780 = ADVANCED_FACE ( 'NONE', ( #206596 ), #130718, .T. ) ;
#244781 = CARTESIAN_POINT ( 'NONE',  ( 18.59999999999999787, 77.83585931145546510, -91.51866831572576189 ) ) ;
#244782 = VERTEX_POINT ( 'NONE', #27997 ) ;
#244783 = DIRECTION ( 'NONE',  ( 1.000000000000000000, 0.000000000000000000, 0.000000000000000000 ) ) ;
#244784 = FILL_AREA_STYLE ('',( #107850 ) ) ;
#244785 = CARTESIAN_POINT ( 'NONE',  ( -18.31331870001081086, -9.536294719169568168, -140.8685786909853732 ) ) ;
#244786 = CIRCLE ( 'NONE', #165134, 0.09999999999999939493 ) ;
#244787 = ORIENTED_EDGE ( 'NONE', *, *, #158432, .F. ) ;
#244788 = DIRECTION ( 'NONE',  ( -1.000000000000000000, -2.683427030341247466E-17, 8.429776912874270765E-16 ) ) ;
#244790 = ORIENTED_EDGE ( 'NONE', *, *, #91905, .T. ) ;
#244789 = AXIS2_PLACEMENT_3D ( 'NONE', #184890, #88327, #24561 ) ;
#244792 = AXIS2_PLACEMENT_3D ( 'NONE', #219932, #140382, #120867 ) ;
#244791 = CARTESIAN_POINT ( 'NONE',  ( -22.94999999999999929, 5.586869315528661062, 16.41686199900910736 ) ) ;
#244793 = EDGE_CURVE ( 'NONE', #57931, #18553, #205722, .T. ) ;
#244794 = DIRECTION ( 'NONE',  ( 0.000000000000000000, 0.000000000000000000, -1.000000000000000000 ) ) ;
#244795 = FACE_OUTER_BOUND ( 'NONE', #247530, .T. ) ;
#244797 = ORIENTED_EDGE ( 'NONE', *, *, #135548, .T. ) ;
#244796 = CARTESIAN_POINT ( 'NONE',  ( -16.97683809663752186, 44.82209472663103611, -234.9913374327310578 ) ) ;
#244798 = EDGE_CURVE ( 'NONE', #125106, #224742, #30983, .T. ) ;
#244799 = DIRECTION ( 'NONE',  ( 1.000000000000000000, -2.952720810173289112E-16, -2.061873921506763405E-30 ) ) ;
#244800 = EDGE_CURVE ( 'NONE', #252694, #14463, #254665, .T. ) ;
#244801 = CARTESIAN_POINT ( 'NONE',  ( -12.68215100488890457, 62.84948463577724453, -216.1128043527995430 ) ) ;
#244802 = AXIS2_PLACEMENT_3D ( 'NONE', #248775, #243624, #106659 ) ;
#244803 = DIRECTION ( 'NONE',  ( -0.000000000000000000, 0.1335171055202901413, 0.9910465087640860649 ) ) ;
#244804 = CIRCLE ( 'NONE', #236435, 0.1000000000000024342 ) ;
#244805 = EDGE_LOOP ( 'NONE', ( #179160, #34706, #208973, #146325 ) ) ;
#244806 = LINE ( 'NONE', #145701, #19254 ) ;
#244807 = CIRCLE ( 'NONE', #257236, 0.1000000000000054040 ) ;
#244808 = VERTEX_POINT ( 'NONE', #57776 ) ;
#244809 = DIRECTION ( 'NONE',  ( 0.000000000000000000, 0.000000000000000000, -1.000000000000000000 ) ) ;
#244810 = ORIENTED_EDGE ( 'NONE', *, *, #118486, .F. ) ;
#244811 = CARTESIAN_POINT ( 'NONE',  ( -16.79139129368505579, 44.15602412204730598, -235.2952688487417277 ) ) ;
#244813 = EDGE_LOOP ( 'NONE', ( #135097, #116208, #193950, #110474, #174011 ) ) ;
#244812 = DIRECTION ( 'NONE',  ( 0.000000000000000000, -0.9274965247785323941, -0.3738317757009769760 ) ) ;
#244814 = ADVANCED_FACE ( 'NONE', ( #36980 ), #168380, .F. ) ;
#244815 = ADVANCED_FACE ( 'NONE', ( #78624 ), #53939, .T. ) ;
#244818 = VERTEX_POINT ( 'NONE', #155648 ) ;
#244817 = ORIENTED_EDGE ( 'NONE', *, *, #85404, .T. ) ;
#244816 = DIRECTION ( 'NONE',  ( 0.000000000000000000, 0.000000000000000000, -1.000000000000000000 ) ) ;
#244819 = CIRCLE ( 'NONE', #174156, 0.09999999999999939493 ) ;
#244820 = DIRECTION ( 'NONE',  ( 1.000000000000000000, 0.000000000000000000, 0.000000000000000000 ) ) ;
#244821 = VECTOR ( 'NONE', #257373, 1000.000000000000000 ) ;
#244823 = EDGE_CURVE ( 'NONE', #221150, #144444, #257226, .T. ) ;
#244822 = DIRECTION ( 'NONE',  ( 0.000000000000000000, 1.000000000000000000, -0.000000000000000000 ) ) ;
#244824 = CIRCLE ( 'NONE', #132424, 0.09999999999999939493 ) ;
#244826 = DIRECTION ( 'NONE',  ( 0.000000000000000000, 0.000000000000000000, 1.000000000000000000 ) ) ;
#244825 = DIRECTION ( 'NONE',  ( 1.000000000000000000, 0.000000000000000000, 0.000000000000000000 ) ) ;
#244827 = DIRECTION ( 'NONE',  ( -0.000000000000000000, -0.1332476588733656764, 0.9910827722268041873 ) ) ;
#244828 = DIRECTION ( 'NONE',  ( -0.000000000000000000, -0.000000000000000000, -1.000000000000000000 ) ) ;
#244829 = CARTESIAN_POINT ( 'NONE',  ( -16.87036670365549540, 66.01058118070992009, -57.00266760182645953 ) ) ;
#244830 = AXIS2_PLACEMENT_3D ( 'NONE', #175606, #217259, #159897 ) ;
#244831 = CARTESIAN_POINT ( 'NONE',  ( -23.15000000000000213, -11.64999999998884483, -130.9000000000000341 ) ) ;
#244832 = CARTESIAN_POINT ( 'NONE',  ( -22.50875500270928953, 76.10085791378683950, -148.2726746119222128 ) ) ;
#244833 = ORIENTED_EDGE ( 'NONE', *, *, #54504, .F. ) ;
#244834 = ORIENTED_EDGE ( 'NONE', *, *, #195307, .T. ) ;
#244835 = CARTESIAN_POINT ( 'NONE',  ( -23.25000000000000000, 46.00954831033281778, -240.7052126169319877 ) ) ;
#244837 = VERTEX_POINT ( 'NONE', #214308 ) ;
#244836 = CARTESIAN_POINT ( 'NONE',  ( 20.04142135623730070, 8.980461154494401299, -187.0187154576991304 ) ) ;
#244838 = VERTEX_POINT ( 'NONE', #14846 ) ;
#244839 = CARTESIAN_POINT ( 'NONE',  ( -20.54999999999999716, 6.757359537351773859, -220.2789794402637824 ) ) ;
#244840 = ORIENTED_EDGE ( 'NONE', *, *, #127696, .F. ) ;
#244841 = CARTESIAN_POINT ( 'NONE',  ( -21.05000000000000071, 69.55922910635067069, -136.5055102975167927 ) ) ;
#244842 = CIRCLE ( 'NONE', #95011, 0.09999999999999971412 ) ;
#244843 = ADVANCED_FACE ( 'NONE', ( #133482 ), #236427, .T. ) ;
#244844 = VERTEX_POINT ( 'NONE', #38242 ) ;
#244845 = DIRECTION ( 'NONE',  ( 0.000000000000000000, -0.9770955615653316162, -0.2128009952263604232 ) ) ;
#244847 = EDGE_CURVE ( 'NONE', #158507, #57412, #209850, .T. ) ;
#244846 = CARTESIAN_POINT ( 'NONE',  ( 21.05000000000000071, 87.48912529308749697, -39.12310748452424747 ) ) ;
#244848 = AXIS2_PLACEMENT_3D ( 'NONE', #209786, #10316, #91114 ) ;
#244850 = EDGE_LOOP ( 'NONE', ( #8589, #141778, #82253, #38604 ) ) ;
#244849 = ORIENTED_EDGE ( 'NONE', *, *, #161018, .F. ) ;
#244851 = ORIENTED_EDGE ( 'NONE', *, *, #197254, .F. ) ;
#244852 = CARTESIAN_POINT ( 'NONE',  ( 21.09696443733127325, 10.72400988392963228, -45.73477752704822308 ) ) ;
#244853 = EDGE_LOOP ( 'NONE', ( #108117, #112166, #251082 ) ) ;
#244854 = VERTEX_POINT ( 'NONE', #56488 ) ;
#244855 = ADVANCED_FACE ( 'NONE', ( #59041 ), #243151, .T. ) ;
#244856 = DIRECTION ( 'NONE',  ( -1.836970198721029441E-16, 0.4721928772777346239, 0.8814952561688430555 ) ) ;
#244857 = CARTESIAN_POINT ( 'NONE',  ( -23.25000000000000000, 77.16412189325330928, -128.6082593989527254 ) ) ;
#244860 = ADVANCED_FACE ( 'NONE', ( #138578, #137315 ), #218128, .T. ) ;
#244859 = ORIENTED_EDGE ( 'NONE', *, *, #190918, .T. ) ;
#244858 = CARTESIAN_POINT ( 'NONE',  ( 18.39999999999999858, -9.399999999988843058, -155.7499999999999716 ) ) ;
#244861 = DIRECTION ( 'NONE',  ( 0.000000000000000000, 6.982962677686267499E-15, -1.000000000000000000 ) ) ;
#244862 = DIRECTION ( 'NONE',  ( 0.000000000000000000, -0.9908441862701596881, -0.1350103645451904977 ) ) ;
#244864 = ORIENTED_EDGE ( 'NONE', *, *, #78544, .T. ) ;
#244863 = DIRECTION ( 'NONE',  ( 0.000000000000000000, 0.2617529984165031243, 0.9651348961777157509 ) ) ;
#244865 = CARTESIAN_POINT ( 'NONE',  ( -21.55000000000000426, 7.750000000011155521, -112.8500000000000369 ) ) ;
#244866 = EDGE_LOOP ( 'NONE', ( #159000, #24753, #255065, #187079 ) ) ;
#244867 = EDGE_CURVE ( 'NONE', #97945, #38825, #201640, .T. ) ;
#244868 = CARTESIAN_POINT ( 'NONE',  ( -16.81744102076748959, 9.950000000011138823, -188.3499999999999659 ) ) ;
#244869 = VERTEX_POINT ( 'NONE', #198579 ) ;
#244870 = DIRECTION ( 'NONE',  ( -1.000000000000000000, 0.000000000000000000, -0.000000000000000000 ) ) ;
#244871 = DIRECTION ( 'NONE',  ( 0.000000000000000000, 0.8700118002898321601, -0.4930308989875230030 ) ) ;
#244872 = ORIENTED_EDGE ( 'NONE', *, *, #85555, .F. ) ;
#244873 = AXIS2_PLACEMENT_3D ( 'NONE', #156833, #117670, #56396 ) ;
#244874 = CIRCLE ( 'NONE', #132454, 0.6000000000000139666 ) ;
#244877 = CARTESIAN_POINT ( 'NONE',  ( -33.72168855820452649, 11.47316190337362585, -143.2500000000000284 ) ) ;
#244876 = AXIS2_PLACEMENT_3D ( 'NONE', #235525, #255030, #238091 ) ;
#244875 = FACE_OUTER_BOUND ( 'NONE', #258001, .T. ) ;
#244878 = CIRCLE ( 'NONE', #115713, 0.09999999999999939493 ) ;
#244879 = EDGE_CURVE ( 'NONE', #237173, #28990, #222461, .T. ) ;
#244880 = CARTESIAN_POINT ( 'NONE',  ( -18.50000000000000000, 64.35000000001195986, -102.9231074845243938 ) ) ;
#244881 = CARTESIAN_POINT ( 'NONE',  ( -12.25000000000000178, 12.65101141449786581, -215.1505311063239674 ) ) ;
#244882 = EDGE_CURVE ( 'NONE', #256969, #160776, #235155, .T. ) ;
#244883 = EDGE_LOOP ( 'NONE', ( #54039, #203938, #48187, #241310, #88005 ) ) ;
#244884 = ORIENTED_EDGE ( 'NONE', *, *, #170637, .F. ) ;
#244885 = CARTESIAN_POINT ( 'NONE',  ( -18.59999999999999787, -1.835859311443637010, -45.00443916879852679 ) ) ;
#244886 = CARTESIAN_POINT ( 'NONE',  ( -18.59999999999999787, 85.40000000001209912, -129.6410656363516125 ) ) ;
#244887 = ORIENTED_EDGE ( 'NONE', *, *, #48207, .F. ) ;
#244888 = CYLINDRICAL_SURFACE ( 'NONE', #247273, 1.749999999999999778 ) ;
#244889 = VERTEX_POINT ( 'NONE', #176480 ) ;
#244890 = ADVANCED_FACE ( 'NONE', ( #77342 ), #255941, .F. ) ;
#244891 = CARTESIAN_POINT ( 'NONE',  ( -16.97683809663752186, 66.15000000001225544, -149.9254715027207396 ) ) ;
#244892 = ORIENTED_EDGE ( 'NONE', *, *, #178945, .F. ) ;
#244893 = FACE_OUTER_BOUND ( 'NONE', #201519, .T. ) ;
#244894 = DIRECTION ( 'NONE',  ( 1.000000000000000000, 0.000000000000000000, 0.000000000000000000 ) ) ;
#244895 = VECTOR ( 'NONE', #237906, 1000.000000000000000 ) ;
#244896 = VERTEX_POINT ( 'NONE', #116494 ) ;
#244897 = CIRCLE ( 'NONE', #149063, 0.1000000000000076522 ) ;
#244898 = CARTESIAN_POINT ( 'NONE',  ( 18.39999999999999858, -9.499999999988844479, -207.9221498493303670 ) ) ;
#244899 = ADVANCED_FACE ( 'NONE', ( #96881 ), #164048, .T. ) ;
#244900 = ADVANCED_FACE ( 'NONE', ( #5498 ), #224559, .T. ) ;
#244901 = ORIENTED_EDGE ( 'NONE', *, *, #44978, .F. ) ;
#244902 = AXIS2_PLACEMENT_3D ( 'NONE', #130358, #173404, #131654 ) ;
#244903 = ORIENTED_EDGE ( 'NONE', *, *, #206162, .F. ) ;
#244904 = ORIENTED_EDGE ( 'NONE', *, *, #172455, .T. ) ;
#244905 = EDGE_CURVE ( 'NONE', #65749, #39261, #51575, .T. ) ;
#244906 = DIRECTION ( 'NONE',  ( 0.000000000000000000, 0.000000000000000000, -1.000000000000000000 ) ) ;
#244907 = DIRECTION ( 'NONE',  ( 0.000000000000000000, 2.664535259100315349E-15, 1.000000000000000000 ) ) ;
#244908 = DIRECTION ( 'NONE',  ( 0.000000000000000000, 0.9126074666063613838, 0.4088369013363628013 ) ) ;
#244909 = CARTESIAN_POINT ( 'NONE',  ( -21.44999999999999929, 29.33122518167236237, -237.2878098217501588 ) ) ;
#244910 = DIRECTION ( 'NONE',  ( 1.000000000000000000, 2.885090398161910739E-16, 6.283419270304611573E-17 ) ) ;
#244912 = DIRECTION ( 'NONE',  ( 0.000000000000000000, -6.982962677686266711E-15, 1.000000000000000000 ) ) ;
#244911 = FACE_OUTER_BOUND ( 'NONE', #108632, .T. ) ;
#244913 = EDGE_CURVE ( 'NONE', #154121, #234753, #162050, .T. ) ;
#244915 = ORIENTED_EDGE ( 'NONE', *, *, #73169, .T. ) ;
#244914 = LINE ( 'NONE', #8879, #185500 ) ;
#244916 = CARTESIAN_POINT ( 'NONE',  ( -6.000000000000003553, -11.34999999999999964, 10.00000000000000178 ) ) ;
#244917 = ORIENTED_EDGE ( 'NONE', *, *, #217732, .T. ) ;
#244918 = CARTESIAN_POINT ( 'NONE',  ( -22.39999999999999858, 7.790779598384560245, -133.9000000000000057 ) ) ;
#244919 = EDGE_CURVE ( 'NONE', #206030, #116136, #230699, .T. ) ;
#244920 = ORIENTED_EDGE ( 'NONE', *, *, #101229, .F. ) ;
#244921 = ORIENTED_EDGE ( 'NONE', *, *, #212802, .F. ) ;
#244922 = CARTESIAN_POINT ( 'NONE',  ( -23.15000000000000213, 1.115600667400684642E-11, -134.0000000000000284 ) ) ;
#244923 = CARTESIAN_POINT ( 'NONE',  ( 22.47071067811865319, 75.90090754531013317, -211.2431822290224090 ) ) ;
#244924 = CARTESIAN_POINT ( 'NONE',  ( -16.96982749440705973, 66.05000000001153637, -49.14788589333611668 ) ) ;
#244925 = DIRECTION ( 'NONE',  ( 1.000000000000000000, -3.265361837132813093E-16, -2.280189983783949500E-30 ) ) ;
#244926 = AXIS2_PLACEMENT_3D ( 'NONE', #238173, #77815, #236901 ) ;
#244927 = VECTOR ( 'NONE', #32404, 1000.000000000000227 ) ;
#244928 = DIRECTION ( 'NONE',  ( 0.000000000000000000, -0.000000000000000000, 1.000000000000000000 ) ) ;
#244929 = ORIENTED_EDGE ( 'NONE', *, *, #49825, .T. ) ;
#244930 = ORIENTED_EDGE ( 'NONE', *, *, #190558, .F. ) ;
#244932 = EDGE_CURVE ( 'NONE', #87663, #183134, #5803, .T. ) ;
#244931 = ORIENTED_EDGE ( 'NONE', *, *, #103614, .T. ) ;
#244933 = CARTESIAN_POINT ( 'NONE',  ( -21.14999999999994174, 74.94272479589878344, -8.023107484524793165 ) ) ;
#244935 = CYLINDRICAL_SURFACE ( 'NONE', #186275, 0.09999999999999945044 ) ;
#244934 = CIRCLE ( 'NONE', #45023, 0.1000000000000013933 ) ;
#244936 = LINE ( 'NONE', #247511, #50322 ) ;
#244937 = DIRECTION ( 'NONE',  ( 0.000000000000000000, -0.000000000000000000, 1.000000000000000000 ) ) ;
#244938 = DIRECTION ( 'NONE',  ( 1.000000000000000000, -2.952720810173289112E-16, -2.061873921506763405E-30 ) ) ;
#244939 = ORIENTED_EDGE ( 'NONE', *, *, #57315, .T. ) ;
#244940 = CARTESIAN_POINT ( 'NONE',  ( 23.24999999999999645, 45.69057616835975466, -239.3688303688244616 ) ) ;
#244941 = LINE ( 'NONE', #224085, #179086 ) ;
#244942 = DIRECTION ( 'NONE',  ( 1.000000000000000000, -0.000000000000000000, -0.000000000000000000 ) ) ;
#244944 = EDGE_CURVE ( 'NONE', #114560, #178866, #101651, .T. ) ;
#244943 = CARTESIAN_POINT ( 'NONE',  ( 23.14999999999999858, 5.000000000011153745, -188.5947339810868755 ) ) ;
#244945 = CARTESIAN_POINT ( 'NONE',  ( -23.15000000000000213, 71.85000000001178933, -81.87310748452433984 ) ) ;
#244946 = AXIS2_PLACEMENT_3D ( 'NONE', #190607, #214011, #254384 ) ;
#244947 = CARTESIAN_POINT ( 'NONE',  ( -18.59999999999999787, 1.835341550224411922, -11.55515129256298046 ) ) ;
#244948 = CIRCLE ( 'NONE', #170162, 0.09999999999999939493 ) ;
#244949 = AXIS2_PLACEMENT_3D ( 'NONE', #130892, #33131, #192177 ) ;
#244950 = ORIENTED_EDGE ( 'NONE', *, *, #218672, .T. ) ;
#244952 = ADVANCED_FACE ( 'NONE', ( #40832 ), #251524, .T. ) ;
#244951 = CARTESIAN_POINT ( 'NONE',  ( -21.53699400380209283, 69.21228820681638183, -136.5231074845243597 ) ) ;
#244953 = ORIENTED_EDGE ( 'NONE', *, *, #135818, .F. ) ;
#244954 = CARTESIAN_POINT ( 'NONE',  ( 18.59999999999999076, 11.75000000001115907, -75.10000000000003695 ) ) ;
#244955 = LINE ( 'NONE', #243678, #110475 ) ;
#244956 = DIRECTION ( 'NONE',  ( 1.000000000000000000, -9.458662978381124901E-16, 5.066746821047763994E-16 ) ) ;
#244957 = ORIENTED_EDGE ( 'NONE', *, *, #254569, .F. ) ;
#244958 = DIRECTION ( 'NONE',  ( 0.000000000000000000, -0.4088369013363783999, 0.9126074666063545004 ) ) ;
#244959 = DIRECTION ( 'NONE',  ( 0.000000000000000000, -1.000000000000000000, 0.000000000000000000 ) ) ;
#244960 = DIRECTION ( 'NONE',  ( -1.000000000000000000, -7.304098846218134667E-16, 0.000000000000000000 ) ) ;
#244961 = AXIS2_PLACEMENT_3D ( 'NONE', #196920, #198205, #14466 ) ;
#244962 = EDGE_CURVE ( 'NONE', #14013, #81650, #221971, .T. ) ;
#244963 = CARTESIAN_POINT ( 'NONE',  ( -20.54999999999999716, 7.250000000011155521, -179.7499999999999716 ) ) ;
#244964 = VECTOR ( 'NONE', #193225, 1000.000000000000000 ) ;
#244965 = CARTESIAN_POINT ( 'NONE',  ( -18.40000000000000213, 70.35000000001159037, -56.87310748452436115 ) ) ;
#244966 = CIRCLE ( 'NONE', #99197, 0.09999999999999939493 ) ;
#244967 = VECTOR ( 'NONE', #190926, 1000.000000000000000 ) ;
#244969 = ORIENTED_EDGE ( 'NONE', *, *, #128903, .F. ) ;
#244968 = CIRCLE ( 'NONE', #178355, 0.1999999999999996503 ) ;
#244970 = ORIENTED_EDGE ( 'NONE', *, *, #68451, .T. ) ;
#244971 = DIRECTION ( 'NONE',  ( -1.000000000000000000, 0.000000000000000000, 0.000000000000000000 ) ) ;
#244974 = VERTEX_POINT ( 'NONE', #25113 ) ;
#244973 = FACE_OUTER_BOUND ( 'NONE', #19532, .T. ) ;
#244972 = CIRCLE ( 'NONE', #103479, 0.1000000000000015737 ) ;
#244975 = DIRECTION ( 'NONE',  ( 0.000000000000000000, 0.8660254037844281605, -0.5000000000000185407 ) ) ;
#244976 = FACE_OUTER_BOUND ( 'NONE', #99408, .T. ) ;
#244977 = VECTOR ( 'NONE', #42469, 1000.000000000000000 ) ;
#244978 = EDGE_LOOP ( 'NONE', ( #200208, #118083, #137119, #226999 ) ) ;
#244979 = DIRECTION ( 'NONE',  ( 1.000000000000000000, -0.000000000000000000, -0.000000000000000000 ) ) ;
#244980 = ITEM_DEFINED_TRANSFORMATION ( 'NONE', 'NONE', #169433,  #2425 ) ;
#244981 = CARTESIAN_POINT ( 'NONE',  ( -23.25000000000000000, 78.48087866980282001, -232.8271061603568910 ) ) ;
#244982 = ORIENTED_EDGE ( 'NONE', *, *, #246090, .T. ) ;
#244983 = CARTESIAN_POINT ( 'NONE',  ( 20.94999999999999929, -8.999999999988842703, -57.50603087734755547 ) ) ;
#244984 = PRODUCT ( 'MAS-200', 'MAS-200', '', ( #52209 ) ) ;
#244985 = VECTOR ( 'NONE', #221362, 1000.000000000000000 ) ;
#244986 = CIRCLE ( 'NONE', #120130, 0.1000000000000024342 ) ;
#244987 = AXIS2_PLACEMENT_3D ( 'NONE', #59988, #182544, #101665 ) ;
#244988 = CARTESIAN_POINT ( 'NONE',  ( -20.94999999999999929, -1.164121893241208960, -41.41484808557160591 ) ) ;
#244989 = ORIENTED_EDGE ( 'NONE', *, *, #18927, .F. ) ;
#244990 = ORIENTED_EDGE ( 'NONE', *, *, #109633, .F. ) ;
#244991 = CARTESIAN_POINT ( 'NONE',  ( 23.14999999999999858, 36.65892442174935439, -249.5511627012433848 ) ) ;
#244992 = DIRECTION ( 'NONE',  ( 0.000000000000000000, -0.2128009952263603677, 0.9770955615653313941 ) ) ;
#244993 = LINE ( 'NONE', #63794, #107545 ) ;
#244994 = LINE ( 'NONE', #168077, #153066 ) ;
#244996 =( GEOMETRIC_REPRESENTATION_CONTEXT ( 3 ) GLOBAL_UNCERTAINTY_ASSIGNED_CONTEXT ( ( #203095 ) ) GLOBAL_UNIT_ASSIGNED_CONTEXT ( ( #48959, #24293, #128509 ) ) REPRESENTATION_CONTEXT ( 'NONE', 'WORKASPACE' ) );
#244995 = LINE ( 'NONE', #68955, #161111 ) ;
#244997 = DIRECTION ( 'NONE',  ( -1.000000000000000000, 0.000000000000000000, 0.000000000000000000 ) ) ;
#244998 = EDGE_CURVE ( 'NONE', #163484, #93865, #22597, .T. ) ;
#244999 = CARTESIAN_POINT ( 'NONE',  ( -16.93230518875208190, 10.00075036141984164, -12.57577834810150108 ) ) ;
#245000 = AXIS2_PLACEMENT_3D ( 'NONE', #89875, #12947, #50734 ) ;
#245002 = CARTESIAN_POINT ( 'NONE',  ( -18.49499033040907037, -9.438148771733516185, -74.19815322592347684 ) ) ;
#245001 = DIRECTION ( 'NONE',  ( -0.000000000000000000, -0.000000000000000000, -1.000000000000000000 ) ) ;
#245004 = TOROIDAL_SURFACE ( 'NONE', #20161, 0.2000000000000000111, 0.1000000000000000056 ) ;
#245003 = B_SPLINE_CURVE_WITH_KNOTS ( 'NONE', 3,
 ( #19063, #198984, #20375, #234249, #175589, #55585, #178166, #94744, #750, #96019 ),
 .UNSPECIFIED., .F., .F.,
 ( 4, 2, 2, 2, 4 ),
 ( 0.000000000000000000, 0.0001584437871624913314, 0.0002376656807437476358, 0.0002772766275343836349, 0.0003168875743250196882 ),
 .UNSPECIFIED. ) ;
#245005 = LINE ( 'NONE', #66373, #256197 ) ;
#245006 = CARTESIAN_POINT ( 'NONE',  ( 18.54999999999999716, 8.750000000011182166, -113.1500000000000341 ) ) ;
#245007 = DIRECTION ( 'NONE',  ( -1.000000000000000000, -0.000000000000000000, -0.000000000000000000 ) ) ;
#245008 = EDGE_LOOP ( 'NONE', ( #36322, #153385, #130225, #98301 ) ) ;
#245009 = VERTEX_POINT ( 'NONE', #143741 ) ;
#245010 = CARTESIAN_POINT ( 'NONE',  ( 13.99999999999999822, 9.850000000011137402, -184.2499999999999716 ) ) ;
#245011 = CARTESIAN_POINT ( 'NONE',  ( -23.25000000000000000, 36.65892442174935439, -249.5511627012433848 ) ) ;
#245013 = DIRECTION ( 'NONE',  ( 1.000000000000000000, 0.000000000000000000, 0.000000000000000000 ) ) ;
#245012 = CARTESIAN_POINT ( 'NONE',  ( -18.59999999999999787, 74.93036000061670165, -233.6816308724374949 ) ) ;
#245014 = CIRCLE ( 'NONE', #36951, 0.1000000000000000472 ) ;
#245015 = FACE_OUTER_BOUND ( 'NONE', #171012, .T. ) ;
#245017 = EDGE_CURVE ( 'NONE', #204155, #247, #39175, .T. ) ;
#245016 = CARTESIAN_POINT ( 'NONE',  ( -20.64999999999999858, 85.00000000001222134, -146.4170766071767389 ) ) ;
#245018 = CARTESIAN_POINT ( 'NONE',  ( -20.54999999999999716, 7.150000000011155876, -184.2499999999999716 ) ) ;
#245019 = CIRCLE ( 'NONE', #178410, 11.74999999999999822 ) ;
#245020 = ORIENTED_EDGE ( 'NONE', *, *, #191744, .F. ) ;
#245021 = VERTEX_POINT ( 'NONE', #239005 ) ;
#245022 = ADVANCED_FACE ( 'NONE', ( #160779 ), #139878, .T. ) ;
#245023 = AXIS2_PLACEMENT_3D ( 'NONE', #59215, #202622, #201340 ) ;
#245024 = AXIS2_PLACEMENT_3D ( 'NONE', #125335, #5351, #84875 ) ;
#245025 = LINE ( 'NONE', #209755, #138700 ) ;
#245026 = VECTOR ( 'NONE', #90527, 1000.000000000000000 ) ;
#245027 = ORIENTED_EDGE ( 'NONE', *, *, #7283, .F. ) ;
#245028 = LINE ( 'NONE', #27302, #247197 ) ;
#245029 = EDGE_CURVE ( 'NONE', #30013, #14308, #181584, .T. ) ;
#245030 = AXIS2_PLACEMENT_3D ( 'NONE', #155066, #232024, #234565 ) ;
#245031 = DIRECTION ( 'NONE',  ( 1.000000000000000000, 1.394253735153569469E-16, 2.602809386958778209E-16 ) ) ;
#245032 = EDGE_CURVE ( 'NONE', #157707, #64893, #201819, .T. ) ;
#245033 = ADVANCED_FACE ( 'NONE', ( #179061 ), #89384, .T. ) ;
#245034 = VERTEX_POINT ( 'NONE', #219415 ) ;
#245035 = DIRECTION ( 'NONE',  ( 1.000000000000000000, 0.000000000000000000, 0.000000000000000000 ) ) ;
#245036 = ORIENTED_EDGE ( 'NONE', *, *, #83493, .T. ) ;
#245037 = EDGE_CURVE ( 'NONE', #207164, #118177, #2940, .T. ) ;
#245038 = CARTESIAN_POINT ( 'NONE',  ( -18.59999999999999787, 85.32100840337361092, -162.7871692354464130 ) ) ;
#245039 = DIRECTION ( 'NONE',  ( 0.000000000000000000, 0.1568667991644355497, -0.9876197685951332295 ) ) ;
#245041 = CARTESIAN_POINT ( 'NONE',  ( -18.59999999999999787, 7.128833340094563376, -233.7327013124401276 ) ) ;
#245040 = AXIS2_PLACEMENT_3D ( 'NONE', #152388, #170691, #74138 ) ;
#245042 = CARTESIAN_POINT ( 'NONE',  ( 18.40000000000000213, -9.499999999988844479, -141.0320693966996828 ) ) ;
#245043 = CARTESIAN_POINT ( 'NONE',  ( 0.8999999999999993561, -8.250000000000005329, 26.00000000000000355 ) ) ;
#245044 = CARTESIAN_POINT ( 'NONE',  ( -21.51976009735018991, 6.910458441670358276, -134.0000000000000000 ) ) ;
#245045 = EDGE_CURVE ( 'NONE', #102805, #118647, #153336, .T. ) ;
#245046 = DIRECTION ( 'NONE',  ( -7.304098846218134667E-16, 1.000000000000000000, 6.982962677686266711E-15 ) ) ;
#245047 = CARTESIAN_POINT ( 'NONE',  ( -21.05000000000000071, 0.000000000000000000, 0.000000000000000000 ) ) ;
#245049 = ORIENTED_EDGE ( 'NONE', *, *, #76715, .F. ) ;
#245048 = CARTESIAN_POINT ( 'NONE',  ( 18.46932045258654398, -0.9001461170050899518, -242.3116320965393982 ) ) ;
#245051 = LINE ( 'NONE', #46828, #218401 ) ;
#245050 = CARTESIAN_POINT ( 'NONE',  ( 23.24999999999999289, 6.650000000011155876, -112.6500000000000341 ) ) ;
#245052 = ORIENTED_EDGE ( 'NONE', *, *, #168921, .F. ) ;
#245054 = ORIENTED_EDGE ( 'NONE', *, *, #177127, .F. ) ;
#245053 = DIRECTION ( 'NONE',  ( -0.000000000000000000, 6.982962677686266711E-15, -1.000000000000000000 ) ) ;
#245055 = VERTEX_POINT ( 'NONE', #109746 ) ;
#245056 = CARTESIAN_POINT ( 'NONE',  ( 18.54116936837189300, 85.46356419838404861, -62.47456499363600102 ) ) ;
#245057 = DIRECTION ( 'NONE',  ( 1.000000000000000000, 0.000000000000000000, 0.000000000000000000 ) ) ;
#245058 = CARTESIAN_POINT ( 'NONE',  ( 20.94999999999999929, 36.65892442174935439, -249.5511627012433848 ) ) ;
#245059 = CARTESIAN_POINT ( 'NONE',  ( -20.54999999999999716, 61.41373750439892376, -221.5848334931070553 ) ) ;
#245060 = CARTESIAN_POINT ( 'NONE',  ( 20.73486653747088582, 68.75000000001227818, -157.3731074845244109 ) ) ;
#245061 = CARTESIAN_POINT ( 'NONE',  ( 21.05000000000000071, -0.09999999998884338825, -160.9593430482987344 ) ) ;
#245063 = ADVANCED_FACE ( 'NONE', ( #227127 ), #135162, .F. ) ;
#245062 = DIRECTION ( 'NONE',  ( 1.000000000000000000, 0.000000000000000000, 0.000000000000000000 ) ) ;
#245064 = CARTESIAN_POINT ( 'NONE',  ( 21.09316766718127667, 69.62984668753773576, -136.5623708868390338 ) ) ;
#245065 = VECTOR ( 'NONE', #209746, 1000.000000000000000 ) ;
#245066 = ORIENTED_EDGE ( 'NONE', *, *, #58095, .T. ) ;
#245067 = ORIENTED_EDGE ( 'NONE', *, *, #76450, .T. ) ;
#245068 = AXIS2_PLACEMENT_3D ( 'NONE', #257305, #237806, #198671 ) ;
#245069 = LINE ( 'NONE', #161709, #68695 ) ;
#245070 = CIRCLE ( 'NONE', #28450, 0.1000000000000028644 ) ;
#245071 = ORIENTED_EDGE ( 'NONE', *, *, #87278, .F. ) ;
#245072 = DIRECTION ( 'NONE',  ( 1.000000000000000000, 0.000000000000000000, 0.000000000000000000 ) ) ;
#245073 = ORIENTED_EDGE ( 'NONE', *, *, #123914, .T. ) ;
#245074 = CARTESIAN_POINT ( 'NONE',  ( 23.24999999999999645, 71.00000000001151079, -48.42837350343745584 ) ) ;
#245075 = ADVANCED_FACE ( 'NONE', ( #26384 ), #146307, .F. ) ;
#245076 = CIRCLE ( 'NONE', #207672, 0.09999999999998898659 ) ;
#245077 = CARTESIAN_POINT ( 'NONE',  ( -16.97092634996677774, 10.00088896635983460, -180.1301427662975243 ) ) ;
#245078 = LINE ( 'NONE', #50696, #34662 ) ;
#245079 = DIRECTION ( 'NONE',  ( 1.000000000000000000, 0.000000000000000000, 0.000000000000000000 ) ) ;
#245080 = FACE_OUTER_BOUND ( 'NONE', #134944, .T. ) ;
#245081 = VERTEX_POINT ( 'NONE', #8102 ) ;
#245082 = DIRECTION ( 'NONE',  ( 1.000000000000000000, -7.304098846218134667E-16, -5.100424963727256530E-30 ) ) ;
#245083 = TOROIDAL_SURFACE ( 'NONE', #49454, 7.800000000000000711, 0.1000000000000000056 ) ;
#245084 = VECTOR ( 'NONE', #59832, 1000.000000000000000 ) ;
#245086 = CIRCLE ( 'NONE', #41102, 0.1000000000000054040 ) ;
#245085 = CYLINDRICAL_SURFACE ( 'NONE', #100451, 0.09999999999999939493 ) ;
#245087 = CARTESIAN_POINT ( 'NONE',  ( -20.94999999999999929, -1.164121893230052995, -74.91484808557160591 ) ) ;
#245089 = EDGE_CURVE ( 'NONE', #181320, #217695, #148900, .T. ) ;
#245088 = DIRECTION ( 'NONE',  ( -1.000000000000000000, 1.652117596168391700E-15, 0.000000000000000000 ) ) ;
#245090 = ORIENTED_EDGE ( 'NONE', *, *, #113747, .F. ) ;
#245092 = DIRECTION ( 'NONE',  ( 0.000000000000000000, 1.000000000000000000, 0.000000000000000000 ) ) ;
#245091 = DIRECTION ( 'NONE',  ( -1.000000000000000000, 0.000000000000000000, -0.000000000000000000 ) ) ;
#245093 = VERTEX_POINT ( 'NONE', #91486 ) ;
#245096 = ORIENTED_EDGE ( 'NONE', *, *, #232160, .F. ) ;
#245095 = DIRECTION ( 'NONE',  ( 0.000000000000000000, 1.000000000000000000, 0.000000000000000000 ) ) ;
#245094 = CARTESIAN_POINT ( 'NONE',  ( 21.93642651522410603, 68.67283376068616008, -103.0231074845243739 ) ) ;
#245097 = EDGE_CURVE ( 'NONE', #208385, #172995, #43612, .T. ) ;
#245098 = ORIENTED_EDGE ( 'NONE', *, *, #93452, .F. ) ;
#245099 = AXIS2_PLACEMENT_3D ( 'NONE', #115630, #79037, #158635 ) ;
#245100 = CARTESIAN_POINT ( 'NONE',  ( 21.05000000000000071, 10.38152206507873387, -207.4259860971185958 ) ) ;
#245101 = DIRECTION ( 'NONE',  ( 1.000000000000000000, -0.000000000000000000, -0.000000000000000000 ) ) ;
#245102 = CARTESIAN_POINT ( 'NONE',  ( -20.90000000000000213, 11.59795743183152972, -1.899104650876408451 ) ) ;
#245103 = EDGE_LOOP ( 'NONE', ( #160889, #151596, #201597, #254064 ) ) ;
#245104 = DIRECTION ( 'NONE',  ( 0.000000000000000000, 0.4721928772777343464, 0.8814952561688431665 ) ) ;
#245107 = ADVANCED_FACE ( 'NONE', ( #225821 ), #90174, .T. ) ;
#245106 = PLANE ( 'NONE',  #11385 ) ;
#245105 =( BOUNDED_CURVE ( )  B_SPLINE_CURVE ( 3, ( #141658, #221184, #201630, #197778 ),
 .UNSPECIFIED., .F., .F. ) 
 B_SPLINE_CURVE_WITH_KNOTS ( ( 4, 4 ),
 ( 3.192897208853993085, 4.712388980384689674 ),
 .UNSPECIFIED. ) 
 CURVE ( )  GEOMETRIC_REPRESENTATION_ITEM ( )  RATIONAL_B_SPLINE_CURVE ( ( 1.000000000000000000, 0.8166740347213228279, 0.8166740347213228279, 1.000000000000000000 ) ) 
 REPRESENTATION_ITEM ( '' )  );
#245109 = CARTESIAN_POINT ( 'NONE',  ( 20.94999999999999929, 74.16465844978715438, -57.96795619196134908 ) ) ;
#245108 = DIRECTION ( 'NONE',  ( 0.000000000000000000, -0.9999631594459056361, -0.008583690987124413183 ) ) ;
#245111 = ORIENTED_EDGE ( 'NONE', *, *, #17849, .T. ) ;
#245110 = DIRECTION ( 'NONE',  ( -1.000000000000000000, -1.875376730785737719E-16, -0.000000000000000000 ) ) ;
#245112 = EDGE_CURVE ( 'NONE', #70808, #256115, #72667, .T. ) ;
#245113 = EDGE_CURVE ( 'NONE', #23601, #237787, #150188, .T. ) ;
#245114 = ORIENTED_EDGE ( 'NONE', *, *, #135245, .T. ) ;
#245115 = VECTOR ( 'NONE', #166390, 1000.000000000000000 ) ;
#245116 = CARTESIAN_POINT ( 'NONE',  ( 23.14999999999999503, 69.35000000001180354, -81.87310748452435405 ) ) ;
#245117 = CARTESIAN_POINT ( 'NONE',  ( 18.39999999999999503, 64.25000000001261924, -190.8731074845244393 ) ) ;
#245118 = AXIS2_PLACEMENT_3D ( 'NONE', #91529, #152820, #215320 ) ;
#245119 = VECTOR ( 'NONE', #197849, 1000.000000000000000 ) ;
#245120 = DIRECTION ( 'NONE',  ( -1.000000000000000000, -0.000000000000000000, 0.000000000000000000 ) ) ;
#245121 = ORIENTED_EDGE ( 'NONE', *, *, #159742, .F. ) ;
#245122 = DIRECTION ( 'NONE',  ( -2.952720810173289112E-16, -1.000000000000000000, -6.982962677686266711E-15 ) ) ;
#245123 = ORIENTED_EDGE ( 'NONE', *, *, #68389, .F. ) ;
#245124 = ADVANCED_FACE ( 'NONE', ( #51031, #88895 ), #130604, .F. ) ;
#245125 = DIRECTION ( 'NONE',  ( 0.000000000000000000, 0.000000000000000000, 1.000000000000000000 ) ) ;
#245126 = CYLINDRICAL_SURFACE ( 'NONE', #253490, 0.09999999999998898659 ) ;
#245127 = DIRECTION ( 'NONE',  ( 0.000000000000000000, 2.891205793294679805E-16, -1.000000000000000000 ) ) ;
#245128 = VECTOR ( 'NONE', #250458, 1000.000000000000000 ) ;
#245129 = ORIENTED_EDGE ( 'NONE', *, *, #151824, .F. ) ;
#245130 = DIRECTION ( 'NONE',  ( 1.000000000000000000, 0.000000000000000000, 0.000000000000000000 ) ) ;
#245131 = EDGE_LOOP ( 'NONE', ( #193983, #165244 ) ) ;
#245132 = AXIS2_PLACEMENT_3D ( 'NONE', #36030, #154708, #234198 ) ;
#245134 = VECTOR ( 'NONE', #254219, 1000.000000000000000 ) ;
#245133 = CARTESIAN_POINT ( 'NONE',  ( -23.24999999999999645, -9.599999999988845900, -73.60018939122203108 ) ) ;
#245135 = CARTESIAN_POINT ( 'NONE',  ( -20.54999999999999716, 21.39147882631411335, -233.2615922652120730 ) ) ;
#245136 = VECTOR ( 'NONE', #105085, 1000.000000000000000 ) ;
#245137 = VERTEX_POINT ( 'NONE', #168499 ) ;
#245138 = VERTEX_POINT ( 'NONE', #190602 ) ;
#245139 = AXIS2_PLACEMENT_3D ( 'NONE', #54798, #74415, #217715 ) ;
#245140 = ORIENTED_EDGE ( 'NONE', *, *, #82864, .F. ) ;
#245141 = LINE ( 'NONE', #48214, #116563 ) ;
#245142 = ORIENTED_EDGE ( 'NONE', *, *, #218641, .T. ) ;
#245144 = EDGE_LOOP ( 'NONE', ( #159591, #215282, #34191, #190663, #141328 ) ) ;
#245143 = CARTESIAN_POINT ( 'NONE',  ( -22.39999999999999858, 1.115488181425289271E-11, -155.8504291924551808 ) ) ;
#245145 = ADVANCED_FACE ( 'NONE', ( #147600 ), #11970, .T. ) ;
#245146 = EDGE_CURVE ( 'NONE', #93777, #212172, #111043, .T. ) ;
#245147 = VERTEX_POINT ( 'NONE', #185448 ) ;
#245149 = ORIENTED_EDGE ( 'NONE', *, *, #45510, .F. ) ;
#245148 = VERTEX_POINT ( 'NONE', #71931 ) ;
#245151 = EDGE_CURVE ( 'NONE', #64290, #205292, #185075, .T. ) ;
#245150 = CARTESIAN_POINT ( 'NONE',  ( -18.50000000000000000, 30.31654117411694571, -235.6601881227570914 ) ) ;
#245153 = ORIENTED_EDGE ( 'NONE', *, *, #40219, .F. ) ;
#245152 = AXIS2_PLACEMENT_3D ( 'NONE', #255561, #213921, #76971 ) ;
#245154 = DIRECTION ( 'NONE',  ( 0.000000000000000000, -1.000000000000000000, -6.982962677686265922E-15 ) ) ;
#245155 = DIRECTION ( 'NONE',  ( 0.000000000000000000, 0.000000000000000000, 1.000000000000000000 ) ) ;
#245156 = DIRECTION ( 'NONE',  ( 0.000000000000000000, -6.352154140967427193E-15, 1.000000000000000000 ) ) ;
#245157 = CIRCLE ( 'NONE', #124353, 4.049999999999998046 ) ;
#245158 = DIRECTION ( 'NONE',  ( 1.000000000000000000, 0.000000000000000000, 0.000000000000000000 ) ) ;
#245159 = AXIS2_PLACEMENT_3D ( 'NONE', #203614, #161943, #182787 ) ;
#245160 = AXIS2_PLACEMENT_3D ( 'NONE', #167001, #45728, #49585 ) ;
#245161 = ORIENTED_EDGE ( 'NONE', *, *, #54687, .F. ) ;
#245162 = EDGE_LOOP ( 'NONE', ( #171086, #85049, #241217, #96252, #159510, #90466, #126222, #2904, #41912 ) ) ;
#245163 = DIRECTION ( 'NONE',  ( -0.000000000000000000, 1.000000000000000000, -0.000000000000000000 ) ) ;
#245165 = EDGE_LOOP ( 'NONE', ( #228389, #249600, #249943, #219947 ) ) ;
#245164 = CARTESIAN_POINT ( 'NONE',  ( 18.50000000000030553, 63.78126560769650411, -209.3017168652885971 ) ) ;
#245166 = CARTESIAN_POINT ( 'NONE',  ( -18.50000000000000000, 1.340746217933695750, 10.27286250542118040 ) ) ;
#245168 = ORIENTED_EDGE ( 'NONE', *, *, #100979, .T. ) ;
#245167 = DIRECTION ( 'NONE',  ( 2.694716079187272946E-16, -1.000000000000000000, 0.000000000000000000 ) ) ;
#245169 = CIRCLE ( 'NONE', #241090, 0.09999999999999939493 ) ;
#245170 = ORIENTED_EDGE ( 'NONE', *, *, #147757, .F. ) ;
#245171 = DIRECTION ( 'NONE',  ( 0.000000000000000000, 0.000000000000000000, 1.000000000000000000 ) ) ;
#245172 = ORIENTED_EDGE ( 'NONE', *, *, #159796, .T. ) ;
#245173 = EDGE_LOOP ( 'NONE', ( #111207, #123334, #194055, #219205 ) ) ;
#245174 = CARTESIAN_POINT ( 'NONE',  ( -18.59999999999999787, 69.15387683765879956, -32.28538121767450519 ) ) ;
#245176 = ADVANCED_FACE ( 'NONE', ( #231017 ), #208227, .T. ) ;
#245175 = LINE ( 'NONE', #66541, #236105 ) ;
#245177 = CIRCLE ( 'NONE', #252972, 0.9000000000000014655 ) ;
#245178 = VECTOR ( 'NONE', #203604, 1000.000000000000114 ) ;
#245180 = VERTEX_POINT ( 'NONE', #216562 ) ;
#245179 = ORIENTED_EDGE ( 'NONE', *, *, #128700, .T. ) ;
#245182 = EDGE_LOOP ( 'NONE', ( #121703, #151170, #108792, #168037 ) ) ;
#245181 = AXIS2_PLACEMENT_3D ( 'NONE', #91121, #111985, #191540 ) ;
#245183 = CARTESIAN_POINT ( 'NONE',  ( -16.84419801905645642, 9.950000000011140600, -54.33051015377797910 ) ) ;
#245184 = ORIENTED_EDGE ( 'NONE', *, *, #258100, .T. ) ;
#245185 = VERTEX_POINT ( 'NONE', #172356 ) ;
#245186 = DIRECTION ( 'NONE',  ( 0.000000000000000000, 0.000000000000000000, 1.000000000000000000 ) ) ;
#245189 = ADVANCED_FACE ( 'NONE', ( #211430 ), #73240, .T. ) ;
#245188 = VERTEX_POINT ( 'NONE', #212726 ) ;
#245187 = DIRECTION ( 'NONE',  ( 0.000000000000000000, 0.3116596277708317264, 0.9501938099239264357 ) ) ;
#245190 = CARTESIAN_POINT ( 'NONE',  ( -19.89999999999999858, 4.513204987021263825, 22.00000000000000355 ) ) ;
#245192 = DIRECTION ( 'NONE',  ( 0.000000000000000000, -7.026728003956686545E-15, 1.000000000000000000 ) ) ;
#245191 = DIRECTION ( 'NONE',  ( 1.000000000000000000, 0.000000000000000000, 0.000000000000000000 ) ) ;
#245193 = CARTESIAN_POINT ( 'NONE',  ( 22.39999999999999503, 76.00000000001173817, -81.17267829206912211 ) ) ;
#245194 = CYLINDRICAL_SURFACE ( 'NONE', #102820, 7.900000000000003908 ) ;
#245195 = ORIENTED_EDGE ( 'NONE', *, *, #24600, .F. ) ;
#245196 = AXIS2_PLACEMENT_3D ( 'NONE', #212575, #13092, #136867 ) ;
#245197 = EDGE_CURVE ( 'NONE', #232353, #237270, #22610, .T. ) ;
#245198 = AXIS2_PLACEMENT_3D ( 'NONE', #152459, #134135, #213683 ) ;
#245199 = ORIENTED_EDGE ( 'NONE', *, *, #159858, .F. ) ;
#245200 = CARTESIAN_POINT ( 'NONE',  ( -20.64999999999999858, 36.65892442174935439, -249.5511627012433848 ) ) ;
#245201 = CARTESIAN_POINT ( 'NONE',  ( 21.05000000000000071, 7.525330762710603416, -212.0571253909869256 ) ) ;
#245202 = EDGE_CURVE ( 'NONE', #32241, #13384, #205918, .T. ) ;
#245203 = CIRCLE ( 'NONE', #182669, 0.1999999999999987899 ) ;
#245204 = VERTEX_POINT ( 'NONE', #234851 ) ;
#245205 = CIRCLE ( 'NONE', #132793, 0.09999999999999939493 ) ;
#245206 = ADVANCED_FACE ( 'NONE', ( #54904 ), #222648, .T. ) ;
#245207 = CARTESIAN_POINT ( 'NONE',  ( -23.25000000000000000, 2.000000000011154189, -87.27537807723794572 ) ) ;
#245209 = ADVANCED_FACE ( 'NONE', ( #13245 ), #39362, .T. ) ;
#245208 = EDGE_CURVE ( 'NONE', #172097, #137324, #17104, .T. ) ;
#245210 = ORIENTED_EDGE ( 'NONE', *, *, #26137, .T. ) ;
#245211 = EDGE_LOOP ( 'NONE', ( #180027, #135400, #249390, #167215 ) ) ;
#245212 = FACE_OUTER_BOUND ( 'NONE', #89338, .T. ) ;
#245213 = DIRECTION ( 'NONE',  ( 0.000000000000000000, 0.000000000000000000, -1.000000000000000000 ) ) ;
#245214 = ORIENTED_EDGE ( 'NONE', *, *, #130486, .F. ) ;
#245215 = DIRECTION ( 'NONE',  ( 0.000000000000000000, 4.336808689942494997E-15, -1.000000000000000000 ) ) ;
#245216 = CARTESIAN_POINT ( 'NONE',  ( 21.14999999999999858, 69.35000000001228670, -157.6731074845243938 ) ) ;
#245217 = ORIENTED_EDGE ( 'NONE', *, *, #132511, .F. ) ;
#245218 = CARTESIAN_POINT ( 'NONE',  ( -21.05000000000000071, -11.48912529306489994, -130.9000000000000341 ) ) ;
#245219 = DIRECTION ( 'NONE',  ( 0.2834754621636439431, -0.2834754621636535465, -0.9161240771326838450 ) ) ;
#245221 = CARTESIAN_POINT ( 'NONE',  ( -21.05000000000000071, 6.540656951712397138, -67.10000000000005116 ) ) ;
#245220 = CARTESIAN_POINT ( 'NONE',  ( 23.24999999999999645, 4.775700934590591196, -155.6512318959540551 ) ) ;
#245222 = CYLINDRICAL_SURFACE ( 'NONE', #243930, 0.1000000000000000472 ) ;
#245224 = CIRCLE ( 'NONE', #78603, 0.1000000000000028644 ) ;
#245223 = FACE_OUTER_BOUND ( 'NONE', #59929, .T. ) ;
#245225 = AXIS2_PLACEMENT_3D ( 'NONE', #67922, #109607, #7964 ) ;
#245226 = CYLINDRICAL_SURFACE ( 'NONE', #228081, 0.09999999999998898659 ) ;
#245227 = DIRECTION ( 'NONE',  ( 0.000000000000000000, 0.000000000000000000, -1.000000000000000000 ) ) ;
#245228 = CIRCLE ( 'NONE', #216153, 0.1000000000000055844 ) ;
#245229 = EDGE_LOOP ( 'NONE', ( #71234, #85775, #1723, #214181 ) ) ;
#245230 = EDGE_CURVE ( 'NONE', #206051, #199909, #68561, .T. ) ;
#245231 = EDGE_CURVE ( 'NONE', #159306, #146245, #209162, .T. ) ;
#245233 = ORIENTED_EDGE ( 'NONE', *, *, #103394, .T. ) ;
#245232 = ORIENTED_EDGE ( 'NONE', *, *, #29780, .F. ) ;
#245234 = ORIENTED_EDGE ( 'NONE', *, *, #75532, .T. ) ;
#245235 = EDGE_CURVE ( 'NONE', #59781, #251339, #227986, .T. ) ;
#245236 = CARTESIAN_POINT ( 'NONE',  ( 21.00000000000000000, 63.38346053167636995, -212.7939182281409956 ) ) ;
#245238 = CARTESIAN_POINT ( 'NONE',  ( -17.04295772865466319, 10.02489942527108369, -146.6500000000000341 ) ) ;
#245237 = CARTESIAN_POINT ( 'NONE',  ( 20.94999999999999574, -1.162701749926853712, -108.6000000000000227 ) ) ;
#245239 = CARTESIAN_POINT ( 'NONE',  ( -21.09316766718153247, 75.96073659769751885, -142.8932607969990158 ) ) ;
#245240 = ORIENTED_EDGE ( 'NONE', *, *, #102683, .F. ) ;
#245241 = AXIS2_PLACEMENT_3D ( 'NONE', #152070, #231593, #15113 ) ;
#245242 = DIRECTION ( 'NONE',  ( 1.000000000000000000, 0.000000000000000000, 0.000000000000000000 ) ) ;
#245243 = ADVANCED_FACE ( 'NONE', ( #92314 ), #188854, .F. ) ;
#245244 = DIRECTION ( 'NONE',  ( 1.000000000000000000, 0.000000000000000000, 0.000000000000000000 ) ) ;
#245245 = FACE_OUTER_BOUND ( 'NONE', #105560, .T. ) ;
#245246 = EDGE_CURVE ( 'NONE', #100635, #43295, #66579, .T. ) ;
#245247 = CARTESIAN_POINT ( 'NONE',  ( -20.00857864376270001, 9.150000000011157653, -188.6499999999999488 ) ) ;
#245248 = ORIENTED_EDGE ( 'NONE', *, *, #129086, .T. ) ;
#245249 = FACE_OUTER_BOUND ( 'NONE', #22564, .T. ) ;
#245250 = DIRECTION ( 'NONE',  ( 0.000000000000000000, -0.9908441862701610203, 0.1350103645451807555 ) ) ;
#245251 = EDGE_LOOP ( 'NONE', ( #88846, #106364, #49892, #108238 ) ) ;
#245252 = VERTEX_POINT ( 'NONE', #186303 ) ;
#245253 = CARTESIAN_POINT ( 'NONE',  ( -16.87331047859649757, 9.950000000011138823, -54.35000000000000142 ) ) ;
#245254 = DIRECTION ( 'NONE',  ( 1.000000000000000000, 0.000000000000000000, 0.000000000000000000 ) ) ;
#245255 = LINE ( 'NONE', #125304, #177856 ) ;
#245256 = EDGE_CURVE ( 'NONE', #224195, #221121, #176900, .T. ) ;
#245257 = CARTESIAN_POINT ( 'NONE',  ( 20.94999999999999574, 67.07338541492450190, -61.05142446530125966 ) ) ;
#245258 = CARTESIAN_POINT ( 'NONE',  ( -23.15000000000000213, 75.39949836213489220, -250.2448839681187849 ) ) ;
#245259 = CARTESIAN_POINT ( 'NONE',  ( -21.05000000000000071, 6.257814610481521989, 0.09779029130922732571 ) ) ;
#245260 = ORIENTED_EDGE ( 'NONE', *, *, #64439, .T. ) ;
#245261 = DIRECTION ( 'NONE',  ( 0.000000000000000000, 0.000000000000000000, -1.000000000000000000 ) ) ;
#245262 = CARTESIAN_POINT ( 'NONE',  ( 21.05000000000096350, 11.98086986275577459, -206.1603386415442856 ) ) ;
#245264 = CARTESIAN_POINT ( 'NONE',  ( -20.94999999999999929, 11.75000000001120171, -174.3416006898970636 ) ) ;
#245263 = LINE ( 'NONE', #48332, #216078 ) ;
#245265 = CARTESIAN_POINT ( 'NONE',  ( -18.40000000000000213, 11.47316190336248809, -20.94999999999999929 ) ) ;
#245267 = ADVANCED_FACE ( 'NONE', ( #91042 ), #110597, .F. ) ;
#245266 = PLANE ( 'NONE',  #79271 ) ;
#245268 = AXIS2_PLACEMENT_3D ( 'NONE', #47747, #84268, #227678 ) ;
#245269 = CIRCLE ( 'NONE', #132837, 0.5000000000000004441 ) ;
#245270 = CARTESIAN_POINT ( 'NONE',  ( 21.05000000000000071, 71.14953271029236248, -115.0573748935260028 ) ) ;
#245271 = DIRECTION ( 'NONE',  ( 2.952720810173289112E-16, -1.000000000000000000, 0.000000000000000000 ) ) ;
#245272 = AXIS2_PLACEMENT_3D ( 'NONE', #137216, #216747, #124092 ) ;
#245273 = CIRCLE ( 'NONE', #195392, 0.09999999999999971412 ) ;
#245275 = ORIENTED_EDGE ( 'NONE', *, *, #166379, .T. ) ;
#245274 = CARTESIAN_POINT ( 'NONE',  ( -20.94999999999999929, 67.23127455305835554, -235.8551265064784559 ) ) ;
#245276 = CIRCLE ( 'NONE', #82906, 12.77499999999999325 ) ;
#245277 = EDGE_CURVE ( 'NONE', #38380, #16525, #97744, .T. ) ;
#245278 = CARTESIAN_POINT ( 'NONE',  ( 18.49999999999999645, 1.835341550235567887, -179.0551512925629538 ) ) ;
#245279 = CIRCLE ( 'NONE', #12247, 0.1000000000000054040 ) ;
#245280 = TOROIDAL_SURFACE ( 'NONE', #132855, 0.4000000000000010214, 0.1000000000000000056 ) ;
#245282 = VECTOR ( 'NONE', #230633, 1000.000000000000000 ) ;
#245281 = CARTESIAN_POINT ( 'NONE',  ( 21.59780538579341780, 65.34350030841025614, -242.4375845506680207 ) ) ;
#245283 = CARTESIAN_POINT ( 'NONE',  ( 21.07094088545368038, 65.48150606888252412, -241.9290547188616074 ) ) ;
#245284 = EDGE_LOOP ( 'NONE', ( #12946, #155157, #216408, #150292 ) ) ;
#245285 = CIRCLE ( 'NONE', #132868, 0.5000000000000022204 ) ;
#245286 = CARTESIAN_POINT ( 'NONE',  ( 23.40000000000005542, 77.83551161375991967, -47.52760213295649550 ) ) ;
#245287 = DIRECTION ( 'NONE',  ( -1.000000000000000000, 0.000000000000000000, -0.000000000000000000 ) ) ;
#245288 = DIRECTION ( 'NONE',  ( 0.000000000000000000, 0.000000000000000000, 1.000000000000000000 ) ) ;
#245289 = VERTEX_POINT ( 'NONE', #191462 ) ;
#245290 = DIRECTION ( 'NONE',  ( 1.000000000000000000, 0.000000000000000000, 0.000000000000000000 ) ) ;
#245292 = VERTEX_POINT ( 'NONE', #170634 ) ;
#245291 = DIRECTION ( 'NONE',  ( -1.000000000000000000, 0.000000000000000000, -0.000000000000000000 ) ) ;
#245294 = DIRECTION ( 'NONE',  ( 0.000000000000000000, -0.8741572761215442577, 0.4856429311786202851 ) ) ;
#245293 = DIRECTION ( 'NONE',  ( 1.000000000000000000, 0.000000000000000000, 0.000000000000000000 ) ) ;
#245295 = FACE_OUTER_BOUND ( 'NONE', #85222, .T. ) ;
#245296 = ORIENTED_EDGE ( 'NONE', *, *, #40321, .F. ) ;
#245297 = CARTESIAN_POINT ( 'NONE',  ( 20.94999999999999929, 5.000000000011153745, -121.5947339810869465 ) ) ;
#245298 = DIRECTION ( 'NONE',  ( 0.000000000000000000, 0.000000000000000000, 1.000000000000000000 ) ) ;
#245299 = DIRECTION ( 'NONE',  ( -0.000000000000000000, 0.4721928772777345684, 0.8814952561688429444 ) ) ;
#245300 = DIRECTION ( 'NONE',  ( -1.000000000000000000, 0.000000000000000000, 0.000000000000000000 ) ) ;
#245301 = DIRECTION ( 'NONE',  ( -1.000000000000000000, -1.836970198721029934E-16, 0.000000000000000000 ) ) ;
#245302 = VERTEX_POINT ( 'NONE', #152326 ) ;
#245303 = CARTESIAN_POINT ( 'NONE',  ( 21.05000000000000071, 87.48912529308852015, -173.1231074845242688 ) ) ;
#245304 = CYLINDRICAL_SURFACE ( 'NONE', #163289, 0.09999999999998898659 ) ;
#245305 = B_SPLINE_CURVE_WITH_KNOTS ( 'NONE', 3,
 ( #49657, #112223, #129206, #170948, #73114, #131762, #127922 ),
 .UNSPECIFIED., .F., .F.,
 ( 4, 3, 4 ),
 ( 0.000000000000000000, 3.357501770813427151E-05, 5.199112466348487506E-05 ),
 .UNSPECIFIED. ) ;
#245306 = VECTOR ( 'NONE', #70412, 1000.000000000000000 ) ;
#245307 = DIRECTION ( 'NONE',  ( 1.000000000000000000, -0.000000000000000000, -0.000000000000000000 ) ) ;
#245308 = CARTESIAN_POINT ( 'NONE',  ( -20.54999999999999716, 24.07562609839690992, -252.7152152143214892 ) ) ;
#245309 = VERTEX_POINT ( 'NONE', #149755 ) ;
#245310 = AXIS2_PLACEMENT_3D ( 'NONE', #170533, #229175, #173095 ) ;
#245311 = ORIENTED_EDGE ( 'NONE', *, *, #137079, .F. ) ;
#245312 = DIRECTION ( 'NONE',  ( 0.000000000000000000, -0.8777080977375715243, 0.4791956752370512551 ) ) ;
#245313 = CARTESIAN_POINT ( 'NONE',  ( -23.15000000000000213, 78.50726470275243685, -228.6618886302502176 ) ) ;
#245314 = DIRECTION ( 'NONE',  ( 1.000000000000000000, 0.000000000000000000, 0.000000000000000000 ) ) ;
#245315 = LINE ( 'NONE', #103205, #178652 ) ;
#245316 = DIRECTION ( 'NONE',  ( 0.000000000000000000, 0.2128009952263485993, -0.9770955615653341697 ) ) ;
#245317 = EDGE_CURVE ( 'NONE', #71198, #247436, #89740, .T. ) ;
#245319 = DIRECTION ( 'NONE',  ( 0.000000000000000000, 0.000000000000000000, -1.000000000000000000 ) ) ;
#245318 = CARTESIAN_POINT ( 'NONE',  ( -16.83794237512073622, 12.42360805125251311, -211.3979450943548954 ) ) ;
#245321 = FACE_OUTER_BOUND ( 'NONE', #239832, .T. ) ;
#245320 = AXIS2_PLACEMENT_3D ( 'NONE', #12449, #191093, #251016 ) ;
#245322 = FACE_OUTER_BOUND ( 'NONE', #31348, .T. ) ;
#245323 = CARTESIAN_POINT ( 'NONE',  ( -22.57320508075686405, 64.25000000001213607, -136.5231074845243313 ) ) ;
#245324 = VECTOR ( 'NONE', #60261, 1000.000000000000000 ) ;
#245325 = DIRECTION ( 'NONE',  ( 0.000000000000000000, 0.000000000000000000, 1.000000000000000000 ) ) ;
#245327 = ORIENTED_EDGE ( 'NONE', *, *, #28471, .F. ) ;
#245326 = DIRECTION ( 'NONE',  ( 1.000000000000000000, 0.000000000000000000, 0.000000000000000000 ) ) ;
#245328 = DIRECTION ( 'NONE',  ( 1.000000000000000000, 0.000000000000000000, 0.000000000000000000 ) ) ;
#245329 = CIRCLE ( 'NONE', #132901, 0.1000000000000013933 ) ;
#245330 = CARTESIAN_POINT ( 'NONE',  ( 23.14999999999999503, 11.65000000001116298, -193.9851942293460070 ) ) ;
#245332 = DIRECTION ( 'NONE',  ( -3.265361837132813093E-16, 0.9770955615653357240, 0.2128009952263411608 ) ) ;
#245331 = DIRECTION ( 'NONE',  ( -3.265361837132813093E-16, 1.000000000000000000, 0.000000000000000000 ) ) ;
#245333 = ORIENTED_EDGE ( 'NONE', *, *, #28481, .T. ) ;
#245334 = DIRECTION ( 'NONE',  ( -1.000000000000000000, -0.000000000000000000, -0.000000000000000000 ) ) ;
#245335 = CARTESIAN_POINT ( 'NONE',  ( -18.59999999999999787, 64.75617845954087670, -200.4736850529726269 ) ) ;
#245336 = FACE_OUTER_BOUND ( 'NONE', #210162, .T. ) ;
#245337 = DIRECTION ( 'NONE',  ( 0.000000000000000000, 0.2617529984165033463, 0.9651348961777156399 ) ) ;
#245338 = LINE ( 'NONE', #8018, #206307 ) ;
#245339 = ORIENTED_EDGE ( 'NONE', *, *, #221798, .T. ) ;
#245340 = VECTOR ( 'NONE', #122763, 1000.000000000000000 ) ;
#245341 = AXIS2_PLACEMENT_3D ( 'NONE', #202029, #2522, #256801 ) ;
#245343 = EDGE_CURVE ( 'NONE', #247011, #151569, #139255, .T. ) ;
#245342 = ORIENTED_EDGE ( 'NONE', *, *, #69755, .F. ) ;
#245344 = ADVANCED_FACE ( 'NONE', ( #190154 ), #169337, .F. ) ;
#245345 = CARTESIAN_POINT ( 'NONE',  ( -21.05000000000000071, 6.257814610487270279, -66.90220970869124528 ) ) ;
#245346 = VERTEX_POINT ( 'NONE', #229278 ) ;
#245347 = DIRECTION ( 'NONE',  ( 1.000000000000000000, 0.000000000000000000, 0.000000000000000000 ) ) ;
#245348 = ORIENTED_EDGE ( 'NONE', *, *, #19330, .F. ) ;
#245349 = AXIS2_PLACEMENT_3D ( 'NONE', #40024, #216044, #257688 ) ;
#245350 = DIRECTION ( 'NONE',  ( -0.000000000000000000, -6.982962677686266711E-15, 1.000000000000000000 ) ) ;
#245352 = CIRCLE ( 'NONE', #257934, 12.77499999999999503 ) ;
#245351 = CARTESIAN_POINT ( 'NONE',  ( -23.25000000000000000, -1.164121893230052995, -208.9148480855715775 ) ) ;
#245353 = VECTOR ( 'NONE', #92212, 1000.000000000000000 ) ;
#245354 = EDGE_CURVE ( 'NONE', #109044, #239723, #127604, .T. ) ;
#245356 = EDGE_CURVE ( 'NONE', #121066, #66860, #56057, .T. ) ;
#245355 = CARTESIAN_POINT ( 'NONE',  ( 18.59999999999999076, 8.006782298343173565, -209.8034900594678618 ) ) ;
#245357 = ORIENTED_EDGE ( 'NONE', *, *, #139206, .T. ) ;
#245358 = VECTOR ( 'NONE', #225295, 1000.000000000000000 ) ;
#245359 = EDGE_CURVE ( 'NONE', #65554, #144682, #67620, .T. ) ;
#245360 = DIRECTION ( 'NONE',  ( -1.000000000000000000, 0.000000000000000000, 0.000000000000000000 ) ) ;
#245361 = DIRECTION ( 'NONE',  ( 0.000000000000000000, 0.000000000000000000, -1.000000000000000000 ) ) ;
#245362 = CARTESIAN_POINT ( 'NONE',  ( 21.05000000000000071, 11.60000000001116049, -160.5717967697245285 ) ) ;
#245363 = CARTESIAN_POINT ( 'NONE',  ( -23.15000000000000213, 1.115600667400684642E-11, -88.70000000000004547 ) ) ;
#245364 = CARTESIAN_POINT ( 'NONE',  ( -16.94225986326249966, 44.40627002368546528, -235.1776217765174977 ) ) ;
#245365 = FACE_OUTER_BOUND ( 'NONE', #249387, .T. ) ;
#245366 = EDGE_CURVE ( 'NONE', #254886, #181805, #207148, .T. ) ;
#245367 = CARTESIAN_POINT ( 'NONE',  ( 18.59999999999996945, 7.021664781911246322, -204.8335654018972605 ) ) ;
#245368 = VERTEX_POINT ( 'NONE', #135279 ) ;
#245370 = CARTESIAN_POINT ( 'NONE',  ( -22.41119224318417125, 76.00000000001276135, -215.1726782920691505 ) ) ;
#245369 = DIRECTION ( 'NONE',  ( -1.000000000000000000, 0.000000000000000000, 0.000000000000000000 ) ) ;
#245371 = AXIS2_PLACEMENT_3D ( 'NONE', #224134, #121238, #142032 ) ;
#245372 = EDGE_LOOP ( 'NONE', ( #178203, #245535, #193839, #181657 ) ) ;
#245374 = ORIENTED_EDGE ( 'NONE', *, *, #228633, .T. ) ;
#245373 = CARTESIAN_POINT ( 'NONE',  ( -21.05000000000000071, 1.162701749938009677, -8.099999999999999645 ) ) ;
#245375 = ORIENTED_EDGE ( 'NONE', *, *, #93725, .T. ) ;
#245376 = CARTESIAN_POINT ( 'NONE',  ( 23.04999999999999716, 8.822561741677553471, -54.34999999999999432 ) ) ;
#245377 = EDGE_CURVE ( 'NONE', #232077, #34228, #114337, .T. ) ;
#245378 = DIRECTION ( 'NONE',  ( 1.000000000000000000, 0.000000000000000000, -0.000000000000000000 ) ) ;
#245379 = CARTESIAN_POINT ( 'NONE',  ( 18.49999999999999289, 65.58283456529535727, -78.17310748510507779 ) ) ;
#245380 = DIRECTION ( 'NONE',  ( 0.000000000000000000, 0.9803012954743849372, 0.1975078988072195840 ) ) ;
#245381 = VERTEX_POINT ( 'NONE', #15373 ) ;
#245382 = DIRECTION ( 'NONE',  ( 0.000000000000000000, -6.982962677686266711E-15, 1.000000000000000000 ) ) ;
#245383 = CARTESIAN_POINT ( 'NONE',  ( 20.85000000000000142, 1.115600667400684642E-11, -100.5000000000000426 ) ) ;
#245384 = AXIS2_PLACEMENT_3D ( 'NONE', #143283, #41645, #42910 ) ;
#245385 = ORIENTED_EDGE ( 'NONE', *, *, #244378, .T. ) ;
#245386 = AXIS2_PLACEMENT_3D ( 'NONE', #162998, #205950, #186408 ) ;
#245388 = EDGE_CURVE ( 'NONE', #225332, #199264, #195304, .T. ) ;
#245387 = DIRECTION ( 'NONE',  ( -1.000000000000000000, -2.952720810173289112E-16, 0.000000000000000000 ) ) ;
#245389 = VECTOR ( 'NONE', #40118, 1000.000000000000000 ) ;
#245390 = CARTESIAN_POINT ( 'NONE',  ( 21.05000000000000071, -11.64999999999999147, -30.39999999999999503 ) ) ;
#245391 = VERTEX_POINT ( 'NONE', #54471 ) ;
#245392 = CARTESIAN_POINT ( 'NONE',  ( 21.14999999999998082, 87.75000000001267608, -203.5231074845243029 ) ) ;
#245393 = CIRCLE ( 'NONE', #186961, 3.999999999999994671 ) ;
#245394 = ORIENTED_EDGE ( 'NONE', *, *, #125975, .T. ) ;
#245395 = DIRECTION ( 'NONE',  ( 0.000000000000000000, 0.2128009952263582305, -0.9770955615653319493 ) ) ;
#245396 = ORIENTED_EDGE ( 'NONE', *, *, #196282, .F. ) ;
#245397 = CARTESIAN_POINT ( 'NONE',  ( 18.59999999999999787, 16.44800918141279311, -240.8068063186265135 ) ) ;
#245398 = CARTESIAN_POINT ( 'NONE',  ( 20.99780126800921209, 64.39461131213516865, -76.43575491281889356 ) ) ;
#245399 = CARTESIAN_POINT ( 'NONE',  ( 18.79999999999999716, 7.900000000000000355, -1.300000000000000044 ) ) ;
#245400 = DIRECTION ( 'NONE',  ( -0.000000000000000000, 0.9274965247785350586, 0.3738317757009704811 ) ) ;
#245401 = CIRCLE ( 'NONE', #91284, 0.09999999999998898659 ) ;
#245402 = AXIS2_PLACEMENT_3D ( 'NONE', #224304, #245163, #187767 ) ;
#245403 = B_SPLINE_CURVE_WITH_KNOTS ( 'NONE', 3,
 ( #241777, #141390, #177972, #38445, #60563, #158429, #102228, #237925, #140092, #63128, #220917, #24042, #42302, #43588, #181810, #142659, #222189, #202649, #103537, #183108, #128266, #83941, #25329, #243060, #66998, #163532, #89129, #48709, #69587, #149126 ),
 .UNSPECIFIED., .F., .F.,
 ( 4, 2, 2, 2, 2, 2, 2, 2, 2, 2, 2, 2, 2, 2, 4 ),
 ( 0.000000000000000000, 0.0003422764154113113887, 0.0006845528308226227774, 0.001026829246233934220, 0.001369105661645245555, 0.002053658492467929590, 0.002738211323290614275, 0.003080487738701953148, 0.003422764154113292889, 0.003765040569524632195, 0.004107316984935971069, 0.004449593400347310809, 0.004791869815758650550, 0.005134146231169990290, 0.005476422646581329164 ),
 .UNSPECIFIED. ) ;
#245404 = LINE ( 'NONE', #203702, #94675 ) ;
#245405 = LINE ( 'NONE', #62902, #134833 ) ;
#245407 = LINE ( 'NONE', #242820, #152179 ) ;
#245406 = AXIS2_PLACEMENT_3D ( 'NONE', #244545, #65924, #46339 ) ;
#245408 = ORIENTED_EDGE ( 'NONE', *, *, #214227, .T. ) ;
#245410 = CARTESIAN_POINT ( 'NONE',  ( 18.59999999999999787, -11.74999999998883737, -121.8500000000000369 ) ) ;
#245409 = DIRECTION ( 'NONE',  ( -0.000000000000000000, -6.982962677686266711E-15, 1.000000000000000000 ) ) ;
#245411 = EDGE_CURVE ( 'NONE', #201638, #226285, #143577, .T. ) ;
#245412 = ORIENTED_EDGE ( 'NONE', *, *, #203376, .T. ) ;
#245413 = EDGE_CURVE ( 'NONE', #208807, #147103, #152940, .T. ) ;
#245414 = CARTESIAN_POINT ( 'NONE',  ( -18.50000000000000000, 66.75000000001199396, -115.1731074845243654 ) ) ;
#245415 = CARTESIAN_POINT ( 'NONE',  ( -16.86445178670658507, 12.41728787639459775, -211.2004468506748083 ) ) ;
#245416 = DIRECTION ( 'NONE',  ( 1.000000000000000000, -0.000000000000000000, -0.000000000000000000 ) ) ;
#245418 = VERTEX_POINT ( 'NONE', #136564 ) ;
#245417 = CARTESIAN_POINT ( 'NONE',  ( -18.36527282682029494, -9.500000599982218574, -207.9221489645163388 ) ) ;
#245420 = VERTEX_POINT ( 'NONE', #58305 ) ;
#245419 = LINE ( 'NONE', #87595, #132991 ) ;
#245422 = ADVANCED_FACE ( 'NONE', ( #98694 ), #217383, .F. ) ;
#245421 = PLANE ( 'NONE',  #114464 ) ;
#245424 = EDGE_CURVE ( 'NONE', #146218, #95294, #251116, .T. ) ;
#245423 = DIRECTION ( 'NONE',  ( 9.044546369203337730E-15, 0.7397360091702647189, 0.6728971962616949742 ) ) ;
#245425 = PLANE ( 'NONE',  #151122 ) ;
#245427 = VERTEX_POINT ( 'NONE', #34954 ) ;
#245426 = CYLINDRICAL_SURFACE ( 'NONE', #94662, 7.899999999999990585 ) ;
#245428 = EDGE_CURVE ( 'NONE', #101037, #124696, #196547, .T. ) ;
#245429 = CIRCLE ( 'NONE', #203727, 0.09999999999999939493 ) ;
#245430 = EDGE_CURVE ( 'NONE', #184336, #39426, #226764, .T. ) ;
#245431 = ADVANCED_FACE ( 'NONE', ( #17906 ), #14087, .F. ) ;
#245432 = CARTESIAN_POINT ( 'NONE',  ( 22.59999985501178799, 11.74986979301414003, -167.4344013302003873 ) ) ;
#245433 = DIRECTION ( 'NONE',  ( 0.000000000000000000, -1.000000000000000000, -2.891205793294679805E-16 ) ) ;
#245434 = ORIENTED_EDGE ( 'NONE', *, *, #237688, .T. ) ;
#245435 = CARTESIAN_POINT ( 'NONE',  ( -17.78043020864320667, 53.36034707231080887, -230.1761842539149256 ) ) ;
#245436 = EDGE_LOOP ( 'NONE', ( #116903, #83908, #27994, #201446 ) ) ;
#245437 = EDGE_CURVE ( 'NONE', #65298, #175048, #57013, .T. ) ;
#245438 = CARTESIAN_POINT ( 'NONE',  ( -18.50000000000000000, 85.40000000001138858, -29.14106563635158764 ) ) ;
#245439 = CARTESIAN_POINT ( 'NONE',  ( 19.80993210785516112, 34.50919645272388436, -235.0699886441803130 ) ) ;
#245440 = VERTEX_POINT ( 'NONE', #97419 ) ;
#245441 = DIRECTION ( 'NONE',  ( 1.000000000000000000, 0.000000000000000000, 0.000000000000000000 ) ) ;
#245442 = EDGE_CURVE ( 'NONE', #193307, #180781, #77877, .T. ) ;
#245443 = CARTESIAN_POINT ( 'NONE',  ( 18.59999999999999076, 19.81721122307411420, -227.1998943584050039 ) ) ;
#245444 = AXIS2_PLACEMENT_3D ( 'NONE', #202986, #144270, #63468 ) ;
#245445 = VECTOR ( 'NONE', #223066, 1000.000000000000000 ) ;
#245446 = ORIENTED_EDGE ( 'NONE', *, *, #68219, .F. ) ;
#245447 = EDGE_CURVE ( 'NONE', #123284, #169627, #247618, .T. ) ;
#245448 = VECTOR ( 'NONE', #133710, 1000.000000000000000 ) ;
#245449 = AXIS2_PLACEMENT_3D ( 'NONE', #84831, #200964, #5297 ) ;
#245450 = CARTESIAN_POINT ( 'NONE',  ( -16.89146115310546037, 66.04855675435506157, -48.66828506557018130 ) ) ;
#245451 = ADVANCED_FACE ( 'NONE', ( #137845 ), #185265, .T. ) ;
#245452 = EDGE_LOOP ( 'NONE', ( #193964, #248258, #234482, #210997 ) ) ;
#245453 = AXIS2_PLACEMENT_3D ( 'NONE', #116059, #74387, #16959 ) ;
#245454 = VERTEX_POINT ( 'NONE', #252663 ) ;
#245455 = DIRECTION ( 'NONE',  ( 0.000000000000000000, -0.8814952561688430555, 0.4721928772777346239 ) ) ;
#245456 = ORIENTED_EDGE ( 'NONE', *, *, #242456, .F. ) ;
#245457 = CARTESIAN_POINT ( 'NONE',  ( 18.39999999999998082, 11.47316190337362585, -176.7499999999999716 ) ) ;
#245458 = ORIENTED_EDGE ( 'NONE', *, *, #248808, .T. ) ;
#245460 = ORIENTED_EDGE ( 'NONE', *, *, #146778, .T. ) ;
#245459 = CARTESIAN_POINT ( 'NONE',  ( -21.05000000000000071, -10.56629024491939894, -206.4738935375009703 ) ) ;
#245461 = EDGE_CURVE ( 'NONE', #28556, #82836, #197829, .T. ) ;
#245462 = EDGE_CURVE ( 'NONE', #244782, #142484, #138851, .T. ) ;
#245463 = DIRECTION ( 'NONE',  ( 0.000000000000000000, 0.000000000000000000, 1.000000000000000000 ) ) ;
#245464 = ORIENTED_EDGE ( 'NONE', *, *, #78286, .F. ) ;
#245465 = DIRECTION ( 'NONE',  ( 0.000000000000000000, -1.000000000000000000, 0.000000000000000000 ) ) ;
#245466 = AXIS2_PLACEMENT_3D ( 'NONE', #153487, #196402, #17751 ) ;
#245467 = AXIS2_PLACEMENT_3D ( 'NONE', #166733, #128869, #143276 ) ;
#245468 = VERTEX_POINT ( 'NONE', #34251 ) ;
#245470 = ORIENTED_EDGE ( 'NONE', *, *, #13267, .T. ) ;
#245469 = ORIENTED_EDGE ( 'NONE', *, *, #79109, .T. ) ;
#245472 = CYLINDRICAL_SURFACE ( 'NONE', #57177, 0.09999999999999939493 ) ;
#245471 = CIRCLE ( 'NONE', #87217, 0.09999999999999939493 ) ;
#245473 = LINE ( 'NONE', #242884, #27497 ) ;
#245474 = ORIENTED_EDGE ( 'NONE', *, *, #197607, .T. ) ;
#245475 = B_SPLINE_CURVE_WITH_KNOTS ( 'NONE', 3,
 ( #182347, #242294, #104050, #80639, #143190, #63660, #44108, #40293, #123653, #68484 ),
 .UNSPECIFIED., .F., .F.,
 ( 4, 3, 3, 4 ),
 ( 1.961400829040844664E-15, 8.145022132830484647E-06, 1.905645951092394214E-05, 2.061107371225745169E-05 ),
 .UNSPECIFIED. ) ;
#245476 = AXIS2_PLACEMENT_3D ( 'NONE', #237543, #172477, #133307 ) ;
#245477 = VERTEX_POINT ( 'NONE', #115039 ) ;
#245478 = CARTESIAN_POINT ( 'NONE',  ( 18.59999999999999076, 30.76917518201224055, -234.8152055956155380 ) ) ;
#245479 = FACE_OUTER_BOUND ( 'NONE', #211692, .T. ) ;
#245480 = ORIENTED_EDGE ( 'NONE', *, *, #161241, .T. ) ;
#245481 = CARTESIAN_POINT ( 'NONE',  ( -20.94999999999999929, 67.46931694187804851, -235.9558427390807083 ) ) ;
#245482 = ORIENTED_EDGE ( 'NONE', *, *, #16207, .T. ) ;
#245483 = CYLINDRICAL_SURFACE ( 'NONE', #103589, 0.09999999999999961697 ) ;
#245484 = DIRECTION ( 'NONE',  ( 3.265361837132813093E-16, -1.000000000000000000, -0.000000000000000000 ) ) ;
#245485 = EDGE_LOOP ( 'NONE', ( #78960, #61837 ) ) ;
#245486 = CARTESIAN_POINT ( 'NONE',  ( 18.44364597020195973, 85.49048731717387284, -62.46512959484039840 ) ) ;
#245487 = DIRECTION ( 'NONE',  ( 0.000000000000000000, 0.5283051335750404975, -0.8490545835446967615 ) ) ;
#245488 = EDGE_LOOP ( 'NONE', ( #100866, #83570, #38439, #156179, #18382, #79314, #167934, #150894, #172358, #7680, #62715, #212992, #185769, #108288 ) ) ;
#245489 = CARTESIAN_POINT ( 'NONE',  ( 23.15000000000000213, -9.599999999988845900, -110.3939691226524786 ) ) ;
#245490 = ORIENTED_EDGE ( 'NONE', *, *, #107725, .T. ) ;
#245491 = CIRCLE ( 'NONE', #149826, 2.099999999999998757 ) ;
#245493 = ORIENTED_EDGE ( 'NONE', *, *, #126176, .F. ) ;
#245492 = ORIENTED_EDGE ( 'NONE', *, *, #33768, .T. ) ;
#245494 = EDGE_LOOP ( 'NONE', ( #87514, #204078, #41424, #246444, #183246 ) ) ;
#245495 = DIRECTION ( 'NONE',  ( 1.476360405086644309E-16, -1.000000000000000000, 0.000000000000000000 ) ) ;
#245496 = ORIENTED_EDGE ( 'NONE', *, *, #214430, .F. ) ;
#245497 = AXIS2_PLACEMENT_3D ( 'NONE', #125295, #24927, #43190 ) ;
#245498 = ORIENTED_EDGE ( 'NONE', *, *, #240337, .T. ) ;
#245499 = CARTESIAN_POINT ( 'NONE',  ( -18.40000000000000213, 59.44312576075365229, -220.7395490299249445 ) ) ;
#245500 = DIRECTION ( 'NONE',  ( 1.000000000000000000, 0.000000000000000000, 0.000000000000000000 ) ) ;
#245501 = EDGE_LOOP ( 'NONE', ( #321, #126060, #105600, #164573, #126398, #155953, #10889 ) ) ;
#245502 = EDGE_CURVE ( 'NONE', #225759, #104197, #217980, .T. ) ;
#245503 = ORIENTED_EDGE ( 'NONE', *, *, #18236, .F. ) ;
#245504 = EDGE_CURVE ( 'NONE', #147015, #157637, #197149, .T. ) ;
#245506 = ORIENTED_EDGE ( 'NONE', *, *, #146673, .F. ) ;
#245505 = CIRCLE ( 'NONE', #224635, 0.2000000000000057288 ) ;
#245507 = AXIS2_PLACEMENT_3D ( 'NONE', #133114, #130532, #171003 ) ;
#245508 = EDGE_CURVE ( 'NONE', #69713, #75413, #73376, .T. ) ;
#245509 = DIRECTION ( 'NONE',  ( 0.000000000000000000, -1.000000000000000000, 0.000000000000000000 ) ) ;
#245510 = EDGE_CURVE ( 'NONE', #239049, #140362, #105547, .T. ) ;
#245511 = EDGE_LOOP ( 'NONE', ( #242502, #123394, #252816, #204535, #84738 ) ) ;
#245512 = SPHERICAL_SURFACE ( 'NONE', #195891, 0.1000000000000000056 ) ;
#245514 = ORIENTED_EDGE ( 'NONE', *, *, #21398, .T. ) ;
#245513 = CARTESIAN_POINT ( 'NONE',  ( 21.05000000000000071, 5.850000000011105428, -177.6324972242779268 ) ) ;
#245515 = FACE_OUTER_BOUND ( 'NONE', #10982, .T. ) ;
#245516 = DIRECTION ( 'NONE',  ( 1.000000000000000000, 0.000000000000000000, 0.000000000000000000 ) ) ;
#245517 = CIRCLE ( 'NONE', #220572, 2.000000000000001776 ) ;
#245519 = VECTOR ( 'NONE', #187301, 1000.000000000000000 ) ;
#245518 = DIRECTION ( 'NONE',  ( -3.265361837132813093E-16, 1.000000000000000000, 0.000000000000000000 ) ) ;
#245520 = FACE_OUTER_BOUND ( 'NONE', #209875, .T. ) ;
#245521 = CARTESIAN_POINT ( 'NONE',  ( -23.25000000000000000, 71.85000000001254250, -182.2731074845243882 ) ) ;
#245523 = DIRECTION ( 'NONE',  ( 0.000000000000000000, -0.1298341882520022694, -0.9915357197604853789 ) ) ;
#245522 = DIRECTION ( 'NONE',  ( 0.000000000000000000, 0.2617529984165152257, 0.9651348961777124202 ) ) ;
#245524 = PLANE ( 'NONE',  #153104 ) ;
#245525 = DIRECTION ( 'NONE',  ( -1.000000000000000000, 2.849773892568378313E-16, -7.728835255496647986E-17 ) ) ;
#245526 = CARTESIAN_POINT ( 'NONE',  ( 5.899999999999995914, -11.65000000000000036, 10.10000000000000142 ) ) ;
#245527 = DIRECTION ( 'NONE',  ( -3.265361837132813093E-16, -1.000000000000000000, -7.086529944415894657E-15 ) ) ;
#245528 = ORIENTED_EDGE ( 'NONE', *, *, #250446, .T. ) ;
#245529 = TOROIDAL_SURFACE ( 'NONE', #153992, 1.900000000000002576, 0.1000000000000000056 ) ;
#245531 = ADVANCED_FACE ( 'NONE', ( #55039 ), #94176, .F. ) ;
#245530 = CIRCLE ( 'NONE', #170565, 0.09999999999999868716 ) ;
#245532 = CIRCLE ( 'NONE', #203999, 0.09999999999998898659 ) ;
#245534 = ORIENTED_EDGE ( 'NONE', *, *, #100, .T. ) ;
#245533 = DIRECTION ( 'NONE',  ( 1.000000000000000000, -0.000000000000000000, 0.000000000000000000 ) ) ;
#245535 = ORIENTED_EDGE ( 'NONE', *, *, #22685, .T. ) ;
#245536 = CIRCLE ( 'NONE', #129021, 0.1000000000000011990 ) ;
#245537 = CARTESIAN_POINT ( 'NONE',  ( 23.14999999999999858, 48.40874555430184500, -244.2873875965402704 ) ) ;
#245538 = CARTESIAN_POINT ( 'NONE',  ( -23.15000000000000213, 48.91146289617405785, -253.9240286733484595 ) ) ;
#245539 = CARTESIAN_POINT ( 'NONE',  ( 20.77766267348356166, 39.31613315723080149, -236.9111090107639939 ) ) ;
#245540 = ORIENTED_EDGE ( 'NONE', *, *, #185994, .F. ) ;
#245541 = SURFACE_STYLE_FILL_AREA ( #89008 ) ;
#245542 = ADVANCED_FACE ( 'NONE', ( #175065 ), #251313, .F. ) ;
#245543 = DIRECTION ( 'NONE',  ( -0.7071067811865388020, 0.7071067811865561215, 0.000000000000000000 ) ) ;
#245544 = EDGE_CURVE ( 'NONE', #235470, #108747, #151396, .T. ) ;
#245545 = DIRECTION ( 'NONE',  ( 0.000000000000000000, 0.000000000000000000, -1.000000000000000000 ) ) ;
#245546 = CIRCLE ( 'NONE', #70605, 11.64999999999999325 ) ;
#245547 = VERTEX_POINT ( 'NONE', #234996 ) ;
#245548 = CARTESIAN_POINT ( 'NONE',  ( 20.94999999999999574, 87.65000000001265335, -200.4231074845242802 ) ) ;
#245549 = DIRECTION ( 'NONE',  ( -1.000000000000000000, -3.265361837132813093E-16, 0.000000000000000000 ) ) ;
#245550 = FACE_OUTER_BOUND ( 'NONE', #101565, .T. ) ;
#245551 = DIRECTION ( 'NONE',  ( 0.000000000000000000, 0.000000000000000000, 1.000000000000000000 ) ) ;
#245553 = ORIENTED_EDGE ( 'NONE', *, *, #202811, .T. ) ;
#245552 = CARTESIAN_POINT ( 'NONE',  ( -20.85000000000000142, 1.115600667400684642E-11, -108.4000000000000483 ) ) ;
#245554 = CARTESIAN_POINT ( 'NONE',  ( -18.59999999999999787, 36.65892442174935439, -249.5511627012433848 ) ) ;
#245555 = EDGE_CURVE ( 'NONE', #195393, #220389, #218542, .T. ) ;
#245556 = CARTESIAN_POINT ( 'NONE',  ( -21.14999999999999858, 11.40444339177023814, -198.6185779617709670 ) ) ;
#245557 = CARTESIAN_POINT ( 'NONE',  ( -21.05000000000000071, 76.00000000001242029, -165.9231074845243654 ) ) ;
#245558 = CARTESIAN_POINT ( 'NONE',  ( 18.39999999999999858, 85.50000000001189449, -95.99103808782457747 ) ) ;
#245559 = ORIENTED_EDGE ( 'NONE', *, *, #189871, .F. ) ;
#245560 = DIRECTION ( 'NONE',  ( 1.000000000000000000, -3.265361837132813093E-16, -2.280189983783949500E-30 ) ) ;
#245561 = EDGE_CURVE ( 'NONE', #253135, #196436, #68166, .T. ) ;
#245562 = VECTOR ( 'NONE', #223900, 1000.000000000000000 ) ;
#245564 = CARTESIAN_POINT ( 'NONE',  ( -21.05000000000000071, 1.162701749949165642, -108.4000000000000341 ) ) ;
#245563 = DIRECTION ( 'NONE',  ( 0.000000000000000000, -0.9126074666063770380, -0.4088369013363281068 ) ) ;
#245565 = AXIS2_PLACEMENT_3D ( 'NONE', #172914, #39500, #73796 ) ;
#245566 = DIRECTION ( 'NONE',  ( 7.304098846218134667E-16, 1.000000000000000000, 6.982962677686266711E-15 ) ) ;
#245568 = EDGE_CURVE ( 'NONE', #670, #81505, #221132, .T. ) ;
#245567 = CARTESIAN_POINT ( 'NONE',  ( -18.51024323315077424, 10.31104185822947095, -39.02045169831058047 ) ) ;
#245569 = DIRECTION ( 'NONE',  ( -1.000000000000000000, -0.000000000000000000, -0.000000000000000000 ) ) ;
#245570 = LINE ( 'NONE', #225956, #121488 ) ;
#245571 = DIRECTION ( 'NONE',  ( 1.000000000000000000, 0.000000000000000000, 0.000000000000000000 ) ) ;
#245573 = VERTEX_POINT ( 'NONE', #77186 ) ;
#245572 = CIRCLE ( 'NONE', #233121, 0.1000000000000028644 ) ;
#245574 = EDGE_LOOP ( 'NONE', ( #246007, #217273, #153512, #131942 ) ) ;
#245575 = ORIENTED_EDGE ( 'NONE', *, *, #135944, .F. ) ;
#245576 = DIRECTION ( 'NONE',  ( -0.000000000000000000, 6.982962677686266711E-15, -1.000000000000000000 ) ) ;
#245577 = CARTESIAN_POINT ( 'NONE',  ( 18.59999999999999432, 77.16270174995010223, -128.4231074845242802 ) ) ;
#245578 = ORIENTED_EDGE ( 'NONE', *, *, #84668, .F. ) ;
#245579 = EDGE_CURVE ( 'NONE', #240031, #18265, #230382, .T. ) ;
#245580 = ORIENTED_EDGE ( 'NONE', *, *, #111898, .F. ) ;
#245581 = EDGE_CURVE ( 'NONE', #127799, #214167, #139453, .T. ) ;
#245582 = AXIS2_PLACEMENT_3D ( 'NONE', #32568, #195483, #15560 ) ;
#245583 = SURFACE_SIDE_STYLE ('',( #239156 ) ) ;
#245584 = ORIENTED_EDGE ( 'NONE', *, *, #244403, .T. ) ;
#245585 = CARTESIAN_POINT ( 'NONE',  ( -20.07928932188135107, 66.77928932189284694, -48.37310748452438247 ) ) ;
#245586 = EDGE_LOOP ( 'NONE', ( #257472, #17125, #24239, #56610 ) ) ;
#245587 = CARTESIAN_POINT ( 'NONE',  ( -20.54999999999999716, 1.925233644859816629, -12.73024353312613144 ) ) ;
#245588 = CARTESIAN_POINT ( 'NONE',  ( 20.94999999999999574, 1.849084418627015891, -11.65601052144712391 ) ) ;
#245589 = CARTESIAN_POINT ( 'NONE',  ( -16.93589915522259304, 30.31383928998786814, -234.7981289524791748 ) ) ;
#245590 = CARTESIAN_POINT ( 'NONE',  ( 20.85000000000000142, 76.00000000001190870, -103.0231074845243029 ) ) ;
#245591 = CARTESIAN_POINT ( 'NONE',  ( -21.08035267497491816, 1.586508777023655892, -230.6700248112038310 ) ) ;
#245592 = CARTESIAN_POINT ( 'NONE',  ( -16.86133551771148831, 30.16343802849835143, -234.7840697211602503 ) ) ;
#245594 = VERTEX_POINT ( 'NONE', #35539 ) ;
#245593 = DIRECTION ( 'NONE',  ( 0.000000000000000000, 0.9126074666063660468, 0.4088369013363524762 ) ) ;
#245596 = DIRECTION ( 'NONE',  ( -1.000000000000000000, -0.000000000000000000, 0.000000000000000000 ) ) ;
#245595 = CARTESIAN_POINT ( 'NONE',  ( 21.04386569057580658, 11.74999999999974598, -26.64283735177988177 ) ) ;
#245597 = CARTESIAN_POINT ( 'NONE',  ( 23.25000000000000000, -13.98128454229088291, -192.0195388455185821 ) ) ;
#245598 = EDGE_LOOP ( 'NONE', ( #154420, #38870, #139421, #176177, #180923 ) ) ;
#245599 = DIRECTION ( 'NONE',  ( -1.000000000000000000, -0.000000000000000000, 0.000000000000000000 ) ) ;
#245600 = CARTESIAN_POINT ( 'NONE',  ( 20.94999999999999929, -8.730841121495327428, -9.598074718984332065 ) ) ;
#245601 = CARTESIAN_POINT ( 'NONE',  ( -22.59999999999999787, 0.1000000000111554016, -21.85042919245520210 ) ) ;
#245602 = ORIENTED_EDGE ( 'NONE', *, *, #225083, .F. ) ;
#245603 = FACE_OUTER_BOUND ( 'NONE', #100123, .T. ) ;
#245604 = B_SPLINE_CURVE_WITH_KNOTS ( 'NONE', 3,
 ( #243135, #84010, #226115, #106175, #63198, #86607 ),
 .UNSPECIFIED., .F., .F.,
 ( 4, 2, 4 ),
 ( 0.000000000000000000, 0.0001497467027049297528, 0.0002994934054098595056 ),
 .UNSPECIFIED. ) ;
#245605 = AXIS2_PLACEMENT_3D ( 'NONE', #163300, #15119, #35972 ) ;
#245606 = VECTOR ( 'NONE', #227112, 1000.000000000000000 ) ;
#245607 = LINE ( 'NONE', #66960, #181453 ) ;
#245608 = VERTEX_POINT ( 'NONE', #74671 ) ;
#245609 = LINE ( 'NONE', #207786, #242868 ) ;
#245610 = DIRECTION ( 'NONE',  ( 0.000000000000000000, -0.2617529984165152257, -0.9651348961777124202 ) ) ;
#245611 = DIRECTION ( 'NONE',  ( 0.000000000000000000, 0.000000000000000000, -1.000000000000000000 ) ) ;
#245612 = CARTESIAN_POINT ( 'NONE',  ( 23.14999999999999858, 1.115600667400684642E-11, -167.5000000000000284 ) ) ;
#245613 = ORIENTED_EDGE ( 'NONE', *, *, #234755, .T. ) ;
#245614 = ORIENTED_EDGE ( 'NONE', *, *, #166911, .T. ) ;
#245615 = LINE ( 'NONE', #66971, #135876 ) ;
#245616 = PLANE ( 'NONE',  #6615 ) ;
#245617 = AXIS2_PLACEMENT_3D ( 'NONE', #205539, #28240, #8644 ) ;
#245618 = DIRECTION ( 'NONE',  ( -1.000000000000000000, -0.000000000000000000, -0.000000000000000000 ) ) ;
#245620 = CARTESIAN_POINT ( 'NONE',  ( -21.05000000000000071, 1.115600667400684642E-11, -67.00000000000004263 ) ) ;
#245619 = AXIS2_PLACEMENT_3D ( 'NONE', #136140, #177885, #54062 ) ;
#245621 = ADVANCED_FACE ( 'NONE', ( #156762 ), #52474, .T. ) ;
#245622 = CARTESIAN_POINT ( 'NONE',  ( 21.05000000000000071, 70.60000000001221565, -146.4170766071768526 ) ) ;
#245623 = DIRECTION ( 'NONE',  ( 7.304098846218134667E-16, -1.000000000000000000, 0.000000000000000000 ) ) ;
#245624 = VERTEX_POINT ( 'NONE', #133323 ) ;
#245625 = CARTESIAN_POINT ( 'NONE',  ( -20.89878130938411616, 65.67252876774529113, -97.44570419949944551 ) ) ;
#245627 = VERTEX_POINT ( 'NONE', #154215 ) ;
#245626 = CARTESIAN_POINT ( 'NONE',  ( -23.49999999999994316, 82.74366731733570646, -26.36310895752070138 ) ) ;
#245628 = LINE ( 'NONE', #146501, #130982 ) ;
#245629 = DIRECTION ( 'NONE',  ( 0.7071359030027766224, -0.7070776581709024011, 0.000000000000000000 ) ) ;
#245630 = CARTESIAN_POINT ( 'NONE',  ( -21.08198257630413508, 75.92735667622712015, -75.85970421853939172 ) ) ;
#245631 = CARTESIAN_POINT ( 'NONE',  ( -16.87401514999235275, 66.05000000001207638, -123.8031254770561844 ) ) ;
#245632 = ADVANCED_FACE ( 'NONE', ( #233717 ), #59758, .F. ) ;
#245633 = ORIENTED_EDGE ( 'NONE', *, *, #247269, .F. ) ;
#245634 = PLANE ( 'NONE',  #221378 ) ;
#245635 = DIRECTION ( 'NONE',  ( 1.000000000000000000, 0.000000000000000000, 0.000000000000000000 ) ) ;
#245636 = CARTESIAN_POINT ( 'NONE',  ( -17.01764560440378204, 63.05955705343778561, -213.2241350757899454 ) ) ;
#245637 = CARTESIAN_POINT ( 'NONE',  ( -20.94999999999999929, 75.74389420792046224, -203.5580039261966760 ) ) ;
#245638 = EDGE_LOOP ( 'NONE', ( #238165, #189814, #37706, #257008 ) ) ;
#245639 = CARTESIAN_POINT ( 'NONE',  ( 18.51997666896887651, -7.657082092440962384, -209.9784881053329855 ) ) ;
#245640 = DIRECTION ( 'NONE',  ( 0.000000000000000000, -0.4721928772777346239, -0.8814952561688430555 ) ) ;
#245641 = EDGE_CURVE ( 'NONE', #204996, #40541, #217963, .T. ) ;
#245643 = EDGE_CURVE ( 'NONE', #73708, #83068, #220562, .T. ) ;
#245642 = CIRCLE ( 'NONE', #162269, 11.64999999999999325 ) ;
#245644 = PLANE ( 'NONE',  #50345 ) ;
#245645 = AXIS2_PLACEMENT_3D ( 'NONE', #165570, #245091, #69043 ) ;
#245646 = CARTESIAN_POINT ( 'NONE',  ( 21.05000000000000071, -11.48912529306489994, -64.10000000000000853 ) ) ;
#245647 = EDGE_LOOP ( 'NONE', ( #181397, #121857, #233019, #118854 ) ) ;
#245648 = DIRECTION ( 'NONE',  ( 1.000000000000000000, 2.952720810173289112E-16, -0.000000000000000000 ) ) ;
#245649 = CIRCLE ( 'NONE', #45731, 2.000000000000001776 ) ;
#245650 = ORIENTED_EDGE ( 'NONE', *, *, #110029, .F. ) ;
#245651 = CARTESIAN_POINT ( 'NONE',  ( 13.99999999999999822, 47.91805600923871822, -233.7139610577891631 ) ) ;
#245652 = DIRECTION ( 'NONE',  ( 0.000000000000000000, 0.000000000000000000, -1.000000000000000000 ) ) ;
#245653 = EDGE_CURVE ( 'NONE', #77835, #96815, #106123, .T. ) ;
#245654 = DIRECTION ( 'NONE',  ( -1.000000000000000000, 0.000000000000000000, 0.000000000000000000 ) ) ;
#245655 = CARTESIAN_POINT ( 'NONE',  ( -20.54999999999999716, 4.350000000011156054, -45.85000000000000142 ) ) ;
#245656 = ORIENTED_EDGE ( 'NONE', *, *, #190127, .T. ) ;
#245657 = CARTESIAN_POINT ( 'NONE',  ( -23.15000000000000213, 76.00000000001216449, -140.4231074845243370 ) ) ;
#245658 = DIRECTION ( 'NONE',  ( 0.000000000000000000, 0.000000000000000000, 1.000000000000000000 ) ) ;
#245659 = CARTESIAN_POINT ( 'NONE',  ( -21.07928932188134041, 6.328516656404449492, -66.90110485434564680 ) ) ;
#245661 = CARTESIAN_POINT ( 'NONE',  ( -16.79270642812308978, 9.946244216938064042, -20.83893327856252142 ) ) ;
#245660 = CIRCLE ( 'NONE', #62510, 0.1000000000000124678 ) ;
#245662 = DIRECTION ( 'NONE',  ( -1.000000000000000000, 0.000000000000000000, -0.000000000000000000 ) ) ;
#245663 = ORIENTED_EDGE ( 'NONE', *, *, #21103, .F. ) ;
#245665 = ORIENTED_EDGE ( 'NONE', *, *, #243537, .F. ) ;
#245664 = CARTESIAN_POINT ( 'NONE',  ( -20.94999999999999929, 76.00000000001159606, -61.62310748452431852 ) ) ;
#245666 = ORIENTED_EDGE ( 'NONE', *, *, #39354, .T. ) ;
#245667 = CARTESIAN_POINT ( 'NONE',  ( 20.94999999999999929, 5.900000000011162093, -90.28090023534366537 ) ) ;
#245668 = ORIENTED_EDGE ( 'NONE', *, *, #70900, .F. ) ;
#245669 = EDGE_CURVE ( 'NONE', #22565, #43985, #151968, .T. ) ;
#245670 = CARTESIAN_POINT ( 'NONE',  ( 21.08750232978087524, 65.27513661400190870, -124.2942493115248084 ) ) ;
#245671 = DIRECTION ( 'NONE',  ( 0.000000000000000000, 1.000000000000000000, 6.982962677686266711E-15 ) ) ;
#245672 = ADVANCED_FACE ( 'NONE', ( #122766 ), #93098, .T. ) ;
#245673 = LINE ( 'NONE', #166171, #20591 ) ;
#245674 = AXIS2_PLACEMENT_3D ( 'NONE', #110859, #167021, #13070 ) ;
#245675 = EDGE_LOOP ( 'NONE', ( #91704, #72043, #47639, #148614 ) ) ;
#245676 = CARTESIAN_POINT ( 'NONE',  ( -16.92778301347306424, 65.99905508317604585, -56.95162559249263268 ) ) ;
#245677 = DIRECTION ( 'NONE',  ( 0.000000000000000000, 0.000000000000000000, -1.000000000000000000 ) ) ;
#245678 = CARTESIAN_POINT ( 'NONE',  ( 20.52683494730037239, 8.980530818312608687, -42.00525272253644715 ) ) ;
#245679 = ORIENTED_EDGE ( 'NONE', *, *, #79135, .T. ) ;
#245680 = DIRECTION ( 'NONE',  ( 0.000000000000000000, 0.000000000000000000, 1.000000000000000000 ) ) ;
#245682 = ORIENTED_EDGE ( 'NONE', *, *, #151848, .F. ) ;
#245681 = DIRECTION ( 'NONE',  ( -0.5932847527679298016, -0.8049926720990051576, -5.621233785078291429E-15 ) ) ;
#245683 = DIRECTION ( 'NONE',  ( 1.000000000000000000, 1.794895427898103559E-16, 3.909090864890002444E-17 ) ) ;
#245685 = EDGE_CURVE ( 'NONE', #103023, #183689, #230485, .T. ) ;
#245684 = DIRECTION ( 'NONE',  ( 0.000000000000000000, 0.000000000000000000, -1.000000000000000000 ) ) ;
#245686 = TOROIDAL_SURFACE ( 'NONE', #4233, 0.4000000000000015210, 0.1000000000000000056 ) ;
#245687 = AXIS2_PLACEMENT_3D ( 'NONE', #157851, #58678, #198209 ) ;
#245688 = ORIENTED_EDGE ( 'NONE', *, *, #45890, .F. ) ;
#245689 = CARTESIAN_POINT ( 'NONE',  ( 18.49999999999999289, 63.77010848770628826, -209.1687319955904911 ) ) ;
#245690 = CARTESIAN_POINT ( 'NONE',  ( -14.11697426661281618, 66.54258905524464751, -121.5230235107343759 ) ) ;
#245691 = DIRECTION ( 'NONE',  ( 0.000000000000000000, 1.000000000000000000, 0.000000000000000000 ) ) ;
#245692 = VERTEX_POINT ( 'NONE', #100574 ) ;
#245693 = DIRECTION ( 'NONE',  ( -1.000000000000000000, -2.952720810173289112E-16, 0.000000000000000000 ) ) ;
#245694 = AXIS2_PLACEMENT_3D ( 'NONE', #97047, #218299, #176653 ) ;
#245695 = FACE_OUTER_BOUND ( 'NONE', #116039, .T. ) ;
#245696 = AXIS2_PLACEMENT_3D ( 'NONE', #70598, #247909, #147535 ) ;
#245697 = ORIENTED_EDGE ( 'NONE', *, *, #176193, .T. ) ;
#245698 = AXIS2_PLACEMENT_3D ( 'NONE', #146463, #190781, #12138 ) ;
#245699 = AXIS2_PLACEMENT_3D ( 'NONE', #167453, #54835, #245680 ) ;
#245700 = VECTOR ( 'NONE', #11812, 1000.000000000000114 ) ;
#245701 = ORIENTED_EDGE ( 'NONE', *, *, #120753, .F. ) ;
#245703 = FACE_BOUND ( 'NONE', #20044, .T. ) ;
#245702 = CIRCLE ( 'NONE', #129015, 0.09999999999999520384 ) ;
#245704 = CIRCLE ( 'NONE', #133283, 0.09999999999998898659 ) ;
#245705 = ADVANCED_FACE ( 'NONE', ( #216 ), #238840, .F. ) ;
#245706 = EDGE_CURVE ( 'NONE', #46773, #15410, #103159, .T. ) ;
#245707 = ORIENTED_EDGE ( 'NONE', *, *, #157249, .F. ) ;
#245708 = DIRECTION ( 'NONE',  ( -1.000000000000000000, 0.000000000000000000, 0.000000000000000000 ) ) ;
#245709 = DIRECTION ( 'NONE',  ( 0.000000000000000000, -1.000000000000000000, 0.000000000000000000 ) ) ;
#245711 = VERTEX_POINT ( 'NONE', #163170 ) ;
#245710 = CARTESIAN_POINT ( 'NONE',  ( -21.05000000000000071, -9.519327731081284938, -140.9729763765593589 ) ) ;
#245712 = CARTESIAN_POINT ( 'NONE',  ( -20.54999999999999716, 74.00000000001156764, -56.79848556176223440 ) ) ;
#245713 = LINE ( 'NONE', #85320, #40695 ) ;
#245715 = ADVANCED_FACE ( 'NONE', ( #58889 ), #27068, .F. ) ;
#245714 = CARTESIAN_POINT ( 'NONE',  ( -20.64999999999999858, -8.999999999988844479, -124.6060308773475924 ) ) ;
#245717 = EDGE_CURVE ( 'NONE', #50955, #91552, #221814, .T. ) ;
#245716 = LINE ( 'NONE', #205283, #187991 ) ;
#245718 = DIRECTION ( 'NONE',  ( -1.020425574104004196E-15, 0.000000000000000000, 1.000000000000000000 ) ) ;
#245719 = CARTESIAN_POINT ( 'NONE',  ( 18.52928932188133970, 10.27928932189250411, -125.2500000000000284 ) ) ;
#245720 = CARTESIAN_POINT ( 'NONE',  ( -16.87242674293850797, 9.950000000011138823, -79.64890975362770575 ) ) ;
#245721 = DIRECTION ( 'NONE',  ( 0.000000000000000000, -0.8700118002898357128, 0.4930308989875171188 ) ) ;
#245723 = ORIENTED_EDGE ( 'NONE', *, *, #206507, .T. ) ;
#245722 = DIRECTION ( 'NONE',  ( 1.000000000000000000, 0.000000000000000000, 0.000000000000000000 ) ) ;
#245724 = PLANE ( 'NONE',  #29213 ) ;
#245726 = EDGE_LOOP ( 'NONE', ( #192332, #224136, #13602, #204244, #236694 ) ) ;
#245725 = EDGE_CURVE ( 'NONE', #17057, #241011, #181451, .T. ) ;
#245727 = EDGE_CURVE ( 'NONE', #5207, #3259, #241417, .T. ) ;
#245729 = ADVANCED_FACE ( 'NONE', ( #158067 ), #126431, .F. ) ;
#245728 = EDGE_CURVE ( 'NONE', #113374, #71995, #34879, .T. ) ;
#245730 = DIRECTION ( 'NONE',  ( 0.000000000000000000, -0.6728971962617102953, -0.7397360091702507301 ) ) ;
#245731 = DIRECTION ( 'NONE',  ( 0.000000000000000000, 0.6728971962616697722, 0.7397360091702875895 ) ) ;
#245732 = EDGE_CURVE ( 'NONE', #13011, #40840, #159746, .T. ) ;
#245733 = CARTESIAN_POINT ( 'NONE',  ( 20.97565083910961548, 65.52538259873381321, -195.9451643079358973 ) ) ;
#245734 = CARTESIAN_POINT ( 'NONE',  ( -23.15000000000000213, 4.350000000011156054, -112.6500000000000483 ) ) ;
#245735 = EDGE_LOOP ( 'NONE', ( #152463, #145334 ) ) ;
#245736 = AXIS2_PLACEMENT_3D ( 'NONE', #104595, #86318, #25119 ) ;
#245737 = CARTESIAN_POINT ( 'NONE',  ( -23.25000000000000000, 64.25000000001173817, -81.27310748452440237 ) ) ;
#245738 = EDGE_CURVE ( 'NONE', #104063, #56714, #47291, .T. ) ;
#245739 = DIRECTION ( 'NONE',  ( 0.000000000000000000, -6.982962677686266711E-15, 1.000000000000000000 ) ) ;
#245740 = AXIS2_PLACEMENT_3D ( 'NONE', #29967, #89897, #65206 ) ;
#245741 = ORIENTED_EDGE ( 'NONE', *, *, #239912, .F. ) ;
#245742 = ADVANCED_FACE ( 'NONE', ( #223115 ), #226357, .T. ) ;
#245743 = EDGE_CURVE ( 'NONE', #10423, #181665, #253138, .T. ) ;
#245744 = CONICAL_SURFACE ( 'NONE', #216519, 7.750000000000027534, 0.7853981633974531640 ) ;
#245745 = CARTESIAN_POINT ( 'NONE',  ( 21.15000000000000213, 76.00000000001271871, -210.0637644362255969 ) ) ;
#245746 = CARTESIAN_POINT ( 'NONE',  ( 20.94999999999999929, 20.66107731230508548, -234.7421556583769302 ) ) ;
#245747 = ADVANCED_FACE ( 'NONE', ( #185289 ), #45768, .T. ) ;
#245748 = ORIENTED_EDGE ( 'NONE', *, *, #194459, .F. ) ;
#245749 = CARTESIAN_POINT ( 'NONE',  ( -21.05000000000000071, 6.540656951712400691, -67.10000000000005116 ) ) ;
#245750 = ORIENTED_EDGE ( 'NONE', *, *, #151323, .F. ) ;
#245751 = CARTESIAN_POINT ( 'NONE',  ( -15.70407651835961005, 9.355806591641288250, -49.79110253154618704 ) ) ;
#245752 = ORIENTED_EDGE ( 'NONE', *, *, #120059, .T. ) ;
#245753 = EDGE_CURVE ( 'NONE', #20940, #220754, #197712, .T. ) ;
#245754 = AXIS2_PLACEMENT_3D ( 'NONE', #155575, #250779, #12202 ) ;
#245755 = DIRECTION ( 'NONE',  ( 0.000000000000000000, -1.000000000000000000, 0.000000000000000000 ) ) ;
#245756 = CIRCLE ( 'NONE', #91813, 12.87499999999999822 ) ;
#245757 = DIRECTION ( 'NONE',  ( 0.000000000000000000, -0.4088369013363280513, 0.9126074666063771490 ) ) ;
#245759 = ORIENTED_EDGE ( 'NONE', *, *, #166766, .T. ) ;
#245758 = EDGE_CURVE ( 'NONE', #116101, #16833, #224399, .T. ) ;
#245760 = ORIENTED_EDGE ( 'NONE', *, *, #148349, .F. ) ;
#245761 = CARTESIAN_POINT ( 'NONE',  ( 11.60000000000000142, -12.24999999999999822, 15.00000000000000355 ) ) ;
#245763 = ORIENTED_EDGE ( 'NONE', *, *, #192474, .F. ) ;
#245762 = DIRECTION ( 'NONE',  ( -1.000000000000000000, 0.000000000000000000, 0.000000000000000000 ) ) ;
#245764 = DIRECTION ( 'NONE',  ( 0.000000000000000000, 0.5341055959866798375, -0.8454177738465836756 ) ) ;
#245765 = CIRCLE ( 'NONE', #25034, 7.791421356237338003 ) ;
#245766 = ORIENTED_EDGE ( 'NONE', *, *, #237772, .T. ) ;
#245767 = AXIS2_PLACEMENT_3D ( 'NONE', #24962, #26236, #86163 ) ;
#245768 = VERTEX_POINT ( 'NONE', #88727 ) ;
#245769 = EDGE_CURVE ( 'NONE', #190104, #245292, #51961, .T. ) ;
#245770 = CARTESIAN_POINT ( 'NONE',  ( -20.94999999999999929, -11.74999999998884448, -130.9000000000000341 ) ) ;
#245771 = DIRECTION ( 'NONE',  ( -1.000000000000000000, 0.000000000000000000, 0.000000000000000000 ) ) ;
#245772 = CARTESIAN_POINT ( 'NONE',  ( -18.46907102845856485, 38.07039079105120294, -261.0545844836100287 ) ) ;
#245773 = CARTESIAN_POINT ( 'NONE',  ( -16.77732147262506146, 9.945966932618629741, -20.83649124327587643 ) ) ;
#245774 = DIRECTION ( 'NONE',  ( 0.000000000000000000, 0.8814952561688444987, -0.4721928772777320149 ) ) ;
#245775 = CARTESIAN_POINT ( 'NONE',  ( -21.05000000000000071, 11.65000000001115232, -100.6000000000000369 ) ) ;
#245776 = ORIENTED_EDGE ( 'NONE', *, *, #29714, .F. ) ;
#245777 = CARTESIAN_POINT ( 'NONE',  ( -16.90128866880176872, 66.04620422280959247, -182.6604313011357874 ) ) ;
#245778 = FACE_OUTER_BOUND ( 'NONE', #53071, .T. ) ;
#245779 = FACE_OUTER_BOUND ( 'NONE', #28744, .T. ) ;
#245780 = CIRCLE ( 'NONE', #116778, 0.09999999999998898659 ) ;
#245781 = DIRECTION ( 'NONE',  ( 0.000000000000000000, -0.2128009952263601456, 0.9770955615653316162 ) ) ;
#245782 = TOROIDAL_SURFACE ( 'NONE', #175102, 11.90000000000000213, 0.1000000000000000056 ) ;
#245783 = EDGE_LOOP ( 'NONE', ( #225922, #198761 ) ) ;
#245784 = DIRECTION ( 'NONE',  ( 0.000000000000000000, 0.000000000000000000, -1.000000000000000000 ) ) ;
#245785 = ORIENTED_EDGE ( 'NONE', *, *, #190924, .T. ) ;
#245786 = CARTESIAN_POINT ( 'NONE',  ( 15.06592377766031632, 9.417789466963361278, -115.8573845439769059 ) ) ;
#245787 = ORIENTED_EDGE ( 'NONE', *, *, #169515, .F. ) ;
#245788 = DIRECTION ( 'NONE',  ( 0.000000000000000000, 0.000000000000000000, -1.000000000000000000 ) ) ;
#245789 = CARTESIAN_POINT ( 'NONE',  ( 21.05000000000000071, 76.00000000001190870, -103.0231074845243029 ) ) ;
#245790 = ORIENTED_EDGE ( 'NONE', *, *, #247990, .F. ) ;
#245791 = ORIENTED_EDGE ( 'NONE', *, *, #53830, .T. ) ;
#245793 = ORIENTED_EDGE ( 'NONE', *, *, #161070, .T. ) ;
#245792 = DIRECTION ( 'NONE',  ( 1.000000000000000000, -7.510212038922875604E-17, 1.676432719286210708E-16 ) ) ;
#245794 = CARTESIAN_POINT ( 'NONE',  ( -18.79999999999999716, -1.467286812112899463, 33.00000000000000000 ) ) ;
#245795 = VERTEX_POINT ( 'NONE', #28831 ) ;
#245796 = CARTESIAN_POINT ( 'NONE',  ( -22.50000000000000000, 0.09263750062063526303, -21.85030279295925126 ) ) ;
#245797 = DIRECTION ( 'NONE',  ( 1.000000000000000000, 0.000000000000000000, 0.000000000000000000 ) ) ;
#245798 = EDGE_LOOP ( 'NONE', ( #124847, #183250, #194384, #155722, #229579, #73801, #244354, #107063, #239744, #148813, #69387, #197162, #177189, #117523 ) ) ;
#245799 = ADVANCED_FACE ( 'NONE', ( #243967 ), #167042, .T. ) ;
#245801 = CIRCLE ( 'NONE', #87565, 12.97499999999999964 ) ;
#245800 = CARTESIAN_POINT ( 'NONE',  ( -20.12071067811865888, 9.320710678129810134, -179.8499999999999943 ) ) ;
#245802 = AXIS2_PLACEMENT_3D ( 'NONE', #196443, #239440, #161185 ) ;
#245804 = CYLINDRICAL_SURFACE ( 'NONE', #178227, 0.1000000000000028644 ) ;
#245803 = CONICAL_SURFACE ( 'NONE', #95751, 4.049999999999987388, 0.7853981633974604915 ) ;
#245805 = EDGE_CURVE ( 'NONE', #134549, #78107, #91344, .T. ) ;
#245806 = ORIENTED_EDGE ( 'NONE', *, *, #10009, .T. ) ;
#245807 = VECTOR ( 'NONE', #230558, 1000.000000000000000 ) ;
#245808 = CARTESIAN_POINT ( 'NONE',  ( 18.49999999999999645, -1.235880796157551309, -222.7862885752216471 ) ) ;
#245809 = EDGE_CURVE ( 'NONE', #20391, #140683, #211968, .T. ) ;
#245810 = CARTESIAN_POINT ( 'NONE',  ( -16.81095280782811230, 22.97806745954164853, -230.9350634111222291 ) ) ;
#245811 = EDGE_CURVE ( 'NONE', #171172, #19155, #62112, .T. ) ;
#245812 = APPLICATION_CONTEXT ( 'automotive_design' ) ;
#245813 = CARTESIAN_POINT ( 'NONE',  ( -23.15000000000000213, -8.999999999988846255, -76.89396912265249284 ) ) ;
#245815 = EDGE_LOOP ( 'NONE', ( #246866, #167404, #219750, #193823 ) ) ;
#245814 = FACE_OUTER_BOUND ( 'NONE', #224415, .T. ) ;
#245816 = DIRECTION ( 'NONE',  ( 0.000000000000000000, 0.8814952561688429444, -0.4721928772777349570 ) ) ;
#245817 = CARTESIAN_POINT ( 'NONE',  ( -21.29999999999995808, 67.23127455305841238, -235.8551265064783991 ) ) ;
#245818 = CARTESIAN_POINT ( 'NONE',  ( -23.25000000000000000, 85.60000000001221565, -146.4170766071767389 ) ) ;
#245819 = CIRCLE ( 'NONE', #200032, 4.900000000000000355 ) ;
#245821 = CARTESIAN_POINT ( 'NONE',  ( 23.24999999999997513, 11.75000000001116263, -160.4851942293460638 ) ) ;
#245820 = DIRECTION ( 'NONE',  ( 0.000000000000000000, 0.2128009952263618110, -0.9770955615653311721 ) ) ;
#245822 = CARTESIAN_POINT ( 'NONE',  ( 18.49999999999996803, 7.070967871809997973, -204.7465642218682547 ) ) ;
#245823 = CARTESIAN_POINT ( 'NONE',  ( -18.50000000000000000, 1.340746217944851715, -123.7271374945788409 ) ) ;
#245824 = DIRECTION ( 'NONE',  ( 0.000000000000000000, 1.000000000000000000, 6.982962677686266711E-15 ) ) ;
#245825 = CARTESIAN_POINT ( 'NONE',  ( -20.65000000000000568, 7.250000000011138646, -146.6500000000000341 ) ) ;
#245826 = ORIENTED_EDGE ( 'NONE', *, *, #169395, .T. ) ;
#245827 = EDGE_CURVE ( 'NONE', #58185, #60353, #178857, .T. ) ;
#245828 = ORIENTED_EDGE ( 'NONE', *, *, #224535, .F. ) ;
#245829 = CARTESIAN_POINT ( 'NONE',  ( -20.64999999999999858, 76.00000000001213607, -136.5231074845242745 ) ) ;
#245830 =( BOUNDED_SURFACE ( )  B_SPLINE_SURFACE ( 3, 2, ( 
 ( #20170, #215771, #80088 ),
 ( #159681, #154570, #56679 ),
 ( #573, #120567, #157126 ),
 ( #99665, #177964, #218333 ),
 ( #100925, #17574, #97084 ),
 ( #78824, #60554, #39754 ) ),
 .UNSPECIFIED., .F., .F., .F. ) 
 B_SPLINE_SURFACE_WITH_KNOTS ( ( 4, 2, 4 ),
 ( 3, 3 ),
 ( 6.719893378898281297E-05, 0.0002757154632485351252, 0.0004842319927080873969 ),
 ( 0.000000000000000000, 1.000000000000000000 ),
 .UNSPECIFIED. ) 
 GEOMETRIC_REPRESENTATION_ITEM ( )  RATIONAL_B_SPLINE_SURFACE ( (
 ( 1.000000000000000000, 0.7250110520819756932, 1.000000000000000000),
 ( 1.000000000000000000, 0.7277932058380179869, 1.000000000000000000),
 ( 1.000000000000000000, 0.7278452872589651346, 1.000000000000000000),
 ( 1.000000000000000000, 0.7221445671577162440, 1.000000000000000000),
 ( 1.000000000000000000, 0.7163662143757810741, 1.000000000000000000),
 ( 1.000000000000000000, 0.7071067811866325048, 1.000000000000000000) ) ) 
 REPRESENTATION_ITEM ( '' )  SURFACE ( )  );
#245831 = ORIENTED_EDGE ( 'NONE', *, *, #30707, .T. ) ;
#245832 = CARTESIAN_POINT ( 'NONE',  ( 23.24999999999999645, 38.50047664313251516, -246.1133312021848951 ) ) ;
#245833 = ORIENTED_EDGE ( 'NONE', *, *, #246539, .F. ) ;
#245834 = LINE ( 'NONE', #219841, #53319 ) ;
#245835 = CARTESIAN_POINT ( 'NONE',  ( 22.59999999999999432, 64.08545097430041437, -247.0723585184913986 ) ) ;
#245836 = AXIS2_PLACEMENT_3D ( 'NONE', #232596, #138563, #94326 ) ;
#245837 = VERTEX_POINT ( 'NONE', #109586 ) ;
#245838 = EDGE_CURVE ( 'NONE', #128716, #119361, #86150, .T. ) ;
#245839 = DIRECTION ( 'NONE',  ( -0.000000000000000000, 0.000000000000000000, -1.000000000000000000 ) ) ;
#245840 = EDGE_LOOP ( 'NONE', ( #165131, #228841, #250306, #84776 ) ) ;
#245841 = ORIENTED_EDGE ( 'NONE', *, *, #122966, .F. ) ;
#245842 = CARTESIAN_POINT ( 'NONE',  ( -16.86337532320262156, 9.979967204235514089, -46.05107553101719020 ) ) ;
#245843 = CARTESIAN_POINT ( 'NONE',  ( -18.59999999999999787, 77.35494420175976416, -241.6200040285045532 ) ) ;
#245845 = ORIENTED_EDGE ( 'NONE', *, *, #229017, .T. ) ;
#245844 = CARTESIAN_POINT ( 'NONE',  ( 21.11345278033268968, 67.11787792663994878, -57.27708531376936918 ) ) ;
#245846 = AXIS2_PLACEMENT_3D ( 'NONE', #54425, #171853, #152274 ) ;
#245847 = CARTESIAN_POINT ( 'NONE',  ( 20.01093837587850288, 11.75000000001116263, -158.7543974345976494 ) ) ;
#245849 = ORIENTED_EDGE ( 'NONE', *, *, #35882, .T. ) ;
#245848 = CYLINDRICAL_SURFACE ( 'NONE', #239296, 12.87499999999999112 ) ;
#245850 = DIRECTION ( 'NONE',  ( -0.000000000000000000, 0.000000000000000000, -1.000000000000000000 ) ) ;
#245851 = CYLINDRICAL_SURFACE ( 'NONE', #74955, 0.09999999999999939493 ) ;
#245852 = ADVANCED_FACE ( 'NONE', ( #183999 ), #126596, .F. ) ;
#245854 = ORIENTED_EDGE ( 'NONE', *, *, #8783, .F. ) ;
#245853 = CARTESIAN_POINT ( 'NONE',  ( -20.64999999999999858, 4.350000000011156054, -179.8499999999999943 ) ) ;
#245855 = CARTESIAN_POINT ( 'NONE',  ( 18.49999999999999645, 74.13328508995527955, -191.7704322382423641 ) ) ;
#245856 = DIRECTION ( 'NONE',  ( 1.000000000000000000, 0.000000000000000000, 0.000000000000000000 ) ) ;
#245857 = ADVANCED_FACE ( 'NONE', ( #168338 ), #10512, .F. ) ;
#245858 = CARTESIAN_POINT ( 'NONE',  ( -16.86132326855785735, 9.950000000011135270, -113.1986357846683688 ) ) ;
#245860 = CYLINDRICAL_SURFACE ( 'NONE', #208136, 0.1000000000000106498 ) ;
#245859 = LINE ( 'NONE', #230144, #90803 ) ;
#245861 = CARTESIAN_POINT ( 'NONE',  ( 18.49999999999999289, 10.20857864377384416, -91.65000000000004832 ) ) ;
#245862 = VECTOR ( 'NONE', #62223, 1000.000000000000000 ) ;
#245863 = CARTESIAN_POINT ( 'NONE',  ( 21.08489834409762054, 65.37767610527676254, -157.6731074845243938 ) ) ;
#245864 = FACE_OUTER_BOUND ( 'NONE', #166858, .T. ) ;
#245865 = DIRECTION ( 'NONE',  ( 0.000000000000000000, 0.000000000000000000, -1.000000000000000000 ) ) ;
#245866 = ORIENTED_EDGE ( 'NONE', *, *, #184746, .T. ) ;
#245867 = ORIENTED_EDGE ( 'NONE', *, *, #158411, .T. ) ;
#245868 = ORIENTED_EDGE ( 'NONE', *, *, #173127, .T. ) ;
#245869 = ADVANCED_FACE ( 'NONE', ( #225663 ), #67903, .T. ) ;
#245870 = DIRECTION ( 'NONE',  ( -1.000000000000000000, -0.000000000000000000, 0.000000000000000000 ) ) ;
#245871 = ORIENTED_EDGE ( 'NONE', *, *, #239272, .T. ) ;
#245873 = CARTESIAN_POINT ( 'NONE',  ( -21.05000000000000071, 76.00000000001210765, -132.4231074845243370 ) ) ;
#245872 = CIRCLE ( 'NONE', #16937, 0.1000000000000028644 ) ;
#245874 = ORIENTED_EDGE ( 'NONE', *, *, #138895, .F. ) ;
#245875 = DIRECTION ( 'NONE',  ( 0.000000000000000000, -6.982962677686266711E-15, 1.000000000000000000 ) ) ;
#245876 = CARTESIAN_POINT ( 'NONE',  ( 18.54116936837188234, -9.463564198361282820, -40.54854249088825213 ) ) ;
#245877 = EDGE_CURVE ( 'NONE', #147074, #184295, #203565, .T. ) ;
#245878 = AXIS2_PLACEMENT_3D ( 'NONE', #168681, #150363, #129508 ) ;
#245879 = EDGE_CURVE ( 'NONE', #125024, #51335, #237077, .T. ) ;
#245880 = AXIS2_PLACEMENT_3D ( 'NONE', #92374, #191518, #254012 ) ;
#245881 = EDGE_LOOP ( 'NONE', ( #76126, #191809, #252364, #162253 ) ) ;
#245882 = EDGE_CURVE ( 'NONE', #241214, #91747, #74623, .T. ) ;
#245883 = CARTESIAN_POINT ( 'NONE',  ( -23.25000000000000000, -0.09999999998884338825, -88.85042919245522341 ) ) ;
#245884 =( NAMED_UNIT ( * ) SI_UNIT ( $, .STERADIAN. ) SOLID_ANGLE_UNIT ( ) );
#245885 = B_SPLINE_CURVE_WITH_KNOTS ( 'NONE', 3,
 ( #183789, #242462, #101644, #161680, #67687, #225456, #241210, #200783, #221600, #63843 ),
 .UNSPECIFIED., .F., .F.,
 ( 4, 2, 2, 2, 4 ),
 ( 5.247129907028296623E-16, 9.930191194501768691E-05, 0.0001986038238895106471, 0.0003972076477784965945, 0.0007944152955563852769 ),
 .UNSPECIFIED. ) ;
#245887 = ORIENTED_EDGE ( 'NONE', *, *, #170640, .T. ) ;
#245886 = AXIS2_PLACEMENT_3D ( 'NONE', #177008, #200393, #81682 ) ;
#245888 = VERTEX_POINT ( 'NONE', #35233 ) ;
#245889 = CIRCLE ( 'NONE', #133458, 0.09999999999999543976 ) ;
#245890 = CIRCLE ( 'NONE', #233268, 0.09999999999999939493 ) ;
#245891 = ORIENTED_EDGE ( 'NONE', *, *, #187947, .F. ) ;
#245892 = AXIS2_PLACEMENT_3D ( 'NONE', #81298, #203842, #160893 ) ;
#245893 = AXIS2_PLACEMENT_3D ( 'NONE', #121484, #116332, #155484 ) ;
#245894 = CARTESIAN_POINT ( 'NONE',  ( -18.50000000000000000, 48.14768554360777841, -246.4498133360871179 ) ) ;
#245895 = CYLINDRICAL_SURFACE ( 'NONE', #209163, 12.87499999999999822 ) ;
#245896 = CARTESIAN_POINT ( 'NONE',  ( 23.24999999999999289, 4.150000000011154988, -100.5000000000000284 ) ) ;
#245897 = LINE ( 'NONE', #149383, #48339 ) ;
#245898 = CARTESIAN_POINT ( 'NONE',  ( -23.25000000000000000, -3.281532336344785694, -226.3283167004137226 ) ) ;
#245899 = EDGE_CURVE ( 'NONE', #200182, #168523, #13088, .T. ) ;
#245901 = CARTESIAN_POINT ( 'NONE',  ( 18.59999999999999787, -10.84999999999999076, 33.00000000000000000 ) ) ;
#245900 = FACE_OUTER_BOUND ( 'NONE', #19484, .T. ) ;
#245902 = CARTESIAN_POINT ( 'NONE',  ( -20.00857864376270001, 30.22839164850006455, -235.6129688350293350 ) ) ;
#245904 = ORIENTED_EDGE ( 'NONE', *, *, #187254, .T. ) ;
#245903 = CARTESIAN_POINT ( 'NONE',  ( 18.39999999999999503, 31.05627573922685514, -233.2203535436961488 ) ) ;
#245906 = CARTESIAN_POINT ( 'NONE',  ( -22.10000000000000497, 3.362550747017869046, 28.82623795144604983 ) ) ;
#245905 = CARTESIAN_POINT ( 'NONE',  ( 20.19326291201655366, 10.15606098791449519, -74.76186180760271327 ) ) ;
#245907 = CARTESIAN_POINT ( 'NONE',  ( -18.59999999999999787, 77.73670573947892137, -24.50568489690058627 ) ) ;
#245908 = ORIENTED_EDGE ( 'NONE', *, *, #202908, .T. ) ;
#245909 = CARTESIAN_POINT ( 'NONE',  ( 20.95566103547454517, 10.61824765095822087, -74.63184019298063276 ) ) ;
#245910 = DIRECTION ( 'NONE',  ( 0.000000000000000000, 0.2617529984165152257, 0.9651348961777124202 ) ) ;
#245911 = CYLINDRICAL_SURFACE ( 'NONE', #228942, 1.500000000000001332 ) ;
#245912 = ORIENTED_EDGE ( 'NONE', *, *, #10389, .T. ) ;
#245913 = CIRCLE ( 'NONE', #45983, 0.1000000000000000472 ) ;
#245914 = DIRECTION ( 'NONE',  ( 0.000000000000000000, 6.982962677686266711E-15, -1.000000000000000000 ) ) ;
#245915 = DIRECTION ( 'NONE',  ( -1.836970198721029934E-16, 1.000000000000000000, 0.000000000000000000 ) ) ;
#245916 = CARTESIAN_POINT ( 'NONE',  ( -18.39999999999999858, 78.24072131640578220, -231.5548844243369047 ) ) ;
#245917 = ORIENTED_EDGE ( 'NONE', *, *, #44466, .T. ) ;
#245918 = ORIENTED_EDGE ( 'NONE', *, *, #196381, .F. ) ;
#245919 = DIRECTION ( 'NONE',  ( 1.000000000000000000, 0.000000000000000000, 0.000000000000000000 ) ) ;
#245920 = ORIENTED_EDGE ( 'NONE', *, *, #197809, .F. ) ;
#245921 = DIRECTION ( 'NONE',  ( -1.000000000000000000, 0.000000000000000000, 0.000000000000000000 ) ) ;
#245922 = CYLINDRICAL_SURFACE ( 'NONE', #169925, 1.749999999999998002 ) ;
#245923 = DIRECTION ( 'NONE',  ( 0.000000000000000000, 0.5868805631290315850, 0.8096735173027156396 ) ) ;
#245924 = PLANE ( 'NONE',  #1008 ) ;
#245925 = ORIENTED_EDGE ( 'NONE', *, *, #177693, .T. ) ;
#245926 = VECTOR ( 'NONE', #83452, 1000.000000000000000 ) ;
#245927 = CARTESIAN_POINT ( 'NONE',  ( -12.92414019175886253, 9.417632963117446465, -118.6489484657322606 ) ) ;
#245928 = CARTESIAN_POINT ( 'NONE',  ( 19.99999999999998934, 64.25000000001199396, -115.1731074845243796 ) ) ;
#245929 = AXIS2_PLACEMENT_3D ( 'NONE', #18069, #1046, #200560 ) ;
#245930 = CARTESIAN_POINT ( 'NONE',  ( 18.49999999999999289, 10.20857864609425825, -192.2025068656295446 ) ) ;
#245931 = LINE ( 'NONE', #145526, #236499 ) ;
#245932 = VECTOR ( 'NONE', #89708, 1000.000000000000000 ) ;
#245933 = EDGE_CURVE ( 'NONE', #4740, #82553, #203758, .T. ) ;
#245934 = ORIENTED_EDGE ( 'NONE', *, *, #161860, .F. ) ;
#245935 = DIRECTION ( 'NONE',  ( 0.000000000000000000, 0.9856811345164827598, 0.1686199900910313187 ) ) ;
#245936 =( BOUNDED_SURFACE ( )  B_SPLINE_SURFACE ( 3, 2, ( 
 ( #17622, #94596, #132451 ),
 ( #153344, #97129, #236671 ),
 ( #112891, #55444, #58023 ),
 ( #176733, #37220, #253665 ),
 ( #213259, #114168, #256179 ),
 ( #115447, #134993, #215815 ) ),
 .UNSPECIFIED., .F., .F., .F. ) 
 B_SPLINE_SURFACE_WITH_KNOTS ( ( 4, 2, 4 ),
 ( 3, 3 ),
 ( 3.141592653589783346, 3.926990816987233845, 4.712388980384684345 ),
 ( 0.000000000000000000, 1.000000000000000000 ),
 .UNSPECIFIED. ) 
 GEOMETRIC_REPRESENTATION_ITEM ( )  RATIONAL_B_SPLINE_SURFACE ( (
 ( 1.000000000000000000, 0.9238795325112774126, 1.000000000000000000),
 ( 1.000000000000000000, 0.9240297172243894241, 1.000000000000000000),
 ( 1.000000000000000000, 0.9038128468038970631, 1.000000000000000000),
 ( 1.000000000000000000, 0.8282379607649767994, 1.000000000000000000),
 ( 1.000000000000000000, 0.7727932973491338231, 1.000000000000000000),
 ( 1.000000000000000000, 0.7071067811865475727, 1.000000000000000000) ) ) 
 REPRESENTATION_ITEM ( '' )  SURFACE ( )  );
#245937 = CIRCLE ( 'NONE', #183574, 4.099999999999989875 ) ;
#245939 = ORIENTED_EDGE ( 'NONE', *, *, #182763, .F. ) ;
#245938 = FACE_BOUND ( 'NONE', #76139, .T. ) ;
#245940 = CARTESIAN_POINT ( 'NONE',  ( -21.05000000000000071, 14.85285025691667293, -236.4388300032497057 ) ) ;
#245941 = CARTESIAN_POINT ( 'NONE',  ( 18.59999999999999787, 7.576017155224048061, -241.7224044826512284 ) ) ;
#245942 = PLANE ( 'NONE',  #238529 ) ;
#245943 = EDGE_CURVE ( 'NONE', #77748, #252845, #162081, .T. ) ;
#245944 = DIRECTION ( 'NONE',  ( 1.000000000000000000, -0.000000000000000000, -0.000000000000000000 ) ) ;
#245945 = CARTESIAN_POINT ( 'NONE',  ( 23.15000000000000213, -8.663551401858002876, -143.5241011180673070 ) ) ;
#245946 = CARTESIAN_POINT ( 'NONE',  ( -23.25000000000000000, 25.97741635855165754, -254.4468634167653249 ) ) ;
#245947 = CARTESIAN_POINT ( 'NONE',  ( -21.05000000000000071, 88.41227409416141825, -72.42310748452422331 ) ) ;
#245948 = ORIENTED_EDGE ( 'NONE', *, *, #252118, .T. ) ;
#245949 = DIRECTION ( 'NONE',  ( 0.000000000000000000, 0.9126074666063545004, 0.4088369013363783999 ) ) ;
#245950 = AXIS2_PLACEMENT_3D ( 'NONE', #178843, #238786, #219204 ) ;
#245951 = DIRECTION ( 'NONE',  ( 0.000000000000000000, 0.000000000000000000, -1.000000000000000000 ) ) ;
#245952 = EDGE_CURVE ( 'NONE', #160946, #102524, #112203, .T. ) ;
#245953 = EDGE_CURVE ( 'NONE', #64282, #85751, #28844, .T. ) ;
#245954 = CARTESIAN_POINT ( 'NONE',  ( 19.58285714285715073, 18.75808650758932217, -228.1810571460606241 ) ) ;
#245956 = CIRCLE ( 'NONE', #87705, 11.80000000000000426 ) ;
#245955 = SPHERICAL_SURFACE ( 'NONE', #21514, 0.1000000000000000056 ) ;
#245957 = FACE_OUTER_BOUND ( 'NONE', #196095, .T. ) ;
#245958 = AXIS2_PLACEMENT_3D ( 'NONE', #157389, #140340, #217301 ) ;
#245959 = VERTEX_POINT ( 'NONE', #96431 ) ;
#245960 = ORIENTED_EDGE ( 'NONE', *, *, #29547, .T. ) ;
#245961 = CIRCLE ( 'NONE', #4323, 6.329289321881357289 ) ;
#245962 = DIRECTION ( 'NONE',  ( 0.000000000000000000, 0.000000000000000000, -1.000000000000000000 ) ) ;
#245963 = CARTESIAN_POINT ( 'NONE',  ( -20.94999999999999929, 46.45388641681647357, -243.1520440498138385 ) ) ;
#245964 = FACE_OUTER_BOUND ( 'NONE', #112022, .T. ) ;
#245965 = ADVANCED_FACE ( 'NONE', ( #151315 ), #233421, .T. ) ;
#245966 = DIRECTION ( 'NONE',  ( 0.000000000000000000, 0.2617529984165055668, 0.9651348961777149738 ) ) ;
#245967 = DIRECTION ( 'NONE',  ( 1.000000000000000000, 0.000000000000000000, 0.000000000000000000 ) ) ;
#245968 = CARTESIAN_POINT ( 'NONE',  ( -21.07928932188134041, 0.09889514566555068775, -60.67148334360675221 ) ) ;
#245969 = CIRCLE ( 'NONE', #83609, 0.09999999999999939493 ) ;
#245970 = CARTESIAN_POINT ( 'NONE',  ( -20.94999999999999218, 17.16609282392352398, -224.6038045889790453 ) ) ;
#245971 = VERTEX_POINT ( 'NONE', #194299 ) ;
#245972 = CARTESIAN_POINT ( 'NONE',  ( -18.40000000000000213, 11.74999999999998224, -20.85000000000000142 ) ) ;
#245973 = VERTEX_POINT ( 'NONE', #92589 ) ;
#245974 = EDGE_CURVE ( 'NONE', #171691, #199040, #195407, .T. ) ;
#245975 = CARTESIAN_POINT ( 'NONE',  ( -21.05000000000000071, 76.09999996531125532, -76.00065966701779985 ) ) ;
#245976 = EDGE_CURVE ( 'NONE', #194720, #47350, #187036, .T. ) ;
#245977 = DIRECTION ( 'NONE',  ( 1.000000000000000000, 0.000000000000000000, 1.073024830501117725E-15 ) ) ;
#245978 = SPHERICAL_SURFACE ( 'NONE', #107731, 0.1000000000000000056 ) ;
#245979 = CARTESIAN_POINT ( 'NONE',  ( -16.77732147278574715, 9.945966932584589415, -46.16350875687581379 ) ) ;
#245980 = DIRECTION ( 'NONE',  ( -0.000000000000000000, 0.000000000000000000, 1.000000000000000000 ) ) ;
#245981 = DIRECTION ( 'NONE',  ( -1.000000000000000000, 7.304098846218134667E-16, 5.100424963727256530E-30 ) ) ;
#245982 = CARTESIAN_POINT ( 'NONE',  ( 20.95512820512820440, 39.31056039967181448, -236.7220595557971023 ) ) ;
#245983 = ORIENTED_EDGE ( 'NONE', *, *, #207607, .F. ) ;
#245984 = DIRECTION ( 'NONE',  ( -1.000000000000000000, -0.000000000000000000, -0.000000000000000000 ) ) ;
#245985 = AXIS2_PLACEMENT_3D ( 'NONE', #222568, #106463, #223856 ) ;
#245986 = DIRECTION ( 'NONE',  ( 0.000000000000000000, 0.9126074666063660468, 0.4088369013363524762 ) ) ;
#245987 = CIRCLE ( 'NONE', #200194, 0.09999999999998898659 ) ;
#245988 = DIRECTION ( 'NONE',  ( 0.000000000000000000, -0.9910827722268055195, 0.1332476588733540468 ) ) ;
#245990 = ADVANCED_FACE ( 'NONE', ( #155184 ), #134279, .F. ) ;
#245989 = CARTESIAN_POINT ( 'NONE',  ( 18.39999999999999858, -9.499999999999998224, -40.10018939122204529 ) ) ;
#245991 = AXIS2_PLACEMENT_3D ( 'NONE', #90353, #248157, #224725 ) ;
#245992 = CARTESIAN_POINT ( 'NONE',  ( -18.59999999999999787, 74.75000000001232081, -162.0231074845243597 ) ) ;
#245993 = CARTESIAN_POINT ( 'NONE',  ( 20.95263205890668345, 8.895740107905178107, -175.9895084069416384 ) ) ;
#245994 = VECTOR ( 'NONE', #194964, 1000.000000000000227 ) ;
#245995 = ORIENTED_EDGE ( 'NONE', *, *, #66430, .T. ) ;
#245996 = CARTESIAN_POINT ( 'NONE',  ( 18.50000000000000355, 85.41907808086162390, -129.6931821343160038 ) ) ;
#245997 = DIRECTION ( 'NONE',  ( 0.000000000000000000, -1.000000000000000000, -6.982962677686265922E-15 ) ) ;
#245998 = VERTEX_POINT ( 'NONE', #215116 ) ;
#245999 = CARTESIAN_POINT ( 'NONE',  ( -21.65000000000000213, 44.68681448124952027, -237.5080042326551393 ) ) ;
#246000 = CARTESIAN_POINT ( 'NONE',  ( 21.07199075132372101, 67.22505500089620512, -157.8095753229115701 ) ) ;
#246001 = CIRCLE ( 'NONE', #229267, 0.1000000000000013933 ) ;
#246002 = ADVANCED_FACE ( 'NONE', ( #52179 ), #133027, .T. ) ;
#246003 = CARTESIAN_POINT ( 'NONE',  ( -21.44999999999999929, 11.68239342655420110, -220.1014838121945161 ) ) ;
#246004 = VERTEX_POINT ( 'NONE', #130442 ) ;
#246005 = CARTESIAN_POINT ( 'NONE',  ( 21.05000000000000071, 64.25000000001145395, -42.86470817442145176 ) ) ;
#246006 = DIRECTION ( 'NONE',  ( 0.000000000000000000, 0.000000000000000000, -1.000000000000000000 ) ) ;
#246007 = ORIENTED_EDGE ( 'NONE', *, *, #210130, .T. ) ;
#246008 = DIRECTION ( 'NONE',  ( 1.000000000000000000, -0.000000000000000000, -0.000000000000000000 ) ) ;
#246009 = EDGE_CURVE ( 'NONE', #105564, #5669, #257866, .T. ) ;
#246010 = EDGE_LOOP ( 'NONE', ( #124224, #138504, #74208 ) ) ;
#246011 = DIRECTION ( 'NONE',  ( 0.000000000000000000, 0.2617529984164955192, 0.9651348961777178603 ) ) ;
#246012 = VECTOR ( 'NONE', #240501, 1000.000000000000114 ) ;
#246013 = DIRECTION ( 'NONE',  ( 1.000000000000000000, 0.000000000000000000, 0.000000000000000000 ) ) ;
#246014 = DIRECTION ( 'NONE',  ( 0.000000000000000000, 0.2128009952263485993, -0.9770955615653341697 ) ) ;
#246016 = CARTESIAN_POINT ( 'NONE',  ( 21.07933241753356768, 33.98632151110914634, -243.8137701776410040 ) ) ;
#246015 = UNCERTAINTY_MEASURE_WITH_UNIT (LENGTH_MEASURE( 1.000000000000000082E-05 ), #197710, 'distance_accuracy_value', 'NONE');
#246017 = ADVANCED_FACE ( 'NONE', ( #251673 ), #73083, .F. ) ;
#246019 = EDGE_CURVE ( 'NONE', #90426, #254695, #116292, .T. ) ;
#246018 = CARTESIAN_POINT ( 'NONE',  ( -21.05000000000000071, -0.09999999998884338825, -93.95934304829879125 ) ) ;
#246020 = DIRECTION ( 'NONE',  ( -1.000000000000000000, 0.000000000000000000, 0.000000000000000000 ) ) ;
#246021 = DIRECTION ( 'NONE',  ( 0.000000000000000000, 0.000000000000000000, -1.000000000000000000 ) ) ;
#246022 = AXIS2_PLACEMENT_3D ( 'NONE', #217357, #3454, #222486 ) ;
#246023 = DIRECTION ( 'NONE',  ( 0.000000000000000000, 0.000000000000000000, -1.000000000000000000 ) ) ;
#246024 = DIRECTION ( 'NONE',  ( 0.000000000000000000, -1.000000000000000000, -6.982962677686266711E-15 ) ) ;
#246026 = ORIENTED_EDGE ( 'NONE', *, *, #257687, .T. ) ;
#246025 = DIRECTION ( 'NONE',  ( -0.000000000000000000, 0.3848449534832920627, 0.9229812358755962176 ) ) ;
#246027 = VERTEX_POINT ( 'NONE', #152611 ) ;
#246029 = CARTESIAN_POINT ( 'NONE',  ( -13.11924609551134857, 9.431689550535258704, -85.27929003223610493 ) ) ;
#246028 = DIRECTION ( 'NONE',  ( -1.000000000000000000, 1.836970198721029934E-16, 1.282749433769087757E-30 ) ) ;
#246031 = ORIENTED_EDGE ( 'NONE', *, *, #182169, .F. ) ;
#246030 = DIRECTION ( 'NONE',  ( 0.000000000000000000, 7.026728003956695223E-15, -1.000000000000000000 ) ) ;
#246032 = CIRCLE ( 'NONE', #117035, 0.1000000000000000472 ) ;
#246033 = VERTEX_POINT ( 'NONE', #232132 ) ;
#246034 = CARTESIAN_POINT ( 'NONE',  ( 19.90000000000000568, 5.488301202077012775, 16.50000000000000000 ) ) ;
#246035 = CARTESIAN_POINT ( 'NONE',  ( 21.00000000000000000, 66.25000000001253397, -182.3731074845244393 ) ) ;
#246036 = EDGE_CURVE ( 'NONE', #17339, #45933, #110883, .T. ) ;
#246037 = EDGE_CURVE ( 'NONE', #192810, #27728, #158018, .T. ) ;
#246038 = FACE_OUTER_BOUND ( 'NONE', #16552, .T. ) ;
#246039 = AXIS2_PLACEMENT_3D ( 'NONE', #231176, #72091, #75932 ) ;
#246040 = CARTESIAN_POINT ( 'NONE',  ( -20.94999999999999929, 10.29288807859936661, -172.9580020160121876 ) ) ;
#246041 = DIRECTION ( 'NONE',  ( 1.000000000000000000, 0.000000000000000000, 0.000000000000000000 ) ) ;
#246042 = CARTESIAN_POINT ( 'NONE',  ( -20.00857864376270001, 66.85000000001200249, -115.3731074845243683 ) ) ;
#246043 = CARTESIAN_POINT ( 'NONE',  ( -20.64999999999999858, 2.000000000011154189, -180.2246219227620543 ) ) ;
#246045 = EDGE_LOOP ( 'NONE', ( #248888, #248711, #225, #78676 ) ) ;
#246044 = ADVANCED_FACE ( 'NONE', ( #241123 ), #149610, .T. ) ;
#246046 = ORIENTED_EDGE ( 'NONE', *, *, #48963, .F. ) ;
#246047 = CARTESIAN_POINT ( 'NONE',  ( 18.59999999999999076, 33.76625905298630670, -236.4206613783598243 ) ) ;
#246048 = EDGE_LOOP ( 'NONE', ( #207969, #50434, #96265, #75724 ) ) ;
#246049 = DIRECTION ( 'NONE',  ( 1.000000000000000000, 0.000000000000000000, 0.000000000000000000 ) ) ;
#246052 = EDGE_CURVE ( 'NONE', #118577, #134638, #232823, .T. ) ;
#246051 = VERTEX_POINT ( 'NONE', #198120 ) ;
#246050 = AXIS2_PLACEMENT_3D ( 'NONE', #159762, #163615, #180605 ) ;
#246053 = CARTESIAN_POINT ( 'NONE',  ( -21.65000000000000213, 66.05000000001182059, -82.27310748452437394 ) ) ;
#246054 = CIRCLE ( 'NONE', #133614, 0.1000000000000075273 ) ;
#246055 = AXIS2_PLACEMENT_3D ( 'NONE', #61210, #161623, #222836 ) ;
#246056 = DIRECTION ( 'NONE',  ( 1.000000000000000000, 0.000000000000000000, -0.000000000000000000 ) ) ;
#246057 = ADVANCED_FACE ( 'NONE', ( #196829 ), #139408, .T. ) ;
#246058 = CARTESIAN_POINT ( 'NONE',  ( 18.59999999999998721, 65.50857864377418593, -44.77310748452440237 ) ) ;
#246059 = LINE ( 'NONE', #121002, #191430 ) ;
#246060 = EDGE_LOOP ( 'NONE', ( #75313, #179482, #213373, #93615 ) ) ;
#246061 = CIRCLE ( 'NONE', #250339, 12.77499999999999503 ) ;
#246063 = VECTOR ( 'NONE', #20569, 1000.000000000000000 ) ;
#246062 = CARTESIAN_POINT ( 'NONE',  ( -20.94999999999999929, 11.74999999999999645, -7.014805770654001016 ) ) ;
#246064 = ORIENTED_EDGE ( 'NONE', *, *, #84295, .T. ) ;
#246065 = EDGE_CURVE ( 'NONE', #125216, #253366, #159028, .T. ) ;
#246066 = CARTESIAN_POINT ( 'NONE',  ( -21.59142135623730852, 65.19104153457237771, -213.3877624147501422 ) ) ;
#246067 = LINE ( 'NONE', #49132, #19061 ) ;
#246068 = EDGE_CURVE ( 'NONE', #42394, #245021, #182926, .T. ) ;
#246069 = DIRECTION ( 'NONE',  ( 0.000000000000000000, 0.000000000000000000, 1.000000000000000000 ) ) ;
#246070 = CARTESIAN_POINT ( 'NONE',  ( -18.59999999999999787, 70.08587962373171365, -198.1273832143211848 ) ) ;
#246072 = ORIENTED_EDGE ( 'NONE', *, *, #254906, .F. ) ;
#246071 = EDGE_CURVE ( 'NONE', #9664, #1847, #216211, .T. ) ;
#246073 = CARTESIAN_POINT ( 'NONE',  ( -23.15000000000000213, 64.25000000001269029, -203.5231074845244166 ) ) ;
#246074 = EDGE_LOOP ( 'NONE', ( #97184, #160297, #172033, #217277 ) ) ;
#246077 = ORIENTED_EDGE ( 'NONE', *, *, #227790, .F. ) ;
#246076 = DIRECTION ( 'NONE',  ( -0.000000000000000000, 1.000000000000000000, -1.224646799147352961E-16 ) ) ;
#246075 = FACE_OUTER_BOUND ( 'NONE', #215234, .T. ) ;
#246078 = VECTOR ( 'NONE', #226344, 1000.000000000000000 ) ;
#246079 = CARTESIAN_POINT ( 'NONE',  ( -20.64999999999999858, 71.65000000001155911, -57.27310748452435263 ) ) ;
#246080 = CIRCLE ( 'NONE', #108705, 0.09999999999999939493 ) ;
#246082 = ORIENTED_EDGE ( 'NONE', *, *, #50270, .F. ) ;
#246081 = CIRCLE ( 'NONE', #204361, 11.80000000000000426 ) ;
#246083 = VECTOR ( 'NONE', #173147, 1000.000000000000000 ) ;
#246084 = AXIS2_PLACEMENT_3D ( 'NONE', #68423, #247036, #147957 ) ;
#246085 = DIRECTION ( 'NONE',  ( 0.000000000000000000, 0.000000000000000000, -1.000000000000000000 ) ) ;
#246086 = ORIENTED_EDGE ( 'NONE', *, *, #1373, .F. ) ;
#246087 = FACE_OUTER_BOUND ( 'NONE', #167114, .T. ) ;
#246088 = EDGE_CURVE ( 'NONE', #5875, #104969, #78835, .T. ) ;
#246089 = FACE_OUTER_BOUND ( 'NONE', #194517, .T. ) ;
#246090 = EDGE_CURVE ( 'NONE', #161343, #3082, #145481, .T. ) ;
#246091 = CARTESIAN_POINT ( 'NONE',  ( -18.50000000000000000, 21.13195309841794867, -243.6318585593224100 ) ) ;
#246092 = CARTESIAN_POINT ( 'NONE',  ( -21.45000000000000284, 68.29142135624960019, -157.7731074845244166 ) ) ;
#246093 = AXIS2_PLACEMENT_3D ( 'NONE', #37697, #61075, #19397 ) ;
#246094 = ORIENTED_EDGE ( 'NONE', *, *, #166734, .F. ) ;
#246095 = CARTESIAN_POINT ( 'NONE',  ( -20.85000000000000142, 36.65892442174935439, -249.5511627012433848 ) ) ;
#246096 = CARTESIAN_POINT ( 'NONE',  ( -22.39999999999999858, 65.09550114356427741, -243.3481044654562879 ) ) ;
#246097 = CARTESIAN_POINT ( 'NONE',  ( -13.40000000000000213, -8.279289321881350361, 11.02928932188134503 ) ) ;
#246098 = ORIENTED_EDGE ( 'NONE', *, *, #186253, .T. ) ;
#246099 = LINE ( 'NONE', #6178, #59390 ) ;
#246100 = ORIENTED_EDGE ( 'NONE', *, *, #242862, .T. ) ;
#246101 = CARTESIAN_POINT ( 'NONE',  ( -23.25000000000000000, 87.75000000001163869, -66.42310748452423752 ) ) ;
#246102 = CARTESIAN_POINT ( 'NONE',  ( -21.05000000000000071, 5.850000000011156942, -90.36750277572211587 ) ) ;
#246103 = CARTESIAN_POINT ( 'NONE',  ( -22.50000000000088463, 75.95463834342467635, -181.6736163187343038 ) ) ;
#246105 = ORIENTED_EDGE ( 'NONE', *, *, #213973, .T. ) ;
#246104 = FACE_OUTER_BOUND ( 'NONE', #97599, .T. ) ;
#246106 = TOROIDAL_SURFACE ( 'NONE', #71333, 7.791421356237316687, 0.1000000000000000056 ) ;
#246107 = DIRECTION ( 'NONE',  ( 0.000000000000000000, -7.026728003956683390E-15, 1.000000000000000000 ) ) ;
#246108 = CARTESIAN_POINT ( 'NONE',  ( 22.59999999999999432, 0.1000000000111554016, -122.3504291924552234 ) ) ;
#246109 = VERTEX_POINT ( 'NONE', #256755 ) ;
#246110 = EDGE_CURVE ( 'NONE', #20227, #149556, #80720, .T. ) ;
#246111 = CARTESIAN_POINT ( 'NONE',  ( -20.85000000000000142, 77.16412189325305349, -95.10825939895268277 ) ) ;
#246112 = CARTESIAN_POINT ( 'NONE',  ( -22.45437739390954945, -3.140208066727175673, -228.2318569518635059 ) ) ;
#246113 = ORIENTED_EDGE ( 'NONE', *, *, #173553, .T. ) ;
#246114 = CARTESIAN_POINT ( 'NONE',  ( -20.85000000000000142, 68.97833521811131163, -32.38954208262708079 ) ) ;
#246115 = AXIS2_PLACEMENT_3D ( 'NONE', #104935, #85373, #244480 ) ;
#246116 = ADVANCED_FACE ( 'NONE', ( #81987 ), #74969, .T. ) ;
#246117 = ORIENTED_EDGE ( 'NONE', *, *, #6134, .F. ) ;
#246119 = DIRECTION ( 'NONE',  ( -7.304098846218134667E-16, -1.000000000000000000, 0.000000000000000000 ) ) ;
#246118 = CIRCLE ( 'NONE', #233650, 0.6000000000000033085 ) ;
#246121 = EDGE_LOOP ( 'NONE', ( #241239, #178869, #41830, #65646 ) ) ;
#246120 = CARTESIAN_POINT ( 'NONE',  ( 18.39999999999997371, 11.47316190336247388, -24.25000000000001066 ) ) ;
#246124 = ORIENTED_EDGE ( 'NONE', *, *, #253354, .T. ) ;
#246123 = EDGE_LOOP ( 'NONE', ( #159818, #194942, #13591, #196993, #61183 ) ) ;
#246122 = FACE_OUTER_BOUND ( 'NONE', #240986, .T. ) ;
#246125 = LINE ( 'NONE', #145717, #73241 ) ;
#246126 = CARTESIAN_POINT ( 'NONE',  ( -21.14999999999999858, 64.27847795353595473, -247.1247091181747066 ) ) ;
#246128 = CARTESIAN_POINT ( 'NONE',  ( -16.92973740335364496, 9.992503814467408318, -20.90605903520226505 ) ) ;
#246127 = DIRECTION ( 'NONE',  ( -0.000000000000000000, -1.000000000000000000, -0.000000000000000000 ) ) ;
#246129 = ADVANCED_FACE ( 'NONE', ( #117306 ), #245280, .F. ) ;
#246130 = FACE_OUTER_BOUND ( 'NONE', #172410, .T. ) ;
#246131 = TOROIDAL_SURFACE ( 'NONE', #167053, 11.65000000000000036, 0.1000000000000000056 ) ;
#246132 = CARTESIAN_POINT ( 'NONE',  ( -22.50485643085239928, 25.96818459189811890, -254.4268134568224298 ) ) ;
#246133 = TOROIDAL_SURFACE ( 'NONE', #125509, 0.4000000000000003553, 0.1000000000000000056 ) ;
#246134 = DIRECTION ( 'NONE',  ( 1.000000000000000000, -0.000000000000000000, -0.000000000000000000 ) ) ;
#246136 = ORIENTED_EDGE ( 'NONE', *, *, #185297, .T. ) ;
#246135 = AXIS2_PLACEMENT_3D ( 'NONE', #111986, #166849, #208524 ) ;
#246137 = VERTEX_POINT ( 'NONE', #102843 ) ;
#246138 = DIRECTION ( 'NONE',  ( 0.000000000000000000, 0.000000000000000000, 1.000000000000000000 ) ) ;
#246140 = ORIENTED_EDGE ( 'NONE', *, *, #242464, .T. ) ;
#246139 = CARTESIAN_POINT ( 'NONE',  ( -21.52071067811865746, 68.22071067813125467, -191.1731074845243938 ) ) ;
#246141 = ORIENTED_EDGE ( 'NONE', *, *, #151713, .F. ) ;
#246142 = FACE_OUTER_BOUND ( 'NONE', #159010, .T. ) ;
#246143 = EDGE_LOOP ( 'NONE', ( #75187, #88449, #17453, #158398, #161098 ) ) ;
#246144 = CARTESIAN_POINT ( 'NONE',  ( -21.05000000000000426, 69.65527659592147813, -136.5378253410474940 ) ) ;
#246145 = ORIENTED_EDGE ( 'NONE', *, *, #130936, .T. ) ;
#246146 = AXIS2_PLACEMENT_3D ( 'NONE', #119083, #138602, #40854 ) ;
#246147 = CARTESIAN_POINT ( 'NONE',  ( -20.54999999999999716, -8.852780557335606204, -215.5675418792430946 ) ) ;
#246149 = ORIENTED_EDGE ( 'NONE', *, *, #8183, .T. ) ;
#246148 = ORIENTED_EDGE ( 'NONE', *, *, #145049, .T. ) ;
#246150 = ORIENTED_EDGE ( 'NONE', *, *, #83781, .F. ) ;
#246151 = CARTESIAN_POINT ( 'NONE',  ( -23.15000000000000213, 74.00000000001205080, -123.2984855617622060 ) ) ;
#246152 = ORIENTED_EDGE ( 'NONE', *, *, #55907, .F. ) ;
#246153 = VERTEX_POINT ( 'NONE', #3773 ) ;
#246154 = CARTESIAN_POINT ( 'NONE',  ( -20.09999999999999787, 4.645987002755569861, 21.91686199900910736 ) ) ;
#246155 = CARTESIAN_POINT ( 'NONE',  ( -18.59999999999999787, 74.83729825007462466, -195.5231074845243597 ) ) ;
#246157 = ORIENTED_EDGE ( 'NONE', *, *, #76768, .T. ) ;
#246156 = CARTESIAN_POINT ( 'NONE',  ( 18.59999999999999787, 70.10000000001163301, -59.30400771986794695 ) ) ;
#246158 = FACE_OUTER_BOUND ( 'NONE', #214337, .T. ) ;
#246159 = DIRECTION ( 'NONE',  ( -1.000000000000000000, -0.000000000000000000, 0.000000000000000000 ) ) ;
#246161 = VERTEX_POINT ( 'NONE', #37787 ) ;
#246160 = CYLINDRICAL_SURFACE ( 'NONE', #101527, 12.87499999999999112 ) ;
#246162 = DIRECTION ( 'NONE',  ( -2.915501640297153790E-16, 1.000000000000000000, 0.000000000000000000 ) ) ;
#246163 = EDGE_LOOP ( 'NONE', ( #82208, #235617, #17999, #201830 ) ) ;
#246164 = CARTESIAN_POINT ( 'NONE',  ( 11.60000000000000142, -8.250000000000003553, 15.00000000000000355 ) ) ;
#246165 = ORIENTED_EDGE ( 'NONE', *, *, #121271, .T. ) ;
#246167 = AXIS2_PLACEMENT_3D ( 'NONE', #135018, #35961, #214571 ) ;
#246166 = CARTESIAN_POINT ( 'NONE',  ( -21.05000000000000071, 18.63703040626447205, -226.6960388224909764 ) ) ;
#246168 = CARTESIAN_POINT ( 'NONE',  ( -16.89797118371380336, 30.29573403885543215, -234.8250098293310941 ) ) ;
#246169 = CIRCLE ( 'NONE', #8843, 0.1000000000000038081 ) ;
#246170 = CIRCLE ( 'NONE', #4719, 0.1000000000000054595 ) ;
#246171 = ADVANCED_FACE ( 'NONE', ( #162872 ), #18203, .T. ) ;
#246172 = VECTOR ( 'NONE', #51872, 1000.000000000000000 ) ;
#246173 = ORIENTED_EDGE ( 'NONE', *, *, #222194, .F. ) ;
#246175 = CARTESIAN_POINT ( 'NONE',  ( -21.14999999999994174, 74.16448838626247664, -47.52760213295649550 ) ) ;
#246174 = DIRECTION ( 'NONE',  ( 0.000000000000000000, 1.000000000000000000, 6.853228547068871147E-15 ) ) ;
#246176 = CARTESIAN_POINT ( 'NONE',  ( -23.25000000000000000, 6.933893972137497030, -137.7856458343736108 ) ) ;
#246177 = VECTOR ( 'NONE', #128257, 1000.000000000000000 ) ;
#246178 = ORIENTED_EDGE ( 'NONE', *, *, #238983, .F. ) ;
#246179 = VERTEX_POINT ( 'NONE', #19496 ) ;
#246180 = EDGE_CURVE ( 'NONE', #161272, #183810, #199691, .T. ) ;
#246181 = DIRECTION ( 'NONE',  ( 1.000000000000000000, 3.265361837132813093E-16, -0.000000000000000000 ) ) ;
#246182 = CARTESIAN_POINT ( 'NONE',  ( -18.59999999999999787, -1.835859311432481045, -78.50443916879852679 ) ) ;
#246183 = ORIENTED_EDGE ( 'NONE', *, *, #41763, .F. ) ;
#246184 = DIRECTION ( 'NONE',  ( -3.265361837132813093E-16, 1.000000000000000000, 0.000000000000000000 ) ) ;
#246185 = ORIENTED_EDGE ( 'NONE', *, *, #134829, .F. ) ;
#246186 = DIRECTION ( 'NONE',  ( 1.000000000000000000, 0.000000000000000000, 0.000000000000000000 ) ) ;
#246187 = VERTEX_POINT ( 'NONE', #109273 ) ;
#246188 = ADVANCED_FACE ( 'NONE', ( #188827 ), #8131, .F. ) ;
#246189 = CIRCLE ( 'NONE', #221036, 0.2000000000000057288 ) ;
#246190 = DIRECTION ( 'NONE',  ( 0.000000000000000000, -0.9654727137038715545, 0.2605042016806676242 ) ) ;
#246191 = PLANE ( 'NONE',  #182992 ) ;
#246192 = ORIENTED_EDGE ( 'NONE', *, *, #192144, .F. ) ;
#246193 = EDGE_CURVE ( 'NONE', #2821, #225035, #25916, .T. ) ;
#246194 = CARTESIAN_POINT ( 'NONE',  ( 18.49999999999999645, -9.480686695267806385, -207.9411151687578183 ) ) ;
#246195 = SHAPE_REPRESENTATION_RELATIONSHIP ( 'NONE' , 'NONE' ,  #205135, #144814 ) ;
#246196 = ORIENTED_EDGE ( 'NONE', *, *, #90030, .T. ) ;
#246197 = ORIENTED_EDGE ( 'NONE', *, *, #232993, .T. ) ;
#246198 = VERTEX_POINT ( 'NONE', #126278 ) ;
#246199 = FACE_OUTER_BOUND ( 'NONE', #194868, .T. ) ;
#246200 = DIRECTION ( 'NONE',  ( 0.000000000000000000, -0.8814952561687010579, 0.4721928772779996342 ) ) ;
#246201 = CARTESIAN_POINT ( 'NONE',  ( -18.50000000000000000, 9.250000000000001776, -21.15000000000000213 ) ) ;
#246202 = CARTESIAN_POINT ( 'NONE',  ( -20.85000000000000142, 36.65892442174935439, -249.5511627012433848 ) ) ;
#246203 = CARTESIAN_POINT ( 'NONE',  ( -16.89268316805465986, 9.951721813242182080, -20.85575247854553993 ) ) ;
#246204 = ADVANCED_FACE ( 'NONE', ( #224089 ), #45465, .F. ) ;
#246205 = CIRCLE ( 'NONE', #167126, 0.09999999999999999167 ) ;
#246207 = CARTESIAN_POINT ( 'NONE',  ( -21.93340585900942941, 1.115541036281197940E-11, -160.1758529778945501 ) ) ;
#246206 = CARTESIAN_POINT ( 'NONE',  ( -20.54999999999999716, 4.250000000011156409, -79.35000000000005116 ) ) ;
#246209 = ORIENTED_EDGE ( 'NONE', *, *, #3317, .F. ) ;
#246208 = DIRECTION ( 'NONE',  ( 1.000000000000000000, 0.000000000000000000, 0.000000000000000000 ) ) ;
#246210 = LINE ( 'NONE', #29762, #20598 ) ;
#246211 = ORIENTED_EDGE ( 'NONE', *, *, #195427, .T. ) ;
#246212 = DIRECTION ( 'NONE',  ( 0.000000000000000000, 0.000000000000000000, 1.000000000000000000 ) ) ;
#246213 = ORIENTED_EDGE ( 'NONE', *, *, #92629, .F. ) ;
#246214 = ORIENTED_EDGE ( 'NONE', *, *, #233362, .F. ) ;
#246215 = DIRECTION ( 'NONE',  ( 0.000000000000000000, -0.8103668758649578141, 0.5859227990963212784 ) ) ;
#246216 = VECTOR ( 'NONE', #228651, 1000.000000000000000 ) ;
#246217 = CARTESIAN_POINT ( 'NONE',  ( -23.15000000000000213, 73.40000000001228386, -156.7984855617622770 ) ) ;
#246218 = CARTESIAN_POINT ( 'NONE',  ( -16.87401514999239893, 66.05000000001153637, -48.74308949199231478 ) ) ;
#246219 = CARTESIAN_POINT ( 'NONE',  ( 21.14999999999999503, 76.00000000001267608, -203.5231074845243597 ) ) ;
#246220 = AXIS2_PLACEMENT_3D ( 'NONE', #58094, #196342, #38563 ) ;
#246221 = CARTESIAN_POINT ( 'NONE',  ( 18.50000000000000000, 85.40000000001190017, -96.02382180668539036 ) ) ;
#246222 = VECTOR ( 'NONE', #17261, 1000.000000000000000 ) ;
#246223 = ORIENTED_EDGE ( 'NONE', *, *, #81952, .F. ) ;
#246224 = ORIENTED_EDGE ( 'NONE', *, *, #187945, .T. ) ;
#246225 = CIRCLE ( 'NONE', #33883, 11.75000000000001066 ) ;
#246226 = DIRECTION ( 'NONE',  ( 0.000000000000000000, 0.8660254037844419273, -0.4999999999999942824 ) ) ;
#246227 = EDGE_LOOP ( 'NONE', ( #249306, #13613, #48970, #198733 ) ) ;
#246228 = CARTESIAN_POINT ( 'NONE',  ( -21.53551880898957904, 0.09896973458281840830, -127.2152022385837142 ) ) ;
#246229 = LINE ( 'NONE', #205808, #181814 ) ;
#246230 = ORIENTED_EDGE ( 'NONE', *, *, #153902, .T. ) ;
#246231 = DIRECTION ( 'NONE',  ( 1.000000000000000000, 0.000000000000000000, 0.000000000000000000 ) ) ;
#246232 = LINE ( 'NONE', #67588, #50503 ) ;
#246233 = CARTESIAN_POINT ( 'NONE',  ( 18.39999999999998082, 64.52683809664941350, -93.77310748452438816 ) ) ;
#246234 = ORIENTED_EDGE ( 'NONE', *, *, #40261, .F. ) ;
#246235 = LINE ( 'NONE', #46731, #12863 ) ;
#246236 = LINE ( 'NONE', #165421, #170921 ) ;
#246237 = CARTESIAN_POINT ( 'NONE',  ( 20.04142135623730070, 11.65000000001115943, -192.1499999999999488 ) ) ;
#246238 = LINE ( 'NONE', #8910, #25338 ) ;
#246239 = CARTESIAN_POINT ( 'NONE',  ( -18.39999999999999858, 85.51932773110434027, -96.05013110796491560 ) ) ;
#246240 = VECTOR ( 'NONE', #57418, 1000.000000000000114 ) ;
#246241 = DIRECTION ( 'NONE',  ( 0.000000000000000000, 1.000000000000000000, 6.982962677686266711E-15 ) ) ;
#246242 = AXIS2_PLACEMENT_3D ( 'NONE', #49456, #212397, #92418 ) ;
#246243 = ADVANCED_FACE ( 'NONE', ( #227956 ), #27221, .T. ) ;
#246244 = ORIENTED_EDGE ( 'NONE', *, *, #21274, .T. ) ;
#246245 = AXIS2_PLACEMENT_3D ( 'NONE', #131122, #191131, #9890 ) ;
#246246 = CARTESIAN_POINT ( 'NONE',  ( -21.93340585972176981, 68.67585297715999104, -136.5231074845243597 ) ) ;
#246247 = ORIENTED_EDGE ( 'NONE', *, *, #146286, .T. ) ;
#246249 = ADVANCED_FACE ( 'NONE', ( #186272 ), #125018, .T. ) ;
#246248 = AXIS2_PLACEMENT_3D ( 'NONE', #102305, #80176, #41114 ) ;
#246250 = CARTESIAN_POINT ( 'NONE',  ( -21.64999999999999858, 10.05000000001113847, -188.2499999999999716 ) ) ;
#246251 = CARTESIAN_POINT ( 'NONE',  ( 21.14999999999999858, -8.874060656858240748, -215.4698323230865640 ) ) ;
#246252 = CARTESIAN_POINT ( 'NONE',  ( -20.94999999999999929, 76.00000000001237765, -170.0231074845243597 ) ) ;
#246253 = LINE ( 'NONE', #67603, #77767 ) ;
#246254 = ORIENTED_EDGE ( 'NONE', *, *, #7219, .F. ) ;
#246255 = DIRECTION ( 'NONE',  ( 0.7071067811865475727, -0.7071067811865475727, 0.000000000000000000 ) ) ;
#246256 = CARTESIAN_POINT ( 'NONE',  ( -21.65000000000000213, 45.23934133962703186, -237.7629717664446787 ) ) ;
#246257 = EDGE_CURVE ( 'NONE', #112749, #81779, #204529, .T. ) ;
#246258 = EDGE_CURVE ( 'NONE', #104591, #199985, #16510, .T. ) ;
#246259 = CARTESIAN_POINT ( 'NONE',  ( 21.13736287352038445, 62.77635462851659298, -221.5399373006264625 ) ) ;
#246260 = AXIS2_PLACEMENT_3D ( 'NONE', #64430, #184357, #124407 ) ;
#246261 = CIRCLE ( 'NONE', #58783, 0.1000000000000028644 ) ;
#246262 = AXIS2_PLACEMENT_3D ( 'NONE', #40050, #122130, #183387 ) ;
#246263 = DIRECTION ( 'NONE',  ( -1.000000000000000000, 0.000000000000000000, 0.000000000000000000 ) ) ;
#246264 = AXIS2_PLACEMENT_3D ( 'NONE', #68961, #51912, #128918 ) ;
#246265 = ORIENTED_EDGE ( 'NONE', *, *, #74097, .F. ) ;
#246266 = ORIENTED_EDGE ( 'NONE', *, *, #102781, .F. ) ;
#246267 = CARTESIAN_POINT ( 'NONE',  ( -21.05000000000000426, 11.60000000001115872, -140.9282032302755852 ) ) ;
#246268 = PLANE ( 'NONE',  #200994 ) ;
#246269 = DIRECTION ( 'NONE',  ( 1.000000000000000000, 0.000000000000000000, 0.000000000000000000 ) ) ;
#246270 = DIRECTION ( 'NONE',  ( 2.694716079187273439E-16, 1.000000000000000000, 6.467318590049456648E-15 ) ) ;
#246271 = EDGE_CURVE ( 'NONE', #99793, #190048, #114908, .T. ) ;
#246272 = DIRECTION ( 'NONE',  ( -0.1538461538461613487, -0.4039696218774022629, 0.9017427047373168802 ) ) ;
#246273 = EDGE_CURVE ( 'NONE', #43801, #26579, #67595, .T. ) ;
#246274 = EDGE_LOOP ( 'NONE', ( #115564, #23640, #185247, #73026 ) ) ;
#246275 = DIRECTION ( 'NONE',  ( 1.000000000000000000, 0.000000000000000000, 0.000000000000000000 ) ) ;
#246276 = EDGE_CURVE ( 'NONE', #213320, #65963, #245642, .T. ) ;
#246277 = DIRECTION ( 'NONE',  ( 0.000000000000000000, -0.000000000000000000, -1.000000000000000000 ) ) ;
#246278 = VERTEX_POINT ( 'NONE', #85840 ) ;
#246279 = CARTESIAN_POINT ( 'NONE',  ( 21.14999999999999503, -3.187427350888460076, -228.3200064793908837 ) ) ;
#246280 = VERTEX_POINT ( 'NONE', #88415 ) ;
#246281 = ORIENTED_EDGE ( 'NONE', *, *, #61535, .T. ) ;
#246282 = EDGE_CURVE ( 'NONE', #165408, #239412, #78999, .T. ) ;
#246283 = ORIENTED_EDGE ( 'NONE', *, *, #28558, .T. ) ;
#246284 = ADVANCED_FACE ( 'NONE', ( #24654 ), #127574, .T. ) ;
#246285 = CARTESIAN_POINT ( 'NONE',  ( 20.95595012432476523, 10.60417921308728673, -74.59576933021817524 ) ) ;
#246286 = EDGE_CURVE ( 'NONE', #1657, #202553, #226658, .T. ) ;
#246287 = CYLINDRICAL_SURFACE ( 'NONE', #79887, 7.900000000000003908 ) ;
#246288 = FACE_OUTER_BOUND ( 'NONE', #126615, .T. ) ;
#246289 = CIRCLE ( 'NONE', #104777, 0.09999999999999892308 ) ;
#246290 = CARTESIAN_POINT ( 'NONE',  ( -21.07946286933444568, 69.67096268100424084, -103.0997913277807498 ) ) ;
#246291 = CARTESIAN_POINT ( 'NONE',  ( -23.25000000000000355, 11.75000000001113953, -180.1499999999999773 ) ) ;
#246292 = CARTESIAN_POINT ( 'NONE',  ( -20.64999999999999858, -6.688413578037177842, -212.5825622730469036 ) ) ;
#246293 = DIRECTION ( 'NONE',  ( -0.000000000000000000, 0.9770955615653313941, 0.2128009952263603954 ) ) ;
#246295 = DIRECTION ( 'NONE',  ( 0.000000000000000000, 0.8777080977375655291, -0.4791956752370622463 ) ) ;
#246294 = PLANE ( 'NONE',  #66058 ) ;
#246296 = CARTESIAN_POINT ( 'NONE',  ( -23.25000000000000355, 5.650000000011139001, -109.7500000000000426 ) ) ;
#246297 = CYLINDRICAL_SURFACE ( 'NONE', #218669, 0.09999999999999939493 ) ;
#246298 = DIRECTION ( 'NONE',  ( 0.000000000000000000, -0.8814952561688449428, 0.4721928772777310157 ) ) ;
#246299 = DIRECTION ( 'NONE',  ( 0.000000000000000000, 1.776356839400246520E-15, -1.000000000000000000 ) ) ;
#246300 = ORIENTED_EDGE ( 'NONE', *, *, #250588, .T. ) ;
#246301 = VERTEX_POINT ( 'NONE', #84543 ) ;
#246302 = DIRECTION ( 'NONE',  ( 0.000000000000000000, -0.9126074666063660468, -0.4088369013363524762 ) ) ;
#246303 = DIRECTION ( 'NONE',  ( 0.000000000000000000, -0.8068669527897506244, -0.5907332058516622242 ) ) ;
#246304 = LINE ( 'NONE', #29850, #145281 ) ;
#246305 = AXIS2_PLACEMENT_3D ( 'NONE', #181757, #142603, #78775 ) ;
#246306 = EDGE_CURVE ( 'NONE', #97650, #43089, #153928, .T. ) ;
#246307 = CYLINDRICAL_SURFACE ( 'NONE', #39533, 4.000000000000003553 ) ;
#246309 = EDGE_CURVE ( 'NONE', #215091, #26497, #150992, .T. ) ;
#246308 = DIRECTION ( 'NONE',  ( -0.000000000000000000, 0.1350103645451876666, 0.9908441862701600211 ) ) ;
#246310 = DIRECTION ( 'NONE',  ( 0.000000000000000000, 1.000000000000000000, 0.000000000000000000 ) ) ;
#246311 = EDGE_LOOP ( 'NONE', ( #134765, #161603, #213459, #171998, #4535, #34964, #180364, #189141 ) ) ;
#246312 = ORIENTED_EDGE ( 'NONE', *, *, #47048, .F. ) ;
#246313 = EDGE_CURVE ( 'NONE', #245711, #55613, #45724, .T. ) ;
#246314 = CARTESIAN_POINT ( 'NONE',  ( -21.65000000000000213, 9.950000000011140600, -113.2500000000000284 ) ) ;
#246315 = VERTEX_POINT ( 'NONE', #153603 ) ;
#246316 = DIRECTION ( 'NONE',  ( 1.000000000000000000, -8.034189347746079853E-16, 2.566115377699053192E-16 ) ) ;
#246317 = AXIS2_PLACEMENT_3D ( 'NONE', #140369, #257698, #141660 ) ;
#246318 = CIRCLE ( 'NONE', #121453, 0.4000000000000114575 ) ;
#246319 = DIRECTION ( 'NONE',  ( 1.000000000000000000, 0.000000000000000000, 0.000000000000000000 ) ) ;
#246320 = AXIS2_PLACEMENT_3D ( 'NONE', #115435, #247584, #68969 ) ;
#246321 = VERTEX_POINT ( 'NONE', #113140 ) ;
#246322 = LINE ( 'NONE', #84630, #43607 ) ;
#246323 = ORIENTED_EDGE ( 'NONE', *, *, #214884, .T. ) ;
#246324 = CARTESIAN_POINT ( 'NONE',  ( -16.87036670365549895, 60.78293754744167643, -221.1029176676855741 ) ) ;
#246325 = DIRECTION ( 'NONE',  ( 0.000000000000000000, -0.4088369013363281068, 0.9126074666063770380 ) ) ;
#246326 = CARTESIAN_POINT ( 'NONE',  ( -18.79999999999999716, 1.250000000000000000, 16.60000000000000142 ) ) ;
#246327 = EDGE_CURVE ( 'NONE', #51994, #205114, #93574, .T. ) ;
#246328 = CARTESIAN_POINT ( 'NONE',  ( -21.05000000000000071, 0.6869237119019852011, -212.7787591058053067 ) ) ;
#246329 = DIRECTION ( 'NONE',  ( 0.000000000000000000, 0.000000000000000000, -1.000000000000000000 ) ) ;
#246330 = CIRCLE ( 'NONE', #42321, 0.09999999999999939493 ) ;
#246331 = DIRECTION ( 'NONE',  ( 0.000000000000000000, 0.4088369013363783999, -0.9126074666063545004 ) ) ;
#246332 = FACE_OUTER_BOUND ( 'NONE', #24242, .T. ) ;
#246333 = EDGE_CURVE ( 'NONE', #16880, #194489, #145658, .T. ) ;
#246335 = ORIENTED_EDGE ( 'NONE', *, *, #66804, .F. ) ;
#246334 = DIRECTION ( 'NONE',  ( -0.000000000000000000, -0.9770955615653317272, -0.2128009952263598126 ) ) ;
#246337 = CARTESIAN_POINT ( 'NONE',  ( 23.14999999999999147, 1.115600667400684642E-11, -33.50000000000000000 ) ) ;
#246336 = LINE ( 'NONE', #66415, #53733 ) ;
#246338 = ORIENTED_EDGE ( 'NONE', *, *, #107267, .T. ) ;
#246340 = ORIENTED_EDGE ( 'NONE', *, *, #11708, .F. ) ;
#246339 = CARTESIAN_POINT ( 'NONE',  ( -18.59999999999999787, 1.115600667400684642E-11, -134.0000000000000284 ) ) ;
#246341 = VERTEX_POINT ( 'NONE', #92285 ) ;
#246342 = CARTESIAN_POINT ( 'NONE',  ( 22.57320508075688537, 64.35000000001268461, -203.5231074845244166 ) ) ;
#246343 = FACE_OUTER_BOUND ( 'NONE', #131158, .T. ) ;
#246344 = ADVANCED_FACE ( 'NONE', ( #152294 ), #173166, .T. ) ;
#246345 = EDGE_CURVE ( 'NONE', #139324, #8217, #41465, .T. ) ;
#246346 = CARTESIAN_POINT ( 'NONE',  ( 21.05000000000000071, 0.09779029132038138949, -127.7421853895184825 ) ) ;
#246347 = CARTESIAN_POINT ( 'NONE',  ( 21.97500000000000497, 14.02742277431099538, -219.5907614236512870 ) ) ;
#246348 = CARTESIAN_POINT ( 'NONE',  ( -20.64999999999999858, 19.98118924431957311, -235.6825596947570602 ) ) ;
#246349 = EDGE_CURVE ( 'NONE', #196020, #162055, #249729, .T. ) ;
#246350 = CARTESIAN_POINT ( 'NONE',  ( -18.40000000000000213, 23.60914413563410008, -229.5451841312037402 ) ) ;
#246351 = DIRECTION ( 'NONE',  ( 0.000000000000000000, 6.982962677686267499E-15, -1.000000000000000000 ) ) ;
#246352 = CARTESIAN_POINT ( 'NONE',  ( 20.94999999999999929, 1.115649653272650466E-11, -163.5000000000000284 ) ) ;
#246353 = AXIS2_PLACEMENT_3D ( 'NONE', #25083, #44624, #64184 ) ;
#246354 = AXIS2_PLACEMENT_3D ( 'NONE', #192394, #193684, #213220 ) ;
#246356 = AXIS2_PLACEMENT_3D ( 'NONE', #144243, #25612, #223787 ) ;
#246355 = CARTESIAN_POINT ( 'NONE',  ( -21.05000000000000071, 74.83729825007462466, -195.4231074845243654 ) ) ;
#246357 = ORIENTED_EDGE ( 'NONE', *, *, #14102, .T. ) ;
#246358 = ORIENTED_EDGE ( 'NONE', *, *, #201903, .T. ) ;
#246359 = CARTESIAN_POINT ( 'NONE',  ( -23.25000000000000355, 64.25000000001224976, -149.1731074845244507 ) ) ;
#246360 = EDGE_CURVE ( 'NONE', #257957, #251754, #251361, .T. ) ;
#246361 = ORIENTED_EDGE ( 'NONE', *, *, #5020, .F. ) ;
#246362 = DIRECTION ( 'NONE',  ( 0.000000000000000000, 0.1350103645451876666, -0.9908441862701600211 ) ) ;
#246364 = ADVANCED_FACE ( 'NONE', ( #169309 ), #74808, .F. ) ;
#246363 = ORIENTED_EDGE ( 'NONE', *, *, #79567, .T. ) ;
#246365 = DIRECTION ( 'NONE',  ( 0.000000000000000000, 0.9740678456249560746, -0.2262561206234139088 ) ) ;
#246366 = CARTESIAN_POINT ( 'NONE',  ( -21.04999999999994387, 67.85000000001119247, -25.52310748452479316 ) ) ;
#246367 = CARTESIAN_POINT ( 'NONE',  ( -22.44366136229477249, -2.469944097043066389, -189.6151238087248601 ) ) ;
#246368 = EDGE_CURVE ( 'NONE', #91747, #190272, #137293, .T. ) ;
#246369 = DIRECTION ( 'NONE',  ( 0.000000000000000000, 1.000000000000000000, -0.000000000000000000 ) ) ;
#246370 = CARTESIAN_POINT ( 'NONE',  ( 21.08804281139612868, 10.62183430185230826, -179.8499999673788068 ) ) ;
#246371 = ORIENTED_EDGE ( 'NONE', *, *, #245544, .T. ) ;
#246372 = CIRCLE ( 'NONE', #187936, 0.5000000000000004441 ) ;
#246373 = DIRECTION ( 'NONE',  ( -2.342056488767301376E-15, -0.3427706569149662763, 0.9394191166662954062 ) ) ;
#246374 = CARTESIAN_POINT ( 'NONE',  ( -16.94445028196807002, 51.64060657411747712, -231.8906364537310196 ) ) ;
#246375 = CARTESIAN_POINT ( 'NONE',  ( 18.45036689428354393, 85.49018414334042859, -62.51041165703842495 ) ) ;
#246376 = CARTESIAN_POINT ( 'NONE',  ( -20.64999999999999858, -8.999999999988846255, -43.39396912265245021 ) ) ;
#246378 = VERTEX_POINT ( 'NONE', #115709 ) ;
#246377 = EDGE_CURVE ( 'NONE', #83264, #220835, #72768, .T. ) ;
#246380 = DIRECTION ( 'NONE',  ( -0.000000000000000000, 6.982962677686266711E-15, -1.000000000000000000 ) ) ;
#246379 = CARTESIAN_POINT ( 'NONE',  ( 21.08376601933332495, 61.09374636974325767, -234.2566552461101708 ) ) ;
#246381 = ORIENTED_EDGE ( 'NONE', *, *, #46038, .T. ) ;
#246384 = ORIENTED_EDGE ( 'NONE', *, *, #230819, .F. ) ;
#246383 = CARTESIAN_POINT ( 'NONE',  ( -18.38204789744325396, 64.52049896284690078, -112.2731074845243739 ) ) ;
#246382 = DIRECTION ( 'NONE',  ( 0.000000000000000000, 0.3042567129659849434, 0.9525900758537926283 ) ) ;
#246385 = VERTEX_POINT ( 'NONE', #51859 ) ;
#246386 = CARTESIAN_POINT ( 'NONE',  ( -21.59142135623730852, 68.15000000001222702, -148.7731074845244166 ) ) ;
#246387 = CARTESIAN_POINT ( 'NONE',  ( -21.04999999999999716, 34.01597830783489940, -243.6159889436117965 ) ) ;
#246388 = EDGE_CURVE ( 'NONE', #243888, #88949, #214799, .T. ) ;
#246389 = LINE ( 'NONE', #147281, #141718 ) ;
#246390 = EDGE_LOOP ( 'NONE', ( #117189, #201595, #58548, #72577 ) ) ;
#246391 = DIRECTION ( 'NONE',  ( -0.000000000000000000, 6.982962677686266711E-15, -1.000000000000000000 ) ) ;
#246392 = VECTOR ( 'NONE', #204124, 1000.000000000000114 ) ;
#246393 = DIRECTION ( 'NONE',  ( 1.000000000000000000, 0.000000000000000000, 0.000000000000000000 ) ) ;
#246394 = ADVANCED_FACE ( 'NONE', ( #230534 ), #54443, .T. ) ;
#246396 = DIRECTION ( 'NONE',  ( 0.000000000000000000, 0.000000000000000000, 1.000000000000000000 ) ) ;
#246395 = DIRECTION ( 'NONE',  ( 0.000000000000000000, 5.329070518200686707E-15, 1.000000000000000000 ) ) ;
#246397 = EDGE_CURVE ( 'NONE', #49225, #88303, #237269, .T. ) ;
#246399 = ORIENTED_EDGE ( 'NONE', *, *, #214076, .F. ) ;
#246398 = LINE ( 'NONE', #71623, #76570 ) ;
#246400 = CIRCLE ( 'NONE', #171413, 0.09999999999998898659 ) ;
#246401 = ORIENTED_EDGE ( 'NONE', *, *, #178239, .F. ) ;
#246402 = CARTESIAN_POINT ( 'NONE',  ( -20.64999999999999858, 71.75000000001180922, -81.87310748452433984 ) ) ;
#246403 = CARTESIAN_POINT ( 'NONE',  ( -21.52071067811865746, 68.22071067813118361, -182.2731074845244166 ) ) ;
#246404 = CARTESIAN_POINT ( 'NONE',  ( -20.85000000000000142, -1.164121893230052995, -208.7148480855715604 ) ) ;
#246406 = ORIENTED_EDGE ( 'NONE', *, *, #152939, .F. ) ;
#246405 = VECTOR ( 'NONE', #71801, 1000.000000000000000 ) ;
#246407 = LINE ( 'NONE', #205994, #114505 ) ;
#246408 = CIRCLE ( 'NONE', #217338, 0.1999999999999987899 ) ;
#246410 = EDGE_CURVE ( 'NONE', #28434, #230635, #213513, .T. ) ;
#246409 = DIRECTION ( 'NONE',  ( 0.000000000000000000, 0.000000000000000000, 1.000000000000000000 ) ) ;
#246411 = DIRECTION ( 'NONE',  ( 1.000000000000000000, 0.000000000000000000, 0.000000000000000000 ) ) ;
#246412 = VERTEX_POINT ( 'NONE', #114427 ) ;
#246413 = SPHERICAL_SURFACE ( 'NONE', #162724, 0.1000000000000000056 ) ;
#246414 = AXIS2_PLACEMENT_3D ( 'NONE', #35801, #138688, #37094 ) ;
#246415 = VERTEX_POINT ( 'NONE', #193975 ) ;
#246416 = AXIS2_PLACEMENT_3D ( 'NONE', #212056, #72548, #68685 ) ;
#246417 = DIRECTION ( 'NONE',  ( -0.000000000000000000, 0.9371753822965236402, -0.3488585713686349066 ) ) ;
#246418 = DIRECTION ( 'NONE',  ( 1.000000000000000000, -0.000000000000000000, -0.000000000000000000 ) ) ;
#246419 = TOROIDAL_SURFACE ( 'NONE', #21568, 0.2000000000000000111, 0.1000000000000000056 ) ;
#246420 = VERTEX_POINT ( 'NONE', #195270 ) ;
#246421 = ORIENTED_EDGE ( 'NONE', *, *, #161292, .T. ) ;
#246422 = AXIS2_PLACEMENT_3D ( 'NONE', #68916, #192699, #32371 ) ;
#246423 = LINE ( 'NONE', #229430, #187498 ) ;
#246424 = EDGE_CURVE ( 'NONE', #169820, #215622, #16624, .T. ) ;
#246425 = ORIENTED_EDGE ( 'NONE', *, *, #126464, .F. ) ;
#246427 = ORIENTED_EDGE ( 'NONE', *, *, #158679, .F. ) ;
#246426 = DIRECTION ( 'NONE',  ( -1.000000000000000000, 3.265361837132813093E-16, 2.280189983783949500E-30 ) ) ;
#246428 = ORIENTED_EDGE ( 'NONE', *, *, #85473, .F. ) ;
#246430 = EDGE_LOOP ( 'NONE', ( #145699, #40070, #147870 ) ) ;
#246429 = EDGE_LOOP ( 'NONE', ( #241806, #30282, #42195 ) ) ;
#246431 = ORIENTED_EDGE ( 'NONE', *, *, #250256, .T. ) ;
#246432 = DIRECTION ( 'NONE',  ( -1.000000000000000000, 0.000000000000000000, 0.000000000000000000 ) ) ;
#246433 = EDGE_CURVE ( 'NONE', #33939, #54754, #12423, .T. ) ;
#246434 = AXIS2_PLACEMENT_3D ( 'NONE', #256191, #37232, #228037 ) ;
#246435 = CIRCLE ( 'NONE', #208841, 0.09999999999998898659 ) ;
#246437 = B_SPLINE_CURVE_WITH_KNOTS ( 'NONE', 3,
 ( #214922, #178396, #252755, #35047, #37590, #174576, #194102 ),
 .UNSPECIFIED., .F., .F.,
 ( 4, 3, 4 ),
 ( 0.000000000000000000, 0.0007844235214594265501, 0.001767853679404345936 ),
 .UNSPECIFIED. ) ;
#246436 = DIRECTION ( 'NONE',  ( -1.000000000000000000, -1.836970198721029934E-16, -3.186635328391151676E-31 ) ) ;
#246439 = DIRECTION ( 'NONE',  ( 0.000000000000000000, 0.000000000000000000, -1.000000000000000000 ) ) ;
#246438 = AXIS2_PLACEMENT_3D ( 'NONE', #146131, #224380, #167024 ) ;
#246440 = ORIENTED_EDGE ( 'NONE', *, *, #235597, .F. ) ;
#246441 = ORIENTED_EDGE ( 'NONE', *, *, #81939, .F. ) ;
#246442 = CARTESIAN_POINT ( 'NONE',  ( -23.25000000000000000, 43.21392023178790964, -245.1418509714632421 ) ) ;
#246444 = ORIENTED_EDGE ( 'NONE', *, *, #97213, .F. ) ;
#246443 = DIRECTION ( 'NONE',  ( -0.000000000000000000, 1.000000000000000000, 8.717686153663073805E-15 ) ) ;
#246445 = DIRECTION ( 'NONE',  ( 0.000000000000000000, -0.8814952561688430555, 0.4721928772777346239 ) ) ;
#246447 = ORIENTED_EDGE ( 'NONE', *, *, #206338, .F. ) ;
#246446 = CARTESIAN_POINT ( 'NONE',  ( -20.85000000000000142, 77.83585931145600512, -158.4186683157258244 ) ) ;
#246448 = ORIENTED_EDGE ( 'NONE', *, *, #47955, .T. ) ;
#246449 = FACE_OUTER_BOUND ( 'NONE', #123827, .T. ) ;
#246450 = ORIENTED_EDGE ( 'NONE', *, *, #247196, .F. ) ;
#246451 = CARTESIAN_POINT ( 'NONE',  ( 20.94999999999999574, -1.162701749938009677, -8.099999999999999645 ) ) ;
#246452 = CARTESIAN_POINT ( 'NONE',  ( -23.49999999999994316, 77.26165318615413469, -44.00978271863746016 ) ) ;
#246453 = AXIS2_PLACEMENT_3D ( 'NONE', #58859, #208025, #29408 ) ;
#246455 = VERTEX_POINT ( 'NONE', #238208 ) ;
#246454 = ORIENTED_EDGE ( 'NONE', *, *, #190956, .T. ) ;
#246456 = ORIENTED_EDGE ( 'NONE', *, *, #66069, .F. ) ;
#246457 = CARTESIAN_POINT ( 'NONE',  ( 20.94999999999999574, 1.835341550235569663, -179.0551512925629538 ) ) ;
#246458 = ORIENTED_EDGE ( 'NONE', *, *, #219532, .T. ) ;
#246459 = EDGE_LOOP ( 'NONE', ( #179770, #129, #90362, #88091 ) ) ;
#246460 = CARTESIAN_POINT ( 'NONE',  ( 20.94999999999999574, 74.26374286841418382, -57.95445515550683524 ) ) ;
#246462 = ORIENTED_EDGE ( 'NONE', *, *, #204426, .T. ) ;
#246461 = DIRECTION ( 'NONE',  ( 0.000000000000000000, 1.000000000000000000, 0.000000000000000000 ) ) ;
#246463 = DIRECTION ( 'NONE',  ( 1.000000000000000000, -3.265361837132813093E-16, -2.280189983783949500E-30 ) ) ;
#246465 = CARTESIAN_POINT ( 'NONE',  ( 18.49999999999999289, 65.79142135625006915, -215.2731074845244450 ) ) ;
#246464 = FACE_OUTER_BOUND ( 'NONE', #198989, .T. ) ;
#246466 = CARTESIAN_POINT ( 'NONE',  ( 18.42595409746872903, 85.49999981257734305, -196.5237451327744225 ) ) ;
#246467 = CARTESIAN_POINT ( 'NONE',  ( -18.36973785203556275, 11.47550320049537476, -191.7499999999999716 ) ) ;
#246468 = ORIENTED_EDGE ( 'NONE', *, *, #227116, .T. ) ;
#246469 = EDGE_CURVE ( 'NONE', #58778, #150130, #224774, .T. ) ;
#246470 = VERTEX_POINT ( 'NONE', #140387 ) ;
#246471 = DIRECTION ( 'NONE',  ( 0.000000000000000000, -0.4930308989874653269, -0.8700118002898649117 ) ) ;
#246472 = DIRECTION ( 'NONE',  ( 1.000000000000000000, 0.000000000000000000, 0.000000000000000000 ) ) ;
#246473 = ORIENTED_EDGE ( 'NONE', *, *, #100, .F. ) ;
#246474 = CIRCLE ( 'NONE', #238086, 0.09999999999999939493 ) ;
#246475 = DIRECTION ( 'NONE',  ( -4.239556034732056743E-17, 0.1298341882520022694, 0.9915357197604853789 ) ) ;
#246476 = ORIENTED_EDGE ( 'NONE', *, *, #60833, .T. ) ;
#246477 = ORIENTED_EDGE ( 'NONE', *, *, #204859, .F. ) ;
#246478 = EDGE_CURVE ( 'NONE', #179371, #92785, #141393, .T. ) ;
#246479 = CARTESIAN_POINT ( 'NONE',  ( -21.05000000000000071, 64.35000000001264198, -196.7392418215462726 ) ) ;
#246480 = DIRECTION ( 'NONE',  ( 1.000000000000000000, 0.000000000000000000, 0.000000000000000000 ) ) ;
#246481 = ORIENTED_EDGE ( 'NONE', *, *, #253871, .F. ) ;
#246482 = DIRECTION ( 'NONE',  ( -1.000000000000000000, 0.000000000000000000, -0.000000000000000000 ) ) ;
#246483 = CARTESIAN_POINT ( 'NONE',  ( 21.08832698747859169, 8.775364393428372267, -112.7287174664641753 ) ) ;
#246484 = ORIENTED_EDGE ( 'NONE', *, *, #173934, .T. ) ;
#246485 = CARTESIAN_POINT ( 'NONE',  ( -23.39999999999994529, 83.88667523412387084, -34.67399920730211704 ) ) ;
#246486 = FACE_OUTER_BOUND ( 'NONE', #132673, .T. ) ;
#246488 = CARTESIAN_POINT ( 'NONE',  ( -20.94999999999999929, 61.95000000001194707, -108.5368025552853197 ) ) ;
#246487 = LINE ( 'NONE', #9167, #128104 ) ;
#246489 = EDGE_CURVE ( 'NONE', #33295, #176263, #208052, .T. ) ;
#246490 = CARTESIAN_POINT ( 'NONE',  ( -17.11825945287481687, 10.05000000001113847, -87.85000000000003695 ) ) ;
#246491 = DIRECTION ( 'NONE',  ( 1.000000000000000000, 0.000000000000000000, 0.000000000000000000 ) ) ;
#246492 = DIRECTION ( 'NONE',  ( 1.000000000000000000, 0.000000000000000000, 0.000000000000000000 ) ) ;
#246493 = LINE ( 'NONE', #249085, #61813 ) ;
#246494 = AXIS2_PLACEMENT_3D ( 'NONE', #61192, #164154, #140726 ) ;
#246495 = ADVANCED_FACE ( 'NONE', ( #77849 ), #62156, .T. ) ;
#246496 = VERTEX_POINT ( 'NONE', #201657 ) ;
#246497 = CIRCLE ( 'NONE', #154386, 0.09999999999999939493 ) ;
#246499 = VERTEX_POINT ( 'NONE', #235641 ) ;
#246498 = ORIENTED_EDGE ( 'NONE', *, *, #121247, .F. ) ;
#246500 = ORIENTED_EDGE ( 'NONE', *, *, #56966, .T. ) ;
#246501 = DIRECTION ( 'NONE',  ( 0.000000000000000000, -1.000000000000000000, 0.000000000000000000 ) ) ;
#246502 = CARTESIAN_POINT ( 'NONE',  ( -18.69999999999999929, 7.973296578895943121, 1.410778198689827345 ) ) ;
#246503 = ADVANCED_FACE ( 'NONE', ( #119578 ), #20477, .T. ) ;
#246505 = CARTESIAN_POINT ( 'NONE',  ( -15.70407651835961005, 9.355806591630130953, -16.29110253154617283 ) ) ;
#246504 = DIRECTION ( 'NONE',  ( 1.000000000000000000, 0.000000000000000000, 0.000000000000000000 ) ) ;
#246506 = CARTESIAN_POINT ( 'NONE',  ( -21.08376601933334271, 75.93622398908230764, -142.8650547558000312 ) ) ;
#246507 = VERTEX_POINT ( 'NONE', #101223 ) ;
#246508 = CARTESIAN_POINT ( 'NONE',  ( 23.14999999999999503, 53.37395138337728895, -234.8857996415767104 ) ) ;
#246509 = EDGE_CURVE ( 'NONE', #109031, #204739, #49813, .T. ) ;
#246511 = AXIS2_PLACEMENT_3D ( 'NONE', #198985, #58168, #179445 ) ;
#246510 = CARTESIAN_POINT ( 'NONE',  ( -16.81744102076749314, 66.05000000001187743, -90.37310748452438247 ) ) ;
#246512 = LINE ( 'NONE', #91305, #70921 ) ;
#246513 = ORIENTED_EDGE ( 'NONE', *, *, #216786, .T. ) ;
#246514 = CARTESIAN_POINT ( 'NONE',  ( -18.59999999999999787, 1.115600667400684642E-11, -167.5000000000000284 ) ) ;
#246515 = DIRECTION ( 'NONE',  ( 0.000000000000000000, -6.982962677686266711E-15, 1.000000000000000000 ) ) ;
#246516 = ORIENTED_EDGE ( 'NONE', *, *, #213629, .F. ) ;
#246517 = ORIENTED_EDGE ( 'NONE', *, *, #176559, .T. ) ;
#246518 = CARTESIAN_POINT ( 'NONE',  ( -23.15000000000000213, -11.64999999998884483, -63.89999999999999858 ) ) ;
#246519 = LINE ( 'NONE', #48322, #256070 ) ;
#246520 = FACE_OUTER_BOUND ( 'NONE', #249194, .T. ) ;
#246521 = CARTESIAN_POINT ( 'NONE',  ( 20.94999999999999574, 43.35747728126469980, -245.1805918474304917 ) ) ;
#246522 = LINE ( 'NONE', #129160, #31821 ) ;
#246523 = FACE_OUTER_BOUND ( 'NONE', #114507, .T. ) ;
#246524 = ORIENTED_EDGE ( 'NONE', *, *, #62845, .F. ) ;
#246525 = CARTESIAN_POINT ( 'NONE',  ( -20.64999999999999858, 7.150000000000000355, -12.34999999999999964 ) ) ;
#246527 = EDGE_CURVE ( 'NONE', #190040, #138100, #83087, .T. ) ;
#246526 = DIRECTION ( 'NONE',  ( 0.7071359030027870585, -0.6452843503173838480, -0.2890794387705646895 ) ) ;
#246530 = CARTESIAN_POINT ( 'NONE',  ( -18.59999999999999787, 5.341242990002807112, -57.19334979351202719 ) ) ;
#246529 = AXIS2_PLACEMENT_3D ( 'NONE', #106831, #142117, #140845 ) ;
#246528 = DIRECTION ( 'NONE',  ( -3.265361837132812600E-16, 0.4721928772777346239, 0.8814952561688430555 ) ) ;
#246532 = DIRECTION ( 'NONE',  ( -0.7071067811865460184, -0.6824534298470606997, 0.1850873201761399356 ) ) ;
#246531 = AXIS2_PLACEMENT_3D ( 'NONE', #250773, #31769, #248217 ) ;
#246533 = CARTESIAN_POINT ( 'NONE',  ( -16.87331047859649757, 66.05000000001153637, -48.67310748452439384 ) ) ;
#246534 = CARTESIAN_POINT ( 'NONE',  ( -20.94999999999999929, 77.83534155023646406, -124.9679561919612922 ) ) ;
#246535 = FACE_OUTER_BOUND ( 'NONE', #203445, .T. ) ;
#246537 = ORIENTED_EDGE ( 'NONE', *, *, #198539, .T. ) ;
#246536 = CARTESIAN_POINT ( 'NONE',  ( 22.47007471830799474, 29.61294623328926789, -252.7076741202934613 ) ) ;
#246538 = EDGE_CURVE ( 'NONE', #63066, #85197, #187382, .T. ) ;
#246539 = EDGE_CURVE ( 'NONE', #82879, #126714, #50006, .T. ) ;
#246540 = AXIS2_PLACEMENT_3D ( 'NONE', #29515, #188549, #115426 ) ;
#246541 = CARTESIAN_POINT ( 'NONE',  ( -18.40000000000000213, 10.68101405709484197, -223.4922417449319028 ) ) ;
#246542 = ADVANCED_FACE ( 'NONE', ( #136530 ), #118283, .T. ) ;
#246543 = EDGE_LOOP ( 'NONE', ( #108563, #128038, #109681 ) ) ;
#246544 = TOROIDAL_SURFACE ( 'NONE', #109164, 11.65000000000000036, 0.1000000000000000056 ) ;
#246545 = ADVANCED_FACE ( 'NONE', ( #98663 ), #159995, .F. ) ;
#246546 = DIRECTION ( 'NONE',  ( 0.000000000000000000, 0.000000000000000000, -1.000000000000000000 ) ) ;
#246547 = CARTESIAN_POINT ( 'NONE',  ( -21.05000000000000426, -0.09999999998884340213, -94.02293297887531764 ) ) ;
#246548 = CARTESIAN_POINT ( 'NONE',  ( -18.50000000000000000, -1.162701749926853712, -142.1000000000000227 ) ) ;
#246549 = ORIENTED_EDGE ( 'NONE', *, *, #129180, .T. ) ;
#246550 = DIRECTION ( 'NONE',  ( 0.000000000000000000, 6.982962677686267499E-15, -1.000000000000000000 ) ) ;
#246552 = ORIENTED_EDGE ( 'NONE', *, *, #63541, .F. ) ;
#246551 = CARTESIAN_POINT ( 'NONE',  ( -16.80070461187835562, 9.950000000011328893, -188.3530361708423868 ) ) ;
#246553 = LINE ( 'NONE', #147467, #163204 ) ;
#246554 = AXIS2_PLACEMENT_3D ( 'NONE', #118505, #79338, #136750 ) ;
#246555 = EDGE_CURVE ( 'NONE', #97103, #178186, #224943, .T. ) ;
#246556 = DIRECTION ( 'NONE',  ( 0.7071067811865463515, -0.7071067811865487940, 4.930380657631324879E-32 ) ) ;
#246557 = VERTEX_POINT ( 'NONE', #19170 ) ;
#246558 = DIRECTION ( 'NONE',  ( 0.000000000000000000, 0.2617529984165044565, 0.9651348961777151958 ) ) ;
#246559 = CIRCLE ( 'NONE', #75880, 0.09999999999998898659 ) ;
#246560 = EDGE_CURVE ( 'NONE', #249313, #102466, #104150, .T. ) ;
#246561 = CARTESIAN_POINT ( 'NONE',  ( 0.000000000000000000, 0.000000000000000000, 0.000000000000000000 ) ) ;
#246562 = CARTESIAN_POINT ( 'NONE',  ( -21.05000000000000071, 69.45934304831089889, -136.4231074845243654 ) ) ;
#246563 = ADVANCED_FACE ( 'NONE', ( #81670 ), #59544, .F. ) ;
#246564 = DIRECTION ( 'NONE',  ( -1.000000000000000000, 0.000000000000000000, -0.000000000000000000 ) ) ;
#246565 = DIRECTION ( 'NONE',  ( 0.000000000000000000, 0.7049548389605068133, -0.7092521942342977503 ) ) ;
#246566 = EDGE_LOOP ( 'NONE', ( #38649, #242890, #119564 ) ) ;
#246567 = CIRCLE ( 'NONE', #125941, 0.09999999999998898659 ) ;
#246568 = DIRECTION ( 'NONE',  ( 0.000000000000000000, 0.9126074666063660468, 0.4088369013363524762 ) ) ;
#246569 = DIRECTION ( 'NONE',  ( -1.000000000000000000, 0.000000000000000000, 0.000000000000000000 ) ) ;
#246570 = AXIS2_PLACEMENT_3D ( 'NONE', #54311, #34798, #184218 ) ;
#246571 = SPHERICAL_SURFACE ( 'NONE', #97261, 0.1000000000000000056 ) ;
#246572 = AXIS2_PLACEMENT_3D ( 'NONE', #80747, #198144, #42931 ) ;
#246573 = EDGE_CURVE ( 'NONE', #6683, #136089, #40052, .T. ) ;
#246574 = ORIENTED_EDGE ( 'NONE', *, *, #85505, .T. ) ;
#246575 = EDGE_LOOP ( 'NONE', ( #257999, #210951, #211392, #251007 ) ) ;
#246576 = EDGE_CURVE ( 'NONE', #45783, #78170, #240792, .T. ) ;
#246578 = CIRCLE ( 'NONE', #88147, 0.09999999999999491240 ) ;
#246577 = CARTESIAN_POINT ( 'NONE',  ( 23.25000000000000000, 87.75000000001192291, -106.1231074845242262 ) ) ;
#246580 = AXIS2_PLACEMENT_3D ( 'NONE', #207455, #163188, #48360 ) ;
#246579 = LINE ( 'NONE', #229599, #69647 ) ;
#246581 = DIRECTION ( 'NONE',  ( 0.000000000000000000, 0.9126074666063660468, 0.4088369013363524762 ) ) ;
#246582 = DIRECTION ( 'NONE',  ( -1.000000000000000000, 0.000000000000000000, -0.000000000000000000 ) ) ;
#246583 = CARTESIAN_POINT ( 'NONE',  ( 21.11345278033253692, 8.882122073382257454, -146.2460221707567030 ) ) ;
#246585 = DIRECTION ( 'NONE',  ( 0.000000000000000000, 0.000000000000000000, 1.000000000000000000 ) ) ;
#246584 = DIRECTION ( 'NONE',  ( 0.000000000000000000, -0.9126074666063770380, -0.4088369013363281068 ) ) ;
#246586 = CARTESIAN_POINT ( 'NONE',  ( 20.85000000000000142, 17.06838326776701109, -224.6250846885016870 ) ) ;
#246587 = CARTESIAN_POINT ( 'NONE',  ( -20.85000000000000142, 68.97833521811159585, -65.78954208262706516 ) ) ;
#246589 = DIRECTION ( 'NONE',  ( 0.000000000000000000, 1.000000000000000000, 0.000000000000000000 ) ) ;
#246588 = TOROIDAL_SURFACE ( 'NONE', #67527, 11.65000000000000036, 0.1000000000000000056 ) ;
#246590 = CARTESIAN_POINT ( 'NONE',  ( -20.94999999999999929, -4.656943609564680564, -233.1535107627236414 ) ) ;
#246592 = EDGE_LOOP ( 'NONE', ( #253859, #141868, #206096, #9333 ) ) ;
#246591 = DIRECTION ( 'NONE',  ( 0.000000000000000000, 0.5273008465188072647, -0.8496786552930167824 ) ) ;
#246593 = FACE_OUTER_BOUND ( 'NONE', #239634, .T. ) ;
#246594 = CARTESIAN_POINT ( 'NONE',  ( -23.25000000000000355, 60.04939757144280321, -224.3231863825903076 ) ) ;
#246596 = DIRECTION ( 'NONE',  ( 0.000000000000000000, 1.000000000000000000, -0.000000000000000000 ) ) ;
#246595 = CARTESIAN_POINT ( 'NONE',  ( 21.14999999999999858, 64.01960172407876826, -222.2915665888316141 ) ) ;
#246597 = VECTOR ( 'NONE', #202950, 1000.000000000000227 ) ;
#246598 = ADVANCED_FACE ( 'NONE', ( #8597 ), #12606, .T. ) ;
#246599 = ORIENTED_EDGE ( 'NONE', *, *, #56297, .F. ) ;
#246600 = FACE_OUTER_BOUND ( 'NONE', #17007, .T. ) ;
#246602 = EDGE_CURVE ( 'NONE', #242014, #218485, #33470, .T. ) ;
#246601 = DIRECTION ( 'NONE',  ( 0.000000000000000000, 0.9654727137038726648, -0.2605042016806632943 ) ) ;
#246603 = DIRECTION ( 'NONE',  ( 0.000000000000000000, 0.000000000000000000, -1.000000000000000000 ) ) ;
#246604 = DIRECTION ( 'NONE',  ( -0.000000000000000000, 0.8814952561688430555, -0.4721928772777346239 ) ) ;
#246606 = DIRECTION ( 'NONE',  ( 1.000000000000000000, -0.000000000000000000, -0.000000000000000000 ) ) ;
#246605 = CIRCLE ( 'NONE', #179987, 0.09999999999998898659 ) ;
#246607 = ORIENTED_EDGE ( 'NONE', *, *, #103123, .F. ) ;
#246608 = VERTEX_POINT ( 'NONE', #25601 ) ;
#246609 = EDGE_CURVE ( 'NONE', #172291, #111426, #8331, .T. ) ;
#246610 = CARTESIAN_POINT ( 'NONE',  ( -21.05000000000000071, 74.26374286841466699, -124.9544551555068068 ) ) ;
#246611 = EDGE_LOOP ( 'NONE', ( #77466, #139677, #95184, #10331 ) ) ;
#246612 = CARTESIAN_POINT ( 'NONE',  ( 21.05000000000000071, 65.51556651037016366, -95.56630168303246364 ) ) ;
#246613 = EDGE_LOOP ( 'NONE', ( #160537, #101000, #212166, #40584 ) ) ;
#246614 = AXIS2_PLACEMENT_3D ( 'NONE', #140134, #103571, #25372 ) ;
#246615 = CYLINDRICAL_SURFACE ( 'NONE', #189452, 0.09999999999999911737 ) ;
#246616 = FACE_OUTER_BOUND ( 'NONE', #41543, .T. ) ;
#246617 = CARTESIAN_POINT ( 'NONE',  ( -23.25000000000000355, 11.75000000001113953, -176.7499999999999716 ) ) ;
#246618 = ORIENTED_EDGE ( 'NONE', *, *, #64339, .F. ) ;
#246619 =( BOUNDED_SURFACE ( )  B_SPLINE_SURFACE ( 3, 2, ( 
 ( #80212, #116814, #39870 ),
 ( #235462, #56801, #21577 ),
 ( #180642, #217173, #215886 ),
 ( #197622, #37295, #178090 ) ),
 .UNSPECIFIED., .F., .F., .F. ) 
 B_SPLINE_SURFACE_WITH_KNOTS ( ( 4, 4 ),
 ( 3, 3 ),
 ( 0.3000847527772381729, 0.5552748953338751958 ),
 ( 0.000000000000000000, 1.000000000000000000 ),
 .UNSPECIFIED. ) 
 GEOMETRIC_REPRESENTATION_ITEM ( )  RATIONAL_B_SPLINE_SURFACE ( (
 ( 1.000000000000000000, 0.9152888060719349683, 1.000000000000000000),
 ( 1.000000000000000000, 0.9104333467450257400, 1.000000000000000000),
 ( 1.000000000000000000, 0.9035312726220622315, 1.000000000000000000),
 ( 1.000000000000000000, 0.8946697475932153809, 1.000000000000000000) ) ) 
 REPRESENTATION_ITEM ( '' )  SURFACE ( )  );
#246620 = PLANE ( 'NONE',  #124502 ) ;
#246621 = CARTESIAN_POINT ( 'NONE',  ( -21.05000000000000071, 0.09779029131994770863, -161.2421853895238542 ) ) ;
#246622 = EDGE_CURVE ( 'NONE', #56206, #104197, #202938, .T. ) ;
#246623 = DIRECTION ( 'NONE',  ( 0.000000000000000000, 6.769652589177795712E-15, -1.000000000000000000 ) ) ;
#246624 = CARTESIAN_POINT ( 'NONE',  ( -11.60000000000000320, -8.279289321881348584, 18.97071067811866030 ) ) ;
#246625 = DIRECTION ( 'NONE',  ( 0.000000000000000000, 6.982962677686266711E-15, -1.000000000000000000 ) ) ;
#246626 = FACE_OUTER_BOUND ( 'NONE', #172970, .T. ) ;
#246627 = ADVANCED_FACE ( 'NONE', ( #102518 ), #205497, .T. ) ;
#246628 = ORIENTED_EDGE ( 'NONE', *, *, #49141, .T. ) ;
#246629 = AXIS2_PLACEMENT_3D ( 'NONE', #106989, #31359, #150008 ) ;
#246631 = CARTESIAN_POINT ( 'NONE',  ( -17.22361732159832215, 10.34515565861359221, -44.87078452586714405 ) ) ;
#246630 = CARTESIAN_POINT ( 'NONE',  ( -16.94225986326250677, 66.05000000001207638, -123.5763881089164755 ) ) ;
#246632 = EDGE_LOOP ( 'NONE', ( #60382, #149724, #213471, #139519 ) ) ;
#246634 = VERTEX_POINT ( 'NONE', #106385 ) ;
#246633 = DIRECTION ( 'NONE',  ( 0.000000000000000000, 0.000000000000000000, -1.000000000000000000 ) ) ;
#246635 = EDGE_LOOP ( 'NONE', ( #224799, #236202, #256345, #17590 ) ) ;
#246636 = PLANE ( 'NONE',  #219728 ) ;
#246637 = CARTESIAN_POINT ( 'NONE',  ( -18.50000000000000000, 13.63658454968486389, -219.6758818217417968 ) ) ;
#246638 =( BOUNDED_SURFACE ( )  B_SPLINE_SURFACE ( 3, 2, ( 
 ( #231839, #12802, #153622 ),
 ( #55704, #193996, #136549 ),
 ( #214816, #234375, #217369 ),
 ( #17893, #233136, #53181 ) ),
 .UNSPECIFIED., .F., .F., .F. ) 
 B_SPLINE_SURFACE_WITH_KNOTS ( ( 4, 4 ),
 ( 3, 3 ),
 ( 3.658908243880847788, 4.712388980384689674 ),
 ( 0.000000000000000000, 1.000000000000000000 ),
 .UNSPECIFIED. ) 
 GEOMETRIC_REPRESENTATION_ITEM ( )  RATIONAL_B_SPLINE_SURFACE ( (
 ( 1.000000000000000000, 0.8984936768950640973, 1.000000000000000000),
 ( 1.000000000000000000, 0.8646876308616029405, 1.000000000000000000),
 ( 1.000000000000000000, 0.7953136715913016186, 1.000000000000000000),
 ( 1.000000000000000000, 0.7071067811865475727, 1.000000000000000000) ) ) 
 REPRESENTATION_ITEM ( '' )  SURFACE ( )  );
#246639 = CARTESIAN_POINT ( 'NONE',  ( -21.64999999999999858, 7.350000000011155166, -79.35000000000005116 ) ) ;
#246640 = CARTESIAN_POINT ( 'NONE',  ( 21.05000000000000071, 65.27628318601242086, -128.9287082486403051 ) ) ;
#246641 = ORIENTED_EDGE ( 'NONE', *, *, #80089, .T. ) ;
#246642 = EDGE_CURVE ( 'NONE', #167228, #128962, #128542, .T. ) ;
#246643 = DIRECTION ( 'NONE',  ( 2.694716079187272946E-16, -1.000000000000000000, 0.000000000000000000 ) ) ;
#246644 = EDGE_CURVE ( 'NONE', #237795, #80942, #241539, .T. ) ;
#246645 = ORIENTED_EDGE ( 'NONE', *, *, #68491, .F. ) ;
#246646 = DIRECTION ( 'NONE',  ( 1.000000000000000000, -2.952720810173289112E-16, -2.061873921506763405E-30 ) ) ;
#246647 = EDGE_CURVE ( 'NONE', #10892, #112516, #29210, .T. ) ;
#246648 = CARTESIAN_POINT ( 'NONE',  ( 18.59999999999999432, 1.637172712981537659, -179.0821533654719815 ) ) ;
#246649 = EDGE_LOOP ( 'NONE', ( #19044, #140041, #115533, #194700 ) ) ;
#246650 = CYLINDRICAL_SURFACE ( 'NONE', #18631, 0.5000000000000004441 ) ;
#246651 =( BOUNDED_SURFACE ( )  B_SPLINE_SURFACE ( 3, 2, ( 
 ( #210677, #189837, #16354 ),
 ( #191143, #153313, #11202 ),
 ( #92010, #213231, #251074 ),
 ( #253636, #132431, #232833 ),
 ( #72470, #51567, #55420 ),
 ( #209392, #111585, #90719 ) ),
 .UNSPECIFIED., .F., .F., .F. ) 
 B_SPLINE_SURFACE_WITH_KNOTS ( ( 4, 2, 4 ),
 ( 3, 3 ),
 ( 1.570796326794895448, 2.356194490192343505, 3.141592653589791784 ),
 ( 0.000000000000000000, 1.000000000000000000 ),
 .UNSPECIFIED. ) 
 GEOMETRIC_REPRESENTATION_ITEM ( )  RATIONAL_B_SPLINE_SURFACE ( (
 ( 1.000000000000000000, 0.7071067811865475727, 1.000000000000000000),
 ( 1.000000000000000000, 0.6611148371782917810, 1.000000000000000000),
 ( 1.000000000000000000, 0.6092287576690524897, 1.000000000000000000),
 ( 1.000000000000000000, 0.5278258667062201148, 1.000000000000000000),
 ( 1.000000000000000000, 0.4993418825330976363, 1.000000000000000000),
 ( 1.000000000000000000, 0.5000000000000339728, 1.000000000000000000) ) ) 
 REPRESENTATION_ITEM ( '' )  SURFACE ( )  );
#246652 = ADVANCED_FACE ( 'NONE', ( #204217 ), #105083, .T. ) ;
#246653 = VECTOR ( 'NONE', #102884, 1000.000000000000000 ) ;
#246654 = ORIENTED_EDGE ( 'NONE', *, *, #69339, .F. ) ;
#246655 = DIRECTION ( 'NONE',  ( 0.000000000000000000, 0.000000000000000000, -1.000000000000000000 ) ) ;
#246658 = ADVANCED_FACE ( 'NONE', ( #28192 ), #208232, .T. ) ;
#246657 = EDGE_CURVE ( 'NONE', #42457, #234879, #62486, .T. ) ;
#246656 = ORIENTED_EDGE ( 'NONE', *, *, #27353, .F. ) ;
#246659 = CYLINDRICAL_SURFACE ( 'NONE', #108680, 1.749999999999998002 ) ;
#246660 = DIRECTION ( 'NONE',  ( 2.952720810173289112E-16, -0.9770955615653302839, -0.2128009952263658355 ) ) ;
#246661 = DIRECTION ( 'NONE',  ( 1.000000000000000000, 0.000000000000000000, 0.000000000000000000 ) ) ;
#246662 = DIRECTION ( 'NONE',  ( -1.000000000000000000, 0.000000000000000000, 0.000000000000000000 ) ) ;
#246663 = AXIS2_PLACEMENT_3D ( 'NONE', #165441, #246255, #66335 ) ;
#246664 = DIRECTION ( 'NONE',  ( 1.000000000000000000, 0.000000000000000000, 0.000000000000000000 ) ) ;
#246665 = CARTESIAN_POINT ( 'NONE',  ( -19.99999999999999645, 4.528782138689107839, 21.95447128030237849 ) ) ;
#246666 = ADVANCED_FACE ( 'NONE', ( #247191 ), #87406, .T. ) ;
#246668 = EDGE_CURVE ( 'NONE', #151679, #165490, #222480, .T. ) ;
#246667 = DIRECTION ( 'NONE',  ( 0.000000000000000000, -1.000000000000000000, -7.272083257015735086E-15 ) ) ;
#246670 = ORIENTED_EDGE ( 'NONE', *, *, #103030, .F. ) ;
#246669 = AXIS2_PLACEMENT_3D ( 'NONE', #54846, #58691, #134379 ) ;
#246672 = DIRECTION ( 'NONE',  ( 0.000000000000000000, 1.000000000000000000, 6.982962677686266711E-15 ) ) ;
#246671 = LINE ( 'NONE', #206274, #32069 ) ;
#246673 = VERTEX_POINT ( 'NONE', #63419 ) ;
#246674 = CARTESIAN_POINT ( 'NONE',  ( -21.05000000000000071, 1.851028230140860487, -11.65391326942249606 ) ) ;
#246676 = CARTESIAN_POINT ( 'NONE',  ( -20.54999999999999716, -8.999999999988844479, -124.1060308773475924 ) ) ;
#246675 = AXIS2_PLACEMENT_3D ( 'NONE', #102810, #83243, #66286 ) ;
#246677 = EDGE_CURVE ( 'NONE', #114980, #18391, #45907, .T. ) ;
#246678 = CARTESIAN_POINT ( 'NONE',  ( -17.04761207306819770, 60.86557236029944562, -221.0217164902426248 ) ) ;
#246680 = VERTEX_POINT ( 'NONE', #123409 ) ;
#246679 = CARTESIAN_POINT ( 'NONE',  ( -23.15000000000000213, 2.000000000011154189, -146.7246219227621111 ) ) ;
#246682 = ORIENTED_EDGE ( 'NONE', *, *, #182863, .T. ) ;
#246681 = CARTESIAN_POINT ( 'NONE',  ( 21.14999999999999503, 87.65000000001275282, -215.2731074845242745 ) ) ;
#246683 = CARTESIAN_POINT ( 'NONE',  ( -18.50000000000000000, 74.83729825007360148, -61.42310748452432989 ) ) ;
#246684 = EDGE_CURVE ( 'NONE', #127923, #58960, #24327, .T. ) ;
#246685 = DIRECTION ( 'NONE',  ( 1.000000000000000000, 0.000000000000000000, 0.000000000000000000 ) ) ;
#246686 = EDGE_CURVE ( 'NONE', #128947, #44761, #195775, .T. ) ;
#246688 = ORIENTED_EDGE ( 'NONE', *, *, #11897, .F. ) ;
#246687 = FACE_OUTER_BOUND ( 'NONE', #133618, .T. ) ;
#246689 = VECTOR ( 'NONE', #222368, 1000.000000000000000 ) ;
#246690 = AXIS2_PLACEMENT_3D ( 'NONE', #29947, #50736, #152462 ) ;
#246691 = ORIENTED_EDGE ( 'NONE', *, *, #181391, .F. ) ;
#246692 = CARTESIAN_POINT ( 'NONE',  ( 21.05000000000000071, 5.400000000011154988, -157.6060308773475640 ) ) ;
#246693 = CARTESIAN_POINT ( 'NONE',  ( -14.00000000000000178, 9.850000000011133849, -184.2499999999999716 ) ) ;
#246694 = ORIENTED_EDGE ( 'NONE', *, *, #156190, .T. ) ;
#246695 = CARTESIAN_POINT ( 'NONE',  ( 21.05000000000000071, 87.65000000001214175, -136.5231074845242176 ) ) ;
#246696 = EDGE_LOOP ( 'NONE', ( #72162, #215037, #97392 ) ) ;
#246697 = VECTOR ( 'NONE', #85967, 1000.000000000000000 ) ;
#246699 = ADVANCED_FACE ( 'NONE', ( #251034 ), #149990, .F. ) ;
#246698 = DIRECTION ( 'NONE',  ( -1.000000000000000000, 0.000000000000000000, 0.000000000000000000 ) ) ;
#246700 = CARTESIAN_POINT ( 'NONE',  ( 19.86930884467611946, 34.45481642863170890, -235.1124302486271347 ) ) ;
#246701 = ORIENTED_EDGE ( 'NONE', *, *, #244384, .T. ) ;
#246702 = DIRECTION ( 'NONE',  ( 0.000000000000000000, -1.000000000000000000, -6.982962677686265922E-15 ) ) ;
#246703 = CIRCLE ( 'NONE', #188439, 0.5000000000000048850 ) ;
#246704 = AXIS2_PLACEMENT_3D ( 'NONE', #76959, #58660, #97779 ) ;
#246705 = DIRECTION ( 'NONE',  ( 0.7071067811865474617, 0.7071067811865474617, 2.044391222244499837E-16 ) ) ;
#246706 = EDGE_CURVE ( 'NONE', #174077, #155848, #229071, .T. ) ;
#246707 = ORIENTED_EDGE ( 'NONE', *, *, #209350, .F. ) ;
#246708 = CARTESIAN_POINT ( 'NONE',  ( -16.87665923198281348, 66.05000000001153637, -48.67310748452439384 ) ) ;
#246709 = ORIENTED_EDGE ( 'NONE', *, *, #193178, .F. ) ;
#246710 = EDGE_LOOP ( 'NONE', ( #87640, #99966, #75075, #229893 ) ) ;
#246711 = CARTESIAN_POINT ( 'NONE',  ( -18.52309608778520911, -9.642476320044279348, -73.71459634116931170 ) ) ;
#246712 = ORIENTED_EDGE ( 'NONE', *, *, #3119, .T. ) ;
#246714 = ADVANCED_FACE ( 'NONE', ( #213194 ), #216591, .T. ) ;
#246713 = FACE_OUTER_BOUND ( 'NONE', #187883, .T. ) ;
#246715 = VERTEX_POINT ( 'NONE', #191105 ) ;
#246717 = ORIENTED_EDGE ( 'NONE', *, *, #35488, .F. ) ;
#246716 = LINE ( 'NONE', #249312, #197276 ) ;
#246718 = DIRECTION ( 'NONE',  ( 1.000000000000000000, 0.000000000000000000, 0.000000000000000000 ) ) ;
#246719 = ORIENTED_EDGE ( 'NONE', *, *, #65886, .F. ) ;
#246720 = FACE_OUTER_BOUND ( 'NONE', #34108, .T. ) ;
#246721 = ORIENTED_EDGE ( 'NONE', *, *, #213846, .T. ) ;
#246724 = ORIENTED_EDGE ( 'NONE', *, *, #241422, .T. ) ;
#246723 = ORIENTED_EDGE ( 'NONE', *, *, #5955, .T. ) ;
#246722 = CARTESIAN_POINT ( 'NONE',  ( -16.93970660449832621, 65.98715860837600644, -56.97082574872992922 ) ) ;
#246725 = CARTESIAN_POINT ( 'NONE',  ( 20.73486653747088937, 7.750000000011182166, -176.7499999999999716 ) ) ;
#246726 = CIRCLE ( 'NONE', #26182, 0.09999999999999693856 ) ;
#246727 = ORIENTED_EDGE ( 'NONE', *, *, #206524, .F. ) ;
#246728 = AXIS2_PLACEMENT_3D ( 'NONE', #178527, #238468, #78099 ) ;
#246729 = ORIENTED_EDGE ( 'NONE', *, *, #34716, .T. ) ;
#246730 = CARTESIAN_POINT ( 'NONE',  ( -21.09107601085562322, 69.63612202465219525, -203.5624146492413900 ) ) ;
#246732 = DIRECTION ( 'NONE',  ( 0.000000000000000000, 0.000000000000000000, -1.000000000000000000 ) ) ;
#246731 = CIRCLE ( 'NONE', #134303, 0.1000000000000008937 ) ;
#246734 = ORIENTED_EDGE ( 'NONE', *, *, #8735, .F. ) ;
#246733 = FACE_OUTER_BOUND ( 'NONE', #32996, .T. ) ;
#246735 = FACE_OUTER_BOUND ( 'NONE', #100218, .T. ) ;
#246736 = ORIENTED_EDGE ( 'NONE', *, *, #71525, .F. ) ;
#246737 = DIRECTION ( 'NONE',  ( 0.000000000000000000, 0.000000000000000000, 1.000000000000000000 ) ) ;
#246738 = CARTESIAN_POINT ( 'NONE',  ( -23.25000000000000355, 5.650000000011139001, -113.1500000000000341 ) ) ;
#246739 = AXIS2_PLACEMENT_3D ( 'NONE', #214479, #89396, #174126 ) ;
#246740 = EDGE_LOOP ( 'NONE', ( #151552, #21576, #11185, #130009, #169235 ) ) ;
#246741 = CARTESIAN_POINT ( 'NONE',  ( -23.15000000000000213, -8.999999999988844479, -57.10603087734755690 ) ) ;
#246742 = CARTESIAN_POINT ( 'NONE',  ( -22.39999999999999858, 59.68594599439717285, -233.9123800762197902 ) ) ;
#246743 = VECTOR ( 'NONE', #141832, 1000.000000000000000 ) ;
#246744 = AXIS2_PLACEMENT_3D ( 'NONE', #74256, #152502, #213722 ) ;
#246745 = VERTEX_POINT ( 'NONE', #73725 ) ;
#246747 = EDGE_LOOP ( 'NONE', ( #113063, #83496, #233024, #228962, #138302 ) ) ;
#246746 = CARTESIAN_POINT ( 'NONE',  ( 19.86930884467603065, 54.45808362210101450, -228.7712941873963928 ) ) ;
#246748 = FACE_OUTER_BOUND ( 'NONE', #35351, .T. ) ;
#246749 = AXIS2_PLACEMENT_3D ( 'NONE', #228965, #75985, #49030 ) ;
#246751 = ORIENTED_EDGE ( 'NONE', *, *, #117857, .T. ) ;
#246750 = VERTEX_POINT ( 'NONE', #90684 ) ;
#246752 = VERTEX_POINT ( 'NONE', #30750 ) ;
#246753 = CARTESIAN_POINT ( 'NONE',  ( -21.05000000000000071, -11.48912529306489994, -97.50000000000004263 ) ) ;
#246754 = ORIENTED_EDGE ( 'NONE', *, *, #130993, .F. ) ;
#246755 = DIRECTION ( 'NONE',  ( -1.000000000000000000, -0.000000000000000000, -0.000000000000000000 ) ) ;
#246756 = ORIENTED_EDGE ( 'NONE', *, *, #215335, .T. ) ;
#246757 = LINE ( 'NONE', #220788, #181363 ) ;
#246758 = CIRCLE ( 'NONE', #71821, 0.09999999999999939493 ) ;
#246759 = DIRECTION ( 'NONE',  ( 0.000000000000000000, 0.000000000000000000, -1.000000000000000000 ) ) ;
#246761 = ORIENTED_EDGE ( 'NONE', *, *, #20511, .F. ) ;
#246760 = AXIS2_PLACEMENT_3D ( 'NONE', #250410, #151342, #113468 ) ;
#246762 = EDGE_CURVE ( 'NONE', #47980, #27728, #153276, .T. ) ;
#246763 = ORIENTED_EDGE ( 'NONE', *, *, #160963, .T. ) ;
#246764 = VECTOR ( 'NONE', #16430, 1000.000000000000000 ) ;
#246765 = VECTOR ( 'NONE', #28772, 1000.000000000000000 ) ;
#246766 = VERTEX_POINT ( 'NONE', #69872 ) ;
#246767 = VECTOR ( 'NONE', #125200, 1000.000000000000000 ) ;
#246768 = CIRCLE ( 'NONE', #21937, 0.09999999999999484301 ) ;
#246769 = DIRECTION ( 'NONE',  ( -0.000000000000000000, -0.4791956752371546724, -0.8777080977375153470 ) ) ;
#246770 = ORIENTED_EDGE ( 'NONE', *, *, #216132, .F. ) ;
#246771 = EDGE_CURVE ( 'NONE', #79128, #57467, #116634, .T. ) ;
#246772 = DIRECTION ( 'NONE',  ( 0.000000000000000000, 0.4999999999999956701, -0.8660254037844411501 ) ) ;
#246773 = CIRCLE ( 'NONE', #117617, 0.09999999999999939493 ) ;
#246775 = ORIENTED_EDGE ( 'NONE', *, *, #128981, .T. ) ;
#246774 = CARTESIAN_POINT ( 'NONE',  ( -21.33487959338958362, 69.27444184810119054, -170.0231074845243882 ) ) ;
#246776 = CARTESIAN_POINT ( 'NONE',  ( -20.64999999999999858, -8.730841121495327428, -9.598074718984330289 ) ) ;
#246777 = CARTESIAN_POINT ( 'NONE',  ( 20.94999999999999574, 1.162701749949165642, -108.5000000000000426 ) ) ;
#246778 = CARTESIAN_POINT ( 'NONE',  ( 23.14999999999998437, 76.00000000001165290, -69.52310748452431710 ) ) ;
#246779 = FACE_OUTER_BOUND ( 'NONE', #117529, .T. ) ;
#246780 = ADVANCED_FACE ( 'NONE', ( #188511 ), #208098, .F. ) ;
#246781 = DIRECTION ( 'NONE',  ( -0.000000000000000000, 1.000000000000000000, 6.982962677686267499E-15 ) ) ;
#246783 = FACE_OUTER_BOUND ( 'NONE', #109353, .T. ) ;
#246782 = SPHERICAL_SURFACE ( 'NONE', #161199, 0.1000000000000000056 ) ;
#246784 = DIRECTION ( 'NONE',  ( 1.000000000000000000, -0.000000000000000000, 0.000000000000000000 ) ) ;
#246785 = LINE ( 'NONE', #207692, #143053 ) ;
#246787 = EDGE_CURVE ( 'NONE', #83828, #241603, #66763, .T. ) ;
#246786 = TOROIDAL_SURFACE ( 'NONE', #84242, 0.4000000000000010214, 0.1000000000000000056 ) ;
#246789 = EDGE_LOOP ( 'NONE', ( #21606, #157342, #21336, #10411 ) ) ;
#246788 = CIRCLE ( 'NONE', #242524, 0.09999999999998898659 ) ;
#246790 = AXIS2_PLACEMENT_3D ( 'NONE', #165087, #242048, #125945 ) ;
#246791 = ADVANCED_FACE ( 'NONE', ( #211940 ), #170280, .F. ) ;
#246792 = ORIENTED_EDGE ( 'NONE', *, *, #232606, .T. ) ;
#246794 = EDGE_LOOP ( 'NONE', ( #223854, #90556, #21499, #16693, #216430, #189451 ) ) ;
#246793 = LINE ( 'NONE', #129424, #132332 ) ;
#246795 = EDGE_CURVE ( 'NONE', #4633, #251099, #100034, .T. ) ;
#246796 = ORIENTED_EDGE ( 'NONE', *, *, #176217, .T. ) ;
#246797 = DIRECTION ( 'NONE',  ( 1.000000000000000000, 0.000000000000000000, 0.000000000000000000 ) ) ;
#246798 = LINE ( 'NONE', #107293, #173752 ) ;
#246799 = ADVANCED_FACE ( 'NONE', ( #9871 ), #199866, .T. ) ;
#246801 = DIRECTION ( 'NONE',  ( 0.000000000000000000, 0.9126074666063772600, 0.4088369013363274407 ) ) ;
#246800 = LINE ( 'NONE', #147716, #161789 ) ;
#246802 = ORIENTED_EDGE ( 'NONE', *, *, #256521, .T. ) ;
#246803 =( NAMED_UNIT ( * ) PLANE_ANGLE_UNIT ( ) SI_UNIT ( $, .RADIAN. ) );
#246804 = EDGE_CURVE ( 'NONE', #125, #95393, #154556, .T. ) ;
#246805 = CARTESIAN_POINT ( 'NONE',  ( -22.94999999999999929, 0.000000000000000000, 0.000000000000000000 ) ) ;
#246806 = AXIS2_PLACEMENT_3D ( 'NONE', #7234, #85462, #166363 ) ;
#246807 = ORIENTED_EDGE ( 'NONE', *, *, #59736, .F. ) ;
#246808 = CARTESIAN_POINT ( 'NONE',  ( -21.55000000000000426, 7.750000000011159074, -188.6499999999999488 ) ) ;
#246809 = CARTESIAN_POINT ( 'NONE',  ( 20.94999999999999929, 45.02833974712562792, -238.5149546970766892 ) ) ;
#246811 = ADVANCED_FACE ( 'NONE', ( #209353 ), #150675, .T. ) ;
#246810 = DIRECTION ( 'NONE',  ( 0.000000000000000000, 0.000000000000000000, -1.000000000000000000 ) ) ;
#246812 = CARTESIAN_POINT ( 'NONE',  ( 21.05000000000000071, 65.52661458509871295, -61.94445302027585853 ) ) ;
#246813 = CIRCLE ( 'NONE', #134382, 0.09999999999999939493 ) ;
#246814 = CARTESIAN_POINT ( 'NONE',  ( -18.52139480978222963, 78.22076358160548182, -231.5572559401365424 ) ) ;
#246816 = VERTEX_POINT ( 'NONE', #89402 ) ;
#246815 = DIRECTION ( 'NONE',  ( -1.000000000000000000, 0.000000000000000000, 0.000000000000000000 ) ) ;
#246817 = ADVANCED_FACE ( 'NONE', ( #168993 ), #199869, .F. ) ;
#246818 = DIRECTION ( 'NONE',  ( 0.000000000000000000, 0.000000000000000000, -1.000000000000000000 ) ) ;
#246819 = FACE_OUTER_BOUND ( 'NONE', #35473, .T. ) ;
#246820 = CARTESIAN_POINT ( 'NONE',  ( -20.54999999999999716, 68.85000000001228670, -157.7731074845244166 ) ) ;
#246821 = DIRECTION ( 'NONE',  ( 0.000000000000000000, -0.9126074666063545004, -0.4088369013363783999 ) ) ;
#246822 = ORIENTED_EDGE ( 'NONE', *, *, #140855, .F. ) ;
#246823 = CARTESIAN_POINT ( 'NONE',  ( -18.40000000000000213, 11.48667500176882861, -124.7500000000000284 ) ) ;
#246825 = EDGE_CURVE ( 'NONE', #235384, #167344, #241453, .T. ) ;
#246824 = CARTESIAN_POINT ( 'NONE',  ( -16.87683809663752399, 28.30820381385230178, -220.9847017323426144 ) ) ;
#246827 = DIRECTION ( 'NONE',  ( -0.000000000000000000, -0.4088369013363281623, 0.9126074666063771490 ) ) ;
#246826 = FACE_OUTER_BOUND ( 'NONE', #232749, .T. ) ;
#246828 = DIRECTION ( 'NONE',  ( 0.000000000000000000, 0.000000000000000000, 1.000000000000000000 ) ) ;
#246829 = DIRECTION ( 'NONE',  ( -2.978066053179067751E-16, 1.000000000000000000, 0.000000000000000000 ) ) ;
#246830 = DIRECTION ( 'NONE',  ( 0.000000000000000000, -1.000000000000000000, -6.860497997771531562E-15 ) ) ;
#246831 = LINE ( 'NONE', #147749, #97800 ) ;
#246832 = CARTESIAN_POINT ( 'NONE',  ( 18.39999999999999858, 85.51932773110452501, -129.5501311079648872 ) ) ;
#246833 = DIRECTION ( 'NONE',  ( 0.000000000000000000, 2.362176648138631684E-15, -1.000000000000000000 ) ) ;
#246834 = ORIENTED_EDGE ( 'NONE', *, *, #7961, .F. ) ;
#246835 = VECTOR ( 'NONE', #5720, 1000.000000000000000 ) ;
#246836 = ORIENTED_EDGE ( 'NONE', *, *, #82498, .F. ) ;
#246837 = VERTEX_POINT ( 'NONE', #141065 ) ;
#246838 = ADVANCED_FACE ( 'NONE', ( #201032 ), #79771, .T. ) ;
#246839 = CARTESIAN_POINT ( 'NONE',  ( -18.59999999999999787, 1.637172712981537659, -45.08215336547201701 ) ) ;
#246840 = DIRECTION ( 'NONE',  ( -1.073024830501117725E-15, 0.000000000000000000, -1.000000000000000000 ) ) ;
#246841 = EDGE_LOOP ( 'NONE', ( #167199, #144013, #36744, #200521 ) ) ;
#246842 = ORIENTED_EDGE ( 'NONE', *, *, #105393, .T. ) ;
#246843 = CIRCLE ( 'NONE', #26297, 0.6000000000000139666 ) ;
#246844 = ORIENTED_EDGE ( 'NONE', *, *, #205126, .F. ) ;
#246845 = LINE ( 'NONE', #223427, #16917 ) ;
#246846 = EDGE_LOOP ( 'NONE', ( #166670, #22605, #10782, #113587 ) ) ;
#246847 = AXIS2_PLACEMENT_3D ( 'NONE', #235749, #257834, #40160 ) ;
#246848 = ADVANCED_FACE ( 'NONE', ( #1533 ), #225123, .F. ) ;
#246849 = CYLINDRICAL_SURFACE ( 'NONE', #42458, 0.09999999999999939493 ) ;
#246850 = CARTESIAN_POINT ( 'NONE',  ( -18.40000000000000213, 11.33174054713631662, -113.1500000000000341 ) ) ;
#246851 = CYLINDRICAL_SURFACE ( 'NONE', #170064, 12.87499999999999822 ) ;
#246852 = CARTESIAN_POINT ( 'NONE',  ( -21.08621493067320429, 1.558495345345466188, -230.6850742879884137 ) ) ;
#246853 = AXIS2_PLACEMENT_3D ( 'NONE', #145495, #225016, #82929 ) ;
#246854 = DIRECTION ( 'NONE',  ( 0.000000000000000000, -7.429790795770644761E-15, 1.000000000000000000 ) ) ;
#246855 = DIRECTION ( 'NONE',  ( 0.7071067811865475727, -0.2890913453342132122, 0.6453109281988448354 ) ) ;
#246857 = ORIENTED_EDGE ( 'NONE', *, *, #171940, .F. ) ;
#246856 = CYLINDRICAL_SURFACE ( 'NONE', #42396, 0.09999999999998898659 ) ;
#246859 = CARTESIAN_POINT ( 'NONE',  ( 21.13461538461538680, 8.885417037985614996, -79.35000000000005116 ) ) ;
#246858 = CARTESIAN_POINT ( 'NONE',  ( 20.99780126800938262, 11.60538868787666011, -26.58735257170533473 ) ) ;
#246860 = CARTESIAN_POINT ( 'NONE',  ( -21.53752568622142505, 75.90102553874106661, -76.30991535907291734 ) ) ;
#246861 = EDGE_CURVE ( 'NONE', #33783, #208409, #142330, .T. ) ;
#246862 = ORIENTED_EDGE ( 'NONE', *, *, #54337, .F. ) ;
#246863 = CARTESIAN_POINT ( 'NONE',  ( 12.47034474403011650, 66.62446189796402507, -120.6532316035334844 ) ) ;
#246864 = CARTESIAN_POINT ( 'NONE',  ( -14.11697426661281263, 9.457410944778569473, -115.5000839737900833 ) ) ;
#246865 = CARTESIAN_POINT ( 'NONE',  ( -20.85000000000000142, 11.74999999999999645, -26.65839931010294350 ) ) ;
#246866 = ORIENTED_EDGE ( 'NONE', *, *, #24740, .T. ) ;
#246867 = CIRCLE ( 'NONE', #121974, 0.09999999999999939493 ) ;
#246868 = EDGE_CURVE ( 'NONE', #135547, #86293, #143619, .T. ) ;
#246870 = DIRECTION ( 'NONE',  ( 0.000000000000000000, -1.000000000000000000, 0.000000000000000000 ) ) ;
#246869 = CIRCLE ( 'NONE', #238508, 0.1000000000000028644 ) ;
#246871 = ADVANCED_FACE ( 'NONE', ( #22419 ), #221847, .F. ) ;
#246872 = EDGE_CURVE ( 'NONE', #91629, #92370, #219303, .T. ) ;
#246873 = CARTESIAN_POINT ( 'NONE',  ( 20.94999999999999574, 4.436385504674529301, -245.3241086753762659 ) ) ;
#246874 = ADVANCED_FACE ( 'NONE', ( #220602 ), #253, .F. ) ;
#246875 = ORIENTED_EDGE ( 'NONE', *, *, #77097, .F. ) ;
#246876 = FACE_OUTER_BOUND ( 'NONE', #39650, .T. ) ;
#246877 = FACE_OUTER_BOUND ( 'NONE', #40857, .T. ) ;
#246878 = EDGE_CURVE ( 'NONE', #224911, #233399, #137637, .T. ) ;
#246879 = AXIS2_PLACEMENT_3D ( 'NONE', #244885, #227897, #109220 ) ;
#246880 = CARTESIAN_POINT ( 'NONE',  ( 16.87683809663750267, 60.93935776605891164, -221.0417277355860790 ) ) ;
#246881 = CARTESIAN_POINT ( 'NONE',  ( 21.05000000000000071, 76.00000000001213607, -136.5231074845242745 ) ) ;
#246882 = VERTEX_POINT ( 'NONE', #199772 ) ;
#246883 = ORIENTED_EDGE ( 'NONE', *, *, #69908, .T. ) ;
#246884 = CIRCLE ( 'NONE', #17933, 0.1000000000000118433 ) ;
#246885 = DIRECTION ( 'NONE',  ( 0.000000000000000000, 0.000000000000000000, -1.000000000000000000 ) ) ;
#246886 = DIRECTION ( 'NONE',  ( 0.000000000000000000, 0.5868805631290340274, 0.8096735173027138632 ) ) ;
#246887 = CARTESIAN_POINT ( 'NONE',  ( 16.27683809663749770, 9.350000000011137402, -42.75000000000000000 ) ) ;
#246888 = CARTESIAN_POINT ( 'NONE',  ( -18.59999999999999787, 11.65000000001115232, -188.8499999999999659 ) ) ;
#246889 = CARTESIAN_POINT ( 'NONE',  ( 15.74999999999999645, 9.350000000011139178, -50.25000000000000000 ) ) ;
#246890 = CARTESIAN_POINT ( 'NONE',  ( 21.14999999999999858, 6.650000000011155876, -45.85000000000000142 ) ) ;
#246891 = ORIENTED_EDGE ( 'NONE', *, *, #200262, .T. ) ;
#246892 = FACE_OUTER_BOUND ( 'NONE', #36008, .T. ) ;
#246893 = EDGE_CURVE ( 'NONE', #24108, #50189, #133565, .T. ) ;
#246895 = ORIENTED_EDGE ( 'NONE', *, *, #232459, .T. ) ;
#246894 = DIRECTION ( 'NONE',  ( 0.000000000000000000, -6.308085367188367561E-15, 1.000000000000000000 ) ) ;
#246896 = CARTESIAN_POINT ( 'NONE',  ( 23.14999999999999858, 76.00000000001126921, -203.5231074845248997 ) ) ;
#246897 = CARTESIAN_POINT ( 'NONE',  ( 23.15000000000000213, -8.999999999988842703, -91.10603087734760663 ) ) ;
#246898 = CARTESIAN_POINT ( 'NONE',  ( -20.85000000000000142, 11.64999999999999680, -33.50000000000000000 ) ) ;
#246899 = CARTESIAN_POINT ( 'NONE',  ( -16.82055514392396489, 66.05000000001183480, -123.8463094099828368 ) ) ;
#246900 = EDGE_CURVE ( 'NONE', #218463, #236987, #21140, .T. ) ;
#246902 = ORIENTED_EDGE ( 'NONE', *, *, #221550, .T. ) ;
#246901 = DIRECTION ( 'NONE',  ( 0.000000000000000000, 0.2617529984165152257, 0.9651348961777124202 ) ) ;
#246903 = FACE_OUTER_BOUND ( 'NONE', #66506, .T. ) ;
#246905 = EDGE_CURVE ( 'NONE', #239007, #127805, #179377, .T. ) ;
#246904 = CARTESIAN_POINT ( 'NONE',  ( -2.995603634470829482E-16, 10.99842653345846699, -220.2504445088529792 ) ) ;
#246906 = DIRECTION ( 'NONE',  ( 1.000000000000000000, 0.000000000000000000, 0.000000000000000000 ) ) ;
#246907 = DIRECTION ( 'NONE',  ( 0.000000000000000000, 1.000000000000000000, -1.224646799147353207E-16 ) ) ;
#246908 = ORIENTED_EDGE ( 'NONE', *, *, #203270, .T. ) ;
#246909 = CARTESIAN_POINT ( 'NONE',  ( 18.47073956224749480, -7.742049366311430703, -209.9614587431316579 ) ) ;
#246910 = CYLINDRICAL_SURFACE ( 'NONE', #152668, 0.09999999999999864553 ) ;
#246911 = ORIENTED_EDGE ( 'NONE', *, *, #180403, .T. ) ;
#246912 = CARTESIAN_POINT ( 'NONE',  ( -18.59999999999999787, 86.96699927712941758, -199.3055931863049466 ) ) ;
#246913 = AXIS2_PLACEMENT_3D ( 'NONE', #181585, #162025, #62899 ) ;
#246914 = CARTESIAN_POINT ( 'NONE',  ( -18.59999999999999787, 2.319530388122570841, -217.8268657444419887 ) ) ;
#246915 = ORIENTED_EDGE ( 'NONE', *, *, #129978, .F. ) ;
#246916 = FACE_OUTER_BOUND ( 'NONE', #214025, .T. ) ;
#246917 = EDGE_LOOP ( 'NONE', ( #152241, #173462, #86962, #204332 ) ) ;
#246918 = CARTESIAN_POINT ( 'NONE',  ( -18.50000000000000000, 68.97833521811131163, -32.18954208262707795 ) ) ;
#246919 = CARTESIAN_POINT ( 'NONE',  ( 21.14999999999999503, 87.75000000001264766, -200.6231074845242688 ) ) ;
#246920 = AXIS2_PLACEMENT_3D ( 'NONE', #187414, #27076, #166584 ) ;
#246921 = TOROIDAL_SURFACE ( 'NONE', #51267, 0.2000000000000000111, 0.1000000000000000056 ) ;
#246922 = DIRECTION ( 'NONE',  ( 0.000000000000000000, 0.000000000000000000, -1.000000000000000000 ) ) ;
#246923 = ORIENTED_EDGE ( 'NONE', *, *, #108021, .T. ) ;
#246924 = AXIS2_PLACEMENT_3D ( 'NONE', #252985, #234719, #73110 ) ;
#246925 = DIRECTION ( 'NONE',  ( 0.000000000000000000, 0.000000000000000000, -1.000000000000000000 ) ) ;
#246926 = AXIS2_PLACEMENT_3D ( 'NONE', #108810, #86656, #224898 ) ;
#246927 = CARTESIAN_POINT ( 'NONE',  ( -21.14999999999999858, 6.257814610487270279, -100.4022097086912311 ) ) ;
#246928 = TOROIDAL_SURFACE ( 'NONE', #105437, 0.2000000000000000111, 0.1000000000000000056 ) ;
#246929 = VECTOR ( 'NONE', #152215, 1000.000000000000000 ) ;
#246930 = CARTESIAN_POINT ( 'NONE',  ( -20.94999999999999929, 64.30000000001147953, -42.77810563404302258 ) ) ;
#246931 = CARTESIAN_POINT ( 'NONE',  ( -16.82055514392389028, 9.949999999999983302, -20.82320192545794768 ) ) ;
#246932 = CARTESIAN_POINT ( 'NONE',  ( 18.59999999999999076, -1.835859311432481045, -112.1044391687985780 ) ) ;
#246933 = EDGE_LOOP ( 'NONE', ( #83235, #22879, #111143, #117491 ) ) ;
#246935 = ORIENTED_EDGE ( 'NONE', *, *, #111160, .T. ) ;
#246934 = CARTESIAN_POINT ( 'NONE',  ( -22.00411653962160585, 7.253442868381348774, -167.4009618942313864 ) ) ;
#246936 = AXIS2_PLACEMENT_3D ( 'NONE', #176802, #21572, #256241 ) ;
#246937 = ORIENTED_EDGE ( 'NONE', *, *, #21445, .T. ) ;
#246938 = PLANE ( 'NONE',  #73843 ) ;
#246939 = EDGE_LOOP ( 'NONE', ( #83772, #189713, #210237, #125637 ) ) ;
#246940 = CARTESIAN_POINT ( 'NONE',  ( 21.13422380239049403, 60.96433854134358654, -234.1554788215306644 ) ) ;
#246941 = DIRECTION ( 'NONE',  ( -1.000000000000000000, 7.304098846218133681E-16, -4.217023435051677994E-16 ) ) ;
#246942 = DIRECTION ( 'NONE',  ( 1.000000000000000000, 0.000000000000000000, 0.000000000000000000 ) ) ;
#246943 = ORIENTED_EDGE ( 'NONE', *, *, #41890, .F. ) ;
#246944 = CARTESIAN_POINT ( 'NONE',  ( 21.05000000000000071, -0.09999999998884338825, -60.45934304829879835 ) ) ;
#246945 = CARTESIAN_POINT ( 'NONE',  ( -18.59999999999999787, 18.81339837015603322, -226.7756228984618190 ) ) ;
#246947 = DIRECTION ( 'NONE',  ( 0.000000000000000000, 6.982962677686266711E-15, -1.000000000000000000 ) ) ;
#246946 = TOROIDAL_SURFACE ( 'NONE', #209349, 0.6000000000000013101, 0.1000000000000000056 ) ;
#246948 = ORIENTED_EDGE ( 'NONE', *, *, #65620, .F. ) ;
#246949 = DIRECTION ( 'NONE',  ( -1.073024830501117528E-15, -0.8814952561688430555, 0.4721928772777346239 ) ) ;
#246950 = CIRCLE ( 'NONE', #134507, 0.09999999999999158173 ) ;
#246951 = EDGE_CURVE ( 'NONE', #38969, #116223, #175145, .T. ) ;
#246953 = ORIENTED_EDGE ( 'NONE', *, *, #113796, .F. ) ;
#246952 = DIRECTION ( 'NONE',  ( 2.840903330521633255E-16, 0.7106264324241464703, -0.7035695228903324772 ) ) ;
#246954 = FACE_OUTER_BOUND ( 'NONE', #53374, .T. ) ;
#246955 = FACE_OUTER_BOUND ( 'NONE', #234318, .T. ) ;
#246956 = AXIS2_PLACEMENT_3D ( 'NONE', #48854, #227483, #31895 ) ;
#246957 = EDGE_CURVE ( 'NONE', #158699, #157707, #87579, .T. ) ;
#246958 = CIRCLE ( 'NONE', #226269, 1.749999999999998002 ) ;
#246959 = ORIENTED_EDGE ( 'NONE', *, *, #89703, .T. ) ;
#246960 = DIRECTION ( 'NONE',  ( -1.000000000000000000, 1.772924042024179204E-16, -4.808324575169891715E-17 ) ) ;
#246962 = EDGE_CURVE ( 'NONE', #101407, #243571, #240169, .T. ) ;
#246961 = CARTESIAN_POINT ( 'NONE',  ( -14.23072895065543264, 66.54401276639934792, -121.5115763176265773 ) ) ;
#246963 = AXIS2_PLACEMENT_3D ( 'NONE', #61838, #141362, #121819 ) ;
#246964 = CARTESIAN_POINT ( 'NONE',  ( 23.14999999999999503, 69.35000000001205933, -124.2731074845243455 ) ) ;
#246966 = EDGE_CURVE ( 'NONE', #199332, #165247, #50162, .T. ) ;
#246965 = ORIENTED_EDGE ( 'NONE', *, *, #181479, .T. ) ;
#246967 = LINE ( 'NONE', #207882, #213106 ) ;
#246968 = DIRECTION ( 'NONE',  ( 1.000000000000000000, 0.000000000000000000, 0.000000000000000000 ) ) ;
#246969 = ORIENTED_EDGE ( 'NONE', *, *, #160011, .T. ) ;
#246970 = CIRCLE ( 'NONE', #184432, 4.041421356237306917 ) ;
#246971 = VECTOR ( 'NONE', #161361, 1000.000000000000000 ) ;
#246973 = EDGE_CURVE ( 'NONE', #32434, #97945, #125205, .T. ) ;
#246972 = AXIS2_PLACEMENT_3D ( 'NONE', #15168, #114254, #212089 ) ;
#246974 = VECTOR ( 'NONE', #250277, 1000.000000000000000 ) ;
#246975 = EDGE_CURVE ( 'NONE', #86047, #38614, #146031, .T. ) ;
#246976 = ORIENTED_EDGE ( 'NONE', *, *, #10049, .F. ) ;
#246977 = CARTESIAN_POINT ( 'NONE',  ( 22.32929514600007792, 68.42135243463620498, -203.6221831626383221 ) ) ;
#246978 = ORIENTED_EDGE ( 'NONE', *, *, #65223, .T. ) ;
#246979 = CARTESIAN_POINT ( 'NONE',  ( -18.58671080940900211, -9.406932858815471477, -174.6241544649046489 ) ) ;
#246980 = CARTESIAN_POINT ( 'NONE',  ( -16.88783316861802319, 66.05000000001255955, -182.7753715265037044 ) ) ;
#246982 = VERTEX_POINT ( 'NONE', #6675 ) ;
#246981 = CARTESIAN_POINT ( 'NONE',  ( -23.25000000000000000, 6.681951250119205987, -231.6808006331528986 ) ) ;
#246983 = DIRECTION ( 'NONE',  ( 0.000000000000000000, 6.982962677686266711E-15, -1.000000000000000000 ) ) ;
#246984 = DIRECTION ( 'NONE',  ( 1.000000000000000000, -0.000000000000000000, -0.000000000000000000 ) ) ;
#246985 = CARTESIAN_POINT ( 'NONE',  ( -20.00857864376270001, 11.54723657985719321, -211.0222915228556246 ) ) ;
#246986 = CARTESIAN_POINT ( 'NONE',  ( -23.49999999999994316, 64.35000000001120668, -18.32310748452480098 ) ) ;
#246987 = LINE ( 'NONE', #68368, #122777 ) ;
#246988 = DIRECTION ( 'NONE',  ( 0.000000000000000000, 0.000000000000000000, 1.000000000000000000 ) ) ;
#246990 = ADVANCED_FACE ( 'NONE', ( #67938 ), #46075, .F. ) ;
#246989 = CARTESIAN_POINT ( 'NONE',  ( -20.54999999999999716, 85.00000000001197975, -112.9170766071766820 ) ) ;
#246992 = ORIENTED_EDGE ( 'NONE', *, *, #191280, .F. ) ;
#246991 = CARTESIAN_POINT ( 'NONE',  ( -20.54999999999999716, 4.250000000011156409, -79.25000000000004263 ) ) ;
#246993 = CARTESIAN_POINT ( 'NONE',  ( -23.15000000000000213, 11.65000000001115588, -188.8499999999999659 ) ) ;
#246994 = ORIENTED_EDGE ( 'NONE', *, *, #91168, .F. ) ;
#246995 = EDGE_CURVE ( 'NONE', #193788, #173035, #83467, .T. ) ;
#246996 = CARTESIAN_POINT ( 'NONE',  ( 23.14999999999999858, -2.000000000000002665, -33.50000000000000000 ) ) ;
#246997 = CIRCLE ( 'NONE', #184460, 0.1000000000000017680 ) ;
#246998 = DIRECTION ( 'NONE',  ( 0.000000000000000000, -0.9998779222360097974, 0.01562500000000363945 ) ) ;
#247000 = EDGE_CURVE ( 'NONE', #30659, #211497, #171044, .T. ) ;
#246999 = CARTESIAN_POINT ( 'NONE',  ( -23.49999999999994316, 76.00000000001119815, -36.02310748452479316 ) ) ;
#247001 = CARTESIAN_POINT ( 'NONE',  ( -18.59999999999999787, 76.00000000001142553, -36.02310748452432421 ) ) ;
#247002 = ORIENTED_EDGE ( 'NONE', *, *, #147036, .T. ) ;
#247003 = CARTESIAN_POINT ( 'NONE',  ( 21.05000000000000071, 9.997527148596393687, -228.1702915402975407 ) ) ;
#247004 = CARTESIAN_POINT ( 'NONE',  ( -21.10257677756356642, 6.398381742543891804, -100.4750492504320931 ) ) ;
#247005 = EDGE_CURVE ( 'NONE', #232621, #102676, #66929, .T. ) ;
#247006 = ORIENTED_EDGE ( 'NONE', *, *, #18431, .T. ) ;
#247007 = AXIS2_PLACEMENT_3D ( 'NONE', #134099, #196644, #216202 ) ;
#247008 = CARTESIAN_POINT ( 'NONE',  ( 21.05000000000000071, 1.115600667400684642E-11, -134.0000000000000000 ) ) ;
#247009 = TOROIDAL_SURFACE ( 'NONE', #230461, 11.70000000000000107, 0.1000000000000000056 ) ;
#247010 = CARTESIAN_POINT ( 'NONE',  ( -16.81744102076749314, 9.950000000011142376, -113.1500000000000341 ) ) ;
#247011 = VERTEX_POINT ( 'NONE', #207470 ) ;
#247012 = CARTESIAN_POINT ( 'NONE',  ( -16.88495309932524080, 66.04537294153973903, -190.8885588107125386 ) ) ;
#247013 = VERTEX_POINT ( 'NONE', #87487 ) ;
#247014 = EDGE_CURVE ( 'NONE', #140654, #39363, #246001, .T. ) ;
#247015 = CARTESIAN_POINT ( 'NONE',  ( -20.00857864376270001, 13.65786464920749843, -219.7735913778983559 ) ) ;
#247016 = ORIENTED_EDGE ( 'NONE', *, *, #146797, .F. ) ;
#247017 = CARTESIAN_POINT ( 'NONE',  ( -18.59999999999999787, 11.65000000001115232, -121.8500000000000369 ) ) ;
#247018 = EDGE_CURVE ( 'NONE', #41810, #229311, #116817, .T. ) ;
#247019 = CARTESIAN_POINT ( 'NONE',  ( 21.05000000000000071, 75.90220970870339556, -142.7809220950004203 ) ) ;
#247020 = ORIENTED_EDGE ( 'NONE', *, *, #241935, .T. ) ;
#247021 = ORIENTED_EDGE ( 'NONE', *, *, #199479, .T. ) ;
#247023 = LINE ( 'NONE', #171398, #98675 ) ;
#247022 = AXIS2_PLACEMENT_3D ( 'NONE', #56406, #214225, #171293 ) ;
#247025 = ORIENTED_EDGE ( 'NONE', *, *, #2906, .F. ) ;
#247024 = DIRECTION ( 'NONE',  ( 0.000000000000000000, -0.2128009952263604232, 0.9770955615653316162 ) ) ;
#247026 = CARTESIAN_POINT ( 'NONE',  ( -22.39999999999999858, 76.00000000001273293, -215.2735403769829645 ) ) ;
#247027 = ORIENTED_EDGE ( 'NONE', *, *, #192194, .F. ) ;
#247028 = AXIS2_PLACEMENT_3D ( 'NONE', #153393, #212055, #55490 ) ;
#247029 = VECTOR ( 'NONE', #198433, 1000.000000000000000 ) ;
#247030 = ORIENTED_EDGE ( 'NONE', *, *, #79583, .F. ) ;
#247031 = PLANE ( 'NONE',  #61874 ) ;
#247032 = DIRECTION ( 'NONE',  ( 0.000000000000000000, 1.000000000000000000, 0.000000000000000000 ) ) ;
#247033 = CARTESIAN_POINT ( 'NONE',  ( 20.95512820512820440, 10.62384868371188062, -7.664913569087605794 ) ) ;
#247034 = DIRECTION ( 'NONE',  ( 2.952720810173288619E-16, -1.000000000000000000, 0.000000000000000000 ) ) ;
#247035 = CARTESIAN_POINT ( 'NONE',  ( 20.95512840106816199, 65.37615130623825621, -57.32062826372554554 ) ) ;
#247036 = DIRECTION ( 'NONE',  ( -1.000000000000000000, 0.000000000000000000, 0.000000000000000000 ) ) ;
#247037 = VECTOR ( 'NONE', #218889, 1000.000000000000000 ) ;
#247038 = EDGE_LOOP ( 'NONE', ( #5622, #91530, #62431, #209437 ) ) ;
#247039 = CIRCLE ( 'NONE', #59771, 0.09999999999999939493 ) ;
#247040 = CARTESIAN_POINT ( 'NONE',  ( -16.94333152882356330, 66.00965798855487776, -182.6310759534229646 ) ) ;
#247041 = LINE ( 'NONE', #127106, #252830 ) ;
#247042 = DIRECTION ( 'NONE',  ( 1.000000000000000000, 0.000000000000000000, 0.000000000000000000 ) ) ;
#247043 = AXIS2_PLACEMENT_3D ( 'NONE', #153331, #208147, #188558 ) ;
#247044 = DIRECTION ( 'NONE',  ( 0.000000000000000000, 0.2617529984165031243, 0.9651348961777157509 ) ) ;
#247045 = EDGE_LOOP ( 'NONE', ( #137592, #163704, #240567, #147356 ) ) ;
#247046 = EDGE_LOOP ( 'NONE', ( #82155, #166560, #127129, #28222 ) ) ;
#247047 = CARTESIAN_POINT ( 'NONE',  ( 14.11444803880197263, 9.457431528860070102, -115.4999169378997408 ) ) ;
#247048 = ORIENTED_EDGE ( 'NONE', *, *, #58847, .F. ) ;
#247049 = CARTESIAN_POINT ( 'NONE',  ( -15.52965525596988705, 25.54511595760794052, -232.9618513057392875 ) ) ;
#247050 = CARTESIAN_POINT ( 'NONE',  ( 21.05000000000000071, 69.45934304831041572, -69.42310748452437963 ) ) ;
#247052 = ORIENTED_EDGE ( 'NONE', *, *, #133833, .T. ) ;
#247051 = AXIS2_PLACEMENT_3D ( 'NONE', #84164, #202884, #64656 ) ;
#247053 = ORIENTED_EDGE ( 'NONE', *, *, #102025, .F. ) ;
#247055 = ORIENTED_EDGE ( 'NONE', *, *, #42049, .T. ) ;
#247054 = DIRECTION ( 'NONE',  ( 1.000000000000000000, -0.000000000000000000, -0.000000000000000000 ) ) ;
#247056 = CARTESIAN_POINT ( 'NONE',  ( -22.39999999999999858, 76.00000000001222134, -148.1726782920690937 ) ) ;
#247057 = ORIENTED_EDGE ( 'NONE', *, *, #3237, .T. ) ;
#247058 = CARTESIAN_POINT ( 'NONE',  ( -22.47886152344871036, 0.03750093887284931815, -21.85001135695206997 ) ) ;
#247059 = CIRCLE ( 'NONE', #155355, 4.000000000000003553 ) ;
#247060 = AXIS2_PLACEMENT_3D ( 'NONE', #135732, #195746, #17105 ) ;
#247061 = VECTOR ( 'NONE', #164219, 1000.000000000000000 ) ;
#247062 = CARTESIAN_POINT ( 'NONE',  ( 23.14999999999999858, 10.93950603019935564, -232.9027774310573022 ) ) ;
#247063 = AXIS2_PLACEMENT_3D ( 'NONE', #189817, #248500, #32048 ) ;
#247064 = VERTEX_POINT ( 'NONE', #147480 ) ;
#247065 = DIRECTION ( 'NONE',  ( 0.7071067811865475727, 0.7071067811865475727, 2.044391222244500083E-16 ) ) ;
#247066 = EDGE_CURVE ( 'NONE', #206536, #156363, #58542, .T. ) ;
#247067 = DIRECTION ( 'NONE',  ( -0.000000000000000000, 0.000000000000000000, 1.000000000000000000 ) ) ;
#247068 = ORIENTED_EDGE ( 'NONE', *, *, #61711, .T. ) ;
#247069 = LINE ( 'NONE', #5888, #130618 ) ;
#247071 = ADVANCED_FACE ( 'NONE', ( #206173 ), #86190, .T. ) ;
#247070 = CARTESIAN_POINT ( 'NONE',  ( -16.79814274880124358, 22.97986866999201894, -230.9368535240658673 ) ) ;
#247072 = DIRECTION ( 'NONE',  ( 0.000000000000000000, -8.267618268485210697E-15, 1.000000000000000000 ) ) ;
#247074 = ORIENTED_EDGE ( 'NONE', *, *, #25258, .F. ) ;
#247073 = FACE_OUTER_BOUND ( 'NONE', #107984, .T. ) ;
#247075 = LINE ( 'NONE', #68466, #120214 ) ;
#247076 = EDGE_CURVE ( 'NONE', #114431, #223845, #108451, .T. ) ;
#247077 = DIRECTION ( 'NONE',  ( 1.000000000000000000, 0.000000000000000000, 0.000000000000000000 ) ) ;
#247078 = CARTESIAN_POINT ( 'NONE',  ( -16.92778301347296832, 10.00094491684660092, -121.4285181079681877 ) ) ;
#247079 = AXIS2_PLACEMENT_3D ( 'NONE', #18601, #79826, #40764 ) ;
#247080 = DIRECTION ( 'NONE',  ( -1.000000000000000000, -7.304098846218134667E-16, -5.311601492717084346E-30 ) ) ;
#247081 = CARTESIAN_POINT ( 'NONE',  ( -20.92356734117541706, 65.68026841930954163, -164.4725740131889893 ) ) ;
#247082 = DIRECTION ( 'NONE',  ( 0.000000000000000000, -0.8149014228131981064, 0.5795995782408966956 ) ) ;
#247083 = CIRCLE ( 'NONE', #134656, 0.1000000000000124678 ) ;
#247084 = DIRECTION ( 'NONE',  ( 1.000000000000000000, 0.000000000000000000, 0.000000000000000000 ) ) ;
#247086 = CARTESIAN_POINT ( 'NONE',  ( -23.25000000000000000, -1.835859311432481045, -78.60443916879853532 ) ) ;
#247085 = CIRCLE ( 'NONE', #18156, 0.09999999999998898659 ) ;
#247087 = VERTEX_POINT ( 'NONE', #110918 ) ;
#247088 = EDGE_LOOP ( 'NONE', ( #72963, #51040, #13604, #79852, #66610, #203371, #23622 ) ) ;
#247089 = EDGE_CURVE ( 'NONE', #105911, #230477, #41836, .T. ) ;
#247090 = TOROIDAL_SURFACE ( 'NONE', #230562, 11.65000000000000036, 0.1000000000000000056 ) ;
#247091 = ORIENTED_EDGE ( 'NONE', *, *, #243558, .T. ) ;
#247092 = EDGE_CURVE ( 'NONE', #138354, #184002, #216776, .T. ) ;
#247093 = CARTESIAN_POINT ( 'NONE',  ( -21.02374657821591342, 64.39999999919201912, -143.4513107143264108 ) ) ;
#247094 = CARTESIAN_POINT ( 'NONE',  ( 20.95561247346651967, 65.40499263480876380, -162.4293247175427837 ) ) ;
#247095 = ORIENTED_EDGE ( 'NONE', *, *, #20013, .T. ) ;
#247097 = AXIS2_PLACEMENT_3D ( 'NONE', #91562, #15906, #92833 ) ;
#247096 = PRESENTATION_STYLE_ASSIGNMENT (( #11077 ) ) ;
#247098 = CARTESIAN_POINT ( 'NONE',  ( 23.15000000000000213, -9.599999999988842347, -157.6060308773475640 ) ) ;
#247099 = VECTOR ( 'NONE', #157647, 1000.000000000000000 ) ;
#247100 = CARTESIAN_POINT ( 'NONE',  ( 20.86777300164944648, 10.33200063080771969, -206.5931674956642610 ) ) ;
#247101 = AXIS2_PLACEMENT_3D ( 'NONE', #248078, #8202, #48589 ) ;
#247102 = PRODUCT ( 'Moving End Attachment Flange', 'Moving End Attachment Flange', '', ( #198151 ) ) ;
#247103 = FACE_OUTER_BOUND ( 'NONE', #39394, .T. ) ;
#247104 = ORIENTED_EDGE ( 'NONE', *, *, #112659, .T. ) ;
#247105 = ORIENTED_EDGE ( 'NONE', *, *, #76576, .T. ) ;
#247106 = CIRCLE ( 'NONE', #43129, 0.09999999999998898659 ) ;
#247107 = CARTESIAN_POINT ( 'NONE',  ( -16.87036670365549895, 9.989418819312803066, -46.02043988269794994 ) ) ;
#247108 = DIRECTION ( 'NONE',  ( 1.000000000000000000, 0.000000000000000000, 0.000000000000000000 ) ) ;
#247109 = EDGE_LOOP ( 'NONE', ( #5681, #181374, #75799, #85060 ) ) ;
#247110 = EDGE_CURVE ( 'NONE', #87379, #3181, #166927, .T. ) ;
#247111 = DIRECTION ( 'NONE',  ( 0.000000000000000000, 0.1298341882519953583, 0.9915357197604862671 ) ) ;
#247113 = ORIENTED_EDGE ( 'NONE', *, *, #233097, .F. ) ;
#247112 = DIRECTION ( 'NONE',  ( 0.000000000000000000, 0.4721928772778128947, 0.8814952561688012000 ) ) ;
#247114 = DIRECTION ( 'NONE',  ( 0.7070776581709139474, -0.7071359030027652981, -2.453168425935592377E-14 ) ) ;
#247115 = CARTESIAN_POINT ( 'NONE',  ( 5.899999999999995914, -11.65000000000000036, 9.900000000000002132 ) ) ;
#247116 = AXIS2_PLACEMENT_3D ( 'NONE', #176336, #214160, #35551 ) ;
#247118 = VERTEX_POINT ( 'NONE', #66666 ) ;
#247117 = CARTESIAN_POINT ( 'NONE',  ( 20.94999999999999574, 74.75000000001232081, -162.0231074845243597 ) ) ;
#247119 = DIRECTION ( 'NONE',  ( 0.9880948137434723000, 0.1538461538461484146, -0.000000000000000000 ) ) ;
#247120 = CARTESIAN_POINT ( 'NONE',  ( -16.97048361161167307, 9.950000000011138823, -87.35888434443047856 ) ) ;
#247121 = CARTESIAN_POINT ( 'NONE',  ( 18.79999999999999716, 1.149999999999999911, 16.60000000000000142 ) ) ;
#247123 = ADVANCED_FACE ( 'NONE', ( #144893 ), #195958, .T. ) ;
#247122 = CARTESIAN_POINT ( 'NONE',  ( 23.15000000000000213, -8.999999999988844479, -143.8939691226524644 ) ) ;
#247124 = AXIS2_PLACEMENT_3D ( 'NONE', #62674, #87342, #242570 ) ;
#247126 = CARTESIAN_POINT ( 'NONE',  ( 20.97565083910961548, 10.47461740128996510, -108.0779431765885903 ) ) ;
#247125 = DIRECTION ( 'NONE',  ( -0.000000000000000000, 1.000000000000000000, 6.982962677686266711E-15 ) ) ;
#247127 = CARTESIAN_POINT ( 'NONE',  ( 18.49999999999999289, 10.41716543472751688, -91.84999999941936721 ) ) ;
#247128 = DIRECTION ( 'NONE',  ( 0.000000000000000000, -0.2128009952263678062, 0.9770955615653298398 ) ) ;
#247129 = FACE_OUTER_BOUND ( 'NONE', #51012, .T. ) ;
#247130 = DIRECTION ( 'NONE',  ( 1.000000000000000000, 0.000000000000000000, 0.000000000000000000 ) ) ;
#247132 = ORIENTED_EDGE ( 'NONE', *, *, #155569, .F. ) ;
#247131 = CIRCLE ( 'NONE', #193183, 0.1000000000000012546 ) ;
#247133 = EDGE_LOOP ( 'NONE', ( #113819, #64993, #82267, #234240 ) ) ;
#247135 = ORIENTED_EDGE ( 'NONE', *, *, #42462, .T. ) ;
#247134 = AXIS2_PLACEMENT_3D ( 'NONE', #24811, #27387, #104290 ) ;
#247136 = LINE ( 'NONE', #47643, #255389 ) ;
#247137 = AXIS2_PLACEMENT_3D ( 'NONE', #96152, #214828, #160022 ) ;
#247138 = VERTEX_POINT ( 'NONE', #225697 ) ;
#247139 = DIRECTION ( 'NONE',  ( 0.000000000000000000, 0.000000000000000000, -1.000000000000000000 ) ) ;
#247140 = ORIENTED_EDGE ( 'NONE', *, *, #180461, .T. ) ;
#247141 = FACE_OUTER_BOUND ( 'NONE', #6853, .T. ) ;
#247142 = CARTESIAN_POINT ( 'NONE',  ( 18.59999999999999076, 65.79142135624910281, -81.67310748452439384 ) ) ;
#247143 = ORIENTED_EDGE ( 'NONE', *, *, #162322, .F. ) ;
#247144 = CARTESIAN_POINT ( 'NONE',  ( -21.13422380239062548, 30.73306616121944046, -252.2058741929238295 ) ) ;
#247145 = AXIS2_PLACEMENT_3D ( 'NONE', #221352, #42735, #100116 ) ;
#247146 = VECTOR ( 'NONE', #218419, 1000.000000000000114 ) ;
#247147 = ORIENTED_EDGE ( 'NONE', *, *, #107678, .F. ) ;
#247148 = AXIS2_PLACEMENT_3D ( 'NONE', #130946, #94370, #111388 ) ;
#247150 = VERTEX_POINT ( 'NONE', #187903 ) ;
#247149 = CIRCLE ( 'NONE', #209573, 0.6000000000000033085 ) ;
#247151 = ORIENTED_EDGE ( 'NONE', *, *, #27256, .T. ) ;
#247152 = EDGE_CURVE ( 'NONE', #104087, #43473, #4377, .T. ) ;
#247153 = CARTESIAN_POINT ( 'NONE',  ( 21.05000000000000071, 6.649999999999999467, -12.15000000000000036 ) ) ;
#247154 = SURFACE_STYLE_FILL_AREA ( #208063 ) ;
#247155 = DIRECTION ( 'NONE',  ( -4.391705002472931063E-16, -0.9651348961777154178, 0.2617529984165040680 ) ) ;
#247156 = EDGE_CURVE ( 'NONE', #143381, #242523, #9249, .T. ) ;
#247157 = FACE_OUTER_BOUND ( 'NONE', #27003, .T. ) ;
#247158 = DIRECTION ( 'NONE',  ( 0.000000000000000000, 0.000000000000000000, 1.000000000000000000 ) ) ;
#247160 = FACE_OUTER_BOUND ( 'NONE', #5956, .T. ) ;
#247159 = DIRECTION ( 'NONE',  ( 0.000000000000000000, -7.189901751995743170E-15, 1.000000000000000000 ) ) ;
#247161 = CARTESIAN_POINT ( 'NONE',  ( 18.49999999999999289, 10.49142135624846439, -58.35000000000000853 ) ) ;
#247162 = ORIENTED_EDGE ( 'NONE', *, *, #101044, .F. ) ;
#247164 = CARTESIAN_POINT ( 'NONE',  ( 20.94999999999999574, 68.48451787451661232, -224.2224406095231757 ) ) ;
#247163 = DIRECTION ( 'NONE',  ( -1.000000000000000000, -0.000000000000000000, -0.000000000000000000 ) ) ;
#247165 = EDGE_CURVE ( 'NONE', #59053, #116446, #250104, .T. ) ;
#247166 = CARTESIAN_POINT ( 'NONE',  ( 20.85000000000000142, 76.00000000001165290, -61.72310748452430573 ) ) ;
#247167 = EDGE_CURVE ( 'NONE', #111741, #89189, #76921, .T. ) ;
#247168 = VERTEX_POINT ( 'NONE', #156507 ) ;
#247169 = CARTESIAN_POINT ( 'NONE',  ( -21.00000000000000000, -1.212568896937008089, -7.800000000000000711 ) ) ;
#247170 = CARTESIAN_POINT ( 'NONE',  ( 22.48660254037844197, 64.35000000001194564, -103.0731074845243853 ) ) ;
#247171 = CARTESIAN_POINT ( 'NONE',  ( 20.94999999999999929, 5.021051876504146399E-16, -29.40000000000000213 ) ) ;
#247172 = ORIENTED_EDGE ( 'NONE', *, *, #114224, .F. ) ;
#247173 = ADVANCED_FACE ( 'NONE', ( #232171 ), #194339, .F. ) ;
#247174 = DIRECTION ( 'NONE',  ( 0.000000000000000000, -1.000000000000000000, 0.000000000000000000 ) ) ;
#247175 = EDGE_CURVE ( 'NONE', #71326, #67212, #67111, .T. ) ;
#247176 = CARTESIAN_POINT ( 'NONE',  ( 21.97500000000000497, 9.750000000011153745, -188.7499999999999716 ) ) ;
#247177 = CARTESIAN_POINT ( 'NONE',  ( -1.739115166359751170E-14, 16.67126802362264826, -222.8016931105129004 ) ) ;
#247179 = EDGE_CURVE ( 'NONE', #99784, #8515, #21351, .T. ) ;
#247178 = ADVANCED_FACE ( 'NONE', ( #16975 ), #14419, .T. ) ;
#247180 = ORIENTED_EDGE ( 'NONE', *, *, #79147, .T. ) ;
#247181 = ORIENTED_EDGE ( 'NONE', *, *, #29314, .T. ) ;
#247182 = VECTOR ( 'NONE', #185397, 1000.000000000000000 ) ;
#247183 = CARTESIAN_POINT ( 'NONE',  ( 18.39999999999999503, 11.75000000001113953, -180.1499999999999773 ) ) ;
#247184 = ORIENTED_EDGE ( 'NONE', *, *, #140070, .T. ) ;
#247185 = CARTESIAN_POINT ( 'NONE',  ( -16.94107738177415357, 65.98576071487568129, -157.4731074845244621 ) ) ;
#247186 = CARTESIAN_POINT ( 'NONE',  ( 18.44444291854882678, 85.49010118095492317, -62.89420351963329381 ) ) ;
#247187 = CARTESIAN_POINT ( 'NONE',  ( -20.94999027547553894, 10.29326151435327219, -206.4592822510414578 ) ) ;
#247188 = ORIENTED_EDGE ( 'NONE', *, *, #70897, .F. ) ;
#247189 = DIRECTION ( 'NONE',  ( 0.000000000000000000, 0.7035695228903320331, 0.7106264324241468033 ) ) ;
#247190 = EDGE_CURVE ( 'NONE', #17539, #153145, #171221, .T. ) ;
#247191 = FACE_OUTER_BOUND ( 'NONE', #176410, .T. ) ;
#247192 = CARTESIAN_POINT ( 'NONE',  ( -18.59999999999999787, 77.83534155023646406, -124.9679561919613064 ) ) ;
#247193 = DIRECTION ( 'NONE',  ( 2.715809747126111577E-16, 0.4088369013363273852, -0.9126074666063772600 ) ) ;
#247194 = ADVANCED_FACE ( 'NONE', ( #33996 ), #83650, .T. ) ;
#247196 = EDGE_CURVE ( 'NONE', #194619, #91227, #133064, .T. ) ;
#247195 = AXIS2_PLACEMENT_3D ( 'NONE', #167502, #68383, #41455 ) ;
#247198 = VERTEX_POINT ( 'NONE', #211307 ) ;
#247197 = VECTOR ( 'NONE', #169388, 1000.000000000000114 ) ;
#247199 = DIRECTION ( 'NONE',  ( -0.000000000000000000, -0.2128009952263603677, 0.9770955615653313941 ) ) ;
#247200 = VECTOR ( 'NONE', #182712, 1000.000000000000000 ) ;
#247201 = EDGE_CURVE ( 'NONE', #56486, #207747, #146219, .T. ) ;
#247203 = ORIENTED_EDGE ( 'NONE', *, *, #11387, .F. ) ;
#247202 = DIRECTION ( 'NONE',  ( -1.000000000000000000, 0.000000000000000000, -0.000000000000000000 ) ) ;
#247204 = DIRECTION ( 'NONE',  ( 0.000000000000000000, 0.9126074666063769270, 0.4088369013363280513 ) ) ;
#247205 = LINE ( 'NONE', #242068, #122530 ) ;
#247206 = CARTESIAN_POINT ( 'NONE',  ( 20.27550659511088682, 66.78395627750377628, -194.2731074845244166 ) ) ;
#247207 = LINE ( 'NONE', #206811, #250353 ) ;
#247208 = CYLINDRICAL_SURFACE ( 'NONE', #58886, 4.049999999999998046 ) ;
#247209 = EDGE_CURVE ( 'NONE', #132867, #47267, #35278, .T. ) ;
#247210 = CARTESIAN_POINT ( 'NONE',  ( 21.14999999999999503, 76.10000000001276987, -215.1726782920691505 ) ) ;
#247211 = FACE_OUTER_BOUND ( 'NONE', #46461, .T. ) ;
#247212 = ORIENTED_EDGE ( 'NONE', *, *, #142093, .F. ) ;
#247213 = DIRECTION ( 'NONE',  ( 0.000000000000000000, 1.000000000000000000, 0.000000000000000000 ) ) ;
#247214 = CARTESIAN_POINT ( 'NONE',  ( 23.14999999999999858, 5.900000000011162093, -90.28090023534366537 ) ) ;
#247215 = DIRECTION ( 'NONE',  ( 1.000000000000000000, 0.000000000000000000, -0.000000000000000000 ) ) ;
#247216 = LINE ( 'NONE', #227652, #129501 ) ;
#247217 = VECTOR ( 'NONE', #176746, 1000.000000000000000 ) ;
#247218 = LINE ( 'NONE', #43896, #117358 ) ;
#247219 = AXIS2_PLACEMENT_3D ( 'NONE', #129309, #228425, #230999 ) ;
#247221 = ORIENTED_EDGE ( 'NONE', *, *, #17319, .F. ) ;
#247220 = AXIS2_PLACEMENT_3D ( 'NONE', #202285, #79737, #23676 ) ;
#247222 = ORIENTED_EDGE ( 'NONE', *, *, #119733, .F. ) ;
#247224 = FACE_OUTER_BOUND ( 'NONE', #233878, .T. ) ;
#247223 = CIRCLE ( 'NONE', #151588, 0.1000000000000028644 ) ;
#247225 = DIRECTION ( 'NONE',  ( 0.000000000000000000, 0.000000000000000000, -1.000000000000000000 ) ) ;
#247226 = CARTESIAN_POINT ( 'NONE',  ( 18.39999999999999503, 54.09900352584866567, -229.1663746252470446 ) ) ;
#247227 = CARTESIAN_POINT ( 'NONE',  ( -23.25000000000000355, 10.05000000001113847, -46.25000000000000711 ) ) ;
#247228 = AXIS2_PLACEMENT_3D ( 'NONE', #234298, #214739, #136466 ) ;
#247229 = VECTOR ( 'NONE', #61061, 1000.000000000000000 ) ;
#247230 = DIRECTION ( 'NONE',  ( 0.000000000000000000, -0.9908441862701596881, 0.1350103645451904977 ) ) ;
#247231 = CIRCLE ( 'NONE', #188804, 0.09999999999999939493 ) ;
#247232 = DIRECTION ( 'NONE',  ( -0.000000000000000000, -1.000000000000000000, 0.000000000000000000 ) ) ;
#247233 = VERTEX_POINT ( 'NONE', #71814 ) ;
#247234 = CARTESIAN_POINT ( 'NONE',  ( -21.44999999999999929, 7.150000000011155876, -112.8500000000000369 ) ) ;
#247235 = VERTEX_POINT ( 'NONE', #96467 ) ;
#247236 = DIRECTION ( 'NONE',  ( 0.000000000000000000, -0.5774316882803290918, -0.8164390028469542537 ) ) ;
#247237 = FACE_OUTER_BOUND ( 'NONE', #195263, .T. ) ;
#247238 = DIRECTION ( 'NONE',  ( 0.000000000000000000, 0.8814952561688513821, -0.4721928772777189698 ) ) ;
#247240 = AXIS2_PLACEMENT_3D ( 'NONE', #199489, #216449, #238589 ) ;
#247239 = CARTESIAN_POINT ( 'NONE',  ( -22.49436431346200038, 11.64995094765345840, 0.06690352972225574457 ) ) ;
#247241 = LINE ( 'NONE', #167748, #177102 ) ;
#247242 = CARTESIAN_POINT ( 'NONE',  ( 18.49999999999998934, 64.35000000001197407, -111.7731074845243739 ) ) ;
#247243 = VECTOR ( 'NONE', #84288, 1000.000000000000000 ) ;
#247244 = CARTESIAN_POINT ( 'NONE',  ( -20.94999999999999929, -1.249999999999999334, -8.000000000000000000 ) ) ;
#247245 = ORIENTED_EDGE ( 'NONE', *, *, #184073, .F. ) ;
#247246 = AXIS2_PLACEMENT_3D ( 'NONE', #110618, #34977, #132773 ) ;
#247247 = EDGE_CURVE ( 'NONE', #174796, #42536, #33846, .T. ) ;
#247248 = DIRECTION ( 'NONE',  ( 0.000000000000000000, 0.2617529984165152257, 0.9651348961777124202 ) ) ;
#247249 = DIRECTION ( 'NONE',  ( 0.000000000000000000, 0.2617529984165152257, 0.9651348961777124202 ) ) ;
#247250 = DIRECTION ( 'NONE',  ( -0.000000000000000000, -0.1298341882519805091, -0.9915357197604881545 ) ) ;
#247251 = EDGE_CURVE ( 'NONE', #142560, #171657, #234724, .T. ) ;
#247252 = DIRECTION ( 'NONE',  ( 0.000000000000000000, 1.000000000000000000, 2.891205793294679805E-16 ) ) ;
#247253 = VERTEX_POINT ( 'NONE', #74403 ) ;
#247254 = CARTESIAN_POINT ( 'NONE',  ( 23.14999999999999858, 80.00000000001215028, -136.5231074845243029 ) ) ;
#247256 = EDGE_CURVE ( 'NONE', #219396, #62719, #176060, .T. ) ;
#247255 = CARTESIAN_POINT ( 'NONE',  ( 23.14999999999999858, 70.05000000001197691, -113.3288097895591591 ) ) ;
#247258 = EDGE_CURVE ( 'NONE', #25677, #197537, #8669, .T. ) ;
#247257 = ORIENTED_EDGE ( 'NONE', *, *, #223417, .T. ) ;
#247259 = ORIENTED_EDGE ( 'NONE', *, *, #184762, .F. ) ;
#247260 = CARTESIAN_POINT ( 'NONE',  ( 18.59999999999999076, 78.57213941646344324, -232.7862224702232652 ) ) ;
#247261 = FACE_BOUND ( 'NONE', #3758, .T. ) ;
#247262 = DIRECTION ( 'NONE',  ( 0.000000000000000000, -1.734723475976757554E-14, 1.000000000000000000 ) ) ;
#247263 = AXIS2_PLACEMENT_3D ( 'NONE', #227699, #25669, #89471 ) ;
#247264 = EDGE_LOOP ( 'NONE', ( #214589, #224336, #20451, #40576 ) ) ;
#247265 = FACE_OUTER_BOUND ( 'NONE', #43280, .T. ) ;
#247266 = DIRECTION ( 'NONE',  ( 0.000000000000000000, 0.000000000000000000, 1.000000000000000000 ) ) ;
#247268 = ORIENTED_EDGE ( 'NONE', *, *, #27624, .F. ) ;
#247267 = AXIS2_PLACEMENT_3D ( 'NONE', #3865, #40466, #143368 ) ;
#247269 = EDGE_CURVE ( 'NONE', #81634, #159242, #204475, .T. ) ;
#247270 = EDGE_CURVE ( 'NONE', #23758, #190290, #212874, .T. ) ;
#247272 = DIRECTION ( 'NONE',  ( -0.000000000000000000, 1.000000000000000000, -1.224646799147352961E-16 ) ) ;
#247271 = CIRCLE ( 'NONE', #201485, 0.09999999999999484301 ) ;
#247273 = AXIS2_PLACEMENT_3D ( 'NONE', #127520, #106641, #207058 ) ;
#247274 = ORIENTED_EDGE ( 'NONE', *, *, #56101, .T. ) ;
#247275 = DIRECTION ( 'NONE',  ( 0.000000000000000000, -1.000000000000000000, 1.387778780781406043E-13 ) ) ;
#247276 = CARTESIAN_POINT ( 'NONE',  ( 18.39999999999999503, 67.23581240663841641, -214.2531594801197627 ) ) ;
#247277 = DIRECTION ( 'NONE',  ( 1.000000000000000000, -0.000000000000000000, -0.000000000000000000 ) ) ;
#247278 = CARTESIAN_POINT ( 'NONE',  ( -20.54999999999999716, 71.75000000001205080, -124.2731074845243313 ) ) ;
#247280 = AXIS2_PLACEMENT_3D ( 'NONE', #85553, #165139, #245966 ) ;
#247279 = DIRECTION ( 'NONE',  ( 0.000000000000000000, 0.000000000000000000, -1.000000000000000000 ) ) ;
#247281 = CARTESIAN_POINT ( 'NONE',  ( -21.53699400380208928, 69.21228820681695026, -203.5231074845244450 ) ) ;
#247282 = CYLINDRICAL_SURFACE ( 'NONE', #1749, 0.09999999999999108213 ) ;
#247283 = DIRECTION ( 'NONE',  ( 0.000000000000000000, 0.000000000000000000, -1.000000000000000000 ) ) ;
#247284 = CIRCLE ( 'NONE', #176586, 14.20833333333333748 ) ;
#247285 = LINE ( 'NONE', #226425, #38900 ) ;
#247286 = DIRECTION ( 'NONE',  ( 0.000000000000000000, 0.000000000000000000, -1.000000000000000000 ) ) ;
#247287 = VECTOR ( 'NONE', #60908, 1000.000000000000227 ) ;
#247290 = ORIENTED_EDGE ( 'NONE', *, *, #86783, .F. ) ;
#247289 = ADVANCED_FACE ( 'NONE', ( #52215 ), #32716, .F. ) ;
#247288 = CARTESIAN_POINT ( 'NONE',  ( 18.50000000000000355, 86.87366311306884370, -199.3414869250131858 ) ) ;
#247291 = EDGE_LOOP ( 'NONE', ( #103323, #62669, #200342, #108926 ) ) ;
#247293 = CARTESIAN_POINT ( 'NONE',  ( -14.56336952470180002, 9.446645344706402270, -85.41080645610024646 ) ) ;
#247292 = FACE_OUTER_BOUND ( 'NONE', #201956, .T. ) ;
#247294 = CIRCLE ( 'NONE', #234848, 0.09999999999999961697 ) ;
#247296 = ORIENTED_EDGE ( 'NONE', *, *, #192520, .F. ) ;
#247295 = DIRECTION ( 'NONE',  ( 1.000000000000000000, 0.000000000000000000, 0.000000000000000000 ) ) ;
#247297 = ORIENTED_EDGE ( 'NONE', *, *, #157215, .T. ) ;
#247298 = EDGE_CURVE ( 'NONE', #33088, #180036, #246189, .T. ) ;
#247299 = DIRECTION ( 'NONE',  ( -0.000000000000000000, -0.000000000000000000, 1.000000000000000000 ) ) ;
#247300 = CARTESIAN_POINT ( 'NONE',  ( 23.14999999999999858, -3.999999999988843147, -134.0000000000000284 ) ) ;
#247301 = AXIS2_PLACEMENT_3D ( 'NONE', #97564, #256610, #42756 ) ;
#247302 = FACE_OUTER_BOUND ( 'NONE', #239617, .T. ) ;
#247303 = DIRECTION ( 'NONE',  ( 0.000000000000000000, 1.000000000000000000, 6.938893903907222067E-15 ) ) ;
#247304 = DIRECTION ( 'NONE',  ( 0.000000000000000000, -1.000000000000000000, 0.000000000000000000 ) ) ;
#247305 = VECTOR ( 'NONE', #170930, 1000.000000000000000 ) ;
#247307 = ADVANCED_FACE ( 'NONE', ( #199466 ), #59907, .T. ) ;
#247306 = LINE ( 'NONE', #68688, #144606 ) ;
#247308 = EDGE_CURVE ( 'NONE', #205206, #235613, #258082, .T. ) ;
#247309 = CARTESIAN_POINT ( 'NONE',  ( 13.99999999999999822, 9.850000000011137402, -184.2499999999999716 ) ) ;
#247310 = AXIS2_PLACEMENT_3D ( 'NONE', #51747, #88300, #152191 ) ;
#247311 = ORIENTED_EDGE ( 'NONE', *, *, #93281, .F. ) ;
#247312 = ORIENTED_EDGE ( 'NONE', *, *, #1025, .T. ) ;
#247313 = DIRECTION ( 'NONE',  ( 0.000000000000000000, 0.000000000000000000, -1.000000000000000000 ) ) ;
#247314 = EDGE_CURVE ( 'NONE', #253610, #171646, #192044, .T. ) ;
#247315 = VERTEX_POINT ( 'NONE', #140751 ) ;
#247316 = DIRECTION ( 'NONE',  ( 1.000000000000000000, 0.000000000000000000, -0.000000000000000000 ) ) ;
#247317 = ORIENTED_EDGE ( 'NONE', *, *, #93407, .T. ) ;
#247319 = CIRCLE ( 'NONE', #201352, 11.65000000000000036 ) ;
#247318 = CARTESIAN_POINT ( 'NONE',  ( 21.14999999999999503, 76.00000000001213607, -136.5231074845242745 ) ) ;
#247320 = AXIS2_PLACEMENT_3D ( 'NONE', #113935, #55218, #235181 ) ;
#247321 = VECTOR ( 'NONE', #6040, 1000.000000000000000 ) ;
#247322 = CARTESIAN_POINT ( 'NONE',  ( -23.25000000000000000, 18.60970618848720903, -231.2322896185303875 ) ) ;
#247323 = CARTESIAN_POINT ( 'NONE',  ( 18.49999999999999289, 65.65621891165837098, -44.69466220664676115 ) ) ;
#247324 = DIRECTION ( 'NONE',  ( 0.000000000000000000, 1.000000000000000000, 6.982962677686266711E-15 ) ) ;
#247325 = ORIENTED_EDGE ( 'NONE', *, *, #250346, .T. ) ;
#247326 = APPLICATION_CONTEXT ( 'automotive_design' ) ;
#247327 = EDGE_CURVE ( 'NONE', #24913, #212760, #92049, .T. ) ;
#247328 = CARTESIAN_POINT ( 'NONE',  ( 21.05000000000000071, 85.00000000001251976, -179.4170766071767389 ) ) ;
#247329 = ORIENTED_EDGE ( 'NONE', *, *, #46232, .F. ) ;
#247330 = CARTESIAN_POINT ( 'NONE',  ( -16.89021194854739605, 66.05000000001153637, -48.78053935292005150 ) ) ;
#247331 = DIRECTION ( 'NONE',  ( -0.000000000000000000, -1.000000000000000000, 0.000000000000000000 ) ) ;
#247332 = DIRECTION ( 'NONE',  ( 2.694716079187273439E-16, 1.000000000000000000, 6.467318590049456648E-15 ) ) ;
#247333 = ADVANCED_FACE ( 'NONE', ( #198155 ), #108628, .T. ) ;
#247334 = EDGE_LOOP ( 'NONE', ( #158183, #94444, #59350 ) ) ;
#247335 = DIRECTION ( 'NONE',  ( 0.000000000000000000, 0.000000000000000000, 1.000000000000000000 ) ) ;
#247336 = EDGE_LOOP ( 'NONE', ( #47531, #13067, #96246, #219721 ) ) ;
#247339 = VERTEX_POINT ( 'NONE', #24686 ) ;
#247338 = DIRECTION ( 'NONE',  ( 0.000000000000000000, 0.000000000000000000, -1.000000000000000000 ) ) ;
#247337 = LINE ( 'NONE', #223912, #82618 ) ;
#247340 = AXIS2_PLACEMENT_3D ( 'NONE', #94333, #155643, #154368 ) ;
#247341 = VECTOR ( 'NONE', #154657, 1000.000000000000000 ) ;
#247342 = CARTESIAN_POINT ( 'NONE',  ( 21.05000000000000071, 76.10000000001245724, -181.6726782920691505 ) ) ;
#247343 = AXIS2_PLACEMENT_3D ( 'NONE', #144113, #42463, #201536 ) ;
#247344 = ORIENTED_EDGE ( 'NONE', *, *, #257792, .T. ) ;
#247345 = FACE_OUTER_BOUND ( 'NONE', #1917, .T. ) ;
#247346 = ORIENTED_EDGE ( 'NONE', *, *, #131754, .F. ) ;
#247347 = EDGE_CURVE ( 'NONE', #143316, #29024, #125395, .T. ) ;
#247349 = CARTESIAN_POINT ( 'NONE',  ( 18.39999999999999503, 11.75000000001113953, -124.7500000000000426 ) ) ;
#247348 =( BOUNDED_SURFACE ( )  B_SPLINE_SURFACE ( 3, 2, ( 
 ( #255220, #14123, #34988 ),
 ( #76631, #156205, #235702 ),
 ( #57041, #231886, #111937 ),
 ( #53227, #37526, #91071 ),
 ( #170661, #250146, #132786 ),
 ( #131478, #211021, #32414 ) ),
 .UNSPECIFIED., .F., .F., .F. ) 
 B_SPLINE_SURFACE_WITH_KNOTS ( ( 4, 2, 4 ),
 ( 3, 3 ),
 ( 0.0001381104793128129277, 0.0002947094729387753141, 0.0004513084665647377276 ),
 ( 0.000000000000000000, 1.000000000000000000 ),
 .UNSPECIFIED. ) 
 GEOMETRIC_REPRESENTATION_ITEM ( )  RATIONAL_B_SPLINE_SURFACE ( (
 ( 1.000000000000000000, 0.7071067811864075736, 1.000000000000000000),
 ( 1.000000000000000000, 0.6919563088091734704, 1.000000000000000000),
 ( 1.000000000000000000, 0.6959445945726734362, 1.000000000000000000),
 ( 1.000000000000000000, 0.7137882985306041039, 1.000000000000000000),
 ( 1.000000000000000000, 0.7257496306101467454, 1.000000000000000000),
 ( 1.000000000000000000, 0.7250110520820811644, 1.000000000000000000) ) ) 
 REPRESENTATION_ITEM ( '' )  SURFACE ( )  );
#247350 = CARTESIAN_POINT ( 'NONE',  ( -23.25000000000000000, 76.00000000001170974, -69.52310748452431710 ) ) ;
#247351 = FACE_OUTER_BOUND ( 'NONE', #23000, .T. ) ;
#247352 = DIRECTION ( 'NONE',  ( -1.000000000000000000, 0.000000000000000000, 0.000000000000000000 ) ) ;
#247353 = ORIENTED_EDGE ( 'NONE', *, *, #229521, .F. ) ;
#247354 = CARTESIAN_POINT ( 'NONE',  ( -16.93302609847409457, 44.05834383477297678, -235.2823355200077344 ) ) ;
#247355 =( NAMED_UNIT ( * ) PLANE_ANGLE_UNIT ( ) SI_UNIT ( $, .RADIAN. ) );
#247356 = CARTESIAN_POINT ( 'NONE',  ( -12.25000000000000178, 66.65000000001228386, -153.2731074845244166 ) ) ;
#247357 = ORIENTED_EDGE ( 'NONE', *, *, #60540, .F. ) ;
#247358 = CARTESIAN_POINT ( 'NONE',  ( 18.59999999999999076, 10.20857864376269575, -21.35000000000000142 ) ) ;
#247359 = ORIENTED_EDGE ( 'NONE', *, *, #103839, .F. ) ;
#247360 = DIRECTION ( 'NONE',  ( -1.000000000000000000, 0.000000000000000000, 0.000000000000000000 ) ) ;
#247361 = EDGE_LOOP ( 'NONE', ( #248322, #190970, #68485, #173710 ) ) ;
#247362 = TOROIDAL_SURFACE ( 'NONE', #172409, 0.2000000000000000111, 0.1000000000000000056 ) ;
#247363 = CARTESIAN_POINT ( 'NONE',  ( -23.25000000000000000, 11.65000000001115588, -155.7499999999999716 ) ) ;
#247364 = CARTESIAN_POINT ( 'NONE',  ( -22.39999999999999858, 76.00000000001246292, -181.6726782920691505 ) ) ;
#247366 = EDGE_LOOP ( 'NONE', ( #95279, #82874, #39838, #34910 ) ) ;
#247365 = DIRECTION ( 'NONE',  ( 0.000000000000000000, -1.000000000000000000, -6.982962677686265922E-15 ) ) ;
#247367 = CARTESIAN_POINT ( 'NONE',  ( -20.54999999999999716, 7.250000000011155521, -79.25000000000004263 ) ) ;
#247368 = LINE ( 'NONE', #148284, #218678 ) ;
#247369 = VERTEX_POINT ( 'NONE', #218998 ) ;
#247370 = CARTESIAN_POINT ( 'NONE',  ( -21.65000000000000213, 9.950000000011140600, -121.2500000000000426 ) ) ;
#247371 = FACE_OUTER_BOUND ( 'NONE', #72868, .T. ) ;
#247372 = ORIENTED_EDGE ( 'NONE', *, *, #122264, .F. ) ;
#247373 = LINE ( 'NONE', #209546, #90702 ) ;
#247374 = CIRCLE ( 'NONE', #39314, 0.09999999999999939493 ) ;
#247375 = ORIENTED_EDGE ( 'NONE', *, *, #64106, .F. ) ;
#247376 = CIRCLE ( 'NONE', #118411, 0.1000000000000028644 ) ;
#247377 = CIRCLE ( 'NONE', #10062, 0.1000000000000055844 ) ;
#247378 = DIRECTION ( 'NONE',  ( 0.000000000000000000, 0.000000000000000000, -1.000000000000000000 ) ) ;
#247379 = DIRECTION ( 'NONE',  ( 0.000000000000000000, -7.056502275159890832E-15, 1.000000000000000000 ) ) ;
#247380 = EDGE_CURVE ( 'NONE', #92448, #136069, #121233, .T. ) ;
#247383 = EDGE_LOOP ( 'NONE', ( #37099, #126118, #181850, #120053 ) ) ;
#247382 = ORIENTED_EDGE ( 'NONE', *, *, #166687, .F. ) ;
#247381 = DIRECTION ( 'NONE',  ( 1.000000000000000000, 0.000000000000000000, 0.000000000000000000 ) ) ;
#247384 = ADVANCED_FACE ( 'NONE', ( #200731 ), #22110, .T. ) ;
#247385 = DIRECTION ( 'NONE',  ( 0.000000000000000000, 0.000000000000000000, -1.000000000000000000 ) ) ;
#247386 = EDGE_CURVE ( 'NONE', #206950, #10892, #63782, .T. ) ;
#247387 = LINE ( 'NONE', #127456, #119009 ) ;
#247388 = DIRECTION ( 'NONE',  ( 0.000000000000000000, 0.7397360091702792628, -0.6728971962616790981 ) ) ;
#247389 = AXIS2_PLACEMENT_3D ( 'NONE', #25088, #61618, #104559 ) ;
#247391 = DIRECTION ( 'NONE',  ( -0.8049926720990042694, -0.5932847527679310229, 0.000000000000000000 ) ) ;
#247390 = CARTESIAN_POINT ( 'NONE',  ( 18.59999999999999076, 6.450000000011156587, -43.51702717044002355 ) ) ;
#247392 = CARTESIAN_POINT ( 'NONE',  ( 22.47071067811865319, 75.90090754530959316, -144.2431822290223522 ) ) ;
#247393 = PLANE ( 'NONE',  #52536 ) ;
#247394 = CARTESIAN_POINT ( 'NONE',  ( 20.94999999999999929, 76.00000000001190870, -103.0231074845243029 ) ) ;
#247395 = CIRCLE ( 'NONE', #218348, 0.1000000000000027534 ) ;
#247396 = CARTESIAN_POINT ( 'NONE',  ( -23.25000000000000355, 20.83093076766827423, -227.7429161672744442 ) ) ;
#247397 = TOROIDAL_SURFACE ( 'NONE', #122334, 0.2000000000000000111, 0.1000000000000000056 ) ;
#247398 = EDGE_LOOP ( 'NONE', ( #122236, #194504, #208201, #67780 ) ) ;
#247399 = ORIENTED_EDGE ( 'NONE', *, *, #234342, .T. ) ;
#247400 = CIRCLE ( 'NONE', #222435, 0.09999999999998898659 ) ;
#247401 = CARTESIAN_POINT ( 'NONE',  ( -20.94560253601877164, 64.25000000001175238, -76.51302397200892358 ) ) ;
#247402 = AXIS2_PLACEMENT_3D ( 'NONE', #130503, #224467, #76949 ) ;
#247404 = ORIENTED_EDGE ( 'NONE', *, *, #36224, .F. ) ;
#247403 = FACE_OUTER_BOUND ( 'NONE', #210690, .T. ) ;
#247405 = ORIENTED_EDGE ( 'NONE', *, *, #195659, .T. ) ;
#247406 = ADVANCED_FACE ( 'NONE', ( #239866 ), #61217, .F. ) ;
#247407 = DIRECTION ( 'NONE',  ( -1.000000000000000000, 0.000000000000000000, -1.020425574104004196E-15 ) ) ;
#247408 = ORIENTED_EDGE ( 'NONE', *, *, #208587, .F. ) ;
#247409 = FACE_OUTER_BOUND ( 'NONE', #98233, .T. ) ;
#247410 = AXIS2_PLACEMENT_3D ( 'NONE', #65944, #25544, #125900 ) ;
#247411 = VECTOR ( 'NONE', #180581, 1000.000000000000000 ) ;
#247412 = ORIENTED_EDGE ( 'NONE', *, *, #193394, .F. ) ;
#247413 = AXIS2_PLACEMENT_3D ( 'NONE', #219060, #20905, #247275 ) ;
#247414 = DIRECTION ( 'NONE',  ( 0.000000000000000000, 1.000000000000000000, 0.000000000000000000 ) ) ;
#247415 = CARTESIAN_POINT ( 'NONE',  ( -20.94999999999999929, 1.835341550235569663, -45.05515129256298223 ) ) ;
#247416 = AXIS2_PLACEMENT_3D ( 'NONE', #33143, #47504, #207907 ) ;
#247418 = EDGE_LOOP ( 'NONE', ( #166743, #84688, #66533, #206373 ) ) ;
#247417 = ORIENTED_EDGE ( 'NONE', *, *, #38022, .F. ) ;
#247419 = ORIENTED_EDGE ( 'NONE', *, *, #136394, .T. ) ;
#247420 = CARTESIAN_POINT ( 'NONE',  ( -20.65000000000000568, 70.35000000001210196, -127.2731074845243313 ) ) ;
#247421 = ORIENTED_EDGE ( 'NONE', *, *, #77527, .F. ) ;
#247422 = ORIENTED_EDGE ( 'NONE', *, *, #103416, .F. ) ;
#247424 = CARTESIAN_POINT ( 'NONE',  ( 20.85000000000000142, 7.120270961708750512, -104.1595630418393768 ) ) ;
#247423 = TOROIDAL_SURFACE ( 'NONE', #139067, 12.77499999999999858, 0.1000000000000000056 ) ;
#247425 = CARTESIAN_POINT ( 'NONE',  ( 18.59999999999999432, -9.480686695267811714, -73.94111516875786094 ) ) ;
#247426 = LINE ( 'NONE', #210875, #122986 ) ;
#247428 = ORIENTED_EDGE ( 'NONE', *, *, #214066, .T. ) ;
#247427 = CARTESIAN_POINT ( 'NONE',  ( 18.59999999999999076, 64.35000000001197407, -111.6731074845243796 ) ) ;
#247429 = EDGE_CURVE ( 'NONE', #209763, #217421, #254351, .T. ) ;
#247430 = ADVANCED_FACE ( 'NONE', ( #82025 ), #241155, .F. ) ;
#247431 = CARTESIAN_POINT ( 'NONE',  ( -21.45000000000000284, 7.708578643773852157, -112.8500000000000369 ) ) ;
#247432 = CARTESIAN_POINT ( 'NONE',  ( 18.52928932188133970, 65.72071067813045886, -81.67310748452439384 ) ) ;
#247434 = VERTEX_POINT ( 'NONE', #203295 ) ;
#247433 = CARTESIAN_POINT ( 'NONE',  ( -16.87683809663752399, 23.65833333334447985, -83.75000000000004263 ) ) ;
#247435 = FACE_OUTER_BOUND ( 'NONE', #253443, .T. ) ;
#247436 = VERTEX_POINT ( 'NONE', #182466 ) ;
#247437 = AXIS2_PLACEMENT_3D ( 'NONE', #253102, #75776, #234844 ) ;
#247438 = DIRECTION ( 'NONE',  ( 0.000000000000000000, -1.000000000000000000, 0.000000000000000000 ) ) ;
#247439 = CIRCLE ( 'NONE', #47510, 0.1000000000000028644 ) ;
#247440 = B_SPLINE_CURVE_WITH_KNOTS ( 'NONE', 3,
 ( #93804, #216316, #15591, #113381, #35167, #95097, #238458, #33891, #136779, #237183 ),
 .UNSPECIFIED., .F., .F.,
 ( 4, 3, 3, 4 ),
 ( 0.000000000000000000, 0.0002000000000008589688, 0.001000000000082969676, 0.001967863649483315904 ),
 .UNSPECIFIED. ) ;
#247441 = VERTEX_POINT ( 'NONE', #3813 ) ;
#247442 = AXIS2_PLACEMENT_3D ( 'NONE', #161315, #240841, #3491 ) ;
#247443 = CARTESIAN_POINT ( 'NONE',  ( -20.95613430942368538, 18.72165599329057883, -226.6130354132794480 ) ) ;
#247444 = LINE ( 'NONE', #31006, #245353 ) ;
#247445 = ADVANCED_FACE ( 'NONE', ( #83311 ), #78199, .F. ) ;
#247446 = VERTEX_POINT ( 'NONE', #217697 ) ;
#247448 = DIRECTION ( 'NONE',  ( 1.000000000000000000, 0.000000000000000000, 0.000000000000000000 ) ) ;
#247447 = DIRECTION ( 'NONE',  ( -1.000000000000000000, 1.836970198721029934E-16, 1.282749433769087582E-30 ) ) ;
#247449 = CARTESIAN_POINT ( 'NONE',  ( -23.15000000000000213, 84.66355140188063899, -45.54720860259156723 ) ) ;
#247450 = DIRECTION ( 'NONE',  ( 1.000000000000000000, -0.000000000000000000, -0.000000000000000000 ) ) ;
#247451 = FACE_OUTER_BOUND ( 'NONE', #147905, .T. ) ;
#247452 = VERTEX_POINT ( 'NONE', #205858 ) ;
#247453 = ORIENTED_EDGE ( 'NONE', *, *, #238232, .F. ) ;
#247454 =( BOUNDED_CURVE ( )  B_SPLINE_CURVE ( 3, ( #192568, #115587, #51740, #175583 ),
 .UNSPECIFIED., .F., .F. ) 
 B_SPLINE_CURVE_WITH_KNOTS ( ( 4, 4 ),
 ( 3.192897208853993085, 4.712388980384689674 ),
 .UNSPECIFIED. ) 
 CURVE ( )  GEOMETRIC_REPRESENTATION_ITEM ( )  RATIONAL_B_SPLINE_CURVE ( ( 1.000000000000000000, 0.8166740347213228279, 0.8166740347213228279, 1.000000000000000000 ) ) 
 REPRESENTATION_ITEM ( '' )  );
#247455 = CARTESIAN_POINT ( 'NONE',  ( -18.40000000000000213, 64.25000000001151079, -45.27310748452440237 ) ) ;
#247456 = DIRECTION ( 'NONE',  ( 1.000000000000000000, 0.000000000000000000, 0.000000000000000000 ) ) ;
#247457 = ORIENTED_EDGE ( 'NONE', *, *, #236087, .T. ) ;
#247458 = DIRECTION ( 'NONE',  ( 0.000000000000000000, -1.000000000000000000, -6.982962677686265922E-15 ) ) ;
#247459 = ORIENTED_EDGE ( 'NONE', *, *, #147406, .T. ) ;
#247460 = LINE ( 'NONE', #31021, #98177 ) ;
#247461 = VERTEX_POINT ( 'NONE', #70235 ) ;
#247462 = DIRECTION ( 'NONE',  ( 0.000000000000000000, -1.000000000000000000, -6.982962677686265922E-15 ) ) ;
#247463 = EDGE_CURVE ( 'NONE', #3601, #159137, #127615, .T. ) ;
#247464 = DIRECTION ( 'NONE',  ( -1.000000000000000000, 1.875376730785737719E-16, 1.309568571767809260E-30 ) ) ;
#247465 = AXIS2_PLACEMENT_3D ( 'NONE', #116130, #195683, #136957 ) ;
#247466 = CIRCLE ( 'NONE', #135008, 0.09999999999999344136 ) ;
#247467 = ORIENTED_EDGE ( 'NONE', *, *, #84327, .T. ) ;
#247468 = CARTESIAN_POINT ( 'NONE',  ( 16.27683809663750125, 66.65000000001234071, -160.7731074845244166 ) ) ;
#247469 = AXIS2_PLACEMENT_3D ( 'NONE', #137596, #159761, #123199 ) ;
#247470 = ORIENTED_EDGE ( 'NONE', *, *, #5094, .T. ) ;
#247471 = EDGE_LOOP ( 'NONE', ( #207933, #242351, #51590, #123684 ) ) ;
#247472 = ORIENTED_EDGE ( 'NONE', *, *, #242448, .F. ) ;
#247473 = AXIS2_PLACEMENT_3D ( 'NONE', #148564, #110711, #70340 ) ;
#247474 = EDGE_CURVE ( 'NONE', #240042, #216736, #175296, .T. ) ;
#247475 = CARTESIAN_POINT ( 'NONE',  ( 23.15000000000000213, 84.66355140188136374, -146.0472086025916099 ) ) ;
#247476 = PLANE ( 'NONE',  #15716 ) ;
#247477 = VECTOR ( 'NONE', #221155, 1000.000000000000000 ) ;
#247478 = CARTESIAN_POINT ( 'NONE',  ( -21.07928932188134041, 0.09889514566555068775, -127.6714833436067238 ) ) ;
#247479 = DIRECTION ( 'NONE',  ( 0.000000000000000000, -0.8814952561688428334, 0.4721928772777350680 ) ) ;
#247480 = CARTESIAN_POINT ( 'NONE',  ( -16.87036670365548474, 9.989418819301645769, -20.97956011730205006 ) ) ;
#247482 = DIRECTION ( 'NONE',  ( 0.000000000000000000, -0.8103668758649578141, 0.5859227990963212784 ) ) ;
#247481 = CARTESIAN_POINT ( 'NONE',  ( 21.05000000000000071, 1.115488181425289110E-11, -160.9593430482987344 ) ) ;
#247484 = VERTEX_POINT ( 'NONE', #87178 ) ;
#247483 = CARTESIAN_POINT ( 'NONE',  ( -20.94999999999999929, 11.65000000001115232, -67.00000000000000000 ) ) ;
#247485 = DIRECTION ( 'NONE',  ( -1.000000000000000000, -9.792504721693619684E-16, -4.386921467590155985E-16 ) ) ;
#247486 = EDGE_LOOP ( 'NONE', ( #142323, #147875, #31564, #93528, #168693 ) ) ;
#247487 = TOROIDAL_SURFACE ( 'NONE', #135023, 0.2000000000000000111, 0.1000000000000000056 ) ;
#247488 = ADVANCED_FACE ( 'NONE', ( #68942 ), #108054, .T. ) ;
#247489 = DIRECTION ( 'NONE',  ( 1.000000000000000000, 0.000000000000000000, 0.000000000000000000 ) ) ;
#247490 = ADVANCED_FACE ( 'NONE', ( #128901 ), #187603, .T. ) ;
#247491 = ORIENTED_EDGE ( 'NONE', *, *, #4567, .T. ) ;
#247492 = ORIENTED_EDGE ( 'NONE', *, *, #146696, .T. ) ;
#247493 = CARTESIAN_POINT ( 'NONE',  ( -18.59999999999999787, 77.16412189325305349, -95.10825939895268277 ) ) ;
#247494 = AXIS2_PLACEMENT_3D ( 'NONE', #230130, #231434, #112757 ) ;
#247495 = DIRECTION ( 'NONE',  ( -1.000000000000000000, 0.000000000000000000, -0.000000000000000000 ) ) ;
#247496 = LINE ( 'NONE', #128844, #112796 ) ;
#247497 = DIRECTION ( 'NONE',  ( 1.000000000000000000, 0.000000000000000000, 0.000000000000000000 ) ) ;
#247498 = CIRCLE ( 'NONE', #55924, 11.65000000000000036 ) ;
#247499 = CIRCLE ( 'NONE', #68436, 0.09999999999999326095 ) ;
#247500 = EDGE_CURVE ( 'NONE', #229697, #181378, #67632, .T. ) ;
#247501 = FACE_OUTER_BOUND ( 'NONE', #210503, .T. ) ;
#247502 = EDGE_CURVE ( 'NONE', #92812, #7533, #150337, .T. ) ;
#247503 = ORIENTED_EDGE ( 'NONE', *, *, #21057, .T. ) ;
#247504 = EDGE_LOOP ( 'NONE', ( #86327, #185676, #140740, #144451 ) ) ;
#247505 = DIRECTION ( 'NONE',  ( -1.000000000000000000, -0.000000000000000000, -0.000000000000000000 ) ) ;
#247506 = VERTEX_POINT ( 'NONE', #208454 ) ;
#247507 = DIRECTION ( 'NONE',  ( 0.000000000000000000, 0.000000000000000000, -1.000000000000000000 ) ) ;
#247508 = DIRECTION ( 'NONE',  ( -0.000000000000000000, 0.2617529984165031243, 0.9651348961777157509 ) ) ;
#247509 = ORIENTED_EDGE ( 'NONE', *, *, #233704, .F. ) ;
#247510 = DIRECTION ( 'NONE',  ( 0.000000000000000000, -0.2617529984165031243, -0.9651348961777157509 ) ) ;
#247512 = ADVANCED_FACE ( 'NONE', ( #148467 ), #104506, .T. ) ;
#247511 = CARTESIAN_POINT ( 'NONE',  ( -23.15000000000000213, 6.757359537351773859, -220.2789794402638108 ) ) ;
#247513 = CARTESIAN_POINT ( 'NONE',  ( -2.995603634470829482E-16, -11.74999999998884448, -88.25000000000005684 ) ) ;
#247514 = DIRECTION ( 'NONE',  ( -0.000000000000000000, -0.000000000000000000, -1.000000000000000000 ) ) ;
#247515 = ORIENTED_EDGE ( 'NONE', *, *, #245706, .F. ) ;
#247516 = DIRECTION ( 'NONE',  ( 0.7071067811865487940, 0.7071067811865462405, -7.215498431451186046E-16 ) ) ;
#247517 = DIRECTION ( 'NONE',  ( 0.000000000000000000, -1.000000000000000000, 0.000000000000000000 ) ) ;
#247518 = DIRECTION ( 'NONE',  ( 1.000000000000000000, 0.000000000000000000, 0.000000000000000000 ) ) ;
#247519 = FACE_OUTER_BOUND ( 'NONE', #212135, .T. ) ;
#247520 = EDGE_CURVE ( 'NONE', #201638, #89621, #46251, .T. ) ;
#247521 = DIRECTION ( 'NONE',  ( 0.7071067811864846231, 0.2890913453341779626, -0.6453109281989296564 ) ) ;
#247522 = EDGE_CURVE ( 'NONE', #62638, #154602, #207157, .T. ) ;
#247523 = ADVANCED_FACE ( 'NONE', ( #247558 ), #10242, .T. ) ;
#247524 = VECTOR ( 'NONE', #125238, 1000.000000000000000 ) ;
#247525 = VECTOR ( 'NONE', #18099, 1000.000000000000000 ) ;
#247526 = ORIENTED_EDGE ( 'NONE', *, *, #130174, .T. ) ;
#247527 = AXIS2_PLACEMENT_3D ( 'NONE', #117690, #233805, #134662 ) ;
#247528 = EDGE_CURVE ( 'NONE', #11869, #5875, #142127, .T. ) ;
#247529 = CARTESIAN_POINT ( 'NONE',  ( 20.85000000000000142, 77.83585931145498193, -24.51866831572578320 ) ) ;
#247530 = EDGE_LOOP ( 'NONE', ( #102798, #43302, #205853, #124938 ) ) ;
#247531 = DIRECTION ( 'NONE',  ( 0.000000000000000000, 1.000000000000000000, 0.000000000000000000 ) ) ;
#247532 = EDGE_CURVE ( 'NONE', #158708, #57292, #21527, .T. ) ;
#247533 = CARTESIAN_POINT ( 'NONE',  ( 20.09999999999999787, 60.24242455067834356, -224.3755369822736156 ) ) ;
#247534 = CARTESIAN_POINT ( 'NONE',  ( -16.91256925476571027, 9.985731158139330432, -46.03235751099472850 ) ) ;
#247535 = CARTESIAN_POINT ( 'NONE',  ( 20.22516295850462598, 66.10063570456208026, -162.1130417724336041 ) ) ;
#247536 = EDGE_CURVE ( 'NONE', #205763, #234522, #100584, .T. ) ;
#247537 = ORIENTED_EDGE ( 'NONE', *, *, #214298, .F. ) ;
#247538 = CARTESIAN_POINT ( 'NONE',  ( -23.25000000000000000, -11.75000000000000000, 3.469446951953614189E-15 ) ) ;
#247540 = EDGE_CURVE ( 'NONE', #42010, #82203, #46772, .T. ) ;
#247539 =( NAMED_UNIT ( * ) SI_UNIT ( $, .STERADIAN. ) SOLID_ANGLE_UNIT ( ) );
#247541 = DIRECTION ( 'NONE',  ( -0.000000000000000000, 6.982962677686266711E-15, -1.000000000000000000 ) ) ;
#247542 = CIRCLE ( 'NONE', #168480, 0.09999999999998898659 ) ;
#247543 = CARTESIAN_POINT ( 'NONE',  ( -18.59999999999999787, 11.64999999999999680, -7.014805770654001016 ) ) ;
#247544 = ORIENTED_EDGE ( 'NONE', *, *, #225427, .F. ) ;
#247545 = ORIENTED_EDGE ( 'NONE', *, *, #2289, .T. ) ;
#247546 = DIRECTION ( 'NONE',  ( 1.000000000000000000, 0.000000000000000000, 0.000000000000000000 ) ) ;
#247547 = CYLINDRICAL_SURFACE ( 'NONE', #156860, 4.049999999999998046 ) ;
#247548 = DIRECTION ( 'NONE',  ( 0.000000000000000000, 0.000000000000000000, -1.000000000000000000 ) ) ;
#247549 = CARTESIAN_POINT ( 'NONE',  ( -18.46902351632712680, -9.509470118669714367, -107.4864539342573408 ) ) ;
#247550 = CIRCLE ( 'NONE', #135087, 0.09999999999999939493 ) ;
#247551 = CARTESIAN_POINT ( 'NONE',  ( 21.05000000000000071, 20.42498087366621817, -235.1829032864613396 ) ) ;
#247552 = EDGE_CURVE ( 'NONE', #116714, #3257, #144585, .T. ) ;
#247553 = VERTEX_POINT ( 'NONE', #244983 ) ;
#247554 = CARTESIAN_POINT ( 'NONE',  ( -23.15000000000000213, 8.882751598337867094, -187.0399955572217721 ) ) ;
#247555 = CONTEXT_DEPENDENT_SHAPE_REPRESENTATION ( #27664, #64332 ) ;
#247556 = DIRECTION ( 'NONE',  ( 0.000000000000000000, -0.2128009952263604232, 0.9770955615653316162 ) ) ;
#247557 = EDGE_LOOP ( 'NONE', ( #156771, #243874, #151799 ) ) ;
#247558 = FACE_OUTER_BOUND ( 'NONE', #216541, .T. ) ;
#247559 = EDGE_LOOP ( 'NONE', ( #240810, #107442, #171292, #26134 ) ) ;
#247560 = ORIENTED_EDGE ( 'NONE', *, *, #25261, .F. ) ;
#247561 = ORIENTED_EDGE ( 'NONE', *, *, #196323, .F. ) ;
#247562 = CARTESIAN_POINT ( 'NONE',  ( -18.59999999999999787, 65.66751761918619934, -30.42826094061123854 ) ) ;
#247563 = DIRECTION ( 'NONE',  ( 2.710505431213777848E-16, 0.4088369013363281623, -0.9126074666063771490 ) ) ;
#247564 = CARTESIAN_POINT ( 'NONE',  ( 21.09793522318394920, 10.72462451022393282, -112.7392908709769586 ) ) ;
#247565 = CARTESIAN_POINT ( 'NONE',  ( -20.64999999999999858, 29.14863708059993286, -237.4168895852561434 ) ) ;
#247566 = DIRECTION ( 'NONE',  ( 1.000000000000000000, 0.000000000000000000, 0.000000000000000000 ) ) ;
#247567 = DIRECTION ( 'NONE',  ( -1.000000000000000000, 0.000000000000000000, 0.000000000000000000 ) ) ;
#247568 = DIRECTION ( 'NONE',  ( 1.000000000000000000, 0.000000000000000000, 0.000000000000000000 ) ) ;
#247570 = PLANE ( 'NONE',  #99555 ) ;
#247569 = DIRECTION ( 'NONE',  ( 0.000000000000000000, 6.982962677686266711E-15, -1.000000000000000000 ) ) ;
#247571 = EDGE_CURVE ( 'NONE', #191888, #12967, #138007, .T. ) ;
#247572 = CARTESIAN_POINT ( 'NONE',  ( 20.73486653747088582, 7.250000000011182166, -143.2500000000000284 ) ) ;
#247573 = CARTESIAN_POINT ( 'NONE',  ( -16.87487986503753845, 9.950007555096753720, -113.1499747396867690 ) ) ;
#247574 = CARTESIAN_POINT ( 'NONE',  ( 22.48508240969612615, 0.04627641452807085970, -155.8499892684264125 ) ) ;
#247576 = DIRECTION ( 'NONE',  ( 0.000000000000000000, 6.982962677686266711E-15, -1.000000000000000000 ) ) ;
#247575 = AXIS2_PLACEMENT_3D ( 'NONE', #214973, #36369, #195442 ) ;
#247577 = ORIENTED_EDGE ( 'NONE', *, *, #185110, .T. ) ;
#247578 = ADVANCED_FACE ( 'NONE', ( #186310 ), #96162, .T. ) ;
#247579 = CIRCLE ( 'NONE', #56015, 0.09999999999999791001 ) ;
#247580 = ORIENTED_EDGE ( 'NONE', *, *, #25622, .T. ) ;
#247581 = CARTESIAN_POINT ( 'NONE',  ( -18.50000000000000000, -9.400000000000005684, -40.38204184817266906 ) ) ;
#247582 = LINE ( 'NONE', #68968, #141152 ) ;
#247585 = DIRECTION ( 'NONE',  ( -0.7071067811865463515, -0.7071067811865487940, 7.587431340288849180E-16 ) ) ;
#247584 = DIRECTION ( 'NONE',  ( 1.000000000000000000, 0.000000000000000000, 0.000000000000000000 ) ) ;
#247583 = AXIS2_PLACEMENT_3D ( 'NONE', #56962, #116972, #180803 ) ;
#247586 = CARTESIAN_POINT ( 'NONE',  ( 20.95496329884391784, 39.25093957328100913, -236.8105868520244996 ) ) ;
#247587 = DIRECTION ( 'NONE',  ( 0.000000000000000000, 0.000000000000000000, 1.000000000000000000 ) ) ;
#247588 = DIRECTION ( 'NONE',  ( -3.265361837132813093E-16, 1.000000000000000000, -0.000000000000000000 ) ) ;
#247589 = ORIENTED_EDGE ( 'NONE', *, *, #159184, .T. ) ;
#247590 = EDGE_LOOP ( 'NONE', ( #154205, #242530, #59804, #53737, #217746, #185847, #69266, #150759, #86082, #206623 ) ) ;
#247592 = VECTOR ( 'NONE', #248944, 1000.000000000000000 ) ;
#247591 = CARTESIAN_POINT ( 'NONE',  ( -23.25000000000000000, 74.00000000001156764, -56.29848556176223440 ) ) ;
#247593 = ORIENTED_EDGE ( 'NONE', *, *, #67323, .T. ) ;
#247594 = ADVANCED_FACE ( 'NONE', ( #154903 ), #175745, .T. ) ;
#247595 = DIRECTION ( 'NONE',  ( -0.000000000000000000, 0.8127272543711119290, -0.5826443254700023333 ) ) ;
#247596 = AXIS2_PLACEMENT_3D ( 'NONE', #175627, #139007, #216001 ) ;
#247597 = DIRECTION ( 'NONE',  ( 1.000000000000000000, 0.000000000000000000, 0.000000000000000000 ) ) ;
#247598 = AXIS2_PLACEMENT_3D ( 'NONE', #117520, #36733, #176233 ) ;
#247599 = CIRCLE ( 'NONE', #197696, 0.1000000000000057648 ) ;
#247600 = VERTEX_POINT ( 'NONE', #33693 ) ;
#247601 = CARTESIAN_POINT ( 'NONE',  ( 18.59999999999999076, 64.35000000001197407, -111.6731074845243796 ) ) ;
#247602 = ORIENTED_EDGE ( 'NONE', *, *, #203286, .T. ) ;
#247603 = CARTESIAN_POINT ( 'NONE',  ( -20.65000000000000568, 7.488999128699433072, -208.8358083214519070 ) ) ;
#247604 = CARTESIAN_POINT ( 'NONE',  ( 23.24999999999999645, 1.115600667400684642E-11, -200.9999999999999432 ) ) ;
#247606 = AXIS2_PLACEMENT_3D ( 'NONE', #147874, #248247, #210420 ) ;
#247605 = CARTESIAN_POINT ( 'NONE',  ( -18.37160782347004329, 64.52438358520920758, -60.27310748452440947 ) ) ;
#247607 = AXIS2_PLACEMENT_3D ( 'NONE', #108618, #106020, #214143 ) ;
#247609 = CARTESIAN_POINT ( 'NONE',  ( -18.59999999999999787, 7.120270961708750512, -137.6595630418393625 ) ) ;
#247608 = AXIS2_PLACEMENT_3D ( 'NONE', #115793, #256519, #160074 ) ;
#247610 = LINE ( 'NONE', #111968, #47351 ) ;
#247611 = CARTESIAN_POINT ( 'NONE',  ( -21.93340585899104056, 1.115541036281197940E-11, -59.67585297787638865 ) ) ;
#247612 = CARTESIAN_POINT ( 'NONE',  ( -16.87331047859651179, 9.950000000011142376, -79.65000000000004832 ) ) ;
#247613 = CARTESIAN_POINT ( 'NONE',  ( -18.50000000000000000, 66.65000000001187175, -90.67310748452437963 ) ) ;
#247615 = ORIENTED_EDGE ( 'NONE', *, *, #25510, .F. ) ;
#247614 = CARTESIAN_POINT ( 'NONE',  ( 18.43630871534865179, -0.9118679986080973077, -242.3006466030380750 ) ) ;
#247617 = CARTESIAN_POINT ( 'NONE',  ( -18.59999999999999787, 11.65000000001115232, -146.1500000000000341 ) ) ;
#247616 = CARTESIAN_POINT ( 'NONE',  ( -18.39999999999999858, 85.51932773110506503, -196.5501311079649724 ) ) ;
#247618 = CIRCLE ( 'NONE', #163850, 12.87500000000000000 ) ;
#247619 = EDGE_LOOP ( 'NONE', ( #255420, #166572 ) ) ;
#247620 = ORIENTED_EDGE ( 'NONE', *, *, #17173, .F. ) ;
#247621 = EDGE_LOOP ( 'NONE', ( #54730, #93100 ) ) ;
#247622 = CYLINDRICAL_SURFACE ( 'NONE', #236484, 0.09999999999999939493 ) ;
#247623 = DIRECTION ( 'NONE',  ( 1.000000000000000000, 0.000000000000000000, 0.000000000000000000 ) ) ;
#247624 = AXIS2_PLACEMENT_3D ( 'NONE', #220104, #238369, #160155 ) ;
#247625 = CARTESIAN_POINT ( 'NONE',  ( 22.47809213839789066, 75.96246293238321812, -81.17308081931213337 ) ) ;
#247626 = CARTESIAN_POINT ( 'NONE',  ( 20.94999999999999574, -1.249999999988843369, -108.5000000000000426 ) ) ;
#247627 = CARTESIAN_POINT ( 'NONE',  ( -20.54999999999999716, 85.40000000001148805, -45.91707660717669626 ) ) ;
#247628 = TOROIDAL_SURFACE ( 'NONE', #26902, 12.77499999999999858, 0.1000000000000000056 ) ;
#247629 = CARTESIAN_POINT ( 'NONE',  ( -22.94999999999999929, 11.49641995933507843, -1.885425182446134107 ) ) ;
#247630 = CIRCLE ( 'NONE', #81015, 0.1000000000000028644 ) ;
#247632 = EDGE_CURVE ( 'NONE', #185697, #94619, #31117, .T. ) ;
#247631 = CARTESIAN_POINT ( 'NONE',  ( -23.15000000000000213, 62.92003201576280702, -207.2439188921395612 ) ) ;
#247633 = FACE_OUTER_BOUND ( 'NONE', #100453, .T. ) ;
#247634 = EDGE_CURVE ( 'NONE', #224326, #175634, #121328, .T. ) ;
#247635 = DIRECTION ( 'NONE',  ( 0.000000000000000000, 0.9908441862701782288, -0.1350103645450542456 ) ) ;
#247636 = EDGE_LOOP ( 'NONE', ( #76295, #81216, #239379, #13035, #110107, #227546, #233557, #210471, #242877, #98669, #256601, #161967 ) ) ;
#247637 = ORIENTED_EDGE ( 'NONE', *, *, #100259, .T. ) ;
#247638 = DIRECTION ( 'NONE',  ( 1.000000000000000000, -0.000000000000000000, -0.000000000000000000 ) ) ;
#247639 = ORIENTED_EDGE ( 'NONE', *, *, #148349, .T. ) ;
#247640 = DIRECTION ( 'NONE',  ( -1.000000000000000000, 0.000000000000000000, 0.000000000000000000 ) ) ;
#247641 = ORIENTED_EDGE ( 'NONE', *, *, #106778, .F. ) ;
#247642 = CARTESIAN_POINT ( 'NONE',  ( 22.39999999999999858, 68.20922040163900135, -170.1231074845244109 ) ) ;
#247643 = EDGE_CURVE ( 'NONE', #153695, #182906, #204656, .T. ) ;
#247644 = FACE_OUTER_BOUND ( 'NONE', #64063, .T. ) ;
#247645 = CARTESIAN_POINT ( 'NONE',  ( -22.42253884134832020, -2.477159594661237474, -189.6168107728914549 ) ) ;
#247646 = EDGE_CURVE ( 'NONE', #59214, #125644, #131457, .T. ) ;
#247647 = DIRECTION ( 'NONE',  ( 2.342056488767301376E-15, 0.1350103645451835865, 0.9908441862701605762 ) ) ;
#247648 = ORIENTED_EDGE ( 'NONE', *, *, #165751, .T. ) ;
#247649 = EDGE_CURVE ( 'NONE', #24454, #130019, #163000, .T. ) ;
#247650 = CARTESIAN_POINT ( 'NONE',  ( 20.94999999999999929, 86.30329675166747450, -209.4258251677035787 ) ) ;
#247651 = CIRCLE ( 'NONE', #222679, 0.09999999999999939493 ) ;
#247652 = AXIS2_PLACEMENT_3D ( 'NONE', #227781, #103963, #49142 ) ;
#247653 = CARTESIAN_POINT ( 'NONE',  ( -20.64999999999999858, 73.50000000001156764, -56.29848556176223440 ) ) ;
#247654 = EDGE_CURVE ( 'NONE', #129211, #247920, #246372, .T. ) ;
#247655 = CARTESIAN_POINT ( 'NONE',  ( 18.46082813848014226, 85.48074965091900879, -62.43873738180850097 ) ) ;
#247656 = PLANE ( 'NONE',  #43468 ) ;
#247657 = VECTOR ( 'NONE', #106178, 1000.000000000000000 ) ;
#247658 = ORIENTED_EDGE ( 'NONE', *, *, #25375, .F. ) ;
#247660 = CARTESIAN_POINT ( 'NONE',  ( -20.64999999999999858, 1.115600667400684642E-11, -67.00000000000004263 ) ) ;
#247659 = LINE ( 'NONE', #10350, #33289 ) ;
#247661 = ORIENTED_EDGE ( 'NONE', *, *, #213629, .T. ) ;
#247664 = ORIENTED_EDGE ( 'NONE', *, *, #112688, .F. ) ;
#247663 = DIRECTION ( 'NONE',  ( -1.000000000000000000, -0.000000000000000000, 0.000000000000000000 ) ) ;
#247662 = CYLINDRICAL_SURFACE ( 'NONE', #111694, 0.4999999999999944489 ) ;
#247665 = ORIENTED_EDGE ( 'NONE', *, *, #130374, .T. ) ;
#247666 = CARTESIAN_POINT ( 'NONE',  ( -16.93388492042258520, 9.988541822527057690, -113.0994548768138657 ) ) ;
#247667 = LINE ( 'NONE', #149875, #86105 ) ;
#247668 = CARTESIAN_POINT ( 'NONE',  ( -18.39999999999999858, 85.50000000001186606, -96.42291809330220076 ) ) ;
#247669 = CIRCLE ( 'NONE', #231121, 0.09999999999999609201 ) ;
#247670 = ORIENTED_EDGE ( 'NONE', *, *, #187557, .T. ) ;
#247671 = CARTESIAN_POINT ( 'NONE',  ( -23.15000000000000213, 71.75000000001229239, -157.7731074845243882 ) ) ;
#247672 = EDGE_CURVE ( 'NONE', #112788, #187434, #67297, .T. ) ;
#247673 = LINE ( 'NONE', #250239, #177991 ) ;
#247675 = CARTESIAN_POINT ( 'NONE',  ( -23.25000000000000000, 1.115600667400684642E-11, -33.50000000000000000 ) ) ;
#247674 = FACE_OUTER_BOUND ( 'NONE', #209752, .T. ) ;
#247677 = ORIENTED_EDGE ( 'NONE', *, *, #130343, .T. ) ;
#247676 = CARTESIAN_POINT ( 'NONE',  ( 21.04386569057601619, 11.75000000001104006, -93.64283735177943413 ) ) ;
#247678 = AXIS2_PLACEMENT_3D ( 'NONE', #55307, #192299, #214410 ) ;
#247679 = VECTOR ( 'NONE', #168439, 1000.000000000000000 ) ;
#247680 = VECTOR ( 'NONE', #250976, 1000.000000000000227 ) ;
#247681 = ORIENTED_EDGE ( 'NONE', *, *, #219950, .T. ) ;
#247682 = CARTESIAN_POINT ( 'NONE',  ( 20.04142135391667168, 64.25000000001176659, -78.32060061889448832 ) ) ;
#247683 = DIRECTION ( 'NONE',  ( 0.000000000000000000, -0.9651348961777157509, 0.2617529984165031243 ) ) ;
#247684 = CARTESIAN_POINT ( 'NONE',  ( -18.50000000000000000, 77.16412189325360771, -162.1082593989527254 ) ) ;
#247685 = ORIENTED_EDGE ( 'NONE', *, *, #253646, .F. ) ;
#247686 = CARTESIAN_POINT ( 'NONE',  ( -16.85312964099708566, 9.913604682078865693, -188.1028157064303912 ) ) ;
#247687 = CARTESIAN_POINT ( 'NONE',  ( 18.49999999999999289, 6.650000000011155876, -188.6499999999999488 ) ) ;
#247688 = CARTESIAN_POINT ( 'NONE',  ( 18.49999999999999645, 71.84303044094815505, -225.1053209871248271 ) ) ;
#247689 = CIRCLE ( 'NONE', #64344, 0.1000000000000028644 ) ;
#247690 = ORIENTED_EDGE ( 'NONE', *, *, #135616, .T. ) ;
#247691 = CARTESIAN_POINT ( 'NONE',  ( -18.59999999999999787, 68.50594083727658301, -224.0235912779512830 ) ) ;
#247692 = CIRCLE ( 'NONE', #47192, 0.09999999999999939493 ) ;
#247693 = VERTEX_POINT ( 'NONE', #235681 ) ;
#247694 = LINE ( 'NONE', #187743, #76532 ) ;
#247695 = FACE_OUTER_BOUND ( 'NONE', #97237, .T. ) ;
#247696 = TOROIDAL_SURFACE ( 'NONE', #55955, 2.100000000000002309, 0.1000000000000000056 ) ;
#247697 = AXIS2_PLACEMENT_3D ( 'NONE', #107902, #147018, #192584 ) ;
#247698 = EDGE_CURVE ( 'NONE', #59420, #84927, #88112, .T. ) ;
#247699 = ORIENTED_EDGE ( 'NONE', *, *, #95387, .F. ) ;
#247700 = AXIS2_PLACEMENT_3D ( 'NONE', #142383, #125403, #160706 ) ;
#247701 = EDGE_LOOP ( 'NONE', ( #170154, #152150, #242303, #216560 ) ) ;
#247702 = LINE ( 'NONE', #7822, #141492 ) ;
#247703 = ORIENTED_EDGE ( 'NONE', *, *, #187274, .T. ) ;
#247705 = ORIENTED_EDGE ( 'NONE', *, *, #6719, .T. ) ;
#247704 = CARTESIAN_POINT ( 'NONE',  ( -23.15000000000000213, 11.48087284840413425, -198.4995883060917663 ) ) ;
#247706 = EDGE_CURVE ( 'NONE', #78372, #123921, #8862, .T. ) ;
#247707 = ORIENTED_EDGE ( 'NONE', *, *, #53352, .T. ) ;
#247709 = EDGE_LOOP ( 'NONE', ( #204600, #159840, #9619, #38831 ) ) ;
#247708 = ORIENTED_EDGE ( 'NONE', *, *, #126761, .T. ) ;
#247710 = EDGE_CURVE ( 'NONE', #171759, #190547, #71420, .T. ) ;
#247711 = ADVANCED_FACE ( 'NONE', ( #194023 ), #133930, .F. ) ;
#247712 = CARTESIAN_POINT ( 'NONE',  ( -18.33981767444014821, -9.569575789793876908, -107.3191618437250696 ) ) ;
#247713 = VERTEX_POINT ( 'NONE', #115745 ) ;
#247714 = CARTESIAN_POINT ( 'NONE',  ( 20.95512820512820795, 22.07448326904560076, -231.6692507597321935 ) ) ;
#247715 = CARTESIAN_POINT ( 'NONE',  ( 21.05000000000000071, 87.75000000001162448, -66.62310748452424036 ) ) ;
#247716 = AXIS2_PLACEMENT_3D ( 'NONE', #238133, #236856, #97314 ) ;
#247717 = DIRECTION ( 'NONE',  ( 1.000000000000000000, -0.000000000000000000, 0.000000000000000000 ) ) ;
#247718 = CARTESIAN_POINT ( 'NONE',  ( -18.37151313414731746, 87.02160168029750764, -199.4493498806463094 ) ) ;
#247719 = ORIENTED_EDGE ( 'NONE', *, *, #74677, .T. ) ;
#247720 = ORIENTED_EDGE ( 'NONE', *, *, #148616, .F. ) ;
#247721 = DIRECTION ( 'NONE',  ( 1.000000000000000000, 3.816239940179503281E-14, -1.218904804407150903E-14 ) ) ;
#247723 = ORIENTED_EDGE ( 'NONE', *, *, #145265, .F. ) ;
#247722 = CARTESIAN_POINT ( 'NONE',  ( 18.59999999999999432, 63.58402440245808407, -209.2218768284338921 ) ) ;
#247724 = DIRECTION ( 'NONE',  ( 1.000000000000000000, 0.000000000000000000, 0.000000000000000000 ) ) ;
#247726 = EDGE_LOOP ( 'NONE', ( #120283, #158083, #47058, #97063 ) ) ;
#247725 = DIRECTION ( 'NONE',  ( -3.265361837132813093E-16, -1.000000000000000000, -6.938893903907229955E-15 ) ) ;
#247727 = EDGE_CURVE ( 'NONE', #210119, #58804, #233888, .T. ) ;
#247728 = ORIENTED_EDGE ( 'NONE', *, *, #128319, .F. ) ;
#247729 = DIRECTION ( 'NONE',  ( 1.000000000000000000, -0.000000000000000000, -0.000000000000000000 ) ) ;
#247730 = EDGE_CURVE ( 'NONE', #137060, #238125, #72801, .T. ) ;
#247732 = ORIENTED_EDGE ( 'NONE', *, *, #195068, .T. ) ;
#247731 = PRODUCT_RELATED_PRODUCT_CATEGORY ( 'part', '', ( #7676 ) ) ;
#247733 = LINE ( 'NONE', #152522, #48652 ) ;
#247736 = VERTEX_POINT ( 'NONE', #53204 ) ;
#247735 = ORIENTED_EDGE ( 'NONE', *, *, #44029, .F. ) ;
#247734 = VECTOR ( 'NONE', #55560, 1000.000000000000000 ) ;
#247737 = AXIS2_PLACEMENT_3D ( 'NONE', #241556, #242834, #26372 ) ;
#247738 = ORIENTED_EDGE ( 'NONE', *, *, #191058, .F. ) ;
#247739 = DIRECTION ( 'NONE',  ( -0.000000000000000000, -6.982962677686266711E-15, 1.000000000000000000 ) ) ;
#247740 = ORIENTED_EDGE ( 'NONE', *, *, #85426, .T. ) ;
#247741 = EDGE_LOOP ( 'NONE', ( #163362, #255258, #100588 ) ) ;
#247742 = ADVANCED_FACE ( 'NONE', ( #132764 ), #212296, .F. ) ;
#247743 = DIRECTION ( 'NONE',  ( 0.000000000000000000, 0.000000000000000000, -1.000000000000000000 ) ) ;
#247745 = ORIENTED_EDGE ( 'NONE', *, *, #222644, .T. ) ;
#247744 = DIRECTION ( 'NONE',  ( -1.000000000000000000, -0.000000000000000000, 0.000000000000000000 ) ) ;
#247746 = ADVANCED_FACE ( 'NONE', ( #253954 ), #36236, .T. ) ;
#247747 = FACE_OUTER_BOUND ( 'NONE', #220544, .T. ) ;
#247748 = EDGE_CURVE ( 'NONE', #174802, #76073, #139120, .T. ) ;
#247750 = CARTESIAN_POINT ( 'NONE',  ( -20.94999999999999929, 87.65000000001246860, -173.1231074845242688 ) ) ;
#247749 = FACE_OUTER_BOUND ( 'NONE', #215978, .T. ) ;
#247751 = CARTESIAN_POINT ( 'NONE',  ( 18.49999999999999645, 85.32100840337396619, -196.2871692354464415 ) ) ;
#247752 = DIRECTION ( 'NONE',  ( 0.000000000000000000, 0.9623856809447771665, 0.2716869542551821892 ) ) ;
#247753 = ORIENTED_EDGE ( 'NONE', *, *, #100477, .T. ) ;
#247754 = ORIENTED_EDGE ( 'NONE', *, *, #137237, .F. ) ;
#247755 = DIRECTION ( 'NONE',  ( -1.836970198721029934E-16, 1.000000000000000000, 0.000000000000000000 ) ) ;
#247756 = CARTESIAN_POINT ( 'NONE',  ( -18.36973785203555920, 64.52449679952728445, -45.27310748452440947 ) ) ;
#247757 = VECTOR ( 'NONE', #215928, 1000.000000000000000 ) ;
#247758 = EDGE_LOOP ( 'NONE', ( #111251, #177509, #232242, #221630, #84585 ) ) ;
#247759 = AXIS2_PLACEMENT_3D ( 'NONE', #226783, #48146, #233234 ) ;
#247760 = AXIS2_PLACEMENT_3D ( 'NONE', #65980, #163809, #127242 ) ;
#247761 = CIRCLE ( 'NONE', #122880, 0.09999999999998898659 ) ;
#247762 = CARTESIAN_POINT ( 'NONE',  ( -20.85000000000000142, 36.65892442174935439, -249.5511627012433848 ) ) ;
#247763 = ORIENTED_EDGE ( 'NONE', *, *, #105086, .F. ) ;
#247764 = ORIENTED_EDGE ( 'NONE', *, *, #89681, .T. ) ;
#247765 = CARTESIAN_POINT ( 'NONE',  ( 21.05000000000000071, -9.399999999988844834, -157.6060308773475640 ) ) ;
#247766 = CARTESIAN_POINT ( 'NONE',  ( -20.54999999999999716, 84.66355140188093742, -79.04720860259155302 ) ) ;
#247767 = ORIENTED_EDGE ( 'NONE', *, *, #119904, .T. ) ;
#247768 = CARTESIAN_POINT ( 'NONE',  ( -21.05000000000000071, 11.65000000001115588, -107.2838656629781724 ) ) ;
#247769 = LINE ( 'NONE', #75254, #206027 ) ;
#247770 = VERTEX_POINT ( 'NONE', #199133 ) ;
#247771 = CARTESIAN_POINT ( 'NONE',  ( 18.46163235739460262, -9.480150806907179373, -140.6576105398774814 ) ) ;
#247772 = DIRECTION ( 'NONE',  ( 0.000000000000000000, 0.4721928772777346239, 0.8814952561688430555 ) ) ;
#247774 = CARTESIAN_POINT ( 'NONE',  ( -18.59999999999999787, 64.35000000001264198, -196.5083017138704236 ) ) ;
#247773 = DIRECTION ( 'NONE',  ( 1.000000000000000000, -0.000000000000000000, -0.000000000000000000 ) ) ;
#247775 = CARTESIAN_POINT ( 'NONE',  ( 19.80993210785486269, 11.75000000000926548, -91.76711774888731554 ) ) ;
#247776 = CARTESIAN_POINT ( 'NONE',  ( 20.93284271247462414, 64.25000000001146816, -43.03791325517833855 ) ) ;
#247777 = FACE_OUTER_BOUND ( 'NONE', #185957, .T. ) ;
#247778 = EDGE_CURVE ( 'NONE', #218857, #148346, #182145, .T. ) ;
#247779 = PLANE ( 'NONE',  #182631 ) ;
#247780 = VERTEX_POINT ( 'NONE', #119615 ) ;
#247781 = CIRCLE ( 'NONE', #135332, 0.1000000000000028644 ) ;
#247782 = AXIS2_PLACEMENT_3D ( 'NONE', #64926, #223998, #45370 ) ;
#247784 = ORIENTED_EDGE ( 'NONE', *, *, #247201, .F. ) ;
#247783 = ORIENTED_EDGE ( 'NONE', *, *, #132208, .T. ) ;
#247785 = EDGE_LOOP ( 'NONE', ( #25273, #227633, #159206, #49504 ) ) ;
#247786 = AXIS2_PLACEMENT_3D ( 'NONE', #6079, #243416, #64776 ) ;
#247787 = ADVANCED_FACE ( 'NONE', ( #137855 ), #117032, .T. ) ;
#247788 = DIRECTION ( 'NONE',  ( 1.000000000000000000, 0.000000000000000000, 0.000000000000000000 ) ) ;
#247789 = CARTESIAN_POINT ( 'NONE',  ( 18.59999999999999432, 70.56573376625485139, -228.3808404818380779 ) ) ;
#247790 = DIRECTION ( 'NONE',  ( -1.000000000000000000, -2.952720810173289112E-16, 0.000000000000000000 ) ) ;
#247791 = FACE_OUTER_BOUND ( 'NONE', #14532, .T. ) ;
#247792 = ORIENTED_EDGE ( 'NONE', *, *, #68489, .T. ) ;
#247793 = ADVANCED_FACE ( 'NONE', ( #240831 ), #117186, .T. ) ;
#247794 = CARTESIAN_POINT ( 'NONE',  ( -22.49544290803751423, 11.74987023786864171, -100.4346880407423015 ) ) ;
#247795 = AXIS2_PLACEMENT_3D ( 'NONE', #197273, #169074, #116465 ) ;
#247796 = CIRCLE ( 'NONE', #6365, 0.09999999999999939493 ) ;
#247797 = ORIENTED_EDGE ( 'NONE', *, *, #30030, .T. ) ;
#247798 = FACE_OUTER_BOUND ( 'NONE', #6825, .T. ) ;
#247799 = DIRECTION ( 'NONE',  ( 0.000000000000000000, 0.000000000000000000, 1.000000000000000000 ) ) ;
#247800 = EDGE_CURVE ( 'NONE', #9861, #189304, #200565, .T. ) ;
#247801 = CARTESIAN_POINT ( 'NONE',  ( 18.39999999999999858, 85.60000000001166143, -62.92291809330219365 ) ) ;
#247802 = ORIENTED_EDGE ( 'NONE', *, *, #238774, .F. ) ;
#247803 = CYLINDRICAL_SURFACE ( 'NONE', #47349, 0.09999999999999939493 ) ;
#247804 = EDGE_CURVE ( 'NONE', #183191, #116722, #171391, .T. ) ;
#247805 = AXIS2_PLACEMENT_3D ( 'NONE', #169145, #232958, #150826 ) ;
#247806 = DIRECTION ( 'NONE',  ( 2.715809747126116015E-16, 0.9651348961777156399, -0.2617529984165029577 ) ) ;
#247807 = ADVANCED_FACE ( 'NONE', ( #219973 ), #197838, .F. ) ;
#247808 = ORIENTED_EDGE ( 'NONE', *, *, #221565, .T. ) ;
#247809 = ORIENTED_EDGE ( 'NONE', *, *, #27846, .T. ) ;
#247810 = DIRECTION ( 'NONE',  ( 0.000000000000000000, 0.8814952561688430555, -0.4721928772777346239 ) ) ;
#247811 = CIRCLE ( 'NONE', #89569, 0.1000000000000106498 ) ;
#247812 = CARTESIAN_POINT ( 'NONE',  ( 21.05000000000000071, 69.45934304831089889, -136.4231074845243654 ) ) ;
#247813 = DIRECTION ( 'NONE',  ( -1.000000000000000000, -2.952720810173289112E-16, 0.000000000000000000 ) ) ;
#247814 = DIRECTION ( 'NONE',  ( -0.000000000000000000, 0.000000000000000000, 1.000000000000000000 ) ) ;
#247815 = DIRECTION ( 'NONE',  ( 0.000000000000000000, 0.000000000000000000, -1.000000000000000000 ) ) ;
#247816 = CIRCLE ( 'NONE', #202024, 0.09999999999998898659 ) ;
#247817 = DIRECTION ( 'NONE',  ( 0.000000000000000000, 0.000000000000000000, -1.000000000000000000 ) ) ;
#247819 = EDGE_LOOP ( 'NONE', ( #105817, #203775, #51291, #3289 ) ) ;
#247818 = TOROIDAL_SURFACE ( 'NONE', #56255, 0.2000000000000000111, 0.1000000000000000056 ) ;
#247820 = CARTESIAN_POINT ( 'NONE',  ( -16.87331047859651179, 9.950000000011142376, -146.6500000000000341 ) ) ;
#247821 = DIRECTION ( 'NONE',  ( -0.000000000000000000, -0.8660254037844411501, -0.4999999999999956701 ) ) ;
#247823 = CARTESIAN_POINT ( 'NONE',  ( -21.14999999999999858, 11.75000000001115197, -174.2838656629781156 ) ) ;
#247822 = CARTESIAN_POINT ( 'NONE',  ( -16.93353400591625757, 10.00461239618409515, -87.93268447020545864 ) ) ;
#247824 = CARTESIAN_POINT ( 'NONE',  ( 21.14999999999999858, 1.115600667400684642E-11, -26.95934304829875927 ) ) ;
#247825 = DIRECTION ( 'NONE',  ( 0.000000000000000000, 0.000000000000000000, -1.000000000000000000 ) ) ;
#247826 = CARTESIAN_POINT ( 'NONE',  ( -21.14999999999999858, 31.98723526783714988, -238.8784020251475511 ) ) ;
#247827 = DIRECTION ( 'NONE',  ( 0.000000000000000000, 0.000000000000000000, -1.000000000000000000 ) ) ;
#247829 = ORIENTED_EDGE ( 'NONE', *, *, #138319, .F. ) ;
#247828 = CARTESIAN_POINT ( 'NONE',  ( -20.54999999999999716, 2.000000000011154189, -147.2246219227621111 ) ) ;
#247830 = EDGE_CURVE ( 'NONE', #210147, #213808, #221220, .T. ) ;
#247831 = EDGE_CURVE ( 'NONE', #6886, #162124, #254528, .T. ) ;
#247832 = ADVANCED_FACE ( 'NONE', ( #82995 ), #17916, .F. ) ;
#247834 = AXIS2_PLACEMENT_3D ( 'NONE', #243449, #64810, #127362 ) ;
#247833 = CARTESIAN_POINT ( 'NONE',  ( 21.05000000000000071, 87.39257802171783851, -139.5970570643562212 ) ) ;
#247835 = EDGE_CURVE ( 'NONE', #27072, #80211, #217113, .T. ) ;
#247836 = CIRCLE ( 'NONE', #52187, 0.09999999999999950595 ) ;
#247837 = DIRECTION ( 'NONE',  ( 0.000000000000000000, 0.9126074666063777041, 0.4088369013363265525 ) ) ;
#247838 = AXIS2_PLACEMENT_3D ( 'NONE', #103951, #203071, #162679 ) ;
#247839 = EDGE_CURVE ( 'NONE', #204044, #131489, #46441, .T. ) ;
#247840 = CARTESIAN_POINT ( 'NONE',  ( 18.39999999999999858, 85.60000000001190301, -95.99103808782457747 ) ) ;
#247841 = ORIENTED_EDGE ( 'NONE', *, *, #122137, .F. ) ;
#247842 = DIRECTION ( 'NONE',  ( -0.000000000000000000, 0.03181660087582099256, -0.9994937237965573207 ) ) ;
#247843 = CARTESIAN_POINT ( 'NONE',  ( -21.44999999999999929, 7.350000000011155166, -88.15000000000004832 ) ) ;
#247844 = FACE_OUTER_BOUND ( 'NONE', #234009, .T. ) ;
#247845 = EDGE_CURVE ( 'NONE', #49226, #243331, #104671, .T. ) ;
#247846 = AXIS2_PLACEMENT_3D ( 'NONE', #239819, #98973, #258035 ) ;
#247847 = ORIENTED_EDGE ( 'NONE', *, *, #226224, .T. ) ;
#247848 = CARTESIAN_POINT ( 'NONE',  ( -16.95709691156365650, 66.05000000001160743, -56.86304992201380060 ) ) ;
#247850 = EDGE_LOOP ( 'NONE', ( #59005, #73991, #247862, #119008 ) ) ;
#247849 = CYLINDRICAL_SURFACE ( 'NONE', #38492, 0.09999999999999031886 ) ;
#247851 = CARTESIAN_POINT ( 'NONE',  ( -21.64999999999999858, 21.48591740176965814, -233.0852932139783036 ) ) ;
#247852 = CARTESIAN_POINT ( 'NONE',  ( -18.69999999999999929, -1.467286812112899463, 32.89999999999999858 ) ) ;
#247853 = ORIENTED_EDGE ( 'NONE', *, *, #26813, .T. ) ;
#247854 = LINE ( 'NONE', #168367, #55357 ) ;
#247855 = EDGE_CURVE ( 'NONE', #1798, #35577, #113096, .T. ) ;
#247856 = VECTOR ( 'NONE', #213486, 1000.000000000000000 ) ;
#247857 = SHAPE_DEFINITION_REPRESENTATION ( #9789, #215063 ) ;
#247858 = CARTESIAN_POINT ( 'NONE',  ( -20.94788355080264353, 65.69792220476300315, -64.03355541284614105 ) ) ;
#247859 = CARTESIAN_POINT ( 'NONE',  ( 18.49999999999999645, -1.135018845899022466, -208.7169768834322952 ) ) ;
#247860 = CARTESIAN_POINT ( 'NONE',  ( 21.05000000000000071, 67.18454772081435067, -94.60271493191011416 ) ) ;
#247861 = CIRCLE ( 'NONE', #139513, 1.900000000000005906 ) ;
#247862 = ORIENTED_EDGE ( 'NONE', *, *, #48242, .F. ) ;
#247863 = CARTESIAN_POINT ( 'NONE',  ( 21.15000000000005187, 82.84256550613280012, -26.34830530078816935 ) ) ;
#247864 = DIRECTION ( 'NONE',  ( 0.000000000000000000, 0.000000000000000000, 1.000000000000000000 ) ) ;
#247865 = VECTOR ( 'NONE', #115820, 1000.000000000000114 ) ;
#247866 = FACE_OUTER_BOUND ( 'NONE', #55737, .T. ) ;
#247867 = VERTEX_POINT ( 'NONE', #179590 ) ;
#247868 = AXIS2_PLACEMENT_3D ( 'NONE', #196892, #15729, #234744 ) ;
#247869 = EDGE_LOOP ( 'NONE', ( #108913, #161058, #140685 ) ) ;
#247870 = DIRECTION ( 'NONE',  ( 1.000000000000000000, 0.000000000000000000, 0.000000000000000000 ) ) ;
#247871 = DIRECTION ( 'NONE',  ( 0.000000000000000000, 0.000000000000000000, 1.000000000000000000 ) ) ;
#247872 = DIRECTION ( 'NONE',  ( 1.000000000000000000, 0.000000000000000000, 0.000000000000000000 ) ) ;
#247873 = CARTESIAN_POINT ( 'NONE',  ( 21.05000000000000071, -12.41227409414968541, -30.50000000000000000 ) ) ;
#247874 = CARTESIAN_POINT ( 'NONE',  ( -20.64999999999999858, 62.08591502004791352, -248.5699171172615820 ) ) ;
#247876 = DIRECTION ( 'NONE',  ( 0.000000000000000000, 6.982962677686267499E-15, -1.000000000000000000 ) ) ;
#247875 = DIRECTION ( 'NONE',  ( 1.000000000000000000, 0.000000000000000000, 0.000000000000000000 ) ) ;
#247877 = CARTESIAN_POINT ( 'NONE',  ( 21.05000000000000071, 65.57661458509971908, -196.0310555606543517 ) ) ;
#247878 = CARTESIAN_POINT ( 'NONE',  ( -21.14999999999999858, -0.1008583690875562017, -21.75043287651061164 ) ) ;
#247879 = LINE ( 'NONE', #9271, #126459 ) ;
#247880 = CIRCLE ( 'NONE', #10569, 0.09999999999999939493 ) ;
#247881 = ADVANCED_FACE ( 'NONE', ( #102560 ), #256471, .T. ) ;
#247883 = ORIENTED_EDGE ( 'NONE', *, *, #28456, .T. ) ;
#247882 = CARTESIAN_POINT ( 'NONE',  ( -21.64999999999999858, 44.18585876254595490, -235.1667871698132046 ) ) ;
#247884 = AXIS2_PLACEMENT_3D ( 'NONE', #239266, #123171, #120620 ) ;
#247885 = DIRECTION ( 'NONE',  ( -0.000000000000000000, -1.000000000000000000, -0.000000000000000000 ) ) ;
#247886 = DIRECTION ( 'NONE',  ( 0.000000000000000000, 0.000000000000000000, 1.000000000000000000 ) ) ;
#247888 = CARTESIAN_POINT ( 'NONE',  ( 18.59999999999999787, 0.6656436123793491033, -212.6810495496487476 ) ) ;
#247887 = DIRECTION ( 'NONE',  ( 1.000000000000000000, 0.000000000000000000, 0.000000000000000000 ) ) ;
#247889 = ORIENTED_EDGE ( 'NONE', *, *, #188236, .F. ) ;
#247890 = CARTESIAN_POINT ( 'NONE',  ( 23.14999999999998437, -11.74999999998884448, -33.50000000000000000 ) ) ;
#247891 = CARTESIAN_POINT ( 'NONE',  ( 19.86930884467576419, 64.31308993304084254, -111.7838848455855327 ) ) ;
#247892 = FACE_OUTER_BOUND ( 'NONE', #256740, .T. ) ;
#247893 = CARTESIAN_POINT ( 'NONE',  ( -22.50000000000000000, 26.02743912001966464, -254.3139371321002216 ) ) ;
#247894 = DIRECTION ( 'NONE',  ( 0.000000000000000000, 1.000000000000000000, 6.982962677686267499E-15 ) ) ;
#247895 = ORIENTED_EDGE ( 'NONE', *, *, #17385, .F. ) ;
#247896 = EDGE_LOOP ( 'NONE', ( #124415, #28462, #84939, #159417 ) ) ;
#247897 = FACE_OUTER_BOUND ( 'NONE', #21228, .T. ) ;
#247898 = VERTEX_POINT ( 'NONE', #895 ) ;
#247899 = EDGE_CURVE ( 'NONE', #107353, #74147, #196468, .T. ) ;
#247900 = CARTESIAN_POINT ( 'NONE',  ( 21.05000000000000426, 65.27628289530437655, -95.42869009291126758 ) ) ;
#247901 = AXIS2_PLACEMENT_3D ( 'NONE', #233978, #214413, #236543 ) ;
#247902 = ORIENTED_EDGE ( 'NONE', *, *, #133410, .F. ) ;
#247903 = CARTESIAN_POINT ( 'NONE',  ( -23.15000000000000213, 76.00000000001244871, -170.0231074845243597 ) ) ;
#247904 = CARTESIAN_POINT ( 'NONE',  ( -18.79999999999999716, 1.311673547813416718, -7.986648289447971116 ) ) ;
#247905 = CARTESIAN_POINT ( 'NONE',  ( 22.39999999999999503, 0.1000000000111554016, -126.2092204016266379 ) ) ;
#247906 = ORIENTED_EDGE ( 'NONE', *, *, #22940, .F. ) ;
#247907 = FACE_OUTER_BOUND ( 'NONE', #159393, .T. ) ;
#247908 = CARTESIAN_POINT ( 'NONE',  ( -18.57399277249657032, 68.10911674539558192, -224.1414149070238864 ) ) ;
#247909 = DIRECTION ( 'NONE',  ( 0.000000000000000000, 1.000000000000000000, 6.982962677686266711E-15 ) ) ;
#247910 = DIRECTION ( 'NONE',  ( 0.000000000000000000, 0.000000000000000000, 1.000000000000000000 ) ) ;
#247911 = DIRECTION ( 'NONE',  ( 1.000000000000000000, 0.000000000000000000, 0.000000000000000000 ) ) ;
#247912 = LINE ( 'NONE', #186680, #190442 ) ;
#247913 = ORIENTED_EDGE ( 'NONE', *, *, #240463, .T. ) ;
#247915 = DIRECTION ( 'NONE',  ( 1.000000000000000000, 1.836970198721029934E-16, 0.000000000000000000 ) ) ;
#247914 = CARTESIAN_POINT ( 'NONE',  ( 23.14999999999999858, 68.22899648672319017, -213.7884437866858889 ) ) ;
#247916 = ORIENTED_EDGE ( 'NONE', *, *, #57309, .F. ) ;
#247918 = EDGE_LOOP ( 'NONE', ( #15253, #79822, #138342, #242918 ) ) ;
#247917 = FACE_OUTER_BOUND ( 'NONE', #134249, .T. ) ;
#247919 = AXIS2_PLACEMENT_3D ( 'NONE', #123283, #243212, #24195 ) ;
#247920 = VERTEX_POINT ( 'NONE', #163864 ) ;
#247921 = CIRCLE ( 'NONE', #181311, 7.899999999999990585 ) ;
#247922 = DIRECTION ( 'NONE',  ( -0.000000000000000000, -1.000000000000000000, -6.982962677686266711E-15 ) ) ;
#247923 = CARTESIAN_POINT ( 'NONE',  ( 13.22461703343584638, 66.56333706821315843, -151.7000707522295215 ) ) ;
#247924 = DIRECTION ( 'NONE',  ( -0.000000000000000000, 0.1480365673253065117, -0.9889818879709273425 ) ) ;
#247925 = CARTESIAN_POINT ( 'NONE',  ( 21.05000000000000071, 65.27628289530457550, -128.8581939154367717 ) ) ;
#247926 = ORIENTED_EDGE ( 'NONE', *, *, #24106, .T. ) ;
#247927 = CARTESIAN_POINT ( 'NONE',  ( -20.90000000000000213, 11.59510167572422112, -1.901609089591594470 ) ) ;
#247929 = EDGE_LOOP ( 'NONE', ( #152672, #80420, #105070, #72526, #74134, #128575, #63425, #60305, #22346, #239343, #34557, #61508, #145753, #35750, #1579, #242395, #42893, #33913 ) ) ;
#247928 = B_SPLINE_CURVE_WITH_KNOTS ( 'NONE', 3,
 ( #198828, #20208, #219669, #237949, #223515, #44903, #197538, #63160, #21501, #22795, #3180, #202679, #162294, #99701 ),
 .UNSPECIFIED., .F., .F.,
 ( 4, 2, 2, 2, 2, 2, 4 ),
 ( 1.398578778534940505E-17, 0.0003823333598417854922, 0.0005735000397626704863, 0.0006690833797231130918, 0.0007168750497033329850, 0.0007407708846934382696, 0.0007646667196835435542 ),
 .UNSPECIFIED. ) ;
#247930 = CARTESIAN_POINT ( 'NONE',  ( -21.05000000000000071, 1.162701749949165642, -175.5999999999999659 ) ) ;
#247931 = EDGE_CURVE ( 'NONE', #26411, #124703, #4751, .T. ) ;
#247933 = AXIS2_PLACEMENT_3D ( 'NONE', #125826, #170148, #147973 ) ;
#247932 = DIRECTION ( 'NONE',  ( -2.952720810173289112E-16, 1.000000000000000000, 0.000000000000000000 ) ) ;
#247934 = ORIENTED_EDGE ( 'NONE', *, *, #202472, .T. ) ;
#247936 = CARTESIAN_POINT ( 'NONE',  ( 20.85000000000000142, 1.115600667400684642E-11, -134.0000000000000284 ) ) ;
#247935 = AXIS2_PLACEMENT_3D ( 'NONE', #42706, #105199, #184775 ) ;
#247937 = CIRCLE ( 'NONE', #143880, 0.09999999999999642508 ) ;
#247938 = CIRCLE ( 'NONE', #252206, 0.09999999999999939493 ) ;
#247939 = ORIENTED_EDGE ( 'NONE', *, *, #87723, .T. ) ;
#247940 = CARTESIAN_POINT ( 'NONE',  ( 18.42555734704283665, -9.497158361925551517, -141.0398304977349824 ) ) ;
#247941 = ORIENTED_EDGE ( 'NONE', *, *, #129975, .T. ) ;
#247942 = DIRECTION ( 'NONE',  ( -1.000000000000000000, -1.541880601228652843E-16, -2.878400969107353907E-16 ) ) ;
#247943 =( GEOMETRIC_REPRESENTATION_CONTEXT ( 3 ) GLOBAL_UNCERTAINTY_ASSIGNED_CONTEXT ( ( #194073 ) ) GLOBAL_UNIT_ASSIGNED_CONTEXT ( ( #236890, #114379, #193931 ) ) REPRESENTATION_CONTEXT ( 'NONE', 'WORKASPACE' ) );
#247944 = EDGE_CURVE ( 'NONE', #243532, #212207, #6050, .T. ) ;
#247945 = CARTESIAN_POINT ( 'NONE',  ( 21.02374657821586013, 64.39999999919189122, -76.45131071432655290 ) ) ;
#247946 = DIRECTION ( 'NONE',  ( 0.000000000000000000, -1.000000000000000000, -6.982962677686265922E-15 ) ) ;
#247947 = EDGE_CURVE ( 'NONE', #77802, #94999, #184691, .T. ) ;
#247948 = LINE ( 'NONE', #45906, #162011 ) ;
#247949 = EDGE_CURVE ( 'NONE', #246745, #117026, #67318, .T. ) ;
#247950 = LINE ( 'NONE', #69341, #32172 ) ;
#247951 = CARTESIAN_POINT ( 'NONE',  ( -21.05000000000000426, 64.40000000001263913, -196.5949042542488883 ) ) ;
#247952 = ORIENTED_EDGE ( 'NONE', *, *, #255759, .F. ) ;
#247953 = CARTESIAN_POINT ( 'NONE',  ( -18.40000000000000213, 54.09347887257330711, -229.1540424707546322 ) ) ;
#247954 = AXIS2_PLACEMENT_3D ( 'NONE', #33821, #113307, #74223 ) ;
#247955 = ORIENTED_EDGE ( 'NONE', *, *, #183324, .T. ) ;
#247957 = DIRECTION ( 'NONE',  ( 0.000000000000000000, -2.775557561562888827E-14, 1.000000000000000000 ) ) ;
#247956 = DIRECTION ( 'NONE',  ( 0.000000000000000000, 0.000000000000000000, 1.000000000000000000 ) ) ;
#247958 = MECHANICAL_DESIGN_GEOMETRIC_PRESENTATION_REPRESENTATION (  '', ( #60681 ), #48230 ) ;
#247959 = ORIENTED_EDGE ( 'NONE', *, *, #25961, .F. ) ;
#247960 = AXIS2_PLACEMENT_3D ( 'NONE', #223899, #121001, #62278 ) ;
#247961 = FACE_OUTER_BOUND ( 'NONE', #31380, .T. ) ;
#247962 = DIRECTION ( 'NONE',  ( 0.000000000000000000, 0.6728388485993177515, -0.7397890806274072251 ) ) ;
#247963 = VERTEX_POINT ( 'NONE', #145564 ) ;
#247965 = ORIENTED_EDGE ( 'NONE', *, *, #156519, .T. ) ;
#247964 = DIRECTION ( 'NONE',  ( 3.265361837132813093E-16, 1.000000000000000000, 6.982962677686266711E-15 ) ) ;
#247966 = CIRCLE ( 'NONE', #81901, 0.5000000000000071054 ) ;
#247967 = ADVANCED_FACE ( 'NONE', ( #46457 ), #88288, .F. ) ;
#247968 = DIRECTION ( 'NONE',  ( 0.000000000000000000, -0.8430646840892555005, -0.5378121776619452232 ) ) ;
#247969 = CIRCLE ( 'NONE', #60690, 0.1000000000000000472 ) ;
#247971 = FACE_OUTER_BOUND ( 'NONE', #86109, .T. ) ;
#247970 = DIRECTION ( 'NONE',  ( 0.000000000000000000, -0.8814952561688476074, 0.4721928772777262417 ) ) ;
#247972 = AXIS2_PLACEMENT_3D ( 'NONE', #105850, #165870, #27663 ) ;
#247973 = AXIS2_PLACEMENT_3D ( 'NONE', #177546, #197050, #137095 ) ;
#247975 = VERTEX_POINT ( 'NONE', #187290 ) ;
#247974 = CARTESIAN_POINT ( 'NONE',  ( -20.94999999999999929, 5.850000000011108092, -77.13249722427801203 ) ) ;
#247976 = ORIENTED_EDGE ( 'NONE', *, *, #64538, .F. ) ;
#247977 = CARTESIAN_POINT ( 'NONE',  ( 20.90000000000000213, -1.885425182446133885, -11.49641995933507843 ) ) ;
#247978 = AXIS2_PLACEMENT_3D ( 'NONE', #5550, #205030, #121692 ) ;
#247979 = DIRECTION ( 'NONE',  ( -1.000000000000000000, -0.000000000000000000, -0.000000000000000000 ) ) ;
#247980 = EDGE_LOOP ( 'NONE', ( #255686, #101324, #68006, #128854 ) ) ;
#247981 = DIRECTION ( 'NONE',  ( 0.000000000000000000, 0.2128009952263605065, -0.9770955615653315052 ) ) ;
#247982 = ORIENTED_EDGE ( 'NONE', *, *, #210825, .T. ) ;
#247983 = CIRCLE ( 'NONE', #77292, 0.09999999999999716060 ) ;
#247984 = CARTESIAN_POINT ( 'NONE',  ( -20.85000000000000142, -1.249999999988843369, -175.3004807544151049 ) ) ;
#247985 = CYLINDRICAL_SURFACE ( 'NONE', #255716, 0.09999999999999939493 ) ;
#247986 = AXIS2_PLACEMENT_3D ( 'NONE', #183885, #1375, #80914 ) ;
#247988 = ORIENTED_EDGE ( 'NONE', *, *, #210966, .T. ) ;
#247987 = TOROIDAL_SURFACE ( 'NONE', #156265, 0.6000000000000009770, 0.1000000000000000056 ) ;
#247989 = CARTESIAN_POINT ( 'NONE',  ( -23.15000000000000213, 6.703231349641842307, -231.7785101893094577 ) ) ;
#247990 = EDGE_CURVE ( 'NONE', #77502, #184791, #142303, .T. ) ;
#247991 = ORIENTED_EDGE ( 'NONE', *, *, #232382, .F. ) ;
#247992 = CARTESIAN_POINT ( 'NONE',  ( 21.08078803292165659, 6.171108002023541594, -199.5749562617978370 ) ) ;
#247993 = ADVANCED_FACE ( 'NONE', ( #45186 ), #24367, .T. ) ;
#247994 = EDGE_LOOP ( 'NONE', ( #76500, #61074, #150819, #65436 ) ) ;
#247995 = ORIENTED_EDGE ( 'NONE', *, *, #174471, .T. ) ;
#247996 = FACE_OUTER_BOUND ( 'NONE', #251503, .T. ) ;
#247997 = ORIENTED_EDGE ( 'NONE', *, *, #252223, .F. ) ;
#247998 = DIRECTION ( 'NONE',  ( -1.000000000000000000, 0.000000000000000000, 0.000000000000000000 ) ) ;
#247999 = ORIENTED_EDGE ( 'NONE', *, *, #64241, .T. ) ;
#248002 = VERTEX_POINT ( 'NONE', #89440 ) ;
#248001 = B_SPLINE_CURVE_WITH_KNOTS ( 'NONE', 3,
 ( #136953, #80813, #19592, #216491, #99088, #37884, #160403, #196924, #159115, #239924, #61275, #97799, #140814, #220360, #78254, #41731, #121289, #181243, #237350 ),
 .UNSPECIFIED., .F., .F.,
 ( 4, 3, 3, 3, 3, 3, 4 ),
 ( -2.000416914662652606E-06, 0.000000000000000000, 4.714008503747417261E-05, 9.979203887777324331E-05, 0.0001372215519229504641, 0.0001635031576221021479, 0.0001900083748504133785 ),
 .UNSPECIFIED. ) ;
#248000 = FACE_OUTER_BOUND ( 'NONE', #195275, .T. ) ;
#248003 = ADVANCED_FACE ( 'NONE', ( #226366 ), #146837, .F. ) ;
#248004 = DIRECTION ( 'NONE',  ( 1.000000000000000000, 0.000000000000000000, 0.000000000000000000 ) ) ;
#248005 = ORIENTED_EDGE ( 'NONE', *, *, #182302, .F. ) ;
#248006 = AXIS2_PLACEMENT_3D ( 'NONE', #70647, #131867, #208840 ) ;
#248007 = SPHERICAL_SURFACE ( 'NONE', #205826, 0.1000000000000000056 ) ;
#248008 = VERTEX_POINT ( 'NONE', #124737 ) ;
#248009 = VECTOR ( 'NONE', #71003, 1000.000000000000000 ) ;
#248012 = ORIENTED_EDGE ( 'NONE', *, *, #41407, .T. ) ;
#248011 = VERTEX_POINT ( 'NONE', #9911 ) ;
#248010 = DIRECTION ( 'NONE',  ( 1.000000000000000000, -0.000000000000000000, -0.000000000000000000 ) ) ;
#248013 = CYLINDRICAL_SURFACE ( 'NONE', #215429, 0.09999999999999939493 ) ;
#248014 = EDGE_CURVE ( 'NONE', #47226, #175899, #66032, .T. ) ;
#248015 = CIRCLE ( 'NONE', #131496, 0.09999999999999939493 ) ;
#248016 = DIRECTION ( 'NONE',  ( 0.000000000000000000, -0.9976611540403004241, -0.06835365183350541884 ) ) ;
#248017 = ORIENTED_EDGE ( 'NONE', *, *, #148904, .T. ) ;
#248018 = CIRCLE ( 'NONE', #181416, 0.1000000000000028644 ) ;
#248019 = ORIENTED_EDGE ( 'NONE', *, *, #113571, .T. ) ;
#248020 = CARTESIAN_POINT ( 'NONE',  ( -20.94999999999999929, -11.39257802169451672, -137.0739495798319467 ) ) ;
#248021 = CARTESIAN_POINT ( 'NONE',  ( -20.94999999999999929, -1.849153571964891274, -212.6059666197970159 ) ) ;
#248022 = EDGE_CURVE ( 'NONE', #97749, #211450, #150692, .T. ) ;
#248024 = ORIENTED_EDGE ( 'NONE', *, *, #95962, .F. ) ;
#248023 = DIRECTION ( 'NONE',  ( -1.000000000000000000, -2.952720810173289112E-16, 0.000000000000000000 ) ) ;
#248025 = DIRECTION ( 'NONE',  ( 0.000000000000000000, 0.2128009952263605897, -0.9770955615653315052 ) ) ;
#248026 = EDGE_LOOP ( 'NONE', ( #123038, #199719, #236645 ) ) ;
#248028 = TOROIDAL_SURFACE ( 'NONE', #68993, 0.2000000000000000111, 0.1000000000000000056 ) ;
#248027 = DIRECTION ( 'NONE',  ( 0.8049926720990051576, 0.5932847527679298016, -0.000000000000000000 ) ) ;
#248029 = LINE ( 'NONE', #8153, #210409 ) ;
#248030 = CIRCLE ( 'NONE', #89800, 0.2000000000000057288 ) ;
#248032 = VERTEX_POINT ( 'NONE', #123450 ) ;
#248031 = ADVANCED_FACE ( 'NONE', ( #88132 ), #248523, .T. ) ;
#248033 = ADVANCED_FACE ( 'NONE', ( #126000, #202976, #205532 ), #26942, .T. ) ;
#248034 = DIRECTION ( 'NONE',  ( -1.000000000000000000, 0.000000000000000000, 0.000000000000000000 ) ) ;
#248035 = CARTESIAN_POINT ( 'NONE',  ( 18.55121869061587958, 18.40663661316796151, -236.9846611508999388 ) ) ;
#248036 = AXIS2_PLACEMENT_3D ( 'NONE', #133992, #152311, #10218 ) ;
#248037 = EDGE_LOOP ( 'NONE', ( #257339, #66224, #61701, #37296 ) ) ;
#248039 = ORIENTED_EDGE ( 'NONE', *, *, #178791, .F. ) ;
#248038 = DIRECTION ( 'NONE',  ( 0.000000000000000000, 0.000000000000000000, -1.000000000000000000 ) ) ;
#248040 = AXIS2_PLACEMENT_3D ( 'NONE', #81786, #203047, #101331 ) ;
#248041 = CARTESIAN_POINT ( 'NONE',  ( 21.05000000000000071, 76.10000000001272724, -210.0637644362255969 ) ) ;
#248042 = EDGE_CURVE ( 'NONE', #10221, #87043, #7347, .T. ) ;
#248044 = VERTEX_POINT ( 'NONE', #245968 ) ;
#248043 = VERTEX_POINT ( 'NONE', #227670 ) ;
#248045 = ORIENTED_EDGE ( 'NONE', *, *, #89371, .T. ) ;
#248046 = DIRECTION ( 'NONE',  ( 1.000000000000000000, 0.000000000000000000, 0.000000000000000000 ) ) ;
#248047 = VERTEX_POINT ( 'NONE', #49038 ) ;
#248048 = ORIENTED_EDGE ( 'NONE', *, *, #149713, .F. ) ;
#248049 = DIRECTION ( 'NONE',  ( 1.000000000000000000, 0.000000000000000000, 0.000000000000000000 ) ) ;
#248050 = CIRCLE ( 'NONE', #239681, 0.6000000000000033085 ) ;
#248051 = ORIENTED_EDGE ( 'NONE', *, *, #139843, .F. ) ;
#248052 = EDGE_CURVE ( 'NONE', #106358, #49789, #163177, .T. ) ;
#248053 = CYLINDRICAL_SURFACE ( 'NONE', #210559, 7.899999999999994138 ) ;
#248054 = EDGE_CURVE ( 'NONE', #206865, #150544, #93298, .T. ) ;
#248055 = CARTESIAN_POINT ( 'NONE',  ( 21.14999999999999503, -0.1008583690875562017, -55.25043287651065782 ) ) ;
#248056 = ORIENTED_EDGE ( 'NONE', *, *, #201434, .F. ) ;
#248057 = ORIENTED_EDGE ( 'NONE', *, *, #111925, .F. ) ;
#248058 = DIRECTION ( 'NONE',  ( 1.000000000000000000, 0.000000000000000000, 0.000000000000000000 ) ) ;
#248059 = EDGE_LOOP ( 'NONE', ( #134509, #23481, #189438, #201781 ) ) ;
#248060 = AXIS2_PLACEMENT_3D ( 'NONE', #16004, #215454, #36859 ) ;
#248061 = VECTOR ( 'NONE', #212520, 1000.000000000000000 ) ;
#248062 = AXIS2_PLACEMENT_3D ( 'NONE', #68338, #108741, #227397 ) ;
#248063 = VECTOR ( 'NONE', #853, 1000.000000000000000 ) ;
#248064 = CARTESIAN_POINT ( 'NONE',  ( -18.60000000000000853, 85.36424052760300185, -129.3428589026834743 ) ) ;
#248065 = ADVANCED_FACE ( 'NONE', ( #210682 ), #232836, .F. ) ;
#248066 = VERTEX_POINT ( 'NONE', #12509 ) ;
#248067 = ADVANCED_FACE ( 'NONE', ( #11207 ), #175435, .T. ) ;
#248068 = DIRECTION ( 'NONE',  ( 0.000000000000000000, 0.4721928772777330696, 0.8814952561688439436 ) ) ;
#248070 = ORIENTED_EDGE ( 'NONE', *, *, #245447, .T. ) ;
#248069 = DIRECTION ( 'NONE',  ( -1.000000000000000000, 2.986185139342070877E-16, -6.665775143889692774E-16 ) ) ;
#248071 = CARTESIAN_POINT ( 'NONE',  ( 19.97071067811864609, 64.27928932189385591, -178.8731074845244393 ) ) ;
#248072 = DIRECTION ( 'NONE',  ( 1.000000000000000000, 0.000000000000000000, -0.000000000000000000 ) ) ;
#248073 = FACE_OUTER_BOUND ( 'NONE', #174589, .T. ) ;
#248074 = DIRECTION ( 'NONE',  ( 1.000000000000000000, 0.000000000000000000, 0.000000000000000000 ) ) ;
#248075 = DIRECTION ( 'NONE',  ( -1.000000000000000000, 0.000000000000000000, 0.000000000000000000 ) ) ;
#248076 = CARTESIAN_POINT ( 'NONE',  ( -21.05000000000000071, 6.258316057343176197, -33.43429838967790602 ) ) ;
#248077 = SPHERICAL_SURFACE ( 'NONE', #115450, 0.1000000000000000056 ) ;
#248078 = CARTESIAN_POINT ( 'NONE',  ( -20.64999999999999858, 85.00000000001251976, -179.9170766071767389 ) ) ;
#248079 = CIRCLE ( 'NONE', #31638, 11.80000000000000426 ) ;
#248080 = ORIENTED_EDGE ( 'NONE', *, *, #146038, .T. ) ;
#248081 = EDGE_LOOP ( 'NONE', ( #76211, #129125, #89926, #20344 ) ) ;
#248082 = VECTOR ( 'NONE', #62216, 1000.000000000000000 ) ;
#248084 = EDGE_LOOP ( 'NONE', ( #43889, #114042 ) ) ;
#248083 = CARTESIAN_POINT ( 'NONE',  ( 23.15000000000000213, -11.48912529306489994, -97.40000000000004832 ) ) ;
#248085 = ORIENTED_EDGE ( 'NONE', *, *, #168100, .T. ) ;
#248086 = DIRECTION ( 'NONE',  ( 0.000000000000000000, 1.000000000000000000, -0.000000000000000000 ) ) ;
#248087 = DIRECTION ( 'NONE',  ( 1.000000000000000000, 0.000000000000000000, 0.000000000000000000 ) ) ;
#248089 = FACE_OUTER_BOUND ( 'NONE', #86651, .T. ) ;
#248088 = CARTESIAN_POINT ( 'NONE',  ( -23.25000000000000000, 69.06610602788578035, -132.7374616501508342 ) ) ;
#248090 = ORIENTED_EDGE ( 'NONE', *, *, #153750, .T. ) ;
#248091 = VERTEX_POINT ( 'NONE', #54166 ) ;
#248092 = ADVANCED_FACE ( 'NONE', ( #129849 ), #117378, .T. ) ;
#248093 = CARTESIAN_POINT ( 'NONE',  ( 18.49351773456760029, -9.443025695134176445, -40.68532552602730590 ) ) ;
#248094 = EDGE_CURVE ( 'NONE', #54306, #199182, #242250, .T. ) ;
#248095 = FACE_OUTER_BOUND ( 'NONE', #257132, .T. ) ;
#248096 = ORIENTED_EDGE ( 'NONE', *, *, #9076, .F. ) ;
#248097 = VERTEX_POINT ( 'NONE', #153319 ) ;
#248098 = DIRECTION ( 'NONE',  ( 0.000000000000000000, 0.000000000000000000, -1.000000000000000000 ) ) ;
#248099 = AXIS2_PLACEMENT_3D ( 'NONE', #70867, #90385, #211642 ) ;
#248100 = CARTESIAN_POINT ( 'NONE',  ( 20.85000000000000142, -1.835859311443637010, -45.00443916879852679 ) ) ;
#248101 = LINE ( 'NONE', #16897, #83017 ) ;
#248102 = CARTESIAN_POINT ( 'NONE',  ( -20.94999999999999929, 1.162701749949165642, -75.00000000000004263 ) ) ;
#248103 = EDGE_CURVE ( 'NONE', #208162, #70123, #67469, .T. ) ;
#248105 = ORIENTED_EDGE ( 'NONE', *, *, #190420, .F. ) ;
#248104 = DIRECTION ( 'NONE',  ( -1.000000000000000000, -2.952720810173289112E-16, 0.000000000000000000 ) ) ;
#248106 = LINE ( 'NONE', #87733, #161093 ) ;
#248107 = LINE ( 'NONE', #12099, #44077 ) ;
#248109 = EDGE_CURVE ( 'NONE', #32344, #138653, #214523, .T. ) ;
#248108 = CARTESIAN_POINT ( 'NONE',  ( -20.54999999999999716, 6.659649981195239654, -220.3002595397864241 ) ) ;
#248110 = DIRECTION ( 'NONE',  ( -0.000000000000000000, -6.982962677686266711E-15, 1.000000000000000000 ) ) ;
#248111 = ORIENTED_EDGE ( 'NONE', *, *, #149449, .T. ) ;
#248112 = CARTESIAN_POINT ( 'NONE',  ( 12.30626653967340722, 66.64320997496595567, -85.81828097591049698 ) ) ;
#248113 = DIRECTION ( 'NONE',  ( 1.000000000000000000, 3.265361837132813093E-16, -0.000000000000000000 ) ) ;
#248115 = CARTESIAN_POINT ( 'NONE',  ( 20.95000000000005613, 66.15000000001120384, -5.923107484524795296 ) ) ;
#248114 = CYLINDRICAL_SURFACE ( 'NONE', #140903, 0.09999999999999939493 ) ;
#248117 = ADVANCED_FACE ( 'NONE', ( #34639 ), #253641, .F. ) ;
#248116 = DIRECTION ( 'NONE',  ( -1.073024830501117725E-15, 0.000000000000000000, 1.000000000000000000 ) ) ;
#248118 = CARTESIAN_POINT ( 'NONE',  ( -16.80070461187925090, 9.950000000011103296, -54.35303617083764749 ) ) ;
#248119 = AXIS2_PLACEMENT_3D ( 'NONE', #124771, #24402, #85593 ) ;
#248120 = LINE ( 'NONE', #190753, #241267 ) ;
#248121 = DIRECTION ( 'NONE',  ( -0.000000000000000000, -0.000000000000000000, -1.000000000000000000 ) ) ;
#248122 = DIRECTION ( 'NONE',  ( -0.000000000000000000, -0.000000000000000000, 1.000000000000000000 ) ) ;
#248123 = AXIS2_PLACEMENT_3D ( 'NONE', #98469, #179361, #3249 ) ;
#248124 = CARTESIAN_POINT ( 'NONE',  ( -21.14999999999994174, 76.00000000001119815, -36.02310748452479316 ) ) ;
#248125 = VECTOR ( 'NONE', #166440, 1000.000000000000000 ) ;
#248126 = ORIENTED_EDGE ( 'NONE', *, *, #109994, .T. ) ;
#248127 = AXIS2_PLACEMENT_3D ( 'NONE', #66516, #202173, #22268 ) ;
#248128 = EDGE_CURVE ( 'NONE', #249995, #91602, #133708, .T. ) ;
#248130 = EDGE_CURVE ( 'NONE', #8661, #246027, #30790, .T. ) ;
#248129 = ADVANCED_FACE ( 'NONE', ( #72475 ), #192387, .F. ) ;
#248131 = ORIENTED_EDGE ( 'NONE', *, *, #45763, .F. ) ;
#248132 = ORIENTED_EDGE ( 'NONE', *, *, #105248, .F. ) ;
#248133 = CARTESIAN_POINT ( 'NONE',  ( -23.15000000000000213, 1.115600667400684642E-11, -200.9999999999999432 ) ) ;
#248134 = LINE ( 'NONE', #69521, #81899 ) ;
#248135 = VERTEX_POINT ( 'NONE', #194995 ) ;
#248136 = ADVANCED_FACE ( 'NONE', ( #211983 ), #114142, .T. ) ;
#248137 = ORIENTED_EDGE ( 'NONE', *, *, #77672, .T. ) ;
#248138 =( LENGTH_UNIT ( ) NAMED_UNIT ( * ) SI_UNIT ( .MILLI., .METRE. ) );
#248139 = EDGE_LOOP ( 'NONE', ( #220590, #17457, #209682, #152254 ) ) ;
#248140 = EDGE_CURVE ( 'NONE', #155898, #97694, #17409, .T. ) ;
#248141 = DIRECTION ( 'NONE',  ( 1.000000000000000000, 0.000000000000000000, 0.000000000000000000 ) ) ;
#248142 = ADVANCED_FACE ( 'NONE', ( #112870 ), #252358, .F. ) ;
#248143 = AXIS2_PLACEMENT_3D ( 'NONE', #241917, #163683, #204074 ) ;
#248144 = VERTEX_POINT ( 'NONE', #134968 ) ;
#248145 = STYLED_ITEM ( 'NONE', ( #247096 ), #191218 ) ;
#248146 = CARTESIAN_POINT ( 'NONE',  ( -21.05000000000000071, -1.835341550213255957, -78.55515129256302487 ) ) ;
#248147 = VECTOR ( 'NONE', #208224, 1000.000000000000000 ) ;
#248148 = DIRECTION ( 'NONE',  ( -2.940209281316621016E-16, 1.000000000000000000, 0.000000000000000000 ) ) ;
#248149 = DIRECTION ( 'NONE',  ( 2.952720810173289605E-16, 0.9651348961777155289, -0.2617529984165038459 ) ) ;
#248150 = ADVANCED_FACE ( 'NONE', ( #35921 ), #95850, .T. ) ;
#248151 = DIRECTION ( 'NONE',  ( 4.239556034732056743E-17, -0.1298341882520022972, -0.9915357197604853789 ) ) ;
#248152 = PLANE ( 'NONE',  #53545 ) ;
#248155 = EDGE_LOOP ( 'NONE', ( #191351, #35154, #143832, #4550 ) ) ;
#248154 = CARTESIAN_POINT ( 'NONE',  ( 23.14999999999999858, 76.00000000001244871, -170.0231074845243597 ) ) ;
#248153 = CIRCLE ( 'NONE', #164771, 0.6000000000000015321 ) ;
#248157 = DIRECTION ( 'NONE',  ( 1.000000000000000000, 0.000000000000000000, 0.000000000000000000 ) ) ;
#248156 = CARTESIAN_POINT ( 'NONE',  ( 23.25000000000000000, -11.74999999998883560, -155.7499999999999716 ) ) ;
#248158 = CARTESIAN_POINT ( 'NONE',  ( -18.40000000000000568, 64.52683809664975456, -149.1316861282871287 ) ) ;
#248159 =( BOUNDED_CURVE ( )  B_SPLINE_CURVE ( 3, ( #51944, #50661, #170688, #152383 ),
 .UNSPECIFIED., .F., .F. ) 
 B_SPLINE_CURVE_WITH_KNOTS ( ( 4, 4 ),
 ( 5.731445031868799056, 5.983100554402348337 ),
 .UNSPECIFIED. ) 
 CURVE ( )  GEOMETRIC_REPRESENTATION_ITEM ( )  RATIONAL_B_SPLINE_CURVE ( ( 1.000000000000000000, 0.9947294176030464508, 0.9947294176030464508, 1.000000000000000000 ) ) 
 REPRESENTATION_ITEM ( '' )  );
#248160 = EDGE_CURVE ( 'NONE', #32552, #83659, #38466, .T. ) ;
#248161 = ORIENTED_EDGE ( 'NONE', *, *, #173914, .F. ) ;
#248162 = CARTESIAN_POINT ( 'NONE',  ( 12.60053434924910043, 66.61046543766534000, -120.8482981801344209 ) ) ;
#248163 = AXIS2_PLACEMENT_3D ( 'NONE', #74476, #194410, #154027 ) ;
#248164 = CARTESIAN_POINT ( 'NONE',  ( -13.43673303185028800, 9.446648990640014176, -115.5891632959231998 ) ) ;
#248165 = DIRECTION ( 'NONE',  ( 1.000000000000000000, 0.000000000000000000, 0.000000000000000000 ) ) ;
#248167 = EDGE_LOOP ( 'NONE', ( #246707, #118428, #15859, #117787 ) ) ;
#248166 = AXIS2_PLACEMENT_3D ( 'NONE', #88647, #91252, #228196 ) ;
#248168 = EDGE_CURVE ( 'NONE', #18671, #197260, #92416, .T. ) ;
#248169 = DIRECTION ( 'NONE',  ( 0.000000000000000000, 0.2617529984165038459, 0.9651348961777155289 ) ) ;
#248170 = FACE_OUTER_BOUND ( 'NONE', #214404, .T. ) ;
#248171 = EDGE_LOOP ( 'NONE', ( #144253, #197834, #180180, #191924 ) ) ;
#248172 = CIRCLE ( 'NONE', #135731, 0.1000000000000124678 ) ;
#248173 = DIRECTION ( 'NONE',  ( 0.000000000000000000, -1.000000000000000000, 0.000000000000000000 ) ) ;
#248174 = CARTESIAN_POINT ( 'NONE',  ( -18.40000000000000213, 5.650000000011139001, -158.2500000000000284 ) ) ;
#248176 =( BOUNDED_CURVE ( )  B_SPLINE_CURVE ( 3, ( #234124, #150749, #252391, #154630 ),
 .UNSPECIFIED., .F., .F. ) 
 B_SPLINE_CURVE_WITH_KNOTS ( ( 4, 4 ),
 ( 4.712388980384690562, 6.283185307179586232 ),
 .UNSPECIFIED. ) 
 CURVE ( )  GEOMETRIC_REPRESENTATION_ITEM ( )  RATIONAL_B_SPLINE_CURVE ( ( 1.000000000000000000, 0.8047378541243652705, 0.8047378541243652705, 1.000000000000000000 ) ) 
 REPRESENTATION_ITEM ( '' )  );
#248175 = CIRCLE ( 'NONE', #223220, 0.09999999999999939493 ) ;
#248177 = DIRECTION ( 'NONE',  ( 0.000000000000000000, -1.776356839400250465E-15, 1.000000000000000000 ) ) ;
#248178 = DIRECTION ( 'NONE',  ( 2.952720810173289112E-16, -1.000000000000000000, 0.000000000000000000 ) ) ;
#248179 = ADVANCED_FACE ( 'NONE', ( #219658 ), #204838, .F. ) ;
#248180 = ORIENTED_EDGE ( 'NONE', *, *, #133997, .T. ) ;
#248181 = CIRCLE ( 'NONE', #48262, 0.6000000000000033085 ) ;
#248182 = VECTOR ( 'NONE', #129205, 1000.000000000000000 ) ;
#248183 = ORIENTED_EDGE ( 'NONE', *, *, #149992, .F. ) ;
#248185 = EDGE_CURVE ( 'NONE', #109684, #170534, #83996, .T. ) ;
#248184 = LINE ( 'NONE', #89097, #173556 ) ;
#248186 = CARTESIAN_POINT ( 'NONE',  ( 21.05000000000000071, 10.72371710470752149, -7.664913569087605794 ) ) ;
#248187 = CARTESIAN_POINT ( 'NONE',  ( -21.04999999999999716, 65.63518786100092939, -242.0677770231893078 ) ) ;
#248188 = DIRECTION ( 'NONE',  ( 1.000000000000000000, 0.000000000000000000, 0.000000000000000000 ) ) ;
#248189 = DIRECTION ( 'NONE',  ( -1.000000000000000000, -2.952720810173289112E-16, 0.000000000000000000 ) ) ;
#248190 = DIRECTION ( 'NONE',  ( -1.000000000000000000, 0.000000000000000000, 0.000000000000000000 ) ) ;
#248191 = DIRECTION ( 'NONE',  ( 0.000000000000000000, -7.116814260417668513E-15, 1.000000000000000000 ) ) ;
#248192 = DIRECTION ( 'NONE',  ( -0.000000000000000000, 6.982962677686266711E-15, -1.000000000000000000 ) ) ;
#248193 = ORIENTED_EDGE ( 'NONE', *, *, #195457, .F. ) ;
#248195 =( BOUNDED_SURFACE ( )  B_SPLINE_SURFACE ( 3, 2, ( 
 ( #182200, #203026, #64802 ),
 ( #83046, #60948, #223862 ),
 ( #24428, #140479, #81767 ),
 ( #45246, #23142, #103907 ),
 ( #124792, #161359, #62245 ),
 ( #29568, #50352, #165195 ),
 ( #188600, #9970, #167791 ),
 ( #7391, #109059, #205585 ),
 ( #226423, #244712, #71250 ),
 ( #204302, #69967, #47790 ) ),
 .UNSPECIFIED., .F., .F., .F. ) 
 B_SPLINE_SURFACE_WITH_KNOTS ( ( 4, 2, 2, 2, 4 ),
 ( 3, 3 ),
 ( 0.002161241639767785133, 0.002579950749617451571, 0.002789305304542284789, 0.002893982582004701182, 0.002998659859467118008 ),
 ( 0.000000000000000000, 1.000000000000000000 ),
 .UNSPECIFIED. ) 
 GEOMETRIC_REPRESENTATION_ITEM ( )  RATIONAL_B_SPLINE_SURFACE ( (
 ( 1.000000000000000000, 0.7071067811864985009, 1.000000000000000000),
 ( 1.000000000000000000, 0.7632447400666292348, 1.000000000000000000),
 ( 1.000000000000000000, 0.8158073005106037945, 1.000000000000000000),
 ( 1.000000000000000000, 0.8906973462397418384, 1.000000000000000000),
 ( 1.000000000000000000, 0.9149408947799445579, 1.000000000000000000),
 ( 1.000000000000000000, 0.9493368785276108390, 1.000000000000000000),
 ( 1.000000000000000000, 0.9605194247158034271, 1.000000000000000000),
 ( 1.000000000000000000, 0.9803630264779761294, 1.000000000000000000),
 ( 1.000000000000000000, 0.9900844824272162503, 1.000000000000000000),
 ( 1.000000000000000000, 0.9894588281429244070, 1.000000000000000000) ) ) 
 REPRESENTATION_ITEM ( '' )  SURFACE ( )  );
#248194 = CYLINDRICAL_SURFACE ( 'NONE', #120112, 0.09999999999999939493 ) ;
#248197 = ORIENTED_EDGE ( 'NONE', *, *, #195356, .F. ) ;
#248196 = DIRECTION ( 'NONE',  ( -1.000000000000000000, 0.000000000000000000, 0.000000000000000000 ) ) ;
#248198 = CARTESIAN_POINT ( 'NONE',  ( -18.50000000000000000, 9.250000000011157297, -54.85000000000000142 ) ) ;
#248199 = CYLINDRICAL_SURFACE ( 'NONE', #199036, 0.09999999999999939493 ) ;
#248200 = CYLINDRICAL_SURFACE ( 'NONE', #133733, 0.09999999999999939493 ) ;
#248201 = FACE_OUTER_BOUND ( 'NONE', #92495, .T. ) ;
#248202 = ADVANCED_FACE ( 'NONE', ( #78853 ), #37939, .T. ) ;
#248203 = CARTESIAN_POINT ( 'NONE',  ( 20.96428641294170703, 11.75000000001150013, -194.1748931779407030 ) ) ;
#248205 = ORIENTED_EDGE ( 'NONE', *, *, #244998, .F. ) ;
#248204 = CARTESIAN_POINT ( 'NONE',  ( -23.15000000000000213, 12.62988036037870643, -223.4632815780722410 ) ) ;
#248206 = DIRECTION ( 'NONE',  ( 0.000000000000000000, 0.1618390714546044939, 0.9868171638914228216 ) ) ;
#248207 = CARTESIAN_POINT ( 'NONE',  ( -18.50000324121759121, 65.70692517833286672, -164.5644653378303985 ) ) ;
#248208 = FACE_OUTER_BOUND ( 'NONE', #216264, .T. ) ;
#248209 = DIRECTION ( 'NONE',  ( 1.000000000000000000, 0.000000000000000000, 0.000000000000000000 ) ) ;
#248210 = VERTEX_POINT ( 'NONE', #200112 ) ;
#248211 = DIRECTION ( 'NONE',  ( -1.000000000000000000, -0.000000000000000000, 0.000000000000000000 ) ) ;
#248212 = AXIS2_PLACEMENT_3D ( 'NONE', #177134, #139232, #57129 ) ;
#248213 = EDGE_LOOP ( 'NONE', ( #173641, #251462, #155398, #254154 ) ) ;
#248214 = CIRCLE ( 'NONE', #168953, 0.09999999999998898659 ) ;
#248215 = CIRCLE ( 'NONE', #52562, 0.1000000000000053069 ) ;
#248216 = TOROIDAL_SURFACE ( 'NONE', #98313, 11.65000000000000036, 0.1000000000000000056 ) ;
#248217 = DIRECTION ( 'NONE',  ( 0.000000000000000000, 0.2128009952263601179, -0.9770955615653315052 ) ) ;
#248218 = ORIENTED_EDGE ( 'NONE', *, *, #160759, .F. ) ;
#248219 = EDGE_CURVE ( 'NONE', #156064, #77477, #113277, .T. ) ;
#248220 = DIRECTION ( 'NONE',  ( 1.000000000000000000, -0.000000000000000000, -0.000000000000000000 ) ) ;
#248221 = VERTEX_POINT ( 'NONE', #21492 ) ;
#248222 = CIRCLE ( 'NONE', #23392, 0.1999999999999995670 ) ;
#248223 = DIRECTION ( 'NONE',  ( 0.000000000000000000, 0.9126074666063501706, 0.4088369013363880589 ) ) ;
#248224 = CARTESIAN_POINT ( 'NONE',  ( -18.59999999999999787, 45.93315328338058379, -256.6017782078560003 ) ) ;
#248225 = FACE_OUTER_BOUND ( 'NONE', #251103, .T. ) ;
#248226 = ORIENTED_EDGE ( 'NONE', *, *, #45729, .T. ) ;
#248227 = AXIS2_PLACEMENT_3D ( 'NONE', #83532, #66583, #183951 ) ;
#248228 = CARTESIAN_POINT ( 'NONE',  ( -16.92280123533711489, 9.949999999999983302, -12.85063231408517659 ) ) ;
#248229 = AXIS2_PLACEMENT_3D ( 'NONE', #212271, #113152, #192698 ) ;
#248230 = LINE ( 'NONE', #109989, #253787 ) ;
#248231 = CARTESIAN_POINT ( 'NONE',  ( -23.15000000000000213, 74.00000000001180922, -82.24772940728641402 ) ) ;
#248232 = DIRECTION ( 'NONE',  ( 0.000000000000000000, 0.2128009952263362758, -0.9770955615653368342 ) ) ;
#248233 = CARTESIAN_POINT ( 'NONE',  ( -20.00857864376270001, 11.76393579169289083, -211.0774408799668720 ) ) ;
#248234 = ORIENTED_EDGE ( 'NONE', *, *, #198613, .F. ) ;
#248236 = VERTEX_POINT ( 'NONE', #41062 ) ;
#248235 = CARTESIAN_POINT ( 'NONE',  ( 20.94999999999999929, 76.00000000001193712, -107.1231074845243114 ) ) ;
#248237 = EDGE_LOOP ( 'NONE', ( #161204, #250330, #93771, #108707 ) ) ;
#248238 = FACE_OUTER_BOUND ( 'NONE', #234959, .T. ) ;
#248239 = ORIENTED_EDGE ( 'NONE', *, *, #206587, .F. ) ;
#248240 = CARTESIAN_POINT ( 'NONE',  ( 20.94999999999999929, 1.115600667400684642E-11, -134.0000000000000000 ) ) ;
#248241 = DIRECTION ( 'NONE',  ( -1.000000000000000000, 1.207181226542539700E-16, -2.694675058168174199E-16 ) ) ;
#248242 = DIRECTION ( 'NONE',  ( -1.000000000000000000, 0.000000000000000000, 0.000000000000000000 ) ) ;
#248244 = ORIENTED_EDGE ( 'NONE', *, *, #117927, .F. ) ;
#248243 = AXIS2_PLACEMENT_3D ( 'NONE', #107887, #49198, #27105 ) ;
#248245 = CYLINDRICAL_SURFACE ( 'NONE', #3227, 2.000000000000001776 ) ;
#248246 = FACE_OUTER_BOUND ( 'NONE', #194248, .T. ) ;
#248247 = DIRECTION ( 'NONE',  ( -0.000000000000000000, 1.000000000000000000, 6.982962677686266711E-15 ) ) ;
#248248 = VERTEX_POINT ( 'NONE', #119295 ) ;
#248250 = ORIENTED_EDGE ( 'NONE', *, *, #153951, .F. ) ;
#248249 = DIRECTION ( 'NONE',  ( 0.000000000000000000, -0.8009761297185381546, 0.5986962832865355688 ) ) ;
#248251 = EDGE_CURVE ( 'NONE', #244003, #165845, #213213, .T. ) ;
#248252 = DIRECTION ( 'NONE',  ( 1.000000000000000000, -3.265361837132813093E-16, -2.280189983783949500E-30 ) ) ;
#248253 = DIRECTION ( 'NONE',  ( 1.000000000000000000, -0.000000000000000000, -0.000000000000000000 ) ) ;
#248254 = CIRCLE ( 'NONE', #90025, 0.09999999999998898659 ) ;
#248255 = CIRCLE ( 'NONE', #6642, 0.09999999999999939493 ) ;
#248256 = AXIS2_PLACEMENT_3D ( 'NONE', #145952, #130237, #204636 ) ;
#248257 = AXIS2_PLACEMENT_3D ( 'NONE', #168677, #69543, #53811 ) ;
#248258 = ORIENTED_EDGE ( 'NONE', *, *, #213877, .F. ) ;
#248259 = CYLINDRICAL_SURFACE ( 'NONE', #214272, 0.09999999999998898659 ) ;
#248260 = CARTESIAN_POINT ( 'NONE',  ( -17.73285935862988083, 41.56619374751048213, -235.4550095799147016 ) ) ;
#248261 = DIRECTION ( 'NONE',  ( 0.7071359030027302151, -0.2890794387707354418, 0.6452843503173697481 ) ) ;
#248262 = ORIENTED_EDGE ( 'NONE', *, *, #115777, .T. ) ;
#248263 = CARTESIAN_POINT ( 'NONE',  ( 20.94999999999999574, 62.00000000001161737, -64.09601495414187866 ) ) ;
#248264 = ADVANCED_FACE ( 'NONE', ( #29222 ), #226056, .F. ) ;
#248265 = LINE ( 'NONE', #211724, #134768 ) ;
#248266 = EDGE_CURVE ( 'NONE', #5558, #145447, #234068, .T. ) ;
#248267 = ORIENTED_EDGE ( 'NONE', *, *, #41955, .T. ) ;
#248268 = CIRCLE ( 'NONE', #81629, 0.8750000000000007772 ) ;
#248269 = VECTOR ( 'NONE', #56317, 1000.000000000000000 ) ;
#248270 = ADVANCED_FACE ( 'NONE', ( #163551 ), #85260, .F. ) ;
#248271 = VERTEX_POINT ( 'NONE', #107425 ) ;
#248272 = CARTESIAN_POINT ( 'NONE',  ( 21.10257677756356642, 0.02495074957913656979, -94.10161825746727970 ) ) ;
#248273 = EDGE_CURVE ( 'NONE', #219135, #2368, #162284, .T. ) ;
#248274 = VERTEX_POINT ( 'NONE', #4463 ) ;
#248275 = ADVANCED_FACE ( 'NONE', ( #104818 ), #103552, .F. ) ;
#248276 = DIRECTION ( 'NONE',  ( 1.000000000000000000, 0.000000000000000000, 0.000000000000000000 ) ) ;
#248277 = CARTESIAN_POINT ( 'NONE',  ( -16.89797118371649276, 9.976380722655642685, -79.56270663244107766 ) ) ;
#248279 = ORIENTED_EDGE ( 'NONE', *, *, #209040, .F. ) ;
#248278 = CARTESIAN_POINT ( 'NONE',  ( -20.54999999999999716, 68.85000000001186038, -90.77310748452435973 ) ) ;
#248280 = FACE_BOUND ( 'NONE', #180031, .T. ) ;
#248281 = DIRECTION ( 'NONE',  ( -1.000000000000000000, -0.000000000000000000, -0.000000000000000000 ) ) ;
#248282 = ADVANCED_FACE ( 'NONE', ( #206530 ), #128287, .T. ) ;
#248283 = FACE_OUTER_BOUND ( 'NONE', #199085, .T. ) ;
#248284 = DIRECTION ( 'NONE',  ( 1.000000000000000000, 0.000000000000000000, 0.000000000000000000 ) ) ;
#248285 = CARTESIAN_POINT ( 'NONE',  ( 20.04142135623730070, 11.65000000001115943, -155.2500000000000284 ) ) ;
#248286 = DIRECTION ( 'NONE',  ( 0.000000000000000000, 0.000000000000000000, -1.000000000000000000 ) ) ;
#248287 = CARTESIAN_POINT ( 'NONE',  ( 19.90000000000000568, 5.572646938319270937, 16.50000000000000000 ) ) ;
#248289 = ORIENTED_EDGE ( 'NONE', *, *, #19670, .T. ) ;
#248288 = CARTESIAN_POINT ( 'NONE',  ( -22.43310005002225438, 75.99436305787115487, -114.6727696116587083 ) ) ;
#248290 = CARTESIAN_POINT ( 'NONE',  ( 21.09551895715259207, 22.93116773457091284, -230.1482378004415352 ) ) ;
#248291 = EDGE_CURVE ( 'NONE', #173652, #244838, #17053, .T. ) ;
#248292 = AXIS2_PLACEMENT_3D ( 'NONE', #70733, #150259, #254445 ) ;
#248293 = PLANE ( 'NONE',  #247416 ) ;
#248294 = CARTESIAN_POINT ( 'NONE',  ( -21.14999999999994174, 74.16448838626247664, -47.52760213295649550 ) ) ;
#248295 = DIRECTION ( 'NONE',  ( 1.000000000000000000, 0.000000000000000000, 0.000000000000000000 ) ) ;
#248296 = CARTESIAN_POINT ( 'NONE',  ( 21.30000000000002558, 10.69888912757691024, -235.6450824654141059 ) ) ;
#248297 = B_SPLINE_CURVE_WITH_KNOTS ( 'NONE', 3,
 ( #37929, #57450, #117448, #97843, #39216, #198252, #19636 ),
 .UNSPECIFIED., .F., .F.,
 ( 4, 3, 4 ),
 ( 0.000000000000000000, 0.0009834301579439998740, 0.001767853679402675614 ),
 .UNSPECIFIED. ) ;
#248298 = EDGE_LOOP ( 'NONE', ( #177038, #227052, #238632 ) ) ;
#248299 = EDGE_CURVE ( 'NONE', #151453, #201773, #129993, .T. ) ;
#248300 = LINE ( 'NONE', #147928, #31379 ) ;
#248301 = CARTESIAN_POINT ( 'NONE',  ( -20.94999999999999929, 1.835341550235567887, -45.05515129256298223 ) ) ;
#248302 = CARTESIAN_POINT ( 'NONE',  ( 23.14999999999999858, 76.00000000001267608, -203.5231074845243597 ) ) ;
#248303 = CIRCLE ( 'NONE', #210888, 0.09999999999999939493 ) ;
#248304 = VERTEX_POINT ( 'NONE', #186992 ) ;
#248305 = CIRCLE ( 'NONE', #90074, 0.1000000000000028644 ) ;
#248306 = CIRCLE ( 'NONE', #15087, 0.1000000000000028644 ) ;
#248307 = FACE_OUTER_BOUND ( 'NONE', #48761, .T. ) ;
#248308 = CARTESIAN_POINT ( 'NONE',  ( 18.59999999999999432, 74.83729825007431202, -161.9231074845243654 ) ) ;
#248309 =( GEOMETRIC_REPRESENTATION_CONTEXT ( 3 ) GLOBAL_UNCERTAINTY_ASSIGNED_CONTEXT ( ( #21836 ) ) GLOBAL_UNIT_ASSIGNED_CONTEXT ( ( #201303, #22700, #83881 ) ) REPRESENTATION_CONTEXT ( 'NONE', 'WORKASPACE' ) );
#248310 = EDGE_CURVE ( 'NONE', #46741, #241487, #171743, .T. ) ;
#248311 = ORIENTED_EDGE ( 'NONE', *, *, #53149, .F. ) ;
#248312 = FACE_OUTER_BOUND ( 'NONE', #248346, .T. ) ;
#248313 = VERTEX_POINT ( 'NONE', #123148 ) ;
#248314 = CARTESIAN_POINT ( 'NONE',  ( 21.87500000000000355, 9.750000000011153745, -155.2500000000000284 ) ) ;
#248315 = ORIENTED_EDGE ( 'NONE', *, *, #3950, .T. ) ;
#248316 = DIRECTION ( 'NONE',  ( 1.000000000000000000, 0.000000000000000000, 0.000000000000000000 ) ) ;
#248317 = DIRECTION ( 'NONE',  ( -0.000000000000000000, -0.8814952561688430555, 0.4721928772777346239 ) ) ;
#248318 = VERTEX_POINT ( 'NONE', #202669 ) ;
#248319 = VERTEX_POINT ( 'NONE', #166158 ) ;
#248320 = DIRECTION ( 'NONE',  ( -1.000000000000000000, 0.000000000000000000, 0.000000000000000000 ) ) ;
#248322 = ORIENTED_EDGE ( 'NONE', *, *, #133598, .T. ) ;
#248321 = DIRECTION ( 'NONE',  ( 0.000000000000000000, 0.1568667991644863147, 0.9876197685951252359 ) ) ;
#248323 = CARTESIAN_POINT ( 'NONE',  ( -23.15000000000000213, 6.268811756569107274, -220.3853799378769622 ) ) ;
#248325 = ORIENTED_EDGE ( 'NONE', *, *, #181485, .F. ) ;
#248324 = VECTOR ( 'NONE', #5685, 1000.000000000000000 ) ;
#248326 = EDGE_CURVE ( 'NONE', #202321, #91017, #242441, .T. ) ;
#248327 = CIRCLE ( 'NONE', #85794, 4.150000000000003020 ) ;
#248328 = ORIENTED_EDGE ( 'NONE', *, *, #17346, .T. ) ;
#248329 = CIRCLE ( 'NONE', #123246, 0.1000000000000055844 ) ;
#248330 = DIRECTION ( 'NONE',  ( -0.000000000000000000, -0.3280696808754172689, -0.9446535261620008228 ) ) ;
#248331 = LINE ( 'NONE', #226159, #72173 ) ;
#248332 = ADVANCED_FACE ( 'NONE', ( #44891 ), #25347, .F. ) ;
#248333 = CARTESIAN_POINT ( 'NONE',  ( 20.85000000000000142, 36.65892442174935439, -249.5511627012433848 ) ) ;
#248334 = AXIS2_PLACEMENT_3D ( 'NONE', #103923, #962, #183497 ) ;
#248335 = CARTESIAN_POINT ( 'NONE',  ( -16.77828822459933633, 9.946229375056461208, -20.83737174908105771 ) ) ;
#248336 = AXIS2_PLACEMENT_3D ( 'NONE', #4629, #84125, #163730 ) ;
#248337 = DIRECTION ( 'NONE',  ( 1.000000000000000000, 0.000000000000000000, 0.000000000000000000 ) ) ;
#248338 = CARTESIAN_POINT ( 'NONE',  ( -21.44999999999999929, 7.349999999999998757, -21.25000000000000000 ) ) ;
#248340 = ORIENTED_EDGE ( 'NONE', *, *, #187398, .F. ) ;
#248339 = EDGE_CURVE ( 'NONE', #219191, #121939, #146530, .T. ) ;
#248342 = EDGE_CURVE ( 'NONE', #42612, #130077, #37906, .T. ) ;
#248341 = CARTESIAN_POINT ( 'NONE',  ( -21.93642651522410247, 60.15957072538983397, -233.9372187734386443 ) ) ;
#248343 = DIRECTION ( 'NONE',  ( -1.000000000000000000, 0.000000000000000000, 0.000000000000000000 ) ) ;
#248344 = CARTESIAN_POINT ( 'NONE',  ( 21.05000000000000071, 70.10000000001149090, -46.24220724918073699 ) ) ;
#248345 = FACE_OUTER_BOUND ( 'NONE', #205437, .T. ) ;
#248346 = EDGE_LOOP ( 'NONE', ( #176484, #250916, #106877, #117018 ) ) ;
#248347 = CARTESIAN_POINT ( 'NONE',  ( 18.50596464788227280, 10.30632246271648889, -106.0041836778896283 ) ) ;
#248348 = ORIENTED_EDGE ( 'NONE', *, *, #153312, .F. ) ;
#248349 = CARTESIAN_POINT ( 'NONE',  ( 23.14999999999999858, 9.273719881888197847, -221.1390486761779925 ) ) ;
#248350 = ORIENTED_EDGE ( 'NONE', *, *, #253906, .F. ) ;
#248351 = CIRCLE ( 'NONE', #44178, 0.09999999999999543976 ) ;
#248352 = AXIS2_PLACEMENT_3D ( 'NONE', #98617, #76520, #156103 ) ;
#248353 = AXIS2_PLACEMENT_3D ( 'NONE', #79170, #234400, #177037 ) ;
#248354 = DIRECTION ( 'NONE',  ( 1.000000000000000000, -1.836970198721029934E-16, -1.282749433769087582E-30 ) ) ;
#248355 = DIRECTION ( 'NONE',  ( -1.000000000000000000, 0.000000000000000000, -0.000000000000000000 ) ) ;
#248356 = EDGE_CURVE ( 'NONE', #244509, #94515, #183126, .T. ) ;
#248357 = EDGE_LOOP ( 'NONE', ( #255121, #85940, #42165, #97572 ) ) ;
#248358 = ORIENTED_EDGE ( 'NONE', *, *, #163596, .T. ) ;
#248360 = ORIENTED_EDGE ( 'NONE', *, *, #199853, .T. ) ;
#248359 = DIRECTION ( 'NONE',  ( -0.000000000000000000, 1.000000000000000000, -0.000000000000000000 ) ) ;
#248361 = DIRECTION ( 'NONE',  ( 0.000000000000000000, 6.982962677686267499E-15, -1.000000000000000000 ) ) ;
#248362 = ORIENTED_EDGE ( 'NONE', *, *, #161076, .T. ) ;
#248363 = AXIS2_PLACEMENT_3D ( 'NONE', #174314, #193837, #70052 ) ;
#248364 = DIRECTION ( 'NONE',  ( 0.000000000000000000, 0.000000000000000000, -1.000000000000000000 ) ) ;
#248365 = SURFACE_STYLE_FILL_AREA ( #9745 ) ;
#248366 = ORIENTED_EDGE ( 'NONE', *, *, #82070, .F. ) ;
#248367 = CARTESIAN_POINT ( 'NONE',  ( 20.94999999999999929, 84.66355140188147743, -160.4990063664569959 ) ) ;
#248368 = VECTOR ( 'NONE', #55583, 1000.000000000000000 ) ;
#248369 = CYLINDRICAL_SURFACE ( 'NONE', #49190, 0.09999999999999939493 ) ;
#248370 = ORIENTED_EDGE ( 'NONE', *, *, #49856, .F. ) ;
#248371 = EDGE_CURVE ( 'NONE', #233233, #171475, #188283, .T. ) ;
#248372 = DIRECTION ( 'NONE',  ( 0.000000000000000000, -7.147358527629762208E-15, 1.000000000000000000 ) ) ;
#248373 = FACE_OUTER_BOUND ( 'NONE', #142617, .T. ) ;
#248374 = EDGE_CURVE ( 'NONE', #82203, #40580, #158716, .T. ) ;
#248375 = ADVANCED_FACE ( 'NONE', ( #14781 ), #233809, .T. ) ;
#248376 = CARTESIAN_POINT ( 'NONE',  ( -20.00857864376270001, 9.150000000000002132, -21.15000000000000213 ) ) ;
#248378 = ORIENTED_EDGE ( 'NONE', *, *, #30025, .T. ) ;
#248377 = PLANE ( 'NONE',  #14148 ) ;
#248379 = CIRCLE ( 'NONE', #44388, 0.2000000000000057288 ) ;
#248380 = CARTESIAN_POINT ( 'NONE',  ( 23.24999999999999645, 71.00000000001158185, -57.11784146561126363 ) ) ;
#248381 = CARTESIAN_POINT ( 'NONE',  ( 21.05000000000000071, 67.18454772081405224, -61.10271493191011416 ) ) ;
#248382 = AXIS2_PLACEMENT_3D ( 'NONE', #122290, #86976, #27066 ) ;
#248383 = CARTESIAN_POINT ( 'NONE',  ( -20.64999999999999858, 76.00000000001243450, -168.1231074845243540 ) ) ;
#248385 = CARTESIAN_POINT ( 'NONE',  ( -17.73285935862742235, 59.43258456655187416, -223.1286478281496954 ) ) ;
#248384 = CARTESIAN_POINT ( 'NONE',  ( -18.52328366898031931, -9.642321089030097880, -140.7148193375701055 ) ) ;
#248387 = CIRCLE ( 'NONE', #135949, 0.1000000000000072220 ) ;
#248386 = CARTESIAN_POINT ( 'NONE',  ( 20.85000000000000142, -11.64999999998883595, -100.5000000000000426 ) ) ;
#248388 = CIRCLE ( 'NONE', #135950, 11.74999999999999645 ) ;
#248389 = CARTESIAN_POINT ( 'NONE',  ( 18.39999999999999858, -9.499999999988842703, -107.5320693966997112 ) ) ;
#248390 = CARTESIAN_POINT ( 'NONE',  ( 20.94999999999999574, 1.851028230152016674, -78.65391326942254580 ) ) ;
#248391 = CARTESIAN_POINT ( 'NONE',  ( -21.05000000000000071, 76.09999996531196587, -176.5006596670181409 ) ) ;
#248392 = EDGE_LOOP ( 'NONE', ( #108790, #52201, #197789, #122644 ) ) ;
#248393 = VERTEX_POINT ( 'NONE', #10908 ) ;
#248394 = ORIENTED_EDGE ( 'NONE', *, *, #60810, .T. ) ;
#248395 = CIRCLE ( 'NONE', #240036, 0.1000000000000028644 ) ;
#248396 = LINE ( 'NONE', #8508, #77616 ) ;
#248397 = CIRCLE ( 'NONE', #119240, 0.09999999999999939493 ) ;
#248398 = DIRECTION ( 'NONE',  ( -1.000000000000000000, 0.000000000000000000, 0.000000000000000000 ) ) ;
#248400 = EDGE_CURVE ( 'NONE', #215723, #46648, #132130, .T. ) ;
#248399 = ORIENTED_EDGE ( 'NONE', *, *, #92532, .T. ) ;
#248401 = AXIS2_PLACEMENT_3D ( 'NONE', #146194, #242725, #184043 ) ;
#248402 =( LENGTH_UNIT ( ) NAMED_UNIT ( * ) SI_UNIT ( .MILLI., .METRE. ) );
#248403 = DIRECTION ( 'NONE',  ( 0.000000000000000000, 0.4721928772777346239, 0.8814952561688430555 ) ) ;
#248404 = DIRECTION ( 'NONE',  ( 0.000000000000000000, -1.387778780781454006E-13, -1.000000000000000000 ) ) ;
#248405 = ADVANCED_FACE ( 'NONE', ( #94275 ), #212953, .F. ) ;
#248406 = DIRECTION ( 'NONE',  ( 0.000000000000000000, -0.4999999999999348299, 0.8660254037844762331 ) ) ;
#248407 = ORIENTED_EDGE ( 'NONE', *, *, #257033, .T. ) ;
#248408 = ORIENTED_EDGE ( 'NONE', *, *, #193042, .T. ) ;
#248409 = DIRECTION ( 'NONE',  ( 0.000000000000000000, 0.000000000000000000, 1.000000000000000000 ) ) ;
#248410 = DIRECTION ( 'NONE',  ( 1.000000000000000000, 0.000000000000000000, 0.000000000000000000 ) ) ;
#248411 = EDGE_LOOP ( 'NONE', ( #130608, #14981, #226782, #42627 ) ) ;
#248412 = AXIS2_PLACEMENT_3D ( 'NONE', #119458, #257606, #138969 ) ;
#248413 = EDGE_CURVE ( 'NONE', #218484, #97104, #25418, .T. ) ;
#248414 = CARTESIAN_POINT ( 'NONE',  ( 23.14999999999998437, 76.00000000001197975, -107.0731074845243143 ) ) ;
#248416 = ORIENTED_EDGE ( 'NONE', *, *, #198243, .F. ) ;
#248415 = DIRECTION ( 'NONE',  ( -1.000000000000000000, -0.000000000000000000, 0.000000000000000000 ) ) ;
#248417 = DIRECTION ( 'NONE',  ( -1.000000000000000000, 0.000000000000000000, 0.000000000000000000 ) ) ;
#248418 = DIRECTION ( 'NONE',  ( 0.000000000000000000, 1.224646799147316229E-16, 1.000000000000000000 ) ) ;
#248420 = ORIENTED_EDGE ( 'NONE', *, *, #3142, .T. ) ;
#248419 = DIRECTION ( 'NONE',  ( -2.602085213965226419E-14, -0.2617529984165031243, -0.9651348961777157509 ) ) ;
#248422 = EDGE_CURVE ( 'NONE', #161112, #20995, #116992, .T. ) ;
#248421 = SURFACE_SIDE_STYLE ('',( #128474 ) ) ;
#248423 = CARTESIAN_POINT ( 'NONE',  ( -20.54999999999999716, 63.44052078637213299, -222.1345147897817185 ) ) ;
#248424 = DIRECTION ( 'NONE',  ( 1.000000000000000000, 0.000000000000000000, -0.000000000000000000 ) ) ;
#248425 = DIRECTION ( 'NONE',  ( 1.000000000000000000, 0.000000000000000000, 0.000000000000000000 ) ) ;
#248427 = CARTESIAN_POINT ( 'NONE',  ( 18.59999999999999787, -11.74999999998883737, -58.35000000000000142 ) ) ;
#248426 = DIRECTION ( 'NONE',  ( 0.000000000000000000, 0.000000000000000000, 1.000000000000000000 ) ) ;
#248429 = ADVANCED_FACE ( 'NONE', ( #108715 ), #188249, .T. ) ;
#248428 = DIRECTION ( 'NONE',  ( 0.000000000000000000, 0.000000000000000000, -1.000000000000000000 ) ) ;
#248430 = CARTESIAN_POINT ( 'NONE',  ( -18.50000000000000000, 85.48068669529139640, -163.0819923157664562 ) ) ;
#248431 = CIRCLE ( 'NONE', #131731, 0.09999999999999939493 ) ;
#248432 = VECTOR ( 'NONE', #189749, 1000.000000000000000 ) ;
#248433 = CARTESIAN_POINT ( 'NONE',  ( -23.25000000000000000, 18.41524492703432614, -237.0006385043383546 ) ) ;
#248434 = AXIS2_PLACEMENT_3D ( 'NONE', #205288, #201445, #223564 ) ;
#248436 = CARTESIAN_POINT ( 'NONE',  ( -20.64999999999999858, 36.65892442174935439, -249.5511627012433848 ) ) ;
#248435 = AXIS2_PLACEMENT_3D ( 'NONE', #4978, #23321, #85789 ) ;
#248437 = ORIENTED_EDGE ( 'NONE', *, *, #203723, .F. ) ;
#248438 = VERTEX_POINT ( 'NONE', #210396 ) ;
#248439 = ADVANCED_FACE ( 'NONE', ( #150430 ), #28030, .F. ) ;
#248440 = DIRECTION ( 'NONE',  ( 0.8049926720990052686, 0.5796958986739292330, 0.1262515858416406456 ) ) ;
#248441 = ADVANCED_FACE ( 'NONE', ( #73471 ), #153016, .T. ) ;
#248442 = ORIENTED_EDGE ( 'NONE', *, *, #226704, .F. ) ;
#248443 = DIRECTION ( 'NONE',  ( 0.000000000000000000, -0.9126074666063660468, -0.4088369013363524762 ) ) ;
#248444 = VERTEX_POINT ( 'NONE', #100666 ) ;
#248445 = DIRECTION ( 'NONE',  ( 0.000000000000000000, 0.2617529984165033463, 0.9651348961777157509 ) ) ;
#248446 = DIRECTION ( 'NONE',  ( -0.000000000000000000, -6.982962677686266711E-15, 1.000000000000000000 ) ) ;
#248447 = VERTEX_POINT ( 'NONE', #1589 ) ;
#248448 = AXIS2_PLACEMENT_3D ( 'NONE', #192355, #133659, #232780 ) ;
#248449 = CARTESIAN_POINT ( 'NONE',  ( -22.10000000000000142, 3.461118860469513336, 28.84309995045515507 ) ) ;
#248450 = VECTOR ( 'NONE', #3760, 1000.000000000000000 ) ;
#248451 = TOROIDAL_SURFACE ( 'NONE', #160983, 11.65000000000000036, 0.1000000000000000056 ) ;
#248452 = ORIENTED_EDGE ( 'NONE', *, *, #47655, .F. ) ;
#248453 = EDGE_CURVE ( 'NONE', #111495, #241979, #71214, .T. ) ;
#248454 = VERTEX_POINT ( 'NONE', #139816 ) ;
#248455 = ADVANCED_FACE ( 'NONE', ( #176412 ), #137254, .T. ) ;
#248456 = VERTEX_POINT ( 'NONE', #38181 ) ;
#248457 = CARTESIAN_POINT ( 'NONE',  ( 20.94999999999999929, 36.65892442174935439, -249.5511627012433848 ) ) ;
#248458 = AXIS2_PLACEMENT_3D ( 'NONE', #172616, #229970, #252096 ) ;
#248459 = DIRECTION ( 'NONE',  ( -4.239556034732055511E-17, -0.8127272543710951647, 0.5826443254700256480 ) ) ;
#248460 = CARTESIAN_POINT ( 'NONE',  ( -21.05000000000000071, 77.16270174995034381, -162.0231074845243313 ) ) ;
#248461 = DIRECTION ( 'NONE',  ( 1.000000000000000000, 0.000000000000000000, 0.000000000000000000 ) ) ;
#248462 = EDGE_CURVE ( 'NONE', #11797, #220002, #5375, .T. ) ;
#248464 = CARTESIAN_POINT ( 'NONE',  ( 21.05000000000000071, 1.148907358139439339E-11, -201.0000000000015064 ) ) ;
#248463 = LINE ( 'NONE', #168967, #45618 ) ;
#248466 = VERTEX_POINT ( 'NONE', #61580 ) ;
#248465 = CARTESIAN_POINT ( 'NONE',  ( -23.25000000000000000, -11.74999999998884448, -33.50000000000000000 ) ) ;
#248468 = DIRECTION ( 'NONE',  ( 1.000000000000000000, 0.000000000000000000, 0.000000000000000000 ) ) ;
#248467 = DIRECTION ( 'NONE',  ( 1.000000000000000000, -0.000000000000000000, -0.000000000000000000 ) ) ;
#248469 = DIRECTION ( 'NONE',  ( -1.000000000000000000, 0.000000000000000000, 0.000000000000000000 ) ) ;
#248470 = ORIENTED_EDGE ( 'NONE', *, *, #243120, .T. ) ;
#248471 = CYLINDRICAL_SURFACE ( 'NONE', #247760, 0.09999999999999609201 ) ;
#248472 = CARTESIAN_POINT ( 'NONE',  ( -16.97683809663752186, 9.849999999999983658, -20.09763598180368405 ) ) ;
#248473 = VERTEX_POINT ( 'NONE', #238939 ) ;
#248474 = EDGE_CURVE ( 'NONE', #212171, #126961, #58703, .T. ) ;
#248475 = FACE_OUTER_BOUND ( 'NONE', #216510, .T. ) ;
#248476 = ADVANCED_FACE ( 'NONE', ( #216790 ), #81120, .F. ) ;
#248477 = AXIS2_PLACEMENT_3D ( 'NONE', #54042, #133580, #33240 ) ;
#248478 = DIRECTION ( 'NONE',  ( 0.000000000000000000, 0.000000000000000000, 1.000000000000000000 ) ) ;
#248479 = CARTESIAN_POINT ( 'NONE',  ( 13.76927104934457446, 66.54401276639910634, -88.01157631762656308 ) ) ;
#248480 = ORIENTED_EDGE ( 'NONE', *, *, #226217, .F. ) ;
#248481 = ORIENTED_EDGE ( 'NONE', *, *, #239800, .T. ) ;
#248482 = CARTESIAN_POINT ( 'NONE',  ( -20.94999999999999929, 77.16270174994990327, -95.02310748452430289 ) ) ;
#248483 = CARTESIAN_POINT ( 'NONE',  ( -18.50000000000000000, 10.29288807859935950, -172.9580020160122160 ) ) ;
#248484 = EDGE_CURVE ( 'NONE', #15834, #108480, #197233, .T. ) ;
#248485 = ORIENTED_EDGE ( 'NONE', *, *, #209698, .F. ) ;
#248486 = CIRCLE ( 'NONE', #73723, 0.09999999999999971412 ) ;
#248487 = DIRECTION ( 'NONE',  ( 0.000000000000000000, 0.7106264324241517993, -0.7035695228903270371 ) ) ;
#248488 = DIRECTION ( 'NONE',  ( -1.000000000000000000, 0.000000000000000000, 0.000000000000000000 ) ) ;
#248489 = CIRCLE ( 'NONE', #206797, 0.3999999999999975797 ) ;
#248491 = ADVANCED_FACE ( 'NONE', ( #307 ), #257152, .T. ) ;
#248490 = DIRECTION ( 'NONE',  ( -0.000000000000000000, 0.1350103645451859180, 0.9908441862701603542 ) ) ;
#248492 = CARTESIAN_POINT ( 'NONE',  ( 21.05000000000000071, 74.16465844978787914, -158.4679561919613775 ) ) ;
#248493 = AXIS2_PLACEMENT_3D ( 'NONE', #148671, #46970, #69143 ) ;
#248494 = CIRCLE ( 'NONE', #61037, 0.5000000000000009992 ) ;
#248495 = ORIENTED_EDGE ( 'NONE', *, *, #98773, .F. ) ;
#248496 = CARTESIAN_POINT ( 'NONE',  ( 20.94403535211772294, 10.30632246270531738, -39.00418367788957852 ) ) ;
#248498 = ORIENTED_EDGE ( 'NONE', *, *, #186682, .T. ) ;
#248497 = DIRECTION ( 'NONE',  ( 0.000000000000000000, -0.9126074666063545004, -0.4088369013363783999 ) ) ;
#248499 = DIRECTION ( 'NONE',  ( 1.000000000000000000, -7.304098846218135653E-16, -5.100424963727256530E-30 ) ) ;
#248500 = DIRECTION ( 'NONE',  ( 1.000000000000000000, 0.000000000000000000, 0.000000000000000000 ) ) ;
#248501 = EDGE_CURVE ( 'NONE', #222143, #110088, #73780, .T. ) ;
#248502 = DIRECTION ( 'NONE',  ( 0.000000000000000000, -1.000000000000000000, -6.982962677686265922E-15 ) ) ;
#248503 = CARTESIAN_POINT ( 'NONE',  ( 21.05000000000000071, 2.326828918379974323E-16, -31.59999999999999787 ) ) ;
#248504 = DIRECTION ( 'NONE',  ( -1.000000000000000000, -3.265361837132813093E-16, 0.000000000000000000 ) ) ;
#248505 = DIRECTION ( 'NONE',  ( 0.000000000000000000, 0.9908441862701605762, -0.1350103645451835310 ) ) ;
#248506 = ORIENTED_EDGE ( 'NONE', *, *, #226465, .F. ) ;
#248507 = CARTESIAN_POINT ( 'NONE',  ( 20.90000000000000213, 7.800000000000000711, -1.300000000000000044 ) ) ;
#248508 = CARTESIAN_POINT ( 'NONE',  ( 20.94999999999999574, 18.75483929237739744, -228.0790484105328630 ) ) ;
#248509 = CARTESIAN_POINT ( 'NONE',  ( 21.05000000000041638, 6.344359042055009112, -167.4851443651052989 ) ) ;
#248510 = AXIS2_PLACEMENT_3D ( 'NONE', #68263, #250737, #87794 ) ;
#248511 = DIRECTION ( 'NONE',  ( 0.000000000000000000, 0.000000000000000000, 1.000000000000000000 ) ) ;
#248512 = AXIS2_PLACEMENT_3D ( 'NONE', #43694, #201468, #240608 ) ;
#248513 = ORIENTED_EDGE ( 'NONE', *, *, #150686, .T. ) ;
#248514 = ORIENTED_EDGE ( 'NONE', *, *, #130312, .F. ) ;
#248515 = CARTESIAN_POINT ( 'NONE',  ( 20.94999999999999929, 18.47808476326695271, -239.8121846073901224 ) ) ;
#248516 = AXIS2_PLACEMENT_3D ( 'NONE', #104425, #183989, #84850 ) ;
#248517 = CARTESIAN_POINT ( 'NONE',  ( 23.15000000000000213, -11.48912529307605546, -30.50000000000000000 ) ) ;
#248518 = FACE_OUTER_BOUND ( 'NONE', #72356, .T. ) ;
#248519 = AXIS2_PLACEMENT_3D ( 'NONE', #177094, #217453, #216177 ) ;
#248520 = AXIS2_PLACEMENT_3D ( 'NONE', #163934, #49104, #223880 ) ;
#248521 = AXIS2_PLACEMENT_3D ( 'NONE', #89001, #51146, #168611 ) ;
#248522 = CARTESIAN_POINT ( 'NONE',  ( -16.27683809663751191, 9.349999999999976552, -12.55000000000000249 ) ) ;
#248523 = CYLINDRICAL_SURFACE ( 'NONE', #154817, 0.1000000000000000472 ) ;
#248524 = CARTESIAN_POINT ( 'NONE',  ( -14.00000000000000178, 66.15000000001258229, -186.7731074845244166 ) ) ;
#248525 = DIRECTION ( 'NONE',  ( 0.000000000000000000, -0.4999999999999088507, 0.8660254037844913322 ) ) ;
#248526 = B_SPLINE_CURVE_WITH_KNOTS ( 'NONE', 3,
 ( #83577, #181448, #163167, #84855, #6635, #24949, #2773, #161891 ),
 .UNSPECIFIED., .F., .F.,
 ( 4, 2, 2, 4 ),
 ( 0.000000000000000000, 0.0001094981963948483966, 0.0002189963927896967932, 0.0004379927855793893038 ),
 .UNSPECIFIED. ) ;
#248527 = CIRCLE ( 'NONE', #185989, 0.5000000000000004441 ) ;
#248528 = CIRCLE ( 'NONE', #78023, 12.87499999999999822 ) ;
#248529 = ORIENTED_EDGE ( 'NONE', *, *, #82133, .T. ) ;
#248531 = CARTESIAN_POINT ( 'NONE',  ( -18.52139480978223318, 85.48135884507851756, -62.49855091740519697 ) ) ;
#248530 = AXIS2_PLACEMENT_3D ( 'NONE', #119301, #239247, #103558 ) ;
#248532 = EDGE_LOOP ( 'NONE', ( #53581, #220297, #123714, #7546 ) ) ;
#248533 = DIRECTION ( 'NONE',  ( 0.000000000000000000, 0.9126074666063844765, 0.4088369013363113980 ) ) ;
#248534 = CARTESIAN_POINT ( 'NONE',  ( -23.15000000000000213, 26.47476584046484049, -241.8269156386531051 ) ) ;
#248535 = CARTESIAN_POINT ( 'NONE',  ( 23.14999999999999503, 66.47189219944506533, -213.6315278230738102 ) ) ;
#248536 = FACE_OUTER_BOUND ( 'NONE', #43317, .T. ) ;
#248537 = CARTESIAN_POINT ( 'NONE',  ( 21.11747605621531321, 22.06760108001729748, -231.7761073644578573 ) ) ;
#248538 = CARTESIAN_POINT ( 'NONE',  ( 18.31325810956326450, 85.53638847601891371, -62.65466727821948467 ) ) ;
#248539 = CARTESIAN_POINT ( 'NONE',  ( -23.15000000000000213, 85.00000000001222134, -146.4170766071767389 ) ) ;
#248540 = ORIENTED_EDGE ( 'NONE', *, *, #4283, .F. ) ;
#248541 = LINE ( 'NONE', #128603, #16587 ) ;
#248542 = LINE ( 'NONE', #191164, #25679 ) ;
#248543 = EDGE_CURVE ( 'NONE', #175608, #40840, #160715, .T. ) ;
#248544 = LINE ( 'NONE', #145584, #93961 ) ;
#248545 = CIRCLE ( 'NONE', #107072, 4.049999999999998046 ) ;
#248546 = LINE ( 'NONE', #49056, #147756 ) ;
#248547 = CARTESIAN_POINT ( 'NONE',  ( -22.49533356619862445, 11.65000000631534149, -167.4348774196772069 ) ) ;
#248548 = VERTEX_POINT ( 'NONE', #141127 ) ;
#248549 = CARTESIAN_POINT ( 'NONE',  ( -16.81744102076749314, 9.950000000011142376, -79.65000000000004832 ) ) ;
#248550 = DIRECTION ( 'NONE',  ( 0.000000000000000000, 0.000000000000000000, 1.000000000000000000 ) ) ;
#248551 = VERTEX_POINT ( 'NONE', #35635 ) ;
#248552 = ORIENTED_EDGE ( 'NONE', *, *, #126182, .F. ) ;
#248553 = CYLINDRICAL_SURFACE ( 'NONE', #234815, 0.09999999999999939493 ) ;
#248554 = DIRECTION ( 'NONE',  ( 0.000000000000000000, -1.000000000000000000, 0.000000000000000000 ) ) ;
#248555 = VECTOR ( 'NONE', #94369, 1000.000000000000000 ) ;
#248556 = EDGE_CURVE ( 'NONE', #200910, #37909, #117170, .T. ) ;
#248557 = CIRCLE ( 'NONE', #219342, 0.09999999999999911737 ) ;
#248558 = ORIENTED_EDGE ( 'NONE', *, *, #79163, .T. ) ;
#248560 = AXIS2_PLACEMENT_3D ( 'NONE', #224385, #221799, #223102 ) ;
#248559 = CARTESIAN_POINT ( 'NONE',  ( 20.94999999999999929, 77.83534155023671985, -158.4679561919613491 ) ) ;
#248561 = DIRECTION ( 'NONE',  ( -1.000000000000000000, 0.000000000000000000, 0.000000000000000000 ) ) ;
#248562 = CIRCLE ( 'NONE', #123683, 1.899999999999997469 ) ;
#248563 = ORIENTED_EDGE ( 'NONE', *, *, #250248, .F. ) ;
#248564 = AXIS2_PLACEMENT_3D ( 'NONE', #103065, #123951, #5243 ) ;
#248565 = DIRECTION ( 'NONE',  ( 1.000000000000000000, 0.000000000000000000, 0.000000000000000000 ) ) ;
#248566 = EDGE_CURVE ( 'NONE', #19374, #94366, #93208, .T. ) ;
#248567 = VERTEX_POINT ( 'NONE', #204921 ) ;
#248568 = EDGE_CURVE ( 'NONE', #169843, #23611, #225762, .T. ) ;
#248569 = DIRECTION ( 'NONE',  ( -1.000000000000000000, 1.836970198721029934E-16, 1.282749433769087757E-30 ) ) ;
#248570 = FACE_OUTER_BOUND ( 'NONE', #89638, .T. ) ;
#248573 = ORIENTED_EDGE ( 'NONE', *, *, #27927, .F. ) ;
#248572 = AXIS2_PLACEMENT_3D ( 'NONE', #246824, #128177, #29120 ) ;
#248571 = LINE ( 'NONE', #69960, #141591 ) ;
#248574 = CARTESIAN_POINT ( 'NONE',  ( -20.54999999999999716, 76.00000000001142553, -36.02310748452432421 ) ) ;
#248576 = UNCERTAINTY_MEASURE_WITH_UNIT (LENGTH_MEASURE( 1.000000000000000082E-05 ), #120538, 'distance_accuracy_value', 'NONE');
#248575 = CARTESIAN_POINT ( 'NONE',  ( -22.49231231312463208, 11.64998490368843953, -133.9389471123986368 ) ) ;
#248577 = EDGE_CURVE ( 'NONE', #72649, #27688, #47119, .T. ) ;
#248578 = CARTESIAN_POINT ( 'NONE',  ( 20.94999999999999574, -1.851028230129704522, -78.65391326942254580 ) ) ;
#248579 = AXIS2_PLACEMENT_3D ( 'NONE', #34316, #74741, #151703 ) ;
#248580 = CARTESIAN_POINT ( 'NONE',  ( -20.00857864376270001, 44.01574086017817677, -236.0100308471058099 ) ) ;
#248581 = CARTESIAN_POINT ( 'NONE',  ( -23.15000000000000213, 76.00000000001139711, -32.12310748452431852 ) ) ;
#248582 = CIRCLE ( 'NONE', #198519, 0.1000000000000028644 ) ;
#248583 = LINE ( 'NONE', #149510, #201192 ) ;
#248584 = CARTESIAN_POINT ( 'NONE',  ( 21.14999999999999858, 42.98415524044398950, -233.9519173640447889 ) ) ;
#248586 = EDGE_LOOP ( 'NONE', ( #150663, #248936, #28606, #126446 ) ) ;
#248585 = CARTESIAN_POINT ( 'NONE',  ( 21.00000000000000000, 9.750000000011153745, -179.7499999999999716 ) ) ;
#248587 = ORIENTED_EDGE ( 'NONE', *, *, #2905, .F. ) ;
#248589 = CARTESIAN_POINT ( 'NONE',  ( -15.75000000000000355, 9.350000000011140955, -83.75000000000004263 ) ) ;
#248588 = CARTESIAN_POINT ( 'NONE',  ( 21.05000000000000071, 1.115600667400684642E-11, -200.9999999999999432 ) ) ;
#248590 = EDGE_CURVE ( 'NONE', #71080, #128626, #125411, .T. ) ;
#248592 = ORIENTED_EDGE ( 'NONE', *, *, #131018, .T. ) ;
#248591 = CARTESIAN_POINT ( 'NONE',  ( 21.13736287352038445, 10.55427114109327036, -211.6479253478778446 ) ) ;
#248593 = VERTEX_POINT ( 'NONE', #146233 ) ;
#248594 = CARTESIAN_POINT ( 'NONE',  ( -16.77683809663752257, 66.05416425680839154, -182.6870565036286393 ) ) ;
#248595 = CYLINDRICAL_SURFACE ( 'NONE', #118041, 0.1000000000000106914 ) ;
#248596 = AXIS2_PLACEMENT_3D ( 'NONE', #129515, #190802, #227320 ) ;
#248597 = EDGE_CURVE ( 'NONE', #188779, #171037, #229984, .T. ) ;
#248598 = CARTESIAN_POINT ( 'NONE',  ( -21.05000000000000071, 77.16270174994990327, -94.92310748452430857 ) ) ;
#248599 = DIRECTION ( 'NONE',  ( 1.836970198721029441E-16, -0.4721928772777346239, -0.8814952561688430555 ) ) ;
#248600 = B_SPLINE_CURVE_WITH_KNOTS ( 'NONE', 3,
 ( #210700, #206852, #187305, #9934, #72495, #32090, #67338, #188567, #33389, #86875, #152038, #228991, #30811, #212003, #71210, #8651, #88151, #111607, #12527 ),
 .UNSPECIFIED., .F., .F.,
 ( 4, 3, 3, 3, 3, 3, 4 ),
 ( 0.0001624081864585825768, 0.0001685232196531684422, 0.0001764526673566856301, 0.0001916878551483259131, 0.0002009890782182699649, 0.0002238845907555212563, 0.0002283406619926391719 ),
 .UNSPECIFIED. ) ;
#248601 = LINE ( 'NONE', #109080, #122059 ) ;
#248602 = EDGE_CURVE ( 'NONE', #133625, #144953, #104519, .T. ) ;
#248603 = LINE ( 'NONE', #229051, #39561 ) ;
#248604 = ORIENTED_EDGE ( 'NONE', *, *, #8307, .T. ) ;
#248605 = ORIENTED_EDGE ( 'NONE', *, *, #120550, .F. ) ;
#248606 = DIRECTION ( 'NONE',  ( 0.000000000000000000, -0.9876197685951252359, -0.1568667991644863424 ) ) ;
#248607 = AXIS2_PLACEMENT_3D ( 'NONE', #127906, #49641, #30106 ) ;
#248608 = AXIS2_PLACEMENT_3D ( 'NONE', #8253, #245576, #68215 ) ;
#248609 = EDGE_LOOP ( 'NONE', ( #197903, #206862 ) ) ;
#248610 = CIRCLE ( 'NONE', #2900, 4.099999999999999645 ) ;
#248612 = DIRECTION ( 'NONE',  ( 0.7071067811865489050, -0.6453109281988438362, -0.2890913453342124906 ) ) ;
#248611 = AXIS2_PLACEMENT_3D ( 'NONE', #74972, #241420, #95770 ) ;
#248613 = ORIENTED_EDGE ( 'NONE', *, *, #23072, .F. ) ;
#248614 = CARTESIAN_POINT ( 'NONE',  ( 23.15000000000000213, 87.75000000001216449, -139.6231074845242688 ) ) ;
#248615 = CARTESIAN_POINT ( 'NONE',  ( 20.85000000000000142, -11.74999999998883560, -97.50000000000004263 ) ) ;
#248616 = FACE_OUTER_BOUND ( 'NONE', #112078, .T. ) ;
#248617 = ORIENTED_EDGE ( 'NONE', *, *, #15609, .F. ) ;
#248618 = DIRECTION ( 'NONE',  ( 0.000000000000000000, -0.1495327102803283015, 0.9887567792719397231 ) ) ;
#248619 = ORIENTED_EDGE ( 'NONE', *, *, #170955, .T. ) ;
#248620 = DIRECTION ( 'NONE',  ( 1.000000000000000000, 0.000000000000000000, 0.000000000000000000 ) ) ;
#248621 = CARTESIAN_POINT ( 'NONE',  ( -16.88005004766534967, 9.950100503332199864, -87.85033611194879200 ) ) ;
#248622 = CARTESIAN_POINT ( 'NONE',  ( 21.05000000000000071, 8.815201804578325806, -108.9205374966854123 ) ) ;
#248623 = VECTOR ( 'NONE', #159357, 1000.000000000000000 ) ;
#248624 = ORIENTED_EDGE ( 'NONE', *, *, #10623, .T. ) ;
#248625 = TOROIDAL_SURFACE ( 'NONE', #90408, 7.791421356237316687, 0.1000000000000000056 ) ;
#248627 = DIRECTION ( 'NONE',  ( 0.000000000000000000, 0.000000000000000000, 1.000000000000000000 ) ) ;
#248626 = AXIS2_PLACEMENT_3D ( 'NONE', #207279, #9054, #226814 ) ;
#248628 = ORIENTED_EDGE ( 'NONE', *, *, #238942, .F. ) ;
#248631 = ORIENTED_EDGE ( 'NONE', *, *, #154483, .F. ) ;
#248630 = CARTESIAN_POINT ( 'NONE',  ( 18.53317502108576420, 46.43483777265582546, -243.0774829958280918 ) ) ;
#248629 = DIRECTION ( 'NONE',  ( 1.000000000000000000, -0.000000000000000000, -0.000000000000000000 ) ) ;
#248632 = ORIENTED_EDGE ( 'NONE', *, *, #172144, .T. ) ;
#248633 = ADVANCED_FACE ( 'NONE', ( #124133 ), #105807, .T. ) ;
#248634 = DIRECTION ( 'NONE',  ( 0.000000000000000000, -0.8814952561688444987, 0.4721928772777320149 ) ) ;
#248635 = AXIS2_PLACEMENT_3D ( 'NONE', #229034, #246025, #129908 ) ;
#248636 = ORIENTED_EDGE ( 'NONE', *, *, #86878, .F. ) ;
#248637 = ADVANCED_FACE ( 'NONE', ( #203656 ), #118360, .T. ) ;
#248638 = CARTESIAN_POINT ( 'NONE',  ( 21.14999999999999858, 76.00000000001213607, -136.5231074845242745 ) ) ;
#248639 = EDGE_CURVE ( 'NONE', #48194, #442, #36370, .T. ) ;
#248640 = DIRECTION ( 'NONE',  ( 0.000000000000000000, 0.000000000000000000, -1.000000000000000000 ) ) ;
#248641 = EDGE_CURVE ( 'NONE', #2421, #206022, #163351, .T. ) ;
#248642 = CARTESIAN_POINT ( 'NONE',  ( -17.73285935861977691, 53.44571795644451129, -230.1331290949856054 ) ) ;
#248644 = ORIENTED_EDGE ( 'NONE', *, *, #253562, .T. ) ;
#248643 = EDGE_CURVE ( 'NONE', #137151, #217322, #5091, .T. ) ;
#248645 = CARTESIAN_POINT ( 'NONE',  ( -21.05000000000000071, 1.835341550235567887, -179.1551512925629197 ) ) ;
#248646 = CARTESIAN_POINT ( 'NONE',  ( -16.92563707711778065, 9.968990694407935393, -188.3807582995239329 ) ) ;
#248647 = CARTESIAN_POINT ( 'NONE',  ( 18.49999999999999289, 10.29270135741298731, -139.4573618871519614 ) ) ;
#248648 = EDGE_CURVE ( 'NONE', #211413, #212703, #70549, .T. ) ;
#248649 = VECTOR ( 'NONE', #57880, 1000.000000000000000 ) ;
#248650 = VERTEX_POINT ( 'NONE', #235720 ) ;
#248651 = CARTESIAN_POINT ( 'NONE',  ( -22.47071067811865319, 0.09909245470260570621, 7.720074744498060859 ) ) ;
#248653 = EDGE_CURVE ( 'NONE', #51770, #44689, #38443, .T. ) ;
#248652 = VERTEX_POINT ( 'NONE', #12857 ) ;
#248654 = CARTESIAN_POINT ( 'NONE',  ( -20.54999999999999716, 48.91146289617405785, -253.9240286733484595 ) ) ;
#248655 = VERTEX_POINT ( 'NONE', #252710 ) ;
#248656 = LINE ( 'NONE', #184823, #251406 ) ;
#248657 = CARTESIAN_POINT ( 'NONE',  ( -22.50875500270927532, 76.10085791378705267, -181.7726746119222696 ) ) ;
#248658 = ADVANCED_FACE ( 'NONE', ( #57063 ), #230610, .F. ) ;
#248660 = ORIENTED_EDGE ( 'NONE', *, *, #52032, .T. ) ;
#248659 = DIRECTION ( 'NONE',  ( -0.000000000000000000, 0.9770955615653313941, 0.2128009952263603954 ) ) ;
#248661 = DIRECTION ( 'NONE',  ( -0.7071067811865474617, 0.7071067811865474617, 5.142139384388980375E-15 ) ) ;
#248662 = AXIS2_PLACEMENT_3D ( 'NONE', #141690, #119592, #236952 ) ;
#248663 = CARTESIAN_POINT ( 'NONE',  ( -12.60829076262180592, 62.83279349218706500, -216.2014764372737829 ) ) ;
#248664 = EDGE_CURVE ( 'NONE', #161112, #220739, #173237, .T. ) ;
#248665 = CARTESIAN_POINT ( 'NONE',  ( -16.82055514392378726, 9.950000000011137047, -113.1767980745418356 ) ) ;
#248666 = ORIENTED_EDGE ( 'NONE', *, *, #189465, .F. ) ;
#248667 = VECTOR ( 'NONE', #115141, 1000.000000000000000 ) ;
#248668 = CARTESIAN_POINT ( 'NONE',  ( -23.15000000000000213, 84.66355140188167638, -179.5472086025916099 ) ) ;
#248669 = LINE ( 'NONE', #129985, #231471 ) ;
#248671 = ORIENTED_EDGE ( 'NONE', *, *, #171624, .T. ) ;
#248670 = EDGE_CURVE ( 'NONE', #137714, #204820, #136611, .T. ) ;
#248673 = ADVANCED_FACE ( 'NONE', ( #74126 ), #17955, .T. ) ;
#248672 = DIRECTION ( 'NONE',  ( 0.000000000000000000, 0.000000000000000000, -1.000000000000000000 ) ) ;
#248674 = AXIS2_PLACEMENT_3D ( 'NONE', #15137, #232916, #54238 ) ;
#248675 = AXIS2_PLACEMENT_3D ( 'NONE', #64306, #218214, #198675 ) ;
#248676 = VERTEX_POINT ( 'NONE', #231903 ) ;
#248677 = PRODUCT_DEFINITION_FORMATION_WITH_SPECIFIED_SOURCE ( 'ANY', '', #228439, .NOT_KNOWN. ) ;
#248678 = EDGE_CURVE ( 'NONE', #2285, #69236, #233196, .T. ) ;
#248679 = CARTESIAN_POINT ( 'NONE',  ( 15.69410316191958898, 9.356746017089403011, -117.7033597213642082 ) ) ;
#248681 = CARTESIAN_POINT ( 'NONE',  ( -20.94999999999999929, 1.115649653272650466E-11, -138.0000000000000284 ) ) ;
#248680 = AXIS2_PLACEMENT_3D ( 'NONE', #200605, #138044, #100187 ) ;
#248682 = AXIS2_PLACEMENT_3D ( 'NONE', #852, #161257, #219929 ) ;
#248683 = ADVANCED_FACE ( 'NONE', ( #177068 ), #112893, .F. ) ;
#248684 = EDGE_CURVE ( 'NONE', #206261, #68241, #71402, .T. ) ;
#248687 = EDGE_LOOP ( 'NONE', ( #34387, #185281, #211229, #115493 ) ) ;
#248686 = ORIENTED_EDGE ( 'NONE', *, *, #176494, .T. ) ;
#248685 = DIRECTION ( 'NONE',  ( -0.000000000000000000, 1.000000000000000000, -0.000000000000000000 ) ) ;
#248688 = FACE_OUTER_BOUND ( 'NONE', #246841, .T. ) ;
#248689 = CARTESIAN_POINT ( 'NONE',  ( -18.59999999999999787, 68.48451787451661232, -224.2224406095231757 ) ) ;
#248690 = CARTESIAN_POINT ( 'NONE',  ( -23.15000000000000213, 84.59626168225457832, -60.07297996737398194 ) ) ;
#248692 = CARTESIAN_POINT ( 'NONE',  ( -15.39126916658603683, 66.61042836546512547, -51.70546677215521925 ) ) ;
#248691 = CARTESIAN_POINT ( 'NONE',  ( -21.05000000000000071, 28.42524210734032053, -258.3567845160494585 ) ) ;
#248693 = CARTESIAN_POINT ( 'NONE',  ( -18.59999999999999787, 22.38308386859736032, -231.4104522272575082 ) ) ;
#248694 = LINE ( 'NONE', #114311, #235885 ) ;
#248695 = VECTOR ( 'NONE', #119951, 1000.000000000000000 ) ;
#248696 = DIRECTION ( 'NONE',  ( 0.000000000000000000, 1.000000000000000000, 0.000000000000000000 ) ) ;
#248697 = DIRECTION ( 'NONE',  ( 0.000000000000000000, -0.4721928772777346239, -0.8814952561688430555 ) ) ;
#248698 = AXIS2_PLACEMENT_3D ( 'NONE', #166587, #47875, #136375 ) ;
#248699 = VERTEX_POINT ( 'NONE', #131494 ) ;
#248700 = VERTEX_POINT ( 'NONE', #134051 ) ;
#248702 = CYLINDRICAL_SURFACE ( 'NONE', #37672, 7.899999999999994138 ) ;
#248701 = AXIS2_PLACEMENT_3D ( 'NONE', #92514, #49552, #74283 ) ;
#248704 = ORIENTED_EDGE ( 'NONE', *, *, #106565, .F. ) ;
#248703 = DIRECTION ( 'NONE',  ( 1.000000000000000000, 0.000000000000000000, 0.000000000000000000 ) ) ;
#248705 = AXIS2_PLACEMENT_3D ( 'NONE', #22521, #60328, #40810 ) ;
#248706 = ORIENTED_EDGE ( 'NONE', *, *, #45667, .F. ) ;
#248707 = DIRECTION ( 'NONE',  ( 1.000000000000000000, -2.849773892568378313E-16, 7.728835255496647986E-17 ) ) ;
#248708 = VERTEX_POINT ( 'NONE', #211042 ) ;
#248709 = CARTESIAN_POINT ( 'NONE',  ( -18.59999999999999787, 70.65875701002109111, -213.3297576910124178 ) ) ;
#248710 = AXIS2_PLACEMENT_3D ( 'NONE', #237407, #176170, #64 ) ;
#248711 = ORIENTED_EDGE ( 'NONE', *, *, #74303, .T. ) ;
#248712 = CARTESIAN_POINT ( 'NONE',  ( -16.89081410710458542, 66.04868147016512125, -149.1687015646880639 ) ) ;
#248713 = CARTESIAN_POINT ( 'NONE',  ( 21.05000000000000071, 6.650000000011155876, -179.6499999999999773 ) ) ;
#248716 = ORIENTED_EDGE ( 'NONE', *, *, #18856, .F. ) ;
#248715 = VERTEX_POINT ( 'NONE', #32435 ) ;
#248714 = VECTOR ( 'NONE', #96670, 1000.000000000000000 ) ;
#248717 = EDGE_LOOP ( 'NONE', ( #194328, #151250, #75525, #91596 ) ) ;
#248719 = VECTOR ( 'NONE', #218025, 1000.000000000000000 ) ;
#248718 = CARTESIAN_POINT ( 'NONE',  ( -23.25000000000000000, 74.86109765932731364, -233.8067614591677454 ) ) ;
#248720 = AXIS2_PLACEMENT_3D ( 'NONE', #247513, #68893, #188816 ) ;
#248721 = ORIENTED_EDGE ( 'NONE', *, *, #98698, .T. ) ;
#248722 = VERTEX_POINT ( 'NONE', #174538 ) ;
#248723 = DIRECTION ( 'NONE',  ( 1.000000000000000000, 0.000000000000000000, 0.000000000000000000 ) ) ;
#248724 = CARTESIAN_POINT ( 'NONE',  ( 21.06490991615909536, 43.41139117757177246, -234.7742192443139118 ) ) ;
#248725 = CARTESIAN_POINT ( 'NONE',  ( 23.15000000000000213, 62.12679871018153932, -248.6611778639222337 ) ) ;
#248727 = ORIENTED_EDGE ( 'NONE', *, *, #184534, .F. ) ;
#248726 = CARTESIAN_POINT ( 'NONE',  ( -21.44999999999999929, 53.04688186230822566, -234.1557136682916394 ) ) ;
#248728 = CARTESIAN_POINT ( 'NONE',  ( 18.59999999999999076, 69.55000000001150795, -48.37310748452436826 ) ) ;
#248729 = FACE_OUTER_BOUND ( 'NONE', #98091, .T. ) ;
#248731 = EDGE_LOOP ( 'NONE', ( #212149, #166879, #41261, #228061 ) ) ;
#248730 = CARTESIAN_POINT ( 'NONE',  ( 21.14999999999999503, 1.115600667400684642E-11, -94.25000000000002842 ) ) ;
#248732 = CARTESIAN_POINT ( 'NONE',  ( -21.05000000000000071, 1.115600667400684642E-11, -67.00000000000004263 ) ) ;
#248733 = VERTEX_POINT ( 'NONE', #213589 ) ;
#248734 = DIRECTION ( 'NONE',  ( 0.000000000000000000, 0.000000000000000000, 1.000000000000000000 ) ) ;
#248735 = EDGE_LOOP ( 'NONE', ( #87256, #119161, #222669, #119134, #196501 ) ) ;
#248736 = CIRCLE ( 'NONE', #236805, 0.1000000000000002554 ) ;
#248737 = FACE_OUTER_BOUND ( 'NONE', #231656, .T. ) ;
#248739 = ADVANCED_FACE ( 'NONE', ( #15420 ), #253999, .T. ) ;
#248738 = DIRECTION ( 'NONE',  ( 1.000000000000000000, 0.000000000000000000, 0.000000000000000000 ) ) ;
#248740 = AXIS2_PLACEMENT_3D ( 'NONE', #208676, #168292, #70469 ) ;
#248741 = EDGE_LOOP ( 'NONE', ( #46108, #157516, #39722, #124551 ) ) ;
#248743 = LINE ( 'NONE', #130056, #199591 ) ;
#248742 = CYLINDRICAL_SURFACE ( 'NONE', #136391, 0.09999999999998898659 ) ;
#248744 = EDGE_CURVE ( 'NONE', #74878, #83103, #171378, .T. ) ;
#248745 = DIRECTION ( 'NONE',  ( 0.000000000000000000, 0.9915357197604973694, -0.1298341882519105928 ) ) ;
#248746 = CYLINDRICAL_SURFACE ( 'NONE', #22411, 0.1000000000000028644 ) ;
#248747 = DIRECTION ( 'NONE',  ( 0.000000000000000000, 0.000000000000000000, 1.000000000000000000 ) ) ;
#248748 = ORIENTED_EDGE ( 'NONE', *, *, #3682, .F. ) ;
#248749 = EDGE_LOOP ( 'NONE', ( #118581, #218040, #145319, #104940, #179710, #20484, #257886, #67092, #116734, #184225, #210338, #102718, #178176, #123647, #98704, #255594 ) ) ;
#248750 = AXIS2_PLACEMENT_3D ( 'NONE', #229131, #203142, #105288 ) ;
#248751 = EDGE_CURVE ( 'NONE', #180828, #148712, #104658, .T. ) ;
#248752 = FACE_OUTER_BOUND ( 'NONE', #231731, .T. ) ;
#248754 = EDGE_CURVE ( 'NONE', #39320, #58384, #113077, .T. ) ;
#248753 = CARTESIAN_POINT ( 'NONE',  ( 23.24999999999999645, 7.128833340094563376, -233.7327013124401276 ) ) ;
#248755 = ORIENTED_EDGE ( 'NONE', *, *, #250454, .F. ) ;
#248756 = DIRECTION ( 'NONE',  ( 0.000000000000000000, 0.9126074666063770380, 0.4088369013363281068 ) ) ;
#248757 = EDGE_LOOP ( 'NONE', ( #67700, #169013, #28724, #238919 ) ) ;
#248758 = DIRECTION ( 'NONE',  ( 0.000000000000000000, 7.026728003956683390E-15, -1.000000000000000000 ) ) ;
#248759 = DIRECTION ( 'NONE',  ( -1.000000000000000000, 0.000000000000000000, 0.000000000000000000 ) ) ;
#248760 = CIRCLE ( 'NONE', #148812, 0.1000000000000013933 ) ;
#248761 = DIRECTION ( 'NONE',  ( -1.000000000000000000, 0.000000000000000000, 0.000000000000000000 ) ) ;
#248762 = VECTOR ( 'NONE', #164662, 1000.000000000000000 ) ;
#248763 = TOROIDAL_SURFACE ( 'NONE', #136289, 11.90000000000000391, 0.1000000000000000056 ) ;
#248764 = AXIS2_PLACEMENT_3D ( 'NONE', #68542, #201622, #205463 ) ;
#248765 = EDGE_LOOP ( 'NONE', ( #173028, #67983, #243418 ) ) ;
#248766 = DIRECTION ( 'NONE',  ( -1.000000000000000000, -0.000000000000000000, -0.000000000000000000 ) ) ;
#248767 = FILL_AREA_STYLE_COLOUR ( '', #127143 ) ;
#248768 = VECTOR ( 'NONE', #156372, 1000.000000000000000 ) ;
#248769 = B_SPLINE_CURVE_WITH_KNOTS ( 'NONE', 3,
 ( #175483, #51628, #251124, #131191, #253701, #15115, #115479, #195047, #32126, #174222, #73825, #214576, #153378, #94631, #111636, #232896, #11259, #55471, #133760 ),
 .UNSPECIFIED., .F., .F.,
 ( 4, 3, 3, 3, 3, 3, 4 ),
 ( -2.000416914646550933E-06, 0.000000000000000000, 4.714008503745887181E-05, 9.979203887778609111E-05, 0.0001372215519229623361, 0.0001635031576221138302, 0.0001900083748504290723 ),
 .UNSPECIFIED. ) ;
#248770 = ORIENTED_EDGE ( 'NONE', *, *, #202421, .F. ) ;
#248771 = EDGE_LOOP ( 'NONE', ( #156650, #52634, #87508, #64812 ) ) ;
#248772 = EDGE_CURVE ( 'NONE', #111426, #237722, #100394, .T. ) ;
#248773 = ORIENTED_EDGE ( 'NONE', *, *, #63166, .F. ) ;
#248774 = DIRECTION ( 'NONE',  ( 0.000000000000000000, 1.000000000000000000, 6.982962677686266711E-15 ) ) ;
#248775 = CARTESIAN_POINT ( 'NONE',  ( -18.59999999999999787, 1.115600667400684642E-11, -33.50000000000000000 ) ) ;
#248776 = FACE_OUTER_BOUND ( 'NONE', #116693, .T. ) ;
#248777 = CARTESIAN_POINT ( 'NONE',  ( -23.15000000000000213, 28.50120599808395028, -258.2149742250584268 ) ) ;
#248778 = CARTESIAN_POINT ( 'NONE',  ( 23.14999999999999503, 69.55000000001228955, -157.6731074845243938 ) ) ;
#248780 = CARTESIAN_POINT ( 'NONE',  ( 21.13920837816993270, 8.783247050119912913, -12.25000000000000000 ) ) ;
#248779 = CARTESIAN_POINT ( 'NONE',  ( 21.13435531349819740, 1.115515320630192923E-11, -161.0062789364080515 ) ) ;
#248782 = VERTEX_POINT ( 'NONE', #42657 ) ;
#248781 = CARTESIAN_POINT ( 'NONE',  ( -21.05000000000000071, 70.47363787294415260, -228.3418745167492432 ) ) ;
#248783 = DIRECTION ( 'NONE',  ( -0.000000000000000000, 0.1332476588733589040, 0.9910827722268049644 ) ) ;
#248784 = ORIENTED_EDGE ( 'NONE', *, *, #170682, .T. ) ;
#248785 = CYLINDRICAL_SURFACE ( 'NONE', #53038, 0.1000000000000124678 ) ;
#248786 = ORIENTED_EDGE ( 'NONE', *, *, #80032, .T. ) ;
#248787 = ORIENTED_EDGE ( 'NONE', *, *, #185934, .T. ) ;
#248788 = DIRECTION ( 'NONE',  ( 1.000000000000000000, -0.000000000000000000, -0.000000000000000000 ) ) ;
#248789 = VECTOR ( 'NONE', #8646, 1000.000000000000114 ) ;
#248790 = CARTESIAN_POINT ( 'NONE',  ( -20.94999999999999929, 39.30548607490320734, -248.3655356873701123 ) ) ;
#248791 = CARTESIAN_POINT ( 'NONE',  ( -18.50000000000000000, 9.783112580922244561, -245.9316685519929422 ) ) ;
#248792 = EDGE_CURVE ( 'NONE', #254598, #19089, #54618, .T. ) ;
#248793 = CARTESIAN_POINT ( 'NONE',  ( 21.05000000000000071, -9.399999999988846611, -143.8939691226524644 ) ) ;
#248794 = EDGE_CURVE ( 'NONE', #224021, #225545, #200382, .T. ) ;
#248795 = TOROIDAL_SURFACE ( 'NONE', #23783, 0.2000000000000000111, 0.1000000000000000056 ) ;
#248796 = DIRECTION ( 'NONE',  ( 0.000000000000000000, -1.000000000000000000, 0.000000000000000000 ) ) ;
#248797 = EDGE_LOOP ( 'NONE', ( #33738, #234458, #55639, #59332 ) ) ;
#248798 = ORIENTED_EDGE ( 'NONE', *, *, #214867, .F. ) ;
#248799 = CARTESIAN_POINT ( 'NONE',  ( 18.39999999999999503, 64.25000000001202238, -115.6731074845243938 ) ) ;
#248800 = ORIENTED_EDGE ( 'NONE', *, *, #225668, .T. ) ;
#248801 = CARTESIAN_POINT ( 'NONE',  ( -20.54999999999999716, -8.999999999988844479, -57.10603087734755690 ) ) ;
#248802 = DIRECTION ( 'NONE',  ( 1.000000000000000000, 0.000000000000000000, 0.000000000000000000 ) ) ;
#248803 = EDGE_LOOP ( 'NONE', ( #1410, #109027, #185459, #208617 ) ) ;
#248804 = DIRECTION ( 'NONE',  ( 1.000000000000000000, 0.000000000000000000, 0.000000000000000000 ) ) ;
#248805 = CARTESIAN_POINT ( 'NONE',  ( 22.47071067811865319, -1.546016791165055304, -193.4356622592196970 ) ) ;
#248806 = DIRECTION ( 'NONE',  ( -0.000000000000000000, 1.000000000000000000, -0.000000000000000000 ) ) ;
#248808 = EDGE_CURVE ( 'NONE', #174607, #94890, #233713, .T. ) ;
#248807 = DIRECTION ( 'NONE',  ( -1.000000000000000000, -0.000000000000000000, -0.000000000000000000 ) ) ;
#248809 = VERTEX_POINT ( 'NONE', #102600 ) ;
#248810 = DIRECTION ( 'NONE',  ( -0.000000000000000000, 0.000000000000000000, -1.000000000000000000 ) ) ;
#248811 = CARTESIAN_POINT ( 'NONE',  ( -20.64999999999999858, 46.15118611352045974, -240.5321844900040844 ) ) ;
#248812 = EDGE_CURVE ( 'NONE', #78569, #200649, #246170, .T. ) ;
#248813 = CARTESIAN_POINT ( 'NONE',  ( 18.79999999999999716, 7.800000000000000711, -1.212568896937008089 ) ) ;
#248814 = CARTESIAN_POINT ( 'NONE',  ( 23.14999999999999503, 64.25000000001179501, -81.77310748452438816 ) ) ;
#248815 = ADVANCED_FACE ( 'NONE', ( #157517 ), #225291, .T. ) ;
#248816 = AXIS2_PLACEMENT_3D ( 'NONE', #247543, #225388, #46757 ) ;
#248818 = VECTOR ( 'NONE', #156142, 1000.000000000000000 ) ;
#248817 = CARTESIAN_POINT ( 'NONE',  ( -20.95613430942416144, 57.68582240677151418, -226.1614418145203445 ) ) ;
#248819 = AXIS2_PLACEMENT_3D ( 'NONE', #235956, #155186, #211274 ) ;
#248820 = EDGE_LOOP ( 'NONE', ( #127342, #222746, #148071 ) ) ;
#248821 = CARTESIAN_POINT ( 'NONE',  ( -16.92209698673622853, 66.05000000001231797, -157.3124719174703898 ) ) ;
#248822 = VERTEX_POINT ( 'NONE', #101293 ) ;
#248823 = CARTESIAN_POINT ( 'NONE',  ( 15.74999999999999645, 66.65000000001228386, -153.2731074845244166 ) ) ;
#248824 = EDGE_CURVE ( 'NONE', #40449, #155056, #221279, .T. ) ;
#248825 = DIRECTION ( 'NONE',  ( -2.812466655313718795E-14, -0.07893460099012014619, 0.9968797965484758050 ) ) ;
#248826 = CARTESIAN_POINT ( 'NONE',  ( 22.39999999999999503, 64.25000000001237765, -169.9231074845244507 ) ) ;
#248827 = CARTESIAN_POINT ( 'NONE',  ( -18.40000000000000213, 11.47316190337364183, -57.75000000000000711 ) ) ;
#248828 = CARTESIAN_POINT ( 'NONE',  ( -23.15000000000000213, 76.00000000001213607, -136.5231074845243313 ) ) ;
#248829 = EDGE_LOOP ( 'NONE', ( #90543, #151837, #171252, #4841 ) ) ;
#248830 = LINE ( 'NONE', #110586, #196781 ) ;
#248831 = EDGE_CURVE ( 'NONE', #1714, #167528, #182281, .T. ) ;
#248832 = DIRECTION ( 'NONE',  ( 1.000000000000000000, -3.265361837132813093E-16, -2.280189983783949500E-30 ) ) ;
#248833 = DIRECTION ( 'NONE',  ( 1.000000000000000000, -0.000000000000000000, 0.000000000000000000 ) ) ;
#248834 = DIRECTION ( 'NONE',  ( 0.000000000000000000, 6.982962677686266711E-15, -1.000000000000000000 ) ) ;
#248835 = CIRCLE ( 'NONE', #111443, 0.1000000000000028644 ) ;
#248836 = FACE_OUTER_BOUND ( 'NONE', #237352, .T. ) ;
#248837 = VECTOR ( 'NONE', #63205, 999.9999999999998863 ) ;
#248838 = VERTEX_POINT ( 'NONE', #19249 ) ;
#248839 = EDGE_LOOP ( 'NONE', ( #257365, #6332, #33877, #204710, #125092, #10825 ) ) ;
#248840 = DIRECTION ( 'NONE',  ( -2.168404344971008868E-16, 0.000000000000000000, -1.000000000000000000 ) ) ;
#248841 = CARTESIAN_POINT ( 'NONE',  ( -18.59999999999999787, 76.00000000001195133, -103.0231074845243171 ) ) ;
#248842 = DIRECTION ( 'NONE',  ( 0.000000000000000000, -1.000000000000000000, 0.000000000000000000 ) ) ;
#248843 = VERTEX_POINT ( 'NONE', #100038 ) ;
#248844 = CARTESIAN_POINT ( 'NONE',  ( 23.15000000000000213, 82.57900542960499024, -215.5587758314583766 ) ) ;
#248845 = ORIENTED_EDGE ( 'NONE', *, *, #196733, .T. ) ;
#248846 = DIRECTION ( 'NONE',  ( 0.000000000000000000, 0.000000000000000000, -1.000000000000000000 ) ) ;
#248847 = VECTOR ( 'NONE', #17212, 1000.000000000000114 ) ;
#248848 = CIRCLE ( 'NONE', #19909, 0.09999999999999939493 ) ;
#248849 = ORIENTED_EDGE ( 'NONE', *, *, #153227, .F. ) ;
#248850 = EDGE_LOOP ( 'NONE', ( #73924, #24544, #126229, #1997 ) ) ;
#248851 = VERTEX_POINT ( 'NONE', #182186 ) ;
#248852 = FACE_OUTER_BOUND ( 'NONE', #243085, .T. ) ;
#248853 = DIRECTION ( 'NONE',  ( 0.000000000000000000, 0.000000000000000000, 1.000000000000000000 ) ) ;
#248854 = AXIS2_PLACEMENT_3D ( 'NONE', #234067, #153296, #95825 ) ;
#248855 = DIRECTION ( 'NONE',  ( -1.000000000000000000, -8.674042436075353235E-17, -1.619280515896125144E-16 ) ) ;
#248856 = CARTESIAN_POINT ( 'NONE',  ( 18.41416235934318024, -9.499999999988844479, -140.6001893912220737 ) ) ;
#248857 = CARTESIAN_POINT ( 'NONE',  ( 21.05000000000000071, 74.83729825007360148, -61.62310748452433273 ) ) ;
#248858 = CARTESIAN_POINT ( 'NONE',  ( -23.15000000000000213, 56.06656052939784018, -228.0911609752645290 ) ) ;
#248859 = CARTESIAN_POINT ( 'NONE',  ( -16.94180778212363236, 9.992443055732147528, -12.60418357053324634 ) ) ;
#248862 = LINE ( 'NONE', #89767, #28914 ) ;
#248861 = VECTOR ( 'NONE', #83670, 1000.000000000000000 ) ;
#248860 = CARTESIAN_POINT ( 'NONE',  ( -18.50000000000000000, 74.65925378207852248, -146.7959699899454904 ) ) ;
#248863 = CARTESIAN_POINT ( 'NONE',  ( -21.05000000000000071, 1.162701749949165642, -108.6000000000000227 ) ) ;
#248864 = DIRECTION ( 'NONE',  ( 0.000000000000000000, 6.982962677686266711E-15, -1.000000000000000000 ) ) ;
#248865 = CARTESIAN_POINT ( 'NONE',  ( 22.49066049874202022, 0.05634325154338429287, -155.8499877624828400 ) ) ;
#248866 = DIRECTION ( 'NONE',  ( 0.000000000000000000, -7.056502275159890832E-15, 1.000000000000000000 ) ) ;
#248867 = CIRCLE ( 'NONE', #32417, 0.1000000000000028644 ) ;
#248868 = ORIENTED_EDGE ( 'NONE', *, *, #72883, .T. ) ;
#248869 = CIRCLE ( 'NONE', #77968, 0.5000000000000004441 ) ;
#248870 = VERTEX_POINT ( 'NONE', #119649 ) ;
#248871 = CARTESIAN_POINT ( 'NONE',  ( -18.59999999999999787, 9.250000000011157297, -188.6499999999999488 ) ) ;
#248872 = AXIS2_PLACEMENT_3D ( 'NONE', #15431, #254009, #235730 ) ;
#248873 = DIRECTION ( 'NONE',  ( 0.000000000000000000, 0.2617529984165038459, 0.9651348961777155289 ) ) ;
#248875 = CARTESIAN_POINT ( 'NONE',  ( -13.11924609551136101, 13.10551310878184061, -216.8535402360471949 ) ) ;
#248874 = CARTESIAN_POINT ( 'NONE',  ( -18.50000000000000000, 86.87366311306884370, -199.3414869250131858 ) ) ;
#248876 = AXIS2_PLACEMENT_3D ( 'NONE', #117859, #253516, #215665 ) ;
#248877 = CARTESIAN_POINT ( 'NONE',  ( 20.94999999999999574, 1.835341550235567887, -179.1551512925629197 ) ) ;
#248878 = DIRECTION ( 'NONE',  ( 0.000000000000000000, 0.8814952561688476074, -0.4721928772777262417 ) ) ;
#248879 = VECTOR ( 'NONE', #128521, 1000.000000000000000 ) ;
#248881 = EDGE_CURVE ( 'NONE', #228115, #164020, #221206, .T. ) ;
#248880 = LINE ( 'NONE', #87210, #81544 ) ;
#248882 = APPLICATION_CONTEXT ( 'automotive_design' ) ;
#248883 = ORIENTED_EDGE ( 'NONE', *, *, #58526, .T. ) ;
#248884 = ORIENTED_EDGE ( 'NONE', *, *, #169239, .T. ) ;
#248885 = ADVANCED_FACE ( 'NONE', ( #237021 ), #83035, .T. ) ;
#248886 = EDGE_CURVE ( 'NONE', #102524, #216004, #154618, .T. ) ;
#248887 = DIRECTION ( 'NONE',  ( 0.000000000000000000, 0.000000000000000000, 1.000000000000000000 ) ) ;
#248888 = ORIENTED_EDGE ( 'NONE', *, *, #237480, .F. ) ;
#248889 = DIRECTION ( 'NONE',  ( 2.952720810173289112E-16, -1.000000000000000000, 0.000000000000000000 ) ) ;
#248890 = CIRCLE ( 'NONE', #165508, 0.1000000000000028644 ) ;
#248891 = CIRCLE ( 'NONE', #215552, 0.09999999999998898659 ) ;
#248892 = CARTESIAN_POINT ( 'NONE',  ( 21.08134388332232234, 6.334680580529113314, -133.9241810824929928 ) ) ;
#248893 = AXIS2_PLACEMENT_3D ( 'NONE', #174685, #115951, #156385 ) ;
#248894 = AXIS2_PLACEMENT_3D ( 'NONE', #56532, #175269, #155698 ) ;
#248896 = ORIENTED_EDGE ( 'NONE', *, *, #34460, .T. ) ;
#248895 = VECTOR ( 'NONE', #61325, 1000.000000000000114 ) ;
#248897 = CARTESIAN_POINT ( 'NONE',  ( -21.05000000000000071, 0.000000000000000000, -4.299999999999956302 ) ) ;
#248898 = EDGE_CURVE ( 'NONE', #8134, #176263, #83804, .T. ) ;
#248899 =( BOUNDED_SURFACE ( )  B_SPLINE_SURFACE ( 3, 2, ( 
 ( #252485, #137663, #232963 ),
 ( #173013, #54285, #16480 ),
 ( #254998, #95974, #38591 ),
 ( #133832, #197648, #37323 ),
 ( #76417, #215918, #196369 ),
 ( #213359, #19017, #17719 ) ),
 .UNSPECIFIED., .F., .F., .F. ) 
 B_SPLINE_SURFACE_WITH_KNOTS ( ( 4, 2, 4 ),
 ( 3, 3 ),
 ( 1.570796326794897668, 2.356194490192346169, 3.141592653589794448 ),
 ( 0.000000000000000000, 1.000000000000000000 ),
 .UNSPECIFIED. ) 
 GEOMETRIC_REPRESENTATION_ITEM ( )  RATIONAL_B_SPLINE_SURFACE ( (
 ( 1.000000000000000000, 0.7071067811865475727, 1.000000000000000000),
 ( 1.000000000000000000, 0.6611148371778342581, 1.000000000000000000),
 ( 1.000000000000000000, 0.6092287576696778784, 1.000000000000000000),
 ( 1.000000000000000000, 0.5278258667056651143, 1.000000000000000000),
 ( 1.000000000000000000, 0.4993418825335158018, 1.000000000000000000),
 ( 1.000000000000000000, 0.5000000000000260902, 1.000000000000000000) ) ) 
 REPRESENTATION_ITEM ( '' )  SURFACE ( )  );
#248900 = EDGE_LOOP ( 'NONE', ( #58514, #231777, #42874, #203069 ) ) ;
#248901 = AXIS2_PLACEMENT_3D ( 'NONE', #254077, #195423, #14221 ) ;
#248902 = DIRECTION ( 'NONE',  ( 1.000000000000000000, 0.000000000000000000, 0.000000000000000000 ) ) ;
#248903 = DIRECTION ( 'NONE',  ( 0.000000000000000000, -0.1298341882520022694, -0.9915357197604853789 ) ) ;
#248904 = DIRECTION ( 'NONE',  ( 0.000000000000000000, 0.008583690987128059571, -0.9999631594459056361 ) ) ;
#248905 = CARTESIAN_POINT ( 'NONE',  ( 18.49999999999998934, 10.25000000001115552, -58.25000000000000000 ) ) ;
#248906 = CYLINDRICAL_SURFACE ( 'NONE', #143224, 0.8750000000000007772 ) ;
#248907 = LINE ( 'NONE', #11587, #24956 ) ;
#248908 = DIRECTION ( 'NONE',  ( -0.8660254037843277963, 0.000000000000000000, 0.5000000000001921796 ) ) ;
#248909 = DIRECTION ( 'NONE',  ( 0.000000000000000000, 0.000000000000000000, -1.000000000000000000 ) ) ;
#248911 = ORIENTED_EDGE ( 'NONE', *, *, #220655, .T. ) ;
#248910 = CARTESIAN_POINT ( 'NONE',  ( 23.04999999999999716, 8.822561741677553471, -76.25000000000004263 ) ) ;
#248913 = CARTESIAN_POINT ( 'NONE',  ( -18.40000000000000213, 11.47316190337362762, -113.1500000000000341 ) ) ;
#248912 = LINE ( 'NONE', #171975, #249382 ) ;
#248914 = ORIENTED_EDGE ( 'NONE', *, *, #172471, .T. ) ;
#248916 = EDGE_LOOP ( 'NONE', ( #60117, #100734, #19131, #53397 ) ) ;
#248915 = DIRECTION ( 'NONE',  ( 0.000000000000000000, 0.000000000000000000, -1.000000000000000000 ) ) ;
#248917 = AXIS2_PLACEMENT_3D ( 'NONE', #182373, #172781, #149347 ) ;
#248918 = ORIENTED_EDGE ( 'NONE', *, *, #178039, .T. ) ;
#248919 = CARTESIAN_POINT ( 'NONE',  ( -18.59999999999999787, 1.835341550235567887, -145.5551512925629822 ) ) ;
#248920 = AXIS2_PLACEMENT_3D ( 'NONE', #105314, #204441, #109190 ) ;
#248921 = AXIS2_PLACEMENT_3D ( 'NONE', #182101, #199090, #158710 ) ;
#248922 = CARTESIAN_POINT ( 'NONE',  ( -21.65000000000000213, 68.29142135624881860, -48.37310748452437537 ) ) ;
#248923 = ADVANCED_FACE ( 'NONE', ( #183467 ), #58347, .T. ) ;
#248925 = ADVANCED_FACE ( 'NONE', ( #118364 ), #42172, .T. ) ;
#248924 = CARTESIAN_POINT ( 'NONE',  ( 20.99749315643148151, 62.82351852664101699, -207.2177435904691833 ) ) ;
#248926 = DIRECTION ( 'NONE',  ( 0.000000000000000000, -0.9887567792719341719, -0.1495327102803664099 ) ) ;
#248927 = CARTESIAN_POINT ( 'NONE',  ( -20.94999999999999929, 87.75000000001247713, -173.1231074845242688 ) ) ;
#248928 = CARTESIAN_POINT ( 'NONE',  ( 20.73486653747090003, 68.75000000001251976, -182.6731074845244223 ) ) ;
#248929 = CARTESIAN_POINT ( 'NONE',  ( -18.59999999999999787, 86.96699927712941758, -199.3055931863049466 ) ) ;
#248930 = CARTESIAN_POINT ( 'NONE',  ( -20.85000000000000142, 6.803341081522319200, -233.7601854879220298 ) ) ;
#248931 = AXIS2_PLACEMENT_3D ( 'NONE', #41605, #200659, #227919 ) ;
#248932 = VECTOR ( 'NONE', #104080, 1000.000000000000000 ) ;
#248933 = EDGE_CURVE ( 'NONE', #121418, #105325, #108783, .T. ) ;
#248934 = DIRECTION ( 'NONE',  ( 0.000000000000000000, 0.9752329468386375932, 0.2211802418852714114 ) ) ;
#248935 = ORIENTED_EDGE ( 'NONE', *, *, #169377, .T. ) ;
#248936 = ORIENTED_EDGE ( 'NONE', *, *, #70103, .F. ) ;
#248937 = FACE_OUTER_BOUND ( 'NONE', #257666, .T. ) ;
#248938 = AXIS2_PLACEMENT_3D ( 'NONE', #244328, #125673, #245629 ) ;
#248939 = EDGE_LOOP ( 'NONE', ( #153973, #247181, #110617, #238996 ) ) ;
#248940 = CARTESIAN_POINT ( 'NONE',  ( -16.81744102076749314, 60.93935776605891164, -221.0417277355860790 ) ) ;
#248941 = EDGE_LOOP ( 'NONE', ( #88584, #236367, #87076 ) ) ;
#248942 = AXIS2_PLACEMENT_3D ( 'NONE', #240383, #176569, #199979 ) ;
#248943 = CARTESIAN_POINT ( 'NONE',  ( -17.01764560440330953, 9.950000000011138823, -180.2499999992110702 ) ) ;
#248944 = DIRECTION ( 'NONE',  ( 0.000000000000000000, 0.9651348961777157509, -0.2617529984165031243 ) ) ;
#248945 = DIRECTION ( 'NONE',  ( 0.000000000000000000, 0.000000000000000000, -1.000000000000000000 ) ) ;
#248946 = CARTESIAN_POINT ( 'NONE',  ( 22.01447462590973458, 75.90096299995320805, -210.7869076857542439 ) ) ;
#248947 = VERTEX_POINT ( 'NONE', #46495 ) ;
#248948 = CARTESIAN_POINT ( 'NONE',  ( -18.59999999999999787, 4.064367954407507533, -211.9684786640956418 ) ) ;
#248949 = AXIS2_PLACEMENT_3D ( 'NONE', #137803, #76561, #14045 ) ;
#248951 = DIRECTION ( 'NONE',  ( 1.000000000000000000, 0.000000000000000000, 0.000000000000000000 ) ) ;
#248950 = CIRCLE ( 'NONE', #36595, 4.149999999999999467 ) ;
#248952 = CARTESIAN_POINT ( 'NONE',  ( -20.94999999999999929, 31.15787740146373253, -259.8205824356103903 ) ) ;
#248953 = AXIS2_PLACEMENT_3D ( 'NONE', #168796, #210454, #48787 ) ;
#248954 = LINE ( 'NONE', #209821, #255805 ) ;
#248955 = EDGE_LOOP ( 'NONE', ( #172233, #44531, #40010, #46114 ) ) ;
#248957 = CYLINDRICAL_SURFACE ( 'NONE', #40127, 0.09999999999999817368 ) ;
#248956 = DIRECTION ( 'NONE',  ( 1.000000000000000000, 0.000000000000000000, 0.000000000000000000 ) ) ;
#248958 = ORIENTED_EDGE ( 'NONE', *, *, #155539, .T. ) ;
#248961 = ORIENTED_EDGE ( 'NONE', *, *, #47550, .F. ) ;
#248960 = CARTESIAN_POINT ( 'NONE',  ( -16.94107738177414291, 10.01423928514777373, -54.44999999999999574 ) ) ;
#248959 = DIRECTION ( 'NONE',  ( 0.000000000000000000, 0.9525900758537791946, -0.3042567129660269654 ) ) ;
#248962 = AXIS2_PLACEMENT_3D ( 'NONE', #76476, #235550, #118185 ) ;
#248963 = LINE ( 'NONE', #152447, #139491 ) ;
#248964 = FACE_OUTER_BOUND ( 'NONE', #190866, .T. ) ;
#248965 = ADVANCED_FACE ( 'NONE', ( #67363 ), #29720, .T. ) ;
#248966 = CARTESIAN_POINT ( 'NONE',  ( 20.94999999999999929, 1.835341550235569663, -112.0551512925630249 ) ) ;
#248967 = VERTEX_POINT ( 'NONE', #229013 ) ;
#248969 = EDGE_CURVE ( 'NONE', #145941, #215011, #146198, .T. ) ;
#248968 = CARTESIAN_POINT ( 'NONE',  ( -18.50000000000000000, 23.38726701055792745, -229.1122755113798632 ) ) ;
#248970 = DIRECTION ( 'NONE',  ( -0.000000000000000000, 0.9651348961777157509, -0.2617529984165031243 ) ) ;
#248971 = EDGE_CURVE ( 'NONE', #22950, #194825, #13129, .T. ) ;
#248973 = DIRECTION ( 'NONE',  ( 1.000000000000000000, -0.000000000000000000, -0.000000000000000000 ) ) ;
#248972 = CARTESIAN_POINT ( 'NONE',  ( 18.59999999999999432, 1.728086936805619311, -53.88443500516780915 ) ) ;
#248974 = ADVANCED_FACE ( 'NONE', ( #148175 ), #129886, .T. ) ;
#248976 = ORIENTED_EDGE ( 'NONE', *, *, #171576, .F. ) ;
#248975 = CARTESIAN_POINT ( 'NONE',  ( 20.94999999999999929, -1.162701749926853712, -175.3999999999999773 ) ) ;
#248977 = CIRCLE ( 'NONE', #169899, 0.09999999999998900047 ) ;
#248978 = ORIENTED_EDGE ( 'NONE', *, *, #85466, .T. ) ;
#248979 = CARTESIAN_POINT ( 'NONE',  ( -16.87036670365549540, 9.989418819312804843, -113.0204398826979713 ) ) ;
#248980 = CARTESIAN_POINT ( 'NONE',  ( -20.85000000000000142, 62.46832465249013921, -225.2232495205141731 ) ) ;
#248981 = AXIS2_PLACEMENT_3D ( 'NONE', #255887, #233819, #13490 ) ;
#248982 = EDGE_CURVE ( 'NONE', #96815, #28931, #179553, .T. ) ;
#248983 = LINE ( 'NONE', #192856, #234204 ) ;
#248986 = ADVANCED_FACE ( 'NONE', ( #247265 ), #30040, .T. ) ;
#248985 = EDGE_CURVE ( 'NONE', #219596, #54007, #46422, .T. ) ;
#248984 = ORIENTED_EDGE ( 'NONE', *, *, #207671, .T. ) ;
#248987 = LINE ( 'NONE', #109440, #214443 ) ;
#248988 = DIRECTION ( 'NONE',  ( -1.000000000000000000, 0.000000000000000000, 0.000000000000000000 ) ) ;
#248989 = CARTESIAN_POINT ( 'NONE',  ( -23.15000000000000213, 85.60000000001188880, -93.12913836187179584 ) ) ;
#248990 = EDGE_CURVE ( 'NONE', #117247, #188642, #67097, .T. ) ;
#248991 = ORIENTED_EDGE ( 'NONE', *, *, #125324, .F. ) ;
#248992 = CARTESIAN_POINT ( 'NONE',  ( 20.77766267348355811, 59.13395343506662272, -225.7920699989196294 ) ) ;
#248993 = EDGE_CURVE ( 'NONE', #104626, #171694, #243423, .T. ) ;
#248994 = ORIENTED_EDGE ( 'NONE', *, *, #222375, .T. ) ;
#248995 = AXIS2_PLACEMENT_3D ( 'NONE', #230555, #194003, #51882 ) ;
#248996 = VECTOR ( 'NONE', #198763, 1000.000000000000114 ) ;
#248997 = DIRECTION ( 'NONE',  ( -4.408576920032448588E-17, -0.1350103645451807832, -0.9908441862701610203 ) ) ;
#248998 = DIRECTION ( 'NONE',  ( 0.000000000000000000, -7.304098846218112382E-15, 1.000000000000000000 ) ) ;
#248999 = ADVANCED_FACE ( 'NONE', ( #26979 ), #91229, .T. ) ;
#249000 = AXIS2_PLACEMENT_3D ( 'NONE', #197801, #19174, #119581 ) ;
#249001 = EDGE_CURVE ( 'NONE', #241144, #157934, #195032, .T. ) ;
#249002 = ORIENTED_EDGE ( 'NONE', *, *, #143947, .T. ) ;
#249003 = ORIENTED_EDGE ( 'NONE', *, *, #94254, .T. ) ;
#249004 =( BOUNDED_SURFACE ( )  B_SPLINE_SURFACE ( 3, 2, ( 
 ( #238903, #60245, #139772 ),
 ( #219322, #105774, #242732 ),
 ( #207493, #125375, #49681 ),
 ( #187922, #203619, #245323 ) ),
 .UNSPECIFIED., .F., .F., .T. ) 
 B_SPLINE_SURFACE_WITH_KNOTS ( ( 4, 4 ),
 ( 3, 3 ),
 ( 0.0006461284895273765793, 0.0007503702773986201200 ),
 ( 0.000000000000000000, 1.000000000000000000 ),
 .UNSPECIFIED. ) 
 GEOMETRIC_REPRESENTATION_ITEM ( )  RATIONAL_B_SPLINE_SURFACE ( (
 ( 1.000000000000000000, 0.7071067811865475727, 1.000000000000000000),
 ( 1.000000000000000000, 0.7076476444648711617, 1.000000000000000000),
 ( 1.000000000000000000, 0.7075727925192061285, 1.000000000000000000),
 ( 1.000000000000000000, 0.7071067811865581199, 1.000000000000000000) ) ) 
 REPRESENTATION_ITEM ( '' )  SURFACE ( )  );
#249005 = EDGE_CURVE ( 'NONE', #222414, #232695, #192198, .T. ) ;
#249006 = CARTESIAN_POINT ( 'NONE',  ( 23.24999999999999645, 70.40000000001222702, -148.9283735034374843 ) ) ;
#249007 = ORIENTED_EDGE ( 'NONE', *, *, #94389, .T. ) ;
#249009 = ORIENTED_EDGE ( 'NONE', *, *, #206821, .T. ) ;
#249008 = CARTESIAN_POINT ( 'NONE',  ( 22.59999954896768770, 25.93893177648351056, -254.3632609673429101 ) ) ;
#249011 = EDGE_CURVE ( 'NONE', #176438, #212994, #196273, .T. ) ;
#249010 = ORIENTED_EDGE ( 'NONE', *, *, #97194, .T. ) ;
#249014 = ORIENTED_EDGE ( 'NONE', *, *, #227422, .F. ) ;
#249013 = ORIENTED_EDGE ( 'NONE', *, *, #34555, .F. ) ;
#249012 = CARTESIAN_POINT ( 'NONE',  ( 20.04142135623730070, 11.65000000001115943, -54.85000000000000142 ) ) ;
#249015 = AXIS2_PLACEMENT_3D ( 'NONE', #7438, #102667, #25731 ) ;
#249016 = EDGE_CURVE ( 'NONE', #45962, #238843, #137992, .T. ) ;
#249017 = CARTESIAN_POINT ( 'NONE',  ( 18.59999999999999076, 10.20857864377385127, -155.2500000000000284 ) ) ;
#249018 = AXIS2_PLACEMENT_3D ( 'NONE', #143681, #161995, #100675 ) ;
#249019 = VERTEX_POINT ( 'NONE', #252394 ) ;
#249020 = CARTESIAN_POINT ( 'NONE',  ( 21.14999999999999858, 0.000000000000000000, 0.000000000000000000 ) ) ;
#249021 = FACE_OUTER_BOUND ( 'NONE', #187527, .T. ) ;
#249022 = DIRECTION ( 'NONE',  ( 0.000000000000000000, 0.2128009952263630322, -0.9770955615653309501 ) ) ;
#249023 = VECTOR ( 'NONE', #10435, 1000.000000000000000 ) ;
#249024 = CARTESIAN_POINT ( 'NONE',  ( -16.87036670365549895, 66.01058118070993430, -57.00266760182645243 ) ) ;
#249025 = ORIENTED_EDGE ( 'NONE', *, *, #158474, .T. ) ;
#249026 = ORIENTED_EDGE ( 'NONE', *, *, #92230, .T. ) ;
#249027 = LINE ( 'NONE', #230744, #70819 ) ;
#249029 = ORIENTED_EDGE ( 'NONE', *, *, #89977, .T. ) ;
#249028 = CARTESIAN_POINT ( 'NONE',  ( 20.94999999999999929, 75.47649400317826007, -205.4533772768803317 ) ) ;
#249030 = CARTESIAN_POINT ( 'NONE',  ( -20.94999999999999929, 11.65000000001115232, -200.9999999999999432 ) ) ;
#249032 = EDGE_LOOP ( 'NONE', ( #180979, #249351, #76478, #79115 ) ) ;
#249031 = DIRECTION ( 'NONE',  ( 0.000000000000000000, -3.664813867694691995E-14, 1.000000000000000000 ) ) ;
#249033 = EDGE_CURVE ( 'NONE', #84512, #42158, #117175, .T. ) ;
#249034 = VERTEX_POINT ( 'NONE', #90756 ) ;
#249035 = DIRECTION ( 'NONE',  ( 0.000000000000000000, 0.8814952561688476074, -0.4721928772777262417 ) ) ;
#249036 = ORIENTED_EDGE ( 'NONE', *, *, #141799, .F. ) ;
#249037 = CARTESIAN_POINT ( 'NONE',  ( -16.94107738177414291, 65.98576071487562444, -149.0731074845244279 ) ) ;
#249038 = FACE_OUTER_BOUND ( 'NONE', #24840, .T. ) ;
#249039 = CIRCLE ( 'NONE', #124141, 11.74999999999999822 ) ;
#249040 = B_SPLINE_CURVE_WITH_KNOTS ( 'NONE', 3,
 ( #77185, #96724, #214141, #55038, #255787, #137165, #159321, #197129 ),
 .UNSPECIFIED., .F., .F.,
 ( 4, 2, 2, 4 ),
 ( 0.000000000000000000, 0.0001306511400391282358, 0.0001959767100586970294, 0.0002613022800782658500 ),
 .UNSPECIFIED. ) ;
#249041 = AXIS2_PLACEMENT_3D ( 'NONE', #198626, #162097, #4268 ) ;
#249042 = AXIS2_PLACEMENT_3D ( 'NONE', #59598, #139133, #218685 ) ;
#249044 = EDGE_LOOP ( 'NONE', ( #46802, #29234 ) ) ;
#249043 = VERTEX_POINT ( 'NONE', #231579 ) ;
#249045 = ORIENTED_EDGE ( 'NONE', *, *, #160720, .F. ) ;
#249046 = CARTESIAN_POINT ( 'NONE',  ( 21.05000000000000071, 6.477067021135910707, -33.60000000000000142 ) ) ;
#249047 = ORIENTED_EDGE ( 'NONE', *, *, #159407, .T. ) ;
#249048 = ORIENTED_EDGE ( 'NONE', *, *, #139982, .T. ) ;
#249049 = LINE ( 'NONE', #49548, #255061 ) ;
#249051 = ORIENTED_EDGE ( 'NONE', *, *, #105872, .T. ) ;
#249050 = CARTESIAN_POINT ( 'NONE',  ( -18.59999999999999787, 77.68707439010330518, -82.33768045106596389 ) ) ;
#249052 = DIRECTION ( 'NONE',  ( 0.000000000000000000, -0.9651348961777158619, 0.2617529984165032353 ) ) ;
#249053 = CIRCLE ( 'NONE', #24192, 0.1000000000000028644 ) ;
#249055 = CARTESIAN_POINT ( 'NONE',  ( 20.95512820512820440, 11.25838014693916378, -210.9828572391344039 ) ) ;
#249054 = CARTESIAN_POINT ( 'NONE',  ( -23.15000000000000213, 11.60058429089262333, -246.3380203656811887 ) ) ;
#249056 = CYLINDRICAL_SURFACE ( 'NONE', #215663, 0.1000000000000028644 ) ;
#249057 = DIRECTION ( 'NONE',  ( -0.000000000000000000, -0.000000000000000000, 1.000000000000000000 ) ) ;
#249058 = ORIENTED_EDGE ( 'NONE', *, *, #78141, .F. ) ;
#249059 = ORIENTED_EDGE ( 'NONE', *, *, #99131, .F. ) ;
#249060 = DIRECTION ( 'NONE',  ( -1.000000000000000000, -0.000000000000000000, -0.000000000000000000 ) ) ;
#249062 = EDGE_CURVE ( 'NONE', #183348, #67538, #34675, .T. ) ;
#249061 = CARTESIAN_POINT ( 'NONE',  ( -18.35668295345803713, 64.52683809664902981, -45.27310748452439526 ) ) ;
#249063 = VERTEX_POINT ( 'NONE', #55458 ) ;
#249064 = CIRCLE ( 'NONE', #244946, 0.1000000000000021289 ) ;
#249065 = CIRCLE ( 'NONE', #203255, 0.09999999999999739653 ) ;
#249066 = EDGE_CURVE ( 'NONE', #110771, #89549, #146513, .T. ) ;
#249067 = VECTOR ( 'NONE', #97155, 1000.000000000000000 ) ;
#249068 = CARTESIAN_POINT ( 'NONE',  ( 20.73486653747088582, 68.75000000001205080, -127.2731074845243597 ) ) ;
#249069 = ORIENTED_EDGE ( 'NONE', *, *, #44445, .T. ) ;
#249070 = ORIENTED_EDGE ( 'NONE', *, *, #192546, .F. ) ;
#249071 = EDGE_CURVE ( 'NONE', #120786, #7171, #16394, .T. ) ;
#249072 = LINE ( 'NONE', #229498, #246765 ) ;
#249074 = EDGE_CURVE ( 'NONE', #85130, #111529, #75678, .T. ) ;
#249073 = FACE_OUTER_BOUND ( 'NONE', #73686, .T. ) ;
#249075 = ORIENTED_EDGE ( 'NONE', *, *, #219576, .T. ) ;
#249076 = FACE_OUTER_BOUND ( 'NONE', #182273, .T. ) ;
#249077 = ORIENTED_EDGE ( 'NONE', *, *, #81242, .F. ) ;
#249078 = CARTESIAN_POINT ( 'NONE',  ( 18.49362639424878552, -9.442604367877253324, -140.7644409335108264 ) ) ;
#249079 = DIRECTION ( 'NONE',  ( -1.000000000000000000, 0.000000000000000000, 0.000000000000000000 ) ) ;
#249081 = DIRECTION ( 'NONE',  ( 0.000000000000000000, 0.000000000000000000, -1.000000000000000000 ) ) ;
#249080 = CARTESIAN_POINT ( 'NONE',  ( -23.25000000000000000, 1.580567032079710055, -244.0902705724231794 ) ) ;
#249082 = LINE ( 'NONE', #11761, #223084 ) ;
#249083 = DIRECTION ( 'NONE',  ( 0.000000000000000000, 0.000000000000000000, -1.000000000000000000 ) ) ;
#249084 = DIRECTION ( 'NONE',  ( -0.7071067811865475727, -0.7071067811865475727, 0.000000000000000000 ) ) ;
#249085 = CARTESIAN_POINT ( 'NONE',  ( 20.94999999999999929, 87.39257802171783851, -139.5970570643562212 ) ) ;
#249086 = VECTOR ( 'NONE', #155583, 1000.000000000000000 ) ;
#249088 = ORIENTED_EDGE ( 'NONE', *, *, #94340, .T. ) ;
#249087 = DIRECTION ( 'NONE',  ( -1.000000000000000000, 0.000000000000000000, 0.000000000000000000 ) ) ;
#249089 = AXIS2_PLACEMENT_3D ( 'NONE', #48560, #207659, #9433 ) ;
#249092 = VERTEX_POINT ( 'NONE', #73809 ) ;
#249091 = ORIENTED_EDGE ( 'NONE', *, *, #62978, .F. ) ;
#249090 = AXIS2_PLACEMENT_3D ( 'NONE', #256680, #37714, #117229 ) ;
#249093 = ORIENTED_EDGE ( 'NONE', *, *, #83353, .F. ) ;
#249094 = VECTOR ( 'NONE', #132207, 1000.000000000000000 ) ;
#249095 = CIRCLE ( 'NONE', #32441, 0.1000000000000000333 ) ;
#249096 = CARTESIAN_POINT ( 'NONE',  ( 21.98333005346336932, 1.115600667400684642E-11, -93.12592467094336257 ) ) ;
#249097 = DIRECTION ( 'NONE',  ( 0.000000000000000000, 0.000000000000000000, -1.000000000000000000 ) ) ;
#249098 = CIRCLE ( 'NONE', #28352, 0.1000000000000033223 ) ;
#249099 = FACE_OUTER_BOUND ( 'NONE', #243843, .T. ) ;
#249100 = DIRECTION ( 'NONE',  ( -0.000000000000000000, 0.4721928772777346239, 0.8814952561688430555 ) ) ;
#249101 = ORIENTED_EDGE ( 'NONE', *, *, #244517, .F. ) ;
#249102 = CYLINDRICAL_SURFACE ( 'NONE', #134194, 0.09999999999999939493 ) ;
#249103 = ORIENTED_EDGE ( 'NONE', *, *, #188627, .T. ) ;
#249104 = CARTESIAN_POINT ( 'NONE',  ( -21.07954763557447109, 0.06587591861840921825, 6.329290990037786280 ) ) ;
#249105 = DIRECTION ( 'NONE',  ( -1.000000000000000000, 0.000000000000000000, 3.469446951953515108E-14 ) ) ;
#249106 = CARTESIAN_POINT ( 'NONE',  ( -21.04999999999997584, 1.442680752426173552, -230.7068865970040861 ) ) ;
#249107 = EDGE_LOOP ( 'NONE', ( #89796, #153987, #164409, #30446 ) ) ;
#249108 = EDGE_CURVE ( 'NONE', #52643, #79334, #185513, .T. ) ;
#249109 = VECTOR ( 'NONE', #209595, 1000.000000000000000 ) ;
#249110 = VECTOR ( 'NONE', #87791, 1000.000000000000000 ) ;
#249111 = CYLINDRICAL_SURFACE ( 'NONE', #98176, 0.09999999999999939493 ) ;
#249112 = FACE_OUTER_BOUND ( 'NONE', #109303, .T. ) ;
#249113 = ORIENTED_EDGE ( 'NONE', *, *, #135063, .F. ) ;
#249114 = ORIENTED_EDGE ( 'NONE', *, *, #76310, .F. ) ;
#249115 = CARTESIAN_POINT ( 'NONE',  ( 23.14999999999999503, 2.272311100394802885, -217.9150152700588592 ) ) ;
#249116 = PLANE ( 'NONE',  #118777 ) ;
#249117 = DIRECTION ( 'NONE',  ( -1.000000000000000000, -0.000000000000000000, 0.000000000000000000 ) ) ;
#249118 = DIRECTION ( 'NONE',  ( 0.000000000000000000, 1.000000000000000000, 0.000000000000000000 ) ) ;
#249119 = DIRECTION ( 'NONE',  ( 0.7070776581709139474, 0.6824815363281155900, -0.1850949428989116519 ) ) ;
#249120 = CARTESIAN_POINT ( 'NONE',  ( 20.90000000000000213, -1.300000000000000044, -7.900000000000000355 ) ) ;
#249121 = ORIENTED_EDGE ( 'NONE', *, *, #113195, .F. ) ;
#249123 = EDGE_CURVE ( 'NONE', #91963, #49667, #12113, .T. ) ;
#249122 = FACE_OUTER_BOUND ( 'NONE', #216302, .T. ) ;
#249124 = CARTESIAN_POINT ( 'NONE',  ( 18.59999999999999076, 30.76917518201224055, -234.8152055956155380 ) ) ;
#249125 = AXIS2_PLACEMENT_3D ( 'NONE', #209314, #250994, #114062 ) ;
#249126 = CARTESIAN_POINT ( 'NONE',  ( -21.05439746398122836, 11.75000000001115197, -174.4899164874849760 ) ) ;
#249127 = CARTESIAN_POINT ( 'NONE',  ( -18.59999999999999787, -8.350000000000004974, 10.52591260281975138 ) ) ;
#249128 = EDGE_CURVE ( 'NONE', #256406, #202799, #125726, .T. ) ;
#249129 = VECTOR ( 'NONE', #61780, 1000.000000000000000 ) ;
#249130 = CARTESIAN_POINT ( 'NONE',  ( -18.50000000000000711, -9.419203418026649288, -7.247785810428664099 ) ) ;
#249131 = CARTESIAN_POINT ( 'NONE',  ( 21.05000000000000071, 5.399999999999998579, -23.60603087734755690 ) ) ;
#249133 = DIRECTION ( 'NONE',  ( 1.652117596168391700E-15, 1.000000000000000000, -0.000000000000000000 ) ) ;
#249132 = AXIS2_PLACEMENT_3D ( 'NONE', #212627, #34019, #208775 ) ;
#249134 = ORIENTED_EDGE ( 'NONE', *, *, #210346, .T. ) ;
#249135 = CIRCLE ( 'NONE', #90878, 0.1000000000000001027 ) ;
#249136 = EDGE_CURVE ( 'NONE', #242569, #195218, #46065, .T. ) ;
#249137 = EDGE_CURVE ( 'NONE', #211183, #15261, #789, .T. ) ;
#249138 = VECTOR ( 'NONE', #222073, 1000.000000000000000 ) ;
#249139 = ADVANCED_FACE ( 'NONE', ( #128186 ), #25769, .F. ) ;
#249140 = DIRECTION ( 'NONE',  ( 2.952720810173289112E-16, 1.000000000000000000, 6.530723674265620862E-15 ) ) ;
#249141 = CIRCLE ( 'NONE', #194979, 0.1000000000000002554 ) ;
#249142 = AXIS2_PLACEMENT_3D ( 'NONE', #219284, #177633, #257084 ) ;
#249143 = DIRECTION ( 'NONE',  ( 0.000000000000000000, -1.000000000000000000, -6.982962677686265922E-15 ) ) ;
#249144 = EDGE_CURVE ( 'NONE', #201406, #217324, #145155, .T. ) ;
#249145 = DIRECTION ( 'NONE',  ( 1.000000000000000000, 0.000000000000000000, 0.000000000000000000 ) ) ;
#249146 = ORIENTED_EDGE ( 'NONE', *, *, #62009, .T. ) ;
#249147 = B_SPLINE_CURVE_WITH_KNOTS ( 'NONE', 3,
 ( #67022, #207850, #128290, #226062, #146533, #168747, #126995, #107427, #29224, #108718, #43611, #89143, #4466, #83962, #163557, #170023, #93002, #12209, #13481, #134678, #91722, #190858, #228683, #111292, #90422, #149148, #214243, #210400, #249525, #211690 ),
 .UNSPECIFIED., .F., .F.,
 ( 4, 2, 2, 2, 2, 2, 2, 2, 2, 2, 2, 2, 2, 2, 4 ),
 ( 0.000000000000000000, 0.0003422764154113329101, 0.0006845528308226658202, 0.001026829246233998622, 0.001369105661645331640, 0.002053658492468000713, 0.002738211323290670220, 0.003080487738702004756, 0.003422764154113339726, 0.003765040569524674696, 0.004107316984936008365, 0.004449593400347343769, 0.004791869815758678305, 0.005134146231170012842, 0.005476422646581347378 ),
 .UNSPECIFIED. ) ;
#249148 = CARTESIAN_POINT ( 'NONE',  ( -18.59999999999999787, -1.162701749926853712, -75.10000000000003695 ) ) ;
#249149 = CARTESIAN_POINT ( 'NONE',  ( -21.05000000000000071, 0.03363273534480401561, -94.24118280531854452 ) ) ;
#249150 = CARTESIAN_POINT ( 'NONE',  ( 20.94999999999999574, 74.75000000001159606, -61.62310748452433273 ) ) ;
#249151 = ORIENTED_EDGE ( 'NONE', *, *, #123370, .T. ) ;
#249152 = CARTESIAN_POINT ( 'NONE',  ( -17.05016517656107311, 66.05000000001159322, -56.85040948852552845 ) ) ;
#249154 = VERTEX_POINT ( 'NONE', #205123 ) ;
#249153 = DIRECTION ( 'NONE',  ( 0.000000000000000000, 0.000000000000000000, -1.000000000000000000 ) ) ;
#249155 = LINE ( 'NONE', #213861, #246405 ) ;
#249156 = ADVANCED_FACE ( 'NONE', ( #129470 ), #188161, .F. ) ;
#249157 = CARTESIAN_POINT ( 'NONE',  ( -14.00000000000000178, 9.850000000011133849, -150.7500000000000284 ) ) ;
#249158 = ORIENTED_EDGE ( 'NONE', *, *, #155993, .T. ) ;
#249159 = CARTESIAN_POINT ( 'NONE',  ( -16.87998658237756189, 66.05000000001261640, -190.6594679167848767 ) ) ;
#249160 = APPLICATION_PROTOCOL_DEFINITION ( 'draft international standard', 'automotive_design', 1998, #198973 ) ;
#249161 = CARTESIAN_POINT ( 'NONE',  ( -20.94999999999999929, -1.835341550213257733, -112.0551512925630249 ) ) ;
#249162 = CARTESIAN_POINT ( 'NONE',  ( -21.70464131381649509, 68.90464198104483273, -203.5231074845243882 ) ) ;
#249163 = VERTEX_POINT ( 'NONE', #190756 ) ;
#249164 = DIRECTION ( 'NONE',  ( 0.000000000000000000, 1.000000000000000000, 0.000000000000000000 ) ) ;
#249165 = DIRECTION ( 'NONE',  ( 0.7071067811865474617, 0.7071067811865474617, 0.000000000000000000 ) ) ;
#249166 = CYLINDRICAL_SURFACE ( 'NONE', #11969, 0.1000000000000054040 ) ;
#249167 = ORIENTED_EDGE ( 'NONE', *, *, #219413, .F. ) ;
#249168 = ORIENTED_EDGE ( 'NONE', *, *, #67122, .T. ) ;
#249169 = CARTESIAN_POINT ( 'NONE',  ( 21.05000000000000071, -11.74999999998883560, -170.3999999999999773 ) ) ;
#249170 = CARTESIAN_POINT ( 'NONE',  ( 23.14999999999999503, 62.92003201576280702, -207.2439188921395612 ) ) ;
#249171 = CYLINDRICAL_SURFACE ( 'NONE', #136806, 0.09999999999999939493 ) ;
#249173 = DIRECTION ( 'NONE',  ( 1.000000000000000000, 0.000000000000000000, 0.000000000000000000 ) ) ;
#249172 = DIRECTION ( 'NONE',  ( 1.000000000000000000, 0.000000000000000000, 0.000000000000000000 ) ) ;
#249174 = CIRCLE ( 'NONE', #219940, 0.2000000000000005107 ) ;
#249175 = AXIS2_PLACEMENT_3D ( 'NONE', #257, #152965, #55077 ) ;
#249177 = CARTESIAN_POINT ( 'NONE',  ( 20.94999999999999929, -11.64999999998883595, -197.9999999999999432 ) ) ;
#249176 = CIRCLE ( 'NONE', #153927, 0.09999999999999939493 ) ;
#249178 = DIRECTION ( 'NONE',  ( -0.000000000000000000, 0.2253241261139106999, -0.9742838591452712693 ) ) ;
#249179 = AXIS2_PLACEMENT_3D ( 'NONE', #114100, #230206, #193657 ) ;
#249180 = FACE_OUTER_BOUND ( 'NONE', #161298, .T. ) ;
#249181 = VERTEX_POINT ( 'NONE', #249426 ) ;
#249182 = EDGE_CURVE ( 'NONE', #18097, #140929, #54796, .T. ) ;
#249184 = ORIENTED_EDGE ( 'NONE', *, *, #221880, .T. ) ;
#249183 = CARTESIAN_POINT ( 'NONE',  ( 12.48201962039796520, 62.79576509294746955, -216.3871738676108691 ) ) ;
#249185 = DIRECTION ( 'NONE',  ( 0.000000000000000000, -1.000000000000000000, -6.982962677686265922E-15 ) ) ;
#249186 = DIRECTION ( 'NONE',  ( -1.000000000000000000, 0.000000000000000000, 0.000000000000000000 ) ) ;
#249187 = DIRECTION ( 'NONE',  ( 0.000000000000000000, -0.2128009952263603677, 0.9770955615653315052 ) ) ;
#249188 = VERTEX_POINT ( 'NONE', #27831 ) ;
#249189 = CARTESIAN_POINT ( 'NONE',  ( 18.49999999999999645, 36.65892442174472876, -249.5511627012454596 ) ) ;
#249190 = CARTESIAN_POINT ( 'NONE',  ( -18.59999999999999787, -11.65000000000000036, 6.000000000000001776 ) ) ;
#249191 = CARTESIAN_POINT ( 'NONE',  ( 22.49999999999999645, 11.64976291804307884, -133.9111900236131021 ) ) ;
#249193 = EDGE_CURVE ( 'NONE', #193967, #83423, #245570, .T. ) ;
#249192 = CARTESIAN_POINT ( 'NONE',  ( 23.15000000000000213, 85.60000000001149090, -45.91707660717669626 ) ) ;
#249194 = EDGE_LOOP ( 'NONE', ( #256741, #61994, #256480, #139642 ) ) ;
#249195 = ORIENTED_EDGE ( 'NONE', *, *, #132905, .F. ) ;
#249196 = EDGE_CURVE ( 'NONE', #7786, #211757, #168647, .T. ) ;
#249197 = VECTOR ( 'NONE', #210354, 1000.000000000000000 ) ;
#249198 = EDGE_CURVE ( 'NONE', #231485, #181753, #142295, .T. ) ;
#249200 = AXIS2_PLACEMENT_3D ( 'NONE', #224503, #109682, #249217 ) ;
#249199 = DIRECTION ( 'NONE',  ( 0.000000000000000000, 0.8814952561688430555, -0.4721928772777346239 ) ) ;
#249201 = ORIENTED_EDGE ( 'NONE', *, *, #81221, .T. ) ;
#249202 = LINE ( 'NONE', #169701, #159552 ) ;
#249204 = CARTESIAN_POINT ( 'NONE',  ( -21.44999999999999929, 7.349999999999998757, -21.15000000000000213 ) ) ;
#249203 = AXIS2_PLACEMENT_3D ( 'NONE', #4943, #64941, #87057 ) ;
#249205 = CARTESIAN_POINT ( 'NONE',  ( -21.08884785362073089, 65.51921272533262197, -241.9776447927261813 ) ) ;
#249206 = CARTESIAN_POINT ( 'NONE',  ( 20.90000000000000213, 6.356682116888462630, 11.91686199900910381 ) ) ;
#249207 = VERTEX_POINT ( 'NONE', #185582 ) ;
#249208 = EDGE_CURVE ( 'NONE', #102524, #251277, #6942, .T. ) ;
#249209 = ADVANCED_FACE ( 'NONE', ( #130747 ), #109886, .T. ) ;
#249210 = CARTESIAN_POINT ( 'NONE',  ( -20.85000000000000142, -11.75000000000000000, -33.50000000000000000 ) ) ;
#249211 = DIRECTION ( 'NONE',  ( 0.000000000000000000, 0.000000000000000000, -1.000000000000000000 ) ) ;
#249212 = DIRECTION ( 'NONE',  ( 0.000000000000000000, 0.000000000000000000, 1.000000000000000000 ) ) ;
#249213 = FACE_OUTER_BOUND ( 'NONE', #180535, .T. ) ;
#249214 = CARTESIAN_POINT ( 'NONE',  ( 20.94999999999999929, -1.164121893230052995, -208.9148480855715775 ) ) ;
#249215 = CIRCLE ( 'NONE', #136761, 4.150000000000001243 ) ;
#249216 = ORIENTED_EDGE ( 'NONE', *, *, #18668, .T. ) ;
#249218 = DIRECTION ( 'NONE',  ( 0.000000000000000000, 1.000000000000000000, 0.000000000000000000 ) ) ;
#249217 = DIRECTION ( 'NONE',  ( 1.000000000000000000, 0.000000000000000000, 0.000000000000000000 ) ) ;
#249220 = EDGE_LOOP ( 'NONE', ( #225581, #122642, #152210 ) ) ;
#249219 = CIRCLE ( 'NONE', #32770, 0.09999999999999939493 ) ;
#249222 = ORIENTED_EDGE ( 'NONE', *, *, #86973, .F. ) ;
#249221 = DIRECTION ( 'NONE',  ( 1.000000000000000000, 0.000000000000000000, 0.000000000000000000 ) ) ;
#249223 = TOROIDAL_SURFACE ( 'NONE', #203430, 0.6000000000000004219, 0.1000000000000000056 ) ;
#249224 = EDGE_LOOP ( 'NONE', ( #80318, #185076, #195926, #137389 ) ) ;
#249225 = DIRECTION ( 'NONE',  ( 1.000000000000000000, 0.000000000000000000, 0.000000000000000000 ) ) ;
#249226 = CARTESIAN_POINT ( 'NONE',  ( -23.15000000000000213, 1.115600667400684642E-11, -200.9999999999999432 ) ) ;
#249227 = CARTESIAN_POINT ( 'NONE',  ( -20.85000000000000142, 69.06610602788505560, -32.23746165015079868 ) ) ;
#249228 = EDGE_CURVE ( 'NONE', #178346, #137777, #146368, .T. ) ;
#249229 = CARTESIAN_POINT ( 'NONE',  ( -20.64999999999999858, 7.250000000011155521, -79.35000000000005116 ) ) ;
#249230 = ORIENTED_EDGE ( 'NONE', *, *, #76117, .F. ) ;
#249231 = ADVANCED_FACE ( 'NONE', ( #70805 ), #210299, .F. ) ;
#249232 = EDGE_CURVE ( 'NONE', #35607, #149274, #124719, .T. ) ;
#249233 = CARTESIAN_POINT ( 'NONE',  ( -23.15000000000000213, 76.00000000001199396, -115.8981074845243029 ) ) ;
#249234 = AXIS2_PLACEMENT_3D ( 'NONE', #26291, #105785, #206204 ) ;
#249235 = CARTESIAN_POINT ( 'NONE',  ( 18.58143601961908331, 10.43572941510574026, -158.7500000000000284 ) ) ;
#249236 = ORIENTED_EDGE ( 'NONE', *, *, #209931, .T. ) ;
#249237 = CARTESIAN_POINT ( 'NONE',  ( -16.94445028196807002, 9.992063609708893068, -154.8926698215815634 ) ) ;
#249238 = EDGE_CURVE ( 'NONE', #257642, #238954, #208933, .T. ) ;
#249239 = LINE ( 'NONE', #69323, #255589 ) ;
#249240 = AXIS2_PLACEMENT_3D ( 'NONE', #235483, #116835, #94693 ) ;
#249241 = ORIENTED_EDGE ( 'NONE', *, *, #142886, .F. ) ;
#249242 = VECTOR ( 'NONE', #193299, 1000.000000000000000 ) ;
#249243 = DIRECTION ( 'NONE',  ( -1.000000000000000000, 0.000000000000000000, -0.000000000000000000 ) ) ;
#249244 = ORIENTED_EDGE ( 'NONE', *, *, #210925, .F. ) ;
#249245 = CARTESIAN_POINT ( 'NONE',  ( 18.50596464788227280, 65.69367753730654158, -97.51892380663477411 ) ) ;
#249247 = VERTEX_POINT ( 'NONE', #28219 ) ;
#249246 = CIRCLE ( 'NONE', #228582, 0.09999999999999939493 ) ;
#249248 = DIRECTION ( 'NONE',  ( -1.000000000000000000, 0.000000000000000000, 0.000000000000000000 ) ) ;
#249249 = CARTESIAN_POINT ( 'NONE',  ( 21.04386569057603751, 64.25000000001175238, -76.38027013274417243 ) ) ;
#249250 = CARTESIAN_POINT ( 'NONE',  ( -20.54999999999999716, 1.115600667400684642E-11, -67.00000000000000000 ) ) ;
#249251 = DIRECTION ( 'NONE',  ( 0.000000000000000000, -0.8814952561688430555, 0.4721928772777346239 ) ) ;
#249252 = EDGE_CURVE ( 'NONE', #201039, #190257, #247218, .T. ) ;
#249253 = VECTOR ( 'NONE', #169708, 1000.000000000000000 ) ;
#249254 = CARTESIAN_POINT ( 'NONE',  ( -20.94999999999999929, 14.61354176542825201, -235.9279552357344016 ) ) ;
#249255 = CARTESIAN_POINT ( 'NONE',  ( 20.94999999999999574, 14.00000000001115730, -72.42709253038259476 ) ) ;
#249256 = ORIENTED_EDGE ( 'NONE', *, *, #218696, .T. ) ;
#249257 = CYLINDRICAL_SURFACE ( 'NONE', #248006, 0.1000000000000018374 ) ;
#249258 = EDGE_LOOP ( 'NONE', ( #230764, #13174, #250904, #44220, #65692 ) ) ;
#249260 = LINE ( 'NONE', #11948, #62904 ) ;
#249259 = FACE_OUTER_BOUND ( 'NONE', #239874, .T. ) ;
#249261 = AXIS2_PLACEMENT_3D ( 'NONE', #15938, #211544, #52443 ) ;
#249262 = EDGE_LOOP ( 'NONE', ( #218578, #72324, #66166, #137468, #110876 ) ) ;
#249263 = DIRECTION ( 'NONE',  ( -1.000000000000000000, -0.000000000000000000, 0.000000000000000000 ) ) ;
#249264 = AXIS2_PLACEMENT_3D ( 'NONE', #73129, #52225, #212617 ) ;
#249265 = CIRCLE ( 'NONE', #232536, 0.1999999999999959310 ) ;
#249266 = CARTESIAN_POINT ( 'NONE',  ( -23.15000000000000213, 2.000000000011154189, -54.27537807723790309 ) ) ;
#249267 = AXIS2_PLACEMENT_3D ( 'NONE', #50402, #70019, #229078 ) ;
#249268 = DIRECTION ( 'NONE',  ( -0.000000000000000000, 1.000000000000000000, 0.000000000000000000 ) ) ;
#249269 = EDGE_CURVE ( 'NONE', #88476, #136640, #88120, .T. ) ;
#249270 = CYLINDRICAL_SURFACE ( 'NONE', #150128, 0.09999999999999939493 ) ;
#249271 = ORIENTED_EDGE ( 'NONE', *, *, #213404, .F. ) ;
#249273 = EDGE_LOOP ( 'NONE', ( #123136, #239033, #255860, #257803 ) ) ;
#249272 = DIRECTION ( 'NONE',  ( 0.000000000000000000, -6.982962677686266711E-15, 1.000000000000000000 ) ) ;
#249274 = CIRCLE ( 'NONE', #170196, 0.09999999999999605038 ) ;
#249275 = CARTESIAN_POINT ( 'NONE',  ( 21.13461538461538325, 10.61458296203669249, -112.8500000000000369 ) ) ;
#249276 = ADVANCED_FACE ( 'NONE', ( #107714 ), #245955, .T. ) ;
#249278 = CARTESIAN_POINT ( 'NONE',  ( -20.94999999999999929, 87.19425987394825484, -209.6674621343692024 ) ) ;
#249277 = FACE_OUTER_BOUND ( 'NONE', #210487, .T. ) ;
#249280 = EDGE_LOOP ( 'NONE', ( #14905, #27198, #209102, #155373 ) ) ;
#249279 = CARTESIAN_POINT ( 'NONE',  ( -16.87665923198281348, 9.950000000011138823, -154.8500000000000227 ) ) ;
#249281 = PRODUCT ( 'Injection Molded Chain Links 8', 'Injection Molded Chain Links 8', '', ( #53511 ) ) ;
#249282 = VERTEX_POINT ( 'NONE', #23074 ) ;
#249283 = CIRCLE ( 'NONE', #16071, 0.5000000000000004441 ) ;
#249284 = VECTOR ( 'NONE', #143623, 1000.000000000000000 ) ;
#249286 = EDGE_CURVE ( 'NONE', #121616, #175543, #42346, .T. ) ;
#249285 = DIRECTION ( 'NONE',  ( 1.000000000000000000, 0.000000000000000000, 0.000000000000000000 ) ) ;
#249288 = CLOSED_SHELL ( 'NONE', ( #128286, #89925, #123142, #135905, #59366, #76957, #129688, #160040, #205158, #153352, #222983, #25086, #180013, #204756, #84553, #251173, #185422, #74529, #211843, #21475, #229289, #253945, #180509, #182411, #164085, #54797, #4715, #90982, #51609, #63186, #257239, #219939, #170874, #65638, #20291, #193036, #4151, #3694, #76515, #156902, #38805, #151847, #61622, #63825, #9828, #159280, #203306, #96852, #210793, #16048, #50702, #163870, #155644, #36498, #75400, #236323, #1634, #147366, #49276, #118345, #133558, #221753, #92009, #112551, #181580, #251520, #155624, #243388, #219251, #217169, #108155, #146877, #34760, #143025, #200697, #149260, #244779, #54449, #202441, #122994, #256008, #63908, #51346, #61803, #235128, #215095, #88118, #218208, #5418, #104693, #186141, #177371, #191717, #223433, #71741, #188689, #97238, #12879, #92614, #52651, #127339, #102318, #99664, #77074, #193554, #176865, #68413, #193349, #219018, #94532, #172303, #138051, #198050, #229463, #2160, #104728, #95947, #55780, #219286, #183709, #231235, #124037, #66406, #44283, #63819, #100704, #243400, #88339, #52372, #184431, #130716, #87587, #151155, #100258, #217927, #43690, #124715, #9382, #248067, #241390, #247832, #196580, #12835, #25448, #128906, #150934, #124049, #209391, #28950, #123267, #7137, #46353, #197802, #131207, #110874, #83946, #81707, #181495, #109041, #242634, #237493, #113038, #122210, #164086, #184859, #193647, #210168, #156892, #145249, #11301, #34782, #35907, #71179, #87904, #165425, #171347, #236738, #87618, #175221, #53426, #195339, #211871, #224827, #131878, #121215, #38129, #155423, #244843, #220340, #64838, #165869, #19710, #54949, #200310, #233246, #198908, #133641, #8254, #5344, #225017, #91179, #130929, #250782, #85196, #31531, #108201, #81687, #137084, #74212, #179718, #161035, #223320, #244707, #125736, #129740, #126854, #64599, #197442, #168318, #234110, #151646, #142722, #5130, #29007, #170953, #68282, #47480, #73875, #157184, #22637, #170168, #129173, #199442, #96007, #80081, #27366, #178641, #133975, #110971, #244221, #103775, #101441, #239039, #49173, #89520, #166846, #41206, #191673, #7578, #80557, #63112, #66012, #256517, #582, #101352, #68110, #140438, #104779, #111199, #72498, #194203, #127368, #88527, #111623, #74239, #118079, #198910, #133921, #164291, #71236, #137828, #113699, #225749, #13508, #136513, #147627, #18637, #128021, #39961, #16868, #224571, #141564, #192723, #107310, #1422, #244149, #166265, #210715, #54492, #46941, #192879, #135290, #215613, #238162, #165601, #110281, #52078, #173484, #12865, #219921, #160633, #111393, #33488, #143590, #202696, #25868, #161464, #36745, #104857, #187759, #245107, #70194, #229866, #161330, #6051, #84774, #236205, #64724, #125308, #105652, #34086, #4291, #13166, #218871, #236600, #89668, #95711, #50331, #223310, #86640, #213109, #150090, #92080, #213089, #252264, #75453, #251280, #94422, #206599, #193050, #123108, #200172, #147594, #227808, #254915, #113500, #50420, #26582, #140302, #63446, #52392, #97394, #155866, #112419, #227204, #111661, #5198, #40411, #181659, #205373, #131369, #44265, #168117, #220424, #96074, #229449, #6814, #244274, #206976, #7120, #74666, #3519, #86428, #40696, #16671, #30267, #54350, #174800, #178620, #148874, #68281, #99630, #255097, #160324, #253180, #190620, #55425, #47540, #191223, #208539, #205016, #302, #213013, #44481, #169842, #204909, #124175, #165655, #15220, #157082, #166291, #48418, #40585, #212436, #176388, #111447, #8382, #242497, #241492, #120701, #76750, #114286, #93065, #39057, #88356, #254649, #162653, #240538, #226932, #64719, #191358, #143891, #219201, #143280, #1380, #144306, #15969, #223712, #19529, #139647, #204499, #41420, #166059, #56888, #179586, #89906, #122618, #133312, #174895, #87599, #2, #99911, #200748, #123213, #203422, #26960, #181471, #46718, #61174, #79685, #135061, #84827, #72515, #40506, #46184, #19183, #223229, #224481, #86570, #239514, #122956, #15395, #22287, #252857, #25023, #205990, #181345, #17548, #249276, #228168, #213541, #142188, #210543, #58825, #9127, #94650, #154303, #13215 ) ) ;
#249287 = CARTESIAN_POINT ( 'NONE',  ( -21.45000000000000284, 7.708578643773852157, -54.65000000000000568 ) ) ;
#249290 = EDGE_CURVE ( 'NONE', #142140, #61821, #192367, .T. ) ;
#249289 = EDGE_LOOP ( 'NONE', ( #198541, #50658, #200764, #190019 ) ) ;
#249291 = DIRECTION ( 'NONE',  ( 0.000000000000000000, 1.000000000000000000, 0.000000000000000000 ) ) ;
#249292 = ORIENTED_EDGE ( 'NONE', *, *, #191182, .F. ) ;
#249293 = DIRECTION ( 'NONE',  ( 1.000000000000000000, -1.186688945009010077E-16, -8.286604613020808509E-31 ) ) ;
#249294 = LINE ( 'NONE', #31555, #230857 ) ;
#249295 = ORIENTED_EDGE ( 'NONE', *, *, #242814, .F. ) ;
#249296 = CYLINDRICAL_SURFACE ( 'NONE', #91795, 0.09999999999998898659 ) ;
#249297 = TOROIDAL_SURFACE ( 'NONE', #28575, 0.2000000000000000111, 0.1000000000000000056 ) ;
#249298 = VECTOR ( 'NONE', #43349, 1000.000000000000000 ) ;
#249299 = EDGE_CURVE ( 'NONE', #133719, #200289, #67303, .T. ) ;
#249301 = VERTEX_POINT ( 'NONE', #46446 ) ;
#249300 = CIRCLE ( 'NONE', #236796, 0.09999999999998898659 ) ;
#249302 = CYLINDRICAL_SURFACE ( 'NONE', #47913, 4.000000000000003553 ) ;
#249303 = EDGE_CURVE ( 'NONE', #20109, #132574, #129814, .T. ) ;
#249304 = AXIS2_PLACEMENT_3D ( 'NONE', #212525, #73033, #14333 ) ;
#249305 = ORIENTED_EDGE ( 'NONE', *, *, #189576, .F. ) ;
#249306 = ORIENTED_EDGE ( 'NONE', *, *, #19429, .T. ) ;
#249307 = CARTESIAN_POINT ( 'NONE',  ( -18.59999999999999787, -9.480686695267820596, -73.94111516875786094 ) ) ;
#249308 = ORIENTED_EDGE ( 'NONE', *, *, #119104, .F. ) ;
#249309 = ADVANCED_FACE ( 'NONE', ( #68601 ), #103841, .T. ) ;
#249310 = CARTESIAN_POINT ( 'NONE',  ( -23.25000000000000000, -1.851617760457748618, -112.1031897196037050 ) ) ;
#249311 = ORIENTED_EDGE ( 'NONE', *, *, #181674, .T. ) ;
#249313 = VERTEX_POINT ( 'NONE', #165126 ) ;
#249312 = CARTESIAN_POINT ( 'NONE',  ( -21.37071067811865532, 67.92928932189320790, -90.77310748452437394 ) ) ;
#249314 = AXIS2_PLACEMENT_3D ( 'NONE', #245236, #243927, #30057 ) ;
#249315 = ORIENTED_EDGE ( 'NONE', *, *, #162874, .F. ) ;
#249316 = DIRECTION ( 'NONE',  ( 0.000000000000000000, 0.000000000000000000, -1.000000000000000000 ) ) ;
#249317 = CIRCLE ( 'NONE', #36960, 14.30833333333333890 ) ;
#249319 = ORIENTED_EDGE ( 'NONE', *, *, #94119, .T. ) ;
#249318 = ADVANCED_FACE ( 'NONE', ( #125987 ), #159073, .T. ) ;
#249322 = EDGE_LOOP ( 'NONE', ( #9398, #8070, #206159, #47197, #237056, #133416, #228590, #254267, #150513 ) ) ;
#249321 = EDGE_LOOP ( 'NONE', ( #203366, #251440 ) ) ;
#249320 = CARTESIAN_POINT ( 'NONE',  ( -23.25000000000000000, -1.736705739456431807, -179.0174225876237415 ) ) ;
#249323 = CARTESIAN_POINT ( 'NONE',  ( 21.30000000000002558, 1.115600667400684642E-11, -171.5499999999999829 ) ) ;
#249324 = AXIS2_PLACEMENT_3D ( 'NONE', #103658, #200221, #3278 ) ;
#249325 = EDGE_CURVE ( 'NONE', #151116, #19947, #38251, .T. ) ;
#249326 = CARTESIAN_POINT ( 'NONE',  ( 18.60000000000000497, 0.000000000000000000, 0.000000000000000000 ) ) ;
#249327 = ORIENTED_EDGE ( 'NONE', *, *, #119899, .T. ) ;
#249328 = CARTESIAN_POINT ( 'NONE',  ( 23.25000000000000000, 16.02417409648693436, -219.3605785455116006 ) ) ;
#249329 = ORIENTED_EDGE ( 'NONE', *, *, #58462, .F. ) ;
#249330 = CARTESIAN_POINT ( 'NONE',  ( -21.05000000000000071, 69.69503888732768360, -203.5017219185864406 ) ) ;
#249332 = ORIENTED_EDGE ( 'NONE', *, *, #170355, .F. ) ;
#249331 = CARTESIAN_POINT ( 'NONE',  ( -23.25000000000000000, 1.115600667400684642E-11, -167.5000000000000284 ) ) ;
#249333 = CARTESIAN_POINT ( 'NONE',  ( 20.94999999999999929, 18.34711819382569686, -236.8747682978092541 ) ) ;
#249334 = VERTEX_POINT ( 'NONE', #105107 ) ;
#249335 = EDGE_CURVE ( 'NONE', #7989, #48943, #3471, .T. ) ;
#249336 = LINE ( 'NONE', #229754, #241193 ) ;
#249337 = CARTESIAN_POINT ( 'NONE',  ( 20.84999999999998721, 62.42744096235649920, -225.1319887738535499 ) ) ;
#249338 = EDGE_CURVE ( 'NONE', #153611, #112125, #50685, .T. ) ;
#249339 = VECTOR ( 'NONE', #58358, 1000.000000000000000 ) ;
#249340 = ORIENTED_EDGE ( 'NONE', *, *, #70480, .F. ) ;
#249341 = CARTESIAN_POINT ( 'NONE',  ( -20.94999999999999929, 1.115600667400684642E-11, -100.5000000000000284 ) ) ;
#249342 = DIRECTION ( 'NONE',  ( 0.000000000000000000, -0.9126074666063769270, -0.4088369013363280513 ) ) ;
#249343 = ORIENTED_EDGE ( 'NONE', *, *, #239345, .F. ) ;
#249345 = VERTEX_POINT ( 'NONE', #102542 ) ;
#249344 = CYLINDRICAL_SURFACE ( 'NONE', #130529, 2.000000000000001776 ) ;
#249346 = CARTESIAN_POINT ( 'NONE',  ( 20.94999999999999574, 65.52661458509918191, -128.9444530202758301 ) ) ;
#249348 = ORIENTED_EDGE ( 'NONE', *, *, #3230, .T. ) ;
#249347 = ORIENTED_EDGE ( 'NONE', *, *, #213960, .T. ) ;
#249349 = ORIENTED_EDGE ( 'NONE', *, *, #237705, .T. ) ;
#249350 = DIRECTION ( 'NONE',  ( 1.000000000000000000, 0.000000000000000000, 0.000000000000000000 ) ) ;
#249351 = ORIENTED_EDGE ( 'NONE', *, *, #257521, .F. ) ;
#249352 = ORIENTED_EDGE ( 'NONE', *, *, #35809, .T. ) ;
#249353 = DIRECTION ( 'NONE',  ( 0.000000000000000000, 0.1350103645451807832, 0.9908441862701610203 ) ) ;
#249354 = ORIENTED_EDGE ( 'NONE', *, *, #31189, .F. ) ;
#249355 = DIRECTION ( 'NONE',  ( 1.000000000000000000, 0.000000000000000000, 0.000000000000000000 ) ) ;
#249356 = CARTESIAN_POINT ( 'NONE',  ( -20.64999999999999858, 2.000000000011154189, -187.7753780772378889 ) ) ;
#249357 = EDGE_LOOP ( 'NONE', ( #153843, #219646, #197245, #170599 ) ) ;
#249358 = ORIENTED_EDGE ( 'NONE', *, *, #142305, .T. ) ;
#249359 = VECTOR ( 'NONE', #255538, 1000.000000000000114 ) ;
#249360 = DIRECTION ( 'NONE',  ( 1.000000000000000000, 1.186688945009009831E-16, 0.000000000000000000 ) ) ;
#249361 = AXIS2_PLACEMENT_3D ( 'NONE', #224647, #164691, #146381 ) ;
#249362 = AXIS2_PLACEMENT_3D ( 'NONE', #147808, #52534, #70859 ) ;
#249363 = EDGE_LOOP ( 'NONE', ( #218761, #17910, #228806 ) ) ;
#249364 = B_SPLINE_CURVE_WITH_KNOTS ( 'NONE', 3,
 ( #102454, #218568, #219866, #123346, #43808, #257646 ),
 .UNSPECIFIED., .F., .F.,
 ( 4, 2, 4 ),
 ( 0.000000000000000000, 0.0002113392456165989763, 0.0004226784912331979526 ),
 .UNSPECIFIED. ) ;
#249365 = ADVANCED_FACE ( 'NONE', ( #185970 ), #25620, .F. ) ;
#249366 = VECTOR ( 'NONE', #63084, 1000.000000000000000 ) ;
#249367 = CARTESIAN_POINT ( 'NONE',  ( -20.54999999999999716, 7.250000000011155521, -45.75000000000000000 ) ) ;
#249368 = VERTEX_POINT ( 'NONE', #45173 ) ;
#249369 = DIRECTION ( 'NONE',  ( 0.000000000000000000, -1.000000000000000000, -7.272083257015735086E-15 ) ) ;
#249371 = VERTEX_POINT ( 'NONE', #184675 ) ;
#249370 = CARTESIAN_POINT ( 'NONE',  ( -21.64999999999999858, 7.350000000011155166, -188.7499999999999716 ) ) ;
#249372 = DIRECTION ( 'NONE',  ( -1.000000000000000000, 0.000000000000000000, 0.000000000000000000 ) ) ;
#249373 = DIRECTION ( 'NONE',  ( 0.7071067811865463515, 0.3338907855510733769, 0.6233112732207632956 ) ) ;
#249374 = CARTESIAN_POINT ( 'NONE',  ( -17.11825945287483108, 12.41403342719999259, -211.2428889513006993 ) ) ;
#249375 = DIRECTION ( 'NONE',  ( -1.000000000000000000, -9.458662978381124901E-16, 5.066746821047763994E-16 ) ) ;
#249376 = DIRECTION ( 'NONE',  ( 1.000000000000000000, 0.000000000000000000, 0.000000000000000000 ) ) ;
#249378 = CARTESIAN_POINT ( 'NONE',  ( 21.05000000000000071, 1.349084418638171412, -175.4864989635454435 ) ) ;
#249377 = AXIS2_PLACEMENT_3D ( 'NONE', #153134, #111401, #115246 ) ;
#249380 = DIRECTION ( 'NONE',  ( 1.000000000000000000, -0.000000000000000000, -0.000000000000000000 ) ) ;
#249379 = AXIS2_PLACEMENT_3D ( 'NONE', #241386, #190409, #30058 ) ;
#249381 = DIRECTION ( 'NONE',  ( 1.000000000000000000, 0.000000000000000000, 0.000000000000000000 ) ) ;
#249382 = VECTOR ( 'NONE', #113236, 1000.000000000000227 ) ;
#249383 = CARTESIAN_POINT ( 'NONE',  ( 21.05000000000005400, 78.47315729244128590, -52.27034697567518862 ) ) ;
#249384 = EDGE_CURVE ( 'NONE', #91733, #141490, #146556, .T. ) ;
#249385 = ORIENTED_EDGE ( 'NONE', *, *, #159943, .F. ) ;
#249386 = TOROIDAL_SURFACE ( 'NONE', #170312, 0.2000000000000000111, 0.1000000000000000056 ) ;
#249387 = EDGE_LOOP ( 'NONE', ( #91958, #7177, #140672, #93925 ) ) ;
#249389 = ORIENTED_EDGE ( 'NONE', *, *, #11629, .F. ) ;
#249388 = FACE_OUTER_BOUND ( 'NONE', #138282, .T. ) ;
#249390 = ORIENTED_EDGE ( 'NONE', *, *, #163691, .T. ) ;
#249391 = FACE_OUTER_BOUND ( 'NONE', #239781, .T. ) ;
#249392 = DIRECTION ( 'NONE',  ( 0.000000000000000000, 0.000000000000000000, 1.000000000000000000 ) ) ;
#249394 = CARTESIAN_POINT ( 'NONE',  ( -18.59999999999999787, -1.263275465217258198, -41.40186466674640542 ) ) ;
#249393 = DIRECTION ( 'NONE',  ( -0.000000000000000000, -0.2617529984165031243, -0.9651348961777157509 ) ) ;
#249395 = ORIENTED_EDGE ( 'NONE', *, *, #186197, .F. ) ;
#249396 = ORIENTED_EDGE ( 'NONE', *, *, #148750, .F. ) ;
#249397 = CARTESIAN_POINT ( 'NONE',  ( 18.45036689428335208, -9.490184143317806686, -40.51269582748633269 ) ) ;
#249398 = DIRECTION ( 'NONE',  ( 1.000000000000000000, 0.000000000000000000, 0.000000000000000000 ) ) ;
#249399 = ORIENTED_EDGE ( 'NONE', *, *, #210333, .T. ) ;
#249400 = EDGE_LOOP ( 'NONE', ( #233635, #86041, #150391, #186912 ) ) ;
#249401 = AXIS2_PLACEMENT_3D ( 'NONE', #178486, #237154, #201871 ) ;
#249402 = AXIS2_PLACEMENT_3D ( 'NONE', #199515, #177396, #59956 ) ;
#249403 = CARTESIAN_POINT ( 'NONE',  ( -23.15000000000000213, 1.115600667400684642E-11, -100.5000000000000426 ) ) ;
#249404 = DIRECTION ( 'NONE',  ( 0.000000000000000000, 0.000000000000000000, -1.000000000000000000 ) ) ;
#249405 = DIRECTION ( 'NONE',  ( 1.000000000000000000, 0.000000000000000000, 0.000000000000000000 ) ) ;
#249406 = DIRECTION ( 'NONE',  ( 0.000000000000000000, 0.000000000000000000, 1.000000000000000000 ) ) ;
#249408 = VERTEX_POINT ( 'NONE', #69901 ) ;
#249407 = DIRECTION ( 'NONE',  ( 0.000000000000000000, 0.000000000000000000, 1.000000000000000000 ) ) ;
#249409 = AXIS2_PLACEMENT_3D ( 'NONE', #226578, #144469, #243593 ) ;
#249410 = DIRECTION ( 'NONE',  ( -1.000000000000000000, 0.000000000000000000, -0.000000000000000000 ) ) ;
#249411 = PLANE ( 'NONE',  #156543 ) ;
#249412 = DIRECTION ( 'NONE',  ( 0.000000000000000000, -0.9908441862701605762, 0.1350103645451835310 ) ) ;
#249413 = CARTESIAN_POINT ( 'NONE',  ( -21.14999999999999858, -11.74999999998884448, -170.3999999999999773 ) ) ;
#249414 = ORIENTED_EDGE ( 'NONE', *, *, #130813, .T. ) ;
#249415 = CARTESIAN_POINT ( 'NONE',  ( 15.07585980824113392, 66.58236703690555203, -84.87415901879209912 ) ) ;
#249416 = DIRECTION ( 'NONE',  ( -1.000000000000000000, 0.000000000000000000, 0.000000000000000000 ) ) ;
#249418 = CARTESIAN_POINT ( 'NONE',  ( 20.94999999999999929, 76.00000000001170974, -69.52310748452431710 ) ) ;
#249417 = LINE ( 'NONE', #186884, #219996 ) ;
#249419 = FACE_OUTER_BOUND ( 'NONE', #244188, .T. ) ;
#249421 = EDGE_CURVE ( 'NONE', #46286, #188358, #183995, .T. ) ;
#249420 = CARTESIAN_POINT ( 'NONE',  ( -16.82055514392389028, 9.950000000011140600, -54.32320192545801518 ) ) ;
#249422 = CARTESIAN_POINT ( 'NONE',  ( -17.11825945287482753, 9.950000000011138823, -180.2499999999999716 ) ) ;
#249423 = DIRECTION ( 'NONE',  ( 0.000000000000000000, -1.000000000000000000, 0.000000000000000000 ) ) ;
#249424 = VECTOR ( 'NONE', #82798, 1000.000000000000114 ) ;
#249425 = VECTOR ( 'NONE', #245914, 1000.000000000000000 ) ;
#249426 = CARTESIAN_POINT ( 'NONE',  ( 18.49999999999999289, 68.00366762990589109, -224.2307594727497815 ) ) ;
#249427 = CARTESIAN_POINT ( 'NONE',  ( -23.25000000000000000, 11.48087284840413425, -198.4995883060917663 ) ) ;
#249428 = ORIENTED_EDGE ( 'NONE', *, *, #59279, .T. ) ;
#249429 = CIRCLE ( 'NONE', #216260, 0.1000000000000009492 ) ;
#249430 = VERTEX_POINT ( 'NONE', #153304 ) ;
#249431 = ORIENTED_EDGE ( 'NONE', *, *, #161726, .F. ) ;
#249432 = ADVANCED_FACE ( 'NONE', ( #89428 ), #211971, .F. ) ;
#249433 = CARTESIAN_POINT ( 'NONE',  ( 20.11144452914043868, 66.06638914889192904, -95.13281403056952001 ) ) ;
#249434 = LINE ( 'NONE', #172506, #77833 ) ;
#249435 = EDGE_LOOP ( 'NONE', ( #114119, #138308, #81550, #167504 ) ) ;
#249436 = EDGE_CURVE ( 'NONE', #129734, #81780, #150700, .T. ) ;
#249437 = VECTOR ( 'NONE', #193300, 1000.000000000000000 ) ;
#249438 = AXIS2_PLACEMENT_3D ( 'NONE', #208467, #244997, #87187 ) ;
#249439 = EDGE_LOOP ( 'NONE', ( #87456, #180675, #122840, #193917 ) ) ;
#249441 = EDGE_CURVE ( 'NONE', #71456, #241932, #104842, .T. ) ;
#249440 = AXIS2_PLACEMENT_3D ( 'NONE', #27318, #109355, #108103 ) ;
#249442 = ORIENTED_EDGE ( 'NONE', *, *, #183639, .F. ) ;
#249443 = DIRECTION ( 'NONE',  ( -1.000000000000000000, -0.000000000000000000, -0.000000000000000000 ) ) ;
#249444 = ORIENTED_EDGE ( 'NONE', *, *, #184216, .F. ) ;
#249445 = AXIS2_PLACEMENT_3D ( 'NONE', #1468, #99274, #22352 ) ;
#249446 = CARTESIAN_POINT ( 'NONE',  ( -23.15000000000000213, 76.54968129668591814, -201.4963242025517047 ) ) ;
#249447 = AXIS2_PLACEMENT_3D ( 'NONE', #195633, #19551, #254276 ) ;
#249448 = AXIS2_PLACEMENT_3D ( 'NONE', #101493, #178543, #183658 ) ;
#249449 = CARTESIAN_POINT ( 'NONE',  ( -20.54999999999999716, 0.000000000000000000, -33.50000000000000000 ) ) ;
#249450 = CARTESIAN_POINT ( 'NONE',  ( 21.05000000000000071, 76.00000000001213607, -136.4231074845243086 ) ) ;
#249451 = AXIS2_PLACEMENT_3D ( 'NONE', #225596, #126530, #206064 ) ;
#249452 = DIRECTION ( 'NONE',  ( 1.000000000000000000, 0.000000000000000000, 0.000000000000000000 ) ) ;
#249453 = DIRECTION ( 'NONE',  ( 0.7071067811865127117, 0.7071067811865821007, 0.000000000000000000 ) ) ;
#249455 = EDGE_LOOP ( 'NONE', ( #85738, #229286, #226435, #218780 ) ) ;
#249454 = CARTESIAN_POINT ( 'NONE',  ( 21.05000000000000071, 10.72371710470752149, 0.000000000000000000 ) ) ;
#249457 = CARTESIAN_POINT ( 'NONE',  ( 21.04105312098515057, 8.875332623054768888, -79.32850674721208861 ) ) ;
#249456 = CARTESIAN_POINT ( 'NONE',  ( 20.95575313997065336, 65.38544669673677845, -61.90181678257957287 ) ) ;
#249458 = AXIS2_PLACEMENT_3D ( 'NONE', #95714, #237810, #136104 ) ;
#249459 = EDGE_CURVE ( 'NONE', #113090, #233410, #250615, .T. ) ;
#249460 = CARTESIAN_POINT ( 'NONE',  ( -16.93388492042257809, 9.988541822515902169, -20.90054512318617697 ) ) ;
#249461 = ORIENTED_EDGE ( 'NONE', *, *, #113534, .F. ) ;
#249462 = DIRECTION ( 'NONE',  ( -1.000000000000000000, 0.000000000000000000, 0.000000000000000000 ) ) ;
#249463 = CARTESIAN_POINT ( 'NONE',  ( -12.60206096961791999, 9.389686005666813884, -116.1728435063513700 ) ) ;
#249464 = CARTESIAN_POINT ( 'NONE',  ( 18.59999999999999076, 1.250000000011167511, -142.0000000000000284 ) ) ;
#249465 = ORIENTED_EDGE ( 'NONE', *, *, #219405, .F. ) ;
#249466 = DIRECTION ( 'NONE',  ( 0.000000000000000000, 0.000000000000000000, 1.000000000000000000 ) ) ;
#249467 = LINE ( 'NONE', #70847, #231901 ) ;
#249468 = EDGE_LOOP ( 'NONE', ( #165456, #162067, #153576, #165766 ) ) ;
#249469 = DIRECTION ( 'NONE',  ( -0.000000000000000000, 0.000000000000000000, -1.000000000000000000 ) ) ;
#249470 = AXIS2_PLACEMENT_3D ( 'NONE', #23487, #5133, #125131 ) ;
#249471 = CARTESIAN_POINT ( 'NONE',  ( 21.07928932188134397, 0.000000000000000000, 0.000000000000000000 ) ) ;
#249472 = DIRECTION ( 'NONE',  ( -3.265361837132812600E-16, 0.9770955615653313941, 0.2128009952263603677 ) ) ;
#249473 = ORIENTED_EDGE ( 'NONE', *, *, #150030, .T. ) ;
#249474 = ORIENTED_EDGE ( 'NONE', *, *, #134759, .F. ) ;
#249475 = AXIS2_PLACEMENT_3D ( 'NONE', #79445, #162880, #58598 ) ;
#249476 = AXIS2_PLACEMENT_3D ( 'NONE', #54872, #51004, #251804 ) ;
#249477 = DIRECTION ( 'NONE',  ( 1.000000000000000000, 0.000000000000000000, 0.000000000000000000 ) ) ;
#249478 = DIRECTION ( 'NONE',  ( -1.000000000000000000, -2.885090398161910739E-16, -6.283419270304611573E-17 ) ) ;
#249479 = CYLINDRICAL_SURFACE ( 'NONE', #57785, 0.1000000000000072220 ) ;
#249480 = CARTESIAN_POINT ( 'NONE',  ( -21.14999999999999858, 12.71802988599559292, -223.5105008658000258 ) ) ;
#249481 = AXIS2_PLACEMENT_3D ( 'NONE', #48090, #229315, #58333 ) ;
#249483 = DIRECTION ( 'NONE',  ( 1.000000000000000000, 0.000000000000000000, 0.000000000000000000 ) ) ;
#249482 = CARTESIAN_POINT ( 'NONE',  ( 20.85000000000000142, 77.85161776048053639, -57.91991776492063337 ) ) ;
#249484 = CARTESIAN_POINT ( 'NONE',  ( 20.94999999999999929, 5.000000000011153745, -45.90526601891310321 ) ) ;
#249485 = FACE_OUTER_BOUND ( 'NONE', #257088, .T. ) ;
#249486 = DIRECTION ( 'NONE',  ( -1.000000000000000000, -1.832422279913646096E-16, -3.990820347355631841E-17 ) ) ;
#249487 = ORIENTED_EDGE ( 'NONE', *, *, #190344, .F. ) ;
#249488 = AXIS2_PLACEMENT_3D ( 'NONE', #157044, #116618, #256064 ) ;
#249489 = ADVANCED_FACE ( 'NONE', ( #13754 ), #54151, .F. ) ;
#249491 = ORIENTED_EDGE ( 'NONE', *, *, #198635, .T. ) ;
#249490 = CARTESIAN_POINT ( 'NONE',  ( 20.94999999999999929, 1.115600667400684642E-11, -64.10000000000000853 ) ) ;
#249492 = CARTESIAN_POINT ( 'NONE',  ( 22.00356870141230914, 68.74575763752079638, -170.0231074845244450 ) ) ;
#249493 = DIRECTION ( 'NONE',  ( 0.000000000000000000, -0.2128009952263403282, 0.9770955615653358350 ) ) ;
#249494 = DIRECTION ( 'NONE',  ( 0.000000000000000000, -1.000000000000000000, 0.000000000000000000 ) ) ;
#249495 = CARTESIAN_POINT ( 'NONE',  ( -16.87683809663752754, 66.13411015068105314, -123.2556806774542935 ) ) ;
#249496 = CARTESIAN_POINT ( 'NONE',  ( 21.05000000000000071, 11.60000000001116049, -194.0717967697244717 ) ) ;
#249498 = ORIENTED_EDGE ( 'NONE', *, *, #21597, .T. ) ;
#249497 = DIRECTION ( 'NONE',  ( 0.000000000000000000, -0.9654727137038715545, -0.2605042016806676242 ) ) ;
#249499 = CYLINDRICAL_SURFACE ( 'NONE', #29900, 0.1000000000000124678 ) ;
#249500 = DIRECTION ( 'NONE',  ( -1.000000000000000000, -0.000000000000000000, -0.000000000000000000 ) ) ;
#249501 = CARTESIAN_POINT ( 'NONE',  ( -5.999999999999938716, 64.75000000001119815, -26.02310748452479316 ) ) ;
#249502 = EDGE_CURVE ( 'NONE', #38036, #32896, #238138, .T. ) ;
#249503 = ORIENTED_EDGE ( 'NONE', *, *, #256019, .T. ) ;
#249504 = LINE ( 'NONE', #252056, #92905 ) ;
#249506 = VERTEX_POINT ( 'NONE', #114126 ) ;
#249505 = TOROIDAL_SURFACE ( 'NONE', #236810, 4.099999999999999645, 0.1000000000000000056 ) ;
#249507 = CIRCLE ( 'NONE', #241138, 0.2000000000000057288 ) ;
#249508 = ADVANCED_FACE ( 'NONE', ( #108988 ), #230230, .F. ) ;
#249509 = ADVANCED_FACE ( 'NONE', ( #188536 ), #29503, .T. ) ;
#249510 = DIRECTION ( 'NONE',  ( 0.000000000000000000, -1.000000000000000000, -6.982962677686265922E-15 ) ) ;
#249511 = ORIENTED_EDGE ( 'NONE', *, *, #87094, .T. ) ;
#249512 = DIRECTION ( 'NONE',  ( 0.000000000000000000, -1.000000000000000000, 0.000000000000000000 ) ) ;
#249513 = VECTOR ( 'NONE', #219404, 1000.000000000000000 ) ;
#249514 = ORIENTED_EDGE ( 'NONE', *, *, #110871, .T. ) ;
#249515 = DIRECTION ( 'NONE',  ( -1.000000000000000000, 0.000000000000000000, -0.000000000000000000 ) ) ;
#249516 = CARTESIAN_POINT ( 'NONE',  ( 23.24999999999999645, 54.46551753941606222, -236.3409998116131021 ) ) ;
#249517 = ADVANCED_FACE ( 'NONE', ( #94561 ), #179581, .T. ) ;
#249518 = DIRECTION ( 'NONE',  ( -0.000000000000000000, -0.000000000000000000, 1.000000000000000000 ) ) ;
#249519 = ORIENTED_EDGE ( 'NONE', *, *, #182746, .F. ) ;
#249520 = ADVANCED_FACE ( 'NONE', ( #251065 ), #72462, .T. ) ;
#249521 = EDGE_CURVE ( 'NONE', #14237, #71369, #39768, .T. ) ;
#249522 = CARTESIAN_POINT ( 'NONE',  ( -16.97683809663752186, 9.949999999999983302, -13.40236401819648648 ) ) ;
#249523 = CARTESIAN_POINT ( 'NONE',  ( 21.05000000000000071, 48.40874555430184500, -244.2873875965402704 ) ) ;
#249524 = DIRECTION ( 'NONE',  ( 1.000000000000000000, 0.000000000000000000, 0.000000000000000000 ) ) ;
#249525 = CARTESIAN_POINT ( 'NONE',  ( 12.25000000000000000, 9.349999999999983658, -16.86426760761609600 ) ) ;
#249526 = DIRECTION ( 'NONE',  ( 0.000000000000000000, 0.2128009952263603399, -0.9770955615653315052 ) ) ;
#249527 = ORIENTED_EDGE ( 'NONE', *, *, #89469, .F. ) ;
#249528 = CARTESIAN_POINT ( 'NONE',  ( 20.94999999999999574, 64.37928932189281284, -42.89152413686537102 ) ) ;
#249529 = ORIENTED_EDGE ( 'NONE', *, *, #116944, .T. ) ;
#249531 = EDGE_LOOP ( 'NONE', ( #61843, #98588, #33255, #156270, #255114 ) ) ;
#249530 = CARTESIAN_POINT ( 'NONE',  ( 20.85882249326303040, 10.33248238083634796, -106.0948465439131922 ) ) ;
#249532 = EDGE_CURVE ( 'NONE', #116896, #83495, #61076, .T. ) ;
#249533 = ORIENTED_EDGE ( 'NONE', *, *, #84027, .T. ) ;
#249534 = CARTESIAN_POINT ( 'NONE',  ( -23.15000000000000213, 1.925233644859816629, -12.73024353312613144 ) ) ;
#249535 = ORIENTED_EDGE ( 'NONE', *, *, #192, .T. ) ;
#249536 = CARTESIAN_POINT ( 'NONE',  ( 22.57320508075688537, 64.35000000001195986, -103.0231074845244024 ) ) ;
#249537 = CARTESIAN_POINT ( 'NONE',  ( 21.53752568622134689, 0.09897446127753155298, -26.71319212545141752 ) ) ;
#249538 = CARTESIAN_POINT ( 'NONE',  ( -23.15000000000000213, 19.96675702282871256, -237.7735354486364088 ) ) ;
#249539 = VERTEX_POINT ( 'NONE', #256144 ) ;
#249540 = EDGE_CURVE ( 'NONE', #122081, #121455, #150847, .T. ) ;
#249541 = ADVANCED_FACE ( 'NONE', ( #80101 ), #221559, .T. ) ;
#249542 = CARTESIAN_POINT ( 'NONE',  ( -23.15000000000000213, 4.350000000011156054, -146.2500000000000284 ) ) ;
#249543 = CARTESIAN_POINT ( 'NONE',  ( -16.86337532320260735, 66.02003279578715933, -48.57418301554158546 ) ) ;
#249544 = CARTESIAN_POINT ( 'NONE',  ( 21.72449340488909897, 30.36402033568042924, -234.5126641304238149 ) ) ;
#249545 = ORIENTED_EDGE ( 'NONE', *, *, #5572, .F. ) ;
#249547 = VERTEX_POINT ( 'NONE', #234074 ) ;
#249546 = CARTESIAN_POINT ( 'NONE',  ( 18.59999999999999076, 11.65000000001115943, -125.3500000000000512 ) ) ;
#249548 = DIRECTION ( 'NONE',  ( 0.8191520442889914655, 0.5735764363510466035, -0.000000000000000000 ) ) ;
#249549 = DIRECTION ( 'NONE',  ( 1.000000000000000000, 0.000000000000000000, 0.000000000000000000 ) ) ;
#249550 = AXIS2_PLACEMENT_3D ( 'NONE', #105127, #204259, #83005 ) ;
#249551 = CIRCLE ( 'NONE', #91129, 0.1000000000000028644 ) ;
#249552 = AXIS2_PLACEMENT_3D ( 'NONE', #192411, #211985, #253643 ) ;
#249553 = CIRCLE ( 'NONE', #133030, 0.1000000000000000472 ) ;
#249554 = ORIENTED_EDGE ( 'NONE', *, *, #86375, .T. ) ;
#249555 = DIRECTION ( 'NONE',  ( 0.000000000000000000, 0.8814952561688438326, -0.4721928772777334582 ) ) ;
#249556 = DIRECTION ( 'NONE',  ( 0.000000000000000000, -7.056502275159890832E-15, 1.000000000000000000 ) ) ;
#249557 = VECTOR ( 'NONE', #238864, 1000.000000000000000 ) ;
#249558 = CARTESIAN_POINT ( 'NONE',  ( -18.40000000000000568, 64.52683809664904402, -48.63168612828709314 ) ) ;
#249559 = ORIENTED_EDGE ( 'NONE', *, *, #64832, .T. ) ;
#249560 = DIRECTION ( 'NONE',  ( 1.000000000000000000, 0.000000000000000000, 0.000000000000000000 ) ) ;
#249561 = EDGE_CURVE ( 'NONE', #218111, #10047, #77549, .T. ) ;
#249562 = EDGE_CURVE ( 'NONE', #181858, #211733, #5071, .T. ) ;
#249563 = DIRECTION ( 'NONE',  ( 0.000000000000000000, -1.000000000000000000, -6.982962677686265922E-15 ) ) ;
#249564 = DIRECTION ( 'NONE',  ( -1.000000000000000000, 0.000000000000000000, 0.000000000000000000 ) ) ;
#249565 = ORIENTED_EDGE ( 'NONE', *, *, #237777, .T. ) ;
#249566 = AXIS2_PLACEMENT_3D ( 'NONE', #249131, #70511, #229559 ) ;
#249567 = EDGE_CURVE ( 'NONE', #224643, #63408, #155854, .T. ) ;
#249568 = AXIS2_PLACEMENT_3D ( 'NONE', #219722, #200179, #176774 ) ;
#249569 = AXIS2_PLACEMENT_3D ( 'NONE', #55022, #254501, #137152 ) ;
#249570 = ORIENTED_EDGE ( 'NONE', *, *, #37632, .T. ) ;
#249571 = CARTESIAN_POINT ( 'NONE',  ( 21.05000000000000071, 18.65488991999774271, -228.0822300706204544 ) ) ;
#249572 = ORIENTED_EDGE ( 'NONE', *, *, #106331, .F. ) ;
#249573 = CARTESIAN_POINT ( 'NONE',  ( -23.25000000000000000, 7.021664781900089913, -37.33356540189728889 ) ) ;
#249574 = CARTESIAN_POINT ( 'NONE',  ( 18.59999999999999787, -1.835341550224411922, -11.55515129256297868 ) ) ;
#249576 = EDGE_LOOP ( 'NONE', ( #156866, #159234, #107864, #47900 ) ) ;
#249575 = FACE_OUTER_BOUND ( 'NONE', #214707, .T. ) ;
#249577 = DIRECTION ( 'NONE',  ( 0.000000000000000000, 0.2128009952263650861, -0.9770955615653305060 ) ) ;
#249578 = CARTESIAN_POINT ( 'NONE',  ( 21.12769345151713196, 65.28071232307100047, -57.27562713832691799 ) ) ;
#249579 = DIRECTION ( 'NONE',  ( 0.000000000000000000, 1.000000000000000000, 6.982962677686266711E-15 ) ) ;
#249580 = DIRECTION ( 'NONE',  ( -0.000000000000000000, 1.000000000000000000, 0.000000000000000000 ) ) ;
#249581 = CARTESIAN_POINT ( 'NONE',  ( 17.23472005113826810, 65.69211804551073897, -47.47653062445572658 ) ) ;
#249582 = EDGE_CURVE ( 'NONE', #13982, #192458, #229969, .T. ) ;
#249583 = DIRECTION ( 'NONE',  ( -0.000000000000000000, 7.272083257015735086E-15, -1.000000000000000000 ) ) ;
#249584 = CARTESIAN_POINT ( 'NONE',  ( 20.94999999999999929, 87.65000000001170122, -69.52310748452423184 ) ) ;
#249586 = ORIENTED_EDGE ( 'NONE', *, *, #31839, .T. ) ;
#249585 = FACE_OUTER_BOUND ( 'NONE', #216123, .T. ) ;
#249587 = ADVANCED_FACE ( 'NONE', ( #138789 ), #116700, .F. ) ;
#249588 = AXIS2_PLACEMENT_3D ( 'NONE', #87537, #126685, #206224 ) ;
#249589 = EDGE_CURVE ( 'NONE', #72694, #41292, #56693, .T. ) ;
#249590 = DIRECTION ( 'NONE',  ( 0.000000000000000000, -0.8814952561688423893, 0.4721928772777359007 ) ) ;
#249591 = EDGE_CURVE ( 'NONE', #202185, #199945, #117535, .T. ) ;
#249592 = CIRCLE ( 'NONE', #191156, 11.89999999999999325 ) ;
#249593 = CARTESIAN_POINT ( 'NONE',  ( 20.12518398540832010, 66.02491127934493420, -195.5264392320576974 ) ) ;
#249594 = DIRECTION ( 'NONE',  ( 0.000000000000000000, -7.086529944415894657E-15, 1.000000000000000000 ) ) ;
#249595 = ADVANCED_FACE ( 'NONE', ( #180540 ), #56615, .T. ) ;
#249596 = VERTEX_POINT ( 'NONE', #65717 ) ;
#249597 = SPHERICAL_SURFACE ( 'NONE', #210706, 0.1000000000000000056 ) ;
#249598 = DIRECTION ( 'NONE',  ( 0.000000000000000000, 0.000000000000000000, -1.000000000000000000 ) ) ;
#249599 = AXIS2_PLACEMENT_3D ( 'NONE', #44829, #142622, #124377 ) ;
#249600 = ORIENTED_EDGE ( 'NONE', *, *, #222853, .F. ) ;
#249601 = AXIS2_PLACEMENT_3D ( 'NONE', #47414, #146509, #29205 ) ;
#249602 = ADVANCED_FACE ( 'NONE', ( #46150 ), #213193, .T. ) ;
#249604 = EDGE_CURVE ( 'NONE', #17954, #113101, #125892, .T. ) ;
#249603 = AXIS2_PLACEMENT_3D ( 'NONE', #99087, #176111, #178689 ) ;
#249605 = CARTESIAN_POINT ( 'NONE',  ( -21.55000000000000071, 68.65000000001205649, -124.1731074845243512 ) ) ;
#249606 = ORIENTED_EDGE ( 'NONE', *, *, #127659, .F. ) ;
#249607 = CARTESIAN_POINT ( 'NONE',  ( -16.89268316805466341, 66.04827818677041762, -190.8788599630699707 ) ) ;
#249608 = ORIENTED_EDGE ( 'NONE', *, *, #80169, .T. ) ;
#249609 = EDGE_CURVE ( 'NONE', #105369, #55681, #86533, .T. ) ;
#249610 = CARTESIAN_POINT ( 'NONE',  ( -23.25000000000000000, -11.74999999998884448, -63.89999999999999858 ) ) ;
#249612 = ORIENTED_EDGE ( 'NONE', *, *, #90594, .F. ) ;
#249611 = DIRECTION ( 'NONE',  ( 1.000000000000000000, -1.186688945009010077E-16, -8.286604613020808509E-31 ) ) ;
#249613 = AXIS2_PLACEMENT_3D ( 'NONE', #172189, #251670, #242369 ) ;
#249614 = AXIS2_PLACEMENT_3D ( 'NONE', #177044, #19226, #17932 ) ;
#249615 = ORIENTED_EDGE ( 'NONE', *, *, #195361, .F. ) ;
#249616 = CARTESIAN_POINT ( 'NONE',  ( 12.25000000000000000, 9.850000000011137402, -184.2499999999999716 ) ) ;
#249617 = ORIENTED_EDGE ( 'NONE', *, *, #247654, .T. ) ;
#249618 = ORIENTED_EDGE ( 'NONE', *, *, #64702, .F. ) ;
#249620 = ORIENTED_EDGE ( 'NONE', *, *, #244882, .T. ) ;
#249619 = CARTESIAN_POINT ( 'NONE',  ( 12.60053434924910221, 9.389534562357860992, -49.17480930438996012 ) ) ;
#249621 = EDGE_CURVE ( 'NONE', #22716, #232095, #95255, .T. ) ;
#249622 = CARTESIAN_POINT ( 'NONE',  ( -5.899999999999938183, 64.25000000001119815, -26.02310748452479316 ) ) ;
#249623 = ORIENTED_EDGE ( 'NONE', *, *, #105908, .F. ) ;
#249624 = VECTOR ( 'NONE', #55984, 1000.000000000000000 ) ;
#249625 = AXIS2_PLACEMENT_3D ( 'NONE', #29530, #127315, #231559 ) ;
#249626 = VECTOR ( 'NONE', #137449, 1000.000000000000114 ) ;
#249627 = AXIS2_PLACEMENT_3D ( 'NONE', #153848, #114667, #75568 ) ;
#249628 = EDGE_CURVE ( 'NONE', #70163, #40334, #159250, .T. ) ;
#249629 = EDGE_LOOP ( 'NONE', ( #73198, #93070, #99790, #103365 ) ) ;
#249630 = DIRECTION ( 'NONE',  ( 0.000000000000000000, 0.000000000000000000, -1.000000000000000000 ) ) ;
#249631 = DIRECTION ( 'NONE',  ( 0.000000000000000000, 0.4999999999999956701, -0.8660254037844411501 ) ) ;
#249633 = EDGE_CURVE ( 'NONE', #35508, #3992, #192551, .T. ) ;
#249632 = CARTESIAN_POINT ( 'NONE',  ( -18.41418431465368144, 37.99112772578840236, -261.0419300540664267 ) ) ;
#249634 = VERTEX_POINT ( 'NONE', #224776 ) ;
#249635 = LINE ( 'NONE', #128393, #171377 ) ;
#249636 = CARTESIAN_POINT ( 'NONE',  ( 21.05000000000000071, 69.25640205380743453, -247.7135141964517402 ) ) ;
#249637 = EDGE_CURVE ( 'NONE', #146487, #223782, #188272, .T. ) ;
#249638 = DIRECTION ( 'NONE',  ( -1.000000000000000000, 0.000000000000000000, 0.000000000000000000 ) ) ;
#249639 = EDGE_LOOP ( 'NONE', ( #103680, #86748, #33441, #76611 ) ) ;
#249640 = CARTESIAN_POINT ( 'NONE',  ( 23.24999999999999645, 5.600000000011153389, -79.40526601891313874 ) ) ;
#249641 = DIRECTION ( 'NONE',  ( -3.469446951953605354E-14, 1.000000000000000000, 0.000000000000000000 ) ) ;
#249642 = PRESENTATION_STYLE_ASSIGNMENT (( #133533 ) ) ;
#249643 = FACE_OUTER_BOUND ( 'NONE', #180055, .T. ) ;
#249644 = ORIENTED_EDGE ( 'NONE', *, *, #163545, .F. ) ;
#249645 = DIRECTION ( 'NONE',  ( 0.000000000000000000, 0.7092521942343630315, 0.7049548389604409770 ) ) ;
#249646 = VERTEX_POINT ( 'NONE', #25332 ) ;
#249648 = AXIS2_PLACEMENT_3D ( 'NONE', #63142, #64451, #143968 ) ;
#249647 = DIRECTION ( 'NONE',  ( 0.000000000000000000, 0.000000000000000000, -1.000000000000000000 ) ) ;
#249649 = ORIENTED_EDGE ( 'NONE', *, *, #68585, .T. ) ;
#249650 = DIRECTION ( 'NONE',  ( 0.000000000000000000, 0.2617529984165152257, 0.9651348961777124202 ) ) ;
#249651 = FACE_OUTER_BOUND ( 'NONE', #182913, .T. ) ;
#249652 = ORIENTED_EDGE ( 'NONE', *, *, #22098, .T. ) ;
#249653 = ORIENTED_EDGE ( 'NONE', *, *, #225705, .F. ) ;
#249654 = DIRECTION ( 'NONE',  ( 0.000000000000000000, 8.881784197002011602E-16, -1.000000000000000000 ) ) ;
#249655 = EDGE_CURVE ( 'NONE', #120342, #248652, #63132, .T. ) ;
#249656 = CARTESIAN_POINT ( 'NONE',  ( -20.85000000000000142, 79.28756800457986742, -196.2274082906208434 ) ) ;
#249657 = ORIENTED_EDGE ( 'NONE', *, *, #153169, .F. ) ;
#249658 = LINE ( 'NONE', #54010, #256101 ) ;
#249659 = CIRCLE ( 'NONE', #45463, 0.1000000000000002554 ) ;
#249660 = ORIENTED_EDGE ( 'NONE', *, *, #22934, .T. ) ;
#249661 = CARTESIAN_POINT ( 'NONE',  ( -33.72168855820451938, 66.05000000001228955, -157.3731074845244962 ) ) ;
#249662 = AXIS2_PLACEMENT_3D ( 'NONE', #199843, #40780, #159424 ) ;
#249663 = ORIENTED_EDGE ( 'NONE', *, *, #69175, .T. ) ;
#249664 = FACE_OUTER_BOUND ( 'NONE', #120147, .T. ) ;
#249665 = ADVANCED_FACE ( 'NONE', ( #183113 ), #223494, .F. ) ;
#249666 = CARTESIAN_POINT ( 'NONE',  ( -16.77779411503078677, 22.98773664223800139, -230.9446655867606637 ) ) ;
#249667 = CARTESIAN_POINT ( 'NONE',  ( -21.12230431290520016, 6.457566653304167126, -66.99479014831103996 ) ) ;
#249669 = EDGE_LOOP ( 'NONE', ( #252894, #154849, #52214, #206603 ) ) ;
#249668 = CARTESIAN_POINT ( 'NONE',  ( 20.94999999999999574, 0.4810385098657082859, -209.0827657365571213 ) ) ;
#249670 = DIRECTION ( 'NONE',  ( 0.000000000000000000, 0.000000000000000000, 1.000000000000000000 ) ) ;
#249671 = VECTOR ( 'NONE', #96153, 1000.000000000000000 ) ;
#249672 = CARTESIAN_POINT ( 'NONE',  ( 23.14999999999998437, 36.65892442174472876, -249.5511627012454596 ) ) ;
#249673 = DIRECTION ( 'NONE',  ( -1.000000000000000000, 2.952720810173289112E-16, 2.061873921506763405E-30 ) ) ;
#249674 = CIRCLE ( 'NONE', #245402, 0.09999999999999939493 ) ;
#249675 = LINE ( 'NONE', #111438, #36127 ) ;
#249676 = CARTESIAN_POINT ( 'NONE',  ( 23.40000000000005187, 74.16448838626247664, -47.62760213295649692 ) ) ;
#249677 = CARTESIAN_POINT ( 'NONE',  ( -21.65000000000000213, 7.708578643773852157, -155.2500000000000284 ) ) ;
#249678 = DIRECTION ( 'NONE',  ( 0.000000000000000000, 0.8814952561688442767, -0.4721928772777322925 ) ) ;
#249679 = EDGE_CURVE ( 'NONE', #82520, #187371, #196631, .T. ) ;
#249680 = DIRECTION ( 'NONE',  ( 1.000000000000000000, 0.000000000000000000, 0.000000000000000000 ) ) ;
#249681 = AXIS2_PLACEMENT_3D ( 'NONE', #181075, #7203, #2394 ) ;
#249682 = B_SPLINE_CURVE_WITH_KNOTS ( 'NONE', 3,
 ( #154635, #199858, #214563, #150752, #112911, #133746 ),
 .UNSPECIFIED., .F., .F.,
 ( 4, 2, 4 ),
 ( 0.000000000000000000, 0.0001895189928937394052, 0.0003790379857874788105 ),
 .UNSPECIFIED. ) ;
#249683 = ORIENTED_EDGE ( 'NONE', *, *, #112252, .T. ) ;
#249684 = VERTEX_POINT ( 'NONE', #141396 ) ;
#249685 = ORIENTED_EDGE ( 'NONE', *, *, #39151, .T. ) ;
#249686 =( BOUNDED_CURVE ( )  B_SPLINE_CURVE ( 3, ( #201441, #101010, #140168, #183186 ),
 .UNSPECIFIED., .F., .F. ) 
 B_SPLINE_CURVE_WITH_KNOTS ( ( 4, 4 ),
 ( 3.141592653589793116, 4.712388980384689674 ),
 .UNSPECIFIED. ) 
 CURVE ( )  GEOMETRIC_REPRESENTATION_ITEM ( )  RATIONAL_B_SPLINE_CURVE ( ( 1.000000000000000000, 0.8047378541243649375, 0.8047378541243649375, 1.000000000000000000 ) ) 
 REPRESENTATION_ITEM ( '' )  );
#249687 = DIRECTION ( 'NONE',  ( 1.000000000000000000, -0.000000000000000000, -0.000000000000000000 ) ) ;
#249688 = DIRECTION ( 'NONE',  ( -0.000000000000000000, 1.000000000000000000, 6.982962677686266711E-15 ) ) ;
#249689 = ORIENTED_EDGE ( 'NONE', *, *, #110518, .F. ) ;
#249690 = FACE_OUTER_BOUND ( 'NONE', #242998, .T. ) ;
#249691 = DIRECTION ( 'NONE',  ( -3.356945627403450689E-14, 0.9868171638914230437, 0.1618390714546045217 ) ) ;
#249692 = CARTESIAN_POINT ( 'NONE',  ( 21.14999999999999858, 76.10000000001268461, -203.5231074845243597 ) ) ;
#249693 = ORIENTED_EDGE ( 'NONE', *, *, #153176, .T. ) ;
#249694 = VERTEX_POINT ( 'NONE', #24045 ) ;
#249695 = DIRECTION ( 'NONE',  ( 0.000000000000000000, 0.9889818879709272315, 0.1480365673253073999 ) ) ;
#249696 = DIRECTION ( 'NONE',  ( 0.000000000000000000, -0.9126074666063660468, -0.4088369013363524762 ) ) ;
#249697 = ORIENTED_EDGE ( 'NONE', *, *, #96693, .F. ) ;
#249698 = DIRECTION ( 'NONE',  ( -1.000000000000000000, 0.000000000000000000, 0.000000000000000000 ) ) ;
#249700 = EDGE_LOOP ( 'NONE', ( #252547, #190874, #42169, #197462 ) ) ;
#249699 = DIRECTION ( 'NONE',  ( 0.000000000000000000, 0.9908441862701791170, 0.1350103645450472789 ) ) ;
#249701 = CARTESIAN_POINT ( 'NONE',  ( -21.05000000000000071, -11.29603075032412463, -97.45210084033617193 ) ) ;
#249702 = DIRECTION ( 'NONE',  ( 0.000000000000000000, 7.086529944415894657E-15, -1.000000000000000000 ) ) ;
#249704 = ORIENTED_EDGE ( 'NONE', *, *, #101636, .T. ) ;
#249703 = CARTESIAN_POINT ( 'NONE',  ( -16.77683809663752257, 48.78215419113038109, -213.4964773079645681 ) ) ;
#249705 = CARTESIAN_POINT ( 'NONE',  ( 20.84999999999998721, 11.75000000001115552, -67.00000000000000000 ) ) ;
#249706 = CARTESIAN_POINT ( 'NONE',  ( -21.44999999999999929, 7.349999999999998757, -12.25000000000000000 ) ) ;
#249707 = EDGE_CURVE ( 'NONE', #65618, #25637, #17560, .T. ) ;
#249708 = DIRECTION ( 'NONE',  ( 0.000000000000000000, 0.000000000000000000, -1.000000000000000000 ) ) ;
#249709 = CYLINDRICAL_SURFACE ( 'NONE', #144134, 0.09999999999999811817 ) ;
#249710 = AXIS2_PLACEMENT_3D ( 'NONE', #59280, #158457, #138822 ) ;
#249713 = CARTESIAN_POINT ( 'NONE',  ( 21.13461538461538680, 8.885417037985614996, -179.8499999999999943 ) ) ;
#249712 = TOROIDAL_SURFACE ( 'NONE', #195577, 11.65000000000000036, 0.1000000000000000056 ) ;
#249711 = CARTESIAN_POINT ( 'NONE',  ( -23.25000000000000000, 64.25000000001222134, -148.6731074845244507 ) ) ;
#249714 = CARTESIAN_POINT ( 'NONE',  ( -22.39999999999999858, 65.19201463318205469, -243.3742797652979561 ) ) ;
#249715 = CIRCLE ( 'NONE', #8115, 0.1000000000000028644 ) ;
#249716 = AXIS2_PLACEMENT_3D ( 'NONE', #4998, #62442, #160282 ) ;
#249717 = DIRECTION ( 'NONE',  ( -1.000000000000000000, 0.000000000000000000, 0.000000000000000000 ) ) ;
#249718 = DIRECTION ( 'NONE',  ( -1.000000000000000000, -0.000000000000000000, -0.000000000000000000 ) ) ;
#249719 =( BOUNDED_SURFACE ( )  B_SPLINE_SURFACE ( 3, 2, ( 
 ( #88691, #48308, #129137 ),
 ( #232103, #91297, #170883 ),
 ( #173454, #53449, #127860 ),
 ( #14351, #10475, #93849 ) ),
 .UNSPECIFIED., .F., .F., .F. ) 
 B_SPLINE_SURFACE_WITH_KNOTS ( ( 4, 4 ),
 ( 3, 3 ),
 ( 0.0006461284895273970708, 0.0007503702773986317210 ),
 ( 0.000000000000000000, 1.000000000000000000 ),
 .UNSPECIFIED. ) 
 GEOMETRIC_REPRESENTATION_ITEM ( )  RATIONAL_B_SPLINE_SURFACE ( (
 ( 1.000000000000000000, 0.7071067811865475727, 1.000000000000000000),
 ( 1.000000000000000000, 0.7076476444648772679, 1.000000000000000000),
 ( 1.000000000000000000, 0.7075727925191758194, 1.000000000000000000),
 ( 1.000000000000000000, 0.7071067811865475727, 1.000000000000000000) ) ) 
 REPRESENTATION_ITEM ( '' )  SURFACE ( )  );
#249720 = ORIENTED_EDGE ( 'NONE', *, *, #250248, .T. ) ;
#249721 = FACE_OUTER_BOUND ( 'NONE', #98652, .T. ) ;
#249722 = CIRCLE ( 'NONE', #224759, 0.09999999999998898659 ) ;
#249723 = ORIENTED_EDGE ( 'NONE', *, *, #171828, .T. ) ;
#249724 = CARTESIAN_POINT ( 'NONE',  ( 20.94999999999999574, 8.926614585098251453, -75.47168301922316402 ) ) ;
#249725 = EDGE_LOOP ( 'NONE', ( #233576, #256764, #121281, #254005 ) ) ;
#249726 = ADVANCED_FACE ( 'NONE', ( #44876 ), #61875, .T. ) ;
#249727 = DIRECTION ( 'NONE',  ( 1.000000000000000000, 0.000000000000000000, 0.000000000000000000 ) ) ;
#249728 = EDGE_CURVE ( 'NONE', #191282, #223911, #47421, .T. ) ;
#249729 = CIRCLE ( 'NONE', #183110, 7.800000000000001599 ) ;
#249730 = EDGE_LOOP ( 'NONE', ( #177550, #121239, #242824, #221161 ) ) ;
#249731 = AXIS2_PLACEMENT_3D ( 'NONE', #241861, #206592, #63209 ) ;
#249732 = CARTESIAN_POINT ( 'NONE',  ( 18.49999999999999645, 67.23127455305835554, -235.8551265064784559 ) ) ;
#249733 = EDGE_CURVE ( 'NONE', #139747, #148869, #124422, .T. ) ;
#249734 = ORIENTED_EDGE ( 'NONE', *, *, #238626, .F. ) ;
#249735 = AXIS2_PLACEMENT_3D ( 'NONE', #176966, #232117, #256400 ) ;
#249736 = ORIENTED_EDGE ( 'NONE', *, *, #238438, .F. ) ;
#249737 = ADVANCED_FACE ( 'NONE', ( #164831 ), #96652, .F. ) ;
#249738 = CARTESIAN_POINT ( 'NONE',  ( 21.05000000000000071, -8.999999999988842703, -90.60603087734760663 ) ) ;
#249739 = CARTESIAN_POINT ( 'NONE',  ( 21.05000000000000071, 10.62872031401550288, -41.16491356908760224 ) ) ;
#249740 = CARTESIAN_POINT ( 'NONE',  ( -18.40000000000000213, 64.52683809664938508, -90.47310748452439100 ) ) ;
#249741 = DIRECTION ( 'NONE',  ( 0.000000000000000000, 0.000000000000000000, -1.000000000000000000 ) ) ;
#249742 = DIRECTION ( 'NONE',  ( -1.000000000000000000, 0.000000000000000000, 0.000000000000000000 ) ) ;
#249744 = DIRECTION ( 'NONE',  ( 1.000000000000000000, 3.265361837132813093E-16, -0.000000000000000000 ) ) ;
#249743 = CARTESIAN_POINT ( 'NONE',  ( -23.15000000000000213, 16.98881331171929787, -224.4946931418895417 ) ) ;
#249745 = CARTESIAN_POINT ( 'NONE',  ( 18.56308993302899069, 10.38069115533549969, -58.23922263893885543 ) ) ;
#249747 = EDGE_LOOP ( 'NONE', ( #156152, #41540, #100133, #215773 ) ) ;
#249746 = CARTESIAN_POINT ( 'NONE',  ( -20.93302460841142931, 10.31565961587945424, -139.5364194119178478 ) ) ;
#249749 = DIRECTION ( 'NONE',  ( 0.000000000000000000, 0.1686199900910448357, -0.9856811345164804283 ) ) ;
#249748 = CARTESIAN_POINT ( 'NONE',  ( 20.30531438145591139, 10.09690106110208596, -74.79601780727338678 ) ) ;
#249750 = ADVANCED_FACE ( 'NONE', ( #102236 ), #149129, .T. ) ;
#249751 = DIRECTION ( 'NONE',  ( 0.000000000000000000, -6.982962677686266711E-15, 1.000000000000000000 ) ) ;
#249752 = EDGE_LOOP ( 'NONE', ( #254652, #24519, #73149, #203764 ) ) ;
#249753 = CARTESIAN_POINT ( 'NONE',  ( -18.43473496883423124, -9.494952410988105385, -174.5458715722282079 ) ) ;
#249754 = LINE ( 'NONE', #149396, #251846 ) ;
#249755 = CARTESIAN_POINT ( 'NONE',  ( 21.05000000000000071, 1.115625160336667635E-11, -98.50000000000004263 ) ) ;
#249756 = EDGE_LOOP ( 'NONE', ( #212116, #192500, #251451, #96943 ) ) ;
#249757 = EDGE_CURVE ( 'NONE', #255281, #89873, #34183, .T. ) ;
#249758 = CARTESIAN_POINT ( 'NONE',  ( 18.49999999999999289, 52.91185528119410009, -244.1460391050142675 ) ) ;
#249759 = AXIS2_PLACEMENT_3D ( 'NONE', #48114, #185058, #127666 ) ;
#249760 = DIRECTION ( 'NONE',  ( 1.000000000000000000, 0.000000000000000000, 0.000000000000000000 ) ) ;
#249761 = CARTESIAN_POINT ( 'NONE',  ( 14.77516762759920788, 66.56332574816902081, -87.84624555352516495 ) ) ;
#249762 = ORIENTED_EDGE ( 'NONE', *, *, #4826, .T. ) ;
#249763 = ORIENTED_EDGE ( 'NONE', *, *, #12914, .T. ) ;
#249764 = CARTESIAN_POINT ( 'NONE',  ( -20.64999999999999858, 2.400000000011155432, -113.7246219227621395 ) ) ;
#249766 = CARTESIAN_POINT ( 'NONE',  ( -18.59117750673696889, 10.33248238083634796, -173.0948465439131496 ) ) ;
#249765 = AXIS2_PLACEMENT_3D ( 'NONE', #56307, #38070, #177596 ) ;
#249767 = CARTESIAN_POINT ( 'NONE',  ( -20.54999999999999716, 1.115600667400684642E-11, -200.9999999999999432 ) ) ;
#249768 = FACE_OUTER_BOUND ( 'NONE', #193995, .T. ) ;
#249769 = EDGE_LOOP ( 'NONE', ( #223395, #41949, #72800 ) ) ;
#249770 = EDGE_CURVE ( 'NONE', #15173, #35759, #142465, .T. ) ;
#249771 = DIRECTION ( 'NONE',  ( 1.000000000000000000, -0.000000000000000000, -0.000000000000000000 ) ) ;
#249772 = CARTESIAN_POINT ( 'NONE',  ( -18.59999999999999787, 42.96960653111219131, -254.4772109693542745 ) ) ;
#249773 = FACE_OUTER_BOUND ( 'NONE', #216604, .T. ) ;
#249774 = DIRECTION ( 'NONE',  ( 0.000000000000000000, -0.9274965247785555977, 0.3738317757009190223 ) ) ;
#249775 = VECTOR ( 'NONE', #208780, 1000.000000000000000 ) ;
#249776 = EDGE_LOOP ( 'NONE', ( #29700, #94219, #20556 ) ) ;
#249778 = CARTESIAN_POINT ( 'NONE',  ( 20.88420186297724257, 10.33025634371521662, -39.08709292826387838 ) ) ;
#249777 = AXIS2_PLACEMENT_3D ( 'NONE', #253046, #74456, #154010 ) ;
#249779 = ADVANCED_FACE ( 'NONE', ( #111274 ), #92984, .F. ) ;
#249781 = ORIENTED_EDGE ( 'NONE', *, *, #157193, .F. ) ;
#249780 = CARTESIAN_POINT ( 'NONE',  ( -16.93521499325732549, 66.00521388020827374, -82.11599894343083861 ) ) ;
#249782 = CARTESIAN_POINT ( 'NONE',  ( 22.39999999999999503, 64.35000000001267040, -203.6231074845244393 ) ) ;
#249783 = FACE_OUTER_BOUND ( 'NONE', #27257, .T. ) ;
#249784 = AXIS2_PLACEMENT_3D ( 'NONE', #227612, #188490, #28170 ) ;
#249785 = DIRECTION ( 'NONE',  ( 1.000000000000000000, 0.000000000000000000, 0.000000000000000000 ) ) ;
#249786 = CARTESIAN_POINT ( 'NONE',  ( -21.55000000000000426, 7.750000000011155521, -146.3500000000000227 ) ) ;
#249787 = EDGE_LOOP ( 'NONE', ( #171127, #15987, #69156, #123438 ) ) ;
#249788 = CARTESIAN_POINT ( 'NONE',  ( 21.11345278033283179, 8.882122073370972259, -12.24602217075528010 ) ) ;
#249789 = CIRCLE ( 'NONE', #45604, 2.000000000000002665 ) ;
#249790 = DIRECTION ( 'NONE',  ( -0.000000000000000000, -6.982962677686266711E-15, 1.000000000000000000 ) ) ;
#249791 = DIRECTION ( 'NONE',  ( -1.000000000000000000, 0.000000000000000000, 0.000000000000000000 ) ) ;
#249792 = AXIS2_PLACEMENT_3D ( 'NONE', #227060, #30177, #10601 ) ;
#249793 = EDGE_LOOP ( 'NONE', ( #148013, #99113, #107631, #125235 ) ) ;
#249794 = DIRECTION ( 'NONE',  ( 1.000000000000000000, 1.186688945009009831E-16, 0.000000000000000000 ) ) ;
#249795 = DIRECTION ( 'NONE',  ( -1.000000000000000000, 0.000000000000000000, 0.000000000000000000 ) ) ;
#249796 = CARTESIAN_POINT ( 'NONE',  ( -16.87786941232801041, 51.64033894800659397, -231.9279124044847151 ) ) ;
#249797 = ADVANCED_FACE ( 'NONE', ( #229932 ), #90409, .F. ) ;
#249798 = CARTESIAN_POINT ( 'NONE',  ( -23.25000000000000000, 1.115600667400684642E-11, -100.5000000000000426 ) ) ;
#249799 = EDGE_CURVE ( 'NONE', #150463, #217530, #52564, .T. ) ;
#249801 = DIRECTION ( 'NONE',  ( 1.000000000000000000, 0.000000000000000000, 0.000000000000000000 ) ) ;
#249800 = CIRCLE ( 'NONE', #178917, 0.09999999999999971412 ) ;
#249802 = VECTOR ( 'NONE', #65754, 1000.000000000000114 ) ;
#249804 = ORIENTED_EDGE ( 'NONE', *, *, #206969, .F. ) ;
#249803 = AXIS2_PLACEMENT_3D ( 'NONE', #86149, #44503, #181450 ) ;
#249805 = VERTEX_POINT ( 'NONE', #112566 ) ;
#249806 = AXIS2_PLACEMENT_3D ( 'NONE', #173098, #93503, #178206 ) ;
#249807 = AXIS2_PLACEMENT_3D ( 'NONE', #67390, #146903, #243453 ) ;
#249808 = CARTESIAN_POINT ( 'NONE',  ( 21.14999999999998082, 87.75000000001213607, -136.5231074845242176 ) ) ;
#249809 = CARTESIAN_POINT ( 'NONE',  ( -17.78043020864321733, 62.81909162847866668, -210.6586991758544798 ) ) ;
#249810 = DIRECTION ( 'NONE',  ( 0.000000000000000000, -0.8814952561688429444, 0.4721928772777347905 ) ) ;
#249811 = CIRCLE ( 'NONE', #187287, 2.099999999999998312 ) ;
#249812 = EDGE_CURVE ( 'NONE', #160776, #197503, #243224, .T. ) ;
#249813 = DIRECTION ( 'NONE',  ( 1.000000000000000000, 0.000000000000000000, 0.000000000000000000 ) ) ;
#249814 = CARTESIAN_POINT ( 'NONE',  ( -21.78635804494510708, 7.035661485164336426, -133.9009949344923314 ) ) ;
#249815 = CARTESIAN_POINT ( 'NONE',  ( 21.76363531954645936, 7.012936547871724713, 0.09900187429945014883 ) ) ;
#249816 = EDGE_CURVE ( 'NONE', #229988, #78573, #167413, .T. ) ;
#249818 = ADVANCED_FACE ( 'NONE', ( #210378 ), #13268, .T. ) ;
#249817 = DIRECTION ( 'NONE',  ( 0.000000000000000000, -0.4088369013363276072, 0.9126074666063772600 ) ) ;
#249819 = CARTESIAN_POINT ( 'NONE',  ( -16.94037747912386394, 10.01353938249748765, -113.0511309579755306 ) ) ;
#249820 = FACE_OUTER_BOUND ( 'NONE', #184375, .T. ) ;
#249821 = ORIENTED_EDGE ( 'NONE', *, *, #109820, .F. ) ;
#249822 = CARTESIAN_POINT ( 'NONE',  ( -21.05000000000000071, 77.16270174995064224, -195.4231074845243370 ) ) ;
#249823 = EDGE_CURVE ( 'NONE', #199182, #145487, #200743, .T. ) ;
#249824 = ORIENTED_EDGE ( 'NONE', *, *, #107633, .F. ) ;
#249825 = DIRECTION ( 'NONE',  ( 1.000000000000000000, 0.000000000000000000, -0.000000000000000000 ) ) ;
#249826 = DIRECTION ( 'NONE',  ( 0.000000000000000000, 0.000000000000000000, -1.000000000000000000 ) ) ;
#249827 = CARTESIAN_POINT ( 'NONE',  ( 21.12802099929860944, 8.780552590233368093, -79.24818998493165623 ) ) ;
#249828 = CYLINDRICAL_SURFACE ( 'NONE', #103015, 0.09999999999999939493 ) ;
#249829 = SURFACE_STYLE_FILL_AREA ( #174187 ) ;
#249830 = FACE_OUTER_BOUND ( 'NONE', #21193, .T. ) ;
#249831 = DIRECTION ( 'NONE',  ( -1.000000000000000000, 0.000000000000000000, 0.000000000000000000 ) ) ;
#249833 = ORIENTED_EDGE ( 'NONE', *, *, #182176, .T. ) ;
#249832 = AXIS2_PLACEMENT_3D ( 'NONE', #29603, #115206, #17395 ) ;
#249834 = LINE ( 'NONE', #47755, #149684 ) ;
#249835 = CYLINDRICAL_SURFACE ( 'NONE', #38173, 0.1000000000000028644 ) ;
#249836 = AXIS2_PLACEMENT_3D ( 'NONE', #129046, #204707, #31266 ) ;
#249837 = CARTESIAN_POINT ( 'NONE',  ( -20.94999999999999929, 56.16603649944111254, -228.1013850343386764 ) ) ;
#249838 = CARTESIAN_POINT ( 'NONE',  ( -21.64999999999999858, 7.249999999999992895, -12.25000000000000000 ) ) ;
#249839 = CIRCLE ( 'NONE', #145769, 0.1000000000000028644 ) ;
#249840 = ORIENTED_EDGE ( 'NONE', *, *, #10747, .T. ) ;
#249841 = CARTESIAN_POINT ( 'NONE',  ( 23.14999999999999858, 71.00000000001180922, -81.92837350343744163 ) ) ;
#249842 = PLANE ( 'NONE',  #87622 ) ;
#249843 = ORIENTED_EDGE ( 'NONE', *, *, #148057, .F. ) ;
#249844 = ADVANCED_FACE ( 'NONE', ( #168724 ), #10895, .F. ) ;
#249845 = ADVANCED_FACE ( 'NONE', ( #109971 ), #46261, .T. ) ;
#249846 = ORIENTED_EDGE ( 'NONE', *, *, #161784, .T. ) ;
#249847 = FACE_OUTER_BOUND ( 'NONE', #90495, .T. ) ;
#249848 = LINE ( 'NONE', #50335, #202329 ) ;
#249849 = AXIS2_PLACEMENT_3D ( 'NONE', #208135, #205528, #26936 ) ;
#249850 = CIRCLE ( 'NONE', #116578, 0.09999999999999939493 ) ;
#249851 = ORIENTED_EDGE ( 'NONE', *, *, #138552, .F. ) ;
#249852 = DIRECTION ( 'NONE',  ( 1.000000000000000000, 0.000000000000000000, 0.000000000000000000 ) ) ;
#249853 = CARTESIAN_POINT ( 'NONE',  ( -20.94999999999999929, 67.85909929089923764, -227.8797997985275856 ) ) ;
#249854 = EDGE_CURVE ( 'NONE', #133612, #176502, #63347, .T. ) ;
#249855 = VERTEX_POINT ( 'NONE', #255863 ) ;
#249856 = CIRCLE ( 'NONE', #79148, 0.1000000000000075273 ) ;
#249857 = CARTESIAN_POINT ( 'NONE',  ( -18.50000000000000000, 77.73625713160970463, -158.4544551555068495 ) ) ;
#249858 = ORIENTED_EDGE ( 'NONE', *, *, #117747, .T. ) ;
#249859 = DIRECTION ( 'NONE',  ( -1.836970198721029934E-16, -1.000000000000000000, -6.982962677686266711E-15 ) ) ;
#249860 = CARTESIAN_POINT ( 'NONE',  ( -18.50000000000000000, 85.50000000001189449, -94.92310748452425173 ) ) ;
#249862 = ORIENTED_EDGE ( 'NONE', *, *, #116787, .T. ) ;
#249861 = LINE ( 'NONE', #132482, #249938 ) ;
#249863 = DIRECTION ( 'NONE',  ( 0.000000000000000000, 0.000000000000000000, -1.000000000000000000 ) ) ;
#249864 = LINE ( 'NONE', #71248, #140590 ) ;
#249865 = CYLINDRICAL_SURFACE ( 'NONE', #255800, 0.09999999999999939493 ) ;
#249866 = CARTESIAN_POINT ( 'NONE',  ( 20.94999999999999929, 77.16412189325360771, -162.1082593989527254 ) ) ;
#249867 = CARTESIAN_POINT ( 'NONE',  ( 20.85000000000000142, 43.24695311518262031, -245.0026972281755491 ) ) ;
#249868 = CARTESIAN_POINT ( 'NONE',  ( -16.80438519320023616, 66.05022090354395914, -157.3723692036031423 ) ) ;
#249870 = ORIENTED_EDGE ( 'NONE', *, *, #79395, .T. ) ;
#249869 = DIRECTION ( 'NONE',  ( 0.000000000000000000, -0.4088369013363783999, 0.9126074666063545004 ) ) ;
#249871 = ORIENTED_EDGE ( 'NONE', *, *, #4987, .F. ) ;
#249874 = CARTESIAN_POINT ( 'NONE',  ( -15.31895204843005232, 9.396533993965077158, -84.90593977917338009 ) ) ;
#249873 = CARTESIAN_POINT ( 'NONE',  ( 18.59999999999999787, 76.00000000001165290, -69.52310748452431710 ) ) ;
#249872 = AXIS2_PLACEMENT_3D ( 'NONE', #248584, #128652, #212044 ) ;
#249875 = AXIS2_PLACEMENT_3D ( 'NONE', #164594, #5478, #83719 ) ;
#249877 = ORIENTED_EDGE ( 'NONE', *, *, #54820, .F. ) ;
#249876 = DIRECTION ( 'NONE',  ( 0.000000000000000000, 1.776356839400250070E-15, 1.000000000000000000 ) ) ;
#249878 = EDGE_CURVE ( 'NONE', #68808, #77018, #242421, .T. ) ;
#249879 = ORIENTED_EDGE ( 'NONE', *, *, #246327, .T. ) ;
#249880 = LINE ( 'NONE', #71265, #20883 ) ;
#249881 = CARTESIAN_POINT ( 'NONE',  ( 20.04142135623730070, 11.65000000001115943, -121.8500000000000369 ) ) ;
#249882 = DIRECTION ( 'NONE',  ( 0.000000000000000000, -0.9126074666063771490, -0.4088369013363281623 ) ) ;
#249883 = DIRECTION ( 'NONE',  ( 0.000000000000000000, 0.2617529984165031243, 0.9651348961777157509 ) ) ;
#249884 = EDGE_CURVE ( 'NONE', #57087, #90690, #195960, .T. ) ;
#249885 = CARTESIAN_POINT ( 'NONE',  ( 20.94999999999999574, -11.64999999999999147, -2.900000000000003464 ) ) ;
#249886 = CARTESIAN_POINT ( 'NONE',  ( 22.10000000000000142, 3.461118860469513336, 28.84309995045515507 ) ) ;
#249887 = EDGE_CURVE ( 'NONE', #110167, #171376, #193397, .T. ) ;
#249888 = AXIS2_PLACEMENT_3D ( 'NONE', #111305, #68326, #227385 ) ;
#249889 = ORIENTED_EDGE ( 'NONE', *, *, #66590, .T. ) ;
#249890 = VERTEX_POINT ( 'NONE', #75994 ) ;
#249891 = CIRCLE ( 'NONE', #99829, 0.09999999999999918676 ) ;
#249892 = EDGE_CURVE ( 'NONE', #72309, #94186, #244416, .T. ) ;
#249893 = CARTESIAN_POINT ( 'NONE',  ( 20.99999999999999645, 9.750000000011137757, -146.6500000000000341 ) ) ;
#249894 = AXIS2_PLACEMENT_3D ( 'NONE', #19902, #156863, #57711 ) ;
#249895 = VECTOR ( 'NONE', #2134, 1000.000000000000000 ) ;
#249896 = ORIENTED_EDGE ( 'NONE', *, *, #233898, .T. ) ;
#249897 = B_SPLINE_CURVE_WITH_KNOTS ( 'NONE', 3,
 ( #64393, #47373, #223445, #128221, #126934, #206468, #27866, #124373, #82628, #186934, #87780, #167370, #246864, #233747, #72107, #212892, #248164, #69544, #150358, #55066, #214173, #249463, #35561, #149081, #134606, #188194 ),
 .UNSPECIFIED., .F., .F.,
 ( 4, 2, 2, 2, 2, 2, 2, 2, 2, 2, 2, 2, 4 ),
 ( 0.005476422646581353450, 0.006160811967703588680, 0.006845201288825822176, 0.007187395949386924179, 0.007529590609948026182, 0.007871785270509128185, 0.008213979931070231055, 0.008556174591631333926, 0.008898369252192435061, 0.009240563912753536197, 0.009582758573314639067, 0.01026714789443684134, 0.01095153721555904534 ),
 .UNSPECIFIED. ) ;
#249898 = DIRECTION ( 'NONE',  ( 0.000000000000000000, 0.000000000000000000, -1.000000000000000000 ) ) ;
#249899 = VERTEX_POINT ( 'NONE', #178990 ) ;
#249900 = FACE_OUTER_BOUND ( 'NONE', #201220, .T. ) ;
#249901 = EDGE_CURVE ( 'NONE', #116241, #90831, #105009, .T. ) ;
#249902 = AXIS2_PLACEMENT_3D ( 'NONE', #212287, #210990, #216105 ) ;
#249904 = EDGE_CURVE ( 'NONE', #167959, #220534, #95551, .T. ) ;
#249903 = ADVANCED_FACE ( 'NONE', ( #36907 ), #138356, .T. ) ;
#249905 = DIRECTION ( 'NONE',  ( 0.000000000000000000, -1.000000000000000000, 0.000000000000000000 ) ) ;
#249906 = DIRECTION ( 'NONE',  ( -1.000000000000000000, 0.000000000000000000, 0.000000000000000000 ) ) ;
#249907 = EDGE_LOOP ( 'NONE', ( #153836, #239555, #13978, #171294, #120731 ) ) ;
#249908 = DIRECTION ( 'NONE',  ( 1.000000000000000000, 0.000000000000000000, 0.000000000000000000 ) ) ;
#249909 = ORIENTED_EDGE ( 'NONE', *, *, #244181, .F. ) ;
#249910 = AXIS2_PLACEMENT_3D ( 'NONE', #124698, #142943, #43874 ) ;
#249911 = DIRECTION ( 'NONE',  ( 0.000000000000000000, 0.9126074666063545004, 0.4088369013363783999 ) ) ;
#249913 = VECTOR ( 'NONE', #131563, 1000.000000000000000 ) ;
#249912 = CARTESIAN_POINT ( 'NONE',  ( 18.49999999999997158, 9.105964803472787139, -245.3658845043482586 ) ) ;
#249914 = ORIENTED_EDGE ( 'NONE', *, *, #244800, .F. ) ;
#249915 = DIRECTION ( 'NONE',  ( 0.000000000000000000, 1.000000000000000000, 0.000000000000000000 ) ) ;
#249916 = EDGE_LOOP ( 'NONE', ( #39220, #234203, #175805, #43625, #149559, #175164, #80838, #139643 ) ) ;
#249919 = ORIENTED_EDGE ( 'NONE', *, *, #205326, .F. ) ;
#249918 = DIRECTION ( 'NONE',  ( 0.000000000000000000, 0.000000000000000000, 1.000000000000000000 ) ) ;
#249917 = CARTESIAN_POINT ( 'NONE',  ( 21.05000000000000071, 1.115600667400684642E-11, -164.6000000000000227 ) ) ;
#249920 = ADVANCED_FACE ( 'NONE', ( #175148 ), #76029, .T. ) ;
#249921 = LINE ( 'NONE', #71305, #89596 ) ;
#249922 = EDGE_CURVE ( 'NONE', #126775, #90553, #236350, .T. ) ;
#249923 = ORIENTED_EDGE ( 'NONE', *, *, #154257, .T. ) ;
#249924 = DIRECTION ( 'NONE',  ( -1.000000000000000000, 0.000000000000000000, 0.000000000000000000 ) ) ;
#249925 = ORIENTED_EDGE ( 'NONE', *, *, #249238, .T. ) ;
#249926 = EDGE_CURVE ( 'NONE', #215045, #123093, #216779, .T. ) ;
#249927 = CARTESIAN_POINT ( 'NONE',  ( -20.64999999999999858, 76.00000000001126921, -203.5231074845248997 ) ) ;
#249928 = VERTEX_POINT ( 'NONE', #159395 ) ;
#249929 = CARTESIAN_POINT ( 'NONE',  ( 21.05000000000000071, 18.81732247075047582, -230.0377732242114632 ) ) ;
#249930 = LINE ( 'NONE', #149568, #97050 ) ;
#249931 = CARTESIAN_POINT ( 'NONE',  ( 18.50596464788227280, 67.49374512151688066, -195.5131169347613707 ) ) ;
#249932 = CARTESIAN_POINT ( 'NONE',  ( 23.14999999999999503, 45.25174493058054281, -238.5244480634700324 ) ) ;
#249933 = ADVANCED_FACE ( 'NONE', ( #60270 ), #139797, .T. ) ;
#249934 = ORIENTED_EDGE ( 'NONE', *, *, #84324, .T. ) ;
#249936 = EDGE_CURVE ( 'NONE', #17057, #133463, #151047, .T. ) ;
#249935 = CARTESIAN_POINT ( 'NONE',  ( -16.93339986808596720, 44.03628838426681824, -235.2829882368675101 ) ) ;
#249937 = CARTESIAN_POINT ( 'NONE',  ( 21.09316766718127667, 6.370153312485568264, -33.46073659768530462 ) ) ;
#249938 = VECTOR ( 'NONE', #230287, 1000.000000000000000 ) ;
#249939 = ORIENTED_EDGE ( 'NONE', *, *, #84312, .T. ) ;
#249940 = CARTESIAN_POINT ( 'NONE',  ( -22.14074124539699895, 0.09905289584407227232, 7.390077851043765911 ) ) ;
#249941 = ORIENTED_EDGE ( 'NONE', *, *, #202191, .T. ) ;
#249942 = CARTESIAN_POINT ( 'NONE',  ( -21.59780538579341069, 33.76925247340353309, -243.3429228916662623 ) ) ;
#249943 = ORIENTED_EDGE ( 'NONE', *, *, #35266, .F. ) ;
#249944 = CARTESIAN_POINT ( 'NONE',  ( -23.39999999999994529, 83.98667523412385094, -37.28476067066772970 ) ) ;
#249945 = DIRECTION ( 'NONE',  ( 1.000000000000000000, 0.000000000000000000, 0.000000000000000000 ) ) ;
#249946 = CIRCLE ( 'NONE', #37581, 0.09999999999998898659 ) ;
#249948 = ORIENTED_EDGE ( 'NONE', *, *, #73916, .T. ) ;
#249947 = CARTESIAN_POINT ( 'NONE',  ( -16.77308656112214891, 44.13565801420894985, -235.2988526227105410 ) ) ;
#249949 = ADVANCED_FACE ( 'NONE', ( #23755 ), #185361, .F. ) ;
#249950 = DIRECTION ( 'NONE',  ( 1.000000000000000000, 3.265361837132813093E-16, -0.000000000000000000 ) ) ;
#249951 = ORIENTED_EDGE ( 'NONE', *, *, #1617, .T. ) ;
#249952 = CARTESIAN_POINT ( 'NONE',  ( -21.29999999999995808, 76.00000000001195133, -103.0231074845243171 ) ) ;
#249953 = CARTESIAN_POINT ( 'NONE',  ( -0.8999999999999430678, 63.75000000001118394, -10.02310748452479139 ) ) ;
#249954 = ORIENTED_EDGE ( 'NONE', *, *, #250668, .T. ) ;
#249955 = ADVANCED_FACE ( 'NONE', ( #44577 ), #83652, .T. ) ;
#249956 = CARTESIAN_POINT ( 'NONE',  ( 22.00411653962159519, 68.74655713164250415, -203.6221455902930302 ) ) ;
#249957 = CARTESIAN_POINT ( 'NONE',  ( -21.65000000000000213, 10.13883017033223943, -211.3290274220034632 ) ) ;
#249958 = ORIENTED_EDGE ( 'NONE', *, *, #54167, .F. ) ;
#249959 = DIRECTION ( 'NONE',  ( 0.000000000000000000, 0.000000000000000000, -1.000000000000000000 ) ) ;
#249960 = AXIS2_PLACEMENT_3D ( 'NONE', #185066, #106802, #246329 ) ;
#249961 = ORIENTED_EDGE ( 'NONE', *, *, #191362, .T. ) ;
#249962 = CARTESIAN_POINT ( 'NONE',  ( 12.48201962039796520, 9.376659938544690931, -118.1281925482173421 ) ) ;
#249963 = CARTESIAN_POINT ( 'NONE',  ( -18.49513951962167013, -9.437725026666541339, -73.77807257502912819 ) ) ;
#249964 = VECTOR ( 'NONE', #116369, 1000.000000000000000 ) ;
#249965 = EDGE_CURVE ( 'NONE', #170630, #126736, #25030, .T. ) ;
#249966 = TOROIDAL_SURFACE ( 'NONE', #166608, 0.2000000000000000111, 0.1000000000000000056 ) ;
#249967 = VECTOR ( 'NONE', #181240, 1000.000000000000000 ) ;
#249970 = ORIENTED_EDGE ( 'NONE', *, *, #131614, .T. ) ;
#249969 = EDGE_LOOP ( 'NONE', ( #128431, #227002, #200176, #245787 ) ) ;
#249968 = DIRECTION ( 'NONE',  ( 0.000000000000000000, 0.000000000000000000, -1.000000000000000000 ) ) ;
#249971 = FACE_OUTER_BOUND ( 'NONE', #130377, .T. ) ;
#249972 = DIRECTION ( 'NONE',  ( -0.000000000000000000, 0.000000000000000000, 1.000000000000000000 ) ) ;
#249973 = DIRECTION ( 'NONE',  ( 0.000000000000000000, 1.000000000000000000, 0.000000000000000000 ) ) ;
#249975 = CARTESIAN_POINT ( 'NONE',  ( -20.94999999999999929, 67.63082410804655353, -211.8415745842588649 ) ) ;
#249974 = CARTESIAN_POINT ( 'NONE',  ( 22.48508240969612615, 0.04627641452807085970, -88.84998926842646938 ) ) ;
#249976 = CARTESIAN_POINT ( 'NONE',  ( 23.15000000000000213, 87.75000000001229239, -157.8731074845242688 ) ) ;
#249977 = CYLINDRICAL_SURFACE ( 'NONE', #156820, 0.09999999999999939493 ) ;
#249978 = CARTESIAN_POINT ( 'NONE',  ( 20.94999999999999929, 1.115600667400684642E-11, -200.9999999999999432 ) ) ;
#249979 = AXIS2_PLACEMENT_3D ( 'NONE', #207765, #171233, #70829 ) ;
#249980 = DIRECTION ( 'NONE',  ( 0.000000000000000000, 0.000000000000000000, -1.000000000000000000 ) ) ;
#249981 = CIRCLE ( 'NONE', #137535, 3.999999999999998224 ) ;
#249982 = VECTOR ( 'NONE', #247825, 1000.000000000000000 ) ;
#249983 = EDGE_LOOP ( 'NONE', ( #83435, #10037, #151590, #14844 ) ) ;
#249984 = VECTOR ( 'NONE', #235261, 1000.000000000000000 ) ;
#249986 = ORIENTED_EDGE ( 'NONE', *, *, #80024, .F. ) ;
#249985 = AXIS2_PLACEMENT_3D ( 'NONE', #237552, #254511, #234989 ) ;
#249987 = DIRECTION ( 'NONE',  ( 1.186688945009010077E-16, -1.000000000000000000, -0.000000000000000000 ) ) ;
#249989 = VERTEX_POINT ( 'NONE', #141111 ) ;
#249988 = CARTESIAN_POINT ( 'NONE',  ( 23.24999999999999289, 6.450000000011156587, -21.75000000000000355 ) ) ;
#249990 = EDGE_LOOP ( 'NONE', ( #7919, #236370, #180103 ) ) ;
#249991 = FACE_OUTER_BOUND ( 'NONE', #134424, .T. ) ;
#249992 = ORIENTED_EDGE ( 'NONE', *, *, #50577, .F. ) ;
#249993 = CARTESIAN_POINT ( 'NONE',  ( 21.05000000000000071, 43.36285386911620776, -234.7972500504784534 ) ) ;
#249994 = CIRCLE ( 'NONE', #96035, 7.899999999999990585 ) ;
#249995 = VERTEX_POINT ( 'NONE', #164530 ) ;
#249996 = CARTESIAN_POINT ( 'NONE',  ( 18.59999999999997655, 64.25000000001215028, -136.5231074845244166 ) ) ;
#249998 = ORIENTED_EDGE ( 'NONE', *, *, #121264, .T. ) ;
#249997 = ORIENTED_EDGE ( 'NONE', *, *, #103249, .T. ) ;
#249999 = ORIENTED_EDGE ( 'NONE', *, *, #25189, .T. ) ;
#250000 = VERTEX_POINT ( 'NONE', #124120 ) ;
#250001 = ORIENTED_EDGE ( 'NONE', *, *, #21145, .F. ) ;
#250002 = CARTESIAN_POINT ( 'NONE',  ( 23.15000000000000213, -4.356730526971939632, -226.1082375506050539 ) ) ;
#250003 = CARTESIAN_POINT ( 'NONE',  ( -12.33960340485503870, 9.360749169926261715, -184.8145701406072874 ) ) ;
#250005 = ORIENTED_EDGE ( 'NONE', *, *, #53108, .F. ) ;
#250004 = DIRECTION ( 'NONE',  ( 0.000000000000000000, 0.000000000000000000, 1.000000000000000000 ) ) ;
#250006 = DIRECTION ( 'NONE',  ( 0.000000000000000000, 0.8660254037844385966, -0.5000000000000003331 ) ) ;
#250008 = VERTEX_POINT ( 'NONE', #121576 ) ;
#250007 = DIRECTION ( 'NONE',  ( 0.000000000000000000, 0.000000000000000000, -1.000000000000000000 ) ) ;
#250009 = CARTESIAN_POINT ( 'NONE',  ( 23.15000000000000213, 12.37888392014804850, -249.8746333190754285 ) ) ;
#250010 = ORIENTED_EDGE ( 'NONE', *, *, #149687, .F. ) ;
#250011 = CARTESIAN_POINT ( 'NONE',  ( -20.64999999999999858, 85.40000000001178648, -79.41707660717668205 ) ) ;
#250012 = VECTOR ( 'NONE', #224566, 1000.000000000000000 ) ;
#250013 = ORIENTED_EDGE ( 'NONE', *, *, #212637, .F. ) ;
#250014 = CARTESIAN_POINT ( 'NONE',  ( -21.14999999999999858, 1.115600667400684642E-11, -167.4999999999999716 ) ) ;
#250015 = CARTESIAN_POINT ( 'NONE',  ( -16.91256925476569251, 30.32690185447398790, -234.8310981037861609 ) ) ;
#250016 = ADVANCED_FACE ( 'NONE', ( #82375 ), #101941, .F. ) ;
#250017 = AXIS2_PLACEMENT_3D ( 'NONE', #175575, #255026, #150857 ) ;
#250018 = ORIENTED_EDGE ( 'NONE', *, *, #62450, .F. ) ;
#250020 = DIRECTION ( 'NONE',  ( -0.000000000000000000, -1.000000000000000000, -6.982962677686266711E-15 ) ) ;
#250019 = CARTESIAN_POINT ( 'NONE',  ( 20.94999999999999929, 87.65000000001172964, -72.52310748452423184 ) ) ;
#250021 = LINE ( 'NONE', #252573, #197406 ) ;
#250022 = CIRCLE ( 'NONE', #121058, 0.6000000000000033085 ) ;
#250023 = DIRECTION ( 'NONE',  ( -1.000000000000000000, 3.469446951953635015E-14, 0.000000000000000000 ) ) ;
#250024 = DIRECTION ( 'NONE',  ( 0.000000000000000000, 0.4930308989875575865, 0.8700118002898125091 ) ) ;
#250025 = ORIENTED_EDGE ( 'NONE', *, *, #201137, .F. ) ;
#250026 = ORIENTED_EDGE ( 'NONE', *, *, #199764, .F. ) ;
#250027 = CARTESIAN_POINT ( 'NONE',  ( 21.04999999999999716, 8.872080675377937098, -8.521047418830562492 ) ) ;
#250028 = DIRECTION ( 'NONE',  ( 2.915501640297155269E-16, -0.9770955615653317272, -0.2128009952263597293 ) ) ;
#250029 = ORIENTED_EDGE ( 'NONE', *, *, #179744, .T. ) ;
#250030 = DIRECTION ( 'NONE',  ( -0.000000000000000000, 0.1686199900910294591, -0.9856811345164832039 ) ) ;
#250031 = ORIENTED_EDGE ( 'NONE', *, *, #22430, .F. ) ;
#250032 = ADVANCED_FACE ( 'NONE', ( #220647 ), #65411, .T. ) ;
#250033 = CARTESIAN_POINT ( 'NONE',  ( -18.50000000000000000, 9.350000000000001421, -12.14999999999999858 ) ) ;
#250034 = DIRECTION ( 'NONE',  ( 0.000000000000000000, -0.4721928772777346239, -0.8814952561688430555 ) ) ;
#250035 = EDGE_CURVE ( 'NONE', #202477, #75011, #161972, .T. ) ;
#250036 = CARTESIAN_POINT ( 'NONE',  ( -23.15000000000000213, 80.83132476063549632, -186.5534105423255653 ) ) ;
#250037 = AXIS2_PLACEMENT_3D ( 'NONE', #90902, #50467, #130010 ) ;
#250038 = ORIENTED_EDGE ( 'NONE', *, *, #55190, .F. ) ;
#250039 = CYLINDRICAL_SURFACE ( 'NONE', #19297, 0.5000000000000004441 ) ;
#250040 = AXIS2_PLACEMENT_3D ( 'NONE', #179837, #217632, #23346 ) ;
#250042 = VERTEX_POINT ( 'NONE', #26296 ) ;
#250041 = VECTOR ( 'NONE', #16294, 1000.000000000000000 ) ;
#250043 = VERTEX_POINT ( 'NONE', #245345 ) ;
#250044 = ORIENTED_EDGE ( 'NONE', *, *, #189286, .T. ) ;
#250045 = VECTOR ( 'NONE', #44745, 1000.000000000000000 ) ;
#250046 = EDGE_CURVE ( 'NONE', #194746, #171691, #105794, .T. ) ;
#250047 = CARTESIAN_POINT ( 'NONE',  ( 22.50014994444007144, 64.25028026812009330, -136.6061876412435367 ) ) ;
#250048 = CARTESIAN_POINT ( 'NONE',  ( 13.76927104934457802, 66.54401276639883633, -54.51157631762657729 ) ) ;
#250049 = CARTESIAN_POINT ( 'NONE',  ( -21.08198257630413508, 0.07264332379574613141, -127.6634032659849680 ) ) ;
#250051 = EDGE_CURVE ( 'NONE', #222999, #9515, #155179, .T. ) ;
#250050 = LINE ( 'NONE', #71432, #44576 ) ;
#250052 = CARTESIAN_POINT ( 'NONE',  ( 18.39999999999999503, 16.64129698264336099, -222.1941556740511032 ) ) ;
#250054 = DIRECTION ( 'NONE',  ( 0.000000000000000000, -1.000000000000000000, 0.000000000000000000 ) ) ;
#250053 = CARTESIAN_POINT ( 'NONE',  ( 22.49999999999999645, -3.098441969362629944, -228.1534806676847893 ) ) ;
#250056 = ORIENTED_EDGE ( 'NONE', *, *, #181160, .T. ) ;
#250055 = CARTESIAN_POINT ( 'NONE',  ( -16.97683809663752186, 50.97313360171293084, -232.3453239361865315 ) ) ;
#250057 = CARTESIAN_POINT ( 'NONE',  ( 21.05000000000000071, -1.835341550213257733, -179.0551512925629538 ) ) ;
#250058 = ORIENTED_EDGE ( 'NONE', *, *, #28836, .T. ) ;
#250059 = EDGE_CURVE ( 'NONE', #77408, #106998, #42021, .T. ) ;
#250060 = CARTESIAN_POINT ( 'NONE',  ( -14.56556274378147542, 9.446557523083688679, -149.0899419543459601 ) ) ;
#250061 = ORIENTED_EDGE ( 'NONE', *, *, #44649, .T. ) ;
#250062 = ORIENTED_EDGE ( 'NONE', *, *, #27414, .T. ) ;
#250063 = DIRECTION ( 'NONE',  ( 1.000000000000000000, 0.000000000000000000, 0.000000000000000000 ) ) ;
#250064 = CARTESIAN_POINT ( 'NONE',  ( -16.93226657140833069, 9.999543822735571297, -46.07871311097362366 ) ) ;
#250065 = DIRECTION ( 'NONE',  ( -1.000000000000000000, -0.000000000000000000, -0.000000000000000000 ) ) ;
#250066 = CARTESIAN_POINT ( 'NONE',  ( -16.94107738177415712, 65.98576071487543970, -123.9731074845243626 ) ) ;
#250067 = AXIS2_PLACEMENT_3D ( 'NONE', #213433, #16541, #37391 ) ;
#250068 = EDGE_CURVE ( 'NONE', #169584, #211426, #201071, .T. ) ;
#250069 = TOROIDAL_SURFACE ( 'NONE', #199995, 11.65000000000000036, 0.1000000000000000056 ) ;
#250070 = CARTESIAN_POINT ( 'NONE',  ( 20.94999027547553894, 18.34807417603272128, -236.8765254748879556 ) ) ;
#250071 = ORIENTED_EDGE ( 'NONE', *, *, #19684, .T. ) ;
#250073 = ORIENTED_EDGE ( 'NONE', *, *, #44984, .T. ) ;
#250072 = EDGE_CURVE ( 'NONE', #198947, #248473, #113624, .T. ) ;
#250074 = CARTESIAN_POINT ( 'NONE',  ( -18.59999999999999787, 64.35000000001174669, -81.27310748452440237 ) ) ;
#250075 = VERTEX_POINT ( 'NONE', #184072 ) ;
#250076 = CARTESIAN_POINT ( 'NONE',  ( 20.94999999999999574, 11.77895973109482952, -206.1023438919106070 ) ) ;
#250077 = DIRECTION ( 'NONE',  ( 1.000000000000000000, 0.000000000000000000, 0.000000000000000000 ) ) ;
#250078 = EDGE_LOOP ( 'NONE', ( #200498, #46375, #136166, #97379 ) ) ;
#250079 = DIRECTION ( 'NONE',  ( -0.000000000000000000, 0.8096735173027155286, -0.5868805631290315850 ) ) ;
#250080 = CARTESIAN_POINT ( 'NONE',  ( -20.99780126800942170, 11.60538868788778544, -60.08735257170526012 ) ) ;
#250081 = DIRECTION ( 'NONE',  ( 0.7071067811865474617, -0.7071067811865474617, -4.937700262164531476E-15 ) ) ;
#250082 = DIRECTION ( 'NONE',  ( 0.000000000000000000, -1.000000000000000000, 0.000000000000000000 ) ) ;
#250083 = EDGE_LOOP ( 'NONE', ( #16051, #195851, #126203, #138110 ) ) ;
#250084 = DIRECTION ( 'NONE',  ( 1.000000000000000000, 0.000000000000000000, 0.000000000000000000 ) ) ;
#250085 = CARTESIAN_POINT ( 'NONE',  ( -16.93262454970419384, 65.99797953208164358, -115.5960312582870557 ) ) ;
#250086 = DIRECTION ( 'NONE',  ( 0.000000000000000000, 1.224646799147363807E-16, 1.000000000000000000 ) ) ;
#250087 = ADVANCED_FACE ( 'NONE', ( #5407 ), #203641, .T. ) ;
#250088 = CYLINDRICAL_SURFACE ( 'NONE', #158607, 0.1000000000000028644 ) ;
#250089 = AXIS2_PLACEMENT_3D ( 'NONE', #66739, #86265, #146253 ) ;
#250090 = VECTOR ( 'NONE', #103147, 1000.000000000000000 ) ;
#250091 = DIRECTION ( 'NONE',  ( -0.000000000000000000, -0.000000000000000000, -1.000000000000000000 ) ) ;
#250092 = CIRCLE ( 'NONE', #141739, 7.800000000000009592 ) ;
#250093 = CARTESIAN_POINT ( 'NONE',  ( -23.15000000000000213, -9.500000000000003553, -9.893969122652446657 ) ) ;
#250094 = ORIENTED_EDGE ( 'NONE', *, *, #139109, .T. ) ;
#250095 = AXIS2_PLACEMENT_3D ( 'NONE', #15040, #251050, #55392 ) ;
#250096 = CARTESIAN_POINT ( 'NONE',  ( -16.87683809663752399, 9.850000000011144508, -120.5976359818037338 ) ) ;
#250097 = ORIENTED_EDGE ( 'NONE', *, *, #3109, .T. ) ;
#250098 = DIRECTION ( 'NONE',  ( -1.000000000000000000, -0.000000000000000000, 0.000000000000000000 ) ) ;
#250099 = CARTESIAN_POINT ( 'NONE',  ( -23.25000000000000000, 36.65892442174472876, -249.5511627012454596 ) ) ;
#250100 = CARTESIAN_POINT ( 'NONE',  ( -16.78493211734302903, 66.05416425680760995, -82.18705650362834092 ) ) ;
#250101 = FACE_OUTER_BOUND ( 'NONE', #96645, .T. ) ;
#250102 = CARTESIAN_POINT ( 'NONE',  ( -18.59999999999999787, 11.65000000001115232, -40.51480577065400013 ) ) ;
#250103 = CARTESIAN_POINT ( 'NONE',  ( -16.87036670365548474, 62.98166273414030059, -212.9957845397927656 ) ) ;
#250104 = CIRCLE ( 'NONE', #204285, 2.000000000000001776 ) ;
#250105 = ORIENTED_EDGE ( 'NONE', *, *, #181980, .F. ) ;
#250106 = DIRECTION ( 'NONE',  ( -0.000000000000000000, -0.4791956752371546724, -0.8777080977375153470 ) ) ;
#250107 = CARTESIAN_POINT ( 'NONE',  ( -23.15000000000000213, 69.14775023293175593, -234.9965690136722003 ) ) ;
#250108 = LINE ( 'NONE', #174473, #23279 ) ;
#250109 = CARTESIAN_POINT ( 'NONE',  ( 21.14999999999999858, 0.09779029131994770863, -60.74218538952391810 ) ) ;
#250110 = CARTESIAN_POINT ( 'NONE',  ( -21.64999999999999858, 68.65000000001199965, -115.2731074845243455 ) ) ;
#250111 = EDGE_CURVE ( 'NONE', #223188, #107706, #146223, .T. ) ;
#250112 = EDGE_LOOP ( 'NONE', ( #235163, #119322, #88103, #79033 ) ) ;
#250113 = ORIENTED_EDGE ( 'NONE', *, *, #251983, .F. ) ;
#250114 = CARTESIAN_POINT ( 'NONE',  ( 23.14999999999999503, 64.25000000001222134, -148.7731074845244450 ) ) ;
#250115 = PLANE ( 'NONE',  #38303 ) ;
#250116 = DIRECTION ( 'NONE',  ( 0.7071067811865474617, -0.7071067811865474617, -4.937700262164531476E-15 ) ) ;
#250117 = CARTESIAN_POINT ( 'NONE',  ( -23.25000000000000355, 58.31215475832291162, -223.8520309854405923 ) ) ;
#250118 = EDGE_CURVE ( 'NONE', #97258, #215894, #14177, .T. ) ;
#250119 = VECTOR ( 'NONE', #138788, 1000.000000000000000 ) ;
#250120 = EDGE_CURVE ( 'NONE', #132943, #30797, #108400, .T. ) ;
#250121 = EDGE_LOOP ( 'NONE', ( #249036, #38935, #258011, #6916 ) ) ;
#250122 = CARTESIAN_POINT ( 'NONE',  ( -19.99999999999999645, 1.250000000000000000, 16.60000000000000142 ) ) ;
#250123 = DIRECTION ( 'NONE',  ( -1.000000000000000000, 0.000000000000000000, 0.000000000000000000 ) ) ;
#250124 = AXIS2_PLACEMENT_3D ( 'NONE', #252328, #155834, #151992 ) ;
#250125 = EDGE_CURVE ( 'NONE', #178001, #200940, #21862, .T. ) ;
#250126 = ORIENTED_EDGE ( 'NONE', *, *, #223575, .F. ) ;
#250128 = EDGE_CURVE ( 'NONE', #204776, #119315, #205181, .T. ) ;
#250127 = DIRECTION ( 'NONE',  ( -1.000000000000000000, 0.000000000000000000, -0.000000000000000000 ) ) ;
#250129 = EDGE_CURVE ( 'NONE', #111770, #155744, #250969, .T. ) ;
#250130 = ADVANCED_FACE ( 'NONE', ( #247897 ), #131802, .F. ) ;
#250131 = EDGE_LOOP ( 'NONE', ( #127929, #15376, #64564, #70199, #34612 ) ) ;
#250132 = ORIENTED_EDGE ( 'NONE', *, *, #17355, .T. ) ;
#250133 = EDGE_CURVE ( 'NONE', #237782, #208580, #70582, .T. ) ;
#250134 = CIRCLE ( 'NONE', #108481, 0.09999999999999939493 ) ;
#250135 = ORIENTED_EDGE ( 'NONE', *, *, #223678, .T. ) ;
#250136 = SPHERICAL_SURFACE ( 'NONE', #213953, 0.1000000000000000056 ) ;
#250137 = CARTESIAN_POINT ( 'NONE',  ( -20.94999999999999929, 87.48912529308779540, -72.62310748452422615 ) ) ;
#250138 = CARTESIAN_POINT ( 'NONE',  ( 20.95512840106819752, 10.62384869378447583, -112.7024792207986650 ) ) ;
#250139 = CARTESIAN_POINT ( 'NONE',  ( -20.54999999999999716, 2.000000000011154189, -46.72462192276210402 ) ) ;
#250140 = CARTESIAN_POINT ( 'NONE',  ( -23.25000000000000000, 1.115600667400684642E-11, -37.54999999999999716 ) ) ;
#250141 = DIRECTION ( 'NONE',  ( 1.000000000000000000, 0.000000000000000000, 0.000000000000000000 ) ) ;
#250142 = CARTESIAN_POINT ( 'NONE',  ( 21.00000000000000000, 11.49641995933507843, -1.885425182446133885 ) ) ;
#250144 = CARTESIAN_POINT ( 'NONE',  ( 21.05000000000000071, 1.115600667400684642E-11, -100.5000000000000284 ) ) ;
#250143 = CARTESIAN_POINT ( 'NONE',  ( 20.95561247346651967, 65.40499263480833747, -95.42932471754275525 ) ) ;
#250145 = CARTESIAN_POINT ( 'NONE',  ( -20.94999999999999929, -1.162701749926853712, -142.0000000000000284 ) ) ;
#250146 = CARTESIAN_POINT ( 'NONE',  ( 21.05000005001341989, 22.05259145179880420, -231.6630504590253565 ) ) ;
#250147 = CARTESIAN_POINT ( 'NONE',  ( 18.49999999999999645, 0.000000000000000000, -33.50000000000000000 ) ) ;
#250148 = DIRECTION ( 'NONE',  ( 0.000000000000000000, -0.9998779222360097974, 0.01562500000000363945 ) ) ;
#250149 = CIRCLE ( 'NONE', #108488, 0.09999999999999939493 ) ;
#250150 = VERTEX_POINT ( 'NONE', #69282 ) ;
#250151 = DIRECTION ( 'NONE',  ( -6.938893903907224433E-15, -1.000000000000000000, -6.982962677686266711E-15 ) ) ;
#250152 = CIRCLE ( 'NONE', #187626, 2.700000000000001066 ) ;
#250153 = CARTESIAN_POINT ( 'NONE',  ( -21.14999999999999858, 1.115600667400684642E-11, -134.0000000000000000 ) ) ;
#250154 = CARTESIAN_POINT ( 'NONE',  ( -20.64999999999999858, 65.77012247227901298, -213.5448142138000378 ) ) ;
#250155 = ADVANCED_FACE ( 'NONE', ( #207513 ), #167117, .T. ) ;
#250156 = AXIS2_PLACEMENT_3D ( 'NONE', #4194, #199863, #241534 ) ;
#250157 = AXIS2_PLACEMENT_3D ( 'NONE', #43239, #164475, #24981 ) ;
#250158 = DIRECTION ( 'NONE',  ( 1.000000000000000000, 0.000000000000000000, 0.000000000000000000 ) ) ;
#250159 = DIRECTION ( 'NONE',  ( -0.000000000000000000, -1.000000000000000000, -0.000000000000000000 ) ) ;
#250160 = ADVANCED_FACE ( 'NONE', ( #148819 ), #10586, .F. ) ;
#250161 = EDGE_CURVE ( 'NONE', #110735, #108899, #142637, .T. ) ;
#250162 = AXIS2_PLACEMENT_3D ( 'NONE', #77217, #138458, #35567 ) ;
#250163 = ORIENTED_EDGE ( 'NONE', *, *, #136399, .T. ) ;
#250164 = VECTOR ( 'NONE', #40144, 1000.000000000000000 ) ;
#250165 = ORIENTED_EDGE ( 'NONE', *, *, #81264, .T. ) ;
#250166 = CARTESIAN_POINT ( 'NONE',  ( -15.69373346032659455, 9.356790025045880199, -17.20482650861390539 ) ) ;
#250167 = VERTEX_POINT ( 'NONE', #9289 ) ;
#250168 = CARTESIAN_POINT ( 'NONE',  ( 22.32929514600007792, 68.42135243463566496, -136.6221831626382652 ) ) ;
#250169 = FACE_OUTER_BOUND ( 'NONE', #243168, .T. ) ;
#250170 = VECTOR ( 'NONE', #219951, 1000.000000000000000 ) ;
#250171 = AXIS2_PLACEMENT_3D ( 'NONE', #207575, #8086, #13225 ) ;
#250172 = CIRCLE ( 'NONE', #179447, 0.09999999999999939493 ) ;
#250173 = VECTOR ( 'NONE', #12762, 1000.000000000000000 ) ;
#250174 = CIRCLE ( 'NONE', #91938, 0.1000000000000028644 ) ;
#250175 = VERTEX_POINT ( 'NONE', #251753 ) ;
#250176 = CARTESIAN_POINT ( 'NONE',  ( -21.29999999999995808, 1.115600667400684642E-11, -67.00000000000004263 ) ) ;
#250177 = EDGE_LOOP ( 'NONE', ( #19974, #143404, #190868, #69529 ) ) ;
#250178 = LINE ( 'NONE', #118373, #128968 ) ;
#250179 = CARTESIAN_POINT ( 'NONE',  ( -20.65000000000000568, 8.212522512469059066, -212.1579332307740344 ) ) ;
#250180 = LINE ( 'NONE', #154953, #207648 ) ;
#250181 = LINE ( 'NONE', #71564, #50058 ) ;
#250182 = CARTESIAN_POINT ( 'NONE',  ( 22.39999999999999503, 0.000000000000000000, 7.790779598373379855 ) ) ;
#250183 = CIRCLE ( 'NONE', #200288, 0.1000000000000028644 ) ;
#250184 = LINE ( 'NONE', #170694, #150037 ) ;
#250185 = DIRECTION ( 'NONE',  ( 0.000000000000000000, 0.9667078373770113808, 0.2558827019434133376 ) ) ;
#250186 = DIRECTION ( 'NONE',  ( -5.603264701231742896E-32, 0.8814952561688430555, -0.4721928772777344019 ) ) ;
#250188 = VERTEX_POINT ( 'NONE', #190525 ) ;
#250187 = CARTESIAN_POINT ( 'NONE',  ( 18.46163235739466302, -0.7174337875998068048, -242.2552085481934512 ) ) ;
#250190 = SPHERICAL_SURFACE ( 'NONE', #22821, 0.1000000000000000056 ) ;
#250189 = CARTESIAN_POINT ( 'NONE',  ( -21.05000000000000071, 6.258316057332023341, 0.06570161032208736429 ) ) ;
#250191 = ORIENTED_EDGE ( 'NONE', *, *, #44065, .T. ) ;
#250192 = ORIENTED_EDGE ( 'NONE', *, *, #94630, .T. ) ;
#250193 = VERTEX_POINT ( 'NONE', #228348 ) ;
#250194 = CARTESIAN_POINT ( 'NONE',  ( -20.94999999999999929, 1.115600667400684642E-11, -100.5000000000000426 ) ) ;
#250195 = CARTESIAN_POINT ( 'NONE',  ( 22.42196299218230493, 75.99755832602443206, -81.17271918717379720 ) ) ;
#250196 = DIRECTION ( 'NONE',  ( -1.073024830501117725E-15, 0.000000000000000000, 1.000000000000000000 ) ) ;
#250197 = DIRECTION ( 'NONE',  ( 3.469446951953498700E-14, -0.7899159663865300551, -0.6132151058540831201 ) ) ;
#250198 = LINE ( 'NONE', #71585, #79518 ) ;
#250199 = VECTOR ( 'NONE', #81, 1000.000000000000000 ) ;
#250200 = FACE_BOUND ( 'NONE', #190269, .T. ) ;
#250201 = EDGE_CURVE ( 'NONE', #147787, #182942, #73151, .T. ) ;
#250202 = CARTESIAN_POINT ( 'NONE',  ( 20.94999999999999929, 36.65892442174472876, -249.5511627012454596 ) ) ;
#250203 = ORIENTED_EDGE ( 'NONE', *, *, #62141, .F. ) ;
#250204 = EDGE_LOOP ( 'NONE', ( #85304, #161172, #34576, #160556 ) ) ;
#250205 = EDGE_CURVE ( 'NONE', #135831, #134210, #47107, .T. ) ;
#250206 = DIRECTION ( 'NONE',  ( 0.7071067811865302533, -0.6909108974501196876, -0.1504730267679053324 ) ) ;
#250207 = VECTOR ( 'NONE', #77391, 1000.000000000000000 ) ;
#250208 = VERTEX_POINT ( 'NONE', #186661 ) ;
#250209 = DIRECTION ( 'NONE',  ( 0.000000000000000000, 0.1144908148674362580, 0.9934243067848653741 ) ) ;
#250210 = ORIENTED_EDGE ( 'NONE', *, *, #154159, .T. ) ;
#250211 = FACE_OUTER_BOUND ( 'NONE', #190943, .T. ) ;
#250212 = EDGE_CURVE ( 'NONE', #54914, #37949, #147906, .T. ) ;
#250213 = AXIS2_PLACEMENT_3D ( 'NONE', #173128, #213479, #101191 ) ;
#250214 = EDGE_CURVE ( 'NONE', #70494, #161523, #91406, .T. ) ;
#250215 = DIRECTION ( 'NONE',  ( 2.694716079187272946E-16, -1.000000000000000000, 0.000000000000000000 ) ) ;
#250216 = FACE_OUTER_BOUND ( 'NONE', #187159, .T. ) ;
#250217 = CARTESIAN_POINT ( 'NONE',  ( -18.59999999999999787, 11.75000000001115197, -55.25000000000004974 ) ) ;
#250218 = ORIENTED_EDGE ( 'NONE', *, *, #27939, .T. ) ;
#250219 = DIRECTION ( 'NONE',  ( -0.000000000000000000, -0.000000000000000000, -1.000000000000000000 ) ) ;
#250220 = TOROIDAL_SURFACE ( 'NONE', #150278, 1.900000000000002576, 0.1000000000000000056 ) ;
#250221 = CYLINDRICAL_SURFACE ( 'NONE', #210443, 0.9000000000000014655 ) ;
#250222 = DIRECTION ( 'NONE',  ( 0.000000000000000000, -0.9651348961777028723, 0.2617529984165503087 ) ) ;
#250223 = CARTESIAN_POINT ( 'NONE',  ( 23.24999999999999645, 76.00000000001237765, -170.0231074845243597 ) ) ;
#250224 = VERTEX_POINT ( 'NONE', #109658 ) ;
#250226 = DIRECTION ( 'NONE',  ( 1.000000000000000000, 0.000000000000000000, 0.000000000000000000 ) ) ;
#250225 = CARTESIAN_POINT ( 'NONE',  ( -21.53699400381697160, 6.787711793192025667, -134.0000000000000000 ) ) ;
#250227 = VERTEX_POINT ( 'NONE', #90092 ) ;
#250230 = ORIENTED_EDGE ( 'NONE', *, *, #153312, .T. ) ;
#250229 = DIRECTION ( 'NONE',  ( 1.000000000000000000, 0.000000000000000000, 0.000000000000000000 ) ) ;
#250228 = CARTESIAN_POINT ( 'NONE',  ( 20.94999999999999929, 9.480858690661944976, -221.0361137499737936 ) ) ;
#250231 = AXIS2_PLACEMENT_3D ( 'NONE', #84489, #7573, #64969 ) ;
#250232 = EDGE_CURVE ( 'NONE', #224509, #59445, #146913, .T. ) ;
#250233 = DIRECTION ( 'NONE',  ( 0.000000000000000000, 0.000000000000000000, -1.000000000000000000 ) ) ;
#250234 = EDGE_CURVE ( 'NONE', #197777, #233325, #180274, .T. ) ;
#250235 = CIRCLE ( 'NONE', #208738, 11.64999999999999325 ) ;
#250236 = CARTESIAN_POINT ( 'NONE',  ( -18.47690164073606667, 85.46484453802410997, -96.32172654468811857 ) ) ;
#250237 = EDGE_LOOP ( 'NONE', ( #156014, #77969, #173592, #20258 ) ) ;
#250238 = CARTESIAN_POINT ( 'NONE',  ( 20.94999999999999929, 67.92720994251783395, -214.1870976236629929 ) ) ;
#250239 = CARTESIAN_POINT ( 'NONE',  ( -18.50000000000000000, 63.89220327960687484, -212.8282812377314883 ) ) ;
#250241 = FACE_OUTER_BOUND ( 'NONE', #83993, .T. ) ;
#250240 = DIRECTION ( 'NONE',  ( -1.000000000000000000, 0.000000000000000000, -0.000000000000000000 ) ) ;
#250243 = VERTEX_POINT ( 'NONE', #157834 ) ;
#250242 = CARTESIAN_POINT ( 'NONE',  ( 20.96428641294244599, 11.75000000001149836, -93.67489317794097303 ) ) ;
#250244 = EDGE_CURVE ( 'NONE', #104351, #169843, #213569, .T. ) ;
#250245 = AXIS2_PLACEMENT_3D ( 'NONE', #68721, #67430, #246085 ) ;
#250246 = ORIENTED_EDGE ( 'NONE', *, *, #60838, .T. ) ;
#250248 = EDGE_CURVE ( 'NONE', #151129, #203482, #55149, .T. ) ;
#250247 = DIRECTION ( 'NONE',  ( 1.000000000000000000, -0.000000000000000000, -0.000000000000000000 ) ) ;
#250249 = CARTESIAN_POINT ( 'NONE',  ( -20.64999999999999858, 74.00000000001199396, -115.7477294072863998 ) ) ;
#250250 = FACE_OUTER_BOUND ( 'NONE', #170376, .T. ) ;
#250251 = ORIENTED_EDGE ( 'NONE', *, *, #102947, .T. ) ;
#250252 = CARTESIAN_POINT ( 'NONE',  ( -33.72168855820452649, 64.52683809665003878, -179.2731074845244450 ) ) ;
#250253 = DIRECTION ( 'NONE',  ( 0.000000000000000000, 1.000000000000000000, 0.000000000000000000 ) ) ;
#250254 = CARTESIAN_POINT ( 'NONE',  ( 18.46921299892754931, -9.509378177812605415, -140.9865787093704625 ) ) ;
#250255 = ORIENTED_EDGE ( 'NONE', *, *, #209547, .T. ) ;
#250256 = EDGE_CURVE ( 'NONE', #209275, #202001, #63537, .T. ) ;
#250257 = CARTESIAN_POINT ( 'NONE',  ( 20.41140022480518823, 59.17705388698332314, -225.7806615260952015 ) ) ;
#250258 = EDGE_CURVE ( 'NONE', #165365, #81754, #74441, .T. ) ;
#250259 = CARTESIAN_POINT ( 'NONE',  ( 20.95000000000000284, 64.40000000001145963, -42.95131071479990936 ) ) ;
#250260 = CIRCLE ( 'NONE', #83620, 1.899999999999999023 ) ;
#250261 = AXIS2_PLACEMENT_3D ( 'NONE', #138116, #81980, #1173 ) ;
#250262 = ORIENTED_EDGE ( 'NONE', *, *, #151131, .T. ) ;
#250263 = AXIS2_PLACEMENT_3D ( 'NONE', #29157, #108644, #215444 ) ;
#250264 = EDGE_CURVE ( 'NONE', #136044, #196832, #177387, .T. ) ;
#250265 = FACE_OUTER_BOUND ( 'NONE', #12229, .T. ) ;
#250266 = DIRECTION ( 'NONE',  ( -0.000000000000000000, 0.4721928772777345684, 0.8814952561688429444 ) ) ;
#250267 = VERTEX_POINT ( 'NONE', #136938 ) ;
#250268 = VECTOR ( 'NONE', #4431, 1000.000000000000000 ) ;
#250269 = ORIENTED_EDGE ( 'NONE', *, *, #116265, .F. ) ;
#250270 = DIRECTION ( 'NONE',  ( 0.000000000000000000, 0.000000000000000000, 1.000000000000000000 ) ) ;
#250271 = ORIENTED_EDGE ( 'NONE', *, *, #155642, .T. ) ;
#250273 = ORIENTED_EDGE ( 'NONE', *, *, #222191, .T. ) ;
#250272 = LINE ( 'NONE', #216263, #96893 ) ;
#250274 = ADVANCED_FACE ( 'NONE', ( #114810 ), #18275, .F. ) ;
#250275 = VERTEX_POINT ( 'NONE', #133096 ) ;
#250276 = AXIS2_PLACEMENT_3D ( 'NONE', #204571, #226696, #248846 ) ;
#250279 = VERTEX_POINT ( 'NONE', #256825 ) ;
#250278 = ORIENTED_EDGE ( 'NONE', *, *, #193118, .T. ) ;
#250277 = DIRECTION ( 'NONE',  ( 1.186688945009010077E-16, -1.000000000000000000, -0.000000000000000000 ) ) ;
#250280 = EDGE_CURVE ( 'NONE', #105113, #100756, #96844, .T. ) ;
#250281 = FACE_OUTER_BOUND ( 'NONE', #250875, .T. ) ;
#250282 = VERTEX_POINT ( 'NONE', #78239 ) ;
#250283 = CARTESIAN_POINT ( 'NONE',  ( 23.40000000000005542, 74.83745509109094485, -43.82310748452479743 ) ) ;
#250284 = LINE ( 'NONE', #230735, #90897 ) ;
#250285 = LINE ( 'NONE', #211159, #80508 ) ;
#250286 = DIRECTION ( 'NONE',  ( 0.000000000000000000, -0.9126074666063773710, -0.4088369013363274962 ) ) ;
#250287 = CARTESIAN_POINT ( 'NONE',  ( 21.05000000000000071, 1.115600667400684642E-11, -167.4999999999999716 ) ) ;
#250288 = ORIENTED_EDGE ( 'NONE', *, *, #253196, .F. ) ;
#250289 = ORIENTED_EDGE ( 'NONE', *, *, #122669, .T. ) ;
#250290 = VERTEX_POINT ( 'NONE', #213905 ) ;
#250291 = CARTESIAN_POINT ( 'NONE',  ( -20.94999999999999929, 5.900000000011102586, -43.71909976465641989 ) ) ;
#250292 = ORIENTED_EDGE ( 'NONE', *, *, #96901, .T. ) ;
#250293 = LINE ( 'NONE', #212468, #92431 ) ;
#250295 = ORIENTED_EDGE ( 'NONE', *, *, #204459, .T. ) ;
#250294 = DIRECTION ( 'NONE',  ( 0.000000000000000000, 0.000000000000000000, -1.000000000000000000 ) ) ;
#250296 = CIRCLE ( 'NONE', #150354, 3.999999999999999112 ) ;
#250297 = ORIENTED_EDGE ( 'NONE', *, *, #38135, .F. ) ;
#250298 = CARTESIAN_POINT ( 'NONE',  ( -21.64999999999999858, 68.75000000001199396, -115.3731074845243540 ) ) ;
#250299 = AXIS2_PLACEMENT_3D ( 'NONE', #57971, #20165, #137509 ) ;
#250300 = ORIENTED_EDGE ( 'NONE', *, *, #140788, .F. ) ;
#250302 = AXIS2_PLACEMENT_3D ( 'NONE', #162039, #139865, #79878 ) ;
#250301 = CARTESIAN_POINT ( 'NONE',  ( -16.80070461187954578, 9.950000000010851053, -180.1469638291620186 ) ) ;
#250303 = CARTESIAN_POINT ( 'NONE',  ( -21.05000000000000071, 76.10000000001241460, -176.5637644362255969 ) ) ;
#250305 = VERTEX_POINT ( 'NONE', #53556 ) ;
#250304 = ORIENTED_EDGE ( 'NONE', *, *, #183954, .F. ) ;
#250306 = ORIENTED_EDGE ( 'NONE', *, *, #48453, .T. ) ;
#250308 = DIRECTION ( 'NONE',  ( 0.000000000000000000, -0.4088369013363280513, 0.9126074666063769270 ) ) ;
#250307 = CIRCLE ( 'NONE', #67145, 0.1000000000000028644 ) ;
#250309 = ORIENTED_EDGE ( 'NONE', *, *, #159260, .T. ) ;
#250310 = ORIENTED_EDGE ( 'NONE', *, *, #167198, .T. ) ;
#250311 = DIRECTION ( 'NONE',  ( 1.000000000000000000, 0.000000000000000000, -0.000000000000000000 ) ) ;
#250312 = CIRCLE ( 'NONE', #137861, 0.09999999999999939493 ) ;
#250314 = ORIENTED_EDGE ( 'NONE', *, *, #8284, .T. ) ;
#250313 = DIRECTION ( 'NONE',  ( 0.000000000000000000, -0.2617529984165152257, -0.9651348961777124202 ) ) ;
#250315 = CARTESIAN_POINT ( 'NONE',  ( 23.14999999999999858, 76.00000000001142553, -36.02310748452432421 ) ) ;
#250317 = FACE_OUTER_BOUND ( 'NONE', #114260, .T. ) ;
#250316 = DIRECTION ( 'NONE',  ( 1.000000000000000000, 3.190570557967288949E-16, 6.948722487160392945E-17 ) ) ;
#250318 = DIRECTION ( 'NONE',  ( 0.000000000000000000, 0.2128009952263603954, -0.9770955615653315052 ) ) ;
#250319 = LINE ( 'NONE', #129095, #206888 ) ;
#250320 = ORIENTED_EDGE ( 'NONE', *, *, #187862, .F. ) ;
#250321 = VERTEX_POINT ( 'NONE', #194375 ) ;
#250322 = CARTESIAN_POINT ( 'NONE',  ( 18.39999999999999858, 85.68240343348824695, -96.36626410711143365 ) ) ;
#250323 = DIRECTION ( 'NONE',  ( 1.000000000000000000, 0.000000000000000000, -0.000000000000000000 ) ) ;
#250324 = EDGE_CURVE ( 'NONE', #159944, #26762, #221929, .T. ) ;
#250326 = ORIENTED_EDGE ( 'NONE', *, *, #209040, .T. ) ;
#250325 = AXIS2_PLACEMENT_3D ( 'NONE', #157869, #138236, #40484 ) ;
#250327 = AXIS2_PLACEMENT_3D ( 'NONE', #159158, #177443, #179992 ) ;
#250328 = CARTESIAN_POINT ( 'NONE',  ( 21.05000000000000071, 12.19249617487739812, -224.2797955561429148 ) ) ;
#250329 = CARTESIAN_POINT ( 'NONE',  ( 21.05000000000000071, 1.115600667400684642E-11, -134.0000000000000284 ) ) ;
#250330 = ORIENTED_EDGE ( 'NONE', *, *, #40129, .T. ) ;
#250331 = ORIENTED_EDGE ( 'NONE', *, *, #212395, .F. ) ;
#250332 = VECTOR ( 'NONE', #52204, 1000.000000000000000 ) ;
#250333 = DIRECTION ( 'NONE',  ( -1.000000000000000000, -7.304098846218105085E-16, -4.217023435051676515E-16 ) ) ;
#250334 = ADVANCED_FACE ( 'NONE', ( #155256 ), #99068, .F. ) ;
#250335 = DIRECTION ( 'NONE',  ( 0.000000000000000000, 0.4999999999999543698, 0.8660254037844650199 ) ) ;
#250336 = EDGE_LOOP ( 'NONE', ( #222666, #181307, #94082, #234374 ) ) ;
#250337 = CARTESIAN_POINT ( 'NONE',  ( 23.24999999999997513, 64.35000000001195986, -110.0379132551783243 ) ) ;
#250338 = ORIENTED_EDGE ( 'NONE', *, *, #197405, .F. ) ;
#250339 = AXIS2_PLACEMENT_3D ( 'NONE', #132602, #114309, #36073 ) ;
#250340 = CARTESIAN_POINT ( 'NONE',  ( -20.85000000000000142, -1.164121893241208960, -41.41484808557160591 ) ) ;
#250342 = CIRCLE ( 'NONE', #179620, 0.1000000000000028644 ) ;
#250341 = CARTESIAN_POINT ( 'NONE',  ( -16.78270389226384651, 9.947372616628161524, -154.8412070369114701 ) ) ;
#250344 = CARTESIAN_POINT ( 'NONE',  ( -18.59999999999999787, 7.021664781911246322, -137.8335654018973457 ) ) ;
#250343 = DIRECTION ( 'NONE',  ( 0.000000000000000000, 0.000000000000000000, 1.000000000000000000 ) ) ;
#250345 = DIRECTION ( 'NONE',  ( -0.000000000000000000, 0.8660254037844383745, -0.5000000000000003331 ) ) ;
#250346 = EDGE_CURVE ( 'NONE', #105040, #121092, #184523, .T. ) ;
#250348 = EDGE_CURVE ( 'NONE', #12040, #127785, #26338, .T. ) ;
#250347 = DIRECTION ( 'NONE',  ( 1.000000000000000000, -0.000000000000000000, -0.000000000000000000 ) ) ;
#250349 = DIRECTION ( 'NONE',  ( -1.000000000000000000, -0.000000000000000000, 0.000000000000000000 ) ) ;
#250350 = DIRECTION ( 'NONE',  ( 0.000000000000000000, 6.982962677686266711E-15, -1.000000000000000000 ) ) ;
#250352 = VERTEX_POINT ( 'NONE', #56092 ) ;
#250351 = DIRECTION ( 'NONE',  ( 0.000000000000000000, 0.09425075112713271475, 0.9955484899852801162 ) ) ;
#250353 = VECTOR ( 'NONE', #221216, 1000.000000000000000 ) ;
#250354 = PRESENTATION_LAYER_ASSIGNMENT (  '', '', ( #33926 ) ) ;
#250355 = AXIS2_PLACEMENT_3D ( 'NONE', #189800, #208097, #108960 ) ;
#250356 = TOROIDAL_SURFACE ( 'NONE', #241965, 0.6000000000000004219, 0.1000000000000000056 ) ;
#250358 = ORIENTED_EDGE ( 'NONE', *, *, #45262, .F. ) ;
#250357 = ORIENTED_EDGE ( 'NONE', *, *, #146679, .F. ) ;
#250359 = VERTEX_POINT ( 'NONE', #236035 ) ;
#250360 = EDGE_CURVE ( 'NONE', #8981, #10090, #47146, .T. ) ;
#250361 = CARTESIAN_POINT ( 'NONE',  ( -16.77732147278574715, 60.94678617778803442, -221.0297456304129753 ) ) ;
#250362 = CARTESIAN_POINT ( 'NONE',  ( 20.94999999999999929, 1.115600667400684642E-11, -100.5000000000000426 ) ) ;
#250364 = CARTESIAN_POINT ( 'NONE',  ( 22.16821283564876666, 7.558973340780761774, 1.462253661542695674E-16 ) ) ;
#250363 = CARTESIAN_POINT ( 'NONE',  ( 20.94999999999999574, 11.84624361595475506, -206.1763227999733203 ) ) ;
#250365 = DIRECTION ( 'NONE',  ( -1.000000000000000000, 0.000000000000000000, 0.000000000000000000 ) ) ;
#250366 = ORIENTED_EDGE ( 'NONE', *, *, #77710, .T. ) ;
#250367 = CARTESIAN_POINT ( 'NONE',  ( 23.15000000000000213, -8.596261682231828516, -191.5498724828496790 ) ) ;
#250368 = VERTEX_POINT ( 'NONE', #156540 ) ;
#250369 = ORIENTED_EDGE ( 'NONE', *, *, #206223, .T. ) ;
#250370 = CARTESIAN_POINT ( 'NONE',  ( -20.94999999999999929, 1.162701749949165642, -142.1000000000000227 ) ) ;
#250371 = CARTESIAN_POINT ( 'NONE',  ( -18.50000000000000000, -1.164121893230052995, -108.4148480855716485 ) ) ;
#250372 = CARTESIAN_POINT ( 'NONE',  ( -21.00000000000000000, 1.212568896937007645, -8.000000000000000000 ) ) ;
#250373 = EDGE_LOOP ( 'NONE', ( #176893, #156506, #208550, #246734 ) ) ;
#250374 = LINE ( 'NONE', #95153, #147146 ) ;
#250375 = LINE ( 'NONE', #173468, #21593 ) ;
#250376 = ORIENTED_EDGE ( 'NONE', *, *, #71398, .T. ) ;
#250378 = VERTEX_POINT ( 'NONE', #17011 ) ;
#250377 = EDGE_CURVE ( 'NONE', #181798, #96638, #212641, .T. ) ;
#250379 = DIRECTION ( 'NONE',  ( 1.000000000000000000, 0.000000000000000000, 0.000000000000000000 ) ) ;
#250380 = CARTESIAN_POINT ( 'NONE',  ( 20.94999999999999929, 86.48473784507378070, -209.3714211149925575 ) ) ;
#250381 = CARTESIAN_POINT ( 'NONE',  ( -23.25000000000000000, -1.736705739456431807, -112.0174225876237699 ) ) ;
#250382 = DIRECTION ( 'NONE',  ( 0.000000000000000000, 1.000000000000000000, 0.000000000000000000 ) ) ;
#250383 = ORIENTED_EDGE ( 'NONE', *, *, #16673, .F. ) ;
#250384 = CARTESIAN_POINT ( 'NONE',  ( 21.05000000000000071, 53.86595165227826243, -236.3638196928718855 ) ) ;
#250385 = AXIS2_PLACEMENT_3D ( 'NONE', #70050, #249950, #92152 ) ;
#250386 = DIRECTION ( 'NONE',  ( 0.000000000000000000, 0.000000000000000000, -1.000000000000000000 ) ) ;
#250388 = DIRECTION ( 'NONE',  ( 0.000000000000000000, 0.2128009952263601456, -0.9770955615653316162 ) ) ;
#250387 = DIRECTION ( 'NONE',  ( -1.000000000000000000, 0.000000000000000000, 0.000000000000000000 ) ) ;
#250389 = CARTESIAN_POINT ( 'NONE',  ( -18.59999999999999787, 77.25000000001136868, -28.22262673010923351 ) ) ;
#250390 = EDGE_CURVE ( 'NONE', #246470, #134706, #128264, .T. ) ;
#250391 = CARTESIAN_POINT ( 'NONE',  ( 22.60000000000000142, 1.115600667400684642E-11, -67.00000000000004263 ) ) ;
#250392 = CARTESIAN_POINT ( 'NONE',  ( -20.65000000000000568, 70.35000000001232934, -160.7731074845243882 ) ) ;
#250394 = EDGE_LOOP ( 'NONE', ( #226493, #252565, #27178 ) ) ;
#250393 = CARTESIAN_POINT ( 'NONE',  ( -21.29999999999995808, 32.96286418198891255, -251.2069521516576174 ) ) ;
#250395 = CIRCLE ( 'NONE', #171343, 3.999999999999996447 ) ;
#250396 = CARTESIAN_POINT ( 'NONE',  ( 22.39999999999999503, 31.76383008438224564, -238.8689086587541510 ) ) ;
#250397 = FACE_OUTER_BOUND ( 'NONE', #134072, .T. ) ;
#250398 = EDGE_CURVE ( 'NONE', #79720, #145358, #80441, .T. ) ;
#250399 = LINE ( 'NONE', #186599, #167414 ) ;
#250400 = DIRECTION ( 'NONE',  ( -0.7071067811865475727, 0.6824534298470373850, -0.1850873201762210096 ) ) ;
#250401 = CARTESIAN_POINT ( 'NONE',  ( -18.39999999999999858, 64.25000000001161027, -60.27310748452440947 ) ) ;
#250402 = AXIS2_PLACEMENT_3D ( 'NONE', #21727, #197781, #3419 ) ;
#250403 = CIRCLE ( 'NONE', #54590, 0.09999999999999939493 ) ;
#250404 = CARTESIAN_POINT ( 'NONE',  ( -20.94999999999999929, 7.021664781911246322, -70.63356540189728605 ) ) ;
#250405 = CARTESIAN_POINT ( 'NONE',  ( 18.39999999999999147, 8.822561741677553471, -42.75000000000000000 ) ) ;
#250406 = EDGE_CURVE ( 'NONE', #235746, #24875, #230316, .T. ) ;
#250407 = EDGE_CURVE ( 'NONE', #184383, #149228, #123803, .T. ) ;
#250408 = ORIENTED_EDGE ( 'NONE', *, *, #61952, .F. ) ;
#250409 = CARTESIAN_POINT ( 'NONE',  ( 23.14999999999999503, 13.96869538424789070, -210.3925794786331949 ) ) ;
#250411 = VERTEX_POINT ( 'NONE', #59945 ) ;
#250410 = CARTESIAN_POINT ( 'NONE',  ( 21.14999999999999858, 70.41157348381892689, -224.1287375179191201 ) ) ;
#250412 = CARTESIAN_POINT ( 'NONE',  ( -16.98495255085918032, 44.09872649034048209, -235.2545122050661064 ) ) ;
#250413 =( BOUNDED_CURVE ( )  B_SPLINE_CURVE ( 3, ( #227516, #69758, #46305, #205374 ),
 .UNSPECIFIED., .F., .F. ) 
 B_SPLINE_CURVE_WITH_KNOTS ( ( 4, 4 ),
 ( 0.000000000000000000, 1.570796326794896558 ),
 .UNSPECIFIED. ) 
 CURVE ( )  GEOMETRIC_REPRESENTATION_ITEM ( )  RATIONAL_B_SPLINE_CURVE ( ( 1.000000000000000000, 0.8047378541243649375, 0.8047378541243649375, 1.000000000000000000 ) ) 
 REPRESENTATION_ITEM ( '' )  );
#250415 = ADVANCED_FACE ( 'NONE', ( #182509 ), #72974, .T. ) ;
#250414 = DIRECTION ( 'NONE',  ( -0.000000000000000000, 0.9908441862701591329, 0.1350103645451946055 ) ) ;
#250416 = EDGE_CURVE ( 'NONE', #18374, #191683, #83352, .T. ) ;
#250417 = VERTEX_POINT ( 'NONE', #162945 ) ;
#250418 = DIRECTION ( 'NONE',  ( 0.000000000000000000, -0.2617529984165152257, -0.9651348961777124202 ) ) ;
#250419 = APPLICATION_PROTOCOL_DEFINITION ( 'draft international standard', 'automotive_design', 1998, #245812 ) ;
#250420 = CARTESIAN_POINT ( 'NONE',  ( -20.94999999999999929, 65.70711192142346135, -64.06510546851221477 ) ) ;
#250421 = DIRECTION ( 'NONE',  ( 0.000000000000000000, -0.9126074666063769270, -0.4088369013363280513 ) ) ;
#250422 = CARTESIAN_POINT ( 'NONE',  ( -18.46946985241255845, 85.50931722872357454, -96.03644491902473135 ) ) ;
#250423 = TOROIDAL_SURFACE ( 'NONE', #212841, 4.099999999999999645, 0.1000000000000000056 ) ;
#250424 = ADVANCED_FACE ( 'NONE', ( #20875 ), #3851, .F. ) ;
#250425 = ORIENTED_EDGE ( 'NONE', *, *, #60650, .F. ) ;
#250426 = DIRECTION ( 'NONE',  ( -1.000000000000000000, 0.000000000000000000, -0.000000000000000000 ) ) ;
#250427 = CARTESIAN_POINT ( 'NONE',  ( -21.64999999999999858, 68.65000000001253966, -182.2731074845244166 ) ) ;
#250428 = EDGE_CURVE ( 'NONE', #203266, #212672, #200765, .T. ) ;
#250430 = ADVANCED_FACE ( 'NONE', ( #40447 ), #22151, .F. ) ;
#250429 = EDGE_CURVE ( 'NONE', #254024, #220753, #24729, .T. ) ;
#250431 = VERTEX_POINT ( 'NONE', #104212 ) ;
#250432 = EDGE_LOOP ( 'NONE', ( #219829, #34756, #251885 ) ) ;
#250433 = CARTESIAN_POINT ( 'NONE',  ( -21.05000000000000071, 76.00000000001237765, -170.0231074845243597 ) ) ;
#250434 = DIRECTION ( 'NONE',  ( 1.000000000000000000, 0.000000000000000000, 0.000000000000000000 ) ) ;
#250435 = DIRECTION ( 'NONE',  ( 1.000000000000000000, 0.000000000000000000, 0.000000000000000000 ) ) ;
#250436 = EDGE_CURVE ( 'NONE', #230638, #211078, #142810, .T. ) ;
#250438 = CARTESIAN_POINT ( 'NONE',  ( -17.11825945287481687, 30.11817903451004952, -234.7598257170722889 ) ) ;
#250437 = AXIS2_PLACEMENT_3D ( 'NONE', #89702, #226648, #8902 ) ;
#250441 = CARTESIAN_POINT ( 'NONE',  ( 20.95512820512820440, 10.62384868372303615, -54.75000000000000000 ) ) ;
#250440 = VECTOR ( 'NONE', #136544, 1000.000000000000000 ) ;
#250439 = CARTESIAN_POINT ( 'NONE',  ( -22.47071067811865319, 75.90090754531013317, -211.2431822290224090 ) ) ;
#250442 = DIRECTION ( 'NONE',  ( 0.000000000000000000, 0.000000000000000000, -1.000000000000000000 ) ) ;
#250444 = EDGE_CURVE ( 'NONE', #134996, #222282, #110473, .T. ) ;
#250443 = DIRECTION ( 'NONE',  ( -1.000000000000000000, -0.000000000000000000, -0.000000000000000000 ) ) ;
#250446 = EDGE_CURVE ( 'NONE', #91291, #135352, #245025, .T. ) ;
#250445 = CARTESIAN_POINT ( 'NONE',  ( 23.14999999999999858, 1.115600667400684642E-11, -100.5000000000000426 ) ) ;
#250447 = ORIENTED_EDGE ( 'NONE', *, *, #6896, .F. ) ;
#250449 = EDGE_LOOP ( 'NONE', ( #47743, #47921, #22504, #122704 ) ) ;
#250448 = CARTESIAN_POINT ( 'NONE',  ( -18.50000000000000000, 1.866714910068465239, -145.7526752462820241 ) ) ;
#250450 = DIRECTION ( 'NONE',  ( 0.000000000000000000, -6.982962677686266711E-15, 1.000000000000000000 ) ) ;
#250451 = DIRECTION ( 'NONE',  ( -1.000000000000000000, -0.000000000000000000, -0.000000000000000000 ) ) ;
#250453 = CARTESIAN_POINT ( 'NONE',  ( -18.50000000000000355, 77.26327546522911405, -95.12124281777788326 ) ) ;
#250452 = CARTESIAN_POINT ( 'NONE',  ( -21.05000000000000071, 5.900000000011162093, -157.2809002353436654 ) ) ;
#250454 = EDGE_CURVE ( 'NONE', #60684, #4010, #92946, .T. ) ;
#250455 = ORIENTED_EDGE ( 'NONE', *, *, #135961, .F. ) ;
#250456 = LINE ( 'NONE', #194369, #35437 ) ;
#250457 = CARTESIAN_POINT ( 'NONE',  ( 19.75857864376269291, 64.35000000001197407, -111.7731074845243739 ) ) ;
#250458 = DIRECTION ( 'NONE',  ( 0.5932847527679310229, -0.8049926720990042694, -6.366092712777067056E-16 ) ) ;
#250459 = DIRECTION ( 'NONE',  ( 1.186688945009009831E-16, 1.000000000000000000, 6.982962677686266711E-15 ) ) ;
#250460 = ORIENTED_EDGE ( 'NONE', *, *, #133924, .F. ) ;
#250461 = ADVANCED_FACE ( 'NONE', ( #226735 ), #87216, .T. ) ;
#250463 = EDGE_LOOP ( 'NONE', ( #120648, #129909, #180742, #234890 ) ) ;
#250462 = AXIS2_PLACEMENT_3D ( 'NONE', #94887, #51896, #110610 ) ;
#250464 = DIRECTION ( 'NONE',  ( 2.428612866367624848E-13, -0.4088369013363783999, 0.9126074666063545004 ) ) ;
#250465 = EDGE_LOOP ( 'NONE', ( #239201, #142803, #32903, #113669, #153641 ) ) ;
#250466 = CARTESIAN_POINT ( 'NONE',  ( -22.39999999999999858, 11.75000000001115552, -33.60000000000000142 ) ) ;
#250467 = CARTESIAN_POINT ( 'NONE',  ( -21.14250536705909411, 65.52512344156484403, -242.1460419336806638 ) ) ;
#250468 = CARTESIAN_POINT ( 'NONE',  ( 21.00983514138059505, 6.346420624576639469, 11.97684634237456613 ) ) ;
#250469 = ORIENTED_EDGE ( 'NONE', *, *, #52197, .T. ) ;
#250470 = CARTESIAN_POINT ( 'NONE',  ( 20.04142135623730070, 11.75000000001115907, -88.75000000000004263 ) ) ;
#250471 = CIRCLE ( 'NONE', #129844, 0.5000000000000004441 ) ;
#250472 = LINE ( 'NONE', #32760, #12091 ) ;
#250473 = DIRECTION ( 'NONE',  ( 0.000000000000000000, -0.9651348961777157509, 0.2617529984165031243 ) ) ;
#250474 = VECTOR ( 'NONE', #54743, 1000.000000000000000 ) ;
#250475 = DIRECTION ( 'NONE',  ( 0.000000000000000000, -1.000000000000000000, -6.352154140967427193E-15 ) ) ;
#250476 = DIRECTION ( 'NONE',  ( -1.000000000000000000, 0.000000000000000000, 0.000000000000000000 ) ) ;
#250477 = CARTESIAN_POINT ( 'NONE',  ( 20.85000000000000142, 69.06610602788607878, -166.2374616501508342 ) ) ;
#250479 = DIRECTION ( 'NONE',  ( 0.000000000000000000, 0.000000000000000000, -1.000000000000000000 ) ) ;
#250478 = AXIS2_PLACEMENT_3D ( 'NONE', #124832, #46549, #25724 ) ;
#250480 = EDGE_LOOP ( 'NONE', ( #135500, #169513, #24143, #198095 ) ) ;
#250482 = DIRECTION ( 'NONE',  ( 0.000000000000000000, 0.000000000000000000, -1.000000000000000000 ) ) ;
#250481 = CARTESIAN_POINT ( 'NONE',  ( -23.25000000000000000, 64.25000000001176659, -76.53791325517833855 ) ) ;
#250483 = ORIENTED_EDGE ( 'NONE', *, *, #177624, .F. ) ;
#250485 = EDGE_LOOP ( 'NONE', ( #67384, #56743, #123713 ) ) ;
#250484 = DIRECTION ( 'NONE',  ( 0.000000000000000000, 0.8777080977375072424, -0.4791956752371691608 ) ) ;
#250486 = EDGE_LOOP ( 'NONE', ( #192247, #68948, #63375, #101633 ) ) ;
#250487 = LINE ( 'NONE', #234786, #128355 ) ;
#250488 = AXIS2_PLACEMENT_3D ( 'NONE', #172221, #114764, #134301 ) ;
#250489 = CARTESIAN_POINT ( 'NONE',  ( 13.77030915526558807, 66.54399267394292394, -151.5344739903776485 ) ) ;
#250490 = CARTESIAN_POINT ( 'NONE',  ( 18.49999999999999289, 65.76093837589027657, -78.26871004992719350 ) ) ;
#250491 = DIRECTION ( 'NONE',  ( 6.938893903907991995E-14, 0.000000000000000000, 1.000000000000000000 ) ) ;
#250492 = AXIS2_PLACEMENT_3D ( 'NONE', #24670, #100295, #101568 ) ;
#250493 = ORIENTED_EDGE ( 'NONE', *, *, #211893, .T. ) ;
#250494 = DIRECTION ( 'NONE',  ( 0.000000000000000000, 0.000000000000000000, -1.000000000000000000 ) ) ;
#250495 = CARTESIAN_POINT ( 'NONE',  ( 18.49999999999999289, 10.20857864609425825, -158.7025068656296014 ) ) ;
#250496 = ORIENTED_EDGE ( 'NONE', *, *, #73247, .T. ) ;
#250497 = CIRCLE ( 'NONE', #204697, 0.1000000000000000472 ) ;
#250498 = CARTESIAN_POINT ( 'NONE',  ( -21.05000000000000071, 74.16465844978765176, -124.9679561919613207 ) ) ;
#250499 = EDGE_CURVE ( 'NONE', #7765, #189565, #176190, .T. ) ;
#250500 = CARTESIAN_POINT ( 'NONE',  ( -23.25000000000000000, -11.64999999998884483, -167.4999999999999432 ) ) ;
#250501 = CIRCLE ( 'NONE', #669, 0.09999999999999996392 ) ;
#250502 = ORIENTED_EDGE ( 'NONE', *, *, #82074, .F. ) ;
#250503 = EDGE_CURVE ( 'NONE', #173650, #67578, #68981, .T. ) ;
#250504 = CARTESIAN_POINT ( 'NONE',  ( 23.14999999999999858, 20.70829660003285611, -234.6540061327600597 ) ) ;
#250505 = ORIENTED_EDGE ( 'NONE', *, *, #76968, .T. ) ;
#250506 = CARTESIAN_POINT ( 'NONE',  ( -17.78043020864321022, 65.14640788800629423, -113.3600583188041497 ) ) ;
#250507 = ORIENTED_EDGE ( 'NONE', *, *, #195975, .F. ) ;
#250508 = LINE ( 'NONE', #215247, #226002 ) ;
#250510 =( BOUNDED_CURVE ( )  B_SPLINE_CURVE ( 3, ( #175209, #38228, #138560, #253404 ),
 .UNSPECIFIED., .F., .T. ) 
 B_SPLINE_CURVE_WITH_KNOTS ( ( 4, 4 ),
 ( 0.3000847527772380063, 0.5497968875596834781 ),
 .UNSPECIFIED. ) 
 CURVE ( )  GEOMETRIC_REPRESENTATION_ITEM ( )  RATIONAL_B_SPLINE_CURVE ( ( 1.000000000000000000, 0.9948104011409417691, 0.9948104011409417691, 1.000000000000000000 ) ) 
 REPRESENTATION_ITEM ( '' )  );
#250509 = CIRCLE ( 'NONE', #212926, 0.1000000000000013933 ) ;
#250511 = EDGE_CURVE ( 'NONE', #47980, #62691, #217836, .T. ) ;
#250512 = EDGE_CURVE ( 'NONE', #207912, #41292, #155357, .T. ) ;
#250513 = FACE_OUTER_BOUND ( 'NONE', #242901, .T. ) ;
#250514 = CARTESIAN_POINT ( 'NONE',  ( -20.64999999999999858, 71.65000000001180069, -81.87310748452433984 ) ) ;
#250515 = CIRCLE ( 'NONE', #117257, 0.09999999999999939493 ) ;
#250516 = CARTESIAN_POINT ( 'NONE',  ( -23.25000000000000000, 20.01397631055648674, -237.6853859230195098 ) ) ;
#250517 = DIRECTION ( 'NONE',  ( -0.000000000000000000, -0.1350103645451876666, 0.9908441862701600211 ) ) ;
#250518 = DIRECTION ( 'NONE',  ( 0.000000000000000000, -0.4088369013363783999, 0.9126074666063545004 ) ) ;
#250519 = DIRECTION ( 'NONE',  ( 0.000000000000000000, 1.000000000000000000, 6.982962677686266711E-15 ) ) ;
#250520 = VECTOR ( 'NONE', #81377, 1000.000000000000000 ) ;
#250521 = ORIENTED_EDGE ( 'NONE', *, *, #131792, .F. ) ;
#250522 = FACE_OUTER_BOUND ( 'NONE', #153459, .T. ) ;
#250523 = AXIS2_PLACEMENT_3D ( 'NONE', #198768, #159662, #239189 ) ;
#250524 = VERTEX_POINT ( 'NONE', #246314 ) ;
#250526 = DIRECTION ( 'NONE',  ( -0.000000000000000000, 0.2128009952263603677, -0.9770955615653313941 ) ) ;
#250525 = PLANE ( 'NONE',  #28155 ) ;
#250527 = AXIS2_PLACEMENT_3D ( 'NONE', #237003, #94904, #17938 ) ;
#250528 = ADVANCED_FACE ( 'NONE', ( #131492 ), #55316, .T. ) ;
#250529 = ORIENTED_EDGE ( 'NONE', *, *, #35283, .T. ) ;
#250530 = CYLINDRICAL_SURFACE ( 'NONE', #122589, 2.000000000000001776 ) ;
#250531 = CIRCLE ( 'NONE', #25680, 0.1000000000000024342 ) ;
#250532 = EDGE_CURVE ( 'NONE', #58292, #206737, #91090, .T. ) ;
#250533 = FACE_OUTER_BOUND ( 'NONE', #59436, .T. ) ;
#250534 = CARTESIAN_POINT ( 'NONE',  ( -17.78043020864319956, 59.46182193223923207, -223.0376142573344111 ) ) ;
#250535 = SPHERICAL_SURFACE ( 'NONE', #116781, 0.1000000000000000056 ) ;
#250536 = ORIENTED_EDGE ( 'NONE', *, *, #36832, .F. ) ;
#250538 = ORIENTED_EDGE ( 'NONE', *, *, #249728, .T. ) ;
#250537 = CARTESIAN_POINT ( 'NONE',  ( 22.84999999999999787, 0.000000000000000000, 0.000000000000000000 ) ) ;
#250540 = DIRECTION ( 'NONE',  ( 0.000000000000000000, 0.1071148137998806232, 0.9942466578594150173 ) ) ;
#250539 = DIRECTION ( 'NONE',  ( 0.000000000000000000, 0.9856811345164832039, 0.1686199900910280158 ) ) ;
#250542 = VERTEX_POINT ( 'NONE', #170677 ) ;
#250541 = DIRECTION ( 'NONE',  ( 0.000000000000000000, -0.9126074666063771490, -0.4088369013363281623 ) ) ;
#250543 = ADVANCED_FACE ( 'NONE', ( #71548 ), #59605, .F. ) ;
#250544 = ORIENTED_EDGE ( 'NONE', *, *, #112734, .F. ) ;
#250545 = EDGE_CURVE ( 'NONE', #196401, #17135, #130195, .T. ) ;
#250546 = AXIS2_PLACEMENT_3D ( 'NONE', #108896, #183972, #242651 ) ;
#250547 = CARTESIAN_POINT ( 'NONE',  ( 21.05000000000000071, 76.00000000001142553, -36.02310748452432421 ) ) ;
#250548 = CARTESIAN_POINT ( 'NONE',  ( 21.05000000000000071, 67.12338541492479749, -94.63802700567968884 ) ) ;
#250549 = VERTEX_POINT ( 'NONE', #205892 ) ;
#250550 = CARTESIAN_POINT ( 'NONE',  ( -23.25000000000000000, 77.83585931145526615, -58.01866831572577610 ) ) ;
#250551 = ORIENTED_EDGE ( 'NONE', *, *, #193771, .T. ) ;
#250552 = DIRECTION ( 'NONE',  ( 1.000000000000000000, 0.000000000000000000, 0.000000000000000000 ) ) ;
#250553 = CARTESIAN_POINT ( 'NONE',  ( 20.94999999999999929, 76.00000000001142553, -36.02310748452432421 ) ) ;
#250554 = ORIENTED_EDGE ( 'NONE', *, *, #75590, .F. ) ;
#250555 = EDGE_CURVE ( 'NONE', #20329, #124432, #28604, .T. ) ;
#250556 = DIRECTION ( 'NONE',  ( 1.000000000000000000, 0.000000000000000000, 0.000000000000000000 ) ) ;
#250557 = AXIS2_PLACEMENT_3D ( 'NONE', #185812, #42446, #226186 ) ;
#250558 = EDGE_CURVE ( 'NONE', #150745, #235335, #68020, .T. ) ;
#250559 = EDGE_LOOP ( 'NONE', ( #177279, #175845, #85795, #189417 ) ) ;
#250560 = CYLINDRICAL_SURFACE ( 'NONE', #131132, 0.09999999999999530098 ) ;
#250561 = ADVANCED_FACE ( 'NONE', ( #106786 ), #191505, .T. ) ;
#250563 = ORIENTED_EDGE ( 'NONE', *, *, #39337, .T. ) ;
#250562 = AXIS2_PLACEMENT_3D ( 'NONE', #213872, #255512, #211309 ) ;
#250564 = ORIENTED_EDGE ( 'NONE', *, *, #71695, .T. ) ;
#250565 = CARTESIAN_POINT ( 'NONE',  ( 20.50589344624752286, 18.75447916118790914, -228.0677351699049495 ) ) ;
#250566 = ORIENTED_EDGE ( 'NONE', *, *, #83812, .T. ) ;
#250567 = LINE ( 'NONE', #193191, #121290 ) ;
#250568 = ORIENTED_EDGE ( 'NONE', *, *, #85599, .F. ) ;
#250570 = ORIENTED_EDGE ( 'NONE', *, *, #136672, .F. ) ;
#250569 = LINE ( 'NONE', #51055, #125970 ) ;
#250571 = ADVANCED_FACE ( 'NONE', ( #235718 ), #154939, .T. ) ;
#250572 = ORIENTED_EDGE ( 'NONE', *, *, #26803, .F. ) ;
#250573 = DIRECTION ( 'NONE',  ( -1.000000000000000000, -0.000000000000000000, 0.000000000000000000 ) ) ;
#250574 = ORIENTED_EDGE ( 'NONE', *, *, #98781, .T. ) ;
#250577 = VERTEX_POINT ( 'NONE', #54520 ) ;
#250576 = ORIENTED_EDGE ( 'NONE', *, *, #64611, .T. ) ;
#250575 = DIRECTION ( 'NONE',  ( 0.000000000000000000, 0.9908441862701596881, -0.1350103645451904977 ) ) ;
#250578 = ADVANCED_FACE ( 'NONE', ( #212337 ), #136609, .T. ) ;
#250579 = CARTESIAN_POINT ( 'NONE',  ( -21.65000000000000213, 12.03275902784684703, -220.0251779199349187 ) ) ;
#250580 = AXIS2_PLACEMENT_3D ( 'NONE', #179873, #239842, #45479 ) ;
#250581 = ORIENTED_EDGE ( 'NONE', *, *, #129260, .T. ) ;
#250582 = AXIS2_PLACEMENT_3D ( 'NONE', #105997, #183011, #188134 ) ;
#250583 = AXIS2_PLACEMENT_3D ( 'NONE', #129581, #72188, #112589 ) ;
#250584 = ADVANCED_BREP_SHAPE_REPRESENTATION ( '', ( #111872, #2425 ), #185415 ) ;
#250585 = CARTESIAN_POINT ( 'NONE',  ( -16.97683809663752186, 9.950000000011138823, -42.75000000000000000 ) ) ;
#250586 = VERTEX_POINT ( 'NONE', #117072 ) ;
#250587 = CARTESIAN_POINT ( 'NONE',  ( -16.94107738177414291, 10.01423928514777373, -154.9500000000000455 ) ) ;
#250588 = EDGE_CURVE ( 'NONE', #14516, #106738, #188624, .T. ) ;
#250590 = EDGE_LOOP ( 'NONE', ( #244752, #101578, #83170, #188295 ) ) ;
#250589 = DIRECTION ( 'NONE',  ( 0.000000000000000000, 0.000000000000000000, -1.000000000000000000 ) ) ;
#250591 = DIRECTION ( 'NONE',  ( 1.000000000000000000, 0.000000000000000000, 0.000000000000000000 ) ) ;
#250592 = VERTEX_POINT ( 'NONE', #115782 ) ;
#250593 = CARTESIAN_POINT ( 'NONE',  ( 20.95429693346636313, 65.45669512011612312, -95.46222494621135013 ) ) ;
#250594 = LINE ( 'NONE', #30286, #239810 ) ;
#250595 = ORIENTED_EDGE ( 'NONE', *, *, #236743, .T. ) ;
#250596 = CARTESIAN_POINT ( 'NONE',  ( -20.85000000000000142, 76.00000000001142553, -36.02310748452432421 ) ) ;
#250597 = CARTESIAN_POINT ( 'NONE',  ( 18.54148534481893762, 18.40294846151842734, -236.9778203247716419 ) ) ;
#250598 = CIRCLE ( 'NONE', #38241, 0.09999999999999939493 ) ;
#250599 = ORIENTED_EDGE ( 'NONE', *, *, #245317, .T. ) ;
#250601 = VERTEX_POINT ( 'NONE', #37544 ) ;
#250600 = CARTESIAN_POINT ( 'NONE',  ( 20.04142135391667168, 54.39878304051241997, -228.7287286064368743 ) ) ;
#250602 = DIRECTION ( 'NONE',  ( 0.000000000000000000, 0.2128009952263568427, -0.9770955615653322823 ) ) ;
#250604 = VERTEX_POINT ( 'NONE', #113210 ) ;
#250603 = EDGE_LOOP ( 'NONE', ( #164265, #84742, #44356, #226626, #113025 ) ) ;
#250605 = EDGE_LOOP ( 'NONE', ( #179738, #78542, #869, #131849 ) ) ;
#250606 = CARTESIAN_POINT ( 'NONE',  ( -21.14999999999999858, 6.093673009692400555, -199.5727803633481301 ) ) ;
#250607 = ORIENTED_EDGE ( 'NONE', *, *, #76895, .T. ) ;
#250608 = ORIENTED_EDGE ( 'NONE', *, *, #69926, .F. ) ;
#250609 = CARTESIAN_POINT ( 'NONE',  ( 20.94999999999999929, -9.000000000000000000, -24.00603087734755547 ) ) ;
#250610 = ORIENTED_EDGE ( 'NONE', *, *, #252388, .T. ) ;
#250611 = DIRECTION ( 'NONE',  ( 0.000000000000000000, 1.156482317317873105E-15, -1.000000000000000000 ) ) ;
#250612 = DIRECTION ( 'NONE',  ( 0.000000000000000000, 0.000000000000000000, 1.000000000000000000 ) ) ;
#250613 = ORIENTED_EDGE ( 'NONE', *, *, #70252, .F. ) ;
#250614 = AXIS2_PLACEMENT_3D ( 'NONE', #126721, #62891, #65454 ) ;
#250615 = CIRCLE ( 'NONE', #59050, 3.900000000000000799 ) ;
#250616 = EDGE_LOOP ( 'NONE', ( #165295, #247537, #212958, #26204 ) ) ;
#250617 = CIRCLE ( 'NONE', #167460, 0.09999999999998898659 ) ;
#250618 = CARTESIAN_POINT ( 'NONE',  ( 20.73486653747088937, 7.750000000011182166, -109.7500000000000426 ) ) ;
#250619 = ORIENTED_EDGE ( 'NONE', *, *, #26630, .T. ) ;
#250620 = CARTESIAN_POINT ( 'NONE',  ( -21.14999999999999858, 76.10000000001245724, -181.6726782920691505 ) ) ;
#250621 = ORIENTED_EDGE ( 'NONE', *, *, #65152, .F. ) ;
#250622 = SPHERICAL_SURFACE ( 'NONE', #145973, 0.1000000000000000056 ) ;
#250623 = EDGE_CURVE ( 'NONE', #202942, #139907, #246884, .T. ) ;
#250625 = ORIENTED_EDGE ( 'NONE', *, *, #253871, .T. ) ;
#250624 = DIRECTION ( 'NONE',  ( 0.000000000000000000, -0.9999176327611369874, 0.01283462868041987913 ) ) ;
#250626 = DIRECTION ( 'NONE',  ( -0.000000000000000000, 0.1350103645451626311, 0.9908441862701635738 ) ) ;
#250627 = CARTESIAN_POINT ( 'NONE',  ( 20.94999999999999574, 74.83729825007408465, -128.5231074845243029 ) ) ;
#250628 = CARTESIAN_POINT ( 'NONE',  ( -18.59999999999999787, 36.65892442174472876, -249.5511627012454596 ) ) ;
#250629 = CARTESIAN_POINT ( 'NONE',  ( 18.59999999999999076, 6.450000000011156587, -144.0170271704400307 ) ) ;
#250630 = AXIS2_PLACEMENT_3D ( 'NONE', #16356, #33373, #13768 ) ;
#250631 = CARTESIAN_POINT ( 'NONE',  ( 23.14999999999999503, 6.550000000011156231, -88.15000000000004832 ) ) ;
#250632 = EDGE_CURVE ( 'NONE', #84368, #132438, #16700, .T. ) ;
#250633 = DIRECTION ( 'NONE',  ( -1.000000000000000000, -0.000000000000000000, -0.000000000000000000 ) ) ;
#250635 = ADVANCED_FACE ( 'NONE', ( #233193 ), #152371, .F. ) ;
#250634 = CARTESIAN_POINT ( 'NONE',  ( 22.94999999999999929, 0.000000000000000000, 4.000000000000000000 ) ) ;
#250636 = CARTESIAN_POINT ( 'NONE',  ( 18.44206774312972641, 38.01831701715774869, -261.0463157240239980 ) ) ;
#250637 = DIRECTION ( 'NONE',  ( 0.000000000000000000, 0.9770955615652945347, 0.2128009952265300653 ) ) ;
#250638 = ORIENTED_EDGE ( 'NONE', *, *, #9631, .T. ) ;
#250640 = ORIENTED_EDGE ( 'NONE', *, *, #204088, .F. ) ;
#250639 = VERTEX_POINT ( 'NONE', #137889 ) ;
#250641 = ORIENTED_EDGE ( 'NONE', *, *, #123417, .T. ) ;
#250642 = EDGE_CURVE ( 'NONE', #61685, #82775, #38802, .T. ) ;
#250643 = CARTESIAN_POINT ( 'NONE',  ( -17.27223548804785125, 65.65460260859495634, -91.65671366372575335 ) ) ;
#250644 = VECTOR ( 'NONE', #33863, 1000.000000000000114 ) ;
#250645 = LINE ( 'NONE', #91592, #194574 ) ;
#250647 = CARTESIAN_POINT ( 'NONE',  ( 21.13614978966382552, 1.399903376081983231, -230.6638703635511831 ) ) ;
#250646 = DIRECTION ( 'NONE',  ( 0.000000000000000000, -7.034366652768095332E-15, 1.000000000000000000 ) ) ;
#250648 = ORIENTED_EDGE ( 'NONE', *, *, #226984, .T. ) ;
#250649 = ORIENTED_EDGE ( 'NONE', *, *, #37597, .T. ) ;
#250650 = AXIS2_PLACEMENT_3D ( 'NONE', #7620, #244938, #147114 ) ;
#250651 =( NAMED_UNIT ( * ) PLANE_ANGLE_UNIT ( ) SI_UNIT ( $, .RADIAN. ) );
#250652 = CARTESIAN_POINT ( 'NONE',  ( 20.95512820512820440, 67.12384868372345181, -57.37310748452438247 ) ) ;
#250653 = AXIS2_PLACEMENT_3D ( 'NONE', #12583, #56783, #73848 ) ;
#250654 = DIRECTION ( 'NONE',  ( 1.000000000000000000, 0.000000000000000000, 0.000000000000000000 ) ) ;
#250655 = AXIS2_PLACEMENT_3D ( 'NONE', #122808, #24998, #45817 ) ;
#250656 = CIRCLE ( 'NONE', #96698, 0.09999999999999939493 ) ;
#250657 = CARTESIAN_POINT ( 'NONE',  ( -23.15000000000000213, 67.23127455305841238, -235.8551265064783991 ) ) ;
#250658 = ORIENTED_EDGE ( 'NONE', *, *, #1938, .T. ) ;
#250659 = ORIENTED_EDGE ( 'NONE', *, *, #59360, .T. ) ;
#250660 = CARTESIAN_POINT ( 'NONE',  ( -16.87683809663752399, 9.850000000011144508, -180.9023640181962662 ) ) ;
#250661 = CIRCLE ( 'NONE', #109185, 0.5999999999999934275 ) ;
#250662 = CARTESIAN_POINT ( 'NONE',  ( 23.24999999999999289, 64.25000000001193712, -102.9231074845243938 ) ) ;
#250663 = AXIS2_PLACEMENT_3D ( 'NONE', #235660, #58297, #34944 ) ;
#250664 = EDGE_CURVE ( 'NONE', #142779, #123629, #194058, .T. ) ;
#250665 = CARTESIAN_POINT ( 'NONE',  ( -18.54118089899633048, 78.20985128365940398, -231.5294076491229589 ) ) ;
#250667 = ORIENTED_EDGE ( 'NONE', *, *, #241797, .F. ) ;
#250666 = DIRECTION ( 'NONE',  ( 2.952720810173289112E-16, -1.000000000000000000, 0.000000000000000000 ) ) ;
#250668 = EDGE_CURVE ( 'NONE', #59743, #132097, #114499, .T. ) ;
#250669 = CARTESIAN_POINT ( 'NONE',  ( 20.94999999999999929, 67.65998959290219261, -227.8609496483021530 ) ) ;
#250670 = PLANE ( 'NONE',  #227230 ) ;
#250671 = CARTESIAN_POINT ( 'NONE',  ( 18.59999999999999787, -1.835859311432481045, -78.50443916879852679 ) ) ;
#250673 = AXIS2_PLACEMENT_3D ( 'NONE', #205102, #105998, #166029 ) ;
#250672 = CARTESIAN_POINT ( 'NONE',  ( 18.43579564894459111, 85.51932753530431341, -96.05013084066375484 ) ) ;
#250674 = EDGE_LOOP ( 'NONE', ( #22653, #232051, #93570, #73872, #139056, #226902, #17549 ) ) ;
#250675 = CARTESIAN_POINT ( 'NONE',  ( 20.94999999999999929, 76.00000000001192291, -105.0231074845243029 ) ) ;
#250676 = CARTESIAN_POINT ( 'NONE',  ( -23.15000000000000213, 74.08971962618002749, -82.15447533972326255 ) ) ;
#250677 = AXIS2_PLACEMENT_3D ( 'NONE', #93227, #114071, #234023 ) ;
#250679 = CARTESIAN_POINT ( 'NONE',  ( 23.15000000000000213, -11.48912529306489994, -164.4000000000000057 ) ) ;
#250678 = CARTESIAN_POINT ( 'NONE',  ( 21.05000000000000071, 4.999999999999997335, -21.49473398108690603 ) ) ;
#250680 = DIRECTION ( 'NONE',  ( 1.000000000000000000, 0.000000000000000000, 0.000000000000000000 ) ) ;
#250681 = CARTESIAN_POINT ( 'NONE',  ( 19.99999999999998934, 64.25000000001222134, -148.6731074845244507 ) ) ;
#250682 = EDGE_CURVE ( 'NONE', #55154, #129211, #196997, .T. ) ;
#250684 = DIRECTION ( 'NONE',  ( 1.000000000000000000, 0.000000000000000000, 0.000000000000000000 ) ) ;
#250683 = AXIS2_PLACEMENT_3D ( 'NONE', #4822, #144329, #166523 ) ;
#250685 = DIRECTION ( 'NONE',  ( 1.000000000000000000, 0.000000000000000000, 0.000000000000000000 ) ) ;
#250686 = DIRECTION ( 'NONE',  ( 0.000000000000000000, 0.8814952561688476074, -0.4721928772777262417 ) ) ;
#250687 = CARTESIAN_POINT ( 'NONE',  ( 12.25000000000000000, 62.59162599727320497, -217.2417264603073761 ) ) ;
#250688 = CIRCLE ( 'NONE', #88158, 0.09999999999999363565 ) ;
#250689 = ORIENTED_EDGE ( 'NONE', *, *, #110469, .F. ) ;
#250690 = ORIENTED_EDGE ( 'NONE', *, *, #11424, .F. ) ;
#250691 = AXIS2_PLACEMENT_3D ( 'NONE', #173181, #74062, #153617 ) ;
#250692 = ORIENTED_EDGE ( 'NONE', *, *, #126828, .T. ) ;
#250693 = FACE_OUTER_BOUND ( 'NONE', #65256, .T. ) ;
#250694 = CARTESIAN_POINT ( 'NONE',  ( -21.65000000000000213, 7.250000000011138646, -176.7499999999999716 ) ) ;
#250695 = ORIENTED_EDGE ( 'NONE', *, *, #166871, .T. ) ;
#250696 = VECTOR ( 'NONE', #46551, 1000.000000000000000 ) ;
#250697 = DIRECTION ( 'NONE',  ( 1.000000000000000000, 0.000000000000000000, 0.000000000000000000 ) ) ;
#250699 = ADVANCED_FACE ( 'NONE', ( #253997 ), #135328, .F. ) ;
#250698 = ORIENTED_EDGE ( 'NONE', *, *, #244547, .T. ) ;
#250701 = ORIENTED_EDGE ( 'NONE', *, *, #215485, .F. ) ;
#250700 = CIRCLE ( 'NONE', #54878, 0.1000000000000002554 ) ;
#250702 = CARTESIAN_POINT ( 'NONE',  ( -22.57320508075687115, 11.75000000001115552, -167.4999999999999716 ) ) ;
#250703 = AXIS2_PLACEMENT_3D ( 'NONE', #137852, #177031, #212294 ) ;
#250704 = ORIENTED_EDGE ( 'NONE', *, *, #111307, .F. ) ;
#250705 = CIRCLE ( 'NONE', #59137, 0.09999999999998898659 ) ;
#250707 = FACE_OUTER_BOUND ( 'NONE', #235549, .T. ) ;
#250706 = VECTOR ( 'NONE', #61160, 1000.000000000000000 ) ;
#250708 = DIRECTION ( 'NONE',  ( 0.000000000000000000, 0.000000000000000000, -1.000000000000000000 ) ) ;
#250709 = CARTESIAN_POINT ( 'NONE',  ( -21.55000000000000426, 29.41239393758413811, -236.9245051605820720 ) ) ;
#250710 = EDGE_CURVE ( 'NONE', #19770, #226091, #5621, .T. ) ;
#250711 = CARTESIAN_POINT ( 'NONE',  ( -22.39999999999999858, 75.90000000001219860, -144.3138870828977076 ) ) ;
#250712 = DIRECTION ( 'NONE',  ( 0.000000000000000000, -0.5000000000000275335, -0.8660254037844228314 ) ) ;
#250714 = ORIENTED_EDGE ( 'NONE', *, *, #219462, .T. ) ;
#250713 = DIRECTION ( 'NONE',  ( -1.000000000000000000, 9.012599976028471648E-15, 6.882867235861662930E-14 ) ) ;
#250716 = DIRECTION ( 'NONE',  ( 1.000000000000000000, 0.000000000000000000, 0.000000000000000000 ) ) ;
#250715 = DIRECTION ( 'NONE',  ( 0.000000000000000000, -7.116814260417668513E-15, 1.000000000000000000 ) ) ;
#250717 = DIRECTION ( 'NONE',  ( 0.000000000000000000, 0.000000000000000000, -1.000000000000000000 ) ) ;
#250718 = CARTESIAN_POINT ( 'NONE',  ( -22.94999999999999929, -1.212568896937008089, -8.000000000000000000 ) ) ;
#250719 = DIRECTION ( 'NONE',  ( -1.000000000000000000, 2.952720810173289112E-16, 2.061873921506763405E-30 ) ) ;
#250721 = EDGE_CURVE ( 'NONE', #160806, #74964, #218013, .T. ) ;
#250720 = CARTESIAN_POINT ( 'NONE',  ( -18.59999999999999787, 64.35000000001259934, -191.3731074845244393 ) ) ;
#250722 = ADVANCED_FACE ( 'NONE', ( #217424 ), #173242, .T. ) ;
#250723 = ORIENTED_EDGE ( 'NONE', *, *, #118833, .T. ) ;
#250724 = FILL_AREA_STYLE ('',( #53816 ) ) ;
#250725 = DIRECTION ( 'NONE',  ( 0.000000000000000000, -0.2128009952263403282, 0.9770955615653358350 ) ) ;
#250726 = DIRECTION ( 'NONE',  ( 0.000000000000000000, 0.8496786552930111203, 0.5273008465188163685 ) ) ;
#250727 = AXIS2_PLACEMENT_3D ( 'NONE', #234653, #195553, #233398 ) ;
#250728 = EDGE_LOOP ( 'NONE', ( #178138, #233332, #44878, #172058 ) ) ;
#250729 = ADVANCED_FACE ( 'NONE', ( #38823 ), #53245, .F. ) ;
#250730 = FACE_OUTER_BOUND ( 'NONE', #246933, .T. ) ;
#250731 = ADVANCED_FACE ( 'NONE', ( #72838 ), #238892, .T. ) ;
#250732 = CARTESIAN_POINT ( 'NONE',  ( 21.14999999999999858, -0.09770955614504285569, -201.0212800995241764 ) ) ;
#250733 = FACE_OUTER_BOUND ( 'NONE', #16253, .T. ) ;
#250734 = ORIENTED_EDGE ( 'NONE', *, *, #53115, .F. ) ;
#250735 = EDGE_CURVE ( 'NONE', #34617, #99386, #76366, .T. ) ;
#250736 = VERTEX_POINT ( 'NONE', #98739 ) ;
#250737 = DIRECTION ( 'NONE',  ( -1.000000000000000000, 0.000000000000000000, -0.000000000000000000 ) ) ;
#250738 = CARTESIAN_POINT ( 'NONE',  ( 20.94999999999999929, 10.72371710470752149, -21.25000000000000000 ) ) ;
#250739 = EDGE_CURVE ( 'NONE', #222373, #125758, #93132, .T. ) ;
#250740 = CARTESIAN_POINT ( 'NONE',  ( -20.54999999999999716, 71.65000000001228386, -157.6731074845243938 ) ) ;
#250741 = LINE ( 'NONE', #224750, #219394 ) ;
#250743 = DIRECTION ( 'NONE',  ( 1.000000000000000000, 0.000000000000000000, 0.000000000000000000 ) ) ;
#250742 = DIRECTION ( 'NONE',  ( 0.000000000000000000, 1.000000000000000000, 0.000000000000000000 ) ) ;
#250744 = CARTESIAN_POINT ( 'NONE',  ( -18.50000000000000711, 11.74999999999999645, -7.014805770653998351 ) ) ;
#250746 = EDGE_CURVE ( 'NONE', #196101, #156778, #120946, .T. ) ;
#250745 = CARTESIAN_POINT ( 'NONE',  ( 15.73863059295127798, 9.351403174152808973, -50.47953043683848762 ) ) ;
#250748 = ADVANCED_FACE ( 'NONE', ( #203009 ), #38995, .F. ) ;
#250747 = CARTESIAN_POINT ( 'NONE',  ( 22.39999999999999858, 68.20922040163827660, -69.62310748452438247 ) ) ;
#250749 = ORIENTED_EDGE ( 'NONE', *, *, #201216, .F. ) ;
#250750 = DIRECTION ( 'NONE',  ( 1.000000000000000000, 0.000000000000000000, 0.000000000000000000 ) ) ;
#250752 = ORIENTED_EDGE ( 'NONE', *, *, #87740, .T. ) ;
#250751 = DIRECTION ( 'NONE',  ( 0.000000000000000000, -0.8814952561688428334, 0.4721928772777349570 ) ) ;
#250753 = CARTESIAN_POINT ( 'NONE',  ( 21.46681500593530956, 69.14248884063026424, -170.0231074845244166 ) ) ;
#250754 = DIRECTION ( 'NONE',  ( 0.000000000000000000, 0.2617529984165045120, 0.9651348961777153068 ) ) ;
#250756 = DIRECTION ( 'NONE',  ( 0.000000000000000000, -0.4791956752371546169, -0.8777080977375152360 ) ) ;
#250755 = CARTESIAN_POINT ( 'NONE',  ( 23.15000000000000213, 11.60058429089262333, -246.3380203656811887 ) ) ;
#250757 = CARTESIAN_POINT ( 'NONE',  ( -16.77308656112214535, 66.05000000001207638, -123.8729142928220455 ) ) ;
#250758 = EDGE_CURVE ( 'NONE', #19000, #154288, #172307, .T. ) ;
#250759 = DIRECTION ( 'NONE',  ( -0.000000000000000000, 1.000000000000000000, 6.982962677686266711E-15 ) ) ;
#250761 = ORIENTED_EDGE ( 'NONE', *, *, #24991, .F. ) ;
#250760 = DIRECTION ( 'NONE',  ( 1.000000000000000000, 0.000000000000000000, 0.000000000000000000 ) ) ;
#250763 = CARTESIAN_POINT ( 'NONE',  ( 21.05000000000000071, 1.115600667400684642E-11, -171.6000000000000227 ) ) ;
#250762 = APPLICATION_CONTEXT ( 'automotive_design' ) ;
#250764 = CARTESIAN_POINT ( 'NONE',  ( -23.25000000000000000, 77.14957036958755054, -95.20719500002232394 ) ) ;
#250765 = CARTESIAN_POINT ( 'NONE',  ( 22.50014994444007499, 11.74971973190315389, -66.91691984328092246 ) ) ;
#250766 = DIRECTION ( 'NONE',  ( -1.000000000000000000, 0.000000000000000000, -0.000000000000000000 ) ) ;
#250767 = VERTEX_POINT ( 'NONE', #179623 ) ;
#250768 = LINE ( 'NONE', #190838, #209628 ) ;
#250769 = EDGE_CURVE ( 'NONE', #192885, #141859, #122204, .T. ) ;
#250770 = ORIENTED_EDGE ( 'NONE', *, *, #62317, .T. ) ;
#250771 = EDGE_CURVE ( 'NONE', #247011, #103860, #240869, .T. ) ;
#250772 = EDGE_CURVE ( 'NONE', #38057, #136029, #188823, .T. ) ;
#250773 = CARTESIAN_POINT ( 'NONE',  ( 21.05000000000000071, -3.770473190032740174, -225.9805569534692324 ) ) ;
#250774 = ORIENTED_EDGE ( 'NONE', *, *, #143162, .F. ) ;
#250775 = CYLINDRICAL_SURFACE ( 'NONE', #159377, 0.09999999999999939493 ) ;
#250776 = EDGE_LOOP ( 'NONE', ( #181219, #202700 ) ) ;
#250777 = CIRCLE ( 'NONE', #204789, 0.5000000000000004441 ) ;
#250778 = DIRECTION ( 'NONE',  ( 0.000000000000000000, 0.000000000000000000, -1.000000000000000000 ) ) ;
#250779 = DIRECTION ( 'NONE',  ( 1.000000000000000000, -0.000000000000000000, -0.000000000000000000 ) ) ;
#250780 = CARTESIAN_POINT ( 'NONE',  ( 20.94999999999999929, 69.35000000001205933, -124.3731074845243540 ) ) ;
#250781 = ORIENTED_EDGE ( 'NONE', *, *, #181940, .T. ) ;
#250782 = ADVANCED_FACE ( 'NONE', ( #200454 ), #122190, .F. ) ;
#250783 = EDGE_CURVE ( 'NONE', #30238, #168004, #197874, .T. ) ;
#250784 = CARTESIAN_POINT ( 'NONE',  ( -16.82055514392378726, 9.949999999999985079, -12.67679807454204344 ) ) ;
#250785 = DIRECTION ( 'NONE',  ( 0.000000000000000000, 0.000000000000000000, -1.000000000000000000 ) ) ;
#250786 = AXIS2_PLACEMENT_3D ( 'NONE', #3332, #200278, #141578 ) ;
#250787 = CARTESIAN_POINT ( 'NONE',  ( 18.39999999999999858, 86.89640087696871262, -199.6396878666313341 ) ) ;
#250788 = CIRCLE ( 'NONE', #242967, 0.5000000000000004441 ) ;
#250789 = LINE ( 'NONE', #133420, #257727 ) ;
#250790 = CARTESIAN_POINT ( 'NONE',  ( 23.25000000000000000, -11.74999999998883560, -55.25000000000004974 ) ) ;
#250791 = ORIENTED_EDGE ( 'NONE', *, *, #138619, .T. ) ;
#250792 = CARTESIAN_POINT ( 'NONE',  ( -18.59999994787167310, 85.52363768977403424, -129.6406579497522387 ) ) ;
#250793 = EDGE_LOOP ( 'NONE', ( #90260, #169681, #219808, #161811 ) ) ;
#250795 = ORIENTED_EDGE ( 'NONE', *, *, #16392, .T. ) ;
#250794 = DIRECTION ( 'NONE',  ( 0.000000000000000000, -6.982962677686266711E-15, 1.000000000000000000 ) ) ;
#250796 = ORIENTED_EDGE ( 'NONE', *, *, #166097, .F. ) ;
#250797 = DIRECTION ( 'NONE',  ( -1.000000000000000000, 0.000000000000000000, -0.000000000000000000 ) ) ;
#250798 = CARTESIAN_POINT ( 'NONE',  ( -21.05000000000000071, 70.42128727326085880, -228.5349014959848262 ) ) ;
#250799 = CARTESIAN_POINT ( 'NONE',  ( 22.00411653889210228, 0.09903810579712941931, -26.24655713235960164 ) ) ;
#250800 = CARTESIAN_POINT ( 'NONE',  ( -22.50000000000088463, 75.95463834342392317, -81.17361631873501437 ) ) ;
#250801 = ORIENTED_EDGE ( 'NONE', *, *, #49861, .F. ) ;
#250802 = FACE_OUTER_BOUND ( 'NONE', #116844, .T. ) ;
#250803 = CARTESIAN_POINT ( 'NONE',  ( -20.94999999999999929, 11.75000000000000000, -7.014805770654001016 ) ) ;
#250804 = ORIENTED_EDGE ( 'NONE', *, *, #180911, .T. ) ;
#250806 = ORIENTED_EDGE ( 'NONE', *, *, #170786, .T. ) ;
#250805 = CARTESIAN_POINT ( 'NONE',  ( -21.05000000000000071, 17.11694853917243364, -224.3781540347815451 ) ) ;
#250807 = CIRCLE ( 'NONE', #184159, 0.1000000000000070832 ) ;
#250808 = AXIS2_PLACEMENT_3D ( 'NONE', #19890, #194693, #156848 ) ;
#250809 = CARTESIAN_POINT ( 'NONE',  ( 21.05000000000000071, 65.27628289530507288, -191.3731074845244393 ) ) ;
#250810 = CARTESIAN_POINT ( 'NONE',  ( 23.14999999999999147, 1.115600667400684642E-11, -134.0000000000000000 ) ) ;
#250811 = CIRCLE ( 'NONE', #163337, 1.900000000000012790 ) ;
#250812 = ADVANCED_FACE ( 'NONE', ( #21822 ), #206219, .T. ) ;
#250813 = EDGE_CURVE ( 'NONE', #177002, #249313, #42655, .T. ) ;
#250814 = ORIENTED_EDGE ( 'NONE', *, *, #80957, .F. ) ;
#250815 = DIRECTION ( 'NONE',  ( 0.000000000000000000, 0.000000000000000000, -1.000000000000000000 ) ) ;
#250816 = CARTESIAN_POINT ( 'NONE',  ( -20.94999999999999929, 18.34711819382569686, -236.8747682978092541 ) ) ;
#250817 = ORIENTED_EDGE ( 'NONE', *, *, #184204, .F. ) ;
#250818 = DIRECTION ( 'NONE',  ( 0.000000000000000000, 0.1568667991644863147, -0.9876197685951252359 ) ) ;
#250819 = AXIS2_PLACEMENT_3D ( 'NONE', #72840, #75407, #194060 ) ;
#250820 = CARTESIAN_POINT ( 'NONE',  ( -20.85000000000000142, -1.835859311432479268, -145.5044391687985694 ) ) ;
#250821 = EDGE_CURVE ( 'NONE', #88325, #53791, #72313, .T. ) ;
#250822 = VECTOR ( 'NONE', #155121, 1000.000000000000000 ) ;
#250823 = ORIENTED_EDGE ( 'NONE', *, *, #208917, .F. ) ;
#250824 = CARTESIAN_POINT ( 'NONE',  ( 23.24999999999999645, 1.115600667400684642E-11, -134.0000000000000284 ) ) ;
#250825 = EDGE_LOOP ( 'NONE', ( #256470, #221386, #24191, #194522, #5013, #189633 ) ) ;
#250826 = CARTESIAN_POINT ( 'NONE',  ( -18.59999999999999787, -1.164121893230052995, -141.9148480855716343 ) ) ;
#250827 = CIRCLE ( 'NONE', #96864, 11.65000000000000391 ) ;
#250829 = ORIENTED_EDGE ( 'NONE', *, *, #20837, .F. ) ;
#250828 = PLANE ( 'NONE',  #212549 ) ;
#250830 = DIRECTION ( 'NONE',  ( 0.000000000000000000, 0.000000000000000000, 1.000000000000000000 ) ) ;
#250831 = FACE_OUTER_BOUND ( 'NONE', #74242, .T. ) ;
#250832 = CYLINDRICAL_SURFACE ( 'NONE', #118394, 0.09999999999999939493 ) ;
#250833 = CARTESIAN_POINT ( 'NONE',  ( -16.87851181299898684, 22.97796121983802209, -230.9349578068793676 ) ) ;
#250834 = DIRECTION ( 'NONE',  ( 0.5932847527679310229, 0.8049926720990042694, 5.621233785078285907E-15 ) ) ;
#250835 = AXIS2_PLACEMENT_3D ( 'NONE', #102515, #3439, #79118 ) ;
#250836 = CARTESIAN_POINT ( 'NONE',  ( -16.91049119928364064, 9.950000000011138823, -79.61827960680922445 ) ) ;
#250837 = DIRECTION ( 'NONE',  ( -0.000000000000000000, -0.000000000000000000, -1.000000000000000000 ) ) ;
#250839 = ORIENTED_EDGE ( 'NONE', *, *, #67135, .T. ) ;
#250838 = CARTESIAN_POINT ( 'NONE',  ( -22.49510344025093644, 75.93287232181778279, -114.6730775896385524 ) ) ;
#250840 = CIRCLE ( 'NONE', #234087, 0.2000000000000100864 ) ;
#250841 = CIRCLE ( 'NONE', #121698, 0.09999999999999939493 ) ;
#250842 = CIRCLE ( 'NONE', #209154, 0.5000000000000004441 ) ;
#250843 = AXIS2_PLACEMENT_3D ( 'NONE', #130253, #12916, #94980 ) ;
#250844 = DIRECTION ( 'NONE',  ( 0.000000000000000000, 1.000000000000000000, 6.982962677686266711E-15 ) ) ;
#250845 = CARTESIAN_POINT ( 'NONE',  ( 21.14999999999999858, 76.00000000001186606, -90.87310748452429721 ) ) ;
#250846 = CARTESIAN_POINT ( 'NONE',  ( -18.59999999999999787, 70.47363787294415260, -228.3418745167492432 ) ) ;
#250847 = DIRECTION ( 'NONE',  ( -1.000000000000000000, -0.000000000000000000, 0.000000000000000000 ) ) ;
#250848 = ORIENTED_EDGE ( 'NONE', *, *, #29377, .F. ) ;
#250849 = EDGE_CURVE ( 'NONE', #136730, #193535, #109699, .T. ) ;
#250850 = VECTOR ( 'NONE', #58904, 1000.000000000000000 ) ;
#250851 = PLANE ( 'NONE',  #235643 ) ;
#250852 = EDGE_CURVE ( 'NONE', #115014, #151151, #63926, .T. ) ;
#250853 = FACE_OUTER_BOUND ( 'NONE', #211493, .T. ) ;
#250854 = VECTOR ( 'NONE', #120667, 1000.000000000000000 ) ;
#250855 = AXIS2_PLACEMENT_3D ( 'NONE', #131670, #33910, #174704 ) ;
#250856 = ORIENTED_EDGE ( 'NONE', *, *, #75245, .T. ) ;
#250857 = CIRCLE ( 'NONE', #63424, 0.09999999999999939493 ) ;
#250858 = CARTESIAN_POINT ( 'NONE',  ( 20.94999999999999929, 71.14953271029236248, -115.0573748935260028 ) ) ;
#250859 = AXIS2_PLACEMENT_3D ( 'NONE', #121666, #239026, #241590 ) ;
#250860 = CIRCLE ( 'NONE', #155054, 4.000000000000000000 ) ;
#250861 = DIRECTION ( 'NONE',  ( -0.000000000000000000, -0.000000000000000000, -1.000000000000000000 ) ) ;
#250862 = EDGE_CURVE ( 'NONE', #177752, #208786, #253385, .T. ) ;
#250863 = ORIENTED_EDGE ( 'NONE', *, *, #181382, .T. ) ;
#250864 = LINE ( 'NONE', #196050, #161034 ) ;
#250865 = ORIENTED_EDGE ( 'NONE', *, *, #164644, .F. ) ;
#250867 = VECTOR ( 'NONE', #176596, 1000.000000000000000 ) ;
#250866 = DIRECTION ( 'NONE',  ( 0.000000000000000000, -0.8660254037844247188, 0.5000000000000245359 ) ) ;
#250869 = VERTEX_POINT ( 'NONE', #186022 ) ;
#250868 = CARTESIAN_POINT ( 'NONE',  ( 18.59999999999999076, 69.55000000001261640, -193.5060803140843859 ) ) ;
#250870 = EDGE_CURVE ( 'NONE', #85926, #101417, #117858, .T. ) ;
#250871 = DIRECTION ( 'NONE',  ( 0.000000000000000000, 0.8814952561688407240, -0.4721928772777390093 ) ) ;
#250872 = VERTEX_POINT ( 'NONE', #6086 ) ;
#250873 = DIRECTION ( 'NONE',  ( 1.000000000000000000, 1.585864606265928695E-14, 4.552022003305584948E-15 ) ) ;
#250874 = EDGE_LOOP ( 'NONE', ( #164302, #60129, #71302, #120345 ) ) ;
#250876 = ORIENTED_EDGE ( 'NONE', *, *, #122668, .F. ) ;
#250875 = EDGE_LOOP ( 'NONE', ( #145796, #120087, #188059, #162745 ) ) ;
#250877 = CARTESIAN_POINT ( 'NONE',  ( 18.49713797159841633, 85.44648232759121242, -129.4516493629137983 ) ) ;
#250878 = EDGE_CURVE ( 'NONE', #33844, #181739, #53908, .T. ) ;
#250880 = ORIENTED_EDGE ( 'NONE', *, *, #145596, .F. ) ;
#250879 = CARTESIAN_POINT ( 'NONE',  ( -20.64999999999999858, 1.925233644870967487, -154.7697564668738721 ) ) ;
#250881 = DIRECTION ( 'NONE',  ( 0.000000000000000000, -0.9651348961777157509, 0.2617529984165031243 ) ) ;
#250883 = ORIENTED_EDGE ( 'NONE', *, *, #37189, .F. ) ;
#250882 = TOROIDAL_SURFACE ( 'NONE', #96740, 0.2000000000000000111, 0.1000000000000000056 ) ;
#250884 = AXIS2_PLACEMENT_3D ( 'NONE', #252729, #250185, #228055 ) ;
#250885 = CIRCLE ( 'NONE', #146828, 0.09999999999999530098 ) ;
#250886 = ORIENTED_EDGE ( 'NONE', *, *, #48648, .T. ) ;
#250887 = CARTESIAN_POINT ( 'NONE',  ( -23.25000000000000355, 13.44928205424795564, -207.5377222505711075 ) ) ;
#250888 = EDGE_CURVE ( 'NONE', #199698, #76744, #46493, .T. ) ;
#250889 = DIRECTION ( 'NONE',  ( 0.000000000000000000, 1.000000000000000000, 0.000000000000000000 ) ) ;
#250890 = ORIENTED_EDGE ( 'NONE', *, *, #167520, .F. ) ;
#250891 = CARTESIAN_POINT ( 'NONE',  ( -21.05000000000000071, 87.65000000001144542, -39.12310748452424747 ) ) ;
#250892 = DIRECTION ( 'NONE',  ( 0.000000000000000000, 0.2605042016806672911, -0.9654727137038716656 ) ) ;
#250893 = FACE_OUTER_BOUND ( 'NONE', #104775, .T. ) ;
#250894 = VERTEX_POINT ( 'NONE', #145597 ) ;
#250895 = DIRECTION ( 'NONE',  ( -1.000000000000000000, -0.000000000000000000, -0.000000000000000000 ) ) ;
#250896 = LINE ( 'NONE', #167548, #215252 ) ;
#250897 = DIRECTION ( 'NONE',  ( 0.000000000000000000, 6.982962677686266711E-15, -1.000000000000000000 ) ) ;
#250898 = DIRECTION ( 'NONE',  ( -1.000000000000000000, 0.000000000000000000, 0.000000000000000000 ) ) ;
#250899 = EDGE_LOOP ( 'NONE', ( #144285, #10442, #228583 ) ) ;
#250901 = CARTESIAN_POINT ( 'NONE',  ( 22.40000000000020819, -0.1008583690885111045, -55.25043287651034518 ) ) ;
#250900 = CIRCLE ( 'NONE', #201034, 0.3999999999999975797 ) ;
#250902 = ORIENTED_EDGE ( 'NONE', *, *, #164398, .F. ) ;
#250903 = CARTESIAN_POINT ( 'NONE',  ( 20.94999999999999574, 77.16270174994990327, -95.02310748452430289 ) ) ;
#250904 = ORIENTED_EDGE ( 'NONE', *, *, #68852, .T. ) ;
#250905 = DIRECTION ( 'NONE',  ( 2.659396599871503635E-15, 0.6132151058540549204, -0.7899159663865520375 ) ) ;
#250906 = ORIENTED_EDGE ( 'NONE', *, *, #195657, .T. ) ;
#250907 = VECTOR ( 'NONE', #154285, 1000.000000000000114 ) ;
#250908 = ORIENTED_EDGE ( 'NONE', *, *, #67061, .T. ) ;
#250909 = DIRECTION ( 'NONE',  ( -1.000000000000000000, -0.000000000000000000, -0.000000000000000000 ) ) ;
#250910 = DIRECTION ( 'NONE',  ( 0.000000000000000000, 0.000000000000000000, -1.000000000000000000 ) ) ;
#250911 = ORIENTED_EDGE ( 'NONE', *, *, #221043, .F. ) ;
#250912 = ORIENTED_EDGE ( 'NONE', *, *, #26293, .T. ) ;
#250913 = LINE ( 'NONE', #190984, #214464 ) ;
#250914 = CARTESIAN_POINT ( 'NONE',  ( 18.59999999999999076, 34.58225676390223668, -235.1091250528070589 ) ) ;
#250915 = ORIENTED_EDGE ( 'NONE', *, *, #134740, .F. ) ;
#250916 = ORIENTED_EDGE ( 'NONE', *, *, #121800, .T. ) ;
#250917 = EDGE_CURVE ( 'NONE', #117101, #158841, #234607, .T. ) ;
#250918 = AXIS2_PLACEMENT_3D ( 'NONE', #60569, #17589, #214512 ) ;
#250919 = CARTESIAN_POINT ( 'NONE',  ( -18.40000000000000213, 11.75000000001113953, -121.3500000000000369 ) ) ;
#250920 = DIRECTION ( 'NONE',  ( 0.000000000000000000, 6.982962677686266711E-15, -1.000000000000000000 ) ) ;
#250921 = EDGE_CURVE ( 'NONE', #21519, #13670, #215735, .T. ) ;
#250922 = DIRECTION ( 'NONE',  ( -0.000000000000000000, 1.000000000000000000, 0.000000000000000000 ) ) ;
#250924 = EDGE_LOOP ( 'NONE', ( #170525, #204688, #106620, #208460 ) ) ;
#250923 = DIRECTION ( 'NONE',  ( 0.000000000000000000, 0.000000000000000000, -1.000000000000000000 ) ) ;
#250925 = CYLINDRICAL_SURFACE ( 'NONE', #16139, 0.9000000000000014655 ) ;
#250926 = DIRECTION ( 'NONE',  ( 0.000000000000000000, -0.1568667991644863147, -0.9876197685951252359 ) ) ;
#250927 = DIRECTION ( 'NONE',  ( 0.000000000000000000, 0.7071067811865472397, -0.7071067811865479058 ) ) ;
#250928 = EDGE_CURVE ( 'NONE', #119060, #23607, #163882, .T. ) ;
#250930 = CARTESIAN_POINT ( 'NONE',  ( -23.15000000000000213, 80.83132476063495631, -119.5534105423255227 ) ) ;
#250929 = CARTESIAN_POINT ( 'NONE',  ( -18.59999999999999787, 68.92903212821255465, -32.27654326265606954 ) ) ;
#250932 = EDGE_CURVE ( 'NONE', #34405, #88666, #68200, .T. ) ;
#250931 = LINE ( 'NONE', #211837, #90692 ) ;
#250933 = CARTESIAN_POINT ( 'NONE',  ( 18.47654891039378100, -9.465274948371153130, -107.6259759051946787 ) ) ;
#250934 = CIRCLE ( 'NONE', #67610, 0.09999999999998898659 ) ;
#250935 = LINE ( 'NONE', #228835, #51658 ) ;
#250936 = CARTESIAN_POINT ( 'NONE',  ( -21.04999999999895977, 75.94867256767074082, -176.3232908207953074 ) ) ;
#250937 = TOROIDAL_SURFACE ( 'NONE', #130148, 12.97499999999999787, 0.1000000000000000056 ) ;
#250938 = ORIENTED_EDGE ( 'NONE', *, *, #111242, .F. ) ;
#250939 = CIRCLE ( 'NONE', #55119, 4.049999999999997158 ) ;
#250940 = ORIENTED_EDGE ( 'NONE', *, *, #75642, .F. ) ;
#250941 = EDGE_CURVE ( 'NONE', #36614, #55132, #84727, .T. ) ;
#250942 = FACE_OUTER_BOUND ( 'NONE', #58727, .T. ) ;
#250943 = EDGE_CURVE ( 'NONE', #61045, #6106, #213951, .T. ) ;
#250944 = EDGE_LOOP ( 'NONE', ( #186214, #227414, #8523, #134374 ) ) ;
#250945 = AXIS2_PLACEMENT_3D ( 'NONE', #52113, #181697, #149973 ) ;
#250947 = VECTOR ( 'NONE', #239676, 1000.000000000000000 ) ;
#250946 = FILL_AREA_STYLE ('',( #91886 ) ) ;
#250948 = DIRECTION ( 'NONE',  ( -0.000000000000000000, 0.000000000000000000, 1.000000000000000000 ) ) ;
#250949 = CARTESIAN_POINT ( 'NONE',  ( -16.89208623190940628, 63.08558943445424916, -213.1221201667474361 ) ) ;
#250950 = ORIENTED_EDGE ( 'NONE', *, *, #135693, .F. ) ;
#250951 = ORIENTED_EDGE ( 'NONE', *, *, #170709, .T. ) ;
#250952 = CARTESIAN_POINT ( 'NONE',  ( 21.08750232978087524, 60.08127493647409523, -221.2453635944128791 ) ) ;
#250953 = CARTESIAN_POINT ( 'NONE',  ( 23.40000000000005187, 77.85126707825561709, -47.62635315998165453 ) ) ;
#250954 = EDGE_LOOP ( 'NONE', ( #182675, #88175, #3972, #74041 ) ) ;
#250955 = EDGE_CURVE ( 'NONE', #194536, #3363, #106451, .T. ) ;
#250956 = VECTOR ( 'NONE', #12912, 1000.000000000000000 ) ;
#250957 = ADVANCED_FACE ( 'NONE', ( #154339 ), #22249, .F. ) ;
#250958 = CARTESIAN_POINT ( 'NONE',  ( 22.01447462590973458, 0.09903700007069084210, -93.23619979877013009 ) ) ;
#250960 = ORIENTED_EDGE ( 'NONE', *, *, #42046, .T. ) ;
#250959 = DIRECTION ( 'NONE',  ( -1.000000000000000000, -0.000000000000000000, -0.000000000000000000 ) ) ;
#250961 = LINE ( 'NONE', #35808, #49627 ) ;
#250962 = EDGE_CURVE ( 'NONE', #162338, #58778, #168023, .T. ) ;
#250964 = ORIENTED_EDGE ( 'NONE', *, *, #212170, .T. ) ;
#250963 = CARTESIAN_POINT ( 'NONE',  ( 23.25000000000000000, -8.777002227904191045, -238.5420042644097975 ) ) ;
#250965 = AXIS2_PLACEMENT_3D ( 'NONE', #135137, #98551, #178162 ) ;
#250966 = CARTESIAN_POINT ( 'NONE',  ( -22.39999999999999858, 11.75000000001115552, -100.5000000000000284 ) ) ;
#250968 = CARTESIAN_POINT ( 'NONE',  ( 20.94560253601876809, 64.25000000001219291, -143.5130239720093641 ) ) ;
#250967 = AXIS2_PLACEMENT_3D ( 'NONE', #231631, #188633, #51663 ) ;
#250969 = CIRCLE ( 'NONE', #213377, 0.09999999999999609201 ) ;
#250970 = DIRECTION ( 'NONE',  ( 2.952720810173289112E-16, -1.000000000000000000, -0.000000000000000000 ) ) ;
#250971 = CARTESIAN_POINT ( 'NONE',  ( -23.30000000000000426, -11.79999999999999893, -347.0000000000001137 ) ) ;
#250972 = CIRCLE ( 'NONE', #46969, 3.999999999999999112 ) ;
#250974 = CARTESIAN_POINT ( 'NONE',  ( 20.22516295850462598, 9.899364295460458152, -108.4100657120914235 ) ) ;
#250973 = DIRECTION ( 'NONE',  ( 0.000000000000000000, 0.000000000000000000, -1.000000000000000000 ) ) ;
#250975 = DIRECTION ( 'NONE',  ( -0.000000000000000000, -1.000000000000000000, -0.000000000000000000 ) ) ;
#250976 = DIRECTION ( 'NONE',  ( -0.000000000000000000, -0.8490545835447252943, -0.5283051335749947564 ) ) ;
#250977 = DIRECTION ( 'NONE',  ( 1.000000000000000000, 0.000000000000000000, 0.000000000000000000 ) ) ;
#250978 = CARTESIAN_POINT ( 'NONE',  ( -23.25000000000000355, 20.94763808724815846, -234.7254930126486556 ) ) ;
#250979 = EDGE_LOOP ( 'NONE', ( #96360, #30033, #97370 ) ) ;
#250980 = DIRECTION ( 'NONE',  ( 0.000000000000000000, -0.9126074666063545004, -0.4088369013363783999 ) ) ;
#250981 = ORIENTED_EDGE ( 'NONE', *, *, #6082, .T. ) ;
#250982 = PLANE ( 'NONE',  #180854 ) ;
#250983 = ORIENTED_EDGE ( 'NONE', *, *, #149765, .T. ) ;
#250984 = DIRECTION ( 'NONE',  ( 0.000000000000000000, 0.000000000000000000, -1.000000000000000000 ) ) ;
#250985 = DIRECTION ( 'NONE',  ( 0.000000000000000000, -0.9126074666063660468, -0.4088369013363524762 ) ) ;
#250987 = EDGE_CURVE ( 'NONE', #147215, #135942, #55497, .T. ) ;
#250986 = ORIENTED_EDGE ( 'NONE', *, *, #18076, .T. ) ;
#250988 = CARTESIAN_POINT ( 'NONE',  ( -21.05000000000000071, 30.90801580390628089, -252.0203440857197279 ) ) ;
#250989 = SHAPE_REPRESENTATION_RELATIONSHIP ( 'NONE' , 'NONE' ,  #170171, #237827 ) ;
#250990 = CIRCLE ( 'NONE', #9401, 0.09999999999999939493 ) ;
#250991 = ORIENTED_EDGE ( 'NONE', *, *, #187524, .T. ) ;
#250992 = VERTEX_POINT ( 'NONE', #8670 ) ;
#250993 = DIRECTION ( 'NONE',  ( 1.000000000000000000, 0.000000000000000000, 0.000000000000000000 ) ) ;
#250994 = DIRECTION ( 'NONE',  ( 0.000000000000000000, 1.000000000000000000, 0.000000000000000000 ) ) ;
#250995 = DIRECTION ( 'NONE',  ( 0.000000000000000000, 1.000000000000000000, -0.000000000000000000 ) ) ;
#250996 = CARTESIAN_POINT ( 'NONE',  ( 21.05000000000000071, 5.000000000011153745, -121.5947339810869465 ) ) ;
#250997 = EDGE_CURVE ( 'NONE', #236196, #69522, #184722, .T. ) ;
#250998 = CIRCLE ( 'NONE', #196852, 12.97499999999998721 ) ;
#251000 = FACE_OUTER_BOUND ( 'NONE', #55945, .T. ) ;
#250999 = CARTESIAN_POINT ( 'NONE',  ( -20.64999999999999858, 7.150000000000000355, -21.15000000000000213 ) ) ;
#251001 = CARTESIAN_POINT ( 'NONE',  ( -13.12432614554022869, 9.430764995433477793, -82.23053739475051316 ) ) ;
#251003 = ORIENTED_EDGE ( 'NONE', *, *, #175125, .T. ) ;
#251002 = CARTESIAN_POINT ( 'NONE',  ( 23.25000000000000000, -8.596261682231833845, -76.45012751715033517 ) ) ;
#251005 = CARTESIAN_POINT ( 'NONE',  ( 20.85000000000000142, 11.75000000001115907, -127.2161343370219413 ) ) ;
#251004 = DIRECTION ( 'NONE',  ( 1.000000000000000000, 3.265361837132813093E-16, -0.000000000000000000 ) ) ;
#251006 = CARTESIAN_POINT ( 'NONE',  ( 23.24999999999999289, 11.65000000001116298, -179.6499999999999773 ) ) ;
#251007 = ORIENTED_EDGE ( 'NONE', *, *, #160343, .T. ) ;
#251008 = LINE ( 'NONE', #151960, #38052 ) ;
#251009 = TOROIDAL_SURFACE ( 'NONE', #217869, 1.900000000000002576, 0.1000000000000000056 ) ;
#251010 = CARTESIAN_POINT ( 'NONE',  ( -20.64999999999999858, -9.000000000000001776, -24.00603087734755903 ) ) ;
#251012 = EDGE_CURVE ( 'NONE', #139104, #225893, #105581, .T. ) ;
#251011 = SPHERICAL_SURFACE ( 'NONE', #62908, 0.1000000000000000056 ) ;
#251013 = VERTEX_POINT ( 'NONE', #187324 ) ;
#251014 = TOROIDAL_SURFACE ( 'NONE', #30291, 0.2000000000000000111, 0.1000000000000000056 ) ;
#251016 = DIRECTION ( 'NONE',  ( 0.000000000000000000, -0.9654727137038715545, 0.2605042016806676242 ) ) ;
#251015 = AXIS2_PLACEMENT_3D ( 'NONE', #182320, #12357, #107566 ) ;
#251017 = ADVANCED_FACE ( 'NONE', ( #117728 ), #83288, .F. ) ;
#251018 = AXIS2_PLACEMENT_3D ( 'NONE', #191660, #156382, #215035 ) ;
#251019 = DIRECTION ( 'NONE',  ( -3.265361837132813093E-16, -1.000000000000000000, -7.026728003956683390E-15 ) ) ;
#251020 = FACE_OUTER_BOUND ( 'NONE', #52171, .T. ) ;
#251021 = ORIENTED_EDGE ( 'NONE', *, *, #96735, .T. ) ;
#251022 = ORIENTED_EDGE ( 'NONE', *, *, #215972, .F. ) ;
#251023 = CIRCLE ( 'NONE', #55369, 0.1000000000000028644 ) ;
#251024 = EDGE_CURVE ( 'NONE', #69452, #251152, #179027, .T. ) ;
#251026 = ADVANCED_FACE ( 'NONE', ( #199856 ), #175186, .T. ) ;
#251025 = DIRECTION ( 'NONE',  ( 0.5932847527679299127, 0.8049926720990051576, 4.984624513800587583E-15 ) ) ;
#251027 = CARTESIAN_POINT ( 'NONE',  ( -17.27223548802716735, 65.65460260865560826, -158.6567136637387705 ) ) ;
#251028 = DIRECTION ( 'NONE',  ( 0.000000000000000000, -1.000000000000000000, 0.000000000000000000 ) ) ;
#251029 = CARTESIAN_POINT ( 'NONE',  ( -20.64999999999999858, 85.00000000001179501, -78.91707660717668205 ) ) ;
#251030 = ORIENTED_EDGE ( 'NONE', *, *, #88743, .T. ) ;
#251031 = AXIS2_PLACEMENT_3D ( 'NONE', #252285, #73697, #47662 ) ;
#251033 = AXIS2_PLACEMENT_3D ( 'NONE', #225393, #143302, #222831 ) ;
#251032 = CARTESIAN_POINT ( 'NONE',  ( 15.39793903038207645, 47.12322829752086761, -234.5744283691288388 ) ) ;
#251034 = FACE_OUTER_BOUND ( 'NONE', #226240, .T. ) ;
#251035 = DIRECTION ( 'NONE',  ( -3.265361837132813093E-16, -1.000000000000000000, 7.445645354460596589E-46 ) ) ;
#251036 = AXIS2_PLACEMENT_3D ( 'NONE', #205345, #67137, #8458 ) ;
#251037 = FACE_OUTER_BOUND ( 'NONE', #243638, .T. ) ;
#251038 = EDGE_CURVE ( 'NONE', #100336, #17038, #254641, .T. ) ;
#251039 = ORIENTED_EDGE ( 'NONE', *, *, #164192, .F. ) ;
#251041 = EDGE_CURVE ( 'NONE', #225791, #56249, #95594, .T. ) ;
#251040 = CARTESIAN_POINT ( 'NONE',  ( 21.05000000000000071, -6.688413578037176066, -212.5825622730469036 ) ) ;
#251042 = AXIS2_PLACEMENT_3D ( 'NONE', #181337, #5212, #99183 ) ;
#251043 = AXIS2_PLACEMENT_3D ( 'NONE', #150407, #149122, #130820 ) ;
#251044 = AXIS2_PLACEMENT_3D ( 'NONE', #116194, #211423, #155335 ) ;
#251046 = ORIENTED_EDGE ( 'NONE', *, *, #9693, .T. ) ;
#251045 = CARTESIAN_POINT ( 'NONE',  ( -16.93826681692523550, 65.98857127972409842, -82.07764901716494421 ) ) ;
#251047 = CIRCLE ( 'NONE', #117969, 0.5000000000000004441 ) ;
#251048 = CARTESIAN_POINT ( 'NONE',  ( 20.94999999999999929, 82.57900542960499024, -215.5587758314583766 ) ) ;
#251049 = CARTESIAN_POINT ( 'NONE',  ( -13.40000000000000036, -12.25000000000000178, 15.00000000000000355 ) ) ;
#251050 = DIRECTION ( 'NONE',  ( 1.000000000000000000, 0.000000000000000000, 0.000000000000000000 ) ) ;
#251051 = CARTESIAN_POINT ( 'NONE',  ( -21.65000000000000213, 7.250000000011139534, -79.65000000000004832 ) ) ;
#251052 = EDGE_CURVE ( 'NONE', #237092, #198825, #18130, .T. ) ;
#251053 = DIRECTION ( 'NONE',  ( -0.000000000000000000, 0.1298341882519668811, 0.9915357197604899309 ) ) ;
#251054 = ORIENTED_EDGE ( 'NONE', *, *, #20308, .T. ) ;
#251055 = CARTESIAN_POINT ( 'NONE',  ( 20.97462148592286013, 8.874737576450577592, -12.25464433173102563 ) ) ;
#251056 = DIRECTION ( 'NONE',  ( 0.000000000000000000, 0.000000000000000000, -1.000000000000000000 ) ) ;
#251057 = CYLINDRICAL_SURFACE ( 'NONE', #90606, 0.09999999999999939493 ) ;
#251058 = ORIENTED_EDGE ( 'NONE', *, *, #256472, .T. ) ;
#251059 = CARTESIAN_POINT ( 'NONE',  ( 23.14999999999998437, 76.00000000001168132, -73.57310748452432847 ) ) ;
#251060 = SPHERICAL_SURFACE ( 'NONE', #94179, 0.1000000000000000056 ) ;
#251061 = DIRECTION ( 'NONE',  ( 1.000000000000000000, -0.000000000000000000, -0.000000000000000000 ) ) ;
#251062 = EDGE_CURVE ( 'NONE', #94361, #40333, #26517, .T. ) ;
#251064 = EDGE_CURVE ( 'NONE', #254860, #150422, #91533, .T. ) ;
#251063 = B_SPLINE_CURVE_WITH_KNOTS ( 'NONE', 3,
 ( #98917, #102771, #182353, #242305, #2395, #217589, #140636, #256690, #178518, #21998 ),
 .UNSPECIFIED., .F., .F.,
 ( 4, 3, 3, 4 ),
 ( 7.632826238681267430E-06, 4.756916949875584252E-05, 9.484459048148792613E-05, 0.0001435500935099677739 ),
 .UNSPECIFIED. ) ;
#251065 = FACE_OUTER_BOUND ( 'NONE', #180093, .T. ) ;
#251066 = AXIS2_PLACEMENT_3D ( 'NONE', #179643, #214899, #16717 ) ;
#251067 = CARTESIAN_POINT ( 'NONE',  ( 13.54577453029516043, 9.450602096099679272, -185.9438959630965655 ) ) ;
#251068 = VECTOR ( 'NONE', #217029, 1000.000000000000000 ) ;
#251069 = ORIENTED_EDGE ( 'NONE', *, *, #99719, .F. ) ;
#251070 = ORIENTED_EDGE ( 'NONE', *, *, #25711, .F. ) ;
#251071 = EDGE_CURVE ( 'NONE', #24291, #90989, #147490, .T. ) ;
#251072 = CARTESIAN_POINT ( 'NONE',  ( -18.59999999999999787, 11.65000000001115232, -174.5148057706539930 ) ) ;
#251073 = DIRECTION ( 'NONE',  ( -0.000000000000000000, -1.000000000000000000, 6.308085367188393199E-16 ) ) ;
#251074 = CARTESIAN_POINT ( 'NONE',  ( -21.12844524849339223, 38.15611011707152755, -236.0052459596564063 ) ) ;
#251075 = CARTESIAN_POINT ( 'NONE',  ( -18.50000000000000000, 7.021664781911246322, -137.6335654018973287 ) ) ;
#251076 = ADVANCED_FACE ( 'NONE', ( #219380 ), #160741, .T. ) ;
#251077 = DIRECTION ( 'NONE',  ( -1.000000000000000000, 0.000000000000000000, 0.000000000000000000 ) ) ;
#251078 = DIRECTION ( 'NONE',  ( 0.000000000000000000, 0.000000000000000000, -1.000000000000000000 ) ) ;
#251079 = CARTESIAN_POINT ( 'NONE',  ( -18.39999999999999858, 11.47316190337362762, -109.8259460668080152 ) ) ;
#251080 = VECTOR ( 'NONE', #133011, 1000.000000000000000 ) ;
#251081 = CARTESIAN_POINT ( 'NONE',  ( -2.995603634470891112E-16, -11.74999999998884448, -192.2499999999999716 ) ) ;
#251082 = ORIENTED_EDGE ( 'NONE', *, *, #75459, .F. ) ;
#251083 = DIRECTION ( 'NONE',  ( 0.000000000000000000, 0.000000000000000000, 1.000000000000000000 ) ) ;
#251084 = ORIENTED_EDGE ( 'NONE', *, *, #6035, .T. ) ;
#251085 = DIRECTION ( 'NONE',  ( 0.000000000000000000, 0.8814952561688444987, -0.4721928772777320149 ) ) ;
#251086 = CARTESIAN_POINT ( 'NONE',  ( 20.95595012432476167, 10.60417921307614542, -7.595769330218145932 ) ) ;
#251087 = CARTESIAN_POINT ( 'NONE',  ( 21.05000000000000071, 43.39590751456783835, -245.0548026989423818 ) ) ;
#251088 = CARTESIAN_POINT ( 'NONE',  ( -21.05000000000000071, 64.37928932189399234, -196.6546908321834053 ) ) ;
#251089 = CARTESIAN_POINT ( 'NONE',  ( 21.13920837816993270, 22.07453692459872130, -231.7746734506518749 ) ) ;
#251090 = CARTESIAN_POINT ( 'NONE',  ( -23.15000000000000213, 2.600000000011156054, -21.75000000000000355 ) ) ;
#251091 = FACE_OUTER_BOUND ( 'NONE', #69474, .T. ) ;
#251092 = EDGE_LOOP ( 'NONE', ( #209067, #85016, #4259, #233589, #88319 ) ) ;
#251093 = DIRECTION ( 'NONE',  ( 1.000000000000000000, 7.304098846218135653E-16, 5.311601492717085047E-30 ) ) ;
#251094 = FACE_OUTER_BOUND ( 'NONE', #190610, .T. ) ;
#251095 = CARTESIAN_POINT ( 'NONE',  ( -18.59999999999999787, 77.86671491006991630, -191.7704322382423356 ) ) ;
#251096 = CARTESIAN_POINT ( 'NONE',  ( 20.94999999999999929, 0.000000000000000000, -30.59999999999999432 ) ) ;
#251097 = DIRECTION ( 'NONE',  ( 1.000000000000000000, 0.000000000000000000, 0.000000000000000000 ) ) ;
#251098 = VECTOR ( 'NONE', #84940, 1000.000000000000000 ) ;
#251099 = VERTEX_POINT ( 'NONE', #47151 ) ;
#251100 = DIRECTION ( 'NONE',  ( -0.000000000000000000, -6.982962677686266711E-15, 1.000000000000000000 ) ) ;
#251101 = DIRECTION ( 'NONE',  ( 0.000000000000000000, 0.8700118002898356018, -0.4930308989875170078 ) ) ;
#251102 = EDGE_CURVE ( 'NONE', #31867, #122206, #126713, .T. ) ;
#251103 = EDGE_LOOP ( 'NONE', ( #67053, #241665, #14046, #45396 ) ) ;
#251104 = ORIENTED_EDGE ( 'NONE', *, *, #43085, .F. ) ;
#251105 = CARTESIAN_POINT ( 'NONE',  ( -20.85000000000000142, 7.128833340094563376, -233.7327013124401276 ) ) ;
#251106 = CARTESIAN_POINT ( 'NONE',  ( 18.45139536634706801, -9.486081720270043149, -174.1405116178106596 ) ) ;
#251107 = EDGE_LOOP ( 'NONE', ( #212157, #176083, #247999, #179792, #44204, #32662, #2880, #134797 ) ) ;
#251108 = CARTESIAN_POINT ( 'NONE',  ( 20.85000000000000142, 1.115600667400684642E-11, -167.5000000000000284 ) ) ;
#251109 = CARTESIAN_POINT ( 'NONE',  ( -16.97683809663752186, 9.950000000011137047, -147.4023640181965220 ) ) ;
#251110 = CIRCLE ( 'NONE', #13631, 7.800000000000001599 ) ;
#251111 = EDGE_CURVE ( 'NONE', #13199, #224018, #184902, .T. ) ;
#251112 = ORIENTED_EDGE ( 'NONE', *, *, #189487, .T. ) ;
#251113 = AXIS2_PLACEMENT_3D ( 'NONE', #252741, #75436, #197906 ) ;
#251114 = PLANE ( 'NONE',  #97915 ) ;
#251115 = VECTOR ( 'NONE', #166389, 1000.000000000000227 ) ;
#251116 =( BOUNDED_CURVE ( )  B_SPLINE_CURVE ( 3, ( #117021, #115738, #79156, #173198 ),
 .UNSPECIFIED., .F., .F. ) 
 B_SPLINE_CURVE_WITH_KNOTS ( ( 4, 4 ),
 ( 0.000000000000000000, 1.570796326794884346 ),
 .UNSPECIFIED. ) 
 CURVE ( )  GEOMETRIC_REPRESENTATION_ITEM ( )  RATIONAL_B_SPLINE_CURVE ( ( 1.000000000000000000, 0.8047378541243679351, 0.8047378541243679351, 1.000000000000000000 ) ) 
 REPRESENTATION_ITEM ( '' )  );
#251117 = ORIENTED_EDGE ( 'NONE', *, *, #73456, .T. ) ;
#251118 = FACE_OUTER_BOUND ( 'NONE', #134543, .T. ) ;
#251120 = ORIENTED_EDGE ( 'NONE', *, *, #13334, .F. ) ;
#251119 = DIRECTION ( 'NONE',  ( 0.000000000000000000, 0.2128009952263603677, -0.9770955615653313941 ) ) ;
#251121 = LINE ( 'NONE', #236700, #57308 ) ;
#251123 = DIRECTION ( 'NONE',  ( 0.000000000000000000, 0.000000000000000000, -1.000000000000000000 ) ) ;
#251122 = UNCERTAINTY_MEASURE_WITH_UNIT (LENGTH_MEASURE( 1.000000000000000082E-05 ), #169260, 'distance_accuracy_value', 'NONE');
#251124 = CARTESIAN_POINT ( 'NONE',  ( -20.94999675878240808, 65.70692517833255408, -131.0644653378304270 ) ) ;
#251125 = CYLINDRICAL_SURFACE ( 'NONE', #97591, 0.5000000000000008882 ) ;
#251126 = CARTESIAN_POINT ( 'NONE',  ( 21.14999999999999858, 64.35000000001186038, -90.87310748452438247 ) ) ;
#251127 = AXIS2_PLACEMENT_3D ( 'NONE', #78098, #175958, #57241 ) ;
#251128 = DIRECTION ( 'NONE',  ( 0.000000000000000000, -0.4088369013363783999, 0.9126074666063545004 ) ) ;
#251130 = CARTESIAN_POINT ( 'NONE',  ( 22.39999999999999858, 75.90000000001170122, -77.31388708289770761 ) ) ;
#251129 = AXIS2_PLACEMENT_3D ( 'NONE', #144087, #180676, #64563 ) ;
#251132 = ORIENTED_EDGE ( 'NONE', *, *, #41407, .F. ) ;
#251131 = CARTESIAN_POINT ( 'NONE',  ( 20.94999999999999929, 76.00000000001170974, -69.52310748452431710 ) ) ;
#251133 = ORIENTED_EDGE ( 'NONE', *, *, #37365, .T. ) ;
#251135 = CARTESIAN_POINT ( 'NONE',  ( -12.25000000000000355, 9.350000000011135626, -83.86574316727397616 ) ) ;
#251134 = CARTESIAN_POINT ( 'NONE',  ( 18.49999999999999289, 10.25000000001115552, -54.85000000000000142 ) ) ;
#251137 = ORIENTED_EDGE ( 'NONE', *, *, #120153, .T. ) ;
#251136 = CARTESIAN_POINT ( 'NONE',  ( -18.59999999999999787, 67.23127455305835554, -235.8551265064784559 ) ) ;
#251138 = ORIENTED_EDGE ( 'NONE', *, *, #38623, .F. ) ;
#251139 = CARTESIAN_POINT ( 'NONE',  ( -16.81744102076748959, 66.05000000001255955, -182.6731074845244223 ) ) ;
#251140 = LINE ( 'NONE', #51646, #226153 ) ;
#251141 = B_SPLINE_CURVE_WITH_KNOTS ( 'NONE', 3,
 ( #72519, #137288, #152061, #188587, #171640, #227710, #230281, #209435 ),
 .UNSPECIFIED., .F., .F.,
 ( 4, 2, 2, 4 ),
 ( 0.000000000000000000, 0.0002181133598168667081, 0.0003271700397253312059, 0.0004362267196337957036 ),
 .UNSPECIFIED. ) ;
#251142 = CARTESIAN_POINT ( 'NONE',  ( -18.50000000000000355, 77.26327546522965406, -162.1212428177779543 ) ) ;
#251143 = CIRCLE ( 'NONE', #255202, 0.1000000000000002554 ) ;
#251144 = CARTESIAN_POINT ( 'NONE',  ( -21.04999999999994387, 65.87745128126655914, -37.09527722473000466 ) ) ;
#251145 = FACE_OUTER_BOUND ( 'NONE', #246429, .T. ) ;
#251146 = TOROIDAL_SURFACE ( 'NONE', #38798, 0.2000000000000000111, 0.1000000000000000056 ) ;
#251147 = AXIS2_PLACEMENT_3D ( 'NONE', #168501, #247979, #218448 ) ;
#251149 = ADVANCED_FACE ( 'NONE', ( #82418 ), #241526, .T. ) ;
#251148 = VECTOR ( 'NONE', #195655, 1000.000000000000000 ) ;
#251151 = CIRCLE ( 'NONE', #188825, 2.099999999999995204 ) ;
#251150 = DIRECTION ( 'NONE',  ( 0.000000000000000000, -6.982962677686266711E-15, 1.000000000000000000 ) ) ;
#251152 = VERTEX_POINT ( 'NONE', #203687 ) ;
#251153 = EDGE_LOOP ( 'NONE', ( #22328, #77696, #110756, #96342 ) ) ;
#251154 = CARTESIAN_POINT ( 'NONE',  ( 21.04999999999999716, 30.78822319289724163, -252.2004468398836536 ) ) ;
#251155 = EDGE_CURVE ( 'NONE', #82161, #85086, #247439, .T. ) ;
#251156 = EDGE_LOOP ( 'NONE', ( #256927, #103115, #199676, #159128 ) ) ;
#251157 = LINE ( 'NONE', #89522, #221742 ) ;
#251158 = EDGE_LOOP ( 'NONE', ( #41647, #34227, #68134, #62119, #34822, #170642, #181415, #143942, #15446, #228030, #139826, #40906, #666, #254921 ) ) ;
#251159 = CARTESIAN_POINT ( 'NONE',  ( 21.13736287352038445, 9.830747757323642588, -208.3258004385557172 ) ) ;
#251160 = LINE ( 'NONE', #132526, #180313 ) ;
#251161 = EDGE_CURVE ( 'NONE', #25144, #226867, #26710, .T. ) ;
#251162 = CARTESIAN_POINT ( 'NONE',  ( -15.69373346032659455, 66.64320997496614041, -119.3182809759104970 ) ) ;
#251163 = ORIENTED_EDGE ( 'NONE', *, *, #208918, .T. ) ;
#251164 = DIRECTION ( 'NONE',  ( 0.000000000000000000, 0.000000000000000000, -1.000000000000000000 ) ) ;
#251165 = ORIENTED_EDGE ( 'NONE', *, *, #116347, .T. ) ;
#251166 = ADVANCED_FACE ( 'NONE', ( #202401 ), #164068, .F. ) ;
#251167 = DIRECTION ( 'NONE',  ( -1.000000000000000000, 0.000000000000000000, 0.000000000000000000 ) ) ;
#251168 = CYLINDRICAL_SURFACE ( 'NONE', #171617, 0.09999999999999854838 ) ;
#251169 = AXIS2_PLACEMENT_3D ( 'NONE', #117692, #76005, #201081 ) ;
#251170 = ORIENTED_EDGE ( 'NONE', *, *, #153983, .F. ) ;
#251171 = CIRCLE ( 'NONE', #59626, 0.1000000000000028644 ) ;
#251172 = DIRECTION ( 'NONE',  ( 0.000000000000000000, -1.000000000000000000, -6.982962677686266711E-15 ) ) ;
#251173 = ADVANCED_FACE ( 'NONE', ( #146264 ), #18314, .F. ) ;
#251174 = ORIENTED_EDGE ( 'NONE', *, *, #94110, .F. ) ;
#251177 = EDGE_LOOP ( 'NONE', ( #59061, #66221, #55561, #170757 ) ) ;
#251176 = DIRECTION ( 'NONE',  ( 0.000000000000000000, -0.8660254037844411501, -0.4999999999999956146 ) ) ;
#251175 = DIRECTION ( 'NONE',  ( 1.000000000000000000, 2.885090398161910739E-16, 6.283419270304611573E-17 ) ) ;
#251178 = DIRECTION ( 'NONE',  ( -0.7071067811865388020, 0.7071067811865561215, 0.000000000000000000 ) ) ;
#251179 = ORIENTED_EDGE ( 'NONE', *, *, #91808, .F. ) ;
#251180 = VERTEX_POINT ( 'NONE', #84984 ) ;
#251181 = AXIS2_PLACEMENT_3D ( 'NONE', #230073, #233924, #51401 ) ;
#251182 = VECTOR ( 'NONE', #120455, 1000.000000000000000 ) ;
#251183 = CARTESIAN_POINT ( 'NONE',  ( 18.39999999999999503, 67.17743825834557470, -112.2731074845243597 ) ) ;
#251184 = ORIENTED_EDGE ( 'NONE', *, *, #179433, .T. ) ;
#251185 = DIRECTION ( 'NONE',  ( 1.000000000000000000, 0.000000000000000000, 0.000000000000000000 ) ) ;
#251186 = EDGE_CURVE ( 'NONE', #172803, #109697, #59989, .T. ) ;
#251187 = DIRECTION ( 'NONE',  ( -0.000000000000000000, -0.000000000000000000, -1.000000000000000000 ) ) ;
#251188 =( BOUNDED_CURVE ( )  B_SPLINE_CURVE ( 3, ( #94053, #32851, #189320, #148916 ),
 .UNSPECIFIED., .F., .F. ) 
 B_SPLINE_CURVE_WITH_KNOTS ( ( 4, 4 ),
 ( 5.733388419619901200, 5.983100554402348337 ),
 .UNSPECIFIED. ) 
 CURVE ( )  GEOMETRIC_REPRESENTATION_ITEM ( )  RATIONAL_B_SPLINE_CURVE ( ( 1.000000000000000000, 0.9948104011409416580, 0.9948104011409416580, 1.000000000000000000 ) ) 
 REPRESENTATION_ITEM ( '' )  );
#251189 = DIRECTION ( 'NONE',  ( 0.000000000000000000, 0.000000000000000000, -1.000000000000000000 ) ) ;
#251190 = CARTESIAN_POINT ( 'NONE',  ( 23.14999999999999503, 11.65000000001116298, -126.9851942293460922 ) ) ;
#251191 = CIRCLE ( 'NONE', #201145, 0.2000000000000005107 ) ;
#251192 = DIRECTION ( 'NONE',  ( 0.000000000000000000, 0.4999999999999949485, -0.8660254037844415942 ) ) ;
#251193 = CIRCLE ( 'NONE', #17971, 4.049999999999998046 ) ;
#251194 = ORIENTED_EDGE ( 'NONE', *, *, #225353, .F. ) ;
#251195 = AXIS2_PLACEMENT_3D ( 'NONE', #130994, #210535, #62362 ) ;
#251196 = AXIS2_PLACEMENT_3D ( 'NONE', #217578, #81903, #38984 ) ;
#251197 = CARTESIAN_POINT ( 'NONE',  ( -16.93583594267724379, 44.02882368590770312, -235.2824757905454760 ) ) ;
#251198 = CARTESIAN_POINT ( 'NONE',  ( -20.87155475150660777, 64.25000000001195133, -109.9275209553671147 ) ) ;
#251199 = PLANE ( 'NONE',  #80327 ) ;
#251200 = ORIENTED_EDGE ( 'NONE', *, *, #132732, .F. ) ;
#251201 = DIRECTION ( 'NONE',  ( -0.7071067811865475727, -0.7071067811865475727, 0.000000000000000000 ) ) ;
#251202 = ORIENTED_EDGE ( 'NONE', *, *, #63189, .T. ) ;
#251203 = DIRECTION ( 'NONE',  ( 1.000000000000000000, 0.000000000000000000, 0.000000000000000000 ) ) ;
#251205 = ORIENTED_EDGE ( 'NONE', *, *, #91802, .F. ) ;
#251204 = VECTOR ( 'NONE', #141204, 1000.000000000000000 ) ;
#251206 = CARTESIAN_POINT ( 'NONE',  ( 23.24999999999999289, 69.35000000001228670, -157.8731074845244109 ) ) ;
#251207 = CARTESIAN_POINT ( 'NONE',  ( 21.05000000000000071, 1.349084418638171412, -74.98649896354552880 ) ) ;
#251209 = EDGE_LOOP ( 'NONE', ( #215328, #68452, #56533, #191341, #117732 ) ) ;
#251208 = DIRECTION ( 'NONE',  ( -1.000000000000000000, -0.000000000000000000, -0.000000000000000000 ) ) ;
#251210 = CARTESIAN_POINT ( 'NONE',  ( 21.05000000000000071, -9.499999999988848032, -143.8939691226524644 ) ) ;
#251211 = ORIENTED_EDGE ( 'NONE', *, *, #113526, .F. ) ;
#251212 = ADVANCED_FACE ( 'NONE', ( #45892 ), #130734, .T. ) ;
#251213 = CARTESIAN_POINT ( 'NONE',  ( -20.94560253601877164, 36.04561250502853653, -235.8930046631029711 ) ) ;
#251214 = AXIS2_PLACEMENT_3D ( 'NONE', #16432, #115499, #58076 ) ;
#251215 = EDGE_LOOP ( 'NONE', ( #143137, #170100, #13108, #31414, #227322 ) ) ;
#251216 = CIRCLE ( 'NONE', #1425, 0.09999999999999939493 ) ;
#251217 = FACE_OUTER_BOUND ( 'NONE', #246635, .T. ) ;
#251218 = DIRECTION ( 'NONE',  ( 0.000000000000000000, 0.000000000000000000, -1.000000000000000000 ) ) ;
#251219 = EDGE_LOOP ( 'NONE', ( #74506, #191793, #149763, #44434 ) ) ;
#251220 = FACE_OUTER_BOUND ( 'NONE', #222252, .T. ) ;
#251221 = ORIENTED_EDGE ( 'NONE', *, *, #242091, .T. ) ;
#251223 =( BOUNDED_SURFACE ( )  B_SPLINE_SURFACE ( 3, 2, ( 
 ( #5611, #27812, #185564 ),
 ( #109864, #189428, #166030 ),
 ( #228559, #124314, #66899 ),
 ( #107305, #186870, #146414 ),
 ( #47313, #8226, #87729 ),
 ( #227252, #246812, #104699 ) ),
 .UNSPECIFIED., .F., .F., .F. ) 
 B_SPLINE_SURFACE_WITH_KNOTS ( ( 4, 2, 4 ),
 ( 3, 3 ),
 ( 6.719893378900507978E-05, 0.0002757154632485607666, 0.0004842319927081164535 ),
 ( 0.000000000000000000, 1.000000000000000000 ),
 .UNSPECIFIED. ) 
 GEOMETRIC_REPRESENTATION_ITEM ( )  RATIONAL_B_SPLINE_SURFACE ( (
 ( 1.000000000000000000, 0.7250110520819756932, 1.000000000000000000),
 ( 1.000000000000000000, 0.7277932058353090428, 1.000000000000000000),
 ( 1.000000000000000000, 0.7278452872625645886, 1.000000000000000000),
 ( 1.000000000000000000, 0.7221445671541159017, 1.000000000000000000),
 ( 1.000000000000000000, 0.7163662143785587411, 1.000000000000000000),
 ( 1.000000000000000000, 0.7071067811865475727, 1.000000000000000000) ) ) 
 REPRESENTATION_ITEM ( '' )  SURFACE ( )  );
#251222 = CIRCLE ( 'NONE', #172199, 0.09999999999999939493 ) ;
#251224 = CONICAL_SURFACE ( 'NONE', #230395, 4.049999999999998046, 0.7853981633974604915 ) ;
#251225 = EDGE_CURVE ( 'NONE', #215142, #170938, #44616, .T. ) ;
#251226 = DIRECTION ( 'NONE',  ( 0.000000000000000000, -0.8814952561688476074, 0.4721928772777262417 ) ) ;
#251227 = CIRCLE ( 'NONE', #84799, 0.1000000000000024342 ) ;
#251228 = DIRECTION ( 'NONE',  ( -0.000000000000000000, 0.2617529984165031243, 0.9651348961777157509 ) ) ;
#251229 = ADVANCED_FACE ( 'NONE', ( #6764 ), #193293, .T. ) ;
#251232 = VERTEX_POINT ( 'NONE', #104547 ) ;
#251231 = ORIENTED_EDGE ( 'NONE', *, *, #249033, .T. ) ;
#251230 = LINE ( 'NONE', #119454, #109786 ) ;
#251233 = CYLINDRICAL_SURFACE ( 'NONE', #99487, 11.75000000000000178 ) ;
#251234 = CARTESIAN_POINT ( 'NONE',  ( -22.49756042579671700, 0.07804633702833754794, -155.8501350388976334 ) ) ;
#251235 = CARTESIAN_POINT ( 'NONE',  ( -23.15000000000000213, 76.00000000001210765, -132.6231074845243540 ) ) ;
#251237 = CARTESIAN_POINT ( 'NONE',  ( 23.24999999999999645, 1.115600667400684642E-11, -200.9999999999999432 ) ) ;
#251236 = DIRECTION ( 'NONE',  ( 0.000000000000000000, -6.982962677686266711E-15, 1.000000000000000000 ) ) ;
#251239 = ADVANCED_FACE ( 'NONE', ( #204946 ), #144973, .T. ) ;
#251238 = CARTESIAN_POINT ( 'NONE',  ( 18.59999999999999787, 86.35479209693686187, -42.26656650145049099 ) ) ;
#251240 = DIRECTION ( 'NONE',  ( 0.000000000000000000, -0.2617529984165031243, -0.9651348961777157509 ) ) ;
#251241 = CIRCLE ( 'NONE', #201373, 0.1000000000000028644 ) ;
#251242 = CARTESIAN_POINT ( 'NONE',  ( -21.59142135623730852, 7.850000000011158718, -155.2500000000000284 ) ) ;
#251243 = AXIS2_PLACEMENT_3D ( 'NONE', #63204, #64511, #99754 ) ;
#251244 = CARTESIAN_POINT ( 'NONE',  ( 21.05000000000000071, -0.09999999998884338825, -67.00000000000004263 ) ) ;
#251245 = AXIS2_PLACEMENT_3D ( 'NONE', #139235, #63564, #103960 ) ;
#251246 = VECTOR ( 'NONE', #109152, 1000.000000000000000 ) ;
#251247 = ORIENTED_EDGE ( 'NONE', *, *, #238008, .T. ) ;
#251248 = ORIENTED_EDGE ( 'NONE', *, *, #49790, .F. ) ;
#251249 = DIRECTION ( 'NONE',  ( 0.000000000000000000, 1.000000000000000000, 6.982962677686266711E-15 ) ) ;
#251251 = ORIENTED_EDGE ( 'NONE', *, *, #253132, .T. ) ;
#251250 = CARTESIAN_POINT ( 'NONE',  ( 20.94999999999999929, 9.459578591139306880, -220.9384041938172345 ) ) ;
#251252 = VERTEX_POINT ( 'NONE', #61605 ) ;
#251253 = DIRECTION ( 'NONE',  ( -0.000000000000000000, 1.000000000000000000, 6.982962677686266711E-15 ) ) ;
#251254 = EDGE_CURVE ( 'NONE', #241330, #208598, #64102, .T. ) ;
#251255 = EDGE_LOOP ( 'NONE', ( #214344, #244701, #249821, #99836 ) ) ;
#251256 = CARTESIAN_POINT ( 'NONE',  ( 21.53699400381148621, 33.88385736505378532, -243.3566462376118693 ) ) ;
#251257 = EDGE_CURVE ( 'NONE', #94704, #174236, #76571, .T. ) ;
#251258 = EDGE_CURVE ( 'NONE', #16182, #151026, #83688, .T. ) ;
#251259 = ORIENTED_EDGE ( 'NONE', *, *, #7963, .F. ) ;
#251260 = DIRECTION ( 'NONE',  ( 1.000000000000000000, 0.000000000000000000, 0.000000000000000000 ) ) ;
#251262 = ORIENTED_EDGE ( 'NONE', *, *, #209126, .F. ) ;
#251261 = EDGE_LOOP ( 'NONE', ( #109217, #15150, #18302, #61988 ) ) ;
#251263 = ORIENTED_EDGE ( 'NONE', *, *, #135745, .T. ) ;
#251264 = ORIENTED_EDGE ( 'NONE', *, *, #211653, .F. ) ;
#251265 = ORIENTED_EDGE ( 'NONE', *, *, #164262, .F. ) ;
#251266 = ADVANCED_FACE ( 'NONE', ( #108437 ), #55877, .T. ) ;
#251267 = DIRECTION ( 'NONE',  ( 1.000000000000000000, 0.000000000000000000, 0.000000000000000000 ) ) ;
#251268 = CARTESIAN_POINT ( 'NONE',  ( 22.57320508075687115, 31.85509083104287598, -238.8280249686205536 ) ) ;
#251269 = CIRCLE ( 'NONE', #80566, 4.049999999999998046 ) ;
#251270 = CARTESIAN_POINT ( 'NONE',  ( 20.94999999999999929, 69.45000000001188312, -93.00608031408432907 ) ) ;
#251272 = ORIENTED_EDGE ( 'NONE', *, *, #87254, .T. ) ;
#251271 = DIRECTION ( 'NONE',  ( -0.000000000000000000, -0.9770955615653316162, -0.2128009952263604232 ) ) ;
#251273 = CYLINDRICAL_SURFACE ( 'NONE', #11575, 0.09999999999999939493 ) ;
#251274 = EDGE_CURVE ( 'NONE', #166912, #252901, #68385, .T. ) ;
#251275 = CARTESIAN_POINT ( 'NONE',  ( 21.46681500593265213, 6.857511159395772715, -167.4999999999999432 ) ) ;
#251277 = VERTEX_POINT ( 'NONE', #250500 ) ;
#251276 = CARTESIAN_POINT ( 'NONE',  ( -18.40000000000000213, 62.49259288703249382, -209.4955626911903721 ) ) ;
#251278 = DIRECTION ( 'NONE',  ( 1.000000000000000000, 0.000000000000000000, 0.000000000000000000 ) ) ;
#251280 = ADVANCED_FACE ( 'NONE', ( #228392 ), #49741, .T. ) ;
#251279 = VERTEX_POINT ( 'NONE', #210118 ) ;
#251281 = DIRECTION ( 'NONE',  ( 1.000000000000000000, 0.000000000000000000, 0.000000000000000000 ) ) ;
#251282 = ORIENTED_EDGE ( 'NONE', *, *, #56101, .F. ) ;
#251283 = CARTESIAN_POINT ( 'NONE',  ( 18.54999999999999716, 8.750000000011182166, -121.3500000000000369 ) ) ;
#251284 = CARTESIAN_POINT ( 'NONE',  ( -16.89318236219975944, 30.21157524432755537, -234.8081138580095626 ) ) ;
#251285 = VERTEX_POINT ( 'NONE', #207548 ) ;
#251287 = DIRECTION ( 'NONE',  ( 0.000000000000000000, 0.8777080977375655291, -0.4791956752370622463 ) ) ;
#251286 = DIRECTION ( 'NONE',  ( 0.000000000000000000, 0.9947597004326452774, -0.1022405907414166287 ) ) ;
#251288 = AXIS2_PLACEMENT_3D ( 'NONE', #112643, #90494, #89214 ) ;
#251289 = DIRECTION ( 'NONE',  ( -1.000000000000000000, -2.952720810173289112E-16, 0.000000000000000000 ) ) ;
#251290 = AXIS2_PLACEMENT_3D ( 'NONE', #147522, #31462, #167119 ) ;
#251291 = CARTESIAN_POINT ( 'NONE',  ( 20.94999999999999929, 45.58907629467868361, -240.2765730862633404 ) ) ;
#251292 = DIRECTION ( 'NONE',  ( -0.7071067811865388020, 0.7071067811865561215, 0.000000000000000000 ) ) ;
#251293 = ORIENTED_EDGE ( 'NONE', *, *, #83020, .T. ) ;
#251295 = ORIENTED_EDGE ( 'NONE', *, *, #21185, .F. ) ;
#251294 = CIRCLE ( 'NONE', #205505, 0.09999999999999939493 ) ;
#251296 = CARTESIAN_POINT ( 'NONE',  ( -21.05000000000000071, 0.05132743235296114565, -127.6998166637300187 ) ) ;
#251297 = CARTESIAN_POINT ( 'NONE',  ( -18.39418127959864435, 62.49526672404898164, -209.4446585493922157 ) ) ;
#251299 = ORIENTED_EDGE ( 'NONE', *, *, #106560, .T. ) ;
#251298 = EDGE_CURVE ( 'NONE', #115598, #185078, #84908, .T. ) ;
#251300 = CARTESIAN_POINT ( 'NONE',  ( -18.40000000000000213, 9.957490673325212427, -220.1701168356097469 ) ) ;
#251301 = VERTEX_POINT ( 'NONE', #53597 ) ;
#251302 = EDGE_CURVE ( 'NONE', #34375, #42715, #101666, .T. ) ;
#251303 = CARTESIAN_POINT ( 'NONE',  ( -21.05000000000000071, 72.02722222756958104, -225.1832529173024398 ) ) ;
#251304 = CARTESIAN_POINT ( 'NONE',  ( 20.84999999999998721, 11.75000000000000000, -33.50000000000000000 ) ) ;
#251305 = CYLINDRICAL_SURFACE ( 'NONE', #95169, 0.09999999999998898659 ) ;
#251307 = ADVANCED_FACE ( 'NONE', ( #208821 ), #51588, .T. ) ;
#251306 = ORIENTED_EDGE ( 'NONE', *, *, #163647, .T. ) ;
#251308 = AXIS2_PLACEMENT_3D ( 'NONE', #76321, #78884, #161031 ) ;
#251309 = DIRECTION ( 'NONE',  ( 0.000000000000000000, 0.000000000000000000, 1.000000000000000000 ) ) ;
#251310 = CIRCLE ( 'NONE', #5592, 0.09999999999999939493 ) ;
#251311 = ORIENTED_EDGE ( 'NONE', *, *, #172169, .T. ) ;
#251312 = ORIENTED_EDGE ( 'NONE', *, *, #39375, .T. ) ;
#251313 = TOROIDAL_SURFACE ( 'NONE', #72867, 11.70000000000000462, 0.1000000000000000056 ) ;
#251314 = ORIENTED_EDGE ( 'NONE', *, *, #159369, .T. ) ;
#251315 = VECTOR ( 'NONE', #92458, 1000.000000000000000 ) ;
#251316 = CARTESIAN_POINT ( 'NONE',  ( 15.15590539855246277, 66.58931770574362474, -54.09196404257614432 ) ) ;
#251317 = DIRECTION ( 'NONE',  ( -1.000000000000000000, 0.000000000000000000, 0.000000000000000000 ) ) ;
#251318 = DIRECTION ( 'NONE',  ( 2.952720810173289112E-16, 1.000000000000000000, 6.982962677686266711E-15 ) ) ;
#251319 = CARTESIAN_POINT ( 'NONE',  ( -20.94999999999999929, 28.50120599808395028, -258.2149742250584268 ) ) ;
#251321 = DIRECTION ( 'NONE',  ( 1.000000000000000000, -0.000000000000000000, 0.000000000000000000 ) ) ;
#251320 = DIRECTION ( 'NONE',  ( 0.000000000000000000, -7.147358527629762208E-15, 1.000000000000000000 ) ) ;
#251323 = ORIENTED_EDGE ( 'NONE', *, *, #182513, .T. ) ;
#251322 = DIRECTION ( 'NONE',  ( 1.000000000000000000, 0.000000000000000000, -0.000000000000000000 ) ) ;
#251324 = CARTESIAN_POINT ( 'NONE',  ( -21.59780538579341425, 10.27473149069560243, -227.6502864689491048 ) ) ;
#251325 = ORIENTED_EDGE ( 'NONE', *, *, #179863, .F. ) ;
#251326 = CARTESIAN_POINT ( 'NONE',  ( -13.12432614554023047, 9.430764995433476017, -149.2305373947504847 ) ) ;
#251327 = VERTEX_POINT ( 'NONE', #28949 ) ;
#251328 = ORIENTED_EDGE ( 'NONE', *, *, #30228, .T. ) ;
#251329 = DIRECTION ( 'NONE',  ( 0.000000000000000000, 0.5000000000000729417, 0.8660254037843965191 ) ) ;
#251331 = VECTOR ( 'NONE', #247450, 1000.000000000000000 ) ;
#251330 = DIRECTION ( 'NONE',  ( 0.000000000000000000, 1.000000000000000000, 1.387778780781444413E-14 ) ) ;
#251332 = EDGE_CURVE ( 'NONE', #252282, #173853, #118279, .T. ) ;
#251333 = AXIS2_PLACEMENT_3D ( 'NONE', #194822, #18725, #53996 ) ;
#251334 = CARTESIAN_POINT ( 'NONE',  ( -20.15000000000000568, 44.13095071803924441, -236.0226064646537054 ) ) ;
#251335 = AXIS2_PLACEMENT_3D ( 'NONE', #132144, #207858, #29236 ) ;
#251336 = EDGE_CURVE ( 'NONE', #64371, #140759, #187980, .T. ) ;
#251337 = CARTESIAN_POINT ( 'NONE',  ( -21.05000000000000071, 77.25000000001232081, -162.0231074845243313 ) ) ;
#251338 = EDGE_LOOP ( 'NONE', ( #223769, #117871, #144215, #184323 ) ) ;
#251339 = VERTEX_POINT ( 'NONE', #109702 ) ;
#251340 = AXIS2_PLACEMENT_3D ( 'NONE', #165047, #245870, #187199 ) ;
#251342 = EDGE_CURVE ( 'NONE', #26458, #106961, #218197, .T. ) ;
#251341 = CARTESIAN_POINT ( 'NONE',  ( 5.900000000000060751, 64.75000000001119815, -22.12310748452479103 ) ) ;
#251343 = ORIENTED_EDGE ( 'NONE', *, *, #62665, .F. ) ;
#251344 = CARTESIAN_POINT ( 'NONE',  ( -18.59999999999999787, 16.50669723772569952, -240.7258389668962479 ) ) ;
#251345 = LINE ( 'NONE', #175692, #123175 ) ;
#251346 = ORIENTED_EDGE ( 'NONE', *, *, #223156, .F. ) ;
#251347 = CARTESIAN_POINT ( 'NONE',  ( 20.94999999999999929, 0.000000000000000000, -12.97499999999999787 ) ) ;
#251348 = CARTESIAN_POINT ( 'NONE',  ( -21.05000000000000071, 11.75000000001115197, -59.98519422934605672 ) ) ;
#251349 = DIRECTION ( 'NONE',  ( 0.000000000000000000, 0.5000000000000078826, -0.8660254037844340447 ) ) ;
#251350 = DIRECTION ( 'NONE',  ( 1.000000000000000000, 8.855395344894292773E-17, 1.653135691717061729E-16 ) ) ;
#251351 = ORIENTED_EDGE ( 'NONE', *, *, #88917, .F. ) ;
#251352 = DIRECTION ( 'NONE',  ( 0.000000000000000000, -1.000000000000000000, -6.982962677686265922E-15 ) ) ;
#251353 = AXIS2_PLACEMENT_3D ( 'NONE', #59928, #140777, #96488 ) ;
#251354 = EDGE_CURVE ( 'NONE', #190057, #193140, #22612, .T. ) ;
#251356 = CARTESIAN_POINT ( 'NONE',  ( -16.94107738177414291, 65.98576071487538286, -115.5731074845243711 ) ) ;
#251355 = VECTOR ( 'NONE', #48193, 1000.000000000000000 ) ;
#251358 = DIRECTION ( 'NONE',  ( 0.000000000000000000, 0.000000000000000000, 1.000000000000000000 ) ) ;
#251357 = AXIS2_PLACEMENT_3D ( 'NONE', #17356, #138546, #79856 ) ;
#251359 = AXIS2_PLACEMENT_3D ( 'NONE', #161635, #41680, #100322 ) ;
#251360 = CARTESIAN_POINT ( 'NONE',  ( 18.60000000000000497, 67.23127455305841238, -235.8551265064783991 ) ) ;
#251362 = EDGE_CURVE ( 'NONE', #210246, #47156, #190559, .T. ) ;
#251361 = LINE ( 'NONE', #210964, #62284 ) ;
#251363 = CARTESIAN_POINT ( 'NONE',  ( -21.05000000000000071, 57.76315019072730905, -226.2583585926041110 ) ) ;
#251364 = EDGE_CURVE ( 'NONE', #19033, #127248, #249239, .T. ) ;
#251365 = ORIENTED_EDGE ( 'NONE', *, *, #187945, .F. ) ;
#251367 = EDGE_CURVE ( 'NONE', #45676, #158833, #105764, .T. ) ;
#251366 = EDGE_CURVE ( 'NONE', #142779, #253844, #201457, .T. ) ;
#251368 = CARTESIAN_POINT ( 'NONE',  ( 21.06280952165543496, 10.62713230060095171, -12.20405388677887260 ) ) ;
#251369 = ORIENTED_EDGE ( 'NONE', *, *, #91321, .F. ) ;
#251370 = DIRECTION ( 'NONE',  ( 0.000000000000000000, 6.982962677686266711E-15, -1.000000000000000000 ) ) ;
#251371 = DIRECTION ( 'NONE',  ( 0.000000000000000000, 0.9126074666063783702, 0.4088369013363252757 ) ) ;
#251372 = DIRECTION ( 'NONE',  ( -0.000000000000000000, 0.1350103645451904977, 0.9908441862701597991 ) ) ;
#251373 = LINE ( 'NONE', #252645, #10547 ) ;
#251374 = CARTESIAN_POINT ( 'NONE',  ( 20.94999999999999929, 76.00000000001185185, -95.22310748452429152 ) ) ;
#251375 = DIRECTION ( 'NONE',  ( 0.000000000000000000, 0.000000000000000000, -1.000000000000000000 ) ) ;
#251376 = ORIENTED_EDGE ( 'NONE', *, *, #81437, .F. ) ;
#251377 = DIRECTION ( 'NONE',  ( 1.000000000000000000, 0.000000000000000000, 0.000000000000000000 ) ) ;
#251378 = AXIS2_PLACEMENT_3D ( 'NONE', #153360, #214559, #131172 ) ;
#251379 = CARTESIAN_POINT ( 'NONE',  ( 21.05000000000000071, 67.22371710471958295, -124.3731074845243683 ) ) ;
#251380 = DIRECTION ( 'NONE',  ( -1.000000000000000000, -0.000000000000000000, 0.000000000000000000 ) ) ;
#251382 = TOROIDAL_SURFACE ( 'NONE', #226409, 0.2000000000000000111, 0.1000000000000000056 ) ;
#251381 = CARTESIAN_POINT ( 'NONE',  ( 18.59999999999999076, 74.25000000001229239, -158.3535959266227451 ) ) ;
#251383 = AXIS2_PLACEMENT_3D ( 'NONE', #242461, #238627, #22166 ) ;
#251384 = EDGE_CURVE ( 'NONE', #35500, #139208, #147561, .T. ) ;
#251385 = EDGE_CURVE ( 'NONE', #126780, #230477, #147409, .T. ) ;
#251386 = DIRECTION ( 'NONE',  ( -1.000000000000000000, -0.000000000000000000, -0.000000000000000000 ) ) ;
#251387 = ORIENTED_EDGE ( 'NONE', *, *, #148297, .T. ) ;
#251388 = EDGE_LOOP ( 'NONE', ( #39826, #243336, #221404, #197764 ) ) ;
#251389 = FACE_OUTER_BOUND ( 'NONE', #1429, .T. ) ;
#251391 = EDGE_CURVE ( 'NONE', #189431, #80026, #18318, .T. ) ;
#251390 = CARTESIAN_POINT ( 'NONE',  ( -23.25000000000000000, 77.25000000001239187, -162.2226267301092548 ) ) ;
#251392 = AXIS2_PLACEMENT_3D ( 'NONE', #139653, #40626, #122710 ) ;
#251393 = CARTESIAN_POINT ( 'NONE',  ( -16.86578989773641979, 44.01660614304713448, -235.3140431590063031 ) ) ;
#251394 = ORIENTED_EDGE ( 'NONE', *, *, #127198, .T. ) ;
#251396 = EDGE_CURVE ( 'NONE', #42929, #50099, #30807, .T. ) ;
#251395 = DIRECTION ( 'NONE',  ( 0.000000000000000000, 0.000000000000000000, -1.000000000000000000 ) ) ;
#251397 = AXIS2_PLACEMENT_3D ( 'NONE', #231859, #175742, #33689 ) ;
#251398 = CONTEXT_DEPENDENT_SHAPE_REPRESENTATION ( #64190, #39239 ) ;
#251399 = ADVANCED_FACE ( 'NONE', ( #174881 ), #78274, .T. ) ;
#251400 = CARTESIAN_POINT ( 'NONE',  ( 21.05000000000000071, 76.00000000001213607, -136.5231074845243313 ) ) ;
#251401 = ORIENTED_EDGE ( 'NONE', *, *, #146937, .T. ) ;
#251402 = DIRECTION ( 'NONE',  ( 0.000000000000000000, -7.429790795770644761E-15, 1.000000000000000000 ) ) ;
#251403 = TOROIDAL_SURFACE ( 'NONE', #68061, 0.6000000000000006439, 0.1000000000000000056 ) ;
#251404 = AXIS2_PLACEMENT_3D ( 'NONE', #147705, #210257, #69465 ) ;
#251405 = PRODUCT_DEFINITION_SHAPE ( 'NONE', 'NONE',  #252419 ) ;
#251406 = VECTOR ( 'NONE', #109132, 1000.000000000000227 ) ;
#251407 = ORIENTED_EDGE ( 'NONE', *, *, #157422, .T. ) ;
#251409 = VERTEX_POINT ( 'NONE', #15785 ) ;
#251408 = CARTESIAN_POINT ( 'NONE',  ( 22.60000000000000142, 11.74956712350054744, -66.89914163090134025 ) ) ;
#251410 = ORIENTED_EDGE ( 'NONE', *, *, #62305, .T. ) ;
#251411 = EDGE_CURVE ( 'NONE', #24859, #188797, #195701, .T. ) ;
#251412 = PLANE ( 'NONE',  #155895 ) ;
#251414 = ADVANCED_FACE ( 'NONE', ( #238651 ), #56139, .F. ) ;
#251413 = DIRECTION ( 'NONE',  ( 2.694716079187272946E-16, -1.000000000000000000, 0.000000000000000000 ) ) ;
#251416 = CIRCLE ( 'NONE', #5682, 0.09999999999999824307 ) ;
#251415 = FACE_OUTER_BOUND ( 'NONE', #196387, .T. ) ;
#251417 = CARTESIAN_POINT ( 'NONE',  ( -23.15000000000000213, 59.59835781587673154, -226.3993831679961488 ) ) ;
#251418 = CYLINDRICAL_SURFACE ( 'NONE', #169528, 11.80000000000000426 ) ;
#251419 = DIRECTION ( 'NONE',  ( 0.000000000000000000, 0.000000000000000000, 1.000000000000000000 ) ) ;
#251420 = DIRECTION ( 'NONE',  ( 1.000000000000000000, 1.186688945009010077E-16, 0.000000000000000000 ) ) ;
#251422 = CARTESIAN_POINT ( 'NONE',  ( 22.57320508075687115, 11.75000000001115552, -167.4999999999999716 ) ) ;
#251421 = DIRECTION ( 'NONE',  ( 0.000000000000000000, 0.8660254037844411501, 0.4999999999999956701 ) ) ;
#251423 = EDGE_CURVE ( 'NONE', #162455, #242379, #59992, .T. ) ;
#251424 = AXIS2_PLACEMENT_3D ( 'NONE', #227838, #248696, #49204 ) ;
#251425 = FACE_OUTER_BOUND ( 'NONE', #169941, .T. ) ;
#251426 = DIRECTION ( 'NONE',  ( 0.000000000000000000, 0.2128009952263605065, -0.9770955615653315052 ) ) ;
#251427 = DIRECTION ( 'NONE',  ( 0.000000000000000000, 0.000000000000000000, -1.000000000000000000 ) ) ;
#251428 = CARTESIAN_POINT ( 'NONE',  ( 21.05000000000000071, 5.000000000011153745, -189.0947339810868755 ) ) ;
#251429 = ORIENTED_EDGE ( 'NONE', *, *, #31224, .F. ) ;
#251430 = CARTESIAN_POINT ( 'NONE',  ( -20.96077737575343392, 11.62390063401577933, -93.64079195710642978 ) ) ;
#251431 = AXIS2_PLACEMENT_3D ( 'NONE', #47584, #206677, #144111 ) ;
#251432 = CARTESIAN_POINT ( 'NONE',  ( 21.05000000000000071, -1.849084418615859926, -145.6560105214471434 ) ) ;
#251433 = DIRECTION ( 'NONE',  ( 1.000000000000000000, 0.000000000000000000, 0.000000000000000000 ) ) ;
#251434 = CIRCLE ( 'NONE', #18210, 0.09999999999999939493 ) ;
#251435 = AXIS2_PLACEMENT_3D ( 'NONE', #154589, #159700, #256150 ) ;
#251436 = LINE ( 'NONE', #230601, #68927 ) ;
#251437 = CARTESIAN_POINT ( 'NONE',  ( 20.94999999999999929, 76.00000000001170974, -69.52310748452431710 ) ) ;
#251438 = ADVANCED_FACE ( 'NONE', ( #97820 ), #216515, .F. ) ;
#251439 = CARTESIAN_POINT ( 'NONE',  ( -20.94999999999999929, 87.29603075034741266, -133.4752083248603469 ) ) ;
#251440 = ORIENTED_EDGE ( 'NONE', *, *, #23388, .T. ) ;
#251441 = ORIENTED_EDGE ( 'NONE', *, *, #166807, .F. ) ;
#251442 = ORIENTED_EDGE ( 'NONE', *, *, #241713, .F. ) ;
#251443 = CARTESIAN_POINT ( 'NONE',  ( -20.54999999999999716, 1.115600667400684642E-11, -167.5000000000000284 ) ) ;
#251444 = DIRECTION ( 'NONE',  ( 0.000000000000000000, 0.9126074666063660468, 0.4088369013363524762 ) ) ;
#251445 = TOROIDAL_SURFACE ( 'NONE', #217537, 2.100000000000002309, 0.1000000000000000056 ) ;
#251446 = EDGE_CURVE ( 'NONE', #166015, #68443, #176134, .T. ) ;
#251447 = CIRCLE ( 'NONE', #180543, 0.1000000000000024342 ) ;
#251448 = AXIS2_PLACEMENT_3D ( 'NONE', #29371, #188397, #8491 ) ;
#251449 = EDGE_LOOP ( 'NONE', ( #120880, #235002, #22921, #119805 ) ) ;
#251450 = DIRECTION ( 'NONE',  ( 0.000000000000000000, -1.000000000000000000, 0.000000000000000000 ) ) ;
#251451 = ORIENTED_EDGE ( 'NONE', *, *, #239075, .F. ) ;
#251452 = CARTESIAN_POINT ( 'NONE',  ( -6.100000000000012079, -11.65000000000000036, -15.00000000000000355 ) ) ;
#251453 = LINE ( 'NONE', #234446, #91099 ) ;
#251454 = DIRECTION ( 'NONE',  ( -1.186688945009010077E-16, 1.000000000000000000, 0.000000000000000000 ) ) ;
#251455 = CARTESIAN_POINT ( 'NONE',  ( -16.85939591225058365, 9.905226478387843869, -12.96006824646904931 ) ) ;
#251456 = LINE ( 'NONE', #147223, #179075 ) ;
#251457 = DIRECTION ( 'NONE',  ( 0.000000000000000000, 0.000000000000000000, -1.000000000000000000 ) ) ;
#251459 = ORIENTED_EDGE ( 'NONE', *, *, #203835, .F. ) ;
#251458 = CARTESIAN_POINT ( 'NONE',  ( 18.59999996954842771, -0.7115290284072351978, -242.4846381375031115 ) ) ;
#251461 = FACE_OUTER_BOUND ( 'NONE', #18625, .T. ) ;
#251460 = FACE_OUTER_BOUND ( 'NONE', #186493, .T. ) ;
#251462 = ORIENTED_EDGE ( 'NONE', *, *, #163565, .T. ) ;
#251463 = EDGE_LOOP ( 'NONE', ( #144535, #109439, #170834, #91198 ) ) ;
#251464 = VERTEX_POINT ( 'NONE', #57425 ) ;
#251465 = DIRECTION ( 'NONE',  ( -0.8049926720990042694, 0.5932847527679310229, 4.142885285818786163E-15 ) ) ;
#251466 = CARTESIAN_POINT ( 'NONE',  ( 21.14999999999999858, 64.35000000001204512, -124.3731074845243825 ) ) ;
#251467 = AXIS2_PLACEMENT_3D ( 'NONE', #190229, #188943, #126392 ) ;
#251468 = DIRECTION ( 'NONE',  ( 1.000000000000000000, 0.000000000000000000, 0.000000000000000000 ) ) ;
#251469 = CARTESIAN_POINT ( 'NONE',  ( 18.42595409746870772, -9.499999812565054214, -6.999362351746812649 ) ) ;
#251470 = DIRECTION ( 'NONE',  ( 1.000000000000000000, 0.000000000000000000, 0.000000000000000000 ) ) ;
#251471 = FACE_OUTER_BOUND ( 'NONE', #102334, .T. ) ;
#251472 = CARTESIAN_POINT ( 'NONE',  ( -16.94107738177415357, 12.45552124806248706, -211.1315092113344463 ) ) ;
#251473 = EDGE_CURVE ( 'NONE', #195077, #186448, #64287, .T. ) ;
#251474 = DIRECTION ( 'NONE',  ( 0.000000000000000000, 0.1568667991644355497, -0.9876197685951332295 ) ) ;
#251475 = ORIENTED_EDGE ( 'NONE', *, *, #65694, .T. ) ;
#251476 = VERTEX_POINT ( 'NONE', #54856 ) ;
#251477 = CARTESIAN_POINT ( 'NONE',  ( 18.57071067811864040, 14.48943966439392206, -219.6948273410279455 ) ) ;
#251478 = CIRCLE ( 'NONE', #80774, 0.09999999999999771572 ) ;
#251479 = AXIS2_PLACEMENT_3D ( 'NONE', #74127, #55770, #113212 ) ;
#251480 = ORIENTED_EDGE ( 'NONE', *, *, #227513, .F. ) ;
#251481 = DIRECTION ( 'NONE',  ( -7.304098846218134667E-16, 1.000000000000000000, 6.982962677686267499E-15 ) ) ;
#251482 = ORIENTED_EDGE ( 'NONE', *, *, #168872, .T. ) ;
#251483 = FACE_OUTER_BOUND ( 'NONE', #180369, .T. ) ;
#251484 = CONICAL_SURFACE ( 'NONE', #230861, 4.299999999999956302, 0.7853981633974466137 ) ;
#251485 = DIRECTION ( 'NONE',  ( 1.000000000000000000, 0.000000000000000000, 0.000000000000000000 ) ) ;
#251486 = DIRECTION ( 'NONE',  ( 0.000000000000000000, 0.000000000000000000, -1.000000000000000000 ) ) ;
#251487 = EDGE_CURVE ( 'NONE', #11297, #202894, #77002, .T. ) ;
#251488 = CARTESIAN_POINT ( 'NONE',  ( 23.24999999999999645, 72.10000000001190301, -103.0231074845243313 ) ) ;
#251489 = CARTESIAN_POINT ( 'NONE',  ( -18.59999999999999787, 1.736257131608553550, -112.0686523290175245 ) ) ;
#251490 = ORIENTED_EDGE ( 'NONE', *, *, #114524, .T. ) ;
#251491 = DIRECTION ( 'NONE',  ( 1.000000000000000000, 0.000000000000000000, 0.000000000000000000 ) ) ;
#251492 = EDGE_CURVE ( 'NONE', #236853, #215160, #217777, .T. ) ;
#251493 = DIRECTION ( 'NONE',  ( 1.000000000000000000, 0.000000000000000000, 0.000000000000000000 ) ) ;
#251494 = CARTESIAN_POINT ( 'NONE',  ( -21.05000000000000071, -11.48912529306490349, -170.3999999999999773 ) ) ;
#251495 = CARTESIAN_POINT ( 'NONE',  ( 16.87683809663749557, 66.05000000001226113, -149.1731074845244223 ) ) ;
#251496 = ORIENTED_EDGE ( 'NONE', *, *, #237553, .T. ) ;
#251498 = CARTESIAN_POINT ( 'NONE',  ( -23.15000000000000213, 85.60000000001150511, -45.91707660717669626 ) ) ;
#251497 = DIRECTION ( 'NONE',  ( -0.000000000000000000, 0.000000000000000000, -1.000000000000000000 ) ) ;
#251499 = EDGE_CURVE ( 'NONE', #248870, #15247, #181004, .T. ) ;
#251500 = VERTEX_POINT ( 'NONE', #36633 ) ;
#251503 = EDGE_LOOP ( 'NONE', ( #257465, #135687, #249315, #28356, #17582, #33758, #28536, #203342, #104117, #151716, #193807, #130904 ) ) ;
#251502 = CARTESIAN_POINT ( 'NONE',  ( -18.59999999999999787, -1.162701749926853712, -41.60000000000000142 ) ) ;
#251501 = CARTESIAN_POINT ( 'NONE',  ( 18.79999999999999716, 8.000000000000000000, -1.212568896937008089 ) ) ;
#251504 = FACE_OUTER_BOUND ( 'NONE', #74633, .T. ) ;
#251505 = AXIS2_PLACEMENT_3D ( 'NONE', #221323, #257855, #96253 ) ;
#251506 = CIRCLE ( 'NONE', #139040, 0.09999999999998898659 ) ;
#251507 = EDGE_CURVE ( 'NONE', #167762, #101102, #74481, .T. ) ;
#251508 = CARTESIAN_POINT ( 'NONE',  ( -23.25000000000000000, 67.23127455305841238, -235.8551265064783991 ) ) ;
#251509 = VERTEX_POINT ( 'NONE', #35355 ) ;
#251510 = DIRECTION ( 'NONE',  ( -1.073024830501117725E-15, 6.982962677686266711E-15, -1.000000000000000000 ) ) ;
#251511 = EDGE_CURVE ( 'NONE', #53673, #230960, #85092, .T. ) ;
#251512 = DIRECTION ( 'NONE',  ( 0.000000000000000000, -7.086529944415886769E-15, 1.000000000000000000 ) ) ;
#251513 = ADVANCED_FACE ( 'NONE', ( #204640 ), #243783, .T. ) ;
#251514 = DIRECTION ( 'NONE',  ( 1.000000000000000000, 0.000000000000000000, 0.000000000000000000 ) ) ;
#251516 = ORIENTED_EDGE ( 'NONE', *, *, #80520, .T. ) ;
#251515 = CARTESIAN_POINT ( 'NONE',  ( 20.94999999999999929, 77.36242903720497566, -61.63422623660309796 ) ) ;
#251517 = AXIS2_PLACEMENT_3D ( 'NONE', #218575, #137756, #38681 ) ;
#251518 = AXIS2_PLACEMENT_3D ( 'NONE', #23260, #182321, #25794 ) ;
#251519 = CIRCLE ( 'NONE', #255568, 1.749999999999999778 ) ;
#251520 = ADVANCED_FACE ( 'NONE', ( #105517 ), #24768, .F. ) ;
#251521 = ORIENTED_EDGE ( 'NONE', *, *, #18814, .T. ) ;
#251522 = DIRECTION ( 'NONE',  ( 0.000000000000000000, 0.000000000000000000, 1.000000000000000000 ) ) ;
#251523 = DIRECTION ( 'NONE',  ( -3.265361837132813093E-16, -1.000000000000000000, -6.982962677686266711E-15 ) ) ;
#251524 = TOROIDAL_SURFACE ( 'NONE', #43429, 0.6000000000000004219, 0.1000000000000000056 ) ;
#251525 = DIRECTION ( 'NONE',  ( 0.000000000000000000, 1.000000000000000000, 6.938893903907222067E-15 ) ) ;
#251526 = ORIENTED_EDGE ( 'NONE', *, *, #94314, .T. ) ;
#251527 = CARTESIAN_POINT ( 'NONE',  ( 21.05000000000000071, 1.115653327213047955E-11, -71.30000000000006821 ) ) ;
#251528 = AXIS2_PLACEMENT_3D ( 'NONE', #103024, #225525, #26087 ) ;
#251529 = LINE ( 'NONE', #115884, #43320 ) ;
#251530 = DIRECTION ( 'NONE',  ( 0.000000000000000000, 4.336808689942494997E-15, -1.000000000000000000 ) ) ;
#251531 = ORIENTED_EDGE ( 'NONE', *, *, #118928, .T. ) ;
#251532 = CARTESIAN_POINT ( 'NONE',  ( 20.97438252431638972, 60.83470529572428376, -225.3418895363082868 ) ) ;
#251533 = AXIS2_PLACEMENT_3D ( 'NONE', #232296, #15825, #118761 ) ;
#251534 = AXIS2_PLACEMENT_3D ( 'NONE', #168465, #13197, #48454 ) ;
#251535 = EDGE_CURVE ( 'NONE', #119120, #117897, #218382, .T. ) ;
#251537 = CIRCLE ( 'NONE', #59991, 2.000000000000001776 ) ;
#251536 = DIRECTION ( 'NONE',  ( 0.000000000000000000, -0.4999999999999348299, 0.8660254037844762331 ) ) ;
#251538 = ORIENTED_EDGE ( 'NONE', *, *, #183247, .T. ) ;
#251539 = FACE_OUTER_BOUND ( 'NONE', #34949, .T. ) ;
#251540 = CARTESIAN_POINT ( 'NONE',  ( 20.94999999999999929, 62.08591502004790641, -248.5699171172615820 ) ) ;
#251541 = ORIENTED_EDGE ( 'NONE', *, *, #148886, .F. ) ;
#251542 = VERTEX_POINT ( 'NONE', #26031 ) ;
#251543 = EDGE_CURVE ( 'NONE', #160394, #43801, #201654, .T. ) ;
#251544 = DIRECTION ( 'NONE',  ( 0.000000000000000000, -0.4999999999999689138, -0.8660254037844565822 ) ) ;
#251545 = ORIENTED_EDGE ( 'NONE', *, *, #140278, .T. ) ;
#251547 = ORIENTED_EDGE ( 'NONE', *, *, #110011, .T. ) ;
#251546 = CARTESIAN_POINT ( 'NONE',  ( -20.54999999999999716, 74.05981308412367525, -48.85222669557766295 ) ) ;
#251548 = VERTEX_POINT ( 'NONE', #100395 ) ;
#251551 = ORIENTED_EDGE ( 'NONE', *, *, #234208, .F. ) ;
#251550 = ORIENTED_EDGE ( 'NONE', *, *, #65280, .F. ) ;
#251549 = CARTESIAN_POINT ( 'NONE',  ( -20.85000000000000142, 69.15387683765983695, -166.2853812176745691 ) ) ;
#251552 = CIRCLE ( 'NONE', #80852, 0.09999999999998898659 ) ;
#251553 = VECTOR ( 'NONE', #94017, 1000.000000000000000 ) ;
#251554 = DIRECTION ( 'NONE',  ( 1.000000000000000000, 0.000000000000000000, 0.000000000000000000 ) ) ;
#251555 = ORIENTED_EDGE ( 'NONE', *, *, #52883, .T. ) ;
#251556 = CARTESIAN_POINT ( 'NONE',  ( 21.00000000000000000, 14.02742277431099538, -219.5907614236512870 ) ) ;
#251557 = CARTESIAN_POINT ( 'NONE',  ( 20.85000000000000142, 78.06784868750165174, -195.8985418047209350 ) ) ;
#251558 = VECTOR ( 'NONE', #191206, 999.9999999999998863 ) ;
#251559 = DIRECTION ( 'NONE',  ( 0.000000000000000000, -1.000000000000000000, 0.000000000000000000 ) ) ;
#251560 =( BOUNDED_CURVE ( )  B_SPLINE_CURVE ( 3, ( #4279, #71981, #172402, #214049 ),
 .UNSPECIFIED., .F., .T. ) 
 B_SPLINE_CURVE_WITH_KNOTS ( ( 4, 4 ),
 ( 3.192897208853993085, 4.712388980384689674 ),
 .UNSPECIFIED. ) 
 CURVE ( )  GEOMETRIC_REPRESENTATION_ITEM ( )  RATIONAL_B_SPLINE_CURVE ( ( 1.000000000000000000, 0.8166740347213228279, 0.8166740347213228279, 1.000000000000000000 ) ) 
 REPRESENTATION_ITEM ( '' )  );
#251561 = EDGE_CURVE ( 'NONE', #41617, #14945, #176729, .T. ) ;
#251562 = DIRECTION ( 'NONE',  ( 1.000000000000000000, 0.000000000000000000, 0.000000000000000000 ) ) ;
#251563 = CARTESIAN_POINT ( 'NONE',  ( -22.39999999999999858, 76.00000000001203659, -114.6726782920691221 ) ) ;
#251564 = ORIENTED_EDGE ( 'NONE', *, *, #3776, .T. ) ;
#251565 = ORIENTED_EDGE ( 'NONE', *, *, #242883, .F. ) ;
#251567 = ORIENTED_EDGE ( 'NONE', *, *, #58971, .F. ) ;
#251566 = CIRCLE ( 'NONE', #39224, 0.09999999999999939493 ) ;
#251568 = DIRECTION ( 'NONE',  ( -1.000000000000000000, -0.000000000000000000, -0.000000000000000000 ) ) ;
#251569 = AXIS2_PLACEMENT_3D ( 'NONE', #23311, #162812, #63680 ) ;
#251571 = VERTEX_POINT ( 'NONE', #162987 ) ;
#251570 = DIRECTION ( 'NONE',  ( -1.000000000000000000, 0.000000000000000000, 0.000000000000000000 ) ) ;
#251572 = FACE_OUTER_BOUND ( 'NONE', #175357, .T. ) ;
#251574 = EDGE_LOOP ( 'NONE', ( #51150, #48594, #58111, #111374, #211721 ) ) ;
#251573 = CARTESIAN_POINT ( 'NONE',  ( 18.59999999999999787, 76.00000000001237765, -170.0231074845243597 ) ) ;
#251575 = ADVANCED_FACE ( 'NONE', ( #85957 ), #183809, .T. ) ;
#251576 = ORIENTED_EDGE ( 'NONE', *, *, #90443, .F. ) ;
#251577 = DIRECTION ( 'NONE',  ( 0.000000000000000000, 0.000000000000000000, 1.000000000000000000 ) ) ;
#251578 = VECTOR ( 'NONE', #56701, 1000.000000000000000 ) ;
#251579 = AXIS2_PLACEMENT_3D ( 'NONE', #159092, #179932, #199500 ) ;
#251580 = ADVANCED_FACE ( 'NONE', ( #241232 ), #145954, .T. ) ;
#251581 = EDGE_CURVE ( 'NONE', #60670, #442, #234716, .T. ) ;
#251582 = VECTOR ( 'NONE', #174515, 1000.000000000000000 ) ;
#251583 = VERTEX_POINT ( 'NONE', #181266 ) ;
#251584 = AXIS2_PLACEMENT_3D ( 'NONE', #216010, #139014, #200317 ) ;
#251585 = CARTESIAN_POINT ( 'NONE',  ( -16.85718274719422283, 66.02385768539039645, -149.0864538167066371 ) ) ;
#251586 = LINE ( 'NONE', #49539, #165379 ) ;
#251587 = EDGE_CURVE ( 'NONE', #248221, #28696, #143397, .T. ) ;
#251588 = VECTOR ( 'NONE', #8768, 1000.000000000000000 ) ;
#251590 = ORIENTED_EDGE ( 'NONE', *, *, #96311, .T. ) ;
#251589 = ORIENTED_EDGE ( 'NONE', *, *, #206244, .F. ) ;
#251591 = ORIENTED_EDGE ( 'NONE', *, *, #106139, .T. ) ;
#251592 = CARTESIAN_POINT ( 'NONE',  ( -23.39999999999994529, 77.83551161375991967, -47.62760213295649692 ) ) ;
#251593 = EDGE_LOOP ( 'NONE', ( #185974, #201068, #80946, #188670, #75763 ) ) ;
#251594 = ORIENTED_EDGE ( 'NONE', *, *, #257151, .F. ) ;
#251595 = ADVANCED_FACE ( 'NONE', ( #61298 ), #239945, .F. ) ;
#251596 = CARTESIAN_POINT ( 'NONE',  ( 21.05000000000000071, 10.72371710471867701, -108.1649135690876449 ) ) ;
#251598 = ORIENTED_EDGE ( 'NONE', *, *, #193896, .F. ) ;
#251597 = CARTESIAN_POINT ( 'NONE',  ( 18.49999999999999289, 10.32573593128807232, -24.85000000000000142 ) ) ;
#251599 = DIRECTION ( 'NONE',  ( 0.000000000000000000, 0.2617529984164915779, 0.9651348961777189706 ) ) ;
#251600 = AXIS2_PLACEMENT_3D ( 'NONE', #214492, #158416, #35889 ) ;
#251602 = CARTESIAN_POINT ( 'NONE',  ( 21.14999999999999858, -11.74999999998884448, -112.7500000000000284 ) ) ;
#251601 = DIRECTION ( 'NONE',  ( -3.265361837132813586E-16, 0.9770955615653357240, 0.2128009952263412996 ) ) ;
#251603 = CARTESIAN_POINT ( 'NONE',  ( 18.59999999999999076, -1.149570369575693807, -41.31591248450196474 ) ) ;
#251604 = CARTESIAN_POINT ( 'NONE',  ( 20.94999999999999929, 6.649999999999999467, -21.25000000000000000 ) ) ;
#251605 = ORIENTED_EDGE ( 'NONE', *, *, #199284, .F. ) ;
#251606 = ORIENTED_EDGE ( 'NONE', *, *, #62311, .F. ) ;
#251607 = CARTESIAN_POINT ( 'NONE',  ( 18.44206774312970154, 85.49102735755195681, -96.39687997982596812 ) ) ;
#251608 = CIRCLE ( 'NONE', #139143, 0.09999999999999939493 ) ;
#251609 = DIRECTION ( 'NONE',  ( 1.000000000000000000, 0.000000000000000000, 0.000000000000000000 ) ) ;
#251610 = CARTESIAN_POINT ( 'NONE',  ( 22.50000000000000000, 0.09999999999999939493, 11.64957080754479968 ) ) ;
#251611 = VERTEX_POINT ( 'NONE', #221627 ) ;
#251612 = DIRECTION ( 'NONE',  ( 0.000000000000000000, -0.000000000000000000, 1.000000000000000000 ) ) ;
#251613 = VECTOR ( 'NONE', #72319, 1000.000000000000000 ) ;
#251614 = VECTOR ( 'NONE', #91515, 1000.000000000000000 ) ;
#251615 = EDGE_CURVE ( 'NONE', #219222, #64828, #101858, .T. ) ;
#251616 = CARTESIAN_POINT ( 'NONE',  ( 20.90000000000000213, -1.311673547813416718, -7.986648289447971116 ) ) ;
#251617 = CIRCLE ( 'NONE', #10213, 6.258578643762696458 ) ;
#251618 = CARTESIAN_POINT ( 'NONE',  ( -23.15000000000000213, 76.00000000001212186, -134.5231074845243313 ) ) ;
#251619 = ORIENTED_EDGE ( 'NONE', *, *, #40204, .F. ) ;
#251620 = ORIENTED_EDGE ( 'NONE', *, *, #103497, .T. ) ;
#251621 = DIRECTION ( 'NONE',  ( 0.000000000000000000, 0.000000000000000000, -1.000000000000000000 ) ) ;
#251622 = CARTESIAN_POINT ( 'NONE',  ( -20.64999999999999858, 73.50000000001186606, -89.79848556176223440 ) ) ;
#251624 = ADVANCED_FACE ( 'NONE', ( #108128 ), #148543, .T. ) ;
#251623 = ORIENTED_EDGE ( 'NONE', *, *, #62454, .T. ) ;
#251625 = CARTESIAN_POINT ( 'NONE',  ( 18.60000000000000497, 76.00000000001267608, -203.5231074845243597 ) ) ;
#251626 = ORIENTED_EDGE ( 'NONE', *, *, #89409, .T. ) ;
#251627 = EDGE_CURVE ( 'NONE', #208155, #114552, #71589, .T. ) ;
#251628 = CARTESIAN_POINT ( 'NONE',  ( 18.37172112093886511, -9.570961652231645189, -140.8167344534842300 ) ) ;
#251629 = CARTESIAN_POINT ( 'NONE',  ( -18.59999999999999787, 51.28888318656202472, -230.2315015618842153 ) ) ;
#251631 = DIRECTION ( 'NONE',  ( 1.000000000000000000, 0.000000000000000000, 0.000000000000000000 ) ) ;
#251630 = DIRECTION ( 'NONE',  ( 4.408576920032447355E-17, -0.1350103645451876666, 0.9908441862701600211 ) ) ;
#251632 = CARTESIAN_POINT ( 'NONE',  ( -22.47071067811865319, 1.115600667400684642E-11, -134.0000000000000000 ) ) ;
#251633 = DIRECTION ( 'NONE',  ( 0.000000000000000000, -0.9126074666063660468, -0.4088369013363524762 ) ) ;
#251634 = DIRECTION ( 'NONE',  ( 1.000000000000000000, -0.000000000000000000, -0.000000000000000000 ) ) ;
#251635 = EDGE_CURVE ( 'NONE', #29429, #2330, #205933, .T. ) ;
#251637 = ORIENTED_EDGE ( 'NONE', *, *, #101358, .T. ) ;
#251636 = DIRECTION ( 'NONE',  ( -1.000000000000000000, -0.000000000000000000, -0.000000000000000000 ) ) ;
#251638 = CIRCLE ( 'NONE', #26802, 4.049999999999998046 ) ;
#251639 = CIRCLE ( 'NONE', #76840, 0.09999999999999939493 ) ;
#251641 = ORIENTED_EDGE ( 'NONE', *, *, #231159, .F. ) ;
#251640 = VERTEX_POINT ( 'NONE', #88536 ) ;
#251642 = VERTEX_POINT ( 'NONE', #208528 ) ;
#251643 = CARTESIAN_POINT ( 'NONE',  ( 21.13736287352038445, 67.95335762362805099, -123.8731074845243540 ) ) ;
#251644 = CARTESIAN_POINT ( 'NONE',  ( -20.00857864376270001, 44.10700160683882132, -235.9691471569722125 ) ) ;
#251646 = DIRECTION ( 'NONE',  ( 0.000000000000000000, -6.454785026890406770E-15, 1.000000000000000000 ) ) ;
#251645 = CARTESIAN_POINT ( 'NONE',  ( -20.94999999999999929, 18.34711819382569686, -236.8747682978092541 ) ) ;
#251647 = CARTESIAN_POINT ( 'NONE',  ( 21.00000000000000000, 66.25000000001206502, -124.1731074845243654 ) ) ;
#251648 = EDGE_LOOP ( 'NONE', ( #255771, #30010, #112325, #236225 ) ) ;
#251649 = CYLINDRICAL_SURFACE ( 'NONE', #250727, 11.80000000000000426 ) ;
#251650 = ORIENTED_EDGE ( 'NONE', *, *, #56339, .T. ) ;
#251652 = ADVANCED_FACE ( 'NONE', ( #207242 ), #31200, .T. ) ;
#251651 = ORIENTED_EDGE ( 'NONE', *, *, #49349, .T. ) ;
#251653 = CARTESIAN_POINT ( 'NONE',  ( 23.15000000000000213, 87.65000000001221281, -148.2731074845242176 ) ) ;
#251654 = FACE_BOUND ( 'NONE', #43389, .T. ) ;
#251655 = CARTESIAN_POINT ( 'NONE',  ( -21.11833042828132889, 1.450380929312672817, -230.6828547334855841 ) ) ;
#251656 = CARTESIAN_POINT ( 'NONE',  ( 21.05000000000000071, 76.00000000001192291, -104.9231074845242944 ) ) ;
#251657 = AXIS2_PLACEMENT_3D ( 'NONE', #156261, #175810, #177104 ) ;
#251658 = DIRECTION ( 'NONE',  ( 1.000000000000000000, 0.000000000000000000, 0.000000000000000000 ) ) ;
#251659 = ORIENTED_EDGE ( 'NONE', *, *, #149217, .T. ) ;
#251660 = ORIENTED_EDGE ( 'NONE', *, *, #256017, .T. ) ;
#251661 = DIRECTION ( 'NONE',  ( -0.000000000000000000, -1.000000000000000000, -5.421010862427649374E-16 ) ) ;
#251662 = SPHERICAL_SURFACE ( 'NONE', #193780, 0.1000000000000000056 ) ;
#251663 = CARTESIAN_POINT ( 'NONE',  ( -23.25000000000000000, 4.150000000011156764, -88.15000000000004832 ) ) ;
#251664 = DIRECTION ( 'NONE',  ( 0.000000000000000000, 0.000000000000000000, -1.000000000000000000 ) ) ;
#251665 = DIRECTION ( 'NONE',  ( -1.000000000000000000, 0.000000000000000000, 0.000000000000000000 ) ) ;
#251666 = LINE ( 'NONE', #152604, #209147 ) ;
#251667 = CARTESIAN_POINT ( 'NONE',  ( -21.14999999999999858, 1.115600667400684642E-11, -167.4999999999999716 ) ) ;
#251668 = EDGE_CURVE ( 'NONE', #182258, #179132, #147680, .T. ) ;
#251670 = DIRECTION ( 'NONE',  ( -1.000000000000000000, 0.000000000000000000, 0.000000000000000000 ) ) ;
#251669 = DIRECTION ( 'NONE',  ( 0.000000000000000000, 0.000000000000000000, 1.000000000000000000 ) ) ;
#251671 = DIRECTION ( 'NONE',  ( -0.000000000000000000, 1.000000000000000000, 1.626303258728266709E-15 ) ) ;
#251672 = CARTESIAN_POINT ( 'NONE',  ( -20.64999999999999858, 68.85000000001186038, -90.67310748452435121 ) ) ;
#251674 = EDGE_CURVE ( 'NONE', #7052, #255010, #43442, .T. ) ;
#251673 = FACE_OUTER_BOUND ( 'NONE', #180147, .T. ) ;
#251675 = DIRECTION ( 'NONE',  ( -1.000000000000000000, -2.952720810173289112E-16, 0.000000000000000000 ) ) ;
#251676 = AXIS2_PLACEMENT_3D ( 'NONE', #88593, #69072, #129034 ) ;
#251678 = VERTEX_POINT ( 'NONE', #147245 ) ;
#251677 = DIRECTION ( 'NONE',  ( 0.000000000000000000, -0.9915357197604853789, 0.1298341882520022694 ) ) ;
#251679 = AXIS2_PLACEMENT_3D ( 'NONE', #161346, #40132, #83036 ) ;
#251680 = VECTOR ( 'NONE', #203230, 1000.000000000000000 ) ;
#251681 = CIRCLE ( 'NONE', #114296, 0.09999999999999939493 ) ;
#251682 = EDGE_CURVE ( 'NONE', #171946, #206620, #214313, .T. ) ;
#251683 = ADVANCED_FACE ( 'NONE', ( #32477 ), #109390, .T. ) ;
#251684 = DIRECTION ( 'NONE',  ( 1.000000000000000000, 0.000000000000000000, 0.000000000000000000 ) ) ;
#251685 = CARTESIAN_POINT ( 'NONE',  ( -22.59066674512261486, 64.25000000001193712, -103.0536116081548101 ) ) ;
#251687 = CARTESIAN_POINT ( 'NONE',  ( 20.94999999999999574, 8.926614585098251453, -142.4716830192231498 ) ) ;
#251686 = TOROIDAL_SURFACE ( 'NONE', #214094, 0.2000000000000000111, 0.1000000000000000056 ) ;
#251688 = CARTESIAN_POINT ( 'NONE',  ( 20.95512820512820795, 8.876151316299273120, -45.70017285912874883 ) ) ;
#251689 = CARTESIAN_POINT ( 'NONE',  ( 21.00000000000000000, 6.258114003436814343, 11.90000000000000036 ) ) ;
#251690 = AXIS2_PLACEMENT_3D ( 'NONE', #110807, #230783, #32605 ) ;
#251691 = EDGE_CURVE ( 'NONE', #159519, #3782, #14427, .T. ) ;
#251692 = CARTESIAN_POINT ( 'NONE',  ( -20.64999999999999858, 68.76258920191057200, -222.5680764032308048 ) ) ;
#251693 = EDGE_CURVE ( 'NONE', #72701, #146536, #149836, .T. ) ;
#251694 = AXIS2_PLACEMENT_3D ( 'NONE', #111046, #147604, #188027 ) ;
#251695 = DIRECTION ( 'NONE',  ( -0.000000000000000000, 0.9126074666063770380, 0.4088369013363281068 ) ) ;
#251696 = DIRECTION ( 'NONE',  ( -1.000000000000000000, -0.000000000000000000, -0.000000000000000000 ) ) ;
#251697 = VECTOR ( 'NONE', #187425, 1000.000000000000000 ) ;
#251698 = TOROIDAL_SURFACE ( 'NONE', #122534, 11.65000000000000036, 0.1000000000000000056 ) ;
#251699 = ORIENTED_EDGE ( 'NONE', *, *, #84568, .F. ) ;
#251700 = DIRECTION ( 'NONE',  ( 0.000000000000000000, 6.982962677686266711E-15, -1.000000000000000000 ) ) ;
#251702 = ORIENTED_EDGE ( 'NONE', *, *, #19022, .F. ) ;
#251701 = CARTESIAN_POINT ( 'NONE',  ( 22.16821283564876666, 68.44102665923161055, -170.0231074845243882 ) ) ;
#251703 = FACE_OUTER_BOUND ( 'NONE', #20992, .T. ) ;
#251704 = PLANE ( 'NONE',  #137880 ) ;
#251705 = EDGE_LOOP ( 'NONE', ( #116561, #206896, #221245, #171629 ) ) ;
#251706 = CARTESIAN_POINT ( 'NONE',  ( -20.94999999999999929, 11.59999999999999609, -6.928203230275558511 ) ) ;
#251707 = CIRCLE ( 'NONE', #214300, 0.09999999999999990841 ) ;
#251708 = APPLICATION_PROTOCOL_DEFINITION ( 'draft international standard', 'automotive_design', 1998, #42461 ) ;
#251709 = VECTOR ( 'NONE', #5765, 1000.000000000000000 ) ;
#251710 = EDGE_CURVE ( 'NONE', #74147, #237782, #51789, .T. ) ;
#251712 = AXIS2_PLACEMENT_3D ( 'NONE', #210731, #89483, #208182 ) ;
#251711 = CARTESIAN_POINT ( 'NONE',  ( 21.14999999999999858, 64.25000000001220712, -148.2731074845243882 ) ) ;
#251713 = LINE ( 'NONE', #71810, #179818 ) ;
#251714 = EDGE_LOOP ( 'NONE', ( #252095, #189981, #155492, #164367 ) ) ;
#251715 = CARTESIAN_POINT ( 'NONE',  ( -18.39999999999999858, -7.883686024897174072, -209.9138933503092233 ) ) ;
#251716 = EDGE_CURVE ( 'NONE', #59486, #166165, #47702, .T. ) ;
#251717 = CIRCLE ( 'NONE', #243334, 0.1000000000000017680 ) ;
#251718 = FACE_OUTER_BOUND ( 'NONE', #166923, .T. ) ;
#251719 = ORIENTED_EDGE ( 'NONE', *, *, #188921, .T. ) ;
#251720 = ORIENTED_EDGE ( 'NONE', *, *, #184609, .F. ) ;
#251721 = EDGE_CURVE ( 'NONE', #251940, #48052, #247630, .T. ) ;
#251722 = VECTOR ( 'NONE', #179702, 1000.000000000000000 ) ;
#251723 = LINE ( 'NONE', #189193, #79770 ) ;
#251724 = VECTOR ( 'NONE', #199549, 1000.000000000000000 ) ;
#251725 = AXIS2_PLACEMENT_3D ( 'NONE', #220952, #21504, #85279 ) ;
#251726 = DIRECTION ( 'NONE',  ( 1.000000000000000000, 0.000000000000000000, 0.000000000000000000 ) ) ;
#251727 = CARTESIAN_POINT ( 'NONE',  ( -23.15000000000000213, 76.00000000001267608, -203.5231074845243597 ) ) ;
#251728 = DIRECTION ( 'NONE',  ( 0.000000000000000000, -0.4721928772777352346, -0.8814952561688428334 ) ) ;
#251730 = LINE ( 'NONE', #250441, #91035 ) ;
#251729 = PLANE ( 'NONE',  #224096 ) ;
#251731 = EDGE_CURVE ( 'NONE', #27052, #220964, #76747, .T. ) ;
#251732 = FACE_OUTER_BOUND ( 'NONE', #19734, .T. ) ;
#251733 = CARTESIAN_POINT ( 'NONE',  ( -16.92925196614875816, 9.972331796421277872, -113.1167448477168307 ) ) ;
#251734 = DIRECTION ( 'NONE',  ( 0.000000000000000000, 0.000000000000000000, -1.000000000000000000 ) ) ;
#251735 = DIRECTION ( 'NONE',  ( -1.000000000000000000, 0.000000000000000000, 0.000000000000000000 ) ) ;
#251736 = ORIENTED_EDGE ( 'NONE', *, *, #227989, .T. ) ;
#251738 = ORIENTED_EDGE ( 'NONE', *, *, #174213, .F. ) ;
#251737 = CARTESIAN_POINT ( 'NONE',  ( -16.89060415895971090, 12.41435804878020832, -211.2386428410039230 ) ) ;
#251739 = CARTESIAN_POINT ( 'NONE',  ( -22.39999999999999858, 11.75000000001115552, -33.40000000000000568 ) ) ;
#251740 = CARTESIAN_POINT ( 'NONE',  ( -21.11927991906891222, -1.363370130417240977, -194.6972729791065149 ) ) ;
#251742 = DIRECTION ( 'NONE',  ( -0.000000000000000000, 0.4721928772777345684, 0.8814952561688429444 ) ) ;
#251741 = FACE_OUTER_BOUND ( 'NONE', #48353, .T. ) ;
#251743 = ORIENTED_EDGE ( 'NONE', *, *, #192345, .T. ) ;
#251744 = DIRECTION ( 'NONE',  ( 1.000000000000000000, 0.000000000000000000, 0.000000000000000000 ) ) ;
#251745 = CARTESIAN_POINT ( 'NONE',  ( -16.87036670365549895, 65.91505003675702312, -157.4731074845244336 ) ) ;
#251746 = EDGE_CURVE ( 'NONE', #6498, #224664, #189194, .T. ) ;
#251747 = CARTESIAN_POINT ( 'NONE',  ( -23.25000000000000000, 77.83585931145570669, -124.9186683157258244 ) ) ;
#251748 = CARTESIAN_POINT ( 'NONE',  ( 14.45963434102923451, 13.16206247923560291, -217.0199023716218676 ) ) ;
#251749 = VERTEX_POINT ( 'NONE', #27348 ) ;
#251750 = ORIENTED_EDGE ( 'NONE', *, *, #159180, .F. ) ;
#251751 = AXIS2_PLACEMENT_3D ( 'NONE', #29884, #109371, #149822 ) ;
#251752 = TOROIDAL_SURFACE ( 'NONE', #60198, 11.65000000000000036, 0.1000000000000000056 ) ;
#251753 = CARTESIAN_POINT ( 'NONE',  ( -21.04999999999994387, 65.19115966511134275, -30.12310748452479103 ) ) ;
#251754 = VERTEX_POINT ( 'NONE', #106823 ) ;
#251755 = CARTESIAN_POINT ( 'NONE',  ( 23.24999999999999645, 22.44569914438688940, -231.9288948874669529 ) ) ;
#251756 = DIRECTION ( 'NONE',  ( 0.000000000000000000, 0.9654727137038715545, -0.2605042016806676242 ) ) ;
#251757 = CARTESIAN_POINT ( 'NONE',  ( 20.94999999999999929, 8.926614585098249677, -142.4716830192231498 ) ) ;
#251758 = AXIS2_PLACEMENT_3D ( 'NONE', #237731, #177781, #240308 ) ;
#251759 = VECTOR ( 'NONE', #180771, 1000.000000000000000 ) ;
#251760 = ORIENTED_EDGE ( 'NONE', *, *, #72508, .F. ) ;
#251761 = DIRECTION ( 'NONE',  ( -1.000000000000000000, -0.000000000000000000, -0.000000000000000000 ) ) ;
#251762 = VECTOR ( 'NONE', #37200, 1000.000000000000000 ) ;
#251763 = CARTESIAN_POINT ( 'NONE',  ( -21.14999999999999858, -0.1008583690987122083, 11.74956712348939192 ) ) ;
#251765 = CIRCLE ( 'NONE', #1764, 0.09999999999999939493 ) ;
#251764 = DIRECTION ( 'NONE',  ( 1.000000000000000000, 0.000000000000000000, 0.000000000000000000 ) ) ;
#251766 = CARTESIAN_POINT ( 'NONE',  ( 21.22070241538126467, 75.90108096947716376, -142.9930537573939091 ) ) ;
#251768 = CIRCLE ( 'NONE', #60222, 0.09999999999999939493 ) ;
#251767 = DIRECTION ( 'NONE',  ( -1.000000000000000000, 0.000000000000000000, 0.000000000000000000 ) ) ;
#251770 = CARTESIAN_POINT ( 'NONE',  ( -20.64999999999999858, 68.85000000001156195, -57.17310748452437252 ) ) ;
#251769 = CARTESIAN_POINT ( 'NONE',  ( -21.65000000000000213, 7.250000000011138646, -146.6500000000000341 ) ) ;
#251771 = CIRCLE ( 'NONE', #130968, 0.09999999999998898659 ) ;
#251772 = CARTESIAN_POINT ( 'NONE',  ( -16.83558968593874994, 66.05000000001224691, -149.1854126721411262 ) ) ;
#251773 = ORIENTED_EDGE ( 'NONE', *, *, #143262, .T. ) ;
#251775 = CARTESIAN_POINT ( 'NONE',  ( -18.40000000000000213, 67.17743825834580207, -145.7731074845244450 ) ) ;
#251774 = LINE ( 'NONE', #250481, #236690 ) ;
#251776 = EDGE_LOOP ( 'NONE', ( #106809, #177192, #110168, #150213 ) ) ;
#251778 = ORIENTED_EDGE ( 'NONE', *, *, #162498, .T. ) ;
#251777 = DIRECTION ( 'NONE',  ( 1.000000000000000000, 0.000000000000000000, -0.000000000000000000 ) ) ;
#251779 = ORIENTED_EDGE ( 'NONE', *, *, #87621, .F. ) ;
#251780 = FACE_OUTER_BOUND ( 'NONE', #126079, .T. ) ;
#251781 = CARTESIAN_POINT ( 'NONE',  ( 18.59117750673696179, 10.33248238083634796, -72.59484654391314962 ) ) ;
#251782 = DIRECTION ( 'NONE',  ( 0.000000000000000000, -0.9915357197604972583, 0.1298341882519109536 ) ) ;
#251783 = CARTESIAN_POINT ( 'NONE',  ( 21.04999999999999716, 65.49746832288708731, -128.9642776674504887 ) ) ;
#251784 = ORIENTED_EDGE ( 'NONE', *, *, #23048, .T. ) ;
#251785 = DIRECTION ( 'NONE',  ( 2.952720810173289112E-16, 0.9651348961777159730, -0.2617529984165024026 ) ) ;
#251787 = LINE ( 'NONE', #232250, #123088 ) ;
#251786 = CIRCLE ( 'NONE', #226839, 0.1000000000000028644 ) ;
#251788 = ORIENTED_EDGE ( 'NONE', *, *, #57099, .T. ) ;
#251789 = CARTESIAN_POINT ( 'NONE',  ( -18.50000000000000711, 11.75000000001115197, -141.0148057706539930 ) ) ;
#251790 = AXIS2_PLACEMENT_3D ( 'NONE', #20063, #141277, #143829 ) ;
#251791 = ADVANCED_FACE ( 'NONE', ( #186394 ), #1905, .F. ) ;
#251792 = DIRECTION ( 'NONE',  ( 0.000000000000000000, -1.000000000000000000, -6.982962677686266711E-15 ) ) ;
#251793 = ORIENTED_EDGE ( 'NONE', *, *, #186327, .T. ) ;
#251794 = CARTESIAN_POINT ( 'NONE',  ( -23.15000000000000213, 6.375212254182287097, -220.8739277186596155 ) ) ;
#251795 = CIRCLE ( 'NONE', #114429, 2.000000000000003109 ) ;
#251796 = VECTOR ( 'NONE', #115929, 1000.000000000000000 ) ;
#251797 = VERTEX_POINT ( 'NONE', #166853 ) ;
#251798 = VECTOR ( 'NONE', #202361, 1000.000000000000000 ) ;
#251799 = CARTESIAN_POINT ( 'NONE',  ( 18.50211644919734866, 65.69792220476318789, -97.53355541284612684 ) ) ;
#251800 = ORIENTED_EDGE ( 'NONE', *, *, #20177, .T. ) ;
#251801 = LINE ( 'NONE', #191865, #59401 ) ;
#251802 = DIRECTION ( 'NONE',  ( -0.000000000000000000, 1.000000000000000000, 6.982962677686266711E-15 ) ) ;
#251803 = CARTESIAN_POINT ( 'NONE',  ( -22.50000000000000000, 76.00000000001271871, -209.7731074845243597 ) ) ;
#251804 = DIRECTION ( 'NONE',  ( 0.000000000000000000, 0.8660254037844420383, -0.4999999999999943379 ) ) ;
#251805 = ADVANCED_FACE ( 'NONE', ( #96244 ), #194099, .F. ) ;
#251806 = LINE ( 'NONE', #213975, #212741 ) ;
#251807 = LINE ( 'NONE', #254353, #252908 ) ;
#251808 = LINE ( 'NONE', #247951, #118110 ) ;
#251809 = VERTEX_POINT ( 'NONE', #33769 ) ;
#251810 = CIRCLE ( 'NONE', #1993, 12.97499999999998721 ) ;
#251811 = CARTESIAN_POINT ( 'NONE',  ( 18.59999999999999432, -1.162701749926853712, -41.50000000000000000 ) ) ;
#251812 = ORIENTED_EDGE ( 'NONE', *, *, #77638, .F. ) ;
#251815 = VERTEX_POINT ( 'NONE', #136653 ) ;
#251814 = DIRECTION ( 'NONE',  ( 0.000000000000000000, 0.000000000000000000, -1.000000000000000000 ) ) ;
#251813 = DIRECTION ( 'NONE',  ( 1.000000000000000000, -0.000000000000000000, -0.000000000000000000 ) ) ;
#251816 = ORIENTED_EDGE ( 'NONE', *, *, #134385, .F. ) ;
#251817 = DIRECTION ( 'NONE',  ( 0.000000000000000000, 0.000000000000000000, -1.000000000000000000 ) ) ;
#251818 = DIRECTION ( 'NONE',  ( 1.020425574104004394E-15, 0.9126074666063770380, 0.4088369013363281068 ) ) ;
#251819 = CARTESIAN_POINT ( 'NONE',  ( -17.29158576265543346, 60.21639215357974706, -222.1229442910193370 ) ) ;
#251820 = ADVANCED_FACE ( 'NONE', ( #233231 ), #114545, .T. ) ;
#251821 = CARTESIAN_POINT ( 'NONE',  ( 20.95561247346651967, 58.99335862822155718, -225.7528268179844417 ) ) ;
#251822 = VECTOR ( 'NONE', #144910, 1000.000000000000000 ) ;
#251823 = ORIENTED_EDGE ( 'NONE', *, *, #193351, .T. ) ;
#251825 = ORIENTED_EDGE ( 'NONE', *, *, #55286, .F. ) ;
#251824 = CARTESIAN_POINT ( 'NONE',  ( 21.14999999999999503, -11.74999999998883560, -103.4000000000000341 ) ) ;
#251826 = ADVANCED_FACE ( 'NONE', ( #98782 ), #55810, .F. ) ;
#251827 = EDGE_CURVE ( 'NONE', #131589, #21663, #122756, .T. ) ;
#251829 = DIRECTION ( 'NONE',  ( 0.000000000000000000, 0.9770955615653551529, 0.2128009952262517601 ) ) ;
#251828 = CARTESIAN_POINT ( 'NONE',  ( 18.49999999999998934, 10.92199707682457088, -220.3694341645321515 ) ) ;
#251831 = ORIENTED_EDGE ( 'NONE', *, *, #115968, .T. ) ;
#251830 = DIRECTION ( 'NONE',  ( 1.000000000000000000, 0.000000000000000000, 0.000000000000000000 ) ) ;
#251832 = VERTEX_POINT ( 'NONE', #35043 ) ;
#251833 = CARTESIAN_POINT ( 'NONE',  ( -22.94999999999999929, -1.467286812112899463, 28.00000000000000000 ) ) ;
#251834 = AXIS2_PLACEMENT_3D ( 'NONE', #177325, #195591, #258061 ) ;
#251835 = FACE_OUTER_BOUND ( 'NONE', #88709, .T. ) ;
#251836 = VERTEX_POINT ( 'NONE', #36305 ) ;
#251837 = EDGE_CURVE ( 'NONE', #6871, #119497, #154978, .T. ) ;
#251838 = ORIENTED_EDGE ( 'NONE', *, *, #31148, .T. ) ;
#251839 = CARTESIAN_POINT ( 'NONE',  ( -18.49513951962167368, -9.437725026666544892, -107.2780725750291850 ) ) ;
#251840 = CARTESIAN_POINT ( 'NONE',  ( -18.59999999999999787, 45.93315328338058379, -256.6017782078560003 ) ) ;
#251841 = ORIENTED_EDGE ( 'NONE', *, *, #168600, .T. ) ;
#251842 = DIRECTION ( 'NONE',  ( 0.000000000000000000, 0.8814952561688444987, -0.4721928772777320149 ) ) ;
#251843 = ADVANCED_FACE ( 'NONE', ( #97505 ), #6190, .T. ) ;
#251844 = VECTOR ( 'NONE', #51712, 1000.000000000000000 ) ;
#251845 = DIRECTION ( 'NONE',  ( -1.000000000000000000, -0.000000000000000000, -0.000000000000000000 ) ) ;
#251846 = VECTOR ( 'NONE', #30735, 1000.000000000000114 ) ;
#251847 = TOROIDAL_SURFACE ( 'NONE', #39518, 12.97499999999999609, 0.1000000000000000056 ) ;
#251848 = ORIENTED_EDGE ( 'NONE', *, *, #79460, .T. ) ;
#251849 = EDGE_LOOP ( 'NONE', ( #43898, #176174, #222475, #156443 ) ) ;
#251850 = CARTESIAN_POINT ( 'NONE',  ( 20.96937028524354929, 18.74928867235112051, -227.9046800076639840 ) ) ;
#251851 = EDGE_LOOP ( 'NONE', ( #109193, #140793, #104829, #246371 ) ) ;
#251852 = DIRECTION ( 'NONE',  ( 1.186688945009010077E-16, 0.9651348961777157509, -0.2617529984165031243 ) ) ;
#251853 = ORIENTED_EDGE ( 'NONE', *, *, #100919, .T. ) ;
#251855 = ORIENTED_EDGE ( 'NONE', *, *, #208146, .T. ) ;
#251854 = LINE ( 'NONE', #216585, #234300 ) ;
#251856 = ORIENTED_EDGE ( 'NONE', *, *, #251561, .F. ) ;
#251857 = CARTESIAN_POINT ( 'NONE',  ( -21.05000000000000071, 76.00000000001213607, -136.5231074845243313 ) ) ;
#251858 = VERTEX_POINT ( 'NONE', #214918 ) ;
#251861 = ORIENTED_EDGE ( 'NONE', *, *, #86158, .F. ) ;
#251860 = ORIENTED_EDGE ( 'NONE', *, *, #258058, .F. ) ;
#251859 = CARTESIAN_POINT ( 'NONE',  ( -16.93583594267724379, 65.99137656495938131, -56.96371664520363964 ) ) ;
#251862 = ORIENTED_EDGE ( 'NONE', *, *, #27763, .T. ) ;
#251863 = CIRCLE ( 'NONE', #247596, 0.1000000000000055844 ) ;
#251864 = AXIS2_PLACEMENT_3D ( 'NONE', #157977, #134493, #99214 ) ;
#251865 = ADVANCED_FACE ( 'NONE', ( #15458 ), #217467, .T. ) ;
#251866 = CARTESIAN_POINT ( 'NONE',  ( -22.39999999999999503, 7.591056067193246548, -199.2444047917219052 ) ) ;
#251868 = EDGE_CURVE ( 'NONE', #69658, #95143, #72881, .T. ) ;
#251867 = VECTOR ( 'NONE', #229320, 1000.000000000000000 ) ;
#251869 = EDGE_LOOP ( 'NONE', ( #235408, #170719, #169955, #192626 ) ) ;
#251870 = LINE ( 'NONE', #155384, #237019 ) ;
#251871 = ORIENTED_EDGE ( 'NONE', *, *, #251423, .T. ) ;
#251872 = CARTESIAN_POINT ( 'NONE',  ( -23.15000000000000213, 74.00000000001229239, -156.7984855617622770 ) ) ;
#251873 = ORIENTED_EDGE ( 'NONE', *, *, #94339, .T. ) ;
#251874 = ADVANCED_FACE ( 'NONE', ( #238330 ), #134089, .T. ) ;
#251875 = EDGE_CURVE ( 'NONE', #255232, #160843, #68751, .T. ) ;
#251876 = VECTOR ( 'NONE', #115778, 1000.000000000000000 ) ;
#251877 = ORIENTED_EDGE ( 'NONE', *, *, #235791, .T. ) ;
#251878 = AXIS2_PLACEMENT_3D ( 'NONE', #66401, #68989, #25996 ) ;
#251879 = CARTESIAN_POINT ( 'NONE',  ( 22.48660254037844197, 64.35000000001194564, -103.0731074845243853 ) ) ;
#251880 = DIRECTION ( 'NONE',  ( 1.000000000000000000, 1.070816960479510500E-16, -0.000000000000000000 ) ) ;
#251881 = VECTOR ( 'NONE', #91473, 1000.000000000000000 ) ;
#251882 = ADVANCED_FACE ( 'NONE', ( #14184 ), #174571, .T. ) ;
#251883 = VERTEX_POINT ( 'NONE', #197914 ) ;
#251885 = ORIENTED_EDGE ( 'NONE', *, *, #257115, .F. ) ;
#251884 = DIRECTION ( 'NONE',  ( 2.694716079187273439E-16, -0.9770955615653316162, -0.2128009952263598958 ) ) ;
#251886 = AXIS2_PLACEMENT_3D ( 'NONE', #118908, #159324, #199734 ) ;
#251888 = EDGE_CURVE ( 'NONE', #242544, #179165, #197732, .T. ) ;
#251887 = CARTESIAN_POINT ( 'NONE',  ( -23.15000000000000213, 68.29137419664525055, -231.9463301769586394 ) ) ;
#251890 = EDGE_CURVE ( 'NONE', #237092, #39976, #93693, .T. ) ;
#251889 = EDGE_CURVE ( 'NONE', #238394, #224002, #43629, .T. ) ;
#251892 = ORIENTED_EDGE ( 'NONE', *, *, #63372, .F. ) ;
#251891 = ORIENTED_EDGE ( 'NONE', *, *, #166119, .F. ) ;
#251893 = ORIENTED_EDGE ( 'NONE', *, *, #214664, .T. ) ;
#251894 = DIRECTION ( 'NONE',  ( 1.734723475976817507E-14, 1.000000000000000000, 6.982962677686266711E-15 ) ) ;
#251895 = ORIENTED_EDGE ( 'NONE', *, *, #59499, .T. ) ;
#251896 = PRESENTATION_LAYER_ASSIGNMENT (  '', '', ( #181189 ) ) ;
#251897 = ORIENTED_EDGE ( 'NONE', *, *, #196253, .F. ) ;
#251898 = CARTESIAN_POINT ( 'NONE',  ( 20.95483826173899899, 18.85359715731150487, -229.9438933533002967 ) ) ;
#251899 = ORIENTED_EDGE ( 'NONE', *, *, #123908, .T. ) ;
#251900 = DIRECTION ( 'NONE',  ( 1.000000000000000000, 0.000000000000000000, 0.000000000000000000 ) ) ;
#251901 = AXIS2_PLACEMENT_3D ( 'NONE', #138921, #181947, #200225 ) ;
#251902 = AXIS2_PLACEMENT_3D ( 'NONE', #123525, #218754, #165215 ) ;
#251903 = DIRECTION ( 'NONE',  ( 0.000000000000000000, -0.9126074666063770380, -0.4088369013363281068 ) ) ;
#251904 = ORIENTED_EDGE ( 'NONE', *, *, #1031, .T. ) ;
#251905 = EDGE_CURVE ( 'NONE', #59419, #62255, #243525, .T. ) ;
#251906 = B_SPLINE_CURVE_WITH_KNOTS ( 'NONE', 3,
 ( #220799, #182978, #78701, #219504, #137400, #98245, #59124, #3018, #158300, #1738 ),
 .UNSPECIFIED., .F., .F.,
 ( 4, 3, 3, 4 ),
 ( -2.000561356211570577E-06, 0.000000000000000000, 1.787822682428561198E-05, 4.206475347089817763E-05 ),
 .UNSPECIFIED. ) ;
#251907 = VERTEX_POINT ( 'NONE', #45269 ) ;
#251908 = LINE ( 'NONE', #148983, #108855 ) ;
#251909 = EDGE_CURVE ( 'NONE', #54640, #167923, #25708, .T. ) ;
#251910 = EDGE_CURVE ( 'NONE', #2694, #181045, #235328, .T. ) ;
#251911 = EDGE_LOOP ( 'NONE', ( #236271, #23553, #137778, #249168, #202451 ) ) ;
#251912 = EDGE_CURVE ( 'NONE', #7751, #158135, #202026, .T. ) ;
#251913 = CARTESIAN_POINT ( 'NONE',  ( -16.94107738177414291, 10.01423928514777373, -154.9500000000000455 ) ) ;
#251914 = ORIENTED_EDGE ( 'NONE', *, *, #206602, .T. ) ;
#251915 = ORIENTED_EDGE ( 'NONE', *, *, #6403, .F. ) ;
#251916 = CARTESIAN_POINT ( 'NONE',  ( -20.54999999999999716, 74.05981308412469843, -182.8522266955776843 ) ) ;
#251919 = EDGE_CURVE ( 'NONE', #13152, #92492, #204327, .T. ) ;
#251918 = EDGE_LOOP ( 'NONE', ( #29319, #43287, #247180 ) ) ;
#251917 = CARTESIAN_POINT ( 'NONE',  ( -21.05000000000000071, 64.25000000001146816, -43.03791325517834565 ) ) ;
#251920 = DIRECTION ( 'NONE',  ( 0.000000000000000000, 0.4088369013363304383, -0.9126074666063759278 ) ) ;
#251921 = CARTESIAN_POINT ( 'NONE',  ( -17.27223548796277441, 31.52452514974837783, -235.0646137750854336 ) ) ;
#251922 = EDGE_CURVE ( 'NONE', #246750, #146046, #160360, .T. ) ;
#251923 = CARTESIAN_POINT ( 'NONE',  ( 20.95132126680579887, 65.51005012986530573, -128.9527829460898545 ) ) ;
#251924 = CARTESIAN_POINT ( 'NONE',  ( -23.25000000000000000, 74.97916330618691916, -207.2871335796180006 ) ) ;
#251925 = FACE_OUTER_BOUND ( 'NONE', #146064, .T. ) ;
#251926 = DIRECTION ( 'NONE',  ( -1.000000000000000000, 0.000000000000000000, 0.000000000000000000 ) ) ;
#251927 = CIRCLE ( 'NONE', #6407, 0.2000000000000057288 ) ;
#251928 = DIRECTION ( 'NONE',  ( -1.000000000000000000, 7.049440681616512959E-16, -1.911869773728117674E-16 ) ) ;
#251929 = DIRECTION ( 'NONE',  ( 2.952720810173289112E-16, -1.000000000000000000, 0.000000000000000000 ) ) ;
#251930 = CARTESIAN_POINT ( 'NONE',  ( 22.59999999999999432, 75.89914163091374633, -181.7726746080137445 ) ) ;
#251931 = VECTOR ( 'NONE', #121019, 999.9999999999998863 ) ;
#251932 = CARTESIAN_POINT ( 'NONE',  ( 22.48508240969612615, 75.95372358549531100, -148.1731182160978619 ) ) ;
#251933 = CARTESIAN_POINT ( 'NONE',  ( 18.49999999999999645, 7.661991824395936845, -241.5144583139544636 ) ) ;
#251934 = CIRCLE ( 'NONE', #189591, 0.09999999999999976963 ) ;
#251935 = ORIENTED_EDGE ( 'NONE', *, *, #238660, .F. ) ;
#251936 = AXIS2_PLACEMENT_3D ( 'NONE', #138591, #120388, #255954 ) ;
#251938 = ORIENTED_EDGE ( 'NONE', *, *, #146312, .T. ) ;
#251937 = ORIENTED_EDGE ( 'NONE', *, *, #246771, .T. ) ;
#251939 = AXIS2_PLACEMENT_3D ( 'NONE', #207422, #124026, #225650 ) ;
#251940 = VERTEX_POINT ( 'NONE', #239628 ) ;
#251941 = CARTESIAN_POINT ( 'NONE',  ( 18.54999999999999716, 61.20755944685601690, -224.6372899806900989 ) ) ;
#251942 =( BOUNDED_CURVE ( )  B_SPLINE_CURVE ( 3, ( #11116, #88046, #110196, #249724 ),
 .UNSPECIFIED., .F., .F. ) 
 B_SPLINE_CURVE_WITH_KNOTS ( ( 4, 4 ),
 ( 0.06456096931748307732, 3.077031684272310219 ),
 .UNSPECIFIED. ) 
 CURVE ( )  GEOMETRIC_REPRESENTATION_ITEM ( )  RATIONAL_B_SPLINE_CURVE ( ( 1.000000000000000000, 0.3763440860215093164, 0.3763440860215093164, 1.000000000000000000 ) ) 
 REPRESENTATION_ITEM ( '' )  );
#251943 = CYLINDRICAL_SURFACE ( 'NONE', #90285, 0.09999999999999939493 ) ;
#251945 = DIRECTION ( 'NONE',  ( -1.000000000000000000, 2.952720810173289112E-16, 2.061873921506763405E-30 ) ) ;
#251944 = CARTESIAN_POINT ( 'NONE',  ( -23.15000000000000213, 76.00000000001192291, -98.87310748452431142 ) ) ;
#251946 = ORIENTED_EDGE ( 'NONE', *, *, #240865, .F. ) ;
#251948 = VERTEX_POINT ( 'NONE', #64824 ) ;
#251947 = CIRCLE ( 'NONE', #106180, 0.09999999999998898659 ) ;
#251949 = PRESENTATION_STYLE_ASSIGNMENT (( #133295 ) ) ;
#251950 = CARTESIAN_POINT ( 'NONE',  ( -18.40000000000000213, 5.650000000011139001, -46.15000000000000568 ) ) ;
#251951 = VECTOR ( 'NONE', #67761, 1000.000000000000000 ) ;
#251952 = CARTESIAN_POINT ( 'NONE',  ( -21.05000000000000071, 14.05000000001115623, -39.01369507076099552 ) ) ;
#251953 = CARTESIAN_POINT ( 'NONE',  ( -18.59999999999999787, 43.26562470876307742, -245.1245614952171081 ) ) ;
#251954 = ORIENTED_EDGE ( 'NONE', *, *, #219203, .T. ) ;
#251955 = EDGE_LOOP ( 'NONE', ( #160064, #67502, #47929 ) ) ;
#251956 = CARTESIAN_POINT ( 'NONE',  ( 23.24999999999999645, 67.23127455305835554, -235.8551265064784559 ) ) ;
#251957 = DIRECTION ( 'NONE',  ( 1.000000000000000000, -0.000000000000000000, 0.000000000000000000 ) ) ;
#251958 = DIRECTION ( 'NONE',  ( 1.000000000000000000, -2.952720810173289112E-16, -2.061873921506763405E-30 ) ) ;
#251960 = ORIENTED_EDGE ( 'NONE', *, *, #182057, .T. ) ;
#251959 = DIRECTION ( 'NONE',  ( 0.000000000000000000, -0.000000000000000000, -1.000000000000000000 ) ) ;
#251961 = CIRCLE ( 'NONE', #143806, 0.09999999999999939493 ) ;
#251962 = CARTESIAN_POINT ( 'NONE',  ( 21.05000000000000071, 69.08367151115869831, -247.5088222940653679 ) ) ;
#251963 = CARTESIAN_POINT ( 'NONE',  ( 18.79999999999999716, 3.461118860469513336, 28.84309995045515507 ) ) ;
#251964 = CARTESIAN_POINT ( 'NONE',  ( 23.14999999999999858, 71.18691588786253988, -124.5815897280005089 ) ) ;
#251965 = VERTEX_POINT ( 'NONE', #41441 ) ;
#251966 = LINE ( 'NONE', #152906, #182067 ) ;
#251967 = CARTESIAN_POINT ( 'NONE',  ( -18.40000000000000213, 11.33174054713631662, -180.1499999999999773 ) ) ;
#251968 = LINE ( 'NONE', #152908, #156857 ) ;
#251969 = EDGE_CURVE ( 'NONE', #816, #194778, #240909, .T. ) ;
#251971 = CARTESIAN_POINT ( 'NONE',  ( -1.820710678118658388, -9.929289321870186313, -91.65000000000004832 ) ) ;
#251970 = CARTESIAN_POINT ( 'NONE',  ( 18.59999999999999076, 69.55000000001179217, -81.77310748452434552 ) ) ;
#251972 = CARTESIAN_POINT ( 'NONE',  ( 23.24999999999999289, 11.65000000001116298, -33.60000000000000142 ) ) ;
#251973 = CYLINDRICAL_SURFACE ( 'NONE', #228960, 0.09999999999998898659 ) ;
#251975 = EDGE_CURVE ( 'NONE', #27724, #34583, #231087, .T. ) ;
#251974 = DIRECTION ( 'NONE',  ( 4.239556034732057360E-17, 0.1298341882519953860, 0.9915357197604862671 ) ) ;
#251976 = CYLINDRICAL_SURFACE ( 'NONE', #39353, 0.09999999999999939493 ) ;
#251978 = EDGE_LOOP ( 'NONE', ( #45988, #170610, #180105, #109248 ) ) ;
#251977 = AXIS2_PLACEMENT_3D ( 'NONE', #194554, #205392, #15917 ) ;
#251979 = AXIS2_PLACEMENT_3D ( 'NONE', #90741, #47759, #152041 ) ;
#251980 = ORIENTED_EDGE ( 'NONE', *, *, #222001, .T. ) ;
#251981 = ADVANCED_FACE ( 'NONE', ( #40166 ), #247818, .T. ) ;
#251982 = CARTESIAN_POINT ( 'NONE',  ( 23.14999999999998437, 71.95000000001238050, -170.0231074845243882 ) ) ;
#251983 = EDGE_CURVE ( 'NONE', #231632, #91302, #89576, .T. ) ;
#251984 = CYLINDRICAL_SURFACE ( 'NONE', #256862, 12.87499999999999822 ) ;
#251985 = ORIENTED_EDGE ( 'NONE', *, *, #102290, .T. ) ;
#251986 = DIRECTION ( 'NONE',  ( 1.000000000000000000, 0.000000000000000000, 0.000000000000000000 ) ) ;
#251987 = ORIENTED_EDGE ( 'NONE', *, *, #97929, .F. ) ;
#251988 =( NAMED_UNIT ( * ) PLANE_ANGLE_UNIT ( ) SI_UNIT ( $, .RADIAN. ) );
#251989 = EDGE_LOOP ( 'NONE', ( #12727, #55811, #29160, #55768 ) ) ;
#251990 = CARTESIAN_POINT ( 'NONE',  ( 21.14999999999999503, 76.00000000001199396, -109.5637644362255543 ) ) ;
#251991 = TOROIDAL_SURFACE ( 'NONE', #43895, 0.2000000000000000111, 0.1000000000000000056 ) ;
#251992 = ORIENTED_EDGE ( 'NONE', *, *, #94403, .F. ) ;
#251993 = EDGE_CURVE ( 'NONE', #13227, #55890, #232886, .T. ) ;
#251994 = CARTESIAN_POINT ( 'NONE',  ( -16.93658211146644987, 30.27501720290998222, -234.7938011734946997 ) ) ;
#251995 = EDGE_CURVE ( 'NONE', #8175, #98180, #118658, .T. ) ;
#251996 = DIRECTION ( 'NONE',  ( 1.000000000000000000, 7.304098846218134667E-16, 5.100424963727256530E-30 ) ) ;
#251997 = DIRECTION ( 'NONE',  ( -2.952720810173289112E-16, 1.000000000000000000, 0.000000000000000000 ) ) ;
#251998 = VECTOR ( 'NONE', #29842, 1000.000000000000114 ) ;
#251999 = DIRECTION ( 'NONE',  ( -7.312726383247846713E-15, 0.1686199900910448357, -0.9856811345164804283 ) ) ;
#252000 = DIRECTION ( 'NONE',  ( 0.000000000000000000, -0.000000000000000000, -1.000000000000000000 ) ) ;
#252001 = ORIENTED_EDGE ( 'NONE', *, *, #152786, .F. ) ;
#252003 = DIRECTION ( 'NONE',  ( 1.000000000000000000, 0.000000000000000000, 0.000000000000000000 ) ) ;
#252002 = DIRECTION ( 'NONE',  ( 0.000000000000000000, -1.000000000000000000, 0.000000000000000000 ) ) ;
#252004 = CARTESIAN_POINT ( 'NONE',  ( 12.29592348164039350, 66.64419340838190919, -120.2320049529782011 ) ) ;
#252005 = DIRECTION ( 'NONE',  ( 0.000000000000000000, 0.2617529984165031243, 0.9651348961777157509 ) ) ;
#252006 = DIRECTION ( 'NONE',  ( 0.000000000000000000, -7.056502275159890832E-15, 1.000000000000000000 ) ) ;
#252007 = EDGE_LOOP ( 'NONE', ( #86624, #3247, #102315, #251606 ) ) ;
#252008 = CARTESIAN_POINT ( 'NONE',  ( -20.65000000000000568, 7.249999999999983125, -12.65000000000000213 ) ) ;
#252009 = EDGE_CURVE ( 'NONE', #184365, #29429, #218563, .T. ) ;
#252010 = VERTEX_POINT ( 'NONE', #222593 ) ;
#252011 = CARTESIAN_POINT ( 'NONE',  ( 18.52928932188133970, 10.27928932189250411, -54.85000000000000142 ) ) ;
#252012 = ADVANCED_FACE ( 'NONE', ( #119686 ), #20590, .F. ) ;
#252013 = ORIENTED_EDGE ( 'NONE', *, *, #97318, .T. ) ;
#252014 = AXIS2_PLACEMENT_3D ( 'NONE', #226192, #162421, #227504 ) ;
#252016 = DIRECTION ( 'NONE',  ( 0.000000000000000000, 0.000000000000000000, 1.000000000000000000 ) ) ;
#252015 = PRESENTATION_LAYER_ASSIGNMENT (  '', '', ( #85560 ) ) ;
#252017 = DIRECTION ( 'NONE',  ( 1.000000000000000000, 0.000000000000000000, 0.000000000000000000 ) ) ;
#252018 = PLANE ( 'NONE',  #24244 ) ;
#252019 = ORIENTED_EDGE ( 'NONE', *, *, #200597, .T. ) ;
#252020 = ORIENTED_EDGE ( 'NONE', *, *, #212451, .T. ) ;
#252021 = ADVANCED_FACE ( 'NONE', ( #180935 ), #2271, .F. ) ;
#252022 = EDGE_CURVE ( 'NONE', #32434, #38825, #76931, .T. ) ;
#252023 = LINE ( 'NONE', #147805, #140153 ) ;
#252024 = DIRECTION ( 'NONE',  ( 0.000000000000000000, 0.000000000000000000, 1.000000000000000000 ) ) ;
#252025 = CARTESIAN_POINT ( 'NONE',  ( 20.94999675878240808, 65.70692517833285251, -164.5644653378303985 ) ) ;
#252026 = CARTESIAN_POINT ( 'NONE',  ( 23.14999999999999503, 64.25000000001219291, -143.5379132551784096 ) ) ;
#252029 = CARTESIAN_POINT ( 'NONE',  ( 21.05000000000000071, 88.41227409416161720, -106.0231074845242176 ) ) ;
#252028 = CIRCLE ( 'NONE', #39857, 0.5000000000000004441 ) ;
#252027 = DIRECTION ( 'NONE',  ( 1.000000000000000000, -0.000000000000000000, -0.000000000000000000 ) ) ;
#252030 = ADVANCED_FACE ( 'NONE', ( #201765 ), #110250, .T. ) ;
#252031 = DIRECTION ( 'NONE',  ( 1.000000000000000000, -0.000000000000000000, 0.000000000000000000 ) ) ;
#252032 = CIRCLE ( 'NONE', #214425, 0.09999999999998898659 ) ;
#252033 = DIRECTION ( 'NONE',  ( -1.000000000000000000, 0.000000000000000000, -0.000000000000000000 ) ) ;
#252034 = LINE ( 'NONE', #229909, #138696 ) ;
#252036 = ORIENTED_EDGE ( 'NONE', *, *, #142428, .F. ) ;
#252035 = CIRCLE ( 'NONE', #198051, 0.1000000000000055844 ) ;
#252037 = LINE ( 'NONE', #73436, #164611 ) ;
#252038 = CIRCLE ( 'NONE', #31322, 0.09999999999999939493 ) ;
#252040 = ORIENTED_EDGE ( 'NONE', *, *, #5033, .F. ) ;
#252039 = CARTESIAN_POINT ( 'NONE',  ( -21.05000000000000071, 76.00000000001210765, -132.5231074845243313 ) ) ;
#252041 = CARTESIAN_POINT ( 'NONE',  ( 18.39999999999997371, 11.47316190337362940, -191.7499999999999716 ) ) ;
#252042 = CYLINDRICAL_SURFACE ( 'NONE', #24094, 0.1999999999999987899 ) ;
#252044 = CARTESIAN_POINT ( 'NONE',  ( 23.14999999999999858, 1.115600667400684642E-11, -134.0000000000000284 ) ) ;
#252043 = LINE ( 'NONE', #10879, #158721 ) ;
#252045 =( BOUNDED_CURVE ( )  B_SPLINE_CURVE ( 3, ( #232352, #191953, #113659, #35450 ),
 .UNSPECIFIED., .F., .T. ) 
 B_SPLINE_CURVE_WITH_KNOTS ( ( 4, 4 ),
 ( 3.141592653589791784, 4.712388980384688786 ),
 .UNSPECIFIED. ) 
 CURVE ( )  GEOMETRIC_REPRESENTATION_ITEM ( )  RATIONAL_B_SPLINE_CURVE ( ( 1.000000000000000000, 0.8047378541243649375, 0.8047378541243649375, 1.000000000000000000 ) ) 
 REPRESENTATION_ITEM ( '' )  );
#252046 = CARTESIAN_POINT ( 'NONE',  ( 21.05000000000000071, 11.75000000001115907, -193.9851942293460070 ) ) ;
#252048 = ORIENTED_EDGE ( 'NONE', *, *, #79439, .T. ) ;
#252047 = DIRECTION ( 'NONE',  ( 0.000000000000000000, 0.000000000000000000, -1.000000000000000000 ) ) ;
#252049 = DIRECTION ( 'NONE',  ( 1.000000000000000000, 0.000000000000000000, 0.000000000000000000 ) ) ;
#252050 = LINE ( 'NONE', #254593, #62161 ) ;
#252051 = EDGE_CURVE ( 'NONE', #202854, #231849, #102641, .T. ) ;
#252052 = DIRECTION ( 'NONE',  ( 1.040834085586049673E-13, 0.7899159663865300551, 0.6132151058540831201 ) ) ;
#252053 = DIRECTION ( 'NONE',  ( 1.000000000000000000, 0.000000000000000000, 0.000000000000000000 ) ) ;
#252054 = CARTESIAN_POINT ( 'NONE',  ( 21.14999999999999858, 11.75000000001116263, -112.6500000000000341 ) ) ;
#252055 = ORIENTED_EDGE ( 'NONE', *, *, #88654, .T. ) ;
#252056 = CARTESIAN_POINT ( 'NONE',  ( 15.74999999999999645, 9.850000000011137402, -117.2500000000000284 ) ) ;
#252057 = VERTEX_POINT ( 'NONE', #12585 ) ;
#252058 = EDGE_CURVE ( 'NONE', #239535, #180828, #31197, .T. ) ;
#252059 = CARTESIAN_POINT ( 'NONE',  ( -16.87242674293850087, 66.05000000001189164, -90.37419773089673924 ) ) ;
#252060 = ORIENTED_EDGE ( 'NONE', *, *, #6762, .F. ) ;
#252061 = FACE_OUTER_BOUND ( 'NONE', #113411, .T. ) ;
#252062 = AXIS2_PLACEMENT_3D ( 'NONE', #2325, #23219, #182277 ) ;
#252063 = VERTEX_POINT ( 'NONE', #246043 ) ;
#252064 = AXIS2_PLACEMENT_3D ( 'NONE', #58496, #37702, #74268 ) ;
#252065 = CARTESIAN_POINT ( 'NONE',  ( -20.85000000000000142, 56.27731819600170837, -227.9967441372480721 ) ) ;
#252066 = CARTESIAN_POINT ( 'NONE',  ( 23.14999999999999858, 1.115600667400684642E-11, -167.5000000000000284 ) ) ;
#252067 = DIRECTION ( 'NONE',  ( -7.304098846218134667E-16, -1.000000000000000000, 0.000000000000000000 ) ) ;
#252068 = VERTEX_POINT ( 'NONE', #189919 ) ;
#252069 = CIRCLE ( 'NONE', #68938, 0.1000000000000013933 ) ;
#252070 = AXIS2_PLACEMENT_3D ( 'NONE', #183471, #25681, #106460 ) ;
#252071 = CARTESIAN_POINT ( 'NONE',  ( -16.82542659449985223, 9.934499891427440943, -12.74463560002616624 ) ) ;
#252072 = FACE_OUTER_BOUND ( 'NONE', #116670, .T. ) ;
#252073 = DIRECTION ( 'NONE',  ( -1.000000000000000000, -0.000000000000000000, -0.000000000000000000 ) ) ;
#252074 = CARTESIAN_POINT ( 'NONE',  ( 22.42357213249528769, 7.476102374361162539, -199.2703749191446434 ) ) ;
#252075 = DIRECTION ( 'NONE',  ( 0.000000000000000000, 1.000000000000000000, -6.308085367188393199E-16 ) ) ;
#252076 = EDGE_LOOP ( 'NONE', ( #2181, #166270, #200178, #131950, #180582 ) ) ;
#252077 = CARTESIAN_POINT ( 'NONE',  ( -16.94107738177414291, 10.01423928514777373, -121.4500000000000313 ) ) ;
#252078 = ORIENTED_EDGE ( 'NONE', *, *, #253546, .F. ) ;
#252080 = ORIENTED_EDGE ( 'NONE', *, *, #155746, .T. ) ;
#252079 = CARTESIAN_POINT ( 'NONE',  ( 21.05995757104869526, 67.22461075529059826, -90.82820236153315818 ) ) ;
#252081 = AXIS2_PLACEMENT_3D ( 'NONE', #180667, #4569, #46267 ) ;
#252082 = ORIENTED_EDGE ( 'NONE', *, *, #60834, .T. ) ;
#252083 = CARTESIAN_POINT ( 'NONE',  ( 22.88900146558018989, 67.29609520889978569, -190.8731074845244109 ) ) ;
#252084 = DIRECTION ( 'NONE',  ( -1.000000000000000000, -0.000000000000000000, -0.000000000000000000 ) ) ;
#252085 = TOROIDAL_SURFACE ( 'NONE', #10673, 11.65000000000000036, 0.1000000000000000056 ) ;
#252086 = FACE_OUTER_BOUND ( 'NONE', #129388, .T. ) ;
#252087 = CARTESIAN_POINT ( 'NONE',  ( 23.14999999999999858, 18.47808476326694915, -239.8121846073901224 ) ) ;
#252088 = ORIENTED_EDGE ( 'NONE', *, *, #61793, .F. ) ;
#252089 = VECTOR ( 'NONE', #60914, 1000.000000000000000 ) ;
#252090 = DIRECTION ( 'NONE',  ( 0.000000000000000000, 0.8660254037844411501, 0.4999999999999956701 ) ) ;
#252091 = CARTESIAN_POINT ( 'NONE',  ( 18.69999999999999929, 11.75000000000000000, 22.10000000000000142 ) ) ;
#252092 = AXIS2_PLACEMENT_3D ( 'NONE', #42395, #120674, #21559 ) ;
#252093 = ORIENTED_EDGE ( 'NONE', *, *, #130354, .T. ) ;
#252095 = ORIENTED_EDGE ( 'NONE', *, *, #105274, .T. ) ;
#252094 = CARTESIAN_POINT ( 'NONE',  ( -20.94999999999999929, 1.835341550224411922, -11.65515129256298010 ) ) ;
#252096 = DIRECTION ( 'NONE',  ( 0.000000000000000000, 0.9126074666063770380, 0.4088369013363281068 ) ) ;
#252097 = DIRECTION ( 'NONE',  ( -0.000000000000000000, -0.9126074666063770380, -0.4088369013363281068 ) ) ;
#252098 = DIRECTION ( 'NONE',  ( -0.000000000000000000, 0.2605042016806385363, 0.9654727137038795481 ) ) ;
#252099 = VERTEX_POINT ( 'NONE', #92093 ) ;
#252100 = ORIENTED_EDGE ( 'NONE', *, *, #176262, .T. ) ;
#252101 = DIRECTION ( 'NONE',  ( 1.073024830501117725E-15, 6.982962677686266711E-15, -1.000000000000000000 ) ) ;
#252102 = CARTESIAN_POINT ( 'NONE',  ( -18.40000000000000213, 64.52683809664902981, -48.57310748452440663 ) ) ;
#252103 = EDGE_LOOP ( 'NONE', ( #147633, #75606, #222291, #103120 ) ) ;
#252104 = FACE_OUTER_BOUND ( 'NONE', #48711, .T. ) ;
#252105 = EDGE_CURVE ( 'NONE', #101102, #198700, #27082, .T. ) ;
#252106 = CARTESIAN_POINT ( 'NONE',  ( -22.50000000000088818, -2.434917201483803861, -189.6066865224547087 ) ) ;
#252107 = CARTESIAN_POINT ( 'NONE',  ( -22.57320508075687115, 31.85509083104287598, -238.8280249686205536 ) ) ;
#252108 = TOROIDAL_SURFACE ( 'NONE', #14821, 0.2000000000000000111, 0.1000000000000000056 ) ;
#252109 = EDGE_CURVE ( 'NONE', #114115, #7849, #248603, .T. ) ;
#252110 = EDGE_CURVE ( 'NONE', #135942, #248011, #30873, .T. ) ;
#252111 = AXIS2_PLACEMENT_3D ( 'NONE', #120702, #119398, #20307 ) ;
#252112 = ORIENTED_EDGE ( 'NONE', *, *, #220705, .T. ) ;
#252113 = CARTESIAN_POINT ( 'NONE',  ( 0.000000000000000000, 1.350000000000000089, 16.60000000000000142 ) ) ;
#252114 = VECTOR ( 'NONE', #123912, 1000.000000000000000 ) ;
#252115 = AXIS2_PLACEMENT_3D ( 'NONE', #155170, #14370, #32666 ) ;
#252116 = VERTEX_POINT ( 'NONE', #71274 ) ;
#252117 = CARTESIAN_POINT ( 'NONE',  ( -16.87242674293849731, 9.950000000011138823, -188.3510902463723369 ) ) ;
#252118 = EDGE_CURVE ( 'NONE', #126149, #70740, #97753, .T. ) ;
#252119 = FACE_OUTER_BOUND ( 'NONE', #84121, .T. ) ;
#252121 = ORIENTED_EDGE ( 'NONE', *, *, #58639, .T. ) ;
#252120 = DIRECTION ( 'NONE',  ( -1.000000000000000000, -0.000000000000000000, -0.000000000000000000 ) ) ;
#252122 = CARTESIAN_POINT ( 'NONE',  ( -17.11825945287482753, 66.05000000001207638, -123.7731074845243739 ) ) ;
#252123 = CARTESIAN_POINT ( 'NONE',  ( -20.64999999999999858, 85.00000000001179501, -79.41707660717668205 ) ) ;
#252124 = CARTESIAN_POINT ( 'NONE',  ( 21.05000000000000071, 77.84908441863859707, -57.86709696307718787 ) ) ;
#252125 = CARTESIAN_POINT ( 'NONE',  ( -20.85000000000000142, 14.83511725869332132, -235.8887435844146978 ) ) ;
#252126 = CARTESIAN_POINT ( 'NONE',  ( 21.09096482362054559, 6.363544365415513937, -33.46055172122586896 ) ) ;
#252127 = CARTESIAN_POINT ( 'NONE',  ( -20.54999999999999716, 2.449293598294709373E-16, -35.50000000000000711 ) ) ;
#252128 = DIRECTION ( 'NONE',  ( 0.000000000000000000, -0.4721928772776434191, -0.8814952561688919053 ) ) ;
#252130 = VERTEX_POINT ( 'NONE', #148219 ) ;
#252129 = CARTESIAN_POINT ( 'NONE',  ( -22.49756042579671700, 75.92195366299485215, -114.6729724456266268 ) ) ;
#252131 = AXIS2_PLACEMENT_3D ( 'NONE', #161600, #62484, #3785 ) ;
#252132 = CARTESIAN_POINT ( 'NONE',  ( -17.01825945287481545, 9.950000000011138823, -121.2500000000000426 ) ) ;
#252133 = EDGE_CURVE ( 'NONE', #187434, #77791, #239441, .T. ) ;
#252134 = ADVANCED_FACE ( 'NONE', ( #50375 ), #129922, .T. ) ;
#252135 = VECTOR ( 'NONE', #45664, 1000.000000000000000 ) ;
#252136 = DIRECTION ( 'NONE',  ( -1.000000000000000000, -0.000000000000000000, -0.000000000000000000 ) ) ;
#252137 = DIRECTION ( 'NONE',  ( 1.000000000000000000, 0.000000000000000000, 0.000000000000000000 ) ) ;
#252138 = ORIENTED_EDGE ( 'NONE', *, *, #235202, .T. ) ;
#252139 = DIRECTION ( 'NONE',  ( 0.000000000000000000, 0.000000000000000000, -1.000000000000000000 ) ) ;
#252140 = CARTESIAN_POINT ( 'NONE',  ( 21.05000000000000071, 1.115600667400684642E-11, -33.60000000000000142 ) ) ;
#252142 = ADVANCED_FACE ( 'NONE', ( #166530 ), #47879, .T. ) ;
#252141 = FACE_OUTER_BOUND ( 'NONE', #183908, .T. ) ;
#252143 = VERTEX_POINT ( 'NONE', #150788 ) ;
#252144 = VECTOR ( 'NONE', #198063, 1000.000000000000000 ) ;
#252145 = CARTESIAN_POINT ( 'NONE',  ( -21.05000000000000071, 6.540656951712397138, -67.10000000000005116 ) ) ;
#252146 = VECTOR ( 'NONE', #107453, 1000.000000000000114 ) ;
#252147 = CARTESIAN_POINT ( 'NONE',  ( -22.00356870141068200, 60.22995210368382146, -233.9563068168642133 ) ) ;
#252148 = VERTEX_POINT ( 'NONE', #111658 ) ;
#252149 = CARTESIAN_POINT ( 'NONE',  ( -16.87036670365548474, 66.01058118070986325, -48.54354736722234520 ) ) ;
#252150 = ORIENTED_EDGE ( 'NONE', *, *, #23772, .T. ) ;
#252152 = ORIENTED_EDGE ( 'NONE', *, *, #151073, .T. ) ;
#252151 = CARTESIAN_POINT ( 'NONE',  ( -20.54999999999999716, 1.115624548013267999E-11, -165.6000000000000227 ) ) ;
#252153 = CARTESIAN_POINT ( 'NONE',  ( 21.00000000000000000, 66.25000000001206502, -124.1731074845243654 ) ) ;
#252154 = ADVANCED_FACE ( 'NONE', ( #32151 ), #102208, .T. ) ;
#252155 = ORIENTED_EDGE ( 'NONE', *, *, #77184, .F. ) ;
#252156 = CARTESIAN_POINT ( 'NONE',  ( -18.59999999999999787, 5.950000000011100632, -144.3057023050348846 ) ) ;
#252157 = ORIENTED_EDGE ( 'NONE', *, *, #158296, .T. ) ;
#252159 = ORIENTED_EDGE ( 'NONE', *, *, #178084, .T. ) ;
#252158 = ORIENTED_EDGE ( 'NONE', *, *, #48714, .T. ) ;
#252160 = LINE ( 'NONE', #232639, #52921 ) ;
#252162 = EDGE_LOOP ( 'NONE', ( #238402, #238445, #84296, #255516 ) ) ;
#252161 = DIRECTION ( 'NONE',  ( 0.000000000000000000, 0.000000000000000000, 1.000000000000000000 ) ) ;
#252163 = CARTESIAN_POINT ( 'NONE',  ( 20.93975676684922504, 65.68895814178220860, -64.00265578621380769 ) ) ;
#252164 = VECTOR ( 'NONE', #94164, 1000.000000000000000 ) ;
#252165 = ORIENTED_EDGE ( 'NONE', *, *, #194834, .F. ) ;
#252166 = EDGE_CURVE ( 'NONE', #231732, #54600, #85450, .T. ) ;
#252167 = CIRCLE ( 'NONE', #139736, 5.000000000000003553 ) ;
#252168 = ADVANCED_FACE ( 'NONE', ( #128671 ), #247987, .T. ) ;
#252169 = ORIENTED_EDGE ( 'NONE', *, *, #254840, .T. ) ;
#252170 = CARTESIAN_POINT ( 'NONE',  ( 18.59999999999999076, 19.00443933019177223, -232.7770257915295531 ) ) ;
#252171 = CARTESIAN_POINT ( 'NONE',  ( 21.07928932188134397, 75.90110485435729970, -75.85162414091763594 ) ) ;
#252172 = DIRECTION ( 'NONE',  ( 1.000000000000000000, 0.000000000000000000, 0.000000000000000000 ) ) ;
#252173 = ORIENTED_EDGE ( 'NONE', *, *, #107874, .T. ) ;
#252174 = EDGE_CURVE ( 'NONE', #213246, #248567, #222858, .T. ) ;
#252176 = ADVANCED_FACE ( 'NONE', ( #167815 ), #109082, .T. ) ;
#252175 = DIRECTION ( 'NONE',  ( 0.000000000000000000, 0.000000000000000000, -1.000000000000000000 ) ) ;
#252177 = DIRECTION ( 'NONE',  ( 0.000000000000000000, -0.1350103645451876666, 0.9908441862701600211 ) ) ;
#252178 = DIRECTION ( 'NONE',  ( -1.000000000000000000, 0.000000000000000000, 0.000000000000000000 ) ) ;
#252179 = EDGE_LOOP ( 'NONE', ( #70961, #40243, #113746, #41281 ) ) ;
#252180 = LINE ( 'NONE', #133530, #75264 ) ;
#252181 = DIRECTION ( 'NONE',  ( 1.000000000000000000, -0.000000000000000000, -0.000000000000000000 ) ) ;
#252182 = VERTEX_POINT ( 'NONE', #89515 ) ;
#252183 = DIRECTION ( 'NONE',  ( 1.000000000000000000, 3.854941057726231589E-15, 0.000000000000000000 ) ) ;
#252184 = ORIENTED_EDGE ( 'NONE', *, *, #57736, .T. ) ;
#252185 = ORIENTED_EDGE ( 'NONE', *, *, #183844, .T. ) ;
#252186 = EDGE_CURVE ( 'NONE', #81824, #157545, #135557, .T. ) ;
#252187 = VECTOR ( 'NONE', #92303, 1000.000000000000000 ) ;
#252188 = EDGE_CURVE ( 'NONE', #201418, #195545, #172962, .T. ) ;
#252189 = LINE ( 'NONE', #69733, #122214 ) ;
#252190 = VERTEX_POINT ( 'NONE', #97182 ) ;
#252191 = ORIENTED_EDGE ( 'NONE', *, *, #111242, .T. ) ;
#252192 = CARTESIAN_POINT ( 'NONE',  ( -21.00000000000000000, 11.49641995933507843, -1.885425182446133885 ) ) ;
#252193 = CARTESIAN_POINT ( 'NONE',  ( -18.59999999999999787, -9.399999999988787991, -40.79725975966329088 ) ) ;
#252194 = VERTEX_POINT ( 'NONE', #137619 ) ;
#252195 = EDGE_CURVE ( 'NONE', #4633, #21708, #52958, .T. ) ;
#252196 = ORIENTED_EDGE ( 'NONE', *, *, #252271, .F. ) ;
#252197 = SPHERICAL_SURFACE ( 'NONE', #122913, 0.1000000000000000056 ) ;
#252198 = CARTESIAN_POINT ( 'NONE',  ( 23.14999999999999858, 70.40000000001187175, -90.61784146561124942 ) ) ;
#252199 = VERTEX_POINT ( 'NONE', #176790 ) ;
#252200 = EDGE_CURVE ( 'NONE', #54519, #73858, #27274, .T. ) ;
#252201 = AXIS2_PLACEMENT_3D ( 'NONE', #41851, #203475, #106920 ) ;
#252202 = CIRCLE ( 'NONE', #18971, 2.100000000000002309 ) ;
#252203 = ADVANCED_FACE ( 'NONE', ( #15138 ), #217155, .F. ) ;
#252204 = EDGE_CURVE ( 'NONE', #178668, #2919, #197912, .T. ) ;
#252205 = ORIENTED_EDGE ( 'NONE', *, *, #200979, .T. ) ;
#252206 = AXIS2_PLACEMENT_3D ( 'NONE', #161788, #62673, #142193 ) ;
#252207 = CARTESIAN_POINT ( 'NONE',  ( 22.39999999999999503, 7.790779598384535376, -33.39999999999999858 ) ) ;
#252208 =( GEOMETRIC_REPRESENTATION_CONTEXT ( 3 ) GLOBAL_UNCERTAINTY_ASSIGNED_CONTEXT ( ( #71247 ) ) GLOBAL_UNIT_ASSIGNED_CONTEXT ( ( #148376, #209630, #87093 ) ) REPRESENTATION_CONTEXT ( 'NONE', 'WORKASPACE' ) );
#252209 = EDGE_CURVE ( 'NONE', #231732, #114424, #143748, .T. ) ;
#252210 = DIRECTION ( 'NONE',  ( 0.000000000000000000, -0.9424537609900501822, -0.3343365196859436339 ) ) ;
#252211 = DIRECTION ( 'NONE',  ( 0.000000000000000000, 1.776356839400250465E-15, -1.000000000000000000 ) ) ;
#252213 = EDGE_LOOP ( 'NONE', ( #214658, #59880, #52816, #37344 ) ) ;
#252212 = CYLINDRICAL_SURFACE ( 'NONE', #64197, 0.5000000000000004441 ) ;
#252214 = ADVANCED_FACE ( 'NONE', ( #55498 ), #171672, .T. ) ;
#252215 = CARTESIAN_POINT ( 'NONE',  ( 18.59999999999999432, 28.08990005499213538, -254.8141779806076670 ) ) ;
#252216 = FACE_OUTER_BOUND ( 'NONE', #227754, .T. ) ;
#252217 = ADVANCED_FACE ( 'NONE', ( #116794 ), #148038, .F. ) ;
#252218 = CARTESIAN_POINT ( 'NONE',  ( 18.49999999999999289, 65.50857864377465489, -111.6731074845243796 ) ) ;
#252220 = CARTESIAN_POINT ( 'NONE',  ( -21.14999999999994174, 76.00000000001119815, -31.97310748452479601 ) ) ;
#252219 = CARTESIAN_POINT ( 'NONE',  ( -21.05000000000000071, 87.65000000001195701, -103.0231074845242318 ) ) ;
#252221 = CARTESIAN_POINT ( 'NONE',  ( 18.49999999999999289, 69.55000000001173532, -81.27310748452437394 ) ) ;
#252223 = EDGE_CURVE ( 'NONE', #135464, #13472, #81363, .T. ) ;
#252222 = CARTESIAN_POINT ( 'NONE',  ( 23.14999999999999858, 1.115600667400684642E-11, -200.9999999999999432 ) ) ;
#252224 = CARTESIAN_POINT ( 'NONE',  ( 21.00000000000000000, 9.750000000011153745, -121.7500000000000426 ) ) ;
#252225 = DIRECTION ( 'NONE',  ( 1.000000000000000000, 0.000000000000000000, 0.000000000000000000 ) ) ;
#252226 = AXIS2_PLACEMENT_3D ( 'NONE', #92145, #39905, #198940 ) ;
#252227 = VERTEX_POINT ( 'NONE', #197603 ) ;
#252228 =( GEOMETRIC_REPRESENTATION_CONTEXT ( 3 ) GLOBAL_UNCERTAINTY_ASSIGNED_CONTEXT ( ( #26992 ) ) GLOBAL_UNIT_ASSIGNED_CONTEXT ( ( #34825, #253825, #37381 ) ) REPRESENTATION_CONTEXT ( 'NONE', 'WORKASPACE' ) );
#252229 = CIRCLE ( 'NONE', #110592, 11.74999999999999645 ) ;
#252230 = VERTEX_POINT ( 'NONE', #153400 ) ;
#252231 = TOROIDAL_SURFACE ( 'NONE', #156433, 0.6000000000000015321, 0.1000000000000000056 ) ;
#252232 = EDGE_CURVE ( 'NONE', #58239, #253517, #206308, .T. ) ;
#252233 = DIRECTION ( 'NONE',  ( -0.000000000000000000, -1.000000000000000000, -6.982962677686266711E-15 ) ) ;
#252234 = AXIS2_PLACEMENT_3D ( 'NONE', #219064, #41751, #102965 ) ;
#252235 = AXIS2_PLACEMENT_3D ( 'NONE', #40500, #41769, #162995 ) ;
#252236 = AXIS2_PLACEMENT_3D ( 'NONE', #188086, #9439, #74594 ) ;
#252237 = DIRECTION ( 'NONE',  ( 0.000000000000000000, 0.000000000000000000, -1.000000000000000000 ) ) ;
#252238 = ORIENTED_EDGE ( 'NONE', *, *, #15574, .F. ) ;
#252239 = SHAPE_REPRESENTATION_RELATIONSHIP ( 'NONE' , 'NONE' ,  #1804, #1633 ) ;
#252240 = CARTESIAN_POINT ( 'NONE',  ( -16.89146115310545682, 63.08560170894831032, -213.1225895282340730 ) ) ;
#252241 = DIRECTION ( 'NONE',  ( 0.000000000000000000, -0.5273008465188072647, 0.8496786552930167824 ) ) ;
#252242 = ORIENTED_EDGE ( 'NONE', *, *, #63068, .T. ) ;
#252243 = ORIENTED_EDGE ( 'NONE', *, *, #171338, .F. ) ;
#252245 = CARTESIAN_POINT ( 'NONE',  ( 21.07189867249812210, 60.07686761660588814, -221.2611677080064965 ) ) ;
#252244 = AXIS2_PLACEMENT_3D ( 'NONE', #68769, #227831, #4908 ) ;
#252246 = DIRECTION ( 'NONE',  ( 1.000000000000000000, 0.000000000000000000, 0.000000000000000000 ) ) ;
#252247 = DIRECTION ( 'NONE',  ( 0.000000000000000000, 1.000000000000000000, 0.000000000000000000 ) ) ;
#252249 = EDGE_LOOP ( 'NONE', ( #139459, #255671 ) ) ;
#252248 = CARTESIAN_POINT ( 'NONE',  ( 23.14999999999999858, 1.115600667400684642E-11, -102.5000000000000426 ) ) ;
#252250 = CARTESIAN_POINT ( 'NONE',  ( -20.94999999999999929, 64.30000000001250271, -176.7781056340430723 ) ) ;
#252251 = TOROIDAL_SURFACE ( 'NONE', #98120, 0.2000000000000000111, 0.1000000000000000056 ) ;
#252252 = AXIS2_PLACEMENT_3D ( 'NONE', #130473, #170947, #52210 ) ;
#252254 = VERTEX_POINT ( 'NONE', #75133 ) ;
#252253 = DIRECTION ( 'NONE',  ( -2.557131231893037478E-16, -0.8660254037844420383, 0.4999999999999941713 ) ) ;
#252255 = DIRECTION ( 'NONE',  ( 1.000000000000000000, 0.000000000000000000, 0.000000000000000000 ) ) ;
#252256 = CARTESIAN_POINT ( 'NONE',  ( 21.05000000000000071, 28.67750504931771616, -258.3094128005139396 ) ) ;
#252257 = LINE ( 'NONE', #253540, #132376 ) ;
#252258 = CARTESIAN_POINT ( 'NONE',  ( -22.48970261584618058, 55.97295988302631997, -232.8591431001882484 ) ) ;
#252259 = EDGE_CURVE ( 'NONE', #49667, #124745, #64640, .T. ) ;
#252261 = CARTESIAN_POINT ( 'NONE',  ( 20.21567752745019320, 10.19811410124265905, -108.3826203476516810 ) ) ;
#252260 = CARTESIAN_POINT ( 'NONE',  ( 18.59999999999999076, 6.649999999999999467, -21.25000000000000000 ) ) ;
#252262 = DIRECTION ( 'NONE',  ( 0.000000000000000000, -0.5859227990963362664, -0.8103668758649469339 ) ) ;
#252263 = FACE_OUTER_BOUND ( 'NONE', #192347, .T. ) ;
#252264 = ADVANCED_FACE ( 'NONE', ( #58079 ), #196322, .F. ) ;
#252265 = DIRECTION ( 'NONE',  ( 0.000000000000000000, 0.000000000000000000, 1.000000000000000000 ) ) ;
#252266 = CARTESIAN_POINT ( 'NONE',  ( -21.64999999999999858, 66.65000000001153069, -48.67310748452439384 ) ) ;
#252267 = ORIENTED_EDGE ( 'NONE', *, *, #184730, .T. ) ;
#252268 = PLANE ( 'NONE',  #26507 ) ;
#252269 = ORIENTED_EDGE ( 'NONE', *, *, #18531, .F. ) ;
#252270 = VERTEX_POINT ( 'NONE', #13852 ) ;
#252271 = EDGE_CURVE ( 'NONE', #13858, #66849, #937, .T. ) ;
#252272 = CARTESIAN_POINT ( 'NONE',  ( 18.60000000000000142, -9.399999999999938183, -7.297259759663296208 ) ) ;
#252273 = EDGE_CURVE ( 'NONE', #37616, #162687, #210421, .T. ) ;
#252274 = DIRECTION ( 'NONE',  ( 0.000000000000000000, 0.000000000000000000, -1.000000000000000000 ) ) ;
#252275 = CIRCLE ( 'NONE', #69167, 0.1999999999999935163 ) ;
#252276 = VERTEX_POINT ( 'NONE', #198895 ) ;
#252277 = LINE ( 'NONE', #31987, #181984 ) ;
#252278 = SURFACE_STYLE_USAGE ( .BOTH. , #47652 ) ;
#252279 = CIRCLE ( 'NONE', #139856, 0.09999999999998898659 ) ;
#252280 = VECTOR ( 'NONE', #78940, 1000.000000000000000 ) ;
#252281 = ORIENTED_EDGE ( 'NONE', *, *, #155308, .T. ) ;
#252282 = VERTEX_POINT ( 'NONE', #41137 ) ;
#252283 = AXIS2_PLACEMENT_3D ( 'NONE', #155049, #55883, #214980 ) ;
#252284 = CARTESIAN_POINT ( 'NONE',  ( -16.77779411503079032, 66.05389855308744984, -56.86005006690456298 ) ) ;
#252285 = CARTESIAN_POINT ( 'NONE',  ( -22.50000000000000000, 1.148907358139439339E-11, -201.0000000000015064 ) ) ;
#252286 = CARTESIAN_POINT ( 'NONE',  ( 18.59999999999999076, 29.00069016757795026, -237.9048565010683376 ) ) ;
#252287 = CARTESIAN_POINT ( 'NONE',  ( 12.29592348164039350, 9.355806591630123847, -16.29110253154616217 ) ) ;
#252289 = CARTESIAN_POINT ( 'NONE',  ( -18.59999999999999787, 31.44980407958351165, -233.5445995079518866 ) ) ;
#252288 = DIRECTION ( 'NONE',  ( 1.000000000000000000, 0.000000000000000000, 0.000000000000000000 ) ) ;
#252290 = CARTESIAN_POINT ( 'NONE',  ( -12.93407622233967658, 9.417789466963357725, -82.35738454397692010 ) ) ;
#252292 = EDGE_LOOP ( 'NONE', ( #89636, #156754, #183335, #240357 ) ) ;
#252291 = CARTESIAN_POINT ( 'NONE',  ( -18.59999999999999787, 46.54514716347711101, -243.1111603596801842 ) ) ;
#252294 = CARTESIAN_POINT ( 'NONE',  ( -21.95218792049439216, 65.25068255281803431, -242.7796317678790956 ) ) ;
#252293 = DIRECTION ( 'NONE',  ( 1.000000000000000000, 0.000000000000000000, 0.000000000000000000 ) ) ;
#252295 = DIRECTION ( 'NONE',  ( 0.000000000000000000, 0.9126074666063769270, 0.4088369013363280513 ) ) ;
#252296 = AXIS2_PLACEMENT_3D ( 'NONE', #168593, #29071, #211526 ) ;
#252297 = VERTEX_POINT ( 'NONE', #4537 ) ;
#252298 = CARTESIAN_POINT ( 'NONE',  ( -18.46946985241279648, -9.509317228700149727, -174.4866625654999552 ) ) ;
#252299 = TOROIDAL_SURFACE ( 'NONE', #102249, 0.4000000000000010214, 0.1000000000000000056 ) ;
#252300 = CARTESIAN_POINT ( 'NONE',  ( 21.07964655665547227, 8.774889614989714204, -146.2219165829640701 ) ) ;
#252301 = DIRECTION ( 'NONE',  ( 1.000000000000000000, 0.000000000000000000, 0.000000000000000000 ) ) ;
#252302 = ORIENTED_EDGE ( 'NONE', *, *, #244028, .F. ) ;
#252303 = CIRCLE ( 'NONE', #98164, 0.09999999999999971412 ) ;
#252304 = LINE ( 'NONE', #88081, #91381 ) ;
#252305 = CARTESIAN_POINT ( 'NONE',  ( -23.15000000000000213, 76.00000000001188027, -99.02310748452428868 ) ) ;
#252306 = EDGE_CURVE ( 'NONE', #178773, #126698, #80198, .T. ) ;
#252307 = CARTESIAN_POINT ( 'NONE',  ( 12.25000000000000000, 66.65000000001185754, -86.27310748452437394 ) ) ;
#252308 = EDGE_LOOP ( 'NONE', ( #9520, #189664, #4783, #94606 ) ) ;
#252309 = ORIENTED_EDGE ( 'NONE', *, *, #142662, .T. ) ;
#252310 = CARTESIAN_POINT ( 'NONE',  ( 21.14999999999999858, 42.98415524044398950, -233.9519173640447889 ) ) ;
#252311 = DIRECTION ( 'NONE',  ( 0.000000000000000000, -0.5469332180710735347, 0.8371762388950247935 ) ) ;
#252312 = CIRCLE ( 'NONE', #198160, 12.87499999999999822 ) ;
#252313 = LINE ( 'NONE', #209346, #36562 ) ;
#252314 = CARTESIAN_POINT ( 'NONE',  ( 18.39999999999998082, 64.52683809664983983, -160.7731074845244450 ) ) ;
#252315 = VERTEX_POINT ( 'NONE', #241871 ) ;
#252316 = EDGE_CURVE ( 'NONE', #85287, #212843, #181385, .T. ) ;
#252317 = CARTESIAN_POINT ( 'NONE',  ( 13.12220780326571834, 46.70395665056641832, -234.7173882531050140 ) ) ;
#252318 = DIRECTION ( 'NONE',  ( 1.000000000000000000, 0.000000000000000000, 0.000000000000000000 ) ) ;
#252319 = ADVANCED_FACE ( 'NONE', ( #665 ), #119374, .F. ) ;
#252320 = CARTESIAN_POINT ( 'NONE',  ( 21.40925344232282868, 0.09895018863080314031, -127.3414811406095595 ) ) ;
#252321 = CARTESIAN_POINT ( 'NONE',  ( 20.94999999999999929, 18.81732247075047937, -230.0377732242114632 ) ) ;
#252322 = CIRCLE ( 'NONE', #164868, 0.1000000000000024342 ) ;
#252323 = AXIS2_PLACEMENT_3D ( 'NONE', #229198, #113094, #192636 ) ;
#252324 = CIRCLE ( 'NONE', #164871, 0.1000000000000124678 ) ;
#252325 = TOROIDAL_SURFACE ( 'NONE', #248257, 0.2000000000000000111, 0.1000000000000000056 ) ;
#252326 = DIRECTION ( 'NONE',  ( 0.000000000000000000, -6.938893903907222067E-15, 1.000000000000000000 ) ) ;
#252327 = ADVANCED_FACE ( 'NONE', ( #59348 ), #118837, .T. ) ;
#252329 = VERTEX_POINT ( 'NONE', #223579 ) ;
#252328 = CARTESIAN_POINT ( 'NONE',  ( -18.50000000000000000, 1.115600667400684642E-11, -134.0000000000000000 ) ) ;
#252330 = FACE_OUTER_BOUND ( 'NONE', #76108, .T. ) ;
#252331 = FACE_OUTER_BOUND ( 'NONE', #191880, .T. ) ;
#252332 = CARTESIAN_POINT ( 'NONE',  ( -23.25000000000000000, 77.73670573947892137, -24.50568489690058627 ) ) ;
#252333 = CARTESIAN_POINT ( 'NONE',  ( -23.15000000000000213, 74.00000000001186606, -89.79848556176222019 ) ) ;
#252334 = DIRECTION ( 'NONE',  ( 1.000000000000000000, 0.000000000000000000, 0.000000000000000000 ) ) ;
#252335 = ADVANCED_FACE ( 'NONE', ( #219736 ), #43684, .T. ) ;
#252337 = VERTEX_POINT ( 'NONE', #138883 ) ;
#252336 = CARTESIAN_POINT ( 'NONE',  ( -20.64999999999999858, 68.75000000001179501, -81.87310748452436826 ) ) ;
#252338 = DIRECTION ( 'NONE',  ( 0.000000000000000000, 0.000000000000000000, 1.000000000000000000 ) ) ;
#252339 = EDGE_CURVE ( 'NONE', #225348, #148199, #56448, .T. ) ;
#252340 = CARTESIAN_POINT ( 'NONE',  ( -18.37160782347004329, 11.47561641480238492, -9.250000000000001776 ) ) ;
#252341 = EDGE_LOOP ( 'NONE', ( #12118, #13636, #162768, #225626 ) ) ;
#252342 = DIRECTION ( 'NONE',  ( 2.952720810173289112E-16, -1.000000000000000000, 0.000000000000000000 ) ) ;
#252343 = CARTESIAN_POINT ( 'NONE',  ( -21.05000000000000071, 77.16270174995010223, -128.5231074845242745 ) ) ;
#252344 = DIRECTION ( 'NONE',  ( 1.000000000000000000, 0.000000000000000000, 0.000000000000000000 ) ) ;
#252345 = DIRECTION ( 'NONE',  ( 1.000000000000000000, 0.000000000000000000, 0.000000000000000000 ) ) ;
#252346 = EDGE_CURVE ( 'NONE', #67694, #76270, #48076, .T. ) ;
#252347 = AXIS2_PLACEMENT_3D ( 'NONE', #109587, #71782, #70512 ) ;
#252348 = AXIS2_PLACEMENT_3D ( 'NONE', #75901, #53765, #36810 ) ;
#252349 = DIRECTION ( 'NONE',  ( 1.000000000000000000, -0.000000000000000000, -0.000000000000000000 ) ) ;
#252350 = DIRECTION ( 'NONE',  ( 1.000000000000000000, 0.000000000000000000, 0.000000000000000000 ) ) ;
#252351 = ORIENTED_EDGE ( 'NONE', *, *, #204163, .T. ) ;
#252352 = EDGE_LOOP ( 'NONE', ( #95330, #199347, #194449, #92530 ) ) ;
#252353 = AXIS2_PLACEMENT_3D ( 'NONE', #56727, #22809, #237963 ) ;
#252354 = CARTESIAN_POINT ( 'NONE',  ( -16.95709691156489995, 66.05000000001200533, -115.6831650470344357 ) ) ;
#252355 = ADVANCED_FACE ( 'NONE', ( #22860 ), #102328, .T. ) ;
#252356 = CARTESIAN_POINT ( 'NONE',  ( -21.17356465864818205, 6.422803126252873973, -133.9010887589861625 ) ) ;
#252357 = CARTESIAN_POINT ( 'NONE',  ( 23.50000000000005684, 77.36076146337680370, -43.99645795275012006 ) ) ;
#252358 = PLANE ( 'NONE',  #50701 ) ;
#252359 = CARTESIAN_POINT ( 'NONE',  ( -22.94999999999999929, 1.786320531569725478, -11.50977166988710820 ) ) ;
#252360 = DIRECTION ( 'NONE',  ( 0.000000000000000000, 0.000000000000000000, -1.000000000000000000 ) ) ;
#252361 = AXIS2_PLACEMENT_3D ( 'NONE', #3006, #222041, #82527 ) ;
#252362 = ORIENTED_EDGE ( 'NONE', *, *, #8157, .F. ) ;
#252363 = CYLINDRICAL_SURFACE ( 'NONE', #11214, 0.1000000000000055844 ) ;
#252364 = ORIENTED_EDGE ( 'NONE', *, *, #212339, .T. ) ;
#252365 = FACE_OUTER_BOUND ( 'NONE', #172174, .T. ) ;
#252366 = DIRECTION ( 'NONE',  ( -0.7071067811865302533, 0.6909108974501196876, 0.1504730267679053324 ) ) ;
#252368 = ORIENTED_EDGE ( 'NONE', *, *, #102265, .F. ) ;
#252367 = DIRECTION ( 'NONE',  ( 0.000000000000000000, 0.000000000000000000, 1.000000000000000000 ) ) ;
#252369 = B_SPLINE_CURVE_WITH_KNOTS ( 'NONE', 3,
 ( #156464, #16926, #57298, #74358, #191733, #234678, #235948, #76874, #73078, #135560, #172188, #173480, #153911, #176013, #195571, #117302 ),
 .UNSPECIFIED., .F., .F.,
 ( 4, 3, 3, 3, 3, 4 ),
 ( 0.000000000000000000, 2.209075297430740031E-05, 5.594258369009624354E-05, 8.979524372342012487E-05, 0.0001236472815274586301, 0.0001574990747609554737 ),
 .UNSPECIFIED. ) ;
#252370 = CARTESIAN_POINT ( 'NONE',  ( 20.04142135623730070, 64.35000000001221565, -148.2731074845243882 ) ) ;
#252371 = CARTESIAN_POINT ( 'NONE',  ( -20.64999999999999858, 11.60058429089262333, -246.3380203656811887 ) ) ;
#252372 = LINE ( 'NONE', #253661, #241249 ) ;
#252373 = CARTESIAN_POINT ( 'NONE',  ( 18.59999999999999787, 74.13328508995527955, -191.7704322382423641 ) ) ;
#252374 = ORIENTED_EDGE ( 'NONE', *, *, #255791, .T. ) ;
#252375 = LINE ( 'NONE', #56724, #178919 ) ;
#252376 = DIRECTION ( 'NONE',  ( 0.000000000000000000, 0.000000000000000000, -1.000000000000000000 ) ) ;
#252377 = FACE_OUTER_BOUND ( 'NONE', #190164, .T. ) ;
#252378 = SPHERICAL_SURFACE ( 'NONE', #193545, 0.1000000000000000056 ) ;
#252379 = AXIS2_PLACEMENT_3D ( 'NONE', #125373, #221866, #64111 ) ;
#252380 = CARTESIAN_POINT ( 'NONE',  ( 18.49999999999999289, 69.15387683765983695, -166.2853812176745691 ) ) ;
#252381 = AXIS2_PLACEMENT_3D ( 'NONE', #139098, #221223, #236956 ) ;
#252382 = AXIS2_PLACEMENT_3D ( 'NONE', #21950, #242257, #162751 ) ;
#252383 = ADVANCED_FACE ( 'NONE', ( #158515 ), #39929, .F. ) ;
#252384 = ORIENTED_EDGE ( 'NONE', *, *, #25772, .F. ) ;
#252385 = DIRECTION ( 'NONE',  ( 0.000000000000000000, 0.000000000000000000, -1.000000000000000000 ) ) ;
#252386 = DIRECTION ( 'NONE',  ( 0.000000000000000000, 0.000000000000000000, -1.000000000000000000 ) ) ;
#252387 = ORIENTED_EDGE ( 'NONE', *, *, #12381, .F. ) ;
#252388 = EDGE_CURVE ( 'NONE', #243103, #4098, #124508, .T. ) ;
#252389 = ORIENTED_EDGE ( 'NONE', *, *, #116300, .F. ) ;
#252390 = CARTESIAN_POINT ( 'NONE',  ( 22.49999999999999645, 55.96169194136206215, -232.9023299069559130 ) ) ;
#252391 = CARTESIAN_POINT ( 'NONE',  ( 20.93284271247462414, 36.02367271998545561, -235.8812521208699309 ) ) ;
#252392 = ADVANCED_FACE ( 'NONE', ( #142757 ), #97937, .F. ) ;
#252393 = ORIENTED_EDGE ( 'NONE', *, *, #126606, .F. ) ;
#252395 = EDGE_CURVE ( 'NONE', #88477, #187198, #196792, .T. ) ;
#252394 = CARTESIAN_POINT ( 'NONE',  ( -18.59999999999999787, 68.97833521811179480, -99.28954208262706516 ) ) ;
#252396 = CARTESIAN_POINT ( 'NONE',  ( -20.64999999999999858, -9.499999999988846255, -90.60603087734760663 ) ) ;
#252397 = ORIENTED_EDGE ( 'NONE', *, *, #157341, .F. ) ;
#252398 = TOROIDAL_SURFACE ( 'NONE', #56747, 11.65000000000000036, 0.1000000000000000056 ) ;
#252399 = CIRCLE ( 'NONE', #177455, 0.6000000000000023093 ) ;
#252400 = ORIENTED_EDGE ( 'NONE', *, *, #125672, .T. ) ;
#252401 = VECTOR ( 'NONE', #131826, 1000.000000000000000 ) ;
#252402 = CARTESIAN_POINT ( 'NONE',  ( 21.08479644141221954, 75.94144555744806269, -142.8681461422562222 ) ) ;
#252403 = EDGE_CURVE ( 'NONE', #33572, #67782, #178073, .T. ) ;
#252404 = DIRECTION ( 'NONE',  ( 0.000000000000000000, -1.000000000000000000, -1.734723475976807292E-15 ) ) ;
#252406 = ORIENTED_EDGE ( 'NONE', *, *, #46474, .F. ) ;
#252405 = LINE ( 'NONE', #73819, #216615 ) ;
#252407 = CARTESIAN_POINT ( 'NONE',  ( 23.14999999999999858, 2.100000000011158274, -67.00000000000000000 ) ) ;
#252409 = AXIS2_PLACEMENT_3D ( 'NONE', #148213, #227745, #166525 ) ;
#252408 = LINE ( 'NONE', #153377, #207265 ) ;
#252410 = EDGE_CURVE ( 'NONE', #35945, #260, #10236, .T. ) ;
#252411 = FACE_OUTER_BOUND ( 'NONE', #159122, .T. ) ;
#252412 = AXIS2_PLACEMENT_3D ( 'NONE', #250315, #212489, #112111 ) ;
#252413 = CARTESIAN_POINT ( 'NONE',  ( -18.34374000495060386, 11.47316190337362585, -76.25000000000004263 ) ) ;
#252414 = CARTESIAN_POINT ( 'NONE',  ( 18.59999999999997655, 1.115600667400684642E-11, -134.0000000000000284 ) ) ;
#252415 = CARTESIAN_POINT ( 'NONE',  ( 23.24999999999999645, -3.899999999988843502, -200.9999999999999432 ) ) ;
#252416 = FACE_OUTER_BOUND ( 'NONE', #99775, .T. ) ;
#252418 = EDGE_LOOP ( 'NONE', ( #110675, #23914, #147028, #257150 ) ) ;
#252417 = DIRECTION ( 'NONE',  ( 0.000000000000000000, 0.9910465087640866200, 0.1335171055202867274 ) ) ;
#252420 = ORIENTED_EDGE ( 'NONE', *, *, #216478, .F. ) ;
#252419 = PRODUCT_DEFINITION ( 'UNKNOWN', '', #107198, #35018 ) ;
#252422 = CARTESIAN_POINT ( 'NONE',  ( -16.87683809663752044, 50.93224991157929082, -232.2540631895258798 ) ) ;
#252421 = DIRECTION ( 'NONE',  ( -2.940209281316621016E-16, -1.000000000000000000, -4.704334850106593625E-15 ) ) ;
#252424 = ORIENTED_EDGE ( 'NONE', *, *, #35582, .F. ) ;
#252423 = CARTESIAN_POINT ( 'NONE',  ( 20.95512820512820440, 8.876151316299273120, -75.55862899514100661 ) ) ;
#252425 = EDGE_LOOP ( 'NONE', ( #231929, #41881, #77668, #62061 ) ) ;
#252426 = CARTESIAN_POINT ( 'NONE',  ( -21.07094088545368038, 1.604332817732114336, -230.6611890373810638 ) ) ;
#252427 = CARTESIAN_POINT ( 'NONE',  ( -23.25000000000000000, -1.149570369564537842, -74.81591248450196474 ) ) ;
#252428 = VECTOR ( 'NONE', #187145, 1000.000000000000000 ) ;
#252429 = AXIS2_PLACEMENT_3D ( 'NONE', #211899, #128495, #250985 ) ;
#252430 = AXIS2_PLACEMENT_3D ( 'NONE', #3489, #6056, #242105 ) ;
#252432 = EDGE_CURVE ( 'NONE', #156851, #220552, #87912, .T. ) ;
#252431 = DIRECTION ( 'NONE',  ( 0.000000000000000000, 0.000000000000000000, 1.000000000000000000 ) ) ;
#252433 = CARTESIAN_POINT ( 'NONE',  ( 21.14999999999999858, 11.75000000001116263, -79.15000000000004832 ) ) ;
#252434 = EDGE_CURVE ( 'NONE', #5885, #228214, #248300, .T. ) ;
#252435 = EDGE_CURVE ( 'NONE', #20503, #236062, #227140, .T. ) ;
#252436 = DIRECTION ( 'NONE',  ( -0.000000000000000000, -0.8103668758649471560, 0.5859227990963360444 ) ) ;
#252437 = DIRECTION ( 'NONE',  ( -7.304098846218136639E-16, -0.4721928772777346239, -0.8814952561688430555 ) ) ;
#252438 = DIRECTION ( 'NONE',  ( -0.000000000000000000, 0.8127272543710951647, -0.5826443254700256480 ) ) ;
#252439 = ORIENTED_EDGE ( 'NONE', *, *, #243642, .F. ) ;
#252440 = VERTEX_POINT ( 'NONE', #205302 ) ;
#252441 = CARTESIAN_POINT ( 'NONE',  ( 21.05000000000000071, 30.68987205111126215, -252.2252246220829193 ) ) ;
#252442 = CIRCLE ( 'NONE', #240004, 0.2000000000000111688 ) ;
#252443 = EDGE_CURVE ( 'NONE', #19091, #133581, #131281, .T. ) ;
#252444 = EDGE_LOOP ( 'NONE', ( #62995, #232052, #24539, #247797, #201006 ) ) ;
#252445 = CARTESIAN_POINT ( 'NONE',  ( -18.59999999999999787, 7.939498413483247141, -209.7295111514051200 ) ) ;
#252446 = ORIENTED_EDGE ( 'NONE', *, *, #155622, .F. ) ;
#252447 = DIRECTION ( 'NONE',  ( 0.000000000000000000, 6.982962677686266711E-15, -1.000000000000000000 ) ) ;
#252448 = PLANE ( 'NONE',  #105251 ) ;
#252449 = DIRECTION ( 'NONE',  ( 0.000000000000000000, 0.000000000000000000, 1.000000000000000000 ) ) ;
#252450 = ORIENTED_EDGE ( 'NONE', *, *, #235438, .T. ) ;
#252451 = FACE_OUTER_BOUND ( 'NONE', #114943, .T. ) ;
#252452 = ORIENTED_EDGE ( 'NONE', *, *, #147786, .T. ) ;
#252453 = AXIS2_PLACEMENT_3D ( 'NONE', #123552, #103957, #4848 ) ;
#252454 = DIRECTION ( 'NONE',  ( 0.000000000000000000, 1.000000000000000000, -8.673617379884043361E-16 ) ) ;
#252455 = CIRCLE ( 'NONE', #210780, 1.749999999999998002 ) ;
#252456 = ADVANCED_FACE ( 'NONE', ( #7106, #166230, #67093 ), #106200, .F. ) ;
#252457 = LINE ( 'NONE', #12608, #59117 ) ;
#252458 = AXIS2_PLACEMENT_3D ( 'NONE', #101483, #83218, #160253 ) ;
#252459 = VECTOR ( 'NONE', #167525, 1000.000000000000000 ) ;
#252460 = ORIENTED_EDGE ( 'NONE', *, *, #152368, .T. ) ;
#252461 = DIRECTION ( 'NONE',  ( 0.000000000000000000, -6.938893903907222067E-15, 1.000000000000000000 ) ) ;
#252462 = ORIENTED_EDGE ( 'NONE', *, *, #169743, .T. ) ;
#252465 = ORIENTED_EDGE ( 'NONE', *, *, #240870, .T. ) ;
#252464 = DIRECTION ( 'NONE',  ( 0.000000000000000000, 0.000000000000000000, 1.000000000000000000 ) ) ;
#252463 = CARTESIAN_POINT ( 'NONE',  ( 22.49436431346199683, 55.96998815520995407, -232.8702878457373231 ) ) ;
#252466 = CARTESIAN_POINT ( 'NONE',  ( -20.87155475150660777, 64.25000000001148237, -42.92752095536695123 ) ) ;
#252467 = VERTEX_POINT ( 'NONE', #244439 ) ;
#252468 = TOROIDAL_SURFACE ( 'NONE', #256718, 0.6000000000000009770, 0.1000000000000000056 ) ;
#252469 = ORIENTED_EDGE ( 'NONE', *, *, #17407, .T. ) ;
#252470 = EDGE_CURVE ( 'NONE', #25818, #51735, #52170, .T. ) ;
#252471 = CARTESIAN_POINT ( 'NONE',  ( -23.15000000000000213, 0.000000000000000000, -20.62500000000000355 ) ) ;
#252472 = ORIENTED_EDGE ( 'NONE', *, *, #37662, .T. ) ;
#252473 = DIRECTION ( 'NONE',  ( 2.259780016855445309E-14, 0.9875055080513753802, -0.1575844902526748192 ) ) ;
#252474 = CARTESIAN_POINT ( 'NONE',  ( 21.07928932188134397, 69.67148334361834827, -69.62200263017876978 ) ) ;
#252475 = CIRCLE ( 'NONE', #235921, 0.09999999999999938105 ) ;
#252476 = CYLINDRICAL_SURFACE ( 'NONE', #224272, 0.1000000000000028644 ) ;
#252477 = DIRECTION ( 'NONE',  ( -1.000000000000000000, -0.000000000000000000, 0.000000000000000000 ) ) ;
#252478 = EDGE_CURVE ( 'NONE', #19042, #235775, #39737, .T. ) ;
#252479 = TOROIDAL_SURFACE ( 'NONE', #185851, 0.2000000000000000111, 0.1000000000000000056 ) ;
#252480 = LINE ( 'NONE', #128709, #89392 ) ;
#252481 = VECTOR ( 'NONE', #118955, 1000.000000000000227 ) ;
#252482 = ORIENTED_EDGE ( 'NONE', *, *, #31560, .F. ) ;
#252483 = CARTESIAN_POINT ( 'NONE',  ( -16.94037747912386394, 44.01927583580262393, -235.2813664045062865 ) ) ;
#252484 = CARTESIAN_POINT ( 'NONE',  ( -20.94999999999999929, 64.36312671090736615, -109.8448666978492838 ) ) ;
#252485 = CARTESIAN_POINT ( 'NONE',  ( -20.94999999999999929, 11.65000000001115055, -160.7161343370219129 ) ) ;
#252486 = ORIENTED_EDGE ( 'NONE', *, *, #54337, .T. ) ;
#252487 = DIRECTION ( 'NONE',  ( 0.000000000000000000, -0.4721928772777346239, -0.8814952561688430555 ) ) ;
#252488 = ORIENTED_EDGE ( 'NONE', *, *, #105567, .F. ) ;
#252489 = CARTESIAN_POINT ( 'NONE',  ( -21.40925344232282512, 33.84637352282563683, -243.5150031621282665 ) ) ;
#252490 = EDGE_LOOP ( 'NONE', ( #99505, #153811, #168342, #82557 ) ) ;
#252491 = EDGE_CURVE ( 'NONE', #100958, #131701, #65806, .T. ) ;
#252492 = EDGE_CURVE ( 'NONE', #143362, #48110, #28002, .T. ) ;
#252493 = CARTESIAN_POINT ( 'NONE',  ( -23.15000000000000213, 11.60058429089262333, -246.3380203656811887 ) ) ;
#252494 = DIRECTION ( 'NONE',  ( 0.000000000000000000, -1.000000000000000000, -2.891205793294679805E-16 ) ) ;
#252495 = CIRCLE ( 'NONE', #160951, 0.09999999999999939493 ) ;
#252497 = ORIENTED_EDGE ( 'NONE', *, *, #195922, .F. ) ;
#252496 = DIRECTION ( 'NONE',  ( 0.000000000000000000, 0.8814952561688429444, -0.4721928772777345684 ) ) ;
#252498 = EDGE_LOOP ( 'NONE', ( #245240, #196711, #24245, #142633 ) ) ;
#252499 = DIRECTION ( 'NONE',  ( -1.000000000000000000, 0.000000000000000000, 0.000000000000000000 ) ) ;
#252500 = CARTESIAN_POINT ( 'NONE',  ( -16.89155683852533230, 9.950000000011138823, -113.7773718495397617 ) ) ;
#252501 = ORIENTED_EDGE ( 'NONE', *, *, #228821, .T. ) ;
#252502 = DIRECTION ( 'NONE',  ( -1.000000000000000000, 0.000000000000000000, 0.000000000000000000 ) ) ;
#252503 = LINE ( 'NONE', #75192, #210987 ) ;
#252504 = ORIENTED_EDGE ( 'NONE', *, *, #19889, .F. ) ;
#252505 = DIRECTION ( 'NONE',  ( -0.000000000000000000, 0.3848449534832604213, 0.9229812358756095403 ) ) ;
#252506 = CIRCLE ( 'NONE', #40170, 0.09999999999999939493 ) ;
#252507 = CIRCLE ( 'NONE', #52612, 0.1000000000000060146 ) ;
#252508 = EDGE_CURVE ( 'NONE', #24254, #128036, #52342, .T. ) ;
#252509 = AXIS2_PLACEMENT_3D ( 'NONE', #224206, #166851, #209797 ) ;
#252510 = CIRCLE ( 'NONE', #94306, 0.09999999999999939493 ) ;
#252511 = EDGE_CURVE ( 'NONE', #99525, #143336, #187066, .T. ) ;
#252512 = VERTEX_POINT ( 'NONE', #128361 ) ;
#252513 = LINE ( 'NONE', #115578, #254274 ) ;
#252514 = DIRECTION ( 'NONE',  ( 0.000000000000000000, -0.9908441862701596881, -0.1350103645451904977 ) ) ;
#252515 = EDGE_CURVE ( 'NONE', #37909, #26422, #148216, .T. ) ;
#252516 = ORIENTED_EDGE ( 'NONE', *, *, #176371, .T. ) ;
#252517 = DIRECTION ( 'NONE',  ( 0.000000000000000000, 0.000000000000000000, 1.000000000000000000 ) ) ;
#252518 = DIRECTION ( 'NONE',  ( 1.000000000000000000, -0.000000000000000000, -0.000000000000000000 ) ) ;
#252519 = ADVANCED_FACE ( 'NONE', ( #141063 ), #64821, .F. ) ;
#252520 = DIRECTION ( 'NONE',  ( 1.000000000000000000, -7.304098846218134667E-16, 0.000000000000000000 ) ) ;
#252521 = VECTOR ( 'NONE', #221192, 1000.000000000000000 ) ;
#252523 = CARTESIAN_POINT ( 'NONE',  ( -15.31895204843005054, 66.60346600605763001, -51.61716770535109333 ) ) ;
#252522 = CARTESIAN_POINT ( 'NONE',  ( 20.95289811251229750, 8.893168004469750088, -42.00180949391852181 ) ) ;
#252524 = CARTESIAN_POINT ( 'NONE',  ( -21.55000000000000071, 68.65000000001253966, -182.3731074845244109 ) ) ;
#252526 = EDGE_CURVE ( 'NONE', #104609, #220164, #160651, .T. ) ;
#252525 = DIRECTION ( 'NONE',  ( 1.000000000000000000, 0.000000000000000000, 0.000000000000000000 ) ) ;
#252527 = CIRCLE ( 'NONE', #77733, 11.80000000000000426 ) ;
#252528 = CIRCLE ( 'NONE', #140098, 11.64999999999999325 ) ;
#252529 = CARTESIAN_POINT ( 'NONE',  ( 20.94999999999999574, 44.10931966560507789, -259.0886734199950183 ) ) ;
#252530 = CARTESIAN_POINT ( 'NONE',  ( 23.14999999999999503, 66.37537870982728805, -213.6053525232321704 ) ) ;
#252531 = ORIENTED_EDGE ( 'NONE', *, *, #257784, .F. ) ;
#252532 = VERTEX_POINT ( 'NONE', #180197 ) ;
#252533 = DIRECTION ( 'NONE',  ( 1.000000000000000000, 0.000000000000000000, 0.000000000000000000 ) ) ;
#252534 = AXIS2_PLACEMENT_3D ( 'NONE', #130219, #205914, #28624 ) ;
#252536 = ORIENTED_EDGE ( 'NONE', *, *, #205007, .F. ) ;
#252535 = CARTESIAN_POINT ( 'NONE',  ( -20.64999999999999858, 74.00000000001254818, -182.8477294072864652 ) ) ;
#252537 = VERTEX_POINT ( 'NONE', #221845 ) ;
#252538 = CARTESIAN_POINT ( 'NONE',  ( 23.14999999999999858, 1.115600667400684642E-11, -67.00000000000000000 ) ) ;
#252539 = ORIENTED_EDGE ( 'NONE', *, *, #48207, .T. ) ;
#252540 = DIRECTION ( 'NONE',  ( 0.000000000000000000, 1.000000000000000000, 0.000000000000000000 ) ) ;
#252541 = ADVANCED_FACE ( 'NONE', ( #103193 ), #241451, .F. ) ;
#252542 = ADVANCED_FACE ( 'NONE', ( #120249 ), #61526, .T. ) ;
#252543 = ORIENTED_EDGE ( 'NONE', *, *, #209944, .T. ) ;
#252544 = DIRECTION ( 'NONE',  ( -0.000000000000000000, -6.982962677686266711E-15, 1.000000000000000000 ) ) ;
#252547 = ORIENTED_EDGE ( 'NONE', *, *, #189190, .F. ) ;
#252546 = ORIENTED_EDGE ( 'NONE', *, *, #48834, .T. ) ;
#252545 = VECTOR ( 'NONE', #91254, 1000.000000000000000 ) ;
#252548 = ORIENTED_EDGE ( 'NONE', *, *, #149566, .F. ) ;
#252549 = ORIENTED_EDGE ( 'NONE', *, *, #195574, .F. ) ;
#252550 = ORIENTED_EDGE ( 'NONE', *, *, #39528, .T. ) ;
#252551 = CARTESIAN_POINT ( 'NONE',  ( 20.04142135623730070, 64.25000000001176659, -78.37310748452439668 ) ) ;
#252552 = CARTESIAN_POINT ( 'NONE',  ( -20.94999999999999929, -11.64999999998884306, -97.40000000000004832 ) ) ;
#252553 = CARTESIAN_POINT ( 'NONE',  ( 21.05000000000000071, 8.876614585098254295, -75.38508047884472774 ) ) ;
#252555 = ORIENTED_EDGE ( 'NONE', *, *, #12500, .T. ) ;
#252554 = DIRECTION ( 'NONE',  ( 0.000000000000000000, 0.000000000000000000, 1.000000000000000000 ) ) ;
#252556 = CYLINDRICAL_SURFACE ( 'NONE', #3528, 11.74999999999999645 ) ;
#252557 = PLANE ( 'NONE',  #215839 ) ;
#252559 = ORIENTED_EDGE ( 'NONE', *, *, #245017, .T. ) ;
#252558 = CARTESIAN_POINT ( 'NONE',  ( -22.39999999999999858, 0.000000000000000000, 7.790779598373403836 ) ) ;
#252560 = DIRECTION ( 'NONE',  ( 0.000000000000000000, 0.000000000000000000, 1.000000000000000000 ) ) ;
#252561 = ORIENTED_EDGE ( 'NONE', *, *, #54292, .T. ) ;
#252563 = CIRCLE ( 'NONE', #131773, 0.09999999999999939493 ) ;
#252562 = DIRECTION ( 'NONE',  ( 0.000000000000000000, 0.000000000000000000, -1.000000000000000000 ) ) ;
#252565 = ORIENTED_EDGE ( 'NONE', *, *, #234230, .F. ) ;
#252564 = CARTESIAN_POINT ( 'NONE',  ( -20.94999999999999929, 77.73625713160926409, -91.45445515550680682 ) ) ;
#252566 = CARTESIAN_POINT ( 'NONE',  ( 21.05000000000000071, 36.75018516840536620, -249.5102790111118338 ) ) ;
#252567 = PLANE ( 'NONE',  #133282 ) ;
#252568 = AXIS2_PLACEMENT_3D ( 'NONE', #30141, #232190, #250442 ) ;
#252569 = EDGE_LOOP ( 'NONE', ( #125827, #214329, #110950, #204574 ) ) ;
#252571 = DIRECTION ( 'NONE',  ( 0.000000000000000000, 8.881784197000696176E-16, -1.000000000000000000 ) ) ;
#252570 = CARTESIAN_POINT ( 'NONE',  ( -22.00411653889199570, 75.90096189422563100, -210.7765503521646622 ) ) ;
#252572 = B_SPLINE_CURVE_WITH_KNOTS ( 'NONE', 3,
 ( #68467, #89292, #167583, #148000 ),
 .UNSPECIFIED., .F., .F.,
 ( 4, 4 ),
 ( 0.000000000000000000, 0.0001048066582182432421 ),
 .UNSPECIFIED. ) ;
#252573 = CARTESIAN_POINT ( 'NONE',  ( -23.25000000000000000, -11.64999999998884483, -64.00000000000000000 ) ) ;
#252574 = AXIS2_PLACEMENT_3D ( 'NONE', #172873, #33356, #52862 ) ;
#252575 = AXIS2_PLACEMENT_3D ( 'NONE', #16217, #137409, #193555 ) ;
#252576 = EDGE_CURVE ( 'NONE', #180347, #99076, #139746, .T. ) ;
#252577 = DIRECTION ( 'NONE',  ( -1.000000000000000000, 0.000000000000000000, 0.000000000000000000 ) ) ;
#252578 = LINE ( 'NONE', #230463, #134929 ) ;
#252579 = EDGE_LOOP ( 'NONE', ( #81868, #247841, #113614, #93143, #127533 ) ) ;
#252580 = ORIENTED_EDGE ( 'NONE', *, *, #212652, .T. ) ;
#252581 =( GEOMETRIC_REPRESENTATION_CONTEXT ( 3 ) GLOBAL_UNCERTAINTY_ASSIGNED_CONTEXT ( ( #217437 ) ) GLOBAL_UNIT_ASSIGNED_CONTEXT ( ( #43531, #78771, #203868 ) ) REPRESENTATION_CONTEXT ( 'NONE', 'WORKASPACE' ) );
#252582 = DIRECTION ( 'NONE',  ( 0.000000000000000000, 1.000000000000000000, 0.000000000000000000 ) ) ;
#252583 = DIRECTION ( 'NONE',  ( -1.000000000000000000, -0.000000000000000000, -0.000000000000000000 ) ) ;
#252584 = ORIENTED_EDGE ( 'NONE', *, *, #193313, .T. ) ;
#252585 = CARTESIAN_POINT ( 'NONE',  ( 18.54999999999999716, 61.20755944685601690, -224.6372899806900989 ) ) ;
#252586 = ORIENTED_EDGE ( 'NONE', *, *, #199872, .F. ) ;
#252587 = DIRECTION ( 'NONE',  ( 0.000000000000000000, -0.8777080977375132376, 0.4791956752371582251 ) ) ;
#252588 = CARTESIAN_POINT ( 'NONE',  ( 20.95512820512820440, 60.17125644644785609, -221.2995001548250684 ) ) ;
#252589 = CARTESIAN_POINT ( 'NONE',  ( -16.81744102076749314, 9.950000000011142376, -79.65000000000004832 ) ) ;
#252590 = ORIENTED_EDGE ( 'NONE', *, *, #82379, .F. ) ;
#252591 = CARTESIAN_POINT ( 'NONE',  ( -16.83199030136658081, 66.06935196689912004, -190.7507064618669688 ) ) ;
#252592 = ADVANCED_FACE ( 'NONE', ( #43245 ), #219301, .T. ) ;
#252593 = CIRCLE ( 'NONE', #110962, 0.09999999999999982514 ) ;
#252594 = ORIENTED_EDGE ( 'NONE', *, *, #187803, .T. ) ;
#252595 = EDGE_LOOP ( 'NONE', ( #144482, #99786, #28054, #130118 ) ) ;
#252596 = TOROIDAL_SURFACE ( 'NONE', #19385, 11.65000000000000036, 0.1000000000000000056 ) ;
#252597 = VERTEX_POINT ( 'NONE', #203596 ) ;
#252599 = CARTESIAN_POINT ( 'NONE',  ( 21.05000000000000071, 10.72371710471867701, -167.4999999999999716 ) ) ;
#252598 = VECTOR ( 'NONE', #3063, 1000.000000000000000 ) ;
#252600 = CARTESIAN_POINT ( 'NONE',  ( 15.52844286134407881, 66.62433047358577198, -53.65531747513846739 ) ) ;
#252601 = CARTESIAN_POINT ( 'NONE',  ( -20.54999999999999716, 27.82649702422227733, -239.8850763025288870 ) ) ;
#252602 = DIRECTION ( 'NONE',  ( 0.000000000000000000, 1.000000000000000000, 0.000000000000000000 ) ) ;
#252603 = AXIS2_PLACEMENT_3D ( 'NONE', #85310, #157548, #204001 ) ;
#252604 = CARTESIAN_POINT ( 'NONE',  ( 15.66039659514496130, 66.63925083009691264, -119.2085373439170866 ) ) ;
#252606 = DIRECTION ( 'NONE',  ( -0.000000000000000000, 0.9651348961777157509, -0.2617529984165031243 ) ) ;
#252605 = CARTESIAN_POINT ( 'NONE',  ( 18.59999999999999432, 74.73821383144687047, -94.93660852097883662 ) ) ;
#252608 = ORIENTED_EDGE ( 'NONE', *, *, #249269, .T. ) ;
#252607 = DIRECTION ( 'NONE',  ( 0.000000000000000000, 0.000000000000000000, 1.000000000000000000 ) ) ;
#252609 = CARTESIAN_POINT ( 'NONE',  ( -20.54999999999999716, 71.65000000001180069, -81.77310748452433131 ) ) ;
#252610 = EDGE_LOOP ( 'NONE', ( #247544, #54205, #107962, #8505 ) ) ;
#252611 = FACE_OUTER_BOUND ( 'NONE', #25710, .T. ) ;
#252612 = AXIS2_PLACEMENT_3D ( 'NONE', #192288, #153188, #115297 ) ;
#252613 = VERTEX_POINT ( 'NONE', #201030 ) ;
#252614 = ORIENTED_EDGE ( 'NONE', *, *, #101785, .T. ) ;
#252615 = DIRECTION ( 'NONE',  ( 0.000000000000000000, -0.4721928772777346239, -0.8814952561688430555 ) ) ;
#252616 = CARTESIAN_POINT ( 'NONE',  ( -21.13435531349819030, 6.493721063603186572, -134.0000000000000284 ) ) ;
#252617 = CARTESIAN_POINT ( 'NONE',  ( -21.05000000000000071, 76.00000000001273293, -210.0637644362255685 ) ) ;
#252618 = PLANE ( 'NONE',  #200064 ) ;
#252619 = VECTOR ( 'NONE', #26474, 999.9999999999998863 ) ;
#252620 = DIRECTION ( 'NONE',  ( 0.000000000000000000, -7.116814260417668513E-15, 1.000000000000000000 ) ) ;
#252622 = ORIENTED_EDGE ( 'NONE', *, *, #69036, .F. ) ;
#252621 = CIRCLE ( 'NONE', #202741, 0.09999999999999761857 ) ;
#252623 = VERTEX_POINT ( 'NONE', #161926 ) ;
#252624 = CIRCLE ( 'NONE', #35629, 0.09999999999999516220 ) ;
#252625 = CARTESIAN_POINT ( 'NONE',  ( 23.15000000000000213, 28.50120599808395028, -258.2149742250584268 ) ) ;
#252626 = ORIENTED_EDGE ( 'NONE', *, *, #138889, .T. ) ;
#252627 = FACE_OUTER_BOUND ( 'NONE', #247590, .T. ) ;
#252628 = EDGE_LOOP ( 'NONE', ( #202708, #160512, #10168, #62041 ) ) ;
#252629 = LINE ( 'NONE', #153598, #117174 ) ;
#252630 = CARTESIAN_POINT ( 'NONE',  ( -18.59999999999999787, 11.65000000001115232, -107.5148057706540357 ) ) ;
#252631 = CARTESIAN_POINT ( 'NONE',  ( 21.09793522318408066, 65.27537548979951509, -157.7838166135473728 ) ) ;
#252632 = ORIENTED_EDGE ( 'NONE', *, *, #22593, .F. ) ;
#252633 = DIRECTION ( 'NONE',  ( 0.000000000000000000, 1.000000000000000000, 6.982962677686266711E-15 ) ) ;
#252634 = CARTESIAN_POINT ( 'NONE',  ( -21.14999999999994174, 77.16254490893143725, -43.82310748452479743 ) ) ;
#252635 = ADVANCED_FACE ( 'NONE', ( #101900 ), #144509, .F. ) ;
#252636 = AXIS2_PLACEMENT_3D ( 'NONE', #145421, #223666, #244522 ) ;
#252637 = CARTESIAN_POINT ( 'NONE',  ( -20.94999999999999929, 57.68174901751925177, -226.1764612035511846 ) ) ;
#252638 = EDGE_LOOP ( 'NONE', ( #44856, #24433, #2161, #28364 ) ) ;
#252639 = EDGE_CURVE ( 'NONE', #9598, #85043, #5365, .T. ) ;
#252640 = DIRECTION ( 'NONE',  ( 0.000000000000000000, -5.956132106358139644E-15, -1.000000000000000000 ) ) ;
#252641 = ORIENTED_EDGE ( 'NONE', *, *, #155392, .F. ) ;
#252642 = DIRECTION ( 'NONE',  ( -1.000000000000000000, 1.207181226542539700E-16, -2.694675058168174199E-16 ) ) ;
#252643 = EDGE_CURVE ( 'NONE', #71370, #240172, #163199, .T. ) ;
#252644 = CARTESIAN_POINT ( 'NONE',  ( -16.87683809663752399, 66.13508655273160741, -82.79882593322042794 ) ) ;
#252645 = CARTESIAN_POINT ( 'NONE',  ( -20.94999999999999929, 5.900000000011162093, -190.7809002353436085 ) ) ;
#252646 = FACE_OUTER_BOUND ( 'NONE', #68001, .T. ) ;
#252647 = CARTESIAN_POINT ( 'NONE',  ( -21.14999999999994174, 64.35000000001120668, -36.02310748452479316 ) ) ;
#252649 = VERTEX_POINT ( 'NONE', #143616 ) ;
#252648 = AXIS2_PLACEMENT_3D ( 'NONE', #22900, #102372, #121978 ) ;
#252650 = DIRECTION ( 'NONE',  ( -1.000000000000000000, 0.000000000000000000, 0.000000000000000000 ) ) ;
#252651 = DIRECTION ( 'NONE',  ( -1.000000000000000000, 0.000000000000000000, 0.000000000000000000 ) ) ;
#252652 = CIRCLE ( 'NONE', #165179, 0.1000000000000055705 ) ;
#252653 = AXIS2_PLACEMENT_3D ( 'NONE', #225845, #27723, #207623 ) ;
#252654 = CARTESIAN_POINT ( 'NONE',  ( 22.00411653962184033, 10.46655577782818369, -227.2920607449376575 ) ) ;
#252655 = DIRECTION ( 'NONE',  ( -0.000000000000000000, 0.9126074666063770380, 0.4088369013363281068 ) ) ;
#252656 = EDGE_CURVE ( 'NONE', #201700, #239369, #238876, .T. ) ;
#252657 = CARTESIAN_POINT ( 'NONE',  ( -20.64999999999999858, 67.23127455305841238, -235.8551265064783991 ) ) ;
#252658 = CIRCLE ( 'NONE', #61132, 0.09999999999999939493 ) ;
#252659 = ORIENTED_EDGE ( 'NONE', *, *, #173899, .F. ) ;
#252660 = EDGE_LOOP ( 'NONE', ( #154260, #217449, #74306, #220794 ) ) ;
#252661 = DIRECTION ( 'NONE',  ( -2.568025086422246928E-15, -0.1480365673253023762, 0.9889818879709281196 ) ) ;
#252662 = CARTESIAN_POINT ( 'NONE',  ( 21.05000000000000071, 5.499999999999998224, -12.40526601891309788 ) ) ;
#252663 = CARTESIAN_POINT ( 'NONE',  ( 18.39999999999999503, 11.75000000001113953, -113.1500000000000341 ) ) ;
#252664 = CARTESIAN_POINT ( 'NONE',  ( -20.54999999999999716, 24.04029978241812415, -253.0016354099517457 ) ) ;
#252665 =( BOUNDED_SURFACE ( )  B_SPLINE_SURFACE ( 3, 2, ( 
 ( #243098, #241814, #81427 ),
 ( #245676, #7053, #64476 ),
 ( #161007, #67039, #61902 ),
 ( #123164, #224810, #141429 ) ),
 .UNSPECIFIED., .F., .F., .F. ) 
 B_SPLINE_SURFACE_WITH_KNOTS ( ( 4, 4 ),
 ( 3, 3 ),
 ( 0.0008258556059633759532, 0.0009616864997632785118 ),
 ( 0.000000000000000000, 1.000000000000000000 ),
 .UNSPECIFIED. ) 
 GEOMETRIC_REPRESENTATION_ITEM ( )  RATIONAL_B_SPLINE_SURFACE ( (
 ( 1.000000000000000000, 0.9152888060719408525, 1.000000000000000000),
 ( 1.000000000000000000, 0.9327727094138127395, 1.000000000000000000),
 ( 1.000000000000000000, 0.9369023509258341820, 1.000000000000000000),
 ( 1.000000000000000000, 0.9246339933864554661, 1.000000000000000000) ) ) 
 REPRESENTATION_ITEM ( '' )  SURFACE ( )  );
#252666 = LINE ( 'NONE', #17908, #249671 ) ;
#252667 = EDGE_CURVE ( 'NONE', #94746, #85340, #144890, .T. ) ;
#252668 = AXIS2_PLACEMENT_3D ( 'NONE', #163450, #47327, #206423 ) ;
#252669 = ORIENTED_EDGE ( 'NONE', *, *, #44767, .F. ) ;
#252670 = LINE ( 'NONE', #153642, #255446 ) ;
#252671 = AXIS2_PLACEMENT_3D ( 'NONE', #42828, #143192, #198036 ) ;
#252672 = LINE ( 'NONE', #132762, #192451 ) ;
#252673 = ORIENTED_EDGE ( 'NONE', *, *, #237723, .T. ) ;
#252674 = CARTESIAN_POINT ( 'NONE',  ( 21.14999999999999858, 26.06832281015329755, -254.4051978787608732 ) ) ;
#252675 = B_SPLINE_CURVE_WITH_KNOTS ( 'NONE', 3,
 ( #43991, #7423, #102653, #227759, #222602, #223896, #46541, #28321, #23174, #244744, #243472, #66124, #83076, #183508 ),
 .UNSPECIFIED., .F., .F.,
 ( 4, 2, 2, 2, 2, 2, 4 ),
 ( 0.000000000000000000, 0.0003823333598417661934, 0.0005735000397626486938, 0.0006690833797230898898, 0.0007168750497033118431, 0.0007407708846934227655, 0.0007646667196835337963 ),
 .UNSPECIFIED. ) ;
#252676 = CARTESIAN_POINT ( 'NONE',  ( -20.54999999999999716, 73.60000000001254250, -183.2477294072864709 ) ) ;
#252677 = VERTEX_POINT ( 'NONE', #204863 ) ;
#252678 = CARTESIAN_POINT ( 'NONE',  ( -21.00219873199057830, 12.81059202956635623, -205.2846788580854422 ) ) ;
#252679 = ORIENTED_EDGE ( 'NONE', *, *, #38007, .T. ) ;
#252680 = DIRECTION ( 'NONE',  ( -2.827886303505248766E-16, -0.8660254037844377084, -0.5000000000000015543 ) ) ;
#252681 = SPHERICAL_SURFACE ( 'NONE', #75668, 0.1000000000000000056 ) ;
#252682 = LINE ( 'NONE', #10251, #86676 ) ;
#252683 = CARTESIAN_POINT ( 'NONE',  ( 18.59999999999999787, -1.835341550224411922, -11.55515129256297868 ) ) ;
#252684 = DIRECTION ( 'NONE',  ( -1.000000000000000000, 0.000000000000000000, 0.000000000000000000 ) ) ;
#252685 = DIRECTION ( 'NONE',  ( 1.000000000000000000, 0.000000000000000000, 0.000000000000000000 ) ) ;
#252686 = CARTESIAN_POINT ( 'NONE',  ( 23.24999999999999289, 5.169232899390497238, -237.3909066255399978 ) ) ;
#252687 = CARTESIAN_POINT ( 'NONE',  ( -16.97683809663752186, 66.15000000001188596, -90.37310748452438247 ) ) ;
#252689 = DIRECTION ( 'NONE',  ( 0.000000000000000000, -1.000000000000000000, 0.000000000000000000 ) ) ;
#252688 = CARTESIAN_POINT ( 'NONE',  ( -20.94999999999999929, 77.16412189325286874, -61.60825939895269698 ) ) ;
#252690 = DIRECTION ( 'NONE',  ( 0.000000000000000000, 1.000000000000000000, 0.000000000000000000 ) ) ;
#252691 = CARTESIAN_POINT ( 'NONE',  ( -20.64999999999999858, 68.85000000001180354, -81.87310748452436826 ) ) ;
#252692 = FACE_OUTER_BOUND ( 'NONE', #87672, .T. ) ;
#252693 = AXIS2_PLACEMENT_3D ( 'NONE', #12136, #72096, #91647 ) ;
#252694 = VERTEX_POINT ( 'NONE', #105750 ) ;
#252695 = AXIS2_PLACEMENT_3D ( 'NONE', #85166, #4374, #63064 ) ;
#252696 = CIRCLE ( 'NONE', #106953, 0.8750000000000007772 ) ;
#252697 = CARTESIAN_POINT ( 'NONE',  ( -18.43634282235122512, -9.679787199927979202, -40.16065188545389475 ) ) ;
#252698 = AXIS2_PLACEMENT_3D ( 'NONE', #71111, #227590, #149372 ) ;
#252699 = CARTESIAN_POINT ( 'NONE',  ( 21.14999999999999858, 10.71339244341104013, -79.25000000000005684 ) ) ;
#252700 = DIRECTION ( 'NONE',  ( -0.000000000000000000, -0.8814952561688430555, 0.4721928772777346239 ) ) ;
#252701 = EDGE_CURVE ( 'NONE', #80661, #87379, #14957, .T. ) ;
#252702 = ORIENTED_EDGE ( 'NONE', *, *, #106997, .F. ) ;
#252703 = CARTESIAN_POINT ( 'NONE',  ( 23.24999999999999289, 64.35000000001178933, -81.67310748452439384 ) ) ;
#252704 = CARTESIAN_POINT ( 'NONE',  ( -20.94999999999999929, -1.164121893230052995, -108.4148480855716485 ) ) ;
#252705 = ADVANCED_FACE ( 'NONE', ( #127921 ), #9243, .T. ) ;
#252706 = ORIENTED_EDGE ( 'NONE', *, *, #88881, .T. ) ;
#252707 = DIRECTION ( 'NONE',  ( 0.000000000000000000, 0.8700118002898393765, -0.4930308989875104575 ) ) ;
#252708 = AXIS2_PLACEMENT_3D ( 'NONE', #195918, #1534, #39425 ) ;
#252709 = EDGE_LOOP ( 'NONE', ( #161021, #134197, #86698 ) ) ;
#252711 = ADVANCED_FACE ( 'NONE', ( #31419 ), #19035, .F. ) ;
#252710 = CARTESIAN_POINT ( 'NONE',  ( 22.60000000000000142, 64.25043287652226809, -69.62396585362311896 ) ) ;
#252712 = CARTESIAN_POINT ( 'NONE',  ( 21.14999999999999503, -8.729782940176418649, -238.4538547387928986 ) ) ;
#252713 = AXIS2_PLACEMENT_3D ( 'NONE', #185621, #27865, #166092 ) ;
#252714 = AXIS2_PLACEMENT_3D ( 'NONE', #95522, #98054, #194660 ) ;
#252715 = CIRCLE ( 'NONE', #27917, 4.049999999999998046 ) ;
#252716 = ORIENTED_EDGE ( 'NONE', *, *, #18776, .T. ) ;
#252717 = PLANE ( 'NONE',  #114332 ) ;
#252718 = ADVANCED_FACE ( 'NONE', ( #190484 ), #146182, .F. ) ;
#252719 = ORIENTED_EDGE ( 'NONE', *, *, #54190, .T. ) ;
#252721 =( BOUNDED_SURFACE ( )  B_SPLINE_SURFACE ( 3, 2, ( 
 ( #28654, #145966, #188959 ),
 ( #29909, #186404, #106837 ),
 ( #108139, #187694, #109402 ),
 ( #144678, #10335, #27361 ),
 ( #5150, #7760, #224219 ),
 ( #104261, #89840, #9034 ) ),
 .UNSPECIFIED., .F., .F., .F. ) 
 B_SPLINE_SURFACE_WITH_KNOTS ( ( 4, 2, 4 ),
 ( 3, 3 ),
 ( 4.712388980384689674, 5.497787143782137953, 6.283185307179586232 ),
 ( 0.000000000000000000, 1.000000000000000000 ),
 .UNSPECIFIED. ) 
 GEOMETRIC_REPRESENTATION_ITEM ( )  RATIONAL_B_SPLINE_SURFACE ( (
 ( 1.000000000000000000, 0.7071067811865536790, 1.000000000000000000),
 ( 1.000000000000000000, 0.7727932973490582169, 1.000000000000000000),
 ( 1.000000000000000000, 0.8282379607650555142, 1.000000000000000000),
 ( 1.000000000000000000, 0.9038128468038272301, 1.000000000000000000),
 ( 1.000000000000000000, 0.9240297172244550383, 1.000000000000000000),
 ( 1.000000000000000000, 0.9238795325112914014, 1.000000000000000000) ) ) 
 REPRESENTATION_ITEM ( '' )  SURFACE ( )  );
#252720 = CARTESIAN_POINT ( 'NONE',  ( 23.24999999999999645, 76.00000000001213607, -136.5231074845243313 ) ) ;
#252722 = CARTESIAN_POINT ( 'NONE',  ( -20.54999999999999716, 9.350000000011156942, -45.75000000000000000 ) ) ;
#252723 = FACE_OUTER_BOUND ( 'NONE', #5218, .T. ) ;
#252724 = EDGE_CURVE ( 'NONE', #171479, #156996, #71809, .T. ) ;
#252725 = DIRECTION ( 'NONE',  ( 0.000000000000000000, 0.4721928772777346239, 0.8814952561688430555 ) ) ;
#252726 = EDGE_CURVE ( 'NONE', #152124, #169487, #185640, .T. ) ;
#252727 = CARTESIAN_POINT ( 'NONE',  ( -16.87683809663752399, 9.849999999999988987, -13.40236401819630530 ) ) ;
#252728 = CARTESIAN_POINT ( 'NONE',  ( -22.47071067811865319, 0.09909245471376178227, -59.27992525550197911 ) ) ;
#252729 = CARTESIAN_POINT ( 'NONE',  ( 20.94999999999999574, 55.13994374908182294, -226.9527081427897315 ) ) ;
#252730 = CARTESIAN_POINT ( 'NONE',  ( 18.59999999999999076, 6.649999999999999467, -21.35000000000000142 ) ) ;
#252732 = ORIENTED_EDGE ( 'NONE', *, *, #257903, .F. ) ;
#252731 = DIRECTION ( 'NONE',  ( -1.836970198721029934E-16, -1.000000000000000000, -6.982962677686266711E-15 ) ) ;
#252734 = LINE ( 'NONE', #136637, #101875 ) ;
#252733 = CARTESIAN_POINT ( 'NONE',  ( -20.64999999999999858, 76.00000000001213607, -136.5231074845243313 ) ) ;
#252735 = ORIENTED_EDGE ( 'NONE', *, *, #180589, .F. ) ;
#252737 = ORIENTED_EDGE ( 'NONE', *, *, #191605, .F. ) ;
#252736 = LINE ( 'NONE', #32459, #31880 ) ;
#252738 = VECTOR ( 'NONE', #194225, 1000.000000000000000 ) ;
#252739 = VERTEX_POINT ( 'NONE', #86187 ) ;
#252740 = DIRECTION ( 'NONE',  ( 1.000000000000000000, 1.186688945009010077E-16, 0.000000000000000000 ) ) ;
#252741 = CARTESIAN_POINT ( 'NONE',  ( -20.64999999999999858, 85.00000000001149658, -45.91707660717669626 ) ) ;
#252743 = EDGE_CURVE ( 'NONE', #197300, #245627, #2464, .T. ) ;
#252742 = B_SPLINE_CURVE_WITH_KNOTS ( 'NONE', 3,
 ( #240697, #163735, #82863, #84130, #205401, #162460, #101128, #4632, #26816, #21659, #64619, #63326, #184564, #182012, #124608, #106295, #145433, #180733, #41244 ),
 .UNSPECIFIED., .F., .F.,
 ( 4, 3, 3, 3, 3, 3, 4 ),
 ( 1.387778780781445676E-17, 2.646747978908693493E-05, 5.271166642129208971E-05, 9.008788829885705832E-05, 0.0001426648776561096276, 0.0001897378458660022580, 0.0001917382627806449270 ),
 .UNSPECIFIED. ) ;
#252744 = CARTESIAN_POINT ( 'NONE',  ( 21.05000000000000071, 4.850467289730776344, -88.46573259099837117 ) ) ;
#252745 = CARTESIAN_POINT ( 'NONE',  ( -20.54999999999999716, 52.22920805963557456, -232.3304987350788906 ) ) ;
#252746 = EDGE_CURVE ( 'NONE', #255181, #136640, #194035, .T. ) ;
#252747 = EDGE_CURVE ( 'NONE', #23132, #144138, #225692, .T. ) ;
#252749 = CARTESIAN_POINT ( 'NONE',  ( 20.73486653747088582, 28.93140779147706709, -237.1870821964558900 ) ) ;
#252748 = VECTOR ( 'NONE', #231836, 1000.000000000000114 ) ;
#252750 = DIRECTION ( 'NONE',  ( -1.836970198721029441E-16, 0.4721928772777346239, 0.8814952561688430555 ) ) ;
#252752 = CIRCLE ( 'NONE', #36121, 0.09999999999999939493 ) ;
#252751 = CARTESIAN_POINT ( 'NONE',  ( 20.94999999999999929, 10.45765418377745526, -207.3040725013013912 ) ) ;
#252753 = ORIENTED_EDGE ( 'NONE', *, *, #245197, .F. ) ;
#252754 = ORIENTED_EDGE ( 'NONE', *, *, #69466, .T. ) ;
#252755 = CARTESIAN_POINT ( 'NONE',  ( 21.51976009735019346, 6.752178271738373816, -199.5294475661460467 ) ) ;
#252756 = ORIENTED_EDGE ( 'NONE', *, *, #104167, .F. ) ;
#252757 = PLANE ( 'NONE',  #255015 ) ;
#252758 = VERTEX_POINT ( 'NONE', #247859 ) ;
#252759 = CARTESIAN_POINT ( 'NONE',  ( 18.39999999999999858, -9.682403433476395094, -40.15684337741279109 ) ) ;
#252760 =( BOUNDED_CURVE ( )  B_SPLINE_CURVE ( 3, ( #42210, #40949, #80007, #63035 ),
 .UNSPECIFIED., .F., .F. ) 
 B_SPLINE_CURVE_WITH_KNOTS ( ( 4, 4 ),
 ( 3.432212674861196522, 3.693332928900582068 ),
 .UNSPECIFIED. ) 
 CURVE ( )  GEOMETRIC_REPRESENTATION_ITEM ( )  RATIONAL_B_SPLINE_CURVE ( ( 1.000000000000000000, 0.9943260843901261525, 0.9943260843901261525, 1.000000000000000000 ) ) 
 REPRESENTATION_ITEM ( '' )  );
#252761 = AXIS2_PLACEMENT_3D ( 'NONE', #65249, #24873, #106933 ) ;
#252762 = ADVANCED_FACE ( 'NONE', ( #6671 ), #208751, .T. ) ;
#252763 = FACE_OUTER_BOUND ( 'NONE', #196415, .T. ) ;
#252764 = CARTESIAN_POINT ( 'NONE',  ( -18.39999999999999858, 78.24390740893980478, -231.6169762517609172 ) ) ;
#252765 = EDGE_CURVE ( 'NONE', #91225, #43942, #214851, .T. ) ;
#252766 = AXIS2_PLACEMENT_3D ( 'NONE', #187558, #8898, #125004 ) ;
#252767 = CARTESIAN_POINT ( 'NONE',  ( -20.85000000000000142, 1.115600667400684642E-11, -67.00000000000000000 ) ) ;
#252768 = DIRECTION ( 'NONE',  ( -1.000000000000000000, 0.000000000000000000, 0.000000000000000000 ) ) ;
#252769 = ORIENTED_EDGE ( 'NONE', *, *, #80409, .F. ) ;
#252770 = FACE_OUTER_BOUND ( 'NONE', #238004, .T. ) ;
#252771 = LINE ( 'NONE', #194121, #77147 ) ;
#252772 = EDGE_CURVE ( 'NONE', #150150, #178868, #6566, .T. ) ;
#252773 = LINE ( 'NONE', #168162, #229675 ) ;
#252774 = LINE ( 'NONE', #135392, #244696 ) ;
#252775 = ORIENTED_EDGE ( 'NONE', *, *, #143760, .F. ) ;
#252777 = CARTESIAN_POINT ( 'NONE',  ( -18.48179518609241612, 85.51832530050492664, -29.13340190776325400 ) ) ;
#252776 = CARTESIAN_POINT ( 'NONE',  ( -16.89268316805466341, 22.97380970494227626, -230.9308293615217451 ) ) ;
#252778 = AXIS2_PLACEMENT_3D ( 'NONE', #213880, #37841, #215163 ) ;
#252779 = EDGE_LOOP ( 'NONE', ( #172066, #234269, #145694, #119345 ) ) ;
#252782 = EDGE_LOOP ( 'NONE', ( #4056, #47219, #156305 ) ) ;
#252781 = LINE ( 'NONE', #175847, #88002 ) ;
#252780 = CARTESIAN_POINT ( 'NONE',  ( 23.14999999999999858, 71.00000000001180922, -81.42837350343744163 ) ) ;
#252783 = AXIS2_PLACEMENT_3D ( 'NONE', #122299, #197004, #240964 ) ;
#252784 = AXIS2_PLACEMENT_3D ( 'NONE', #81017, #160608, #61410 ) ;
#252785 = DIRECTION ( 'NONE',  ( -1.000000000000000000, 0.000000000000000000, 0.000000000000000000 ) ) ;
#252786 = ORIENTED_EDGE ( 'NONE', *, *, #128428, .T. ) ;
#252787 = CARTESIAN_POINT ( 'NONE',  ( 20.85000000000000142, 76.00000000001207923, -128.7231074845243484 ) ) ;
#252788 = CIRCLE ( 'NONE', #94570, 4.000000000000003553 ) ;
#252789 = CYLINDRICAL_SURFACE ( 'NONE', #136427, 0.09999999999999939493 ) ;
#252790 = CIRCLE ( 'NONE', #244419, 7.791421356237338003 ) ;
#252791 = CARTESIAN_POINT ( 'NONE',  ( -18.59999999999999787, 7.021664781911246322, -104.3335654018973315 ) ) ;
#252792 = AXIS2_PLACEMENT_3D ( 'NONE', #191999, #53745, #249392 ) ;
#252794 = ORIENTED_EDGE ( 'NONE', *, *, #105274, .F. ) ;
#252793 = DIRECTION ( 'NONE',  ( 1.000000000000000000, 0.000000000000000000, 0.000000000000000000 ) ) ;
#252795 = EDGE_CURVE ( 'NONE', #172330, #48880, #73250, .T. ) ;
#252796 = VERTEX_POINT ( 'NONE', #131761 ) ;
#252797 = EDGE_CURVE ( 'NONE', #52702, #108203, #186619, .T. ) ;
#252798 = DIRECTION ( 'NONE',  ( 0.000000000000000000, -0.1298341882519953860, -0.9915357197604862671 ) ) ;
#252799 = CARTESIAN_POINT ( 'NONE',  ( -20.94999999999999929, 5.900000000011162093, -56.78090023534362984 ) ) ;
#252800 = CARTESIAN_POINT ( 'NONE',  ( -18.40000000000000213, 70.35000000001153353, -48.67310748452436542 ) ) ;
#252801 = AXIS2_PLACEMENT_3D ( 'NONE', #134528, #97960, #158012 ) ;
#252802 = FACE_OUTER_BOUND ( 'NONE', #12001, .T. ) ;
#252803 = ORIENTED_EDGE ( 'NONE', *, *, #30461, .T. ) ;
#252805 = CIRCLE ( 'NONE', #32260, 4.000000000000002665 ) ;
#252804 = DIRECTION ( 'NONE',  ( 0.000000000000000000, 1.000000000000000000, 0.000000000000000000 ) ) ;
#252806 = B_SPLINE_CURVE_WITH_KNOTS ( 'NONE', 3,
 ( #240201, #159381, #155550, #214213, #35601, #115105, #257129 ),
 .UNSPECIFIED., .F., .F.,
 ( 4, 3, 4 ),
 ( 0.000000000000000000, 3.357501770815708719E-05, 5.199112466349179362E-05 ),
 .UNSPECIFIED. ) ;
#252807 = EDGE_CURVE ( 'NONE', #26532, #213775, #7977, .T. ) ;
#252808 = EDGE_CURVE ( 'NONE', #4716, #177211, #164795, .T. ) ;
#252809 = CARTESIAN_POINT ( 'NONE',  ( 23.14999999999999503, 11.65000000001116298, -45.65000000000000568 ) ) ;
#252810 = CARTESIAN_POINT ( 'NONE',  ( -23.25000000000000000, 85.60000000001262777, -193.6291383618718385 ) ) ;
#252811 = EDGE_LOOP ( 'NONE', ( #76094, #133933, #21019, #243958 ) ) ;
#252812 = CARTESIAN_POINT ( 'NONE',  ( 20.54374330479356914, 59.11474337034464099, -225.6490816854725949 ) ) ;
#252813 = EDGE_CURVE ( 'NONE', #224878, #178186, #10545, .T. ) ;
#252814 = LINE ( 'NONE', #33827, #122160 ) ;
#252815 = CIRCLE ( 'NONE', #132029, 3.970710678118656300 ) ;
#252816 = ORIENTED_EDGE ( 'NONE', *, *, #73781, .T. ) ;
#252817 = DIRECTION ( 'NONE',  ( 2.952720810173289112E-16, -1.000000000000000000, 0.000000000000000000 ) ) ;
#252818 = DIRECTION ( 'NONE',  ( 1.000000000000000000, 0.000000000000000000, 0.000000000000000000 ) ) ;
#252819 = EDGE_CURVE ( 'NONE', #170452, #28569, #143670, .T. ) ;
#252820 = VERTEX_POINT ( 'NONE', #191774 ) ;
#252821 = ORIENTED_EDGE ( 'NONE', *, *, #177394, .F. ) ;
#252822 = EDGE_CURVE ( 'NONE', #108916, #160136, #233460, .T. ) ;
#252823 = AXIS2_PLACEMENT_3D ( 'NONE', #4912, #208295, #187449 ) ;
#252824 = DIRECTION ( 'NONE',  ( -0.000000000000000000, 1.000000000000000000, 6.982962677686266711E-15 ) ) ;
#252825 = EDGE_LOOP ( 'NONE', ( #43488, #190673, #153403, #8548 ) ) ;
#252827 = ORIENTED_EDGE ( 'NONE', *, *, #159943, .T. ) ;
#252826 = CARTESIAN_POINT ( 'NONE',  ( 13.99999999999999822, 9.850000000011137402, -117.2500000000000284 ) ) ;
#252828 = ADVANCED_FACE ( 'NONE', ( #75666 ), #191500, .T. ) ;
#252829 = VECTOR ( 'NONE', #115231, 1000.000000000000114 ) ;
#252830 = VECTOR ( 'NONE', #170136, 1000.000000000000000 ) ;
#252833 = EDGE_LOOP ( 'NONE', ( #187201, #83805, #106568, #21220 ) ) ;
#252832 = ORIENTED_EDGE ( 'NONE', *, *, #32878, .T. ) ;
#252831 = CARTESIAN_POINT ( 'NONE',  ( 21.70464131381650219, 60.38329692807814553, -233.9978952701749506 ) ) ;
#252834 = CIRCLE ( 'NONE', #240384, 0.09999999999998898659 ) ;
#252835 = TOROIDAL_SURFACE ( 'NONE', #236094, 0.2000000000000000111, 0.1000000000000000056 ) ;
#252836 = DIRECTION ( 'NONE',  ( 0.000000000000000000, -6.982962677686266711E-15, 1.000000000000000000 ) ) ;
#252837 = DIRECTION ( 'NONE',  ( 1.734723475976817507E-14, -6.982962677686266711E-15, 1.000000000000000000 ) ) ;
#252838 = CARTESIAN_POINT ( 'NONE',  ( 21.14999999999999858, 10.71339244341104013, -112.7500000000000284 ) ) ;
#252839 = EDGE_CURVE ( 'NONE', #41107, #217842, #27466, .T. ) ;
#252840 = CARTESIAN_POINT ( 'NONE',  ( 21.05000000000000071, 8.776282895303632259, -142.5586289951409640 ) ) ;
#252841 = CIRCLE ( 'NONE', #107107, 0.09999999999999939493 ) ;
#252842 = CARTESIAN_POINT ( 'NONE',  ( 23.14999999999999503, 64.35000000001178933, -81.67310748452439384 ) ) ;
#252843 = DIRECTION ( 'NONE',  ( 1.000000000000000000, 0.000000000000000000, 0.000000000000000000 ) ) ;
#252844 = ORIENTED_EDGE ( 'NONE', *, *, #189030, .T. ) ;
#252845 = VERTEX_POINT ( 'NONE', #216428 ) ;
#252846 = ORIENTED_EDGE ( 'NONE', *, *, #12047, .F. ) ;
#252847 = EDGE_CURVE ( 'NONE', #9216, #71227, #243891, .T. ) ;
#252848 = DIRECTION ( 'NONE',  ( 1.000000000000000000, 0.000000000000000000, 0.000000000000000000 ) ) ;
#252850 = VERTEX_POINT ( 'NONE', #232168 ) ;
#252849 = CARTESIAN_POINT ( 'NONE',  ( 13.99999999999999822, 9.850000000011137402, -83.75000000000004263 ) ) ;
#252851 = CYLINDRICAL_SURFACE ( 'NONE', #188293, 0.09999999999999939493 ) ;
#252852 = ORIENTED_EDGE ( 'NONE', *, *, #69982, .F. ) ;
#252853 = ORIENTED_EDGE ( 'NONE', *, *, #119507, .T. ) ;
#252854 = EDGE_CURVE ( 'NONE', #142489, #186873, #156503, .T. ) ;
#252855 = DIRECTION ( 'NONE',  ( 0.000000000000000000, 0.8814952561688476074, -0.4721928772777262417 ) ) ;
#252856 = VECTOR ( 'NONE', #256701, 1000.000000000000000 ) ;
#252857 = ADVANCED_FACE ( 'NONE', ( #234721 ), #255508, .T. ) ;
#252858 = TOROIDAL_SURFACE ( 'NONE', #115482, 11.65000000000000036, 0.1000000000000000056 ) ;
#252859 = ORIENTED_EDGE ( 'NONE', *, *, #206019, .T. ) ;
#252860 = CARTESIAN_POINT ( 'NONE',  ( -18.79999999999999716, 1.350000000000000089, 22.10000000000000142 ) ) ;
#252861 = CARTESIAN_POINT ( 'NONE',  ( -23.25000000000000000, 67.23127455305835554, -235.8551265064784559 ) ) ;
#252862 = B_SPLINE_CURVE_WITH_KNOTS ( 'NONE', 3,
 ( #237233, #58569, #136834, #138107, #256738, #220249, #160290, #139388, #3750, #199408, #179840, #80700, #102827, #224067, #101531, #119875, #41621, #20769, #122424, #25898, #44177, #83257, #164122, #23349, #121170, #218936 ),
 .UNSPECIFIED., .F., .F.,
 ( 4, 2, 2, 2, 2, 2, 2, 2, 2, 2, 2, 2, 4 ),
 ( 0.005476422646581343041, 0.006160811967703550517, 0.006845201288825757992, 0.007187395949386863464, 0.007529590609947969804, 0.007871785270509074409, 0.008213979931070180748, 0.008556174591631285353, 0.008898369252192391693, 0.009240563912753498033, 0.009582758573314604372, 0.01026714789443681358, 0.01095153721555902800 ),
 .UNSPECIFIED. ) ;
#252863 = VECTOR ( 'NONE', #26642, 1000.000000000000000 ) ;
#252865 = ORIENTED_EDGE ( 'NONE', *, *, #39955, .T. ) ;
#252864 = ORIENTED_EDGE ( 'NONE', *, *, #13309, .T. ) ;
#252866 = ORIENTED_EDGE ( 'NONE', *, *, #28610, .F. ) ;
#252867 = CARTESIAN_POINT ( 'NONE',  ( 21.05000000000000071, 8.776282895292474961, -8.558628995140949769 ) ) ;
#252868 = ORIENTED_EDGE ( 'NONE', *, *, #187968, .F. ) ;
#252869 = VERTEX_POINT ( 'NONE', #95207 ) ;
#252870 = CYLINDRICAL_SURFACE ( 'NONE', #13543, 0.1000000000000028644 ) ;
#252872 = EDGE_LOOP ( 'NONE', ( #47251, #188125, #134114, #106900 ) ) ;
#252871 = CARTESIAN_POINT ( 'NONE',  ( -21.05000000000000071, 76.00000000001232081, -162.1231074845243540 ) ) ;
#252873 = EDGE_CURVE ( 'NONE', #2919, #43634, #235694, .T. ) ;
#252874 = CARTESIAN_POINT ( 'NONE',  ( -20.90000000000000213, 7.986648289447971116, 1.311673547813416718 ) ) ;
#252876 = DIRECTION ( 'NONE',  ( 0.000000000000000000, -6.982962677686266711E-15, 1.000000000000000000 ) ) ;
#252875 = CARTESIAN_POINT ( 'NONE',  ( 18.59999999999998721, 19.85039924724470950, -136.2803030578013761 ) ) ;
#252877 = CARTESIAN_POINT ( 'NONE',  ( 21.14999999999999503, 76.10000000001245724, -181.6726782920691505 ) ) ;
#252878 = CARTESIAN_POINT ( 'NONE',  ( -21.05000000000000071, 76.00000000001216449, -140.6231074845243256 ) ) ;
#252879 = DIRECTION ( 'NONE',  ( 0.000000000000000000, -6.517943393102675675E-15, 1.000000000000000000 ) ) ;
#252880 = ORIENTED_EDGE ( 'NONE', *, *, #217117, .F. ) ;
#252881 = ORIENTED_EDGE ( 'NONE', *, *, #25871, .F. ) ;
#252882 = CARTESIAN_POINT ( 'NONE',  ( 18.49362639424906263, 85.44260436789993207, -96.25866655101246749 ) ) ;
#252883 = EDGE_CURVE ( 'NONE', #2960, #207654, #213868, .T. ) ;
#252884 = CARTESIAN_POINT ( 'NONE',  ( -21.05000000000000071, 75.90220970870339556, -142.7809220950004203 ) ) ;
#252885 = CARTESIAN_POINT ( 'NONE',  ( 21.13736287352038445, 41.81077915253129618, -238.4259954500851109 ) ) ;
#252886 = EDGE_LOOP ( 'NONE', ( #112806, #88354, #133806, #55397 ) ) ;
#252887 = CIRCLE ( 'NONE', #207120, 0.1999999999999987899 ) ;
#252888 = CIRCLE ( 'NONE', #157241, 0.9000000000000014655 ) ;
#252889 = CARTESIAN_POINT ( 'NONE',  ( -17.04761207306817283, 30.24242811800702668, -234.7396539225699428 ) ) ;
#252890 = AXIS2_PLACEMENT_3D ( 'NONE', #158218, #56485, #77338 ) ;
#252891 = AXIS2_PLACEMENT_3D ( 'NONE', #59868, #42907, #122447 ) ;
#252892 = CARTESIAN_POINT ( 'NONE',  ( -16.93826681692523195, 51.68086471459877629, -231.8513817628493712 ) ) ;
#252893 = DIRECTION ( 'NONE',  ( 0.000000000000000000, -6.982962677686266711E-15, 1.000000000000000000 ) ) ;
#252894 = ORIENTED_EDGE ( 'NONE', *, *, #4805, .T. ) ;
#252895 = ORIENTED_EDGE ( 'NONE', *, *, #48816, .T. ) ;
#252896 = LINE ( 'NONE', #57245, #71829 ) ;
#252897 = EDGE_CURVE ( 'NONE', #225850, #215500, #44190, .T. ) ;
#252898 = LINE ( 'NONE', #96375, #40533 ) ;
#252899 = ORIENTED_EDGE ( 'NONE', *, *, #57498, .F. ) ;
#252900 = DIRECTION ( 'NONE',  ( 1.000000000000000000, 0.000000000000000000, 0.000000000000000000 ) ) ;
#252901 = VERTEX_POINT ( 'NONE', #254258 ) ;
#252902 = LINE ( 'NONE', #149984, #248061 ) ;
#252903 = CARTESIAN_POINT ( 'NONE',  ( -20.64999999999999858, 76.00000000001190870, -103.0231074845243029 ) ) ;
#252905 = CARTESIAN_POINT ( 'NONE',  ( -21.07954763557489741, -1.282512354049770265, -194.8016594047362844 ) ) ;
#252904 = CARTESIAN_POINT ( 'NONE',  ( 23.40000000000005542, 74.63923853664559260, -43.99645795275012006 ) ) ;
#252906 = CARTESIAN_POINT ( 'NONE',  ( 18.55807992284871588, 65.67101464000555211, -164.4404391622479977 ) ) ;
#252907 = DIRECTION ( 'NONE',  ( -1.000000000000000000, -2.952720810173289112E-16, 0.000000000000000000 ) ) ;
#252908 = VECTOR ( 'NONE', #154048, 1000.000000000000000 ) ;
#252909 = AXIS2_PLACEMENT_3D ( 'NONE', #24711, #104195, #185033 ) ;
#252910 = CARTESIAN_POINT ( 'NONE',  ( -20.94999999999999929, 70.10000000001163301, -59.30400771986794695 ) ) ;
#252911 = EDGE_CURVE ( 'NONE', #129114, #257242, #21777, .T. ) ;
#252913 = ORIENTED_EDGE ( 'NONE', *, *, #169257, .T. ) ;
#252912 = ORIENTED_EDGE ( 'NONE', *, *, #34578, .F. ) ;
#252914 = VECTOR ( 'NONE', #211745, 1000.000000000000000 ) ;
#252915 = ORIENTED_EDGE ( 'NONE', *, *, #208554, .F. ) ;
#252916 = CARTESIAN_POINT ( 'NONE',  ( -18.50000000000000000, 11.74999999999999645, 11.75000000000000000 ) ) ;
#252917 = CARTESIAN_POINT ( 'NONE',  ( -20.94999999999999929, -1.362429037182149694, -175.3888812479212334 ) ) ;
#252918 = DIRECTION ( 'NONE',  ( -1.000000000000000000, 0.000000000000000000, 0.000000000000000000 ) ) ;
#252920 = CARTESIAN_POINT ( 'NONE',  ( -18.50000000000000000, 76.00000000001126921, -203.5231074845248997 ) ) ;
#252919 = DIRECTION ( 'NONE',  ( -1.000000000000000000, 0.000000000000000000, 0.000000000000000000 ) ) ;
#252921 = ORIENTED_EDGE ( 'NONE', *, *, #45469, .T. ) ;
#252922 = CARTESIAN_POINT ( 'NONE',  ( -22.50000000000000000, 76.00000000001199396, -109.2731074845243171 ) ) ;
#252923 = VERTEX_POINT ( 'NONE', #174794 ) ;
#252924 = ORIENTED_EDGE ( 'NONE', *, *, #115142, .F. ) ;
#252925 = CARTESIAN_POINT ( 'NONE',  ( -21.13435531349822583, 69.50627893641943444, -69.52310748452437394 ) ) ;
#252926 = CARTESIAN_POINT ( 'NONE',  ( -22.49072729836729678, 0.05648193274477467801, -88.84999175084509204 ) ) ;
#252927 = DIRECTION ( 'NONE',  ( 2.879366945564059217E-14, -0.9875055080513751582, 0.1575844902526747915 ) ) ;
#252928 = CIRCLE ( 'NONE', #148719, 0.09999999999999939493 ) ;
#252929 = CARTESIAN_POINT ( 'NONE',  ( -23.25000000000000000, 66.14499960962993441, -239.8604363256158933 ) ) ;
#252930 = CARTESIAN_POINT ( 'NONE',  ( -20.54999999999999716, 0.000000000000000000, -35.40000000000000568 ) ) ;
#252931 = ORIENTED_EDGE ( 'NONE', *, *, #8783, .T. ) ;
#252932 = VERTEX_POINT ( 'NONE', #116068 ) ;
#252933 = CARTESIAN_POINT ( 'NONE',  ( 20.94999999999999929, 8.776282895303628706, -176.0586289951409071 ) ) ;
#252934 = CARTESIAN_POINT ( 'NONE',  ( -18.39999999999999858, -9.519327731081281385, -40.47297637655933045 ) ) ;
#252935 = DIRECTION ( 'NONE',  ( 0.000000000000000000, 0.9964539953858966292, 0.08413937888696132461 ) ) ;
#252936 = DIRECTION ( 'NONE',  ( 1.000000000000000000, 0.000000000000000000, 0.000000000000000000 ) ) ;
#252937 = CIRCLE ( 'NONE', #194718, 0.1000000000000028644 ) ;
#252938 = DIRECTION ( 'NONE',  ( 1.836970198721029934E-16, -1.000000000000000000, -0.000000000000000000 ) ) ;
#252939 = FACE_OUTER_BOUND ( 'NONE', #203457, .T. ) ;
#252940 = CARTESIAN_POINT ( 'NONE',  ( 22.47071067811865319, 75.90090754530983475, -177.7431822290224090 ) ) ;
#252942 = DIRECTION ( 'NONE',  ( 0.000000000000000000, 0.000000000000000000, -1.000000000000000000 ) ) ;
#252941 = LINE ( 'NONE', #95165, #41141 ) ;
#252944 = EDGE_CURVE ( 'NONE', #253697, #5980, #113479, .T. ) ;
#252943 = FACE_OUTER_BOUND ( 'NONE', #66304, .T. ) ;
#252945 = AXIS2_PLACEMENT_3D ( 'NONE', #38471, #138810, #81413 ) ;
#252946 = DIRECTION ( 'NONE',  ( 1.000000000000000000, 0.000000000000000000, 0.000000000000000000 ) ) ;
#252947 = CARTESIAN_POINT ( 'NONE',  ( -23.15000000000000213, 2.600000000011156054, -180.7246219227620543 ) ) ;
#252948 = CARTESIAN_POINT ( 'NONE',  ( -21.55000000000000426, 68.25000000001253397, -182.2731074845244166 ) ) ;
#252949 = AXIS2_PLACEMENT_3D ( 'NONE', #237051, #77960, #35041 ) ;
#252951 = ORIENTED_EDGE ( 'NONE', *, *, #70821, .F. ) ;
#252950 = FACE_OUTER_BOUND ( 'NONE', #156285, .T. ) ;
#252952 = AXIS2_PLACEMENT_3D ( 'NONE', #113081, #33588, #208349 ) ;
#252953 = B_SPLINE_CURVE_WITH_KNOTS ( 'NONE', 3,
 ( #142460, #221974, #122922, #202449, #23837, #69374, #206305, #48503, #147606, #245438 ),
 .UNSPECIFIED., .F., .F.,
 ( 4, 2, 2, 2, 4 ),
 ( 0.000000000000000000, 4.221631689686969747E-05, 8.443263379373939495E-05, 0.0001688652675874697639, 0.0003377305351749538393 ),
 .UNSPECIFIED. ) ;
#252954 = PRODUCT_DEFINITION_FORMATION_WITH_SPECIFIED_SOURCE ( 'ANY', '', #170204, .NOT_KNOWN. ) ;
#252955 = CIRCLE ( 'NONE', #140511, 0.1000000000000028644 ) ;
#252956 = EDGE_CURVE ( 'NONE', #196832, #243879, #193034, .T. ) ;
#252957 = FACE_OUTER_BOUND ( 'NONE', #29372, .T. ) ;
#252958 = CIRCLE ( 'NONE', #136398, 0.09999999999999939493 ) ;
#252959 = EDGE_CURVE ( 'NONE', #89242, #136488, #136897, .T. ) ;
#252960 = CARTESIAN_POINT ( 'NONE',  ( 21.05000000000000071, 43.08177281680065818, -239.3869926993485535 ) ) ;
#252961 = CARTESIAN_POINT ( 'NONE',  ( 18.59999999999999432, 74.83729825007388570, -94.92310748452432279 ) ) ;
#252962 = DIRECTION ( 'NONE',  ( 0.000000000000000000, 0.1350103645451876666, -0.9908441862701600211 ) ) ;
#252963 = CARTESIAN_POINT ( 'NONE',  ( 18.52928932188133970, 33.79964813154141723, -236.3583302510377564 ) ) ;
#252965 = ADVANCED_FACE ( 'NONE', ( #73113 ), #152645, .F. ) ;
#252964 = AXIS2_PLACEMENT_3D ( 'NONE', #140764, #220313, #41682 ) ;
#252966 = DIRECTION ( 'NONE',  ( 0.000000000000000000, -0.5000000000000004441, -0.8660254037844384856 ) ) ;
#252967 = AXIS2_PLACEMENT_3D ( 'NONE', #146659, #250909, #150550 ) ;
#252968 = DIRECTION ( 'NONE',  ( 1.000000000000000000, -0.000000000000000000, -0.000000000000000000 ) ) ;
#252969 = DIRECTION ( 'NONE',  ( -0.000000000000000000, 0.9667078373770112698, 0.2558827019434132821 ) ) ;
#252970 = EDGE_CURVE ( 'NONE', #160790, #149361, #69319, .T. ) ;
#252971 = AXIS2_PLACEMENT_3D ( 'NONE', #252875, #89951, #151232 ) ;
#252972 = AXIS2_PLACEMENT_3D ( 'NONE', #202792, #241910, #141527 ) ;
#252974 = ORIENTED_EDGE ( 'NONE', *, *, #27732, .T. ) ;
#252973 = EDGE_CURVE ( 'NONE', #180226, #135449, #86992, .T. ) ;
#252975 = CARTESIAN_POINT ( 'NONE',  ( -14.00000000000000178, 9.850000000011133849, -83.75000000000004263 ) ) ;
#252978 = EDGE_LOOP ( 'NONE', ( #151993, #13777, #109814 ) ) ;
#252977 = DIRECTION ( 'NONE',  ( 0.000000000000000000, -1.000000000000000000, 0.000000000000000000 ) ) ;
#252976 = TOROIDAL_SURFACE ( 'NONE', #3164, 11.65000000000000036, 0.1000000000000000056 ) ;
#252979 = DIRECTION ( 'NONE',  ( 0.000000000000000000, 0.8814952561688476074, -0.4721928772777262417 ) ) ;
#252980 = CARTESIAN_POINT ( 'NONE',  ( -21.17356465864818560, 69.57719687377066009, -170.1220187255382541 ) ) ;
#252981 = CIRCLE ( 'NONE', #148955, 0.09999999999999939493 ) ;
#252982 = ADVANCED_FACE ( 'NONE', ( #107862 ), #24503, .F. ) ;
#252983 = CARTESIAN_POINT ( 'NONE',  ( 21.05000000000000071, 1.115600667400684642E-11, -167.4999999999999716 ) ) ;
#252984 = ORIENTED_EDGE ( 'NONE', *, *, #194278, .T. ) ;
#252985 = CARTESIAN_POINT ( 'NONE',  ( 13.99999999999999822, 13.18880795147152618, -215.2702608532411830 ) ) ;
#252986 = PRODUCT_CONTEXT ( 'NONE', #207378, 'mechanical' ) ;
#252988 = EDGE_CURVE ( 'NONE', #5597, #58739, #225222, .T. ) ;
#252987 = CARTESIAN_POINT ( 'NONE',  ( 22.40000000000020819, -2.598867842140045958, -189.5410128746470946 ) ) ;
#252989 = ORIENTED_EDGE ( 'NONE', *, *, #143997, .F. ) ;
#252990 = DIRECTION ( 'NONE',  ( 1.000000000000000000, -0.000000000000000000, -0.000000000000000000 ) ) ;
#252991 = DIRECTION ( 'NONE',  ( -0.000000000000000000, 0.4088369013363281068, -0.9126074666063770380 ) ) ;
#252992 = CIRCLE ( 'NONE', #48982, 11.90000000000000391 ) ;
#252993 = AXIS2_PLACEMENT_3D ( 'NONE', #61551, #242735, #227031 ) ;
#252994 = CIRCLE ( 'NONE', #44898, 0.9000000000000014655 ) ;
#252995 = CARTESIAN_POINT ( 'NONE',  ( -22.50000000000000000, 0.3085173699977072914, -229.9658011520297691 ) ) ;
#252996 = ORIENTED_EDGE ( 'NONE', *, *, #165966, .F. ) ;
#252997 = EDGE_LOOP ( 'NONE', ( #11147, #110984, #2378, #198430 ) ) ;
#252998 = LINE ( 'NONE', #74411, #142329 ) ;
#252999 = EDGE_CURVE ( 'NONE', #44597, #83361, #115086, .T. ) ;
#253000 = CARTESIAN_POINT ( 'NONE',  ( -22.50000000000000000, 11.75000000000000000, -3.469446951953614189E-15 ) ) ;
#253002 = AXIS2_PLACEMENT_3D ( 'NONE', #57265, #101509, #39029 ) ;
#253001 = CARTESIAN_POINT ( 'NONE',  ( 21.05000000000000071, 1.115600667400684642E-11, -33.50000000000000000 ) ) ;
#253003 = CARTESIAN_POINT ( 'NONE',  ( -17.05016517656507347, 30.18632038432621201, -234.7963271727524557 ) ) ;
#253004 = VECTOR ( 'NONE', #48294, 1000.000000000000000 ) ;
#253006 = CARTESIAN_POINT ( 'NONE',  ( -18.40000000000000213, 64.52132590001231449, -145.7978007008650252 ) ) ;
#253005 = CARTESIAN_POINT ( 'NONE',  ( 21.14999999999999503, -1.391858308744749806, -194.6091531227728240 ) ) ;
#253007 = CARTESIAN_POINT ( 'NONE',  ( -21.08884785362073089, 75.95021690494570521, -176.3803008519499826 ) ) ;
#253008 = AXIS2_PLACEMENT_3D ( 'NONE', #200080, #116680, #176682 ) ;
#253009 = DIRECTION ( 'NONE',  ( 0.7071067811865127117, 0.7071067811865821007, 0.000000000000000000 ) ) ;
#253010 = FACE_OUTER_BOUND ( 'NONE', #163823, .T. ) ;
#253011 = CARTESIAN_POINT ( 'NONE',  ( -16.87036670365549895, 12.42497885867826390, -211.1079079717509046 ) ) ;
#253012 = ORIENTED_EDGE ( 'NONE', *, *, #143468, .F. ) ;
#253013 = EDGE_LOOP ( 'NONE', ( #236032, #119249, #25699, #17736 ) ) ;
#253014 = DIRECTION ( 'NONE',  ( -4.391705002472927119E-16, -1.000000000000000000, -7.026728003956683390E-15 ) ) ;
#253015 = DIRECTION ( 'NONE',  ( 0.000000000000000000, -0.9274965247785323941, -0.3738317757009769760 ) ) ;
#253017 = CARTESIAN_POINT ( 'NONE',  ( -21.14999999999999503, 11.75000000001115197, -140.9191472459588113 ) ) ;
#253016 = DIRECTION ( 'NONE',  ( 2.715809747126116508E-16, 0.4088369013363282178, -0.9126074666063770380 ) ) ;
#253018 = VECTOR ( 'NONE', #230100, 1000.000000000000000 ) ;
#253019 = EDGE_CURVE ( 'NONE', #39812, #247339, #7480, .T. ) ;
#253020 = ORIENTED_EDGE ( 'NONE', *, *, #225082, .F. ) ;
#253021 = CARTESIAN_POINT ( 'NONE',  ( 18.49999999999999289, 6.650000000011155876, -88.35000000000003695 ) ) ;
#253022 = DIRECTION ( 'NONE',  ( 0.000000000000000000, 0.000000000000000000, -1.000000000000000000 ) ) ;
#253023 = CARTESIAN_POINT ( 'NONE',  ( 15.39170923737820473, 12.96596579538267946, -216.4109158611323949 ) ) ;
#253024 = VERTEX_POINT ( 'NONE', #206972 ) ;
#253025 = VERTEX_POINT ( 'NONE', #222664 ) ;
#253026 = CIRCLE ( 'NONE', #198858, 0.1000000000000028644 ) ;
#253027 = CARTESIAN_POINT ( 'NONE',  ( -18.39999999999999858, -9.599999999988849453, -73.60018939122203108 ) ) ;
#253028 = AXIS2_PLACEMENT_3D ( 'NONE', #212039, #198872, #200169 ) ;
#253029 = ORIENTED_EDGE ( 'NONE', *, *, #137755, .F. ) ;
#253030 = EDGE_CURVE ( 'NONE', #54007, #243260, #102575, .T. ) ;
#253031 = DIRECTION ( 'NONE',  ( 0.000000000000000000, 0.2128009952263485993, -0.9770955615653341697 ) ) ;
#253032 = CIRCLE ( 'NONE', #140595, 0.8750000000000007772 ) ;
#253033 = ADVANCED_FACE ( 'NONE', ( #4885 ), #103988, .T. ) ;
#253034 = DIRECTION ( 'NONE',  ( 0.000000000000000000, 0.9126074666063660468, 0.4088369013363524762 ) ) ;
#253035 = LINE ( 'NONE', #229634, #239969 ) ;
#253036 = ORIENTED_EDGE ( 'NONE', *, *, #179573, .F. ) ;
#253037 = CARTESIAN_POINT ( 'NONE',  ( -20.54999999999999716, 7.554435330547284444, -235.6868924355707691 ) ) ;
#253038 = EDGE_CURVE ( 'NONE', #151077, #242911, #47117, .T. ) ;
#253039 = DIRECTION ( 'NONE',  ( -0.000000000000000000, -6.982962677686266711E-15, 1.000000000000000000 ) ) ;
#253040 = CARTESIAN_POINT ( 'NONE',  ( 21.05000000000000426, 0.03486800302426364129, -27.22991413631085678 ) ) ;
#253041 = CIRCLE ( 'NONE', #240577, 0.6000000000000033085 ) ;
#253042 = ADVANCED_FACE ( 'NONE', ( #183564 ), #195138, .T. ) ;
#253043 = CARTESIAN_POINT ( 'NONE',  ( 23.04999999999999716, 8.822561741677553471, -79.65000000000004832 ) ) ;
#253044 = EDGE_CURVE ( 'NONE', #22444, #154058, #135912, .T. ) ;
#253045 = DIRECTION ( 'NONE',  ( 0.000000000000000000, 0.000000000000000000, -1.000000000000000000 ) ) ;
#253047 = CARTESIAN_POINT ( 'NONE',  ( -16.97683809663752186, 9.850000000011137402, -87.09763598180373378 ) ) ;
#253046 = CARTESIAN_POINT ( 'NONE',  ( 20.85000000000000142, 76.00000000001213607, -136.5231074845243313 ) ) ;
#253048 = DIRECTION ( 'NONE',  ( 0.000000000000000000, -0.8660254037844377084, -0.5000000000000016653 ) ) ;
#253049 = ORIENTED_EDGE ( 'NONE', *, *, #28260, .F. ) ;
#253051 = DIRECTION ( 'NONE',  ( 0.000000000000000000, 0.8855159391400492241, -0.4646089985449236570 ) ) ;
#253050 = FACE_OUTER_BOUND ( 'NONE', #209929, .T. ) ;
#253052 = ORIENTED_EDGE ( 'NONE', *, *, #181833, .F. ) ;
#253054 = ORIENTED_EDGE ( 'NONE', *, *, #15154, .T. ) ;
#253053 = CARTESIAN_POINT ( 'NONE',  ( 23.14999999999999858, 76.00000000001244871, -170.0231074845243597 ) ) ;
#253055 = ORIENTED_EDGE ( 'NONE', *, *, #33845, .F. ) ;
#253056 = CARTESIAN_POINT ( 'NONE',  ( -22.10000000000000142, -11.65000000000000036, 32.89999999999999858 ) ) ;
#253057 = CARTESIAN_POINT ( 'NONE',  ( 15.31784899511108655, 66.60336962369454739, -152.1160500917061427 ) ) ;
#253058 = DIRECTION ( 'NONE',  ( -2.561896900575096011E-15, -0.7489048840758921743, 0.6626775042260560911 ) ) ;
#253059 = ADVANCED_FACE ( 'NONE', ( #230385 ), #210823, .F. ) ;
#253060 = PLANE ( 'NONE',  #62648 ) ;
#253061 = EDGE_LOOP ( 'NONE', ( #204277, #83753, #233483, #195413 ) ) ;
#253062 = CARTESIAN_POINT ( 'NONE',  ( 21.11345278033283179, 8.882122073382040739, -112.7460221707548698 ) ) ;
#253063 = ORIENTED_EDGE ( 'NONE', *, *, #220734, .T. ) ;
#253064 = DIRECTION ( 'NONE',  ( 0.000000000000000000, 0.000000000000000000, -1.000000000000000000 ) ) ;
#253065 = CARTESIAN_POINT ( 'NONE',  ( -23.25000000000000000, 64.35000000001275566, -215.2731074845244450 ) ) ;
#253066 = ORIENTED_EDGE ( 'NONE', *, *, #249198, .F. ) ;
#253067 = CIRCLE ( 'NONE', #149049, 0.1000000000000028644 ) ;
#253068 = CYLINDRICAL_SURFACE ( 'NONE', #97881, 0.09999999999999939493 ) ;
#253069 = ORIENTED_EDGE ( 'NONE', *, *, #255650, .T. ) ;
#253070 = CARTESIAN_POINT ( 'NONE',  ( 18.45068634130097607, -9.486506073331600675, -141.0687784311681128 ) ) ;
#253071 = ORIENTED_EDGE ( 'NONE', *, *, #81242, .T. ) ;
#253072 = LINE ( 'NONE', #155305, #5250 ) ;
#253073 = EDGE_CURVE ( 'NONE', #12212, #211228, #119184, .T. ) ;
#253074 = CYLINDRICAL_SURFACE ( 'NONE', #135537, 0.09999999999999986677 ) ;
#253075 = CARTESIAN_POINT ( 'NONE',  ( 21.05000000000000071, 60.83337574417770810, -225.3422414619149095 ) ) ;
#253076 = ADVANCED_FACE ( 'NONE', ( #212119 ), #231686, .F. ) ;
#253077 = CARTESIAN_POINT ( 'NONE',  ( 23.25000000000000000, -11.74999999998883560, -63.89999999999999858 ) ) ;
#253078 = CIRCLE ( 'NONE', #219755, 0.09999999999998898659 ) ;
#253079 = EDGE_CURVE ( 'NONE', #111919, #105079, #23552, .T. ) ;
#253081 = CIRCLE ( 'NONE', #257313, 0.1000000000000033223 ) ;
#253080 = CARTESIAN_POINT ( 'NONE',  ( -20.94999999999999929, 69.19063053712525857, -247.5666987377248631 ) ) ;
#253082 = CARTESIAN_POINT ( 'NONE',  ( 23.15000000000000213, 69.16514130714681130, -247.7543978865853660 ) ) ;
#253083 = FACE_OUTER_BOUND ( 'NONE', #73525, .T. ) ;
#253084 = VERTEX_POINT ( 'NONE', #53021 ) ;
#253086 = CARTESIAN_POINT ( 'NONE',  ( 23.15000000000000213, -11.64999999999999147, -30.39999999999999503 ) ) ;
#253085 = DIRECTION ( 'NONE',  ( 0.000000000000000000, -0.9126074666063769270, -0.4088369013363280513 ) ) ;
#253087 = ORIENTED_EDGE ( 'NONE', *, *, #57178, .F. ) ;
#253091 = EDGE_LOOP ( 'NONE', ( #125387, #152934, #208864, #21788, #47061 ) ) ;
#253090 =( BOUNDED_CURVE ( )  B_SPLINE_CURVE ( 3, ( #2877, #84964, #246631, #104529 ),
 .UNSPECIFIED., .F., .T. ) 
 B_SPLINE_CURVE_WITH_KNOTS ( ( 4, 4 ),
 ( 5.731445031868799056, 5.983100554402348337 ),
 .UNSPECIFIED. ) 
 CURVE ( )  GEOMETRIC_REPRESENTATION_ITEM ( )  RATIONAL_B_SPLINE_CURVE ( ( 1.000000000000000000, 0.9947294176030464508, 0.9947294176030464508, 1.000000000000000000 ) ) 
 REPRESENTATION_ITEM ( '' )  );
#253089 = CARTESIAN_POINT ( 'NONE',  ( 21.00000000000000000, 9.749999999999998224, -21.25000000000000000 ) ) ;
#253088 = DIRECTION ( 'NONE',  ( 0.000000000000000000, 0.8814952561688430555, -0.4721928772777346239 ) ) ;
#253092 = ORIENTED_EDGE ( 'NONE', *, *, #50951, .F. ) ;
#253093 = CARTESIAN_POINT ( 'NONE',  ( 11.60000000000006182, 67.75000000001118394, -18.42310748452479530 ) ) ;
#253094 = CARTESIAN_POINT ( 'NONE',  ( 21.05000000000000071, 1.115486826172573664E-11, -60.45934304829880546 ) ) ;
#253095 = DIRECTION ( 'NONE',  ( -1.000000000000000000, -8.855395344894292773E-17, -1.653135691717061729E-16 ) ) ;
#253096 = LINE ( 'NONE', #28976, #208395 ) ;
#253097 = ORIENTED_EDGE ( 'NONE', *, *, #79613, .T. ) ;
#253099 = VERTEX_POINT ( 'NONE', #54300 ) ;
#253098 = CARTESIAN_POINT ( 'NONE',  ( -16.86733706339143524, 66.03400947037232527, -115.6199921825256638 ) ) ;
#253101 = CARTESIAN_POINT ( 'NONE',  ( 20.95017935633852346, 10.47548927962532339, -7.577439797390487008 ) ) ;
#253100 = CARTESIAN_POINT ( 'NONE',  ( 21.05000000000000071, 76.00000000001139711, -32.02310748452432421 ) ) ;
#253103 = ORIENTED_EDGE ( 'NONE', *, *, #160897, .T. ) ;
#253102 = CARTESIAN_POINT ( 'NONE',  ( -20.54999999999999716, 67.23127455305841238, -235.8551265064783991 ) ) ;
#253104 = ORIENTED_EDGE ( 'NONE', *, *, #90291, .F. ) ;
#253105 = ADVANCED_FACE ( 'NONE', ( #149589 ), #54645, .T. ) ;
#253106 = AXIS2_PLACEMENT_3D ( 'NONE', #102073, #83775, #163368 ) ;
#253107 = DIRECTION ( 'NONE',  ( 0.000000000000000000, -1.411300455031978166E-14, 1.000000000000000000 ) ) ;
#253108 = ORIENTED_EDGE ( 'NONE', *, *, #194459, .T. ) ;
#253109 = DIRECTION ( 'NONE',  ( 0.000000000000000000, 0.000000000000000000, 1.000000000000000000 ) ) ;
#253110 = VERTEX_POINT ( 'NONE', #170463 ) ;
#253111 = EDGE_CURVE ( 'NONE', #149634, #246680, #131282, .T. ) ;
#253112 = CARTESIAN_POINT ( 'NONE',  ( -18.40000000000000213, 11.48667500176882861, -158.2500000000000284 ) ) ;
#253113 = DIRECTION ( 'NONE',  ( 0.000000000000000000, 0.9947597004326491632, -0.1022405907413782566 ) ) ;
#253114 = AXIS2_PLACEMENT_3D ( 'NONE', #245637, #5709, #146512 ) ;
#253115 = ORIENTED_EDGE ( 'NONE', *, *, #93825, .T. ) ;
#253116 = FACE_OUTER_BOUND ( 'NONE', #13840, .T. ) ;
#253117 = EDGE_CURVE ( 'NONE', #114510, #35657, #185814, .T. ) ;
#253118 = AXIS2_PLACEMENT_3D ( 'NONE', #155276, #13173, #74458 ) ;
#253119 = EDGE_CURVE ( 'NONE', #128152, #75854, #48449, .T. ) ;
#253120 = AXIS2_PLACEMENT_3D ( 'NONE', #106196, #207910, #127067 ) ;
#253121 = CIRCLE ( 'NONE', #165680, 0.2000000000000057288 ) ;
#253122 = CYLINDRICAL_SURFACE ( 'NONE', #222889, 0.09999999999999939493 ) ;
#253123 = B_SPLINE_CURVE_WITH_KNOTS ( 'NONE', 3,
 ( #34574, #131082, #114077, #171530, #112812, #193632, #95788, #253586, #252300, #13702, #73710, #232774, #54108, #94513, #154540, #234029 ),
 .UNSPECIFIED., .F., .F.,
 ( 4, 3, 3, 3, 3, 4 ),
 ( 0.000000000000000000, 2.372700795694929318E-05, 5.739057815867159087E-05, 9.073899019181866019E-05, 0.0001243544287365815515, 0.0001585386695601353146 ),
 .UNSPECIFIED. ) ;
#253124 = TOROIDAL_SURFACE ( 'NONE', #165681, 0.2000000000000000111, 0.1000000000000000056 ) ;
#253125 = ORIENTED_EDGE ( 'NONE', *, *, #234376, .F. ) ;
#253126 = EDGE_CURVE ( 'NONE', #216303, #167394, #169300, .T. ) ;
#253127 = ORIENTED_EDGE ( 'NONE', *, *, #25293, .F. ) ;
#253128 = VERTEX_POINT ( 'NONE', #115567 ) ;
#253132 = EDGE_CURVE ( 'NONE', #66177, #170483, #139999, .T. ) ;
#253131 = EDGE_CURVE ( 'NONE', #231902, #147657, #190114, .T. ) ;
#253130 = CARTESIAN_POINT ( 'NONE',  ( 18.60000000000000853, -9.364236010355611484, -107.6802544007246354 ) ) ;
#253129 = CIRCLE ( 'NONE', #28322, 0.3999999999999926392 ) ;
#253133 = ORIENTED_EDGE ( 'NONE', *, *, #236787, .T. ) ;
#253134 = AXIS2_PLACEMENT_3D ( 'NONE', #236586, #198751, #137480 ) ;
#253135 = VERTEX_POINT ( 'NONE', #78977 ) ;
#253137 = ORIENTED_EDGE ( 'NONE', *, *, #90525, .F. ) ;
#253136 = DIRECTION ( 'NONE',  ( 0.000000000000000000, 0.000000000000000000, 1.000000000000000000 ) ) ;
#253138 =( BOUNDED_CURVE ( )  B_SPLINE_CURVE ( 3, ( #69216, #84857, #104433, #90023 ),
 .UNSPECIFIED., .F., .F. ) 
 B_SPLINE_CURVE_WITH_KNOTS ( ( 4, 4 ),
 ( 3.141592653589793116, 4.712388980384689674 ),
 .UNSPECIFIED. ) 
 CURVE ( )  GEOMETRIC_REPRESENTATION_ITEM ( )  RATIONAL_B_SPLINE_CURVE ( ( 1.000000000000000000, 0.8047378541243649375, 0.8047378541243649375, 1.000000000000000000 ) ) 
 REPRESENTATION_ITEM ( '' )  );
#253139 = EDGE_LOOP ( 'NONE', ( #39566, #255668, #131829, #34766 ) ) ;
#253140 = CYLINDRICAL_SURFACE ( 'NONE', #72563, 2.000000000000001776 ) ;
#253141 = ORIENTED_EDGE ( 'NONE', *, *, #180682, .F. ) ;
#253144 = ORIENTED_EDGE ( 'NONE', *, *, #182304, .T. ) ;
#253143 = VERTEX_POINT ( 'NONE', #196383 ) ;
#253142 = CARTESIAN_POINT ( 'NONE',  ( 20.04142135623731136, 11.75000000001116085, -192.2671572875253219 ) ) ;
#253146 = ORIENTED_EDGE ( 'NONE', *, *, #179227, .F. ) ;
#253145 = TOROIDAL_SURFACE ( 'NONE', #203273, 0.4000000000000012990, 0.1000000000000000056 ) ;
#253147 = ADVANCED_FACE ( 'NONE', ( #238075 ), #40103, .T. ) ;
#253149 = EDGE_CURVE ( 'NONE', #168221, #9791, #206669, .T. ) ;
#253148 = TOROIDAL_SURFACE ( 'NONE', #7448, 3.899999999999999467, 0.1000000000000000056 ) ;
#253150 = CIRCLE ( 'NONE', #170012, 2.000000000000001776 ) ;
#253151 = CARTESIAN_POINT ( 'NONE',  ( 21.12802099929860944, 8.780552590233368093, -45.74818998493161359 ) ) ;
#253152 = AXIS2_PLACEMENT_3D ( 'NONE', #165965, #9419, #245487 ) ;
#253153 = ORIENTED_EDGE ( 'NONE', *, *, #204103, .F. ) ;
#253154 = CIRCLE ( 'NONE', #36720, 0.5000000000000004441 ) ;
#253155 = EDGE_CURVE ( 'NONE', #126571, #151965, #58138, .T. ) ;
#253156 = CARTESIAN_POINT ( 'NONE',  ( -18.59999999999999787, 7.021664781911246322, -171.2335654018973230 ) ) ;
#253158 = ORIENTED_EDGE ( 'NONE', *, *, #116143, .T. ) ;
#253157 = DIRECTION ( 'NONE',  ( 1.000000000000000000, -0.000000000000000000, -0.000000000000000000 ) ) ;
#253159 = CARTESIAN_POINT ( 'NONE',  ( 20.94999999999999929, 4.813084112160680661, -45.44151775652382952 ) ) ;
#253160 = ORIENTED_EDGE ( 'NONE', *, *, #209129, .T. ) ;
#253161 = AXIS2_PLACEMENT_3D ( 'NONE', #248638, #205646, #131254 ) ;
#253162 = ORIENTED_EDGE ( 'NONE', *, *, #79356, .F. ) ;
#253164 = EDGE_CURVE ( 'NONE', #224621, #8217, #159853, .T. ) ;
#253163 = DIRECTION ( 'NONE',  ( 0.000000000000000000, -1.734723475976757554E-14, -1.000000000000000000 ) ) ;
#253165 = ORIENTED_EDGE ( 'NONE', *, *, #217386, .T. ) ;
#253166 = ADVANCED_FACE ( 'NONE', ( #221077 ), #240000, .T. ) ;
#253167 = EDGE_LOOP ( 'NONE', ( #173699, #207497, #132152, #32101 ) ) ;
#253168 = LINE ( 'NONE', #74585, #235910 ) ;
#253169 = CIRCLE ( 'NONE', #240152, 0.09999999999999939493 ) ;
#253170 = AXIS2_PLACEMENT_3D ( 'NONE', #254674, #236436, #119071 ) ;
#253171 = AXIS2_PLACEMENT_3D ( 'NONE', #14728, #89093, #128234 ) ;
#253173 = ORIENTED_EDGE ( 'NONE', *, *, #232325, .F. ) ;
#253172 = ORIENTED_EDGE ( 'NONE', *, *, #21198, .T. ) ;
#253174 = EDGE_LOOP ( 'NONE', ( #167298, #173859, #39221, #204392, #61493, #233994, #236857, #116855, #220669, #34679, #111108, #58119, #82530, #28997, #224238, #98455, #68847, #97578, #109171, #101261, #44413, #27474, #18992 ) ) ;
#253175 = DIRECTION ( 'NONE',  ( 0.000000000000000000, 0.8814952561688438326, -0.4721928772777330696 ) ) ;
#253176 = EDGE_LOOP ( 'NONE', ( #151546, #240649, #9946, #158297, #220172, #193908, #199339, #153292, #3532, #175916 ) ) ;
#253177 = ORIENTED_EDGE ( 'NONE', *, *, #143355, .F. ) ;
#253178 = DIRECTION ( 'NONE',  ( 1.000000000000000000, 0.000000000000000000, 0.000000000000000000 ) ) ;
#253179 = ORIENTED_EDGE ( 'NONE', *, *, #198049, .T. ) ;
#253180 = ADVANCED_FACE ( 'NONE', ( #158577 ), #98524, .T. ) ;
#253181 = DIRECTION ( 'NONE',  ( 0.000000000000000000, -1.000000000000000000, -6.982962677686266711E-15 ) ) ;
#253182 = DIRECTION ( 'NONE',  ( -1.000000000000000000, 0.000000000000000000, 0.000000000000000000 ) ) ;
#253183 = ORIENTED_EDGE ( 'NONE', *, *, #18954, .T. ) ;
#253184 = CIRCLE ( 'NONE', #45082, 0.5000000000000004441 ) ;
#253185 = AXIS2_PLACEMENT_3D ( 'NONE', #1128, #61124, #130076 ) ;
#253186 = VERTEX_POINT ( 'NONE', #97246 ) ;
#253187 = EDGE_CURVE ( 'NONE', #184662, #136469, #127566, .T. ) ;
#253188 = DIRECTION ( 'NONE',  ( -0.000000000000000000, -6.982962677686266711E-15, 1.000000000000000000 ) ) ;
#253189 = TOROIDAL_SURFACE ( 'NONE', #136657, 0.2000000000000000111, 0.1000000000000000056 ) ;
#253190 = ORIENTED_EDGE ( 'NONE', *, *, #192194, .T. ) ;
#253191 = CIRCLE ( 'NONE', #28384, 0.1000000000000024342 ) ;
#253192 = DIRECTION ( 'NONE',  ( -1.000000000000000000, 0.000000000000000000, 0.000000000000000000 ) ) ;
#253193 = ORIENTED_EDGE ( 'NONE', *, *, #194030, .T. ) ;
#253194 = VERTEX_POINT ( 'NONE', #60714 ) ;
#253195 = CARTESIAN_POINT ( 'NONE',  ( -21.64999999999999858, 10.05000000001113847, -146.6500000000000341 ) ) ;
#253196 = EDGE_CURVE ( 'NONE', #10002, #61748, #223226, .T. ) ;
#253198 = EDGE_LOOP ( 'NONE', ( #229447, #28330 ) ) ;
#253197 = FACE_OUTER_BOUND ( 'NONE', #15194, .T. ) ;
#253199 = DIRECTION ( 'NONE',  ( 2.694716079187272946E-16, -1.000000000000000000, 0.000000000000000000 ) ) ;
#253200 = CARTESIAN_POINT ( 'NONE',  ( -20.94999999999999929, 76.00000000001195133, -103.0231074845243171 ) ) ;
#253201 = AXIS2_PLACEMENT_3D ( 'NONE', #220131, #121057, #166597 ) ;
#253202 = DIRECTION ( 'NONE',  ( 0.000000000000000000, -0.000000000000000000, 1.000000000000000000 ) ) ;
#253203 = DIRECTION ( 'NONE',  ( 1.000000000000000000, 0.000000000000000000, 0.000000000000000000 ) ) ;
#253204 = CARTESIAN_POINT ( 'NONE',  ( -20.94999999999999929, 62.46832465249013921, -225.2232495205141731 ) ) ;
#253205 = CARTESIAN_POINT ( 'NONE',  ( -23.25000000000000000, -9.682403433476396870, -40.15684337741279109 ) ) ;
#253206 = DIRECTION ( 'NONE',  ( 0.000000000000000000, 1.000000000000000000, 0.000000000000000000 ) ) ;
#253208 = TOROIDAL_SURFACE ( 'NONE', #111572, 0.2000000000000000111, 0.1000000000000000056 ) ;
#253207 = CARTESIAN_POINT ( 'NONE',  ( 18.79999999999999361, -11.65000000000000036, -15.00000000000000000 ) ) ;
#253209 = AXIS2_PLACEMENT_3D ( 'NONE', #166080, #104748, #26550 ) ;
#253210 = DIRECTION ( 'NONE',  ( 1.000000000000000000, 2.952720810173289112E-16, -0.000000000000000000 ) ) ;
#253211 = DIRECTION ( 'NONE',  ( -1.000000000000000000, 0.000000000000000000, 0.000000000000000000 ) ) ;
#253213 = CARTESIAN_POINT ( 'NONE',  ( 18.49999999999999289, 33.98796489282361932, -236.2185561567993091 ) ) ;
#253212 = AXIS2_PLACEMENT_3D ( 'NONE', #52185, #54760, #134288 ) ;
#253215 = ORIENTED_EDGE ( 'NONE', *, *, #134582, .F. ) ;
#253214 = VECTOR ( 'NONE', #220152, 1000.000000000000000 ) ;
#253217 = ORIENTED_EDGE ( 'NONE', *, *, #51991, .T. ) ;
#253216 = ORIENTED_EDGE ( 'NONE', *, *, #90496, .T. ) ;
#253218 = ORIENTED_EDGE ( 'NONE', *, *, #77853, .F. ) ;
#253219 = CARTESIAN_POINT ( 'NONE',  ( 23.50000000000005684, 62.43959356634987046, -37.55748533175129467 ) ) ;
#253220 = DIRECTION ( 'NONE',  ( 0.000000000000000000, 1.000000000000000000, 0.000000000000000000 ) ) ;
#253222 = DIRECTION ( 'NONE',  ( 0.000000000000000000, -0.7106264324241465813, 0.7035695228903323661 ) ) ;
#253221 = DIRECTION ( 'NONE',  ( -1.000000000000000000, 0.000000000000000000, 0.000000000000000000 ) ) ;
#253223 = ORIENTED_EDGE ( 'NONE', *, *, #243411, .F. ) ;
#253224 = ORIENTED_EDGE ( 'NONE', *, *, #132477, .F. ) ;
#253225 = VECTOR ( 'NONE', #161677, 1000.000000000000000 ) ;
#253226 = CARTESIAN_POINT ( 'NONE',  ( -18.50000000000000000, 13.44116543737180081, -219.7184420207870801 ) ) ;
#253227 = CARTESIAN_POINT ( 'NONE',  ( -21.05000000000000071, -1.851028230129704522, -179.1539132694224463 ) ) ;
#253228 = CARTESIAN_POINT ( 'NONE',  ( 20.85000000000000142, 62.46832465249013921, -225.2232495205141731 ) ) ;
#253229 = ORIENTED_EDGE ( 'NONE', *, *, #111114, .F. ) ;
#253230 = EDGE_LOOP ( 'NONE', ( #145274, #138385, #154681, #69517, #140378, #64018, #101480, #51601, #251779, #169120, #80167, #92381 ) ) ;
#253231 = VECTOR ( 'NONE', #62574, 1000.000000000000000 ) ;
#253232 = DIRECTION ( 'NONE',  ( -0.000000000000000000, 6.982962677686266711E-15, -1.000000000000000000 ) ) ;
#253233 = DIRECTION ( 'NONE',  ( -1.000000000000000000, 0.000000000000000000, 0.000000000000000000 ) ) ;
#253234 = ORIENTED_EDGE ( 'NONE', *, *, #161467, .T. ) ;
#253235 = LINE ( 'NONE', #217949, #207888 ) ;
#253237 = ORIENTED_EDGE ( 'NONE', *, *, #30240, .F. ) ;
#253236 = FACE_OUTER_BOUND ( 'NONE', #217924, .T. ) ;
#253238 = CARTESIAN_POINT ( 'NONE',  ( -18.39999999999999858, 8.812838127540084443, -245.4119190891508708 ) ) ;
#253239 = CARTESIAN_POINT ( 'NONE',  ( -18.50000000000000000, 64.25000000001254818, -182.1731074845244507 ) ) ;
#253240 = DIRECTION ( 'NONE',  ( 0.000000000000000000, 0.000000000000000000, -1.000000000000000000 ) ) ;
#253241 = VERTEX_POINT ( 'NONE', #116856 ) ;
#253242 = DIRECTION ( 'NONE',  ( 0.000000000000000000, 1.000000000000000000, 0.000000000000000000 ) ) ;
#253243 = CARTESIAN_POINT ( 'NONE',  ( -18.39999999999999858, -9.400000000000005684, 11.75000000000000000 ) ) ;
#253244 = DIRECTION ( 'NONE',  ( 0.000000000000000000, -0.1575844902526579161, -0.9875055080513779338 ) ) ;
#253246 = CARTESIAN_POINT ( 'NONE',  ( 20.85000000000000142, 86.58125133469154378, -209.3975964148341973 ) ) ;
#253245 = LINE ( 'NONE', #214138, #190987 ) ;
#253248 = EDGE_CURVE ( 'NONE', #52715, #192523, #140246, .T. ) ;
#253247 = CARTESIAN_POINT ( 'NONE',  ( -20.54999999999999716, -8.999999999988844479, -90.60603087734760663 ) ) ;
#253249 = LINE ( 'NONE', #135863, #66643 ) ;
#253250 = CIRCLE ( 'NONE', #74230, 7.720710678118662074 ) ;
#253251 = CIRCLE ( 'NONE', #120022, 0.09999999999999939493 ) ;
#253252 = CARTESIAN_POINT ( 'NONE',  ( 18.54286124688534443, 85.62391757881020737, -163.2819051526615510 ) ) ;
#253253 = DIRECTION ( 'NONE',  ( 0.000000000000000000, -0.8777080977375715243, 0.4791956752370512551 ) ) ;
#253254 = AXIS2_PLACEMENT_3D ( 'NONE', #191109, #249774, #171554 ) ;
#253255 = ORIENTED_EDGE ( 'NONE', *, *, #42198, .F. ) ;
#253256 = ORIENTED_EDGE ( 'NONE', *, *, #240521, .T. ) ;
#253257 = DIRECTION ( 'NONE',  ( -0.000000000000000000, 1.000000000000000000, 6.982962677686266711E-15 ) ) ;
#253258 = CARTESIAN_POINT ( 'NONE',  ( -21.30740335185486245, 75.90106547423633288, -143.0797654065522977 ) ) ;
#253259 = ORIENTED_EDGE ( 'NONE', *, *, #225547, .F. ) ;
#253260 = FACE_OUTER_BOUND ( 'NONE', #23872, .T. ) ;
#253261 = ADVANCED_FACE ( 'NONE', ( #217217 ), #38606, .T. ) ;
#253262 = ORIENTED_EDGE ( 'NONE', *, *, #28288, .T. ) ;
#253263 = AXIS2_PLACEMENT_3D ( 'NONE', #41021, #180514, #81368 ) ;
#253264 = VECTOR ( 'NONE', #9311, 1000.000000000000000 ) ;
#253265 = VERTEX_POINT ( 'NONE', #77707 ) ;
#253266 = CARTESIAN_POINT ( 'NONE',  ( 22.32929514600007792, 7.578647565387638174, -66.90092432188612293 ) ) ;
#253267 = ORIENTED_EDGE ( 'NONE', *, *, #177174, .T. ) ;
#253268 = AXIS2_PLACEMENT_3D ( 'NONE', #131337, #68818, #51782 ) ;
#253269 = CARTESIAN_POINT ( 'NONE',  ( 21.05000000000000071, -9.499999999988844479, -57.10603087734755690 ) ) ;
#253270 = FACE_OUTER_BOUND ( 'NONE', #230483, .T. ) ;
#253271 = CARTESIAN_POINT ( 'NONE',  ( 20.94999999999999929, 77.34915357198789820, -95.23561014893439847 ) ) ;
#253272 = EDGE_CURVE ( 'NONE', #10849, #122787, #164970, .T. ) ;
#253273 = DIRECTION ( 'NONE',  ( 0.000000000000000000, 0.9856811345164800953, 0.1686199900910462790 ) ) ;
#253274 = EDGE_CURVE ( 'NONE', #236886, #117760, #240653, .T. ) ;
#253275 = LINE ( 'NONE', #39408, #57973 ) ;
#253277 = ORIENTED_EDGE ( 'NONE', *, *, #207799, .T. ) ;
#253276 = LINE ( 'NONE', #249454, #50928 ) ;
#253279 = CARTESIAN_POINT ( 'NONE',  ( 19.75857864376269291, 11.75000000001116263, -192.3499999999999659 ) ) ;
#253278 = CARTESIAN_POINT ( 'NONE',  ( 21.05000000000000071, 6.285328434420313748, -199.7189328463573190 ) ) ;
#253280 = DIRECTION ( 'NONE',  ( 0.000000000000000000, -0.2605042016806740079, 0.9654727137038698892 ) ) ;
#253281 = CARTESIAN_POINT ( 'NONE',  ( 21.05000000000000071, 64.25000000001146816, -43.03791325517834565 ) ) ;
#253283 = EDGE_CURVE ( 'NONE', #168869, #179511, #210757, .T. ) ;
#253282 = DIRECTION ( 'NONE',  ( 1.000000000000000000, 7.304098846218134667E-16, 0.000000000000000000 ) ) ;
#253284 = CYLINDRICAL_SURFACE ( 'NONE', #216825, 0.09999999999998898659 ) ;
#253285 = ORIENTED_EDGE ( 'NONE', *, *, #107610, .T. ) ;
#253286 = DIRECTION ( 'NONE',  ( 0.000000000000000000, -1.265107689135680095E-16, 1.000000000000000000 ) ) ;
#253287 = ADVANCED_FACE ( 'NONE', ( #39917, #17732 ), #62030, .T. ) ;
#253288 = EDGE_LOOP ( 'NONE', ( #158329, #12171, #62274, #254319 ) ) ;
#253289 = AXIS2_PLACEMENT_3D ( 'NONE', #109244, #53131, #128834 ) ;
#253290 = FACE_OUTER_BOUND ( 'NONE', #184214, .T. ) ;
#253291 = VERTEX_POINT ( 'NONE', #215936 ) ;
#253292 = AXIS2_PLACEMENT_3D ( 'NONE', #190651, #12011, #94079 ) ;
#253293 = VECTOR ( 'NONE', #179600, 1000.000000000000000 ) ;
#253294 = DIRECTION ( 'NONE',  ( 1.000000000000000000, 3.265361837132813093E-16, -0.000000000000000000 ) ) ;
#253295 = ADVANCED_FACE ( 'NONE', ( #102391 ), #255013, .T. ) ;
#253296 = CARTESIAN_POINT ( 'NONE',  ( -21.65000000000000213, 7.708578643773852157, -146.2500000000000284 ) ) ;
#253297 = CARTESIAN_POINT ( 'NONE',  ( -18.39999999999999858, -9.682403433465239573, -73.65684337741279819 ) ) ;
#253298 = ORIENTED_EDGE ( 'NONE', *, *, #242091, .F. ) ;
#253299 = VECTOR ( 'NONE', #253329, 1000.000000000000000 ) ;
#253300 = B_SPLINE_CURVE_WITH_KNOTS ( 'NONE', 3,
 ( #62828, #204890, #146204, #184054, #225727, #105776, #5390, #186644, #84921, #164512, #47092, #65393, #144914, #101925, #126653, #8005, #82357, #142357, #11870, #191795, #9272, #112245, #133081, #249183, #70566, #169680, #212624, #10571, #151375, #148797 ),
 .UNSPECIFIED., .F., .F.,
 ( 4, 2, 2, 2, 2, 2, 2, 2, 2, 2, 2, 2, 2, 2, 4 ),
 ( 0.000000000000000000, 0.0003422764154113342653, 0.0006845528308226685307, 0.001026829246234002742, 0.001369105661645337061, 0.002053658492468007218, 0.002738211323290677159, 0.003080487738702009527, 0.003422764154113341895, 0.003765040569524674696, 0.004107316984936006631, 0.004449593400347339432, 0.004791869815758671367, 0.005134146231170004168, 0.005476422646581336103 ),
 .UNSPECIFIED. ) ;
#253301 = VERTEX_POINT ( 'NONE', #202807 ) ;
#253302 = EDGE_CURVE ( 'NONE', #135981, #121455, #227501, .T. ) ;
#253303 = DIRECTION ( 'NONE',  ( 0.000000000000000000, 0.000000000000000000, 1.000000000000000000 ) ) ;
#253304 = PLANE ( 'NONE',  #181777 ) ;
#253305 = FACE_OUTER_BOUND ( 'NONE', #28472, .T. ) ;
#253306 = DIRECTION ( 'NONE',  ( -0.000000000000000000, -0.9126074666063770380, -0.4088369013363282178 ) ) ;
#253308 = CARTESIAN_POINT ( 'NONE',  ( 21.00000000000000000, 30.37633856152204359, -235.1250019192171408 ) ) ;
#253307 = LINE ( 'NONE', #29183, #92651 ) ;
#253309 = VECTOR ( 'NONE', #189312, 1000.000000000000000 ) ;
#253311 = CARTESIAN_POINT ( 'NONE',  ( 21.07928932188134397, 6.328516656404459262, -167.4011048543455615 ) ) ;
#253310 = AXIS2_PLACEMENT_3D ( 'NONE', #251970, #14680, #158062 ) ;
#253312 = CARTESIAN_POINT ( 'NONE',  ( 12.84435279558019793, 9.410708747058235346, -51.56920840584410826 ) ) ;
#253313 = CARTESIAN_POINT ( 'NONE',  ( 21.05000000000000071, 30.89539159176859684, -252.1742849677607978 ) ) ;
#253314 = AXIS2_PLACEMENT_3D ( 'NONE', #188296, #205279, #106174 ) ;
#253315 = ORIENTED_EDGE ( 'NONE', *, *, #254868, .T. ) ;
#253316 = FACE_OUTER_BOUND ( 'NONE', #207162, .T. ) ;
#253318 = VERTEX_POINT ( 'NONE', #87972 ) ;
#253317 = CARTESIAN_POINT ( 'NONE',  ( -5.899999999999938183, 64.35000000001120668, -25.92310748452479174 ) ) ;
#253319 = CARTESIAN_POINT ( 'NONE',  ( 22.48660254037843842, 11.74999999999999822, 0.04999999999999833744 ) ) ;
#253320 = CIRCLE ( 'NONE', #207557, 0.1000000000000028644 ) ;
#253321 = CARTESIAN_POINT ( 'NONE',  ( 20.94999999999999574, 65.37642973952928571, -129.0311622812938310 ) ) ;
#253323 = DIRECTION ( 'NONE',  ( 0.000000000000000000, 0.9955484899852913294, -0.09425075112701486457 ) ) ;
#253322 = DIRECTION ( 'NONE',  ( 1.000000000000000000, 0.000000000000000000, 0.000000000000000000 ) ) ;
#253325 = ORIENTED_EDGE ( 'NONE', *, *, #179024, .T. ) ;
#253324 = CARTESIAN_POINT ( 'NONE',  ( 22.39999999999999147, 68.20922040163875977, -136.5231074845243597 ) ) ;
#253326 = DIRECTION ( 'NONE',  ( 0.000000000000000000, 0.000000000000000000, 1.000000000000000000 ) ) ;
#253327 = DIRECTION ( 'NONE',  ( 1.000000000000000000, 0.000000000000000000, 0.000000000000000000 ) ) ;
#253328 = CARTESIAN_POINT ( 'NONE',  ( -20.94999999999999929, -11.64999999998884483, -136.9000000000000341 ) ) ;
#253329 = DIRECTION ( 'NONE',  ( 1.000000000000000000, 7.304098846218133681E-16, -4.217023435051677501E-16 ) ) ;
#253330 = CARTESIAN_POINT ( 'NONE',  ( -20.94999999999999929, 79.33069327855442054, -236.1318330389568985 ) ) ;
#253331 = ORIENTED_EDGE ( 'NONE', *, *, #255744, .T. ) ;
#253332 = DIRECTION ( 'NONE',  ( 0.000000000000000000, 0.8700118002898356018, -0.4930308989875170078 ) ) ;
#253333 = AXIS2_PLACEMENT_3D ( 'NONE', #194351, #15717, #174810 ) ;
#253334 = ORIENTED_EDGE ( 'NONE', *, *, #171588, .T. ) ;
#253335 = DIRECTION ( 'NONE',  ( 1.000000000000000000, 0.000000000000000000, 0.000000000000000000 ) ) ;
#253336 = CIRCLE ( 'NONE', #140920, 6.329289321881370611 ) ;
#253337 = VERTEX_POINT ( 'NONE', #226188 ) ;
#253338 = CARTESIAN_POINT ( 'NONE',  ( -20.89192007715127986, 46.45729338110133710, -243.0823073233429170 ) ) ;
#253339 = AXIS2_PLACEMENT_3D ( 'NONE', #209916, #172098, #234591 ) ;
#253340 = VERTEX_POINT ( 'NONE', #4595 ) ;
#253342 = ADVANCED_FACE ( 'NONE', ( #167568 ), #48870, .F. ) ;
#253341 = B_SPLINE_CURVE_WITH_KNOTS ( 'NONE', 3,
 ( #239071, #104648, #184215, #78685, #27755, #185511 ),
 .UNSPECIFIED., .F., .F.,
 ( 4, 2, 4 ),
 ( 0.000000000000000000, 0.0001891491689349617238, 0.0003782983378699234477 ),
 .UNSPECIFIED. ) ;
#253343 = FACE_OUTER_BOUND ( 'NONE', #77176, .T. ) ;
#253346 = ADVANCED_FACE ( 'NONE', ( #24194 ), #103681, .F. ) ;
#253345 = FACE_OUTER_BOUND ( 'NONE', #53780, .T. ) ;
#253344 = CIRCLE ( 'NONE', #161614, 0.1000000000000026007 ) ;
#253347 = AXIS2_PLACEMENT_3D ( 'NONE', #121449, #180118, #183955 ) ;
#253348 = CARTESIAN_POINT ( 'NONE',  ( 23.25000000000000000, -11.65000000000000036, 3.469446951953614189E-15 ) ) ;
#253349 = ORIENTED_EDGE ( 'NONE', *, *, #202724, .F. ) ;
#253350 = EDGE_CURVE ( 'NONE', #150591, #4584, #14780, .T. ) ;
#253351 = ADVANCED_FACE ( 'NONE', ( #82824 ), #52150, .T. ) ;
#253352 = CARTESIAN_POINT ( 'NONE',  ( -23.15000000000000213, 84.59626168225447884, -45.47323500167453858 ) ) ;
#253353 = FACE_OUTER_BOUND ( 'NONE', #224779, .T. ) ;
#253354 = EDGE_CURVE ( 'NONE', #175784, #17340, #131262, .T. ) ;
#253355 = DIRECTION ( 'NONE',  ( 1.000000000000000000, 0.000000000000000000, -0.000000000000000000 ) ) ;
#253356 = DIRECTION ( 'NONE',  ( 0.000000000000000000, 0.000000000000000000, 1.000000000000000000 ) ) ;
#253357 = CARTESIAN_POINT ( 'NONE',  ( -16.91776028072577631, 66.03659960638225357, -115.6480834698222537 ) ) ;
#253358 = EDGE_CURVE ( 'NONE', #107651, #68335, #173008, .T. ) ;
#253359 = ORIENTED_EDGE ( 'NONE', *, *, #89643, .T. ) ;
#253362 = EDGE_CURVE ( 'NONE', #237327, #173389, #158922, .T. ) ;
#253361 = STYLED_ITEM ( 'NONE', ( #187406 ), #20981 ) ;
#253360 = CARTESIAN_POINT ( 'NONE',  ( -20.85000000000000142, 7.021664781900089913, -37.33356540189728889 ) ) ;
#253363 = AXIS2_PLACEMENT_3D ( 'NONE', #117651, #180207, #139757 ) ;
#253364 = ORIENTED_EDGE ( 'NONE', *, *, #228179, .T. ) ;
#253366 = VERTEX_POINT ( 'NONE', #29357 ) ;
#253365 = LINE ( 'NONE', #35643, #102360 ) ;
#253367 = ORIENTED_EDGE ( 'NONE', *, *, #139581, .T. ) ;
#253368 = DIRECTION ( 'NONE',  ( -1.000000000000000000, 0.000000000000000000, 0.000000000000000000 ) ) ;
#253369 = LINE ( 'NONE', #193420, #71733 ) ;
#253370 = CARTESIAN_POINT ( 'NONE',  ( -20.64999999999999858, 74.07476635515169505, -48.75335101765046630 ) ) ;
#253371 = EDGE_CURVE ( 'NONE', #110689, #161820, #106293, .T. ) ;
#253372 = CARTESIAN_POINT ( 'NONE',  ( -23.15000000000000213, -11.64999999998884483, -55.25000000000004974 ) ) ;
#253373 = VERTEX_POINT ( 'NONE', #46291 ) ;
#253374 = CARTESIAN_POINT ( 'NONE',  ( 20.94999999999999574, -1.349084418615859482, -41.48649896354548616 ) ) ;
#253375 = DIRECTION ( 'NONE',  ( 1.000000000000000000, -1.387778780781444413E-14, 0.000000000000000000 ) ) ;
#253376 = ORIENTED_EDGE ( 'NONE', *, *, #7693, .F. ) ;
#253377 = CIRCLE ( 'NONE', #49372, 11.80000000000000426 ) ;
#253378 = ADVANCED_FACE ( 'NONE', ( #106257 ), #104955, .F. ) ;
#253379 = VERTEX_POINT ( 'NONE', #222342 ) ;
#253380 = FACE_OUTER_BOUND ( 'NONE', #90235, .T. ) ;
#253381 = CIRCLE ( 'NONE', #228453, 0.1000000000000021844 ) ;
#253382 = CARTESIAN_POINT ( 'NONE',  ( 23.14999999999999858, 5.000000000011153745, -121.5947339810869465 ) ) ;
#253383 = AXIS2_PLACEMENT_3D ( 'NONE', #200754, #22137, #143338 ) ;
#253384 = EDGE_CURVE ( 'NONE', #226219, #154016, #43741, .T. ) ;
#253385 = LINE ( 'NONE', #212978, #255401 ) ;
#253386 = ORIENTED_EDGE ( 'NONE', *, *, #153010, .F. ) ;
#253387 = EDGE_LOOP ( 'NONE', ( #172578, #65279, #228548, #89955 ) ) ;
#253388 = VECTOR ( 'NONE', #124634, 1000.000000000000114 ) ;
#253389 = ADVANCED_FACE ( 'NONE', ( #210524 ), #153157, .F. ) ;
#253390 = CARTESIAN_POINT ( 'NONE',  ( -20.89192007715127986, 18.40923646582965034, -236.9894833875398206 ) ) ;
#253391 = ORIENTED_EDGE ( 'NONE', *, *, #95806, .F. ) ;
#253392 = CARTESIAN_POINT ( 'NONE',  ( -20.54999999999999716, -9.000000000000001776, -23.60603087734756045 ) ) ;
#253393 = ADVANCED_FACE ( 'NONE', ( #172729 ), #252197, .T. ) ;
#253394 = CARTESIAN_POINT ( 'NONE',  ( 20.85000000000000142, 64.25000000001249134, -176.8069731475025321 ) ) ;
#253395 = EDGE_CURVE ( 'NONE', #26064, #209604, #132263, .T. ) ;
#253396 = CARTESIAN_POINT ( 'NONE',  ( 21.05000000000000071, 4.813084112160684214, -55.05848224347618469 ) ) ;
#253397 = AXIS2_PLACEMENT_3D ( 'NONE', #256110, #134915, #171542 ) ;
#253398 = AXIS2_PLACEMENT_3D ( 'NONE', #31402, #110901, #112211 ) ;
#253399 = AXIS2_PLACEMENT_3D ( 'NONE', #150524, #26740, #188360 ) ;
#253400 = CIRCLE ( 'NONE', #107471, 0.1000000000000074440 ) ;
#253401 = VERTEX_POINT ( 'NONE', #73609 ) ;
#253402 = CARTESIAN_POINT ( 'NONE',  ( 21.05000000000000071, 11.75000000001116263, -59.98519422934605672 ) ) ;
#253403 = ORIENTED_EDGE ( 'NONE', *, *, #55642, .T. ) ;
#253404 = CARTESIAN_POINT ( 'NONE',  ( -18.39999999999999858, 13.19494617735151465, -207.6708402378485516 ) ) ;
#253405 = FACE_OUTER_BOUND ( 'NONE', #167294, .T. ) ;
#253407 = ORIENTED_EDGE ( 'NONE', *, *, #34887, .F. ) ;
#253406 = CARTESIAN_POINT ( 'NONE',  ( -21.14999999999999858, 1.115600667400684642E-11, -60.45934304829880546 ) ) ;
#253408 = DIRECTION ( 'NONE',  ( -0.000000000000000000, -0.2128009952263604232, 0.9770955615653316162 ) ) ;
#253409 = CARTESIAN_POINT ( 'NONE',  ( -23.25000000000000000, 76.00000000001210765, -132.6231074845243540 ) ) ;
#253410 = PLANE ( 'NONE',  #105878 ) ;
#253411 = CARTESIAN_POINT ( 'NONE',  ( -21.64999999999999858, 60.86901957628278836, -220.9190389461266477 ) ) ;
#253412 = CARTESIAN_POINT ( 'NONE',  ( 21.05000000000000071, 6.477552182504587641, -33.59999996530019928 ) ) ;
#253413 = CIRCLE ( 'NONE', #95205, 7.900000000000000355 ) ;
#253414 = DIRECTION ( 'NONE',  ( 1.186688945009009831E-16, 0.9651348961777157509, -0.2617529984165031243 ) ) ;
#253415 = DIRECTION ( 'NONE',  ( 0.7071067811865474617, 0.7071067811865474617, -0.000000000000000000 ) ) ;
#253417 = ORIENTED_EDGE ( 'NONE', *, *, #157775, .F. ) ;
#253416 = LINE ( 'NONE', #156922, #123732 ) ;
#253418 = DIRECTION ( 'NONE',  ( 1.073024830501117725E-15, -0.000000000000000000, -1.000000000000000000 ) ) ;
#253419 = FACE_OUTER_BOUND ( 'NONE', #803, .T. ) ;
#253420 = CARTESIAN_POINT ( 'NONE',  ( 20.94999999999999929, 71.18691588786198565, -47.96462524104817504 ) ) ;
#253421 = ORIENTED_EDGE ( 'NONE', *, *, #234929, .F. ) ;
#253422 = EDGE_CURVE ( 'NONE', #138157, #140576, #249658, .T. ) ;
#253423 = DIRECTION ( 'NONE',  ( -1.000000000000000000, 0.000000000000000000, 0.000000000000000000 ) ) ;
#253424 = DIRECTION ( 'NONE',  ( 1.000000000000000000, -0.000000000000000000, 0.000000000000000000 ) ) ;
#253425 = AXIS2_PLACEMENT_3D ( 'NONE', #17000, #96496, #176088 ) ;
#253426 = AXIS2_PLACEMENT_3D ( 'NONE', #145414, #31924, #8494 ) ;
#253427 = ADVANCED_FACE ( 'NONE', ( #174009 ), #213078, .F. ) ;
#253428 = ORIENTED_EDGE ( 'NONE', *, *, #254569, .T. ) ;
#253429 = VECTOR ( 'NONE', #245618, 1000.000000000000000 ) ;
#253430 = DIRECTION ( 'NONE',  ( -1.000000000000000000, 2.952720810173289112E-16, 2.061873921506763405E-30 ) ) ;
#253431 = CARTESIAN_POINT ( 'NONE',  ( -21.07094088545304800, 61.10557489434068401, -234.2962495489933872 ) ) ;
#253432 = EDGE_CURVE ( 'NONE', #184556, #100083, #143738, .T. ) ;
#253433 = ORIENTED_EDGE ( 'NONE', *, *, #106727, .T. ) ;
#253435 = EDGE_CURVE ( 'NONE', #205761, #245795, #250913, .T. ) ;
#253434 = DIRECTION ( 'NONE',  ( -1.000000000000000000, 0.000000000000000000, -0.000000000000000000 ) ) ;
#253436 = ORIENTED_EDGE ( 'NONE', *, *, #150906, .F. ) ;
#253438 = ORIENTED_EDGE ( 'NONE', *, *, #91863, .T. ) ;
#253437 = CYLINDRICAL_SURFACE ( 'NONE', #88931, 0.1000000000000028644 ) ;
#253439 = CARTESIAN_POINT ( 'NONE',  ( 20.85000000000000142, 36.65892442174935439, -249.5511627012433848 ) ) ;
#253440 = ORIENTED_EDGE ( 'NONE', *, *, #31853, .T. ) ;
#253441 = DIRECTION ( 'NONE',  ( 0.000000000000000000, 0.000000000000000000, -1.000000000000000000 ) ) ;
#253442 = CIRCLE ( 'NONE', #32930, 0.1999999999999987899 ) ;
#253443 = EDGE_LOOP ( 'NONE', ( #158694, #17153, #215915, #209278 ) ) ;
#253445 = VERTEX_POINT ( 'NONE', #31911 ) ;
#253444 = ORIENTED_EDGE ( 'NONE', *, *, #94095, .T. ) ;
#253447 = LINE ( 'NONE', #233895, #173611 ) ;
#253446 = AXIS2_PLACEMENT_3D ( 'NONE', #185073, #6431, #26014 ) ;
#253449 = VERTEX_POINT ( 'NONE', #209228 ) ;
#253448 = DIRECTION ( 'NONE',  ( -1.000000000000000000, -2.952720810173289112E-16, 0.000000000000000000 ) ) ;
#253450 = DIRECTION ( 'NONE',  ( 0.000000000000000000, 0.9908441862701420355, 0.1350103645453197554 ) ) ;
#253451 = ORIENTED_EDGE ( 'NONE', *, *, #139976, .F. ) ;
#253452 = VECTOR ( 'NONE', #142568, 1000.000000000000000 ) ;
#253453 = ADVANCED_FACE ( 'NONE', ( #14908 ), #151859, .F. ) ;
#253454 = ORIENTED_EDGE ( 'NONE', *, *, #216199, .T. ) ;
#253455 = DIRECTION ( 'NONE',  ( -1.000000000000000000, 0.000000000000000000, -0.000000000000000000 ) ) ;
#253456 = CARTESIAN_POINT ( 'NONE',  ( -20.85000000000000142, 67.85909929089923764, -227.8797997985275856 ) ) ;
#253457 =( BOUNDED_SURFACE ( )  B_SPLINE_SURFACE ( 3, 2, ( 
 ( #11785, #30063, #89996 ),
 ( #110852, #65305, #167017 ),
 ( #88695, #247794, #229530 ),
 ( #67872, #48311, #50851 ) ),
 .UNSPECIFIED., .F., .F., .F. ) 
 B_SPLINE_SURFACE_WITH_KNOTS ( ( 4, 4 ),
 ( 3, 3 ),
 ( 0.0006461284895274040097, 0.0007503702773986315041 ),
 ( 0.000000000000000000, 1.000000000000000000 ),
 .UNSPECIFIED. ) 
 GEOMETRIC_REPRESENTATION_ITEM ( )  RATIONAL_B_SPLINE_SURFACE ( (
 ( 1.000000000000000000, 0.7071067811865475727, 1.000000000000000000),
 ( 1.000000000000000000, 0.7076476444649029141, 1.000000000000000000),
 ( 1.000000000000000000, 0.7075727925191180878, 1.000000000000000000),
 ( 1.000000000000000000, 0.7071067811865719976, 1.000000000000000000) ) ) 
 REPRESENTATION_ITEM ( '' )  SURFACE ( )  );
#253458 = DIRECTION ( 'NONE',  ( 1.000000000000000000, 0.000000000000000000, 0.000000000000000000 ) ) ;
#253459 = ORIENTED_EDGE ( 'NONE', *, *, #146369, .T. ) ;
#253460 = CARTESIAN_POINT ( 'NONE',  ( -20.94999999999999929, 74.14897176987143723, -158.3691942151018850 ) ) ;
#253461 = CARTESIAN_POINT ( 'NONE',  ( -17.01473183483382812, 9.950000000011137047, -146.7500000000000284 ) ) ;
#253462 = DIRECTION ( 'NONE',  ( 0.000000000000000000, 0.000000000000000000, 1.000000000000000000 ) ) ;
#253463 = ORIENTED_EDGE ( 'NONE', *, *, #134438, .F. ) ;
#253464 = DIRECTION ( 'NONE',  ( -1.000000000000000000, 2.952720810173289112E-16, 2.061873921506763405E-30 ) ) ;
#253466 = ADVANCED_FACE ( 'NONE', ( #154438 ), #33211, .T. ) ;
#253465 = CARTESIAN_POINT ( 'NONE',  ( -18.54260524012581612, 38.05639603915591351, -261.2178114574803089 ) ) ;
#253467 = CARTESIAN_POINT ( 'NONE',  ( -16.94107738177415712, 10.01423928513662176, -12.55000000000000249 ) ) ;
#253468 = CIRCLE ( 'NONE', #61954, 11.65000000000001457 ) ;
#253469 = ORIENTED_EDGE ( 'NONE', *, *, #37533, .T. ) ;
#253470 = ADVANCED_FACE ( 'NONE', ( #188384 ), #202012, .T. ) ;
#253471 = CARTESIAN_POINT ( 'NONE',  ( 20.94999999999999929, 6.650000000011155876, -179.6499999999999773 ) ) ;
#253472 = ORIENTED_EDGE ( 'NONE', *, *, #82021, .F. ) ;
#253473 = CIRCLE ( 'NONE', #70362, 0.2000000000000057288 ) ;
#253474 = VERTEX_POINT ( 'NONE', #111423 ) ;
#253475 = CIRCLE ( 'NONE', #41130, 0.1000000000000028644 ) ;
#253476 = CARTESIAN_POINT ( 'NONE',  ( -13.12432614554022869, 25.00761986058640929, -232.6112779818446938 ) ) ;
#253477 = ORIENTED_EDGE ( 'NONE', *, *, #213005, .F. ) ;
#253478 = ORIENTED_EDGE ( 'NONE', *, *, #213624, .F. ) ;
#253479 = DIRECTION ( 'NONE',  ( 1.000000000000000000, 0.000000000000000000, 0.000000000000000000 ) ) ;
#253480 = CYLINDRICAL_SURFACE ( 'NONE', #225031, 0.09999999999999939493 ) ;
#253481 = VERTEX_POINT ( 'NONE', #134807 ) ;
#253482 = VECTOR ( 'NONE', #87063, 1000.000000000000000 ) ;
#253483 = ORIENTED_EDGE ( 'NONE', *, *, #130271, .F. ) ;
#253484 = EDGE_CURVE ( 'NONE', #12197, #97363, #89274, .T. ) ;
#253485 = CARTESIAN_POINT ( 'NONE',  ( -21.05000000000000071, 14.00000000001115374, -162.0729074696175473 ) ) ;
#253486 = DIRECTION ( 'NONE',  ( 1.734723475976817507E-14, -1.000000000000000000, 0.000000000000000000 ) ) ;
#253487 = EDGE_CURVE ( 'NONE', #116722, #149671, #112708, .T. ) ;
#253488 = VERTEX_POINT ( 'NONE', #150553 ) ;
#253489 = EDGE_CURVE ( 'NONE', #201868, #34147, #89556, .T. ) ;
#253490 = AXIS2_PLACEMENT_3D ( 'NONE', #106881, #135092, #213350 ) ;
#253491 = CIRCLE ( 'NONE', #7815, 3.999999999999996447 ) ;
#253492 = ORIENTED_EDGE ( 'NONE', *, *, #227729, .F. ) ;
#253494 = LINE ( 'NONE', #129706, #160055 ) ;
#253493 = VECTOR ( 'NONE', #50632, 1000.000000000000000 ) ;
#253495 = DIRECTION ( 'NONE',  ( 0.000000000000000000, 0.000000000000000000, -1.000000000000000000 ) ) ;
#253496 = EDGE_CURVE ( 'NONE', #9346, #64966, #228811, .T. ) ;
#253497 = DIRECTION ( 'NONE',  ( 0.000000000000000000, -0.8700118002898321601, 0.4930308989875230030 ) ) ;
#253498 = CARTESIAN_POINT ( 'NONE',  ( -20.94999999999999929, 76.00000000001237765, -170.0231074845243597 ) ) ;
#253499 = AXIS2_PLACEMENT_3D ( 'NONE', #82586, #26523, #64355 ) ;
#253501 = CIRCLE ( 'NONE', #103642, 0.09999999999999516220 ) ;
#253500 = CYLINDRICAL_SURFACE ( 'NONE', #195210, 0.09999999999999939493 ) ;
#253502 = FACE_OUTER_BOUND ( 'NONE', #84188, .T. ) ;
#253503 = EDGE_CURVE ( 'NONE', #76480, #41443, #48064, .T. ) ;
#253505 = CARTESIAN_POINT ( 'NONE',  ( -18.59999999999999787, 66.65000000001187175, -90.67310748452437963 ) ) ;
#253504 = CARTESIAN_POINT ( 'NONE',  ( 21.09107601085543493, 75.96069283529440952, -75.88698545988413002 ) ) ;
#253506 = LINE ( 'NONE', #170181, #3199 ) ;
#253507 = CARTESIAN_POINT ( 'NONE',  ( 21.72449340488910252, 65.71604372252147641, -190.8731074845244393 ) ) ;
#253508 = VECTOR ( 'NONE', #128952, 1000.000000000000227 ) ;
#253509 = DIRECTION ( 'NONE',  ( 0.000000000000000000, 0.000000000000000000, -1.000000000000000000 ) ) ;
#253510 = CARTESIAN_POINT ( 'NONE',  ( -20.94999999999999929, 87.48912529308822172, -139.6231074845242688 ) ) ;
#253511 = VERTEX_POINT ( 'NONE', #79960 ) ;
#253512 = AXIS2_PLACEMENT_3D ( 'NONE', #41918, #197100, #178874 ) ;
#253513 = VECTOR ( 'NONE', #84916, 1000.000000000000000 ) ;
#253514 = CIRCLE ( 'NONE', #161982, 0.09999999999999939493 ) ;
#253515 = VECTOR ( 'NONE', #221747, 1000.000000000000000 ) ;
#253517 = VERTEX_POINT ( 'NONE', #136087 ) ;
#253516 = DIRECTION ( 'NONE',  ( -0.000000000000000000, 0.9770955615653313941, 0.2128009952263603954 ) ) ;
#253518 = AXIS2_PLACEMENT_3D ( 'NONE', #31634, #12062, #126848 ) ;
#253519 = CARTESIAN_POINT ( 'NONE',  ( -23.25000000000000000, 76.00000000001244871, -170.0231074845243597 ) ) ;
#253520 = CARTESIAN_POINT ( 'NONE',  ( -20.94999999999999929, 76.00000000001126921, -203.5231074845248997 ) ) ;
#253521 = ORIENTED_EDGE ( 'NONE', *, *, #148583, .T. ) ;
#253522 = SURFACE_STYLE_FILL_AREA ( #250946 ) ;
#253523 = CARTESIAN_POINT ( 'NONE',  ( 21.14999999999999858, 64.35000000001258513, -191.2731074845244450 ) ) ;
#253524 = DIRECTION ( 'NONE',  ( 1.000000000000000000, 0.000000000000000000, -0.000000000000000000 ) ) ;
#253525 = AXIS2_PLACEMENT_3D ( 'NONE', #168852, #183239, #247042 ) ;
#253526 = VECTOR ( 'NONE', #80109, 1000.000000000000114 ) ;
#253527 = ORIENTED_EDGE ( 'NONE', *, *, #139135, .F. ) ;
#253528 = DIRECTION ( 'NONE',  ( 1.000000000000000000, 0.000000000000000000, 0.000000000000000000 ) ) ;
#253529 = CARTESIAN_POINT ( 'NONE',  ( 21.72449340488910607, 65.71604372252041060, -48.67310748452440095 ) ) ;
#253530 = DIRECTION ( 'NONE',  ( -1.000000000000000000, 0.000000000000000000, 0.000000000000000000 ) ) ;
#253532 = ORIENTED_EDGE ( 'NONE', *, *, #41732, .F. ) ;
#253531 = CARTESIAN_POINT ( 'NONE',  ( 21.05000000000000071, 1.115600667400684642E-11, -134.0000000000000000 ) ) ;
#253533 = DIRECTION ( 'NONE',  ( -0.000000000000000000, 0.9651348961777157509, -0.2617529984165031243 ) ) ;
#253535 = ORIENTED_EDGE ( 'NONE', *, *, #80089, .F. ) ;
#253534 = CYLINDRICAL_SURFACE ( 'NONE', #231177, 7.899999999999994138 ) ;
#253536 = B_SPLINE_CURVE_WITH_KNOTS ( 'NONE', 3,
 ( #82721, #179317, #123178, #102284, #164875, #623, #161024, #181867, #224826, #162314, #222242, #99724, #180580, #202703, #241827, #198848 ),
 .UNSPECIFIED., .F., .F.,
 ( 4, 3, 3, 3, 3, 4 ),
 ( 0.000000000000000000, 3.357088238232317244E-05, 6.714213034886757942E-05, 0.0001007408646120921551, 0.0001343627955914185768, 0.0001573956632895995484 ),
 .UNSPECIFIED. ) ;
#253537 = AXIS2_PLACEMENT_3D ( 'NONE', #14063, #115716, #37476 ) ;
#253538 = CARTESIAN_POINT ( 'NONE',  ( -18.50000000000000000, 9.250000000011157297, -188.6499999999999488 ) ) ;
#253539 = FACE_OUTER_BOUND ( 'NONE', #190016, .T. ) ;
#253540 = CARTESIAN_POINT ( 'NONE',  ( 18.49999999999998934, 11.65000000001115943, -58.25000000000000000 ) ) ;
#253541 = CIRCLE ( 'NONE', #128670, 0.09999999999999971412 ) ;
#253542 = DIRECTION ( 'NONE',  ( 0.000000000000000000, -1.000000000000000000, 0.000000000000000000 ) ) ;
#253544 = CARTESIAN_POINT ( 'NONE',  ( 20.04142135623730070, 15.92646454033040015, -219.3818586450342423 ) ) ;
#253543 = CARTESIAN_POINT ( 'NONE',  ( -16.87333278164157946, 9.882609784590092872, -154.3668321938465624 ) ) ;
#253546 = EDGE_CURVE ( 'NONE', #25360, #82095, #77100, .T. ) ;
#253545 = FACE_OUTER_BOUND ( 'NONE', #221065, .T. ) ;
#253547 = CIRCLE ( 'NONE', #237004, 0.09999999999998898659 ) ;
#253548 = FACE_OUTER_BOUND ( 'NONE', #56420, .T. ) ;
#253549 = DIRECTION ( 'NONE',  ( 0.000000000000000000, 0.000000000000000000, 1.000000000000000000 ) ) ;
#253550 = CARTESIAN_POINT ( 'NONE',  ( 21.13435531349839991, 1.404649027653016802, -230.6664124791826964 ) ) ;
#253551 = LINE ( 'NONE', #240114, #13771 ) ;
#253553 = ORIENTED_EDGE ( 'NONE', *, *, #26308, .F. ) ;
#253552 = CIRCLE ( 'NONE', #12173, 0.1000000000000054595 ) ;
#253554 = DIRECTION ( 'NONE',  ( -7.304098846218419643E-16, 0.9770955615653543758, 0.2128009952262553683 ) ) ;
#253555 = VERTEX_POINT ( 'NONE', #17449 ) ;
#253556 =( BOUNDED_SURFACE ( )  B_SPLINE_SURFACE ( 3, 2, ( 
 ( #9062, #31244, #126441 ),
 ( #205982, #11653, #91169 ),
 ( #226824, #247676, #108177 ),
 ( #185135, #186434, #48185 ),
 ( #168185, #250242, #127742 ),
 ( #165589, #27389, #125173 ) ),
 .UNSPECIFIED., .F., .F., .T. ) 
 B_SPLINE_SURFACE_WITH_KNOTS ( ( 4, 2, 4 ),
 ( 3, 3 ),
 ( -1.776356839400250465E-15, 0.7853981633974468357, 1.570796326794895448 ),
 ( 0.000000000000000000, 1.000000000000000000 ),
 .UNSPECIFIED. ) 
 GEOMETRIC_REPRESENTATION_ITEM ( )  RATIONAL_B_SPLINE_SURFACE ( (
 ( 1.000000000000000000, 0.4999999999999960587, 1.000000000000000000),
 ( 1.000000000000000000, 0.4993418825332500144, 1.000000000000000000),
 ( 1.000000000000000000, 0.5278258667060371501, 1.000000000000000000),
 ( 1.000000000000000000, 0.6092287576694621620, 1.000000000000000000),
 ( 1.000000000000000000, 0.6611148371779838051, 1.000000000000000000),
 ( 1.000000000000000000, 0.7071067811865719976, 1.000000000000000000) ) ) 
 REPRESENTATION_ITEM ( '' )  SURFACE ( )  );
#253557 = ORIENTED_EDGE ( 'NONE', *, *, #237695, .F. ) ;
#253558 = CARTESIAN_POINT ( 'NONE',  ( -21.05000000000000071, 74.83729825007360148, -61.62310748452433273 ) ) ;
#253559 = ADVANCED_FACE ( 'NONE', ( #160839 ), #180390, .F. ) ;
#253560 = CARTESIAN_POINT ( 'NONE',  ( -20.85000000000000142, 64.25000000001244871, -170.0231074845244166 ) ) ;
#253561 = ORIENTED_EDGE ( 'NONE', *, *, #153792, .T. ) ;
#253562 = EDGE_CURVE ( 'NONE', #88538, #148964, #194836, .T. ) ;
#253564 = ADVANCED_FACE ( 'NONE', ( #219492 ), #159545, .T. ) ;
#253563 = AXIS2_PLACEMENT_3D ( 'NONE', #128231, #85205, #64404 ) ;
#253565 = CIRCLE ( 'NONE', #57754, 0.09999999999999363565 ) ;
#253566 = ORIENTED_EDGE ( 'NONE', *, *, #43085, .T. ) ;
#253567 = CIRCLE ( 'NONE', #166145, 11.75000000000000355 ) ;
#253568 = CARTESIAN_POINT ( 'NONE',  ( -18.37013991200266005, 11.49974761622312691, -143.2069769894829108 ) ) ;
#253569 = FILL_AREA_STYLE_COLOUR ( '', #139786 ) ;
#253570 = ORIENTED_EDGE ( 'NONE', *, *, #225931, .F. ) ;
#253571 = ORIENTED_EDGE ( 'NONE', *, *, #200496, .T. ) ;
#253572 = DIRECTION ( 'NONE',  ( 1.000000000000000000, 0.000000000000000000, 0.000000000000000000 ) ) ;
#253573 = DIRECTION ( 'NONE',  ( 1.000000000000000000, -0.000000000000000000, -0.000000000000000000 ) ) ;
#253574 = CARTESIAN_POINT ( 'NONE',  ( 20.94999999999999574, 8.926614585098251453, -41.97168301922312850 ) ) ;
#253575 = CARTESIAN_POINT ( 'NONE',  ( 13.88302573338718915, 9.457410944767412175, -15.00008397379001934 ) ) ;
#253576 = EDGE_CURVE ( 'NONE', #104512, #228853, #102019, .T. ) ;
#253578 = DIRECTION ( 'NONE',  ( 0.000000000000000000, 0.000000000000000000, 1.000000000000000000 ) ) ;
#253577 = PLANE ( 'NONE',  #33360 ) ;
#253579 = CARTESIAN_POINT ( 'NONE',  ( 23.15000000000000213, 84.66355140188167638, -179.5472086025916099 ) ) ;
#253581 = ORIENTED_EDGE ( 'NONE', *, *, #185636, .F. ) ;
#253580 = LINE ( 'NONE', #153249, #84035 ) ;
#253583 = FACE_OUTER_BOUND ( 'NONE', #82523, .T. ) ;
#253582 = CARTESIAN_POINT ( 'NONE',  ( -22.59999999999999787, 0.000000000000000000, 0.000000000000000000 ) ) ;
#253584 = DIRECTION ( 'NONE',  ( 3.265361837132813093E-16, -1.000000000000000000, -0.000000000000000000 ) ) ;
#253585 = VERTEX_POINT ( 'NONE', #40902 ) ;
#253586 = CARTESIAN_POINT ( 'NONE',  ( 21.07199075132372101, 8.774944999127242795, -146.2135321616128749 ) ) ;
#253587 = DIRECTION ( 'NONE',  ( 1.000000000000000000, 0.000000000000000000, 0.000000000000000000 ) ) ;
#253588 = ORIENTED_EDGE ( 'NONE', *, *, #229554, .T. ) ;
#253589 = CARTESIAN_POINT ( 'NONE',  ( -21.14999999999999858, 69.45934304831089889, -136.5231074845243313 ) ) ;
#253590 = DIRECTION ( 'NONE',  ( -1.000000000000000000, -0.000000000000000000, -0.000000000000000000 ) ) ;
#253591 = CARTESIAN_POINT ( 'NONE',  ( 14.22821877134046176, 66.54397173950393096, -88.01190944945867045 ) ) ;
#253592 = ORIENTED_EDGE ( 'NONE', *, *, #165950, .T. ) ;
#253593 = EDGE_LOOP ( 'NONE', ( #250493, #148487, #6140, #140671 ) ) ;
#253594 = DIRECTION ( 'NONE',  ( 1.000000000000000000, 0.000000000000000000, 0.000000000000000000 ) ) ;
#253595 = ADVANCED_FACE ( 'NONE', ( #257290 ), #176549, .T. ) ;
#253596 = CARTESIAN_POINT ( 'NONE',  ( -21.05000000000000071, 86.45856254523214091, -209.4679346046102921 ) ) ;
#253597 = DIRECTION ( 'NONE',  ( 0.000000000000000000, -0.4999999999999649170, 0.8660254037844589137 ) ) ;
#253598 = CARTESIAN_POINT ( 'NONE',  ( 16.87683809663750267, 66.05000000001230376, -157.3731074845244393 ) ) ;
#253599 = VERTEX_POINT ( 'NONE', #16196 ) ;
#253600 = CARTESIAN_POINT ( 'NONE',  ( 12.84233041328156766, 46.89553527312528303, -234.6535825622730158 ) ) ;
#253601 = CARTESIAN_POINT ( 'NONE',  ( -22.57320508075686405, 64.25000000001236344, -170.0231074845243882 ) ) ;
#253602 = EDGE_CURVE ( 'NONE', #57106, #163009, #247796, .T. ) ;
#253603 = CARTESIAN_POINT ( 'NONE',  ( -18.41431012584569160, 11.48747202921933130, -124.7732360131017231 ) ) ;
#253604 = CARTESIAN_POINT ( 'NONE',  ( -21.05000000000000071, 1.115600667400684642E-11, -134.0000000000000000 ) ) ;
#253605 = CIRCLE ( 'NONE', #170469, 0.1000000000000028644 ) ;
#253606 = VECTOR ( 'NONE', #41373, 1000.000000000000000 ) ;
#253607 = CIRCLE ( 'NONE', #137106, 0.09999999999999939493 ) ;
#253608 = DIRECTION ( 'NONE',  ( 0.000000000000000000, -6.982962677686266711E-15, 1.000000000000000000 ) ) ;
#253610 = VERTEX_POINT ( 'NONE', #235222 ) ;
#253609 = CARTESIAN_POINT ( 'NONE',  ( -16.93353400591625757, 65.99538760383886427, -82.09042301431897215 ) ) ;
#253611 = DIRECTION ( 'NONE',  ( 0.000000000000000000, -0.7049548389605068133, 0.7092521942342977503 ) ) ;
#253612 = LINE ( 'NONE', #112838, #7907 ) ;
#253613 = CARTESIAN_POINT ( 'NONE',  ( -23.25000000000000000, 7.128833340094563376, -233.7327013124401276 ) ) ;
#253615 = ORIENTED_EDGE ( 'NONE', *, *, #252944, .T. ) ;
#253614 = CARTESIAN_POINT ( 'NONE',  ( -20.54999999999999716, 78.37638820354418101, -229.1444560783390898 ) ) ;
#253616 = DIRECTION ( 'NONE',  ( 0.000000000000000000, -6.308085367188393199E-16, -1.000000000000000000 ) ) ;
#253617 = DIRECTION ( 'NONE',  ( 0.000000000000000000, 6.982962677686267499E-15, -1.000000000000000000 ) ) ;
#253618 = LINE ( 'NONE', #75038, #115755 ) ;
#253619 = ORIENTED_EDGE ( 'NONE', *, *, #110661, .F. ) ;
#253620 = CARTESIAN_POINT ( 'NONE',  ( 18.49999999999998934, 6.550000000000000711, -10.01702717044001822 ) ) ;
#253621 = CARTESIAN_POINT ( 'NONE',  ( -17.11825945287481332, 51.57797924205760864, -231.8552082689889460 ) ) ;
#253622 = CARTESIAN_POINT ( 'NONE',  ( -20.54999999999999716, 18.56623428888383387, -239.8594038951179073 ) ) ;
#253623 = AXIS2_PLACEMENT_3D ( 'NONE', #83149, #220145, #204407 ) ;
#253624 = AXIS2_PLACEMENT_3D ( 'NONE', #247826, #6638, #147441 ) ;
#253625 = CARTESIAN_POINT ( 'NONE',  ( 20.95000000000005613, 66.15000000001120384, -4.623107484524796362 ) ) ;
#253626 = CONICAL_SURFACE ( 'NONE', #161908, 7.750000000000034639, 0.7853981633974531640 ) ;
#253627 = CARTESIAN_POINT ( 'NONE',  ( 21.05000000000000071, 6.258847123090474973, -167.4682416469444206 ) ) ;
#253628 = FACE_OUTER_BOUND ( 'NONE', #89431, .T. ) ;
#253629 = AXIS2_PLACEMENT_3D ( 'NONE', #183981, #5313, #84843 ) ;
#253630 = ORIENTED_EDGE ( 'NONE', *, *, #119452, .T. ) ;
#253631 = EDGE_LOOP ( 'NONE', ( #64573, #71427, #126667, #181595 ) ) ;
#253632 = EDGE_CURVE ( 'NONE', #136769, #126189, #222842, .T. ) ;
#253633 = CARTESIAN_POINT ( 'NONE',  ( 18.59999999999999432, 74.83729825007388570, -94.92310748452432279 ) ) ;
#253635 = EDGE_CURVE ( 'NONE', #172698, #147150, #64617, .T. ) ;
#253634 = DIRECTION ( 'NONE',  ( 0.000000000000000000, -6.853228547068871147E-15, 1.000000000000000000 ) ) ;
#253636 = CARTESIAN_POINT ( 'NONE',  ( -21.00219873199050724, 38.22274692886851000, -236.1338529772052084 ) ) ;
#253637 = DIRECTION ( 'NONE',  ( 0.000000000000000000, -8.673617379883787770E-15, 1.000000000000000000 ) ) ;
#253638 = EDGE_CURVE ( 'NONE', #180985, #191649, #84810, .T. ) ;
#253639 = EDGE_CURVE ( 'NONE', #108803, #232204, #158290, .T. ) ;
#253640 = CARTESIAN_POINT ( 'NONE',  ( -18.50000000000000000, -9.399999999988850163, -174.7972597596632625 ) ) ;
#253641 = PLANE ( 'NONE',  #154995 ) ;
#253642 = EDGE_CURVE ( 'NONE', #137759, #57651, #73055, .T. ) ;
#253643 = DIRECTION ( 'NONE',  ( 0.000000000000000000, 0.000000000000000000, 1.000000000000000000 ) ) ;
#253645 = DIRECTION ( 'NONE',  ( 0.000000000000000000, 0.000000000000000000, 1.000000000000000000 ) ) ;
#253644 = AXIS2_PLACEMENT_3D ( 'NONE', #172276, #194387, #213919 ) ;
#253646 = EDGE_CURVE ( 'NONE', #238394, #213256, #81254, .T. ) ;
#253648 = EDGE_CURVE ( 'NONE', #61931, #220134, #243700, .T. ) ;
#253647 = EDGE_CURVE ( 'NONE', #102738, #163909, #206293, .T. ) ;
#253649 = ORIENTED_EDGE ( 'NONE', *, *, #8410, .T. ) ;
#253650 = LINE ( 'NONE', #75063, #135528 ) ;
#253651 = VERTEX_POINT ( 'NONE', #38312 ) ;
#253652 = ORIENTED_EDGE ( 'NONE', *, *, #342, .F. ) ;
#253653 = FACE_OUTER_BOUND ( 'NONE', #125407, .T. ) ;
#253654 = CARTESIAN_POINT ( 'NONE',  ( -21.13435531349828267, 6.493721063603252297, -100.5000000000000284 ) ) ;
#253655 = DIRECTION ( 'NONE',  ( -1.000000000000000000, 0.000000000000000000, 0.000000000000000000 ) ) ;
#253656 = CIRCLE ( 'NONE', #57840, 0.1000000000000028644 ) ;
#253659 = EDGE_CURVE ( 'NONE', #74892, #110439, #117831, .T. ) ;
#253658 = ORIENTED_EDGE ( 'NONE', *, *, #158539, .F. ) ;
#253657 = CARTESIAN_POINT ( 'NONE',  ( 20.94999999999999929, 87.48912529308852015, -173.1231074845242688 ) ) ;
#253660 = CARTESIAN_POINT ( 'NONE',  ( -18.50000000000000000, 59.19392724319018129, -220.9828015967491126 ) ) ;
#253661 = CARTESIAN_POINT ( 'NONE',  ( -23.15000000000000213, 26.18196512540240661, -241.1028522842020152 ) ) ;
#253662 = ORIENTED_EDGE ( 'NONE', *, *, #56555, .T. ) ;
#253663 = CARTESIAN_POINT ( 'NONE',  ( -12.26136940704872025, 9.351403174152810749, -150.9795304368385302 ) ) ;
#253664 = EDGE_CURVE ( 'NONE', #175321, #156593, #114708, .T. ) ;
#253665 = CARTESIAN_POINT ( 'NONE',  ( 18.49999999999999289, 65.65621891165909574, -145.1946622066474504 ) ) ;
#253666 = DIRECTION ( 'NONE',  ( 1.000000000000000000, -8.623019343401624248E-17, -8.389849937938898203E-16 ) ) ;
#253667 = CARTESIAN_POINT ( 'NONE',  ( 20.95512820512820440, 10.62384868372303615, -146.1500000000000341 ) ) ;
#253668 = ADVANCED_FACE ( 'NONE', ( #4292 ), #35448, .T. ) ;
#253669 = EDGE_CURVE ( 'NONE', #135320, #102830, #185517, .T. ) ;
#253670 = CIRCLE ( 'NONE', #212009, 0.4000000000000045186 ) ;
#253671 = FACE_OUTER_BOUND ( 'NONE', #136904, .T. ) ;
#253672 = AXIS2_PLACEMENT_3D ( 'NONE', #42037, #17332, #219361 ) ;
#253673 = ORIENTED_EDGE ( 'NONE', *, *, #157397, .T. ) ;
#253674 = CARTESIAN_POINT ( 'NONE',  ( -18.50000000000000000, 9.350000000011156942, -179.8499999999999943 ) ) ;
#253676 = EDGE_CURVE ( 'NONE', #123059, #55661, #123092, .T. ) ;
#253675 = CARTESIAN_POINT ( 'NONE',  ( -16.87683809663753109, 66.13508622147344340, -89.74739184888585442 ) ) ;
#253677 = ORIENTED_EDGE ( 'NONE', *, *, #205688, .T. ) ;
#253678 = DIRECTION ( 'NONE',  ( -1.000000000000000000, 0.000000000000000000, -0.000000000000000000 ) ) ;
#253679 = CARTESIAN_POINT ( 'NONE',  ( 23.24999999999999645, 1.115600667400684642E-11, -100.5000000000000284 ) ) ;
#253680 = FACE_OUTER_BOUND ( 'NONE', #8065, .T. ) ;
#253681 = EDGE_CURVE ( 'NONE', #113056, #166805, #185626, .T. ) ;
#253682 = AXIS2_PLACEMENT_3D ( 'NONE', #72069, #92888, #89037 ) ;
#253683 = VERTEX_POINT ( 'NONE', #62993 ) ;
#253684 = DIRECTION ( 'NONE',  ( -1.000000000000000000, -0.000000000000000000, -0.000000000000000000 ) ) ;
#253685 = DIRECTION ( 'NONE',  ( 0.000000000000000000, -0.9964539953858966292, -0.08413937888696132461 ) ) ;
#253686 = ADVANCED_FACE ( 'NONE', ( #23905 ), #103382, .F. ) ;
#253687 = ORIENTED_EDGE ( 'NONE', *, *, #98462, .T. ) ;
#253688 = CIRCLE ( 'NONE', #66276, 0.1000000000000028644 ) ;
#253689 = AXIS2_PLACEMENT_3D ( 'NONE', #68960, #252689, #226712 ) ;
#253690 = STYLED_ITEM ( 'NONE', ( #3070 ), #111872 ) ;
#253691 = ORIENTED_EDGE ( 'NONE', *, *, #114407, .F. ) ;
#253692 = DIRECTION ( 'NONE',  ( 1.000000000000000000, 0.000000000000000000, 0.000000000000000000 ) ) ;
#253693 = EDGE_CURVE ( 'NONE', #81780, #37627, #26454, .T. ) ;
#253694 = VECTOR ( 'NONE', #105331, 1000.000000000000000 ) ;
#253695 = DIRECTION ( 'NONE',  ( -1.000000000000000000, -2.952720810173289112E-16, 0.000000000000000000 ) ) ;
#253697 = VERTEX_POINT ( 'NONE', #245499 ) ;
#253696 = DIRECTION ( 'NONE',  ( 1.000000000000000000, 0.000000000000000000, 0.000000000000000000 ) ) ;
#253698 = FACE_OUTER_BOUND ( 'NONE', #231717, .T. ) ;
#253700 = CARTESIAN_POINT ( 'NONE',  ( -17.01473183483381391, 9.950000000011138823, -113.2500000000000426 ) ) ;
#253699 = UNCERTAINTY_MEASURE_WITH_UNIT (LENGTH_MEASURE( 1.000000000000000082E-05 ), #80301, 'distance_accuracy_value', 'NONE');
#253701 = CARTESIAN_POINT ( 'NONE',  ( -20.94983749550516450, 65.70233904877032671, -131.0487410911968880 ) ) ;
#253702 = DIRECTION ( 'NONE',  ( 0.000000000000000000, 0.2617529984165152257, 0.9651348961777124202 ) ) ;
#253703 = CARTESIAN_POINT ( 'NONE',  ( -21.44999999999999929, 21.39147882631411335, -233.2615922652120730 ) ) ;
#253704 = LINE ( 'NONE', #54221, #247146 ) ;
#253705 = CARTESIAN_POINT ( 'NONE',  ( -23.25000000000000355, 64.25000000001202238, -115.6731074845243938 ) ) ;
#253707 = ORIENTED_EDGE ( 'NONE', *, *, #173646, .T. ) ;
#253706 = DIRECTION ( 'NONE',  ( -1.000000000000000000, 7.304098846218134667E-16, 5.100424963727256530E-30 ) ) ;
#253708 = ORIENTED_EDGE ( 'NONE', *, *, #36091, .T. ) ;
#253710 = CARTESIAN_POINT ( 'NONE',  ( -20.94999999999999929, -11.48912529306489994, -197.8999999999999773 ) ) ;
#253709 = CYLINDRICAL_SURFACE ( 'NONE', #133043, 0.09999999999998898659 ) ;
#253712 = EDGE_LOOP ( 'NONE', ( #183707, #125800, #193515 ) ) ;
#253711 = CARTESIAN_POINT ( 'NONE',  ( 18.49999999999999645, 77.63717271298224887, -91.44095411905229298 ) ) ;
#253713 = ORIENTED_EDGE ( 'NONE', *, *, #46197, .T. ) ;
#253714 = CARTESIAN_POINT ( 'NONE',  ( -18.50000000000000000, 10.29288807859935950, -105.9580020160122302 ) ) ;
#253715 = AXIS2_PLACEMENT_3D ( 'NONE', #208673, #7903, #144804 ) ;
#253716 = FACE_OUTER_BOUND ( 'NONE', #158929, .T. ) ;
#253717 = CYLINDRICAL_SURFACE ( 'NONE', #231793, 0.09999999999999939493 ) ;
#253718 = CARTESIAN_POINT ( 'NONE',  ( -23.15000000000000213, 86.45856254523214091, -209.4679346046102921 ) ) ;
#253719 = FACE_OUTER_BOUND ( 'NONE', #10422, .T. ) ;
#253720 = AXIS2_PLACEMENT_3D ( 'NONE', #224223, #26050, #166867 ) ;
#253721 = DIRECTION ( 'NONE',  ( 0.000000000000000000, -0.9908441862701596881, 0.1350103645451904977 ) ) ;
#253723 = ORIENTED_EDGE ( 'NONE', *, *, #63741, .F. ) ;
#253722 = ADVANCED_FACE ( 'NONE', ( #186815 ), #65032, .T. ) ;
#253724 = EDGE_LOOP ( 'NONE', ( #44404, #190010, #125159, #241887, #83377, #141559 ) ) ;
#253725 = FACE_OUTER_BOUND ( 'NONE', #97511, .T. ) ;
#253726 = AXIS2_PLACEMENT_3D ( 'NONE', #208977, #228558, #206412 ) ;
#253727 = ADVANCED_FACE ( 'NONE', ( #165981 ), #177283, .F. ) ;
#253728 = ORIENTED_EDGE ( 'NONE', *, *, #221477, .F. ) ;
#253729 = CARTESIAN_POINT ( 'NONE',  ( 21.05000000000000071, 61.16604239671103471, -234.3115055913011417 ) ) ;
#253730 = DIRECTION ( 'NONE',  ( 0.000000000000000000, 0.1350103645451904977, -0.9908441862701596881 ) ) ;
#253731 = AXIS2_PLACEMENT_3D ( 'NONE', #216699, #66623, #86147 ) ;
#253732 = DIRECTION ( 'NONE',  ( 1.000000000000000000, 0.000000000000000000, 0.000000000000000000 ) ) ;
#253733 = EDGE_CURVE ( 'NONE', #97650, #254207, #5566, .T. ) ;
#253734 = ORIENTED_EDGE ( 'NONE', *, *, #120904, .T. ) ;
#253736 = ADVANCED_FACE ( 'NONE', ( #44730 ), #87678, .T. ) ;
#253735 = LINE ( 'NONE', #137633, #52496 ) ;
#253737 = ORIENTED_EDGE ( 'NONE', *, *, #218969, .F. ) ;
#253738 = CARTESIAN_POINT ( 'NONE',  ( 21.14999999999999503, 76.00000000001217870, -142.7731074845243029 ) ) ;
#253739 = VERTEX_POINT ( 'NONE', #125539 ) ;
#253740 = EDGE_CURVE ( 'NONE', #51015, #176803, #60692, .T. ) ;
#253741 = AXIS2_PLACEMENT_3D ( 'NONE', #119609, #101253, #242090 ) ;
#253742 = DIRECTION ( 'NONE',  ( -6.938893903907224433E-15, -1.000000000000000000, -6.982962677686266711E-15 ) ) ;
#253743 = CARTESIAN_POINT ( 'NONE',  ( -23.15000000000000213, 67.55989888862310977, -211.9120700681549465 ) ) ;
#253744 = AXIS2_PLACEMENT_3D ( 'NONE', #49528, #189037, #243862 ) ;
#253745 = ORIENTED_EDGE ( 'NONE', *, *, #14755, .T. ) ;
#253746 = CARTESIAN_POINT ( 'NONE',  ( 20.94999999999999574, 6.400000000011158541, -110.4304246300616086 ) ) ;
#253747 = VERTEX_POINT ( 'NONE', #167269 ) ;
#253750 = ORIENTED_EDGE ( 'NONE', *, *, #129135, .F. ) ;
#253749 = CARTESIAN_POINT ( 'NONE',  ( -18.50000000000000000, 11.75000000001115197, -155.7499999999999716 ) ) ;
#253748 = DIRECTION ( 'NONE',  ( 0.7071067811865474617, 0.7071067811865474617, 0.000000000000000000 ) ) ;
#253751 = CARTESIAN_POINT ( 'NONE',  ( -21.04386569057605527, 64.25000000001146816, -42.88027013274443533 ) ) ;
#253752 = EDGE_LOOP ( 'NONE', ( #8506, #86261, #195702, #177930 ) ) ;
#253753 = EDGE_CURVE ( 'NONE', #130620, #242949, #246757, .T. ) ;
#253754 = ORIENTED_EDGE ( 'NONE', *, *, #83079, .T. ) ;
#253755 = DIRECTION ( 'NONE',  ( 1.000000000000000000, 0.000000000000000000, 0.000000000000000000 ) ) ;
#253756 = EDGE_LOOP ( 'NONE', ( #211801, #188732, #67306, #148632, #80570, #114797, #238279, #59998, #120021, #62368, #126372, #258056, #199285, #55071, #138388, #53122 ) ) ;
#253757 = CARTESIAN_POINT ( 'NONE',  ( 18.59999999999999076, 11.65000000001115943, -125.3500000000000512 ) ) ;
#253758 = CARTESIAN_POINT ( 'NONE',  ( 23.14999999999999503, 10.90071697730193456, -220.2717246083756208 ) ) ;
#253759 = DIRECTION ( 'NONE',  ( 1.441126678808781001E-14, -0.9942466578594195692, 0.1071148137998398919 ) ) ;
#253760 = DIRECTION ( 'NONE',  ( 1.000000000000000000, 0.000000000000000000, 0.000000000000000000 ) ) ;
#253761 = ORIENTED_EDGE ( 'NONE', *, *, #193734, .F. ) ;
#253762 = DIRECTION ( 'NONE',  ( 0.000000000000000000, -0.4999999999999608646, -0.8660254037844612451 ) ) ;
#253763 = CARTESIAN_POINT ( 'NONE',  ( 18.42636655943170254, 86.89577902249435226, -199.6303068441001187 ) ) ;
#253764 = AXIS2_PLACEMENT_3D ( 'NONE', #240891, #222577, #103909 ) ;
#253765 = CARTESIAN_POINT ( 'NONE',  ( 18.55121869061587958, 10.32747123227773400, -139.5774032850249569 ) ) ;
#253766 = ORIENTED_EDGE ( 'NONE', *, *, #31925, .F. ) ;
#253767 = ADVANCED_FACE ( 'NONE', ( #201221 ), #181675, .T. ) ;
#253768 = CARTESIAN_POINT ( 'NONE',  ( 21.00023020733438273, 6.244489974106956609, -199.6400166642470140 ) ) ;
#253769 = ORIENTED_EDGE ( 'NONE', *, *, #153621, .F. ) ;
#253770 = FACE_OUTER_BOUND ( 'NONE', #54178, .T. ) ;
#253771 = ORIENTED_EDGE ( 'NONE', *, *, #9033, .F. ) ;
#253772 = DIRECTION ( 'NONE',  ( 1.000000000000000000, 0.000000000000000000, 0.000000000000000000 ) ) ;
#253773 = CYLINDRICAL_SURFACE ( 'NONE', #60309, 0.1000000000000026007 ) ;
#253775 = EDGE_LOOP ( 'NONE', ( #70295, #89775, #46332, #51456 ) ) ;
#253774 = DIRECTION ( 'NONE',  ( 1.000000000000000000, -0.000000000000000000, -0.000000000000000000 ) ) ;
#253776 = CARTESIAN_POINT ( 'NONE',  ( 18.59999999999999076, 10.20857864377385127, -155.3500000000000227 ) ) ;
#253777 = EDGE_LOOP ( 'NONE', ( #197631, #72662, #253267, #187937, #43010 ) ) ;
#253778 = EDGE_CURVE ( 'NONE', #36405, #181631, #72000, .T. ) ;
#253779 = CARTESIAN_POINT ( 'NONE',  ( -16.80070461187914788, 9.950000000011138823, -113.1469638291613649 ) ) ;
#253780 = EDGE_CURVE ( 'NONE', #116426, #110689, #131954, .T. ) ;
#253781 = EDGE_LOOP ( 'NONE', ( #200452, #140977, #69572, #72343 ) ) ;
#253782 = TOROIDAL_SURFACE ( 'NONE', #258045, 12.77499999999999858, 0.1000000000000000056 ) ;
#253784 = CIRCLE ( 'NONE', #208034, 0.4999999999999987232 ) ;
#253783 = CARTESIAN_POINT ( 'NONE',  ( 21.05000000000000071, 4.999999999999997335, -21.09473398108690390 ) ) ;
#253785 = CARTESIAN_POINT ( 'NONE',  ( -20.99551997958277383, 11.75000000001053202, -194.1516591376910128 ) ) ;
#253786 = EDGE_LOOP ( 'NONE', ( #249311, #245098, #243067, #115573 ) ) ;
#253787 = VECTOR ( 'NONE', #190857, 1000.000000000000000 ) ;
#253789 = DIRECTION ( 'NONE',  ( -1.000000000000000000, 0.000000000000000000, 0.000000000000000000 ) ) ;
#253788 = AXIS2_PLACEMENT_3D ( 'NONE', #255444, #18170, #136826 ) ;
#253790 = ORIENTED_EDGE ( 'NONE', *, *, #121649, .F. ) ;
#253791 = EDGE_CURVE ( 'NONE', #206647, #93015, #73232, .T. ) ;
#253792 = CARTESIAN_POINT ( 'NONE',  ( 13.88638282980484639, 9.457426452500058645, -119.0000418684000749 ) ) ;
#253793 = AXIS2_PLACEMENT_3D ( 'NONE', #234710, #53502, #114761 ) ;
#253794 = LINE ( 'NONE', #171741, #97072 ) ;
#253795 = EDGE_CURVE ( 'NONE', #45115, #146870, #223022, .T. ) ;
#253796 = ADVANCED_FACE ( 'NONE', ( #111111 ), #248053, .T. ) ;
#253798 = ORIENTED_EDGE ( 'NONE', *, *, #175034, .F. ) ;
#253797 = DIRECTION ( 'NONE',  ( -1.000000000000000000, 0.000000000000000000, 0.000000000000000000 ) ) ;
#253800 = CARTESIAN_POINT ( 'NONE',  ( 21.00000000000000000, 66.25000000001206502, -124.2731074845243597 ) ) ;
#253799 = AXIS2_PLACEMENT_3D ( 'NONE', #138967, #80277, #218513 ) ;
#253801 = VECTOR ( 'NONE', #149731, 1000.000000000000000 ) ;
#253802 = CARTESIAN_POINT ( 'NONE',  ( 23.24999999999999645, 3.900000000011155432, -67.00000000000000000 ) ) ;
#253803 = B_SPLINE_CURVE_WITH_KNOTS ( 'NONE', 3,
 ( #31417, #47070, #107050, #190483, #71808, #129203, #110914, #246562 ),
 .UNSPECIFIED., .F., .F.,
 ( 4, 2, 2, 4 ),
 ( 0.000000000000000000, 9.550056980124347803E-05, 0.0001910011396024869561, 0.0003820022792049804173 ),
 .UNSPECIFIED. ) ;
#253804 = DIRECTION ( 'NONE',  ( 0.000000000000000000, 0.000000000000000000, -1.000000000000000000 ) ) ;
#253805 = TOROIDAL_SURFACE ( 'NONE', #99678, 0.2000000000000000111, 0.1000000000000000056 ) ;
#253806 = ADVANCED_FACE ( 'NONE', ( #70732 ), #193230, .F. ) ;
#253808 = CYLINDRICAL_SURFACE ( 'NONE', #101089, 0.1000000000000028644 ) ;
#253807 = CARTESIAN_POINT ( 'NONE',  ( 20.46382478191415188, 59.01186707245664564, -225.6707791561468639 ) ) ;
#253809 = DIRECTION ( 'NONE',  ( 0.000000000000000000, 0.4088369013363281623, -0.9126074666063771490 ) ) ;
#253810 = FACE_OUTER_BOUND ( 'NONE', #87658, .T. ) ;
#253811 = CARTESIAN_POINT ( 'NONE',  ( 22.50000000000000000, 7.790779598384538929, -133.9000000000000057 ) ) ;
#253812 = LINE ( 'NONE', #152192, #71752 ) ;
#253813 = AXIS2_PLACEMENT_3D ( 'NONE', #221179, #142914, #42549 ) ;
#253814 = VERTEX_POINT ( 'NONE', #189376 ) ;
#253815 = ORIENTED_EDGE ( 'NONE', *, *, #1169, .F. ) ;
#253816 = CARTESIAN_POINT ( 'NONE',  ( -20.94999999999999929, 38.29773864426885410, -236.0513742605307925 ) ) ;
#253818 = ORIENTED_EDGE ( 'NONE', *, *, #219564, .T. ) ;
#253817 = DIRECTION ( 'NONE',  ( 0.000000000000000000, -1.000000000000000000, -6.982962677686265922E-15 ) ) ;
#253819 = ORIENTED_EDGE ( 'NONE', *, *, #144457, .T. ) ;
#253820 = EDGE_CURVE ( 'NONE', #245009, #239159, #168906, .T. ) ;
#253821 = LINE ( 'NONE', #256333, #172735 ) ;
#253822 = EDGE_LOOP ( 'NONE', ( #4290, #226663, #149686, #247147 ) ) ;
#253823 = CARTESIAN_POINT ( 'NONE',  ( 21.08804281139605408, 43.58702878209024334, -234.8084616901626873 ) ) ;
#253824 = ORIENTED_EDGE ( 'NONE', *, *, #179917, .T. ) ;
#253825 =( NAMED_UNIT ( * ) PLANE_ANGLE_UNIT ( ) SI_UNIT ( $, .RADIAN. ) );
#253826 = CARTESIAN_POINT ( 'NONE',  ( -22.50000000000000000, -2.479040261793999722, -189.6172560698084624 ) ) ;
#253827 = CIRCLE ( 'NONE', #33142, 7.800000000000001599 ) ;
#253829 = ORIENTED_EDGE ( 'NONE', *, *, #24328, .F. ) ;
#253828 = VERTEX_POINT ( 'NONE', #30307 ) ;
#253830 = ORIENTED_EDGE ( 'NONE', *, *, #232078, .F. ) ;
#253831 = ORIENTED_EDGE ( 'NONE', *, *, #41153, .F. ) ;
#253832 = EDGE_LOOP ( 'NONE', ( #31570, #223426, #73712, #112353 ) ) ;
#253833 = CARTESIAN_POINT ( 'NONE',  ( -20.94999999999994600, 64.35000000001119247, -5.923107484524795296 ) ) ;
#253834 = DIRECTION ( 'NONE',  ( 0.000000000000000000, 0.000000000000000000, -1.000000000000000000 ) ) ;
#253835 = DIRECTION ( 'NONE',  ( -1.000000000000000000, -0.000000000000000000, 0.000000000000000000 ) ) ;
#253837 = ORIENTED_EDGE ( 'NONE', *, *, #23845, .F. ) ;
#253836 = DIRECTION ( 'NONE',  ( 1.000000000000000000, 0.000000000000000000, 0.000000000000000000 ) ) ;
#253838 = AXIS2_PLACEMENT_3D ( 'NONE', #233691, #134553, #77164 ) ;
#253839 = CARTESIAN_POINT ( 'NONE',  ( 20.97217846901851956, 40.78860018870523163, -237.9757527299901199 ) ) ;
#253840 = DIRECTION ( 'NONE',  ( 1.000000000000000000, 0.000000000000000000, 0.000000000000000000 ) ) ;
#253842 = ORIENTED_EDGE ( 'NONE', *, *, #99439, .F. ) ;
#253841 = DIRECTION ( 'NONE',  ( 1.000000000000000000, 0.000000000000000000, 0.000000000000000000 ) ) ;
#253843 = CARTESIAN_POINT ( 'NONE',  ( -16.87683809663752399, 22.93084817181464530, -231.0232129367395260 ) ) ;
#253844 = VERTEX_POINT ( 'NONE', #69438 ) ;
#253846 = ORIENTED_EDGE ( 'NONE', *, *, #63243, .T. ) ;
#253845 = CARTESIAN_POINT ( 'NONE',  ( -21.07928932188134041, 6.328516656404449492, -167.4011048543455615 ) ) ;
#253847 = CARTESIAN_POINT ( 'NONE',  ( 20.90000000000000213, -1.212568896937008089, -8.000000000000000000 ) ) ;
#253848 = DIRECTION ( 'NONE',  ( -4.448008912761041834E-16, 0.4721928772777335692, 0.8814952561688436106 ) ) ;
#253849 = ORIENTED_EDGE ( 'NONE', *, *, #106210, .T. ) ;
#253851 = CARTESIAN_POINT ( 'NONE',  ( -22.39999999999999858, 0.1000000000111554016, -59.20922040162664501 ) ) ;
#253850 = CARTESIAN_POINT ( 'NONE',  ( -16.77308656112215246, 9.950000000011137047, -46.15019319170230716 ) ) ;
#253852 = AXIS2_PLACEMENT_3D ( 'NONE', #127953, #45840, #144922 ) ;
#253853 = CARTESIAN_POINT ( 'NONE',  ( 22.32929514600007792, 7.578647565387638174, -133.9009243218860945 ) ) ;
#253854 = ADVANCED_FACE ( 'NONE', ( #14607 ), #109816, .T. ) ;
#253855 = DIRECTION ( 'NONE',  ( 1.000000000000000000, 0.000000000000000000, 0.000000000000000000 ) ) ;
#253856 = CYLINDRICAL_SURFACE ( 'NONE', #76693, 0.09999999999999892308 ) ;
#253857 = TOROIDAL_SURFACE ( 'NONE', #158073, 0.6000000000000017542, 0.1000000000000000056 ) ;
#253858 = VERTEX_POINT ( 'NONE', #150258 ) ;
#253859 = ORIENTED_EDGE ( 'NONE', *, *, #76582, .T. ) ;
#253860 = DIRECTION ( 'NONE',  ( 0.000000000000000000, 0.000000000000000000, -1.000000000000000000 ) ) ;
#253861 = FACE_OUTER_BOUND ( 'NONE', #148762, .T. ) ;
#253862 = VERTEX_POINT ( 'NONE', #113675 ) ;
#253864 = CARTESIAN_POINT ( 'NONE',  ( 20.90000000000000213, 1.410778198689825347, -7.973296578895943121 ) ) ;
#253863 = VECTOR ( 'NONE', #33313, 1000.000000000000114 ) ;
#253865 = VERTEX_POINT ( 'NONE', #49849 ) ;
#253866 = DIRECTION ( 'NONE',  ( -1.000000000000000000, 0.000000000000000000, -0.000000000000000000 ) ) ;
#253867 = EDGE_CURVE ( 'NONE', #151223, #185811, #229774, .T. ) ;
#253868 = CARTESIAN_POINT ( 'NONE',  ( 20.94999999999999929, 87.65000000001192859, -105.9231074845242091 ) ) ;
#253869 = VECTOR ( 'NONE', #216389, 1000.000000000000000 ) ;
#253870 = AXIS2_PLACEMENT_3D ( 'NONE', #195011, #97126, #176728 ) ;
#253871 = EDGE_CURVE ( 'NONE', #240058, #151240, #194019, .T. ) ;
#253872 = EDGE_CURVE ( 'NONE', #254486, #242741, #202189, .T. ) ;
#253873 = EDGE_LOOP ( 'NONE', ( #92324, #105572, #90907, #15465 ) ) ;
#253874 = DIRECTION ( 'NONE',  ( 1.000000000000000000, 0.000000000000000000, 0.000000000000000000 ) ) ;
#253875 =( NAMED_UNIT ( * ) SI_UNIT ( $, .STERADIAN. ) SOLID_ANGLE_UNIT ( ) );
#253877 = VERTEX_POINT ( 'NONE', #210233 ) ;
#253876 = AXIS2_PLACEMENT_3D ( 'NONE', #223742, #145497, #146757 ) ;
#253878 = ORIENTED_EDGE ( 'NONE', *, *, #130897, .T. ) ;
#253879 = CIRCLE ( 'NONE', #199754, 11.70000000000000284 ) ;
#253880 = AXIS2_PLACEMENT_3D ( 'NONE', #178903, #98010, #233716 ) ;
#253881 = ORIENTED_EDGE ( 'NONE', *, *, #173785, .F. ) ;
#253882 = AXIS2_PLACEMENT_3D ( 'NONE', #28444, #107936, #131346 ) ;
#253883 = CIRCLE ( 'NONE', #20687, 0.1000000000000021289 ) ;
#253884 = DIRECTION ( 'NONE',  ( -1.000000000000000000, -0.000000000000000000, -0.000000000000000000 ) ) ;
#253885 = DIRECTION ( 'NONE',  ( 0.000000000000000000, -1.000000000000000000, 0.000000000000000000 ) ) ;
#253886 = DIRECTION ( 'NONE',  ( 0.000000000000000000, -6.938893903907222067E-15, 1.000000000000000000 ) ) ;
#253887 = DIRECTION ( 'NONE',  ( 0.000000000000000000, -0.1350103645451945777, 0.9908441862701590219 ) ) ;
#253888 = ADVANCED_FACE ( 'NONE', ( #211501 ), #228506, .T. ) ;
#253890 = CARTESIAN_POINT ( 'NONE',  ( -23.25000000000000000, 76.00000000001165290, -69.52310748452431710 ) ) ;
#253889 = CARTESIAN_POINT ( 'NONE',  ( 21.05000000000000071, -0.02138556592634376433, -161.1950388873158317 ) ) ;
#253892 = ORIENTED_EDGE ( 'NONE', *, *, #211534, .F. ) ;
#253891 = FACE_OUTER_BOUND ( 'NONE', #80590, .T. ) ;
#253893 = PLANE ( 'NONE',  #133382 ) ;
#253894 = VERTEX_POINT ( 'NONE', #32905 ) ;
#253895 = CARTESIAN_POINT ( 'NONE',  ( -16.87036670365549895, 22.88247411645692253, -230.8391385443351282 ) ) ;
#253896 = ORIENTED_EDGE ( 'NONE', *, *, #61182, .T. ) ;
#253897 = ORIENTED_EDGE ( 'NONE', *, *, #63720, .T. ) ;
#253898 = DIRECTION ( 'NONE',  ( 1.000000000000000000, 3.265361837132813093E-16, -0.000000000000000000 ) ) ;
#253899 = CARTESIAN_POINT ( 'NONE',  ( -21.05000000000000071, 6.478078221105875834, -134.0999999353045098 ) ) ;
#253900 = CARTESIAN_POINT ( 'NONE',  ( 20.94999999999999929, 76.00000000001188027, -98.92310748452429436 ) ) ;
#253901 = CARTESIAN_POINT ( 'NONE',  ( 21.00000000000000000, 9.750000000011153745, -79.35000000000005116 ) ) ;
#253902 = DIRECTION ( 'NONE',  ( 0.000000000000000000, 0.9126074666063844765, 0.4088369013363114535 ) ) ;
#253903 = ORIENTED_EDGE ( 'NONE', *, *, #46841, .F. ) ;
#253904 = VERTEX_POINT ( 'NONE', #173707 ) ;
#253905 = DIRECTION ( 'NONE',  ( -1.000000000000000000, 0.000000000000000000, 0.000000000000000000 ) ) ;
#253907 = ORIENTED_EDGE ( 'NONE', *, *, #114112, .T. ) ;
#253906 = EDGE_CURVE ( 'NONE', #122105, #18925, #48564, .T. ) ;
#253908 = DIRECTION ( 'NONE',  ( 6.484947573744954877E-15, 0.9274965247785529332, -0.3738317757009255171 ) ) ;
#253909 = CARTESIAN_POINT ( 'NONE',  ( 23.14999999999999858, 69.35000000001205933, -124.1731074845243370 ) ) ;
#253910 = VERTEX_POINT ( 'NONE', #227203 ) ;
#253911 = EDGE_CURVE ( 'NONE', #88007, #117767, #128115, .T. ) ;
#253912 = DIRECTION ( 'NONE',  ( 1.073024830501117725E-15, 0.000000000000000000, 1.000000000000000000 ) ) ;
#253913 = CARTESIAN_POINT ( 'NONE',  ( 18.59999999999999432, 74.26374286841490857, -158.4544551555068779 ) ) ;
#253914 = CARTESIAN_POINT ( 'NONE',  ( -22.49231231312463208, 64.35001509633437422, -69.58416037212577976 ) ) ;
#253915 = CARTESIAN_POINT ( 'NONE',  ( -23.25000000000000000, 81.82295291318693842, -214.8938525951558915 ) ) ;
#253916 = ORIENTED_EDGE ( 'NONE', *, *, #123615, .T. ) ;
#253917 = VECTOR ( 'NONE', #76074, 1000.000000000000227 ) ;
#253918 = DIRECTION ( 'NONE',  ( 1.000000000000000000, 0.000000000000000000, 0.000000000000000000 ) ) ;
#253919 = DIRECTION ( 'NONE',  ( 0.000000000000000000, -0.8660254037844412611, -0.4999999999999956701 ) ) ;
#253920 = EDGE_CURVE ( 'NONE', #201487, #99338, #114894, .T. ) ;
#253921 = CARTESIAN_POINT ( 'NONE',  ( 20.85000000000000142, 7.070967871809997973, -104.2465642218683541 ) ) ;
#253922 = AXIS2_PLACEMENT_3D ( 'NONE', #53477, #10510, #52176 ) ;
#253923 = VERTEX_POINT ( 'NONE', #95400 ) ;
#253924 = DIRECTION ( 'NONE',  ( 0.000000000000000000, 0.2617529984164955192, 0.9651348961777178603 ) ) ;
#253925 = EDGE_LOOP ( 'NONE', ( #250950, #63360, #35624, #192829, #66197, #42805, #120357, #118782, #81541, #124460 ) ) ;
#253926 = CARTESIAN_POINT ( 'NONE',  ( -20.94999999999999929, 43.57568952063339651, -245.1784935019914826 ) ) ;
#253927 = DIRECTION ( 'NONE',  ( 0.000000000000000000, -0.8127272543710951647, 0.5826443254700257590 ) ) ;
#253928 = CARTESIAN_POINT ( 'NONE',  ( -21.14999999999999858, 76.00000000001242029, -176.2816861282870775 ) ) ;
#253929 = DIRECTION ( 'NONE',  ( 0.000000000000000000, -6.982962677686266711E-15, 1.000000000000000000 ) ) ;
#253930 = FACE_OUTER_BOUND ( 'NONE', #52605, .T. ) ;
#253931 = LINE ( 'NONE', #92299, #252748 ) ;
#253932 = EDGE_LOOP ( 'NONE', ( #148946, #180746, #246234, #138077 ) ) ;
#253933 = EDGE_CURVE ( 'NONE', #50484, #163089, #254444, .T. ) ;
#253934 = CARTESIAN_POINT ( 'NONE',  ( -16.93583594267724379, 65.99137656495986448, -123.9637166452036183 ) ) ;
#253935 = VECTOR ( 'NONE', #105613, 1000.000000000000000 ) ;
#253936 = DIRECTION ( 'NONE',  ( 1.000000000000000000, 0.000000000000000000, 0.000000000000000000 ) ) ;
#253937 = CARTESIAN_POINT ( 'NONE',  ( 21.07016717456945187, 10.11353658153798563, -228.1608219491299678 ) ) ;
#253938 = CARTESIAN_POINT ( 'NONE',  ( 21.05000000000000071, -1.736257131586239844, -145.5686523290175387 ) ) ;
#253939 = CARTESIAN_POINT ( 'NONE',  ( -18.50000000000000355, -1.263275465206102233, -175.4018646667464338 ) ) ;
#253940 = VERTEX_POINT ( 'NONE', #174989 ) ;
#253941 = VERTEX_POINT ( 'NONE', #216626 ) ;
#253942 = DIRECTION ( 'NONE',  ( 2.952720810173290098E-16, -0.4721928772777468364, -0.8814952561688365051 ) ) ;
#253943 = FACE_OUTER_BOUND ( 'NONE', #144942, .T. ) ;
#253945 = ADVANCED_FACE ( 'NONE', ( #139635 ), #19729, .F. ) ;
#253944 = CARTESIAN_POINT ( 'NONE',  ( 18.43709777086139567, -9.682403433476389765, -40.15684337741277687 ) ) ;
#253946 = DIRECTION ( 'NONE',  ( 0.000000000000000000, 0.000000000000000000, -1.000000000000000000 ) ) ;
#253947 = DIRECTION ( 'NONE',  ( -1.000000000000000000, 0.000000000000000000, 0.000000000000000000 ) ) ;
#253948 = ORIENTED_EDGE ( 'NONE', *, *, #234159, .F. ) ;
#253949 = DIRECTION ( 'NONE',  ( 0.000000000000000000, -0.2128009952263403282, 0.9770955615653358350 ) ) ;
#253950 = EDGE_CURVE ( 'NONE', #3082, #105588, #89749, .T. ) ;
#253951 = ADVANCED_FACE ( 'NONE', ( #138351 ), #6548, .T. ) ;
#253952 = DIRECTION ( 'NONE',  ( -1.000000000000000000, -0.000000000000000000, -0.000000000000000000 ) ) ;
#253953 = ORIENTED_EDGE ( 'NONE', *, *, #5178, .T. ) ;
#253954 = FACE_OUTER_BOUND ( 'NONE', #19085, .T. ) ;
#253955 = CIRCLE ( 'NONE', #62452, 0.1000000000000028783 ) ;
#253956 = AXIS2_PLACEMENT_3D ( 'NONE', #70959, #170071, #154361 ) ;
#253957 = DIRECTION ( 'NONE',  ( -0.000000000000000000, -1.000000000000000000, -6.982962677686266711E-15 ) ) ;
#253958 = ADVANCED_FACE ( 'NONE', ( #195813 ), #143917, .T. ) ;
#253959 = ADVANCED_FACE ( 'NONE', ( #40603 ), #38023, .F. ) ;
#253960 = ORIENTED_EDGE ( 'NONE', *, *, #23875, .T. ) ;
#253961 = DIRECTION ( 'NONE',  ( 0.000000000000000000, -0.7049548389605067023, 0.7092521942342977503 ) ) ;
#253962 = ORIENTED_EDGE ( 'NONE', *, *, #218595, .T. ) ;
#253963 = FACE_OUTER_BOUND ( 'NONE', #42732, .T. ) ;
#253964 = CARTESIAN_POINT ( 'NONE',  ( -20.64999999999999858, 8.751106741858205140, -220.7398867978735950 ) ) ;
#253966 = EDGE_CURVE ( 'NONE', #234584, #204749, #80801, .T. ) ;
#253965 = DIRECTION ( 'NONE',  ( 1.186688945009010077E-16, 1.000000000000000000, 6.982962677686266711E-15 ) ) ;
#253967 = CARTESIAN_POINT ( 'NONE',  ( 13.40000000000000036, -8.350000000000004974, 15.00000000000000355 ) ) ;
#253968 = CARTESIAN_POINT ( 'NONE',  ( -21.05000000000000071, 77.83534155023646406, -124.9679561919613064 ) ) ;
#253969 = DIRECTION ( 'NONE',  ( 0.000000000000000000, -7.056502275159890043E-15, 1.000000000000000000 ) ) ;
#253970 = CYLINDRICAL_SURFACE ( 'NONE', #170558, 0.1000000000000008937 ) ;
#253971 = CARTESIAN_POINT ( 'NONE',  ( 23.14999999999999858, 71.00000000001230660, -157.6178414656113205 ) ) ;
#253973 = CARTESIAN_POINT ( 'NONE',  ( -23.25000000000000000, 76.00000000001192291, -98.97310748452431994 ) ) ;
#253972 = CARTESIAN_POINT ( 'NONE',  ( 20.95132126680579887, 10.48994987015794322, -108.0703245384345621 ) ) ;
#253974 = CIRCLE ( 'NONE', #125016, 0.09999999999999982514 ) ;
#253975 = EDGE_CURVE ( 'NONE', #30313, #103754, #157988, .T. ) ;
#253976 = CARTESIAN_POINT ( 'NONE',  ( -21.44999999999999929, 7.150000000011155876, -79.25000000000004263 ) ) ;
#253977 = DIRECTION ( 'NONE',  ( -1.000000000000000000, 0.000000000000000000, -0.000000000000000000 ) ) ;
#253979 = CARTESIAN_POINT ( 'NONE',  ( -21.05000000000000071, -0.09999999998884338825, -21.85000000000000142 ) ) ;
#253978 = CIRCLE ( 'NONE', #233361, 0.09999999999999602263 ) ;
#253981 = CARTESIAN_POINT ( 'NONE',  ( 20.95512820512820440, 18.90192396791320562, -227.9871466877642661 ) ) ;
#253980 = AXIS2_PLACEMENT_3D ( 'NONE', #8881, #231791, #132685 ) ;
#253982 = ORIENTED_EDGE ( 'NONE', *, *, #167886, .T. ) ;
#253983 = ADVANCED_FACE ( 'NONE', ( #214064 ), #100499, .T. ) ;
#253984 = EDGE_CURVE ( 'NONE', #193833, #117705, #2446, .T. ) ;
#253985 = CARTESIAN_POINT ( 'NONE',  ( -20.54999999999999716, 2.000000000011154189, -46.72462192276210402 ) ) ;
#253986 = DIRECTION ( 'NONE',  ( 0.000000000000000000, 0.000000000000000000, -1.000000000000000000 ) ) ;
#253987 = CIRCLE ( 'NONE', #191680, 0.4000000000000114575 ) ;
#253988 = VERTEX_POINT ( 'NONE', #35466 ) ;
#253989 = FACE_OUTER_BOUND ( 'NONE', #77026, .T. ) ;
#253991 = ADVANCED_FACE ( 'NONE', ( #114964 ), #22308, .T. ) ;
#253990 = DIRECTION ( 'NONE',  ( 0.000000000000000000, 1.000000000000000000, 0.000000000000000000 ) ) ;
#253992 = CARTESIAN_POINT ( 'NONE',  ( -20.94999999999999929, 57.82359945636608956, -226.0354702357591350 ) ) ;
#253993 = ORIENTED_EDGE ( 'NONE', *, *, #59058, .F. ) ;
#253994 = ADVANCED_FACE ( 'NONE', ( #45693 ), #103077, .F. ) ;
#253995 = AXIS2_PLACEMENT_3D ( 'NONE', #199094, #97389, #137817 ) ;
#253996 = EDGE_CURVE ( 'NONE', #252194, #171376, #121421, .T. ) ;
#253997 = FACE_OUTER_BOUND ( 'NONE', #242359, .T. ) ;
#253998 = ORIENTED_EDGE ( 'NONE', *, *, #41956, .F. ) ;
#253999 = SPHERICAL_SURFACE ( 'NONE', #92214, 0.1000000000000000056 ) ;
#254000 = DIRECTION ( 'NONE',  ( -1.000000000000000000, 0.000000000000000000, 0.000000000000000000 ) ) ;
#254001 = EDGE_CURVE ( 'NONE', #139309, #256176, #10663, .T. ) ;
#254002 = AXIS2_PLACEMENT_3D ( 'NONE', #53804, #10832, #167362 ) ;
#254003 = ORIENTED_EDGE ( 'NONE', *, *, #131381, .F. ) ;
#254004 = DIRECTION ( 'NONE',  ( 1.000000000000000000, 0.000000000000000000, 0.000000000000000000 ) ) ;
#254005 = ORIENTED_EDGE ( 'NONE', *, *, #166301, .F. ) ;
#254006 = EDGE_CURVE ( 'NONE', #176836, #42537, #146069, .T. ) ;
#254007 = CARTESIAN_POINT ( 'NONE',  ( 0.9000000000000547562, 64.35000000001120668, -12.62310748452478926 ) ) ;
#254008 = EDGE_CURVE ( 'NONE', #172675, #177620, #189893, .T. ) ;
#254009 = DIRECTION ( 'NONE',  ( 1.000000000000000000, 0.000000000000000000, 0.000000000000000000 ) ) ;
#254011 = DIRECTION ( 'NONE',  ( -4.391705002472929091E-16, 1.000000000000000000, 0.000000000000000000 ) ) ;
#254010 = PRODUCT_DEFINITION_CONTEXT ( 'detailed design', #77473, 'design' ) ;
#254012 = DIRECTION ( 'NONE',  ( -4.448008912761042820E-16, -1.000000000000000000, -7.116814260417668513E-15 ) ) ;
#254013 = CARTESIAN_POINT ( 'NONE',  ( 20.90000000000000213, 1.885425182446133885, -11.49641995933507843 ) ) ;
#254014 = CARTESIAN_POINT ( 'NONE',  ( -18.59999999999999787, 66.65000000001198543, -115.2731074845243597 ) ) ;
#254015 = CARTESIAN_POINT ( 'NONE',  ( -20.94999999999999929, 1.115600667400684642E-11, -141.9000000000000341 ) ) ;
#254016 = CARTESIAN_POINT ( 'NONE',  ( 21.05000000000000071, 5.000000000011153745, -88.49473398108695221 ) ) ;
#254018 = ORIENTED_EDGE ( 'NONE', *, *, #159800, .T. ) ;
#254017 = CYLINDRICAL_SURFACE ( 'NONE', #56879, 0.09999999999999939493 ) ;
#254019 = ORIENTED_EDGE ( 'NONE', *, *, #43647, .F. ) ;
#254021 = DIRECTION ( 'NONE',  ( 1.000000000000000000, 0.000000000000000000, 0.000000000000000000 ) ) ;
#254020 = DIRECTION ( 'NONE',  ( 1.000000000000000000, -7.304098846218135653E-16, 0.000000000000000000 ) ) ;
#254022 = ORIENTED_EDGE ( 'NONE', *, *, #82634, .T. ) ;
#254024 = VERTEX_POINT ( 'NONE', #105641 ) ;
#254023 = DIRECTION ( 'NONE',  ( 0.000000000000000000, 0.9908441862701420355, 0.1350103645453197554 ) ) ;
#254025 = AXIS2_PLACEMENT_3D ( 'NONE', #221288, #223857, #46507 ) ;
#254026 = ORIENTED_EDGE ( 'NONE', *, *, #80919, .T. ) ;
#254027 = CARTESIAN_POINT ( 'NONE',  ( -20.00857864376270001, 9.250000000011157297, -88.25000000000005684 ) ) ;
#254028 = DIRECTION ( 'NONE',  ( 0.000000000000000000, 0.1350103645451876666, 0.9908441862701600211 ) ) ;
#254029 = FACE_OUTER_BOUND ( 'NONE', #58616, .T. ) ;
#254030 = CARTESIAN_POINT ( 'NONE',  ( 21.05000000000000071, -11.74999999998883560, -103.4000000000000341 ) ) ;
#254031 = CIRCLE ( 'NONE', #154135, 0.5000000000000004441 ) ;
#254032 = LINE ( 'NONE', #201761, #198270 ) ;
#254033 = DIRECTION ( 'NONE',  ( 0.000000000000000000, -0.4721928772777346239, -0.8814952561688430555 ) ) ;
#254034 = CARTESIAN_POINT ( 'NONE',  ( -16.81744102076748959, 14.15900158805613884, -219.2550725561364118 ) ) ;
#254035 = DIRECTION ( 'NONE',  ( -0.000000000000000000, -0.000000000000000000, -1.000000000000000000 ) ) ;
#254037 = ORIENTED_EDGE ( 'NONE', *, *, #62538, .T. ) ;
#254036 = ADVANCED_FACE ( 'NONE', ( #221737 ), #44428, .T. ) ;
#254038 = ORIENTED_EDGE ( 'NONE', *, *, #86400, .F. ) ;
#254039 = CARTESIAN_POINT ( 'NONE',  ( 20.85000000000000142, 64.25000000001190870, -103.0231074845243882 ) ) ;
#254040 = AXIS2_PLACEMENT_3D ( 'NONE', #27293, #246308, #225433 ) ;
#254041 = EDGE_CURVE ( 'NONE', #136089, #195479, #102367, .T. ) ;
#254042 = ORIENTED_EDGE ( 'NONE', *, *, #132758, .F. ) ;
#254043 = SPHERICAL_SURFACE ( 'NONE', #209285, 0.1000000000000000056 ) ;
#254045 = ORIENTED_EDGE ( 'NONE', *, *, #226367, .F. ) ;
#254044 = AXIS2_PLACEMENT_3D ( 'NONE', #123823, #85935, #164238 ) ;
#254046 = DIRECTION ( 'NONE',  ( 0.000000000000000000, 0.8814952561688439436, -0.4721928772777332362 ) ) ;
#254047 = LINE ( 'NONE', #233243, #71816 ) ;
#254048 = DIRECTION ( 'NONE',  ( -1.000000000000000000, 0.000000000000000000, 0.000000000000000000 ) ) ;
#254050 = ORIENTED_EDGE ( 'NONE', *, *, #187017, .F. ) ;
#254049 = CARTESIAN_POINT ( 'NONE',  ( -23.25000000000000355, 8.212522512469059066, -212.1579332307740344 ) ) ;
#254051 = CYLINDRICAL_SURFACE ( 'NONE', #170603, 0.09999999999999939493 ) ;
#254052 = ORIENTED_EDGE ( 'NONE', *, *, #79073, .F. ) ;
#254053 = CIRCLE ( 'NONE', #145711, 0.09999999999999484301 ) ;
#254055 = AXIS2_PLACEMENT_3D ( 'NONE', #115801, #235733, #57078 ) ;
#254054 = DIRECTION ( 'NONE',  ( 1.000000000000000000, 0.000000000000000000, 0.000000000000000000 ) ) ;
#254056 = FACE_OUTER_BOUND ( 'NONE', #4970, .T. ) ;
#254057 = DIRECTION ( 'NONE',  ( -1.000000000000000000, -0.000000000000000000, 0.000000000000000000 ) ) ;
#254058 = CARTESIAN_POINT ( 'NONE',  ( -23.39999999999994529, 74.15089172278851493, -47.62873275725970501 ) ) ;
#254059 = DIRECTION ( 'NONE',  ( -1.000000000000000000, 0.000000000000000000, 0.000000000000000000 ) ) ;
#254060 = ADVANCED_FACE ( 'NONE', ( #24879 ), #202209, .T. ) ;
#254061 = ORIENTED_EDGE ( 'NONE', *, *, #219609, .F. ) ;
#254063 = CARTESIAN_POINT ( 'NONE',  ( -21.64999999999999858, 68.65000000001229807, -157.6731074845243938 ) ) ;
#254062 = CARTESIAN_POINT ( 'NONE',  ( -22.94999999999999929, 11.59510167572422112, -1.901609089591594692 ) ) ;
#254064 = ORIENTED_EDGE ( 'NONE', *, *, #125197, .F. ) ;
#254067 = EDGE_LOOP ( 'NONE', ( #116220, #142930, #54955, #178895 ) ) ;
#254066 = DIRECTION ( 'NONE',  ( 0.000000000000000000, 0.8814952561688476074, -0.4721928772777262417 ) ) ;
#254065 = DIRECTION ( 'NONE',  ( -1.020425574104004196E-15, -1.210927747993693964E-31, -1.000000000000000000 ) ) ;
#254068 = VECTOR ( 'NONE', #181153, 1000.000000000000114 ) ;
#254069 = DIRECTION ( 'NONE',  ( -1.000000000000000000, 2.849773892568378313E-16, -7.728835255496647986E-17 ) ) ;
#254070 = CIRCLE ( 'NONE', #237335, 0.1000000000000004496 ) ;
#254071 = AXIS2_PLACEMENT_3D ( 'NONE', #135564, #16929, #97702 ) ;
#254072 = CIRCLE ( 'NONE', #158438, 0.09999999999999982514 ) ;
#254073 = DIRECTION ( 'NONE',  ( 0.000000000000000000, -0.2128009952263604232, 0.9770955615653315052 ) ) ;
#254074 = ORIENTED_EDGE ( 'NONE', *, *, #36632, .F. ) ;
#254075 = CARTESIAN_POINT ( 'NONE',  ( -21.05000000000000071, 1.115600667400684642E-11, -55.30000000000000426 ) ) ;
#254076 = AXIS2_PLACEMENT_3D ( 'NONE', #250679, #167328, #8239 ) ;
#254077 = CARTESIAN_POINT ( 'NONE',  ( 23.04999999999999716, 8.822561741677553471, -176.7499999999999716 ) ) ;
#254079 = ORIENTED_EDGE ( 'NONE', *, *, #190794, .F. ) ;
#254078 = CARTESIAN_POINT ( 'NONE',  ( 20.94999999999999574, 1.835341550224411922, -11.55515129256298046 ) ) ;
#254080 = VERTEX_POINT ( 'NONE', #245190 ) ;
#254081 = DIRECTION ( 'NONE',  ( 1.000000000000000000, 0.000000000000000000, 0.000000000000000000 ) ) ;
#254082 = DIRECTION ( 'NONE',  ( -1.000000000000000000, -0.000000000000000000, -0.000000000000000000 ) ) ;
#254083 = FACE_OUTER_BOUND ( 'NONE', #200818, .T. ) ;
#254084 = DIRECTION ( 'NONE',  ( -1.000000000000000000, -3.265361837132813093E-16, 0.000000000000000000 ) ) ;
#254085 = ORIENTED_EDGE ( 'NONE', *, *, #108814, .F. ) ;
#254086 = DIRECTION ( 'NONE',  ( -0.000000000000000000, 0.1298341882519668811, 0.9915357197604899309 ) ) ;
#254087 = DIRECTION ( 'NONE',  ( 1.000000000000000000, 0.000000000000000000, 0.000000000000000000 ) ) ;
#254088 = CARTESIAN_POINT ( 'NONE',  ( -17.01764560440443930, 9.950000000011138823, -46.24999999921458738 ) ) ;
#254089 = ORIENTED_EDGE ( 'NONE', *, *, #38099, .T. ) ;
#254090 = CARTESIAN_POINT ( 'NONE',  ( 20.30531438145590784, 59.52703403250789904, -225.6880235420007352 ) ) ;
#254091 = ADVANCED_FACE ( 'NONE', ( #3998 ), #106674, .F. ) ;
#254092 = CIRCLE ( 'NONE', #95872, 0.09999999999999939493 ) ;
#254093 = DIRECTION ( 'NONE',  ( 0.000000000000000000, 0.2617529984165503087, 0.9651348961777028723 ) ) ;
#254094 = AXIS2_PLACEMENT_3D ( 'NONE', #75509, #153793, #194172 ) ;
#254095 = EDGE_CURVE ( 'NONE', #74203, #98621, #181544, .T. ) ;
#254096 = ORIENTED_EDGE ( 'NONE', *, *, #147658, .F. ) ;
#254097 = FACE_OUTER_BOUND ( 'NONE', #122336, .T. ) ;
#254098 = DIRECTION ( 'NONE',  ( 1.000000000000000000, 0.000000000000000000, 0.000000000000000000 ) ) ;
#254099 = AXIS2_PLACEMENT_3D ( 'NONE', #48022, #188824, #207116 ) ;
#254100 = ORIENTED_EDGE ( 'NONE', *, *, #209231, .T. ) ;
#254101 = ORIENTED_EDGE ( 'NONE', *, *, #85531, .F. ) ;
#254102 = EDGE_CURVE ( 'NONE', #41617, #8661, #244052, .T. ) ;
#254103 = CARTESIAN_POINT ( 'NONE',  ( 19.58285714285715073, 66.98499851036373798, -161.6024546684427037 ) ) ;
#254104 = ORIENTED_EDGE ( 'NONE', *, *, #246555, .F. ) ;
#254106 = VERTEX_POINT ( 'NONE', #106940 ) ;
#254105 = DIRECTION ( 'NONE',  ( 1.000000000000000000, 0.000000000000000000, 0.000000000000000000 ) ) ;
#254107 = EDGE_CURVE ( 'NONE', #105519, #205739, #173381, .T. ) ;
#254108 = AXIS2_PLACEMENT_3D ( 'NONE', #206523, #164837, #146526 ) ;
#254111 = ORIENTED_EDGE ( 'NONE', *, *, #51924, .T. ) ;
#254110 = VERTEX_POINT ( 'NONE', #2703 ) ;
#254109 = CARTESIAN_POINT ( 'NONE',  ( 21.93642651522410603, 60.15957072538984107, -233.9372187734386728 ) ) ;
#254112 = CIRCLE ( 'NONE', #83409, 0.09999999999999722999 ) ;
#254113 = DIRECTION ( 'NONE',  ( -1.000000000000000000, 0.000000000000000000, 0.000000000000000000 ) ) ;
#254114 = EDGE_CURVE ( 'NONE', #145044, #109487, #243889, .T. ) ;
#254115 = CARTESIAN_POINT ( 'NONE',  ( -16.92280123533699054, 12.45672818331194520, -211.4389258949002226 ) ) ;
#254116 = CARTESIAN_POINT ( 'NONE',  ( 23.14999999999998437, 76.00000000001267608, -203.5231074845243597 ) ) ;
#254117 = CIRCLE ( 'NONE', #149924, 0.1000000000000028783 ) ;
#254118 = FACE_OUTER_BOUND ( 'NONE', #57219, .T. ) ;
#254119 = CIRCLE ( 'NONE', #216717, 0.1000000000000028644 ) ;
#254120 = LINE ( 'NONE', #195475, #234660 ) ;
#254121 = CARTESIAN_POINT ( 'NONE',  ( -18.39999999999999858, 86.98067499225015808, -199.3289525933214463 ) ) ;
#254122 = VERTEX_POINT ( 'NONE', #163098 ) ;
#254123 = ORIENTED_EDGE ( 'NONE', *, *, #182302, .T. ) ;
#254124 = VERTEX_POINT ( 'NONE', #242600 ) ;
#254125 = PLANE ( 'NONE',  #54028 ) ;
#254127 = VERTEX_POINT ( 'NONE', #144773 ) ;
#254126 = CARTESIAN_POINT ( 'NONE',  ( 20.94999999999999574, 14.85285025691667293, -236.4388300032497057 ) ) ;
#254128 = CARTESIAN_POINT ( 'NONE',  ( 21.00000000000000000, 9.750000000011153745, -179.8499999999999943 ) ) ;
#254129 = ORIENTED_EDGE ( 'NONE', *, *, #50259, .T. ) ;
#254130 = ADVANCED_FACE ( 'NONE', ( #65257 ), #200919, .T. ) ;
#254131 = FACE_OUTER_BOUND ( 'NONE', #112562, .T. ) ;
#254132 = ORIENTED_EDGE ( 'NONE', *, *, #148405, .F. ) ;
#254133 = DIRECTION ( 'NONE',  ( -1.000000000000000000, -2.885090398161910739E-16, -6.283419270304611573E-17 ) ) ;
#254134 = ORIENTED_EDGE ( 'NONE', *, *, #24399, .T. ) ;
#254135 = AXIS2_PLACEMENT_3D ( 'NONE', #62074, #43793, #2074 ) ;
#254136 = AXIS2_PLACEMENT_3D ( 'NONE', #72916, #131572, #113289 ) ;
#254137 = CARTESIAN_POINT ( 'NONE',  ( -19.99999999999999645, 11.61130914238355771, 22.00000000000000355 ) ) ;
#254138 = LINE ( 'NONE', #98895, #102801 ) ;
#254140 = ORIENTED_EDGE ( 'NONE', *, *, #125044, .T. ) ;
#254139 = VERTEX_POINT ( 'NONE', #172106 ) ;
#254141 = VERTEX_POINT ( 'NONE', #189062 ) ;
#254142 = CARTESIAN_POINT ( 'NONE',  ( -20.85000000000000142, 87.75000000001142553, -36.02310748452423894 ) ) ;
#254143 = EDGE_LOOP ( 'NONE', ( #144353, #20958, #30826, #103713 ) ) ;
#254144 = ORIENTED_EDGE ( 'NONE', *, *, #128146, .T. ) ;
#254145 = DIRECTION ( 'NONE',  ( 1.000000000000000000, 0.000000000000000000, 0.000000000000000000 ) ) ;
#254147 = ORIENTED_EDGE ( 'NONE', *, *, #167127, .F. ) ;
#254146 = CARTESIAN_POINT ( 'NONE',  ( 18.31325810956244382, -9.536388475995861924, -107.3684402063055074 ) ) ;
#254148 = SPHERICAL_SURFACE ( 'NONE', #164946, 0.1000000000000000056 ) ;
#254150 = DIRECTION ( 'NONE',  ( 1.000000000000000000, 0.000000000000000000, 0.000000000000000000 ) ) ;
#254149 = CARTESIAN_POINT ( 'NONE',  ( 18.49999999999999645, -1.164121893230052995, -208.9148480855715775 ) ) ;
#254151 = DIRECTION ( 'NONE',  ( -1.000000000000000000, 0.000000000000000000, 0.000000000000000000 ) ) ;
#254152 = LINE ( 'NONE', #182349, #148650 ) ;
#254153 = CARTESIAN_POINT ( 'NONE',  ( -21.64999999999999858, 68.65000000001157332, -57.27310748452437394 ) ) ;
#254154 = ORIENTED_EDGE ( 'NONE', *, *, #236138, .T. ) ;
#254155 = ORIENTED_EDGE ( 'NONE', *, *, #8015, .F. ) ;
#254156 = DIRECTION ( 'NONE',  ( -1.000000000000000000, -1.836970198721029934E-16, 0.000000000000000000 ) ) ;
#254158 = AXIS2_PLACEMENT_3D ( 'NONE', #68012, #169725, #171019 ) ;
#254157 = CARTESIAN_POINT ( 'NONE',  ( 21.05000000000000071, 64.35000000001228670, -157.8731074845244393 ) ) ;
#254159 = FACE_BOUND ( 'NONE', #137730, .T. ) ;
#254160 = AXIS2_PLACEMENT_3D ( 'NONE', #78786, #94511, #38403 ) ;
#254161 = ORIENTED_EDGE ( 'NONE', *, *, #112597, .F. ) ;
#254162 = DIRECTION ( 'NONE',  ( 0.000000000000000000, 0.000000000000000000, -1.000000000000000000 ) ) ;
#254163 = EDGE_CURVE ( 'NONE', #25295, #255163, #40089, .T. ) ;
#254164 = CARTESIAN_POINT ( 'NONE',  ( -20.64999999999999858, 0.000000000000000000, -33.50000000000000000 ) ) ;
#254165 = AXIS2_PLACEMENT_3D ( 'NONE', #59232, #198784, #138776 ) ;
#254166 = DIRECTION ( 'NONE',  ( 4.408576920032447355E-17, 0.1350103645451807555, 0.9908441862701610203 ) ) ;
#254167 = ORIENTED_EDGE ( 'NONE', *, *, #133915, .F. ) ;
#254168 = EDGE_LOOP ( 'NONE', ( #161633, #32025, #143181, #169969 ) ) ;
#254169 = PLANE ( 'NONE',  #234114 ) ;
#254170 = CARTESIAN_POINT ( 'NONE',  ( -21.65000000000000213, 65.95000000001225260, -149.1731074845244223 ) ) ;
#254171 = ORIENTED_EDGE ( 'NONE', *, *, #249733, .T. ) ;
#254172 = CARTESIAN_POINT ( 'NONE',  ( 23.24999999999999289, 11.65000000001116298, -67.10000000000005116 ) ) ;
#254173 = ORIENTED_EDGE ( 'NONE', *, *, #133045, .T. ) ;
#254174 = DIRECTION ( 'NONE',  ( 1.000000000000000000, 0.000000000000000000, 0.000000000000000000 ) ) ;
#254176 = EDGE_CURVE ( 'NONE', #129441, #169534, #23343, .T. ) ;
#254175 = CARTESIAN_POINT ( 'NONE',  ( -20.54999999999999716, 85.50000000001179501, -79.41707660717668205 ) ) ;
#254178 = CARTESIAN_POINT ( 'NONE',  ( -18.59999999999999787, 76.00000000001190870, -103.0231074845243029 ) ) ;
#254177 = LINE ( 'NONE', #118559, #257223 ) ;
#254179 = CARTESIAN_POINT ( 'NONE',  ( 18.50000972452444969, 65.70673848567014375, -164.5638252334829872 ) ) ;
#254180 = CARTESIAN_POINT ( 'NONE',  ( 21.05193202509564543, 65.27606398031468871, -90.85057288119861596 ) ) ;
#254181 = EDGE_CURVE ( 'NONE', #103692, #237439, #166968, .T. ) ;
#254182 = EDGE_CURVE ( 'NONE', #179110, #121258, #70435, .T. ) ;
#254183 = DIRECTION ( 'NONE',  ( 0.000000000000000000, -0.3896596508880098009, -0.9209589331071360574 ) ) ;
#254185 = ORIENTED_EDGE ( 'NONE', *, *, #120823, .T. ) ;
#254184 = EDGE_LOOP ( 'NONE', ( #166721, #131014, #209800, #216537 ) ) ;
#254186 = ORIENTED_EDGE ( 'NONE', *, *, #139548, .T. ) ;
#254187 = CARTESIAN_POINT ( 'NONE',  ( 20.27550659511089037, 66.78395627750266783, -48.67310748452439384 ) ) ;
#254188 = CARTESIAN_POINT ( 'NONE',  ( -16.81744102076749314, 66.05000000001187743, -90.37310748452438247 ) ) ;
#254189 =( BOUNDED_CURVE ( )  B_SPLINE_CURVE ( 3, ( #94629, #174220, #253700, #154645 ),
 .UNSPECIFIED., .F., .F. ) 
 B_SPLINE_CURVE_WITH_KNOTS ( ( 4, 4 ),
 ( 0.5235987755982449698, 1.570796326794896558 ),
 .UNSPECIFIED. ) 
 CURVE ( )  GEOMETRIC_REPRESENTATION_ITEM ( )  RATIONAL_B_SPLINE_CURVE ( ( 1.000000000000000000, 0.9106836025229499976, 0.9106836025229499976, 1.000000000000000000 ) ) 
 REPRESENTATION_ITEM ( '' )  );
#254190 = DIRECTION ( 'NONE',  ( 0.000000000000000000, 0.9126074666063769270, 0.4088369013363280513 ) ) ;
#254191 = DIRECTION ( 'NONE',  ( 0.000000000000000000, -6.789366196018718420E-15, 1.000000000000000000 ) ) ;
#254192 = ADVANCED_FACE ( 'NONE', ( #110799 ), #149955, .T. ) ;
#254194 = CARTESIAN_POINT ( 'NONE',  ( 18.49999999999999645, 74.16465844978765176, -124.9679561919613207 ) ) ;
#254193 = DIRECTION ( 'NONE',  ( -7.304098846218134667E-16, 1.000000000000000000, 6.982962677686266711E-15 ) ) ;
#254195 = CARTESIAN_POINT ( 'NONE',  ( -16.83794479845802172, 66.07364258066000673, -48.82666278030208673 ) ) ;
#254196 = ORIENTED_EDGE ( 'NONE', *, *, #53365, .T. ) ;
#254197 = ADVANCED_FACE ( 'NONE', ( #247747 ), #147365, .T. ) ;
#254198 = DIRECTION ( 'NONE',  ( 0.000000000000000000, -6.982962677686266711E-15, 1.000000000000000000 ) ) ;
#254199 = ORIENTED_EDGE ( 'NONE', *, *, #40051, .T. ) ;
#254200 = ORIENTED_EDGE ( 'NONE', *, *, #243746, .F. ) ;
#254201 = DIRECTION ( 'NONE',  ( 1.000000000000000000, 0.000000000000000000, 0.000000000000000000 ) ) ;
#254202 = CARTESIAN_POINT ( 'NONE',  ( -21.05000000000000071, 76.00000000001237765, -170.0231074845243597 ) ) ;
#254203 = DIRECTION ( 'NONE',  ( 0.000000000000000000, 0.9770955615653316162, 0.2128009952263604232 ) ) ;
#254204 = CIRCLE ( 'NONE', #116843, 0.09999999999999939493 ) ;
#254205 = DIRECTION ( 'NONE',  ( 1.000000000000000000, 0.000000000000000000, 0.000000000000000000 ) ) ;
#254206 = DIRECTION ( 'NONE',  ( -0.000000000000000000, -0.000000000000000000, 1.000000000000000000 ) ) ;
#254207 = VERTEX_POINT ( 'NONE', #50805 ) ;
#254208 = ORIENTED_EDGE ( 'NONE', *, *, #219597, .F. ) ;
#254209 = EDGE_CURVE ( 'NONE', #233373, #109083, #2632, .T. ) ;
#254210 = AXIS2_PLACEMENT_3D ( 'NONE', #216058, #240442, #37455 ) ;
#254211 = CARTESIAN_POINT ( 'NONE',  ( -20.54999999999999716, 7.150000000000000355, -21.15000000000000213 ) ) ;
#254212 = EDGE_CURVE ( 'NONE', #248271, #36408, #202372, .T. ) ;
#254213 = FACE_OUTER_BOUND ( 'NONE', #40722, .T. ) ;
#254214 = DIRECTION ( 'NONE',  ( 0.000000000000000000, 0.000000000000000000, -1.000000000000000000 ) ) ;
#254215 = EDGE_CURVE ( 'NONE', #6281, #100799, #227475, .T. ) ;
#254216 = CARTESIAN_POINT ( 'NONE',  ( 18.59999999999999787, 11.75000000000000000, 5.900000000000001243 ) ) ;
#254217 = DIRECTION ( 'NONE',  ( 0.5932847527679299127, -0.8049926720990051576, 6.366092712777055223E-16 ) ) ;
#254218 = CARTESIAN_POINT ( 'NONE',  ( 18.59999999999999787, 26.26588584238432489, -255.7307459359297468 ) ) ;
#254220 = CARTESIAN_POINT ( 'NONE',  ( 21.05000000000000071, 76.00000000001244871, -170.0231074845243597 ) ) ;
#254219 = DIRECTION ( 'NONE',  ( -1.000000000000000000, 0.000000000000000000, 0.000000000000000000 ) ) ;
#254221 = FACE_OUTER_BOUND ( 'NONE', #210154, .T. ) ;
#254222 = LINE ( 'NONE', #116033, #145918 ) ;
#254223 = CARTESIAN_POINT ( 'NONE',  ( 20.99999999999999645, 9.750000000011137757, -87.85000000000003695 ) ) ;
#254224 = FACE_OUTER_BOUND ( 'NONE', #164539, .T. ) ;
#254225 = VECTOR ( 'NONE', #20547, 1000.000000000000000 ) ;
#254226 = ORIENTED_EDGE ( 'NONE', *, *, #7197, .F. ) ;
#254227 = AXIS2_PLACEMENT_3D ( 'NONE', #72531, #152075, #186046 ) ;
#254228 = EDGE_CURVE ( 'NONE', #130445, #172317, #69133, .T. ) ;
#254229 = CARTESIAN_POINT ( 'NONE',  ( 20.94999999999999574, 10.47338541492405994, -41.07865446424855094 ) ) ;
#254230 = ORIENTED_EDGE ( 'NONE', *, *, #248643, .T. ) ;
#254231 = B_SPLINE_CURVE_WITH_KNOTS ( 'NONE', 3,
 ( #246203, #88381, #209641, #67559, #111833, #31041, #132680, #28480, #8875, #247480 ),
 .UNSPECIFIED., .F., .F.,
 ( 4, 3, 3, 4 ),
 ( 7.632826238683908479E-06, 4.756916949875909513E-05, 9.484459048150660151E-05, 0.0001435500935099896477 ),
 .UNSPECIFIED. ) ;
#254232 = AXIS2_PLACEMENT_3D ( 'NONE', #64084, #240166, #40712 ) ;
#254233 = AXIS2_PLACEMENT_3D ( 'NONE', #119662, #201745, #102617 ) ;
#254234 = DIRECTION ( 'NONE',  ( 0.000000000000000000, 0.000000000000000000, 1.000000000000000000 ) ) ;
#254235 = ORIENTED_EDGE ( 'NONE', *, *, #27157, .T. ) ;
#254236 = ADVANCED_FACE ( 'NONE', ( #129091 ), #13017, .F. ) ;
#254237 = CARTESIAN_POINT ( 'NONE',  ( 22.49999999999999645, 11.64976291804307884, -100.4111900236131021 ) ) ;
#254238 = CARTESIAN_POINT ( 'NONE',  ( 13.54577453029516043, 9.450602096099677496, -85.44389596309672186 ) ) ;
#254239 = CARTESIAN_POINT ( 'NONE',  ( 22.48508240969612615, 0.04627641452807086664, -21.84998926842643385 ) ) ;
#254240 = CYLINDRICAL_SURFACE ( 'NONE', #93185, 0.09999999999998898659 ) ;
#254241 = CARTESIAN_POINT ( 'NONE',  ( -23.25000000000000000, 64.65966496992309942, -200.4475097531309586 ) ) ;
#254242 = CARTESIAN_POINT ( 'NONE',  ( -21.10000000000000142, 4.898587196589412829E-16, 4.000000000000000000 ) ) ;
#254243 = VECTOR ( 'NONE', #177288, 1000.000000000000000 ) ;
#254244 = AXIS2_PLACEMENT_3D ( 'NONE', #198114, #75627, #116027 ) ;
#254245 = ORIENTED_EDGE ( 'NONE', *, *, #212210, .F. ) ;
#254246 = DIRECTION ( 'NONE',  ( 1.000000000000000000, -0.000000000000000000, -0.000000000000000000 ) ) ;
#254248 = ORIENTED_EDGE ( 'NONE', *, *, #66275, .F. ) ;
#254247 = CARTESIAN_POINT ( 'NONE',  ( -22.50000000000000000, 1.115600667400684642E-11, -27.25000000000000355 ) ) ;
#254249 = CYLINDRICAL_SURFACE ( 'NONE', #242284, 7.899999999999990585 ) ;
#254250 = EDGE_CURVE ( 'NONE', #175526, #154676, #170835, .T. ) ;
#254251 = CARTESIAN_POINT ( 'NONE',  ( -16.78805706634180339, 9.948252493082335945, -188.3441532080318268 ) ) ;
#254252 = DIRECTION ( 'NONE',  ( -1.000000000000000000, 2.952720810173289112E-16, 2.061873921506763405E-30 ) ) ;
#254253 = ORIENTED_EDGE ( 'NONE', *, *, #126909, .T. ) ;
#254254 = CARTESIAN_POINT ( 'NONE',  ( -21.05000000000000071, 11.64999999999999680, -6.783865662978151967 ) ) ;
#254255 = EDGE_CURVE ( 'NONE', #175346, #126775, #223203, .T. ) ;
#254256 = APPLICATION_PROTOCOL_DEFINITION ( 'draft international standard', 'automotive_design', 1998, #208885 ) ;
#254257 = CIRCLE ( 'NONE', #87665, 0.09999999999999939493 ) ;
#254258 = CARTESIAN_POINT ( 'NONE',  ( -23.15000000000000213, 74.07476635515278929, -190.7928639513982318 ) ) ;
#254259 = CARTESIAN_POINT ( 'NONE',  ( -18.52186455168995494, 85.48101848145434190, -95.99809100660965555 ) ) ;
#254260 = ORIENTED_EDGE ( 'NONE', *, *, #145991, .T. ) ;
#254262 = ADVANCED_FACE ( 'NONE', ( #131650 ), #33886, .F. ) ;
#254261 = DIRECTION ( 'NONE',  ( 1.000000000000000000, 0.000000000000000000, 0.000000000000000000 ) ) ;
#254263 = CARTESIAN_POINT ( 'NONE',  ( -23.15000000000000213, 11.65000000001115588, -146.1500000000000341 ) ) ;
#254264 = EDGE_CURVE ( 'NONE', #148565, #78772, #48422, .T. ) ;
#254265 = EDGE_CURVE ( 'NONE', #209902, #4726, #131634, .T. ) ;
#254266 = CARTESIAN_POINT ( 'NONE',  ( -16.80117486205003630, 9.949657268323468529, -121.3488548729255143 ) ) ;
#254267 = ORIENTED_EDGE ( 'NONE', *, *, #28142, .T. ) ;
#254268 = ORIENTED_EDGE ( 'NONE', *, *, #199870, .F. ) ;
#254269 = CARTESIAN_POINT ( 'NONE',  ( 20.94999999999999574, 1.851028230140860487, -11.65391326942249250 ) ) ;
#254270 = TOROIDAL_SURFACE ( 'NONE', #141850, 0.2000000000000000111, 0.1000000000000000056 ) ;
#254271 = CARTESIAN_POINT ( 'NONE',  ( 21.30000000000002558, 1.115600667400684642E-11, -67.00000000000004263 ) ) ;
#254272 = DIRECTION ( 'NONE',  ( -0.000000000000000000, 1.000000000000000000, 6.982962677686266711E-15 ) ) ;
#254273 = CARTESIAN_POINT ( 'NONE',  ( -17.11825945287481687, 30.20632856012695200, -234.8070450048001021 ) ) ;
#254274 = VECTOR ( 'NONE', #11354, 1000.000000000000000 ) ;
#254276 = DIRECTION ( 'NONE',  ( 0.000000000000000000, 0.000000000000000000, -1.000000000000000000 ) ) ;
#254275 = LINE ( 'NONE', #78217, #186898 ) ;
#254277 = CARTESIAN_POINT ( 'NONE',  ( 20.89192007715127986, 65.67101464000451472, -30.44043916224795510 ) ) ;
#254278 = LINE ( 'NONE', #37846, #18600 ) ;
#254279 = CARTESIAN_POINT ( 'NONE',  ( 18.59999999999999076, 77.25000000001263345, -195.5231074845243313 ) ) ;
#254280 = CARTESIAN_POINT ( 'NONE',  ( -18.59999999999999787, 14.76289716703255728, -235.7888246855571026 ) ) ;
#254281 = ORIENTED_EDGE ( 'NONE', *, *, #179288, .T. ) ;
#254282 = AXIS2_PLACEMENT_3D ( 'NONE', #37026, #156974, #59089 ) ;
#254283 = ADVANCED_FACE ( 'NONE', ( #232056 ), #7874, .F. ) ;
#254284 = ORIENTED_EDGE ( 'NONE', *, *, #136116, .T. ) ;
#254285 = DIRECTION ( 'NONE',  ( 0.000000000000000000, -0.1350103645451807555, -0.9908441862701610203 ) ) ;
#254286 = EDGE_CURVE ( 'NONE', #24117, #217574, #235677, .T. ) ;
#254287 = CARTESIAN_POINT ( 'NONE',  ( -17.27223548800608199, 65.65460260867664033, -147.8895013053080731 ) ) ;
#254289 = CARTESIAN_POINT ( 'NONE',  ( -23.15000000000000213, 11.65000000001115588, -193.9851942293460070 ) ) ;
#254288 = DIRECTION ( 'NONE',  ( 1.000000000000000000, 0.000000000000000000, 0.000000000000000000 ) ) ;
#254290 =( BOUNDED_SURFACE ( )  B_SPLINE_SURFACE ( 3, 2, ( 
 ( #109467, #148631, #226860 ),
 ( #169506, #28715, #127776 ),
 ( #165626, #105604, #187758 ),
 ( #6526, #206024, #9106 ),
 ( #49518, #247712, #46921 ),
 ( #69093, #186464, #228159 ),
 ( #27423, #48224, #129057 ),
 ( #144741, #110762, #208606 ),
 ( #29978, #26111, #224291 ),
 ( #106908, #189026, #190325 ) ),
 .UNSPECIFIED., .F., .F., .F. ) 
 B_SPLINE_SURFACE_WITH_KNOTS ( ( 4, 2, 2, 2, 4 ),
 ( 3, 3 ),
 ( 0.0001836757140119193922, 0.0004000170051583608419, 0.0005081876507315815803, 0.0005622729735181920038, 0.0006163582963048023187 ),
 ( 0.000000000000000000, 1.000000000000000000 ),
 .UNSPECIFIED. ) 
 GEOMETRIC_REPRESENTATION_ITEM ( )  RATIONAL_B_SPLINE_SURFACE ( (
 ( 1.000000000000000000, 0.7071067811865135999, 1.000000000000000000),
 ( 1.000000000000000000, 0.6461995200032549791, 1.000000000000000000),
 ( 1.000000000000000000, 0.5776453529546025090, 1.000000000000000000),
 ( 1.000000000000000000, 0.4585233068353464780, 1.000000000000000000),
 ( 1.000000000000000000, 0.4154092989903095390, 1.000000000000000000),
 ( 1.000000000000000000, 0.3550093145854532617, 1.000000000000000000),
 ( 1.000000000000000000, 0.3354498651685169364, 1.000000000000000000),
 ( 1.000000000000000000, 0.3060347992257099192, 1.000000000000000000),
 ( 1.000000000000000000, 0.2963555829624704985, 1.000000000000000000),
 ( 1.000000000000000000, 0.2966190024560417804, 1.000000000000000000) ) ) 
 REPRESENTATION_ITEM ( '' )  SURFACE ( )  );
#254291 = AXIS2_PLACEMENT_3D ( 'NONE', #233390, #54719, #174725 ) ;
#254292 = CARTESIAN_POINT ( 'NONE',  ( -20.94999999999994600, 61.72892516158560028, -36.56695479651062897 ) ) ;
#254294 = ADVANCED_FACE ( 'NONE', ( #113375 ), #254148, .F. ) ;
#254293 = FACE_OUTER_BOUND ( 'NONE', #236281, .T. ) ;
#254295 = CARTESIAN_POINT ( 'NONE',  ( -12.25000000000000178, 66.15000000001228386, -153.2731074845244166 ) ) ;
#254296 = ORIENTED_EDGE ( 'NONE', *, *, #73038, .F. ) ;
#254297 = ORIENTED_EDGE ( 'NONE', *, *, #133454, .F. ) ;
#254298 = VECTOR ( 'NONE', #103097, 1000.000000000000000 ) ;
#254299 = DIRECTION ( 'NONE',  ( 0.000000000000000000, 0.5000000000000209832, 0.8660254037844264952 ) ) ;
#254300 = VERTEX_POINT ( 'NONE', #213753 ) ;
#254301 = DIRECTION ( 'NONE',  ( 0.000000000000000000, 0.4166553800442402977, -0.9090645160164321226 ) ) ;
#254302 = ADVANCED_FACE ( 'NONE', ( #173400 ), #240693, .F. ) ;
#254303 = CIRCLE ( 'NONE', #66879, 3.999999999999999112 ) ;
#254304 = CIRCLE ( 'NONE', #196068, 0.2000000000000057288 ) ;
#254305 = CARTESIAN_POINT ( 'NONE',  ( -21.08621493067320785, 65.51509213395192432, -241.9683428252619706 ) ) ;
#254306 = VECTOR ( 'NONE', #72654, 1000.000000000000114 ) ;
#254307 = EDGE_CURVE ( 'NONE', #248782, #126073, #110784, .T. ) ;
#254308 = VERTEX_POINT ( 'NONE', #14300 ) ;
#254309 = ORIENTED_EDGE ( 'NONE', *, *, #186001, .F. ) ;
#254310 = CARTESIAN_POINT ( 'NONE',  ( -20.64999999999999858, 7.250000000011155521, -79.25000000000004263 ) ) ;
#254311 = EDGE_CURVE ( 'NONE', #135971, #21878, #64995, .T. ) ;
#254312 = DIRECTION ( 'NONE',  ( 0.000000000000000000, -1.000000000000000000, 0.000000000000000000 ) ) ;
#254313 = FACE_OUTER_BOUND ( 'NONE', #20795, .T. ) ;
#254314 = CARTESIAN_POINT ( 'NONE',  ( 23.40000000000005187, 74.94272479589878344, -3.023107484524792277 ) ) ;
#254316 = FACE_OUTER_BOUND ( 'NONE', #185046, .T. ) ;
#254315 = DIRECTION ( 'NONE',  ( 0.000000000000000000, 0.4999999999999943379, 0.8660254037844420383 ) ) ;
#254317 = CIRCLE ( 'NONE', #100181, 4.050000000000006040 ) ;
#254318 = CARTESIAN_POINT ( 'NONE',  ( -23.15000000000000213, -11.64999999998884483, -130.9000000000000341 ) ) ;
#254319 = ORIENTED_EDGE ( 'NONE', *, *, #237553, .F. ) ;
#254321 = CARTESIAN_POINT ( 'NONE',  ( -16.80469485234340254, 66.05784833687096125, -115.7131406405931671 ) ) ;
#254320 = DIRECTION ( 'NONE',  ( 1.000000000000000000, 0.000000000000000000, 0.000000000000000000 ) ) ;
#254322 = EDGE_LOOP ( 'NONE', ( #18804, #75535, #234588, #66525 ) ) ;
#254324 = VERTEX_POINT ( 'NONE', #159894 ) ;
#254323 = CARTESIAN_POINT ( 'NONE',  ( 20.94999999999999929, 28.08470566095357057, -239.2860081655328770 ) ) ;
#254325 = VERTEX_POINT ( 'NONE', #135482 ) ;
#254326 = CARTESIAN_POINT ( 'NONE',  ( -21.00857864376268935, 18.71344899777637849, -226.7788045585494103 ) ) ;
#254327 = PLANE ( 'NONE',  #254981 ) ;
#254328 = DIRECTION ( 'NONE',  ( -0.000000000000000000, 1.000000000000000000, 0.000000000000000000 ) ) ;
#254329 = CARTESIAN_POINT ( 'NONE',  ( -17.78241384936779212, 21.28923697791310587, -229.0030853712114549 ) ) ;
#254330 = ORIENTED_EDGE ( 'NONE', *, *, #114067, .F. ) ;
#254331 = EDGE_CURVE ( 'NONE', #242236, #181057, #6734, .T. ) ;
#254332 = CARTESIAN_POINT ( 'NONE',  ( -21.05000000000000071, 76.00000000001237765, -170.0231074845243597 ) ) ;
#254333 = CARTESIAN_POINT ( 'NONE',  ( -18.34804628011471195, 40.40989152675304297, -235.2989281452920807 ) ) ;
#254334 = CARTESIAN_POINT ( 'NONE',  ( 22.49533356619864577, 64.34999999370857893, -203.5882300648472381 ) ) ;
#254335 = ORIENTED_EDGE ( 'NONE', *, *, #49621, .T. ) ;
#254336 = CARTESIAN_POINT ( 'NONE',  ( 23.24999999999999645, 36.65892442174472876, -249.5511627012454596 ) ) ;
#254337 = CIRCLE ( 'NONE', #241875, 0.09999999999998898659 ) ;
#254339 = AXIS2_PLACEMENT_3D ( 'NONE', #53808, #17262, #252003 ) ;
#254338 = DIRECTION ( 'NONE',  ( 2.952720810173289112E-16, -1.000000000000000000, -0.000000000000000000 ) ) ;
#254340 = ORIENTED_EDGE ( 'NONE', *, *, #215716, .T. ) ;
#254341 = ORIENTED_EDGE ( 'NONE', *, *, #90626, .F. ) ;
#254342 = LINE ( 'NONE', #18321, #43571 ) ;
#254343 = ORIENTED_EDGE ( 'NONE', *, *, #86341, .F. ) ;
#254344 = AXIS2_PLACEMENT_3D ( 'NONE', #115106, #237628, #257130 ) ;
#254345 = CYLINDRICAL_SURFACE ( 'NONE', #46780, 0.09999999999999939493 ) ;
#254346 = EDGE_LOOP ( 'NONE', ( #228890, #163103, #71428 ) ) ;
#254347 = DIRECTION ( 'NONE',  ( -0.000000000000000000, 0.2128009952263603677, -0.9770955615653313941 ) ) ;
#254348 = EDGE_CURVE ( 'NONE', #21732, #84289, #85810, .T. ) ;
#254349 = DIRECTION ( 'NONE',  ( -1.000000000000000000, 0.000000000000000000, 0.000000000000000000 ) ) ;
#254350 = DIRECTION ( 'NONE',  ( 1.000000000000000000, 0.000000000000000000, 0.000000000000000000 ) ) ;
#254351 = CIRCLE ( 'NONE', #229435, 0.1000000000000028644 ) ;
#254352 = LINE ( 'NONE', #245719, #50382 ) ;
#254353 = CARTESIAN_POINT ( 'NONE',  ( 23.24999999999999289, 64.25000000001237765, -169.9231074845244507 ) ) ;
#254355 = EDGE_CURVE ( 'NONE', #221154, #252282, #74281, .T. ) ;
#254354 = DIRECTION ( 'NONE',  ( 1.000000000000000000, 0.000000000000000000, 0.000000000000000000 ) ) ;
#254356 = EDGE_LOOP ( 'NONE', ( #104359, #2859, #91687, #162115 ) ) ;
#254358 = FACE_OUTER_BOUND ( 'NONE', #228893, .T. ) ;
#254357 = CARTESIAN_POINT ( 'NONE',  ( -22.50000000000000000, 76.00000000001165290, -69.52310748452431710 ) ) ;
#254359 = ORIENTED_EDGE ( 'NONE', *, *, #249799, .F. ) ;
#254362 = ORIENTED_EDGE ( 'NONE', *, *, #190344, .T. ) ;
#254361 = CARTESIAN_POINT ( 'NONE',  ( -18.59999999999999787, -1.149570369564537842, -141.8159124845019790 ) ) ;
#254360 = LINE ( 'NONE', #196966, #82259 ) ;
#254363 = ORIENTED_EDGE ( 'NONE', *, *, #188004, .T. ) ;
#254364 = DIRECTION ( 'NONE',  ( 0.000000000000000000, 7.116814260417668513E-15, -1.000000000000000000 ) ) ;
#254365 = DIRECTION ( 'NONE',  ( 1.000000000000000000, 3.265361837132813093E-16, -0.000000000000000000 ) ) ;
#254366 = DIRECTION ( 'NONE',  ( 0.000000000000000000, -6.982962677686266711E-15, 1.000000000000000000 ) ) ;
#254367 = CARTESIAN_POINT ( 'NONE',  ( -16.87683809663752754, 9.864913778549569301, -113.7757156356385480 ) ) ;
#254368 = ORIENTED_EDGE ( 'NONE', *, *, #59038, .F. ) ;
#254370 = EDGE_LOOP ( 'NONE', ( #257360, #166645, #167782 ) ) ;
#254369 = CARTESIAN_POINT ( 'NONE',  ( -22.39999999999999858, 64.35000000001238618, -170.1231074845244393 ) ) ;
#254371 = CIRCLE ( 'NONE', #175311, 0.09999999999999939493 ) ;
#254373 = CARTESIAN_POINT ( 'NONE',  ( 20.95496329884391784, 10.56743320609303716, -7.574309932284823965 ) ) ;
#254372 = DIRECTION ( 'NONE',  ( -1.000000000000000000, -0.000000000000000000, -0.000000000000000000 ) ) ;
#254375 = EDGE_LOOP ( 'NONE', ( #235190, #189324, #14233 ) ) ;
#254374 = LINE ( 'NONE', #94034, #10121 ) ;
#254376 = AXIS2_PLACEMENT_3D ( 'NONE', #71162, #192374, #174137 ) ;
#254377 = ORIENTED_EDGE ( 'NONE', *, *, #174875, .F. ) ;
#254378 = AXIS2_PLACEMENT_3D ( 'NONE', #85013, #185434, #199879 ) ;
#254379 = CARTESIAN_POINT ( 'NONE',  ( 22.57320508075688537, 11.75000000001115552, -167.4999999999999432 ) ) ;
#254380 = CARTESIAN_POINT ( 'NONE',  ( -16.86445178670659217, 44.09327534691641404, -235.3044585041410244 ) ) ;
#254381 = EDGE_LOOP ( 'NONE', ( #251576, #241270, #79548, #5001, #211813, #135967, #142473, #161540 ) ) ;
#254382 = CARTESIAN_POINT ( 'NONE',  ( 18.59999999999999432, 13.71992543034163781, -238.5823796952984992 ) ) ;
#254383 = ORIENTED_EDGE ( 'NONE', *, *, #164182, .F. ) ;
#254384 = DIRECTION ( 'NONE',  ( 0.7071359030027593029, -0.7070776581709197206, 0.000000000000000000 ) ) ;
#254385 = CARTESIAN_POINT ( 'NONE',  ( 20.94999999999999929, -9.500000000000000000, -23.60603087734755690 ) ) ;
#254386 = EDGE_LOOP ( 'NONE', ( #196432, #229753, #230322, #105595 ) ) ;
#254387 = CARTESIAN_POINT ( 'NONE',  ( -23.25000000000000000, -1.736705739467587772, -45.01742258762372728 ) ) ;
#254388 = EDGE_CURVE ( 'NONE', #140279, #154872, #135724, .T. ) ;
#254389 = CIRCLE ( 'NONE', #8717, 0.09999999999998802902 ) ;
#254390 = CARTESIAN_POINT ( 'NONE',  ( -16.85939681242906119, 9.905225185936458843, -54.03992195519148822 ) ) ;
#254391 = CIRCLE ( 'NONE', #141991, 0.1000000000000028644 ) ;
#254393 = ORIENTED_EDGE ( 'NONE', *, *, #233668, .F. ) ;
#254392 = AXIS2_PLACEMENT_3D ( 'NONE', #95601, #113886, #52620 ) ;
#254394 = ORIENTED_EDGE ( 'NONE', *, *, #8809, .T. ) ;
#254395 = DIRECTION ( 'NONE',  ( 0.000000000000000000, 0.000000000000000000, -1.000000000000000000 ) ) ;
#254396 = AXIS2_PLACEMENT_3D ( 'NONE', #150061, #152641, #16965 ) ;
#254397 = VERTEX_POINT ( 'NONE', #252874 ) ;
#254398 = EDGE_CURVE ( 'NONE', #201799, #224021, #155101, .T. ) ;
#254399 = EDGE_LOOP ( 'NONE', ( #184013, #98670, #121128, #121145 ) ) ;
#254401 = ORIENTED_EDGE ( 'NONE', *, *, #145031, .T. ) ;
#254400 = DIRECTION ( 'NONE',  ( 0.000000000000000000, 0.2128009952263604232, -0.9770955615653316162 ) ) ;
#254402 = AXIS2_PLACEMENT_3D ( 'NONE', #160649, #61525, #10544 ) ;
#254403 = AXIS2_PLACEMENT_3D ( 'NONE', #159459, #78616, #238999 ) ;
#254404 = EDGE_CURVE ( 'NONE', #155368, #248700, #44170, .T. ) ;
#254405 = VERTEX_POINT ( 'NONE', #234598 ) ;
#254406 = DIRECTION ( 'NONE',  ( 0.000000000000000000, -0.008583690987162452199, 0.9999631594459053030 ) ) ;
#254407 = EDGE_LOOP ( 'NONE', ( #216355, #181534, #5963, #187112 ) ) ;
#254410 = ORIENTED_EDGE ( 'NONE', *, *, #192046, .F. ) ;
#254409 = ORIENTED_EDGE ( 'NONE', *, *, #195401, .T. ) ;
#254408 = DIRECTION ( 'NONE',  ( 1.000000000000000000, 0.000000000000000000, 0.000000000000000000 ) ) ;
#254412 = ADVANCED_FACE ( 'NONE', ( #115949 ), #61078, .T. ) ;
#254411 = ORIENTED_EDGE ( 'NONE', *, *, #109609, .T. ) ;
#254413 = CARTESIAN_POINT ( 'NONE',  ( -23.15000000000000213, 76.00000000001126921, -203.5231074845248997 ) ) ;
#254414 = AXIS2_PLACEMENT_3D ( 'NONE', #140085, #179260, #200086 ) ;
#254415 = AXIS2_PLACEMENT_3D ( 'NONE', #121338, #20942, #125160 ) ;
#254416 = AXIS2_PLACEMENT_3D ( 'NONE', #105752, #124077, #197482 ) ;
#254417 = AXIS2_PLACEMENT_3D ( 'NONE', #208079, #149397, #13703 ) ;
#254418 = AXIS2_PLACEMENT_3D ( 'NONE', #7694, #209737, #31135 ) ;
#254419 = DIRECTION ( 'NONE',  ( 0.000000000000000000, -0.000000000000000000, 1.000000000000000000 ) ) ;
#254420 = EDGE_LOOP ( 'NONE', ( #69062, #174427, #142507, #193500 ) ) ;
#254421 = CARTESIAN_POINT ( 'NONE',  ( -16.93433913041102912, 10.00597842153509376, -154.9353654273951975 ) ) ;
#254423 = VERTEX_POINT ( 'NONE', #140286 ) ;
#254422 = DIRECTION ( 'NONE',  ( 0.000000000000000000, 0.2128009952263601179, -0.9770955615653315052 ) ) ;
#254424 = DIRECTION ( 'NONE',  ( -1.000000000000000000, 0.000000000000000000, 0.000000000000000000 ) ) ;
#254425 = VERTEX_POINT ( 'NONE', #81580 ) ;
#254426 = EDGE_CURVE ( 'NONE', #94746, #157975, #109967, .T. ) ;
#254427 = ORIENTED_EDGE ( 'NONE', *, *, #185727, .T. ) ;
#254428 = CARTESIAN_POINT ( 'NONE',  ( 21.93340585900761397, 1.115541036281197940E-11, -160.1758529778929301 ) ) ;
#254429 = AXIS2_PLACEMENT_3D ( 'NONE', #102747, #183602, #127475 ) ;
#254430 = FACE_OUTER_BOUND ( 'NONE', #13457, .T. ) ;
#254431 = EDGE_CURVE ( 'NONE', #49221, #10139, #24486, .T. ) ;
#254432 = ORIENTED_EDGE ( 'NONE', *, *, #48590, .T. ) ;
#254433 = VERTEX_POINT ( 'NONE', #184557 ) ;
#254434 = CARTESIAN_POINT ( 'NONE',  ( -16.94062896051973865, 9.992719105111833144, -180.1025165421187637 ) ) ;
#254435 = CARTESIAN_POINT ( 'NONE',  ( -18.59999999999999787, -1.164121893230052995, -208.9148480855715775 ) ) ;
#254437 = ORIENTED_EDGE ( 'NONE', *, *, #38474, .T. ) ;
#254436 = ORIENTED_EDGE ( 'NONE', *, *, #48446, .T. ) ;
#254438 = ORIENTED_EDGE ( 'NONE', *, *, #156724, .F. ) ;
#254439 = DIRECTION ( 'NONE',  ( 1.000000000000000000, 0.000000000000000000, 0.000000000000000000 ) ) ;
#254440 = VERTEX_POINT ( 'NONE', #144135 ) ;
#254441 = ORIENTED_EDGE ( 'NONE', *, *, #173443, .T. ) ;
#254442 = LINE ( 'NONE', #75836, #25816 ) ;
#254443 = ORIENTED_EDGE ( 'NONE', *, *, #80765, .T. ) ;
#254444 = LINE ( 'NONE', #57538, #81523 ) ;
#254445 = DIRECTION ( 'NONE',  ( 0.000000000000000000, 0.8660254037844411501, 0.4999999999999956701 ) ) ;
#254446 = AXIS2_PLACEMENT_3D ( 'NONE', #137988, #119751, #96294 ) ;
#254447 = ADVANCED_FACE ( 'NONE', ( #5911 ), #202842, .T. ) ;
#254448 = ORIENTED_EDGE ( 'NONE', *, *, #179362, .F. ) ;
#254449 = ORIENTED_EDGE ( 'NONE', *, *, #227428, .T. ) ;
#254450 = DIRECTION ( 'NONE',  ( 0.000000000000000000, 0.000000000000000000, -1.000000000000000000 ) ) ;
#254451 = ORIENTED_EDGE ( 'NONE', *, *, #138946, .T. ) ;
#254452 = ADVANCED_FACE ( 'NONE', ( #165005 ), #136606, .T. ) ;
#254453 = VECTOR ( 'NONE', #217311, 1000.000000000000000 ) ;
#254454 = ORIENTED_EDGE ( 'NONE', *, *, #174924, .T. ) ;
#254455 = VERTEX_POINT ( 'NONE', #148014 ) ;
#254456 = DIRECTION ( 'NONE',  ( 0.000000000000000000, 0.2617529984165031243, 0.9651348961777157509 ) ) ;
#254458 = ORIENTED_EDGE ( 'NONE', *, *, #21380, .F. ) ;
#254457 = CARTESIAN_POINT ( 'NONE',  ( -21.65000000000000213, 68.29142135624960019, -157.6731074845243938 ) ) ;
#254459 = CARTESIAN_POINT ( 'NONE',  ( 23.14999999999999858, 76.00000000001244871, -170.0231074845243597 ) ) ;
#254460 = DIRECTION ( 'NONE',  ( 0.000000000000000000, 0.000000000000000000, -1.000000000000000000 ) ) ;
#254461 = ORIENTED_EDGE ( 'NONE', *, *, #187128, .F. ) ;
#254462 = DIRECTION ( 'NONE',  ( 0.000000000000000000, -0.8660254037844377084, -0.5000000000000016653 ) ) ;
#254464 = EDGE_CURVE ( 'NONE', #5761, #20715, #65180, .T. ) ;
#254463 = CARTESIAN_POINT ( 'NONE',  ( -23.25000000000000000, 77.83585931145498193, -24.51866831572578675 ) ) ;
#254465 = DIRECTION ( 'NONE',  ( 0.000000000000000000, 0.2617529984165083423, 0.9651348961777143076 ) ) ;
#254466 = DIRECTION ( 'NONE',  ( 0.000000000000000000, 0.7397890806274222131, 0.6728388485993012091 ) ) ;
#254467 = DIRECTION ( 'NONE',  ( -0.000000000000000000, 6.982962677686266711E-15, -1.000000000000000000 ) ) ;
#254468 = CARTESIAN_POINT ( 'NONE',  ( -16.86133551771150607, 63.07299635117417580, -213.1745817361760089 ) ) ;
#254469 = CARTESIAN_POINT ( 'NONE',  ( -18.79999999999999716, 1.350000000000000089, 16.39999999999999858 ) ) ;
#254470 = CARTESIAN_POINT ( 'NONE',  ( 23.15000000000000213, 87.65000000001202807, -114.7731074845242318 ) ) ;
#254471 = DIRECTION ( 'NONE',  ( 1.000000000000000000, -0.000000000000000000, -0.000000000000000000 ) ) ;
#254472 = EDGE_CURVE ( 'NONE', #8977, #38476, #227542, .T. ) ;
#254473 = CIRCLE ( 'NONE', #21304, 12.87499999999999822 ) ;
#254474 = ORIENTED_EDGE ( 'NONE', *, *, #217372, .T. ) ;
#254475 = EDGE_CURVE ( 'NONE', #93776, #39887, #146697, .T. ) ;
#254476 = CONICAL_SURFACE ( 'NONE', #409, 4.049999999999998934, 0.7853981633974604915 ) ;
#254477 = AXIS2_PLACEMENT_3D ( 'NONE', #210245, #52421, #35479 ) ;
#254479 = ORIENTED_EDGE ( 'NONE', *, *, #191305, .F. ) ;
#254478 = EDGE_LOOP ( 'NONE', ( #106892, #178194, #25396, #181820 ) ) ;
#254480 = ORIENTED_EDGE ( 'NONE', *, *, #93083, .F. ) ;
#254481 = DIRECTION ( 'NONE',  ( -0.000000000000000000, 1.000000000000000000, -0.000000000000000000 ) ) ;
#254482 = EDGE_CURVE ( 'NONE', #172515, #236242, #187160, .T. ) ;
#254483 = SPHERICAL_SURFACE ( 'NONE', #186839, 0.1000000000000000056 ) ;
#254485 = CARTESIAN_POINT ( 'NONE',  ( -18.59999999999999787, 14.81796439977981272, -236.5325475414793743 ) ) ;
#254484 = CARTESIAN_POINT ( 'NONE',  ( -20.64999999999999858, 2.500000000011154633, -120.7753780772379315 ) ) ;
#254486 = VERTEX_POINT ( 'NONE', #245832 ) ;
#254487 = ORIENTED_EDGE ( 'NONE', *, *, #96761, .F. ) ;
#254488 = EDGE_CURVE ( 'NONE', #180506, #62035, #248396, .T. ) ;
#254489 = PLANE ( 'NONE',  #100674 ) ;
#254490 = EDGE_CURVE ( 'NONE', #151096, #103650, #231795, .T. ) ;
#254491 = DIRECTION ( 'NONE',  ( 0.000000000000000000, -0.2605042016806740079, 0.9654727137038698892 ) ) ;
#254493 = CIRCLE ( 'NONE', #75487, 11.65000000000000036 ) ;
#254492 = LINE ( 'NONE', #96696, #84676 ) ;
#254494 = DIRECTION ( 'NONE',  ( 0.7071067811865474617, -0.7071067811865474617, -5.142139384388980375E-15 ) ) ;
#254495 = ORIENTED_EDGE ( 'NONE', *, *, #230621, .T. ) ;
#254496 = ORIENTED_EDGE ( 'NONE', *, *, #129365, .F. ) ;
#254497 = CARTESIAN_POINT ( 'NONE',  ( -21.05000000000000071, 87.48912529308779540, -72.62310748452422615 ) ) ;
#254498 = DIRECTION ( 'NONE',  ( 0.000000000000000000, 0.1568667991644863147, -0.9876197685951252359 ) ) ;
#254499 = EDGE_CURVE ( 'NONE', #210104, #200509, #56761, .T. ) ;
#254500 = ORIENTED_EDGE ( 'NONE', *, *, #82646, .T. ) ;
#254501 = DIRECTION ( 'NONE',  ( 1.734723475976817192E-14, 0.8814952561688430555, -0.4721928772777346239 ) ) ;
#254502 = CARTESIAN_POINT ( 'NONE',  ( 18.31572054635686797, 77.38692514556900903, -241.7683706053347805 ) ) ;
#254503 = CARTESIAN_POINT ( 'NONE',  ( 16.87683809663750267, 44.13548170601895038, -235.2989316066074821 ) ) ;
#254504 = ADVANCED_FACE ( 'NONE', ( #47604 ), #127168, .F. ) ;
#254505 = DIRECTION ( 'NONE',  ( 0.000000000000000000, -6.982962677686267499E-15, 1.000000000000000000 ) ) ;
#254506 = EDGE_CURVE ( 'NONE', #20503, #142551, #169280, .T. ) ;
#254507 = CARTESIAN_POINT ( 'NONE',  ( -16.87683809663752399, 9.850000000011144508, -187.5976359818036769 ) ) ;
#254508 = ORIENTED_EDGE ( 'NONE', *, *, #247110, .F. ) ;
#254509 = DIRECTION ( 'NONE',  ( 1.476360405086644309E-16, -1.000000000000000000, -1.445602896647339410E-16 ) ) ;
#254510 = CARTESIAN_POINT ( 'NONE',  ( 21.13461538461538325, 44.29694026544699170, -236.3931290369747842 ) ) ;
#254511 = DIRECTION ( 'NONE',  ( 1.000000000000000000, 0.000000000000000000, 0.000000000000000000 ) ) ;
#254514 = DIRECTION ( 'NONE',  ( 0.7071067811865475727, 0.7071067811865475727, 0.000000000000000000 ) ) ;
#254513 = AXIS2_PLACEMENT_3D ( 'NONE', #85831, #225359, #46726 ) ;
#254512 = CARTESIAN_POINT ( 'NONE',  ( -16.81930730667005847, 66.06300193113798969, -123.7963397539861745 ) ) ;
#254516 = CARTESIAN_POINT ( 'NONE',  ( -21.14999999999999858, 12.71802988599559292, -223.5105008658000258 ) ) ;
#254515 = AXIS2_PLACEMENT_3D ( 'NONE', #2231, #220014, #143020 ) ;
#254517 = AXIS2_PLACEMENT_3D ( 'NONE', #63434, #142955, #84233 ) ;
#254518 = CARTESIAN_POINT ( 'NONE',  ( 21.05000000000000071, 85.00000000001149658, -45.91707660717670336 ) ) ;
#254519 = CARTESIAN_POINT ( 'NONE',  ( -20.85000000000000142, -1.835859311432481045, -179.0044391687985410 ) ) ;
#254520 = CARTESIAN_POINT ( 'NONE',  ( 22.41477678272288188, 75.99917613424908325, -114.6726927690397133 ) ) ;
#254521 = ORIENTED_EDGE ( 'NONE', *, *, #228883, .F. ) ;
#254522 = VERTEX_POINT ( 'NONE', #149321 ) ;
#254523 = CARTESIAN_POINT ( 'NONE',  ( 24.30000000000000071, 3.175288713399624818, -347.0000000000001137 ) ) ;
#254524 = EDGE_CURVE ( 'NONE', #125487, #59470, #202546, .T. ) ;
#254525 = EDGE_LOOP ( 'NONE', ( #27438, #94550, #136967, #96289 ) ) ;
#254526 = ADVANCED_FACE ( 'NONE', ( #170198 ), #94450, .T. ) ;
#254527 = DIRECTION ( 'NONE',  ( 0.000000000000000000, 0.000000000000000000, -1.000000000000000000 ) ) ;
#254528 = CIRCLE ( 'NONE', #50524, 0.09999999999999939493 ) ;
#254529 = ORIENTED_EDGE ( 'NONE', *, *, #142615, .T. ) ;
#254530 = SURFACE_SIDE_STYLE ('',( #75930 ) ) ;
#254531 = ADVANCED_FACE ( 'NONE', ( #250942 ), #191017, .T. ) ;
#254532 = DIRECTION ( 'NONE',  ( -1.000000000000000000, 0.000000000000000000, 0.000000000000000000 ) ) ;
#254533 = ORIENTED_EDGE ( 'NONE', *, *, #227136, .T. ) ;
#254534 = DIRECTION ( 'NONE',  ( -1.000000000000000000, 0.000000000000000000, 0.000000000000000000 ) ) ;
#254535 = CARTESIAN_POINT ( 'NONE',  ( -12.92414019175885898, 9.417632963117450018, -51.64894846573227483 ) ) ;
#254536 = LINE ( 'NONE', #113766, #98535 ) ;
#254537 = CARTESIAN_POINT ( 'NONE',  ( -18.50000000000000000, 66.65000000001205649, -124.1731074845243654 ) ) ;
#254539 = ORIENTED_EDGE ( 'NONE', *, *, #72040, .F. ) ;
#254538 = CARTESIAN_POINT ( 'NONE',  ( -16.87401514999240248, 30.14463975252685302, -234.7739999993361266 ) ) ;
#254541 = DIRECTION ( 'NONE',  ( 0.000000000000000000, 0.8814952561688428334, -0.4721928772777349570 ) ) ;
#254540 = CARTESIAN_POINT ( 'NONE',  ( 21.04999999999953886, 6.144958646240215927, -199.6091629096070790 ) ) ;
#254543 = CARTESIAN_POINT ( 'NONE',  ( 18.49999999999999289, 65.79142135624907439, -78.37310748452438247 ) ) ;
#254542 = CIRCLE ( 'NONE', #204490, 0.1000000000000028644 ) ;
#254544 = CARTESIAN_POINT ( 'NONE',  ( 15.74999999999999645, 66.65000000001204228, -119.7731074845243739 ) ) ;
#254545 = DIRECTION ( 'NONE',  ( 0.000000000000000000, 1.000000000000000000, 0.000000000000000000 ) ) ;
#254546 = FACE_OUTER_BOUND ( 'NONE', #203636, .T. ) ;
#254547 = ORIENTED_EDGE ( 'NONE', *, *, #210910, .T. ) ;
#254548 = AXIS2_PLACEMENT_3D ( 'NONE', #239200, #37167, #241759 ) ;
#254549 = ADVANCED_FACE ( 'NONE', ( #171467 ), #72344, .T. ) ;
#254550 = CARTESIAN_POINT ( 'NONE',  ( -20.64999999999999858, 85.00000000001188027, -93.62913836187181005 ) ) ;
#254551 = ORIENTED_EDGE ( 'NONE', *, *, #48956, .F. ) ;
#254552 = CIRCLE ( 'NONE', #217141, 0.09999999999999939493 ) ;
#254553 = ADVANCED_FACE ( 'NONE', ( #74925 ), #148587, .F. ) ;
#254554 = FACE_OUTER_BOUND ( 'NONE', #158921, .T. ) ;
#254555 = ORIENTED_EDGE ( 'NONE', *, *, #241797, .T. ) ;
#254556 = CYLINDRICAL_SURFACE ( 'NONE', #205260, 0.1000000000000028644 ) ;
#254557 = VECTOR ( 'NONE', #232766, 1000.000000000000000 ) ;
#254558 = FACE_OUTER_BOUND ( 'NONE', #3351, .T. ) ;
#254559 = EDGE_CURVE ( 'NONE', #151679, #73109, #102749, .T. ) ;
#254560 = DIRECTION ( 'NONE',  ( 0.000000000000000000, 0.7106264324241465813, -0.7035695228903323661 ) ) ;
#254561 = ORIENTED_EDGE ( 'NONE', *, *, #139149, .T. ) ;
#254562 = ORIENTED_EDGE ( 'NONE', *, *, #231527, .F. ) ;
#254563 = EDGE_CURVE ( 'NONE', #60863, #101410, #227668, .T. ) ;
#254564 = AXIS2_PLACEMENT_3D ( 'NONE', #91603, #6918, #66898 ) ;
#254565 = LINE ( 'NONE', #75964, #165127 ) ;
#254566 = CARTESIAN_POINT ( 'NONE',  ( 20.95512820512820440, 10.49413282287806481, -207.4737445703522383 ) ) ;
#254567 = DIRECTION ( 'NONE',  ( -1.000000000000000000, 7.304098846218135653E-16, -4.607487905232624742E-31 ) ) ;
#254568 = DIRECTION ( 'NONE',  ( 0.000000000000000000, 0.000000000000000000, 1.000000000000000000 ) ) ;
#254569 = EDGE_CURVE ( 'NONE', #101850, #68928, #52692, .T. ) ;
#254571 = DIRECTION ( 'NONE',  ( 1.000000000000000000, 0.000000000000000000, 0.000000000000000000 ) ) ;
#254570 = DIRECTION ( 'NONE',  ( -3.469446951953605354E-14, -0.9999176327611372095, -0.01283462868039623485 ) ) ;
#254572 = VECTOR ( 'NONE', #196939, 999.9999999999998863 ) ;
#254573 = CARTESIAN_POINT ( 'NONE',  ( 21.08078803292165659, 6.333012964448272442, -167.4208140128421860 ) ) ;
#254574 = CARTESIAN_POINT ( 'NONE',  ( 12.93279065517211990, 9.417690691074255938, -51.64160069676457709 ) ) ;
#254576 = SPHERICAL_SURFACE ( 'NONE', #255210, 0.1000000000000000056 ) ;
#254575 = AXIS2_PLACEMENT_3D ( 'NONE', #129001, #53308, #169444 ) ;
#254577 = VERTEX_POINT ( 'NONE', #154469 ) ;
#254578 = CARTESIAN_POINT ( 'NONE',  ( -21.55000000000000071, 7.350000000011155166, -79.35000000000005116 ) ) ;
#254579 = EDGE_CURVE ( 'NONE', #85514, #205599, #19399, .T. ) ;
#254581 = EDGE_LOOP ( 'NONE', ( #97374, #37666, #153734, #115520, #19414 ) ) ;
#254580 = SPHERICAL_SURFACE ( 'NONE', #107247, 0.1000000000000000056 ) ;
#254582 = DIRECTION ( 'NONE',  ( 0.000000000000000000, 1.000000000000000000, 0.000000000000000000 ) ) ;
#254584 = ADVANCED_FACE ( 'NONE', ( #150588 ), #129731, .F. ) ;
#254583 = EDGE_CURVE ( 'NONE', #86349, #204570, #198455, .T. ) ;
#254585 = FACE_OUTER_BOUND ( 'NONE', #204736, .T. ) ;
#254587 = CARTESIAN_POINT ( 'NONE',  ( 21.14999999999999858, 6.650000000011155876, -79.15000000000004832 ) ) ;
#254586 = CARTESIAN_POINT ( 'NONE',  ( -20.94999999999999929, 1.835341550235569663, -145.5551512925629822 ) ) ;
#254588 = VECTOR ( 'NONE', #57987, 1000.000000000000114 ) ;
#254590 = ORIENTED_EDGE ( 'NONE', *, *, #200678, .T. ) ;
#254589 = DIRECTION ( 'NONE',  ( -1.000000000000000000, 0.000000000000000000, 0.000000000000000000 ) ) ;
#254592 = DIRECTION ( 'NONE',  ( 1.000000000000000000, 0.000000000000000000, 0.000000000000000000 ) ) ;
#254591 = LINE ( 'NONE', #248515, #234958 ) ;
#254593 = CARTESIAN_POINT ( 'NONE',  ( -18.50000000000000000, 64.35000000001276987, -215.2731074845244450 ) ) ;
#254594 = CARTESIAN_POINT ( 'NONE',  ( 18.39999999999999503, 64.52683809664981140, -157.3731074845244393 ) ) ;
#254595 = CARTESIAN_POINT ( 'NONE',  ( -20.85000000000000142, 77.85161776048127535, -158.4199177649206831 ) ) ;
#254597 = DIRECTION ( 'NONE',  ( 0.000000000000000000, -2.910293365522255334E-14, 1.000000000000000000 ) ) ;
#254596 = VECTOR ( 'NONE', #21260, 1000.000000000000000 ) ;
#254598 = VERTEX_POINT ( 'NONE', #134837 ) ;
#254599 = FACE_OUTER_BOUND ( 'NONE', #184918, .T. ) ;
#254600 = ORIENTED_EDGE ( 'NONE', *, *, #236566, .T. ) ;
#254601 = DIRECTION ( 'NONE',  ( -1.000000000000000000, 0.000000000000000000, 0.000000000000000000 ) ) ;
#254602 = ORIENTED_EDGE ( 'NONE', *, *, #148210, .T. ) ;
#254604 = CARTESIAN_POINT ( 'NONE',  ( -16.87331047859649757, 9.950000000011138823, -154.8500000000000227 ) ) ;
#254603 = AXIS2_PLACEMENT_3D ( 'NONE', #77973, #40453, #101628 ) ;
#254605 = EDGE_CURVE ( 'NONE', #202021, #13934, #115247, .T. ) ;
#254607 = ADVANCED_FACE ( 'NONE', ( #233963 ), #54041, .F. ) ;
#254606 = CIRCLE ( 'NONE', #67186, 11.75000000000001066 ) ;
#254608 = CIRCLE ( 'NONE', #142196, 0.1000000000000028644 ) ;
#254609 = ORIENTED_EDGE ( 'NONE', *, *, #9864, .T. ) ;
#254610 =( BOUNDED_SURFACE ( )  B_SPLINE_SURFACE ( 3, 2, ( 
 ( #50568, #234355, #91000 ),
 ( #233111, #175697, #114423 ),
 ( #55685, #214796, #72762 ),
 ( #255152, #15343, #252631 ),
 ( #71466, #76567, #92278 ),
 ( #74045, #150985, #230525 ) ),
 .UNSPECIFIED., .F., .F., .T. ) 
 B_SPLINE_SURFACE_WITH_KNOTS ( ( 4, 2, 4 ),
 ( 3, 3 ),
 ( 0.0001342700090130149982, 0.0002909192928057525150, 0.0004475685765984900046 ),
 ( 0.000000000000000000, 1.000000000000000000 ),
 .UNSPECIFIED. ) 
 GEOMETRIC_REPRESENTATION_ITEM ( )  RATIONAL_B_SPLINE_SURFACE ( (
 ( 1.000000000000000000, 0.7250110520819876836, 1.000000000000000000),
 ( 1.000000000000000000, 0.7257599279136385251, 1.000000000000000000),
 ( 1.000000000000000000, 0.7137594617280956788, 1.000000000000000000),
 ( 1.000000000000000000, 0.6959270178813491414, 1.000000000000000000),
 ( 1.000000000000000000, 0.6919879549336065416, 1.000000000000000000),
 ( 1.000000000000000000, 0.7071067811865494601, 1.000000000000000000) ) ) 
 REPRESENTATION_ITEM ( '' )  SURFACE ( )  );
#254611 = CARTESIAN_POINT ( 'NONE',  ( -23.25000000000000000, -1.164121893241208960, -41.41484808557160591 ) ) ;
#254612 = CARTESIAN_POINT ( 'NONE',  ( 21.97500000000000497, 66.25000000001229239, -157.6731074845244223 ) ) ;
#254613 = ADVANCED_FACE ( 'NONE', ( #114007 ), #131012, .T. ) ;
#254614 = CARTESIAN_POINT ( 'NONE',  ( -18.59999999999999787, 9.250000000011157297, -88.15000000000004832 ) ) ;
#254615 = VERTEX_POINT ( 'NONE', #228843 ) ;
#254616 = ADVANCED_FACE ( 'NONE', ( #194866 ), #16233, .T. ) ;
#254617 = CARTESIAN_POINT ( 'NONE',  ( -20.94999999999999929, 70.10000000001197407, -113.2422072491807086 ) ) ;
#254618 = ADVANCED_FACE ( 'NONE', ( #110161 ), #40274, .F. ) ;
#254619 = DIRECTION ( 'NONE',  ( 1.000000000000000000, 0.000000000000000000, -0.000000000000000000 ) ) ;
#254620 = DIRECTION ( 'NONE',  ( 1.000000000000000000, 0.000000000000000000, 0.000000000000000000 ) ) ;
#254621 = DIRECTION ( 'NONE',  ( 1.186688945009010077E-16, -1.000000000000000000, -0.000000000000000000 ) ) ;
#254622 = ORIENTED_EDGE ( 'NONE', *, *, #5172, .T. ) ;
#254623 = CARTESIAN_POINT ( 'NONE',  ( -18.36527282682031625, 85.50000060001103463, -129.6009585200223455 ) ) ;
#254624 = ORIENTED_EDGE ( 'NONE', *, *, #247089, .F. ) ;
#254626 = ORIENTED_EDGE ( 'NONE', *, *, #196250, .F. ) ;
#254625 = DIRECTION ( 'NONE',  ( 1.000000000000000000, 0.000000000000000000, 0.000000000000000000 ) ) ;
#254627 = ORIENTED_EDGE ( 'NONE', *, *, #40615, .T. ) ;
#254628 = CARTESIAN_POINT ( 'NONE',  ( 18.50000000000000711, 85.41920976342188965, -196.2753380217653785 ) ) ;
#254629 = DIRECTION ( 'NONE',  ( 0.000000000000000000, -1.000000000000000000, 0.000000000000000000 ) ) ;
#254630 = DIRECTION ( 'NONE',  ( 0.000000000000000000, 0.000000000000000000, 1.000000000000000000 ) ) ;
#254631 = LINE ( 'NONE', #19919, #82 ) ;
#254632 = ORIENTED_EDGE ( 'NONE', *, *, #69680, .F. ) ;
#254633 = EDGE_CURVE ( 'NONE', #234345, #53002, #73586, .T. ) ;
#254634 = DIRECTION ( 'NONE',  ( -1.000000000000000000, 0.000000000000000000, 0.000000000000000000 ) ) ;
#254636 = ORIENTED_EDGE ( 'NONE', *, *, #252432, .T. ) ;
#254635 = VECTOR ( 'NONE', #222339, 1000.000000000000000 ) ;
#254638 = VERTEX_POINT ( 'NONE', #20072 ) ;
#254637 = DIRECTION ( 'NONE',  ( 1.000000000000000000, 0.000000000000000000, 0.000000000000000000 ) ) ;
#254639 = CARTESIAN_POINT ( 'NONE',  ( -21.65000000000000213, 66.05000000001230376, -157.2731074845244166 ) ) ;
#254640 = EDGE_CURVE ( 'NONE', #97822, #123700, #219297, .T. ) ;
#254641 = LINE ( 'NONE', #218091, #9744 ) ;
#254642 = AXIS2_PLACEMENT_3D ( 'NONE', #16286, #76215, #51501 ) ;
#254643 = LINE ( 'NONE', #61612, #217280 ) ;
#254644 = ORIENTED_EDGE ( 'NONE', *, *, #435, .F. ) ;
#254645 = DIRECTION ( 'NONE',  ( 0.000000000000000000, -0.9876197685951252359, -0.1568667991644863424 ) ) ;
#254646 = ADVANCED_FACE ( 'NONE', ( #17483 ), #106867, .F. ) ;
#254647 = CARTESIAN_POINT ( 'NONE',  ( 12.25000000000000000, 66.65000000001155911, -52.77310748452440237 ) ) ;
#254648 = FACE_OUTER_BOUND ( 'NONE', #91301, .T. ) ;
#254649 = ADVANCED_FACE ( 'NONE', ( #98266 ), #176582, .T. ) ;
#254650 = CIRCLE ( 'NONE', #204788, 0.09999999999999939493 ) ;
#254652 = ORIENTED_EDGE ( 'NONE', *, *, #60810, .F. ) ;
#254651 = CIRCLE ( 'NONE', #33981, 11.64999999999999325 ) ;
#254653 = FACE_BOUND ( 'NONE', #33555, .T. ) ;
#254654 = ORIENTED_EDGE ( 'NONE', *, *, #217702, .T. ) ;
#254655 = FACE_OUTER_BOUND ( 'NONE', #529, .T. ) ;
#254657 = ORIENTED_EDGE ( 'NONE', *, *, #156013, .T. ) ;
#254656 = CARTESIAN_POINT ( 'NONE',  ( 20.97468175916176847, 10.62526516438217605, -146.2547614354128314 ) ) ;
#254658 = DIRECTION ( 'NONE',  ( 0.000000000000000000, 0.000000000000000000, 1.000000000000000000 ) ) ;
#254659 = DIRECTION ( 'NONE',  ( 1.000000000000000000, 0.000000000000000000, 0.000000000000000000 ) ) ;
#254660 = DIRECTION ( 'NONE',  ( -0.7071067811865463515, 0.7071067811865487940, 4.178957128135655137E-15 ) ) ;
#254661 = CYLINDRICAL_SURFACE ( 'NONE', #22515, 11.80000000000000426 ) ;
#254662 = CARTESIAN_POINT ( 'NONE',  ( 21.08078803292165659, 6.333012964448272442, -66.92081401284225706 ) ) ;
#254664 = ORIENTED_EDGE ( 'NONE', *, *, #12537, .T. ) ;
#254663 = CARTESIAN_POINT ( 'NONE',  ( -21.22070241538126112, 69.53005372714252985, -136.6220265150593605 ) ) ;
#254665 = LINE ( 'NONE', #117766, #189184 ) ;
#254666 = CARTESIAN_POINT ( 'NONE',  ( -18.34374000495059676, 16.37079970714665933, -222.2530670965321349 ) ) ;
#254667 = FACE_OUTER_BOUND ( 'NONE', #37957, .T. ) ;
#254668 = EDGE_LOOP ( 'NONE', ( #135612, #241581, #37328, #213165 ) ) ;
#254669 = CARTESIAN_POINT ( 'NONE',  ( 21.05000000000000071, -4.756823075239758225, -233.1486023682345490 ) ) ;
#254670 = VECTOR ( 'NONE', #92713, 1000.000000000000000 ) ;
#254672 = ADVANCED_FACE ( 'NONE', ( #159575 ), #27801, .T. ) ;
#254671 = AXIS2_PLACEMENT_3D ( 'NONE', #167720, #204239, #24352 ) ;
#254673 = CARTESIAN_POINT ( 'NONE',  ( 23.24999999999999289, 6.450000000000001066, -21.15000000000000213 ) ) ;
#254674 = CARTESIAN_POINT ( 'NONE',  ( 20.04142135623730070, 51.38014393322265505, -230.1906178717505611 ) ) ;
#254675 = AXIS2_PLACEMENT_3D ( 'NONE', #133688, #232814, #154573 ) ;
#254676 = EDGE_LOOP ( 'NONE', ( #28733, #109310 ) ) ;
#254677 = CARTESIAN_POINT ( 'NONE',  ( 20.94999999999999574, 69.65000000001205649, -126.6792853948412159 ) ) ;
#254678 = CARTESIAN_POINT ( 'NONE',  ( 21.05000000000000071, 5.850000000011105428, -43.63249722427796939 ) ) ;
#254679 = ORIENTED_EDGE ( 'NONE', *, *, #234061, .F. ) ;
#254680 = LINE ( 'NONE', #33157, #110964 ) ;
#254681 = EDGE_LOOP ( 'NONE', ( #43032, #72517, #115000 ) ) ;
#254682 = EDGE_CURVE ( 'NONE', #34877, #85029, #196130, .T. ) ;
#254683 = DIRECTION ( 'NONE',  ( 0.000000000000000000, -0.2617529984164915779, -0.9651348961777189706 ) ) ;
#254685 = ORIENTED_EDGE ( 'NONE', *, *, #54576, .F. ) ;
#254684 = CARTESIAN_POINT ( 'NONE',  ( 21.05000000000000071, 6.413978881499349249, -134.0857991162740177 ) ) ;
#254686 = AXIS2_PLACEMENT_3D ( 'NONE', #128583, #28231, #243384 ) ;
#254688 = ADVANCED_FACE ( 'NONE', ( #38349 ), #237822, .T. ) ;
#254687 = PLANE ( 'NONE',  #102416 ) ;
#254689 = VERTEX_POINT ( 'NONE', #60451 ) ;
#254690 = CARTESIAN_POINT ( 'NONE',  ( 21.05000000000000071, 6.650000000011155876, -110.5170271704400591 ) ) ;
#254691 = VERTEX_POINT ( 'NONE', #136118 ) ;
#254693 = EDGE_LOOP ( 'NONE', ( #38684, #195656, #29333, #54961 ) ) ;
#254692 = ORIENTED_EDGE ( 'NONE', *, *, #103472, .T. ) ;
#254694 = CARTESIAN_POINT ( 'NONE',  ( 18.46947024752525479, 85.50929715716807777, -129.5364180358261592 ) ) ;
#254695 = VERTEX_POINT ( 'NONE', #219525 ) ;
#254696 = CARTESIAN_POINT ( 'NONE',  ( 23.14999999999999503, 64.35000000001245724, -181.7731074845244450 ) ) ;
#254698 = EDGE_CURVE ( 'NONE', #116061, #158643, #39653, .T. ) ;
#254697 = ORIENTED_EDGE ( 'NONE', *, *, #197697, .F. ) ;
#254699 = EDGE_CURVE ( 'NONE', #248676, #14789, #117862, .T. ) ;
#254700 = ADVANCED_FACE ( 'NONE', ( #160870 ), #119164, .F. ) ;
#254701 = ORIENTED_EDGE ( 'NONE', *, *, #142671, .T. ) ;
#254702 = DIRECTION ( 'NONE',  ( -1.000000000000000000, 0.000000000000000000, 0.000000000000000000 ) ) ;
#254704 = CARTESIAN_POINT ( 'NONE',  ( -23.15000000000000213, 11.65000000001115588, -134.0000000000000000 ) ) ;
#254703 = CIRCLE ( 'NONE', #171406, 11.80000000000000426 ) ;
#254705 = LINE ( 'NONE', #173987, #65674 ) ;
#254706 = ORIENTED_EDGE ( 'NONE', *, *, #1998, .F. ) ;
#254707 = ADVANCED_FACE ( 'NONE', ( #61750 ), #141292, .T. ) ;
#254708 = DIRECTION ( 'NONE',  ( 0.000000000000000000, -1.000000000000000000, 0.000000000000000000 ) ) ;
#254709 = CARTESIAN_POINT ( 'NONE',  ( 20.97239005616515328, 67.12515615866219321, -157.7729546823712496 ) ) ;
#254710 = DIRECTION ( 'NONE',  ( 0.000000000000000000, 0.8814952561688427224, -0.4721928772777352901 ) ) ;
#254711 = CIRCLE ( 'NONE', #42377, 11.80000000000000426 ) ;
#254712 = ORIENTED_EDGE ( 'NONE', *, *, #92875, .F. ) ;
#254713 = LINE ( 'NONE', #134791, #104436 ) ;
#254714 = CARTESIAN_POINT ( 'NONE',  ( -18.39999999999999858, 38.27493434228537694, -261.1939574891503639 ) ) ;
#254715 = DIRECTION ( 'NONE',  ( 1.000000000000000000, 0.000000000000000000, 0.000000000000000000 ) ) ;
#254716 = ADVANCED_FACE ( 'NONE', ( #18764 ), #61269, .T. ) ;
#254717 = CIRCLE ( 'NONE', #229817, 0.5000000000000004441 ) ;
#254718 = ORIENTED_EDGE ( 'NONE', *, *, #120521, .F. ) ;
#254719 = CARTESIAN_POINT ( 'NONE',  ( -20.65000000000000568, 65.69159657275406516, -213.8343546826533839 ) ) ;
#254720 = ORIENTED_EDGE ( 'NONE', *, *, #237643, .F. ) ;
#254721 = EDGE_LOOP ( 'NONE', ( #28644, #204973, #230818, #197310 ) ) ;
#254722 = CIRCLE ( 'NONE', #250488, 0.09999999999999971412 ) ;
#254723 = ADVANCED_FACE ( 'NONE', ( #3041 ), #182083, .T. ) ;
#254724 = DIRECTION ( 'NONE',  ( 1.000000000000000000, 2.952720810173289112E-16, -0.000000000000000000 ) ) ;
#254725 = ORIENTED_EDGE ( 'NONE', *, *, #26630, .F. ) ;
#254726 = VECTOR ( 'NONE', #157459, 1000.000000000000000 ) ;
#254727 = ORIENTED_EDGE ( 'NONE', *, *, #107950, .T. ) ;
#254728 = DIRECTION ( 'NONE',  ( 0.000000000000000000, 0.2128009952263485993, -0.9770955615653341697 ) ) ;
#254729 = CARTESIAN_POINT ( 'NONE',  ( -16.94107738177414291, 10.01423928514777373, -188.4499999999999886 ) ) ;
#254730 = ORIENTED_EDGE ( 'NONE', *, *, #205105, .F. ) ;
#254731 = EDGE_CURVE ( 'NONE', #191682, #217247, #186172, .T. ) ;
#254732 = VERTEX_POINT ( 'NONE', #203826 ) ;
#254733 = DIRECTION ( 'NONE',  ( -1.073024830501117725E-15, 0.000000000000000000, 1.000000000000000000 ) ) ;
#254734 = VECTOR ( 'NONE', #253232, 1000.000000000000000 ) ;
#254735 = FACE_OUTER_BOUND ( 'NONE', #193498, .T. ) ;
#254736 = EDGE_CURVE ( 'NONE', #5729, #64826, #246798, .T. ) ;
#254737 = ORIENTED_EDGE ( 'NONE', *, *, #73687, .F. ) ;
#254738 = CIRCLE ( 'NONE', #96546, 0.1000000000000008937 ) ;
#254739 = AXIS2_PLACEMENT_3D ( 'NONE', #67417, #83090, #7437 ) ;
#254740 = ORIENTED_EDGE ( 'NONE', *, *, #81730, .T. ) ;
#254741 = CARTESIAN_POINT ( 'NONE',  ( -20.85000000000000142, 1.115600667400684642E-11, -100.5000000000000426 ) ) ;
#254742 = CIRCLE ( 'NONE', #142363, 0.9750000000000036415 ) ;
#254743 = ADVANCED_FACE ( 'NONE', ( #227239 ), #184262, .F. ) ;
#254744 = DIRECTION ( 'NONE',  ( 0.5000000000001141309, 0.000000000000000000, -0.8660254037843729824 ) ) ;
#254745 = AXIS2_PLACEMENT_3D ( 'NONE', #48486, #125473, #65481 ) ;
#254746 = FACE_BOUND ( 'NONE', #203483, .T. ) ;
#254747 = CARTESIAN_POINT ( 'NONE',  ( -23.15000000000000213, 11.65000000001115588, -88.35000000000003695 ) ) ;
#254748 = CARTESIAN_POINT ( 'NONE',  ( -24.30000000000000071, -12.80000000000000249, -347.0000000000001137 ) ) ;
#254749 = DIRECTION ( 'NONE',  ( 1.000000000000000000, 0.000000000000000000, 0.000000000000000000 ) ) ;
#254750 = CARTESIAN_POINT ( 'NONE',  ( -21.14999999999999858, 11.75000000000000000, -6.783865662978153743 ) ) ;
#254751 = CARTESIAN_POINT ( 'NONE',  ( -16.87368910959167678, 9.961273816691395666, -12.61249309664058948 ) ) ;
#254752 = DIRECTION ( 'NONE',  ( 1.000000000000000000, 0.000000000000000000, 0.000000000000000000 ) ) ;
#254753 = CARTESIAN_POINT ( 'NONE',  ( -16.97683809663752186, 23.64127277249475156, -231.2903243416350847 ) ) ;
#254754 = CARTESIAN_POINT ( 'NONE',  ( -18.59999999999999787, 11.65000000001115232, -179.6499999999999773 ) ) ;
#254755 = CIRCLE ( 'NONE', #184075, 0.1000000000000001860 ) ;
#254756 = CARTESIAN_POINT ( 'NONE',  ( 18.49999999999999289, 10.20857864377385127, -188.8499999999999659 ) ) ;
#254757 = AXIS2_PLACEMENT_3D ( 'NONE', #122169, #60892, #2192 ) ;
#254759 = ORIENTED_EDGE ( 'NONE', *, *, #241836, .F. ) ;
#254758 = AXIS2_PLACEMENT_3D ( 'NONE', #53901, #235114, #16088 ) ;
#254760 = EDGE_CURVE ( 'NONE', #228853, #229059, #86417, .T. ) ;
#254761 = VECTOR ( 'NONE', #244928, 1000.000000000000000 ) ;
#254763 = EDGE_LOOP ( 'NONE', ( #74742, #88056, #253421, #11717 ) ) ;
#254762 = CARTESIAN_POINT ( 'NONE',  ( -23.25000000000000355, 11.75000000001113953, -158.2500000000000284 ) ) ;
#254764 = EDGE_CURVE ( 'NONE', #100166, #27850, #189934, .T. ) ;
#254765 = DIRECTION ( 'NONE',  ( 1.000000000000000000, -7.049440681616510987E-16, 1.911869773728121864E-16 ) ) ;
#254766 = CARTESIAN_POINT ( 'NONE',  ( 18.49999999999998934, 6.450000000011156587, -43.51702717044002355 ) ) ;
#254767 = VERTEX_POINT ( 'NONE', #245538 ) ;
#254768 = ADVANCED_FACE ( 'NONE', ( #26494 ), #23937, .F. ) ;
#254769 = ADVANCED_FACE ( 'NONE', ( #166020 ), #244219, .F. ) ;
#254770 = DIRECTION ( 'NONE',  ( 1.000000000000000000, 0.000000000000000000, 0.000000000000000000 ) ) ;
#254771 = CARTESIAN_POINT ( 'NONE',  ( -17.11825945287482043, 9.950000000011145929, -54.35000000000000853 ) ) ;
#254772 = TOROIDAL_SURFACE ( 'NONE', #138108, 12.77499999999999858, 0.1000000000000000056 ) ;
#254773 = ADVANCED_FACE ( 'NONE', ( #164710 ), #11757, .T. ) ;
#254774 = ORIENTED_EDGE ( 'NONE', *, *, #144061, .F. ) ;
#254775 = CYLINDRICAL_SURFACE ( 'NONE', #21481, 0.09999999999999939493 ) ;
#254776 = CARTESIAN_POINT ( 'NONE',  ( 20.04142135623730070, 64.25000000001199396, -115.1731074845243796 ) ) ;
#254777 = EDGE_CURVE ( 'NONE', #100115, #134738, #115424, .T. ) ;
#254778 = DIRECTION ( 'NONE',  ( 0.000000000000000000, 0.000000000000000000, 1.000000000000000000 ) ) ;
#254780 = ORIENTED_EDGE ( 'NONE', *, *, #194321, .F. ) ;
#254779 = LINE ( 'NONE', #211873, #160214 ) ;
#254782 = EDGE_LOOP ( 'NONE', ( #118234, #87212, #11532, #233870 ) ) ;
#254781 = CARTESIAN_POINT ( 'NONE',  ( -18.31331870001012163, 85.53629471919282423, -96.15452879353861704 ) ) ;
#254783 = LINE ( 'NONE', #257340, #137539 ) ;
#254784 = CARTESIAN_POINT ( 'NONE',  ( -18.59999999999999787, 61.57587952878036930, -212.2000740415318774 ) ) ;
#254785 = DIRECTION ( 'NONE',  ( 0.000000000000000000, 0.000000000000000000, -1.000000000000000000 ) ) ;
#254786 = CARTESIAN_POINT ( 'NONE',  ( -23.25000000000000000, -8.596261682231832069, -91.04987248284976431 ) ) ;
#254788 = DIRECTION ( 'NONE',  ( -1.000000000000000000, -3.448943450116723568E-16, -6.438528483529607644E-16 ) ) ;
#254787 = CARTESIAN_POINT ( 'NONE',  ( -16.80621392010912629, 9.942202577518866491, -154.8104080345828777 ) ) ;
#254789 = CARTESIAN_POINT ( 'NONE',  ( -22.39999999999999858, 29.50811709945089945, -252.6450601445781103 ) ) ;
#254790 = DIRECTION ( 'NONE',  ( -1.000000000000000000, -0.000000000000000000, 0.000000000000000000 ) ) ;
#254791 = LINE ( 'NONE', #14969, #101901 ) ;
#254792 = CARTESIAN_POINT ( 'NONE',  ( 18.69999999999999929, -8.150000000000007461, 32.89999999999999858 ) ) ;
#254793 = ORIENTED_EDGE ( 'NONE', *, *, #173284, .F. ) ;
#254794 = EDGE_CURVE ( 'NONE', #71381, #91407, #140366, .T. ) ;
#254796 = CIRCLE ( 'NONE', #204768, 4.049999999999998934 ) ;
#254795 = DIRECTION ( 'NONE',  ( 1.000000000000000000, 0.000000000000000000, 0.000000000000000000 ) ) ;
#254797 = ORIENTED_EDGE ( 'NONE', *, *, #138465, .T. ) ;
#254798 = EDGE_LOOP ( 'NONE', ( #79763, #256311, #151822, #91643, #105760 ) ) ;
#254799 = LINE ( 'NONE', #17515, #115166 ) ;
#254800 = CARTESIAN_POINT ( 'NONE',  ( -21.14999999999994174, 64.25000000001119815, -5.923107484524795296 ) ) ;
#254801 = EDGE_CURVE ( 'NONE', #216892, #185811, #111155, .T. ) ;
#254802 = ORIENTED_EDGE ( 'NONE', *, *, #204840, .F. ) ;
#254803 = EDGE_CURVE ( 'NONE', #177843, #97884, #214108, .T. ) ;
#254804 = ORIENTED_EDGE ( 'NONE', *, *, #25214, .F. ) ;
#254805 = DIRECTION ( 'NONE',  ( 1.000000000000000000, 3.448943450116723568E-16, 6.438528483529607644E-16 ) ) ;
#254806 = FILL_AREA_STYLE_COLOUR ( '', #10813 ) ;
#254807 = EDGE_CURVE ( 'NONE', #211829, #206022, #13343, .T. ) ;
#254808 = CIRCLE ( 'NONE', #21644, 0.1000000000000001860 ) ;
#254809 = ORIENTED_EDGE ( 'NONE', *, *, #244798, .T. ) ;
#254810 = VERTEX_POINT ( 'NONE', #193267 ) ;
#254811 = VECTOR ( 'NONE', #218375, 1000.000000000000000 ) ;
#254812 = DIRECTION ( 'NONE',  ( 0.000000000000000000, 0.000000000000000000, -1.000000000000000000 ) ) ;
#254813 = CARTESIAN_POINT ( 'NONE',  ( -18.59999999999999787, 11.65000000001115232, -40.51480577065400013 ) ) ;
#254814 = DIRECTION ( 'NONE',  ( 1.000000000000000000, 0.000000000000000000, 0.000000000000000000 ) ) ;
#254815 = DIRECTION ( 'NONE',  ( -1.000000000000000000, -0.000000000000000000, -0.000000000000000000 ) ) ;
#254816 = CARTESIAN_POINT ( 'NONE',  ( 12.47034474403012361, 9.375538102048006195, -15.86987588099082735 ) ) ;
#254817 = CARTESIAN_POINT ( 'NONE',  ( 18.49999999999999645, 77.29973367124252093, -79.49497796165491081 ) ) ;
#254818 = DIRECTION ( 'NONE',  ( 1.000000000000000000, 0.000000000000000000, 0.000000000000000000 ) ) ;
#254820 = EDGE_LOOP ( 'NONE', ( #91987, #187560, #27758, #228799 ) ) ;
#254819 = CARTESIAN_POINT ( 'NONE',  ( 23.14999999999999503, 64.35000000001218723, -143.5379132551784096 ) ) ;
#254822 = CARTESIAN_POINT ( 'NONE',  ( -21.05000000000000071, 68.48451787451661232, -224.2224406095231757 ) ) ;
#254821 = DIRECTION ( 'NONE',  ( -0.000000000000000000, -0.000000000000000000, 1.000000000000000000 ) ) ;
#254823 = CARTESIAN_POINT ( 'NONE',  ( 23.15000000000000213, 87.75000000001143974, -39.12310748452424747 ) ) ;
#254824 = ORIENTED_EDGE ( 'NONE', *, *, #250512, .T. ) ;
#254825 = DIRECTION ( 'NONE',  ( 0.000000000000000000, 0.000000000000000000, -1.000000000000000000 ) ) ;
#254826 = DIRECTION ( 'NONE',  ( 1.000000000000000000, 0.000000000000000000, 0.000000000000000000 ) ) ;
#254827 = EDGE_LOOP ( 'NONE', ( #233555, #200459, #108845, #198636 ) ) ;
#254828 = ADVANCED_FACE ( 'NONE', ( #129429 ), #251943, .T. ) ;
#254829 = VECTOR ( 'NONE', #246134, 1000.000000000000000 ) ;
#254830 = CARTESIAN_POINT ( 'NONE',  ( -23.25000000000000000, 62.12148660976906456, -247.5636999539406133 ) ) ;
#254831 = DIRECTION ( 'NONE',  ( 0.000000000000000000, 0.000000000000000000, -1.000000000000000000 ) ) ;
#254832 = ORIENTED_EDGE ( 'NONE', *, *, #173386, .T. ) ;
#254833 = ORIENTED_EDGE ( 'NONE', *, *, #247092, .T. ) ;
#254834 = DIRECTION ( 'NONE',  ( 0.000000000000000000, -0.8814952561688430555, 0.4721928772777346239 ) ) ;
#254835 = LINE ( 'NONE', #234041, #3252 ) ;
#254836 = DIRECTION ( 'NONE',  ( 1.000000000000000000, 0.000000000000000000, 0.000000000000000000 ) ) ;
#254837 = LINE ( 'NONE', #84887, #5487 ) ;
#254838 = VERTEX_POINT ( 'NONE', #113719 ) ;
#254839 = CARTESIAN_POINT ( 'NONE',  ( 13.76927104934457979, 46.49260333018392544, -234.7842902611276941 ) ) ;
#254840 = EDGE_CURVE ( 'NONE', #73105, #235787, #52881, .T. ) ;
#254841 = CONICAL_SURFACE ( 'NONE', #34368, 4.299999999999970512, 0.7853981633974466137 ) ;
#254842 = AXIS2_PLACEMENT_3D ( 'NONE', #154289, #233787, #253326 ) ;
#254843 = CARTESIAN_POINT ( 'NONE',  ( -18.50000000000000000, -1.164121893230052995, -141.7148480855716457 ) ) ;
#254844 = CARTESIAN_POINT ( 'NONE',  ( -23.25000000000000000, 71.65000000001180069, -81.67310748452435121 ) ) ;
#254845 = EDGE_CURVE ( 'NONE', #146449, #155707, #148770, .T. ) ;
#254846 = CARTESIAN_POINT ( 'NONE',  ( -18.50000000000000000, -9.399999999988850163, -207.8820418481726335 ) ) ;
#254847 = EDGE_CURVE ( 'NONE', #223143, #176594, #36353, .T. ) ;
#254849 = ORIENTED_EDGE ( 'NONE', *, *, #7214, .F. ) ;
#254848 = CARTESIAN_POINT ( 'NONE',  ( -22.59999999999999787, 11.74956712350054744, -66.89914163090134025 ) ) ;
#254850 = EDGE_CURVE ( 'NONE', #160408, #177524, #250645, .T. ) ;
#254851 = CARTESIAN_POINT ( 'NONE',  ( -16.87683809663752399, 66.15000000001190017, -89.62074346632789457 ) ) ;
#254852 = DIRECTION ( 'NONE',  ( 0.000000000000000000, -1.000000000000000000, 0.000000000000000000 ) ) ;
#254853 = CARTESIAN_POINT ( 'NONE',  ( -20.85000000000000142, 42.20719072976272912, -239.1935934412594804 ) ) ;
#254854 = CARTESIAN_POINT ( 'NONE',  ( 23.14999999999999858, 70.50000000001223555, -148.9283735034374843 ) ) ;
#254856 = ORIENTED_EDGE ( 'NONE', *, *, #240803, .T. ) ;
#254855 = DIRECTION ( 'NONE',  ( 0.000000000000000000, 0.000000000000000000, 1.000000000000000000 ) ) ;
#254857 = SPHERICAL_SURFACE ( 'NONE', #159493, 0.1000000000000000056 ) ;
#254858 = DIRECTION ( 'NONE',  ( 0.000000000000000000, -0.9126074666063771490, -0.4088369013363281623 ) ) ;
#254859 = VECTOR ( 'NONE', #103244, 1000.000000000000114 ) ;
#254860 = VERTEX_POINT ( 'NONE', #208964 ) ;
#254861 = CARTESIAN_POINT ( 'NONE',  ( -18.59999999999999787, 63.79568978998910467, -212.8021059378898485 ) ) ;
#254862 = DIRECTION ( 'NONE',  ( 0.000000000000000000, 0.000000000000000000, 1.000000000000000000 ) ) ;
#254863 = LINE ( 'NONE', #115409, #254588 ) ;
#254864 = CARTESIAN_POINT ( 'NONE',  ( 20.94999999999999929, 78.50726470275242264, -228.6618886302502176 ) ) ;
#254865 = DIRECTION ( 'NONE',  ( 0.000000000000000000, -0.9915357197604972583, 0.1298341882519109536 ) ) ;
#254866 = CARTESIAN_POINT ( 'NONE',  ( 18.59999999999999432, 1.728086936805619311, -154.3844350051677452 ) ) ;
#254867 = ADVANCED_FACE ( 'NONE', ( #73343 ), #74638, .F. ) ;
#254868 = EDGE_CURVE ( 'NONE', #20227, #31671, #86182, .T. ) ;
#254869 = ORIENTED_EDGE ( 'NONE', *, *, #41955, .F. ) ;
#254870 = ORIENTED_EDGE ( 'NONE', *, *, #253867, .F. ) ;
#254871 = CARTESIAN_POINT ( 'NONE',  ( 22.47007471830800895, -1.642974910573245850, -193.4561278898739829 ) ) ;
#254872 = CARTESIAN_POINT ( 'NONE',  ( -23.25000000000000000, -0.09999999998884338825, -122.3504291924552234 ) ) ;
#254873 = TOROIDAL_SURFACE ( 'NONE', #134122, 0.9750000000000019762, 0.1000000000000000056 ) ;
#254874 = CARTESIAN_POINT ( 'NONE',  ( 18.49505816908824940, -0.6505778444486189915, -242.3635087541469773 ) ) ;
#254875 = DIRECTION ( 'NONE',  ( 1.000000000000000000, 0.000000000000000000, 0.000000000000000000 ) ) ;
#254876 = FACE_OUTER_BOUND ( 'NONE', #97774, .T. ) ;
#254877 = AXIS2_PLACEMENT_3D ( 'NONE', #145828, #186266, #188817 ) ;
#254878 = CARTESIAN_POINT ( 'NONE',  ( 20.30466543256790501, 10.84751624358901623, -207.0846662628387946 ) ) ;
#254879 = EDGE_CURVE ( 'NONE', #137789, #229678, #102938, .T. ) ;
#254880 = VECTOR ( 'NONE', #205980, 1000.000000000000114 ) ;
#254881 = AXIS2_PLACEMENT_3D ( 'NONE', #198317, #197021, #217858 ) ;
#254882 = CIRCLE ( 'NONE', #246570, 0.09999999999999741040 ) ;
#254883 = ADVANCED_FACE ( 'NONE', ( #172454 ), #9476, .F. ) ;
#254884 = DIRECTION ( 'NONE',  ( 0.000000000000000000, -0.1335171055202867274, -0.9910465087640866200 ) ) ;
#254885 = AXIS2_PLACEMENT_3D ( 'NONE', #72793, #231852, #14086 ) ;
#254886 = VERTEX_POINT ( 'NONE', #189411 ) ;
#254887 = FACE_OUTER_BOUND ( 'NONE', #70552, .T. ) ;
#254888 = ORIENTED_EDGE ( 'NONE', *, *, #156655, .F. ) ;
#254889 = ORIENTED_EDGE ( 'NONE', *, *, #199095, .T. ) ;
#254890 = CARTESIAN_POINT ( 'NONE',  ( 24.30000000000000071, 3.175288713399624818, 33.00000000000000000 ) ) ;
#254891 = CARTESIAN_POINT ( 'NONE',  ( -20.85000000000000142, 7.021664781911246322, -137.7335654018973514 ) ) ;
#254892 = PLANE ( 'NONE',  #224747 ) ;
#254893 = ORIENTED_EDGE ( 'NONE', *, *, #111124, .F. ) ;
#254894 = EDGE_CURVE ( 'NONE', #162422, #109178, #23707, .T. ) ;
#254895 = DIRECTION ( 'NONE',  ( -0.000000000000000000, 1.000000000000000000, 6.982962677686267499E-15 ) ) ;
#254896 = LINE ( 'NONE', #78868, #155474 ) ;
#254898 = FACE_OUTER_BOUND ( 'NONE', #92827, .T. ) ;
#254897 = TOROIDAL_SURFACE ( 'NONE', #38488, 1.900000000000002576, 0.1000000000000000056 ) ;
#254899 = EDGE_LOOP ( 'NONE', ( #105627, #214585 ) ) ;
#254900 = CARTESIAN_POINT ( 'NONE',  ( -12.25000000000000178, 9.350000000011139178, -150.7500000000000284 ) ) ;
#254901 = VECTOR ( 'NONE', #81047, 1000.000000000000000 ) ;
#254902 = CARTESIAN_POINT ( 'NONE',  ( -21.05000000000000071, -1.835341550213257733, -112.0551512925630249 ) ) ;
#254903 = DIRECTION ( 'NONE',  ( -0.000000000000000000, -0.000000000000000000, -1.000000000000000000 ) ) ;
#254904 = FACE_OUTER_BOUND ( 'NONE', #73611, .T. ) ;
#254906 = EDGE_CURVE ( 'NONE', #99805, #61430, #152884, .T. ) ;
#254905 = CIRCLE ( 'NONE', #192616, 4.150000000000001243 ) ;
#254907 = AXIS2_PLACEMENT_3D ( 'NONE', #175962, #1119, #78102 ) ;
#254908 = VECTOR ( 'NONE', #176004, 1000.000000000000000 ) ;
#254909 = ORIENTED_EDGE ( 'NONE', *, *, #203713, .F. ) ;
#254910 = CIRCLE ( 'NONE', #92661, 0.09999999999998898659 ) ;
#254911 = CARTESIAN_POINT ( 'NONE',  ( 20.95512820512820440, 10.62384868372303615, -121.7500000000000426 ) ) ;
#254912 = DIRECTION ( 'NONE',  ( 0.000000000000000000, 0.000000000000000000, -1.000000000000000000 ) ) ;
#254913 = ORIENTED_EDGE ( 'NONE', *, *, #188171, .T. ) ;
#254914 = CARTESIAN_POINT ( 'NONE',  ( 21.13498764882293557, 6.495618143485025975, -133.9983436052687011 ) ) ;
#254915 = ADVANCED_FACE ( 'NONE', ( #228545 ), #178873, .T. ) ;
#254916 = VECTOR ( 'NONE', #181791, 1000.000000000000000 ) ;
#254917 = CARTESIAN_POINT ( 'NONE',  ( -16.87683809663752399, 66.15000000001255387, -183.4254715027207396 ) ) ;
#254918 = DIRECTION ( 'NONE',  ( 0.000000000000000000, 0.000000000000000000, -1.000000000000000000 ) ) ;
#254919 = ORIENTED_EDGE ( 'NONE', *, *, #200813, .T. ) ;
#254920 = CARTESIAN_POINT ( 'NONE',  ( 18.49999999999999289, 68.97833521811233481, -166.1895420826271277 ) ) ;
#254921 = ORIENTED_EDGE ( 'NONE', *, *, #163530, .T. ) ;
#254922 = AXIS2_PLACEMENT_3D ( 'NONE', #15063, #58002, #171586 ) ;
#254923 = AXIS2_PLACEMENT_3D ( 'NONE', #243762, #245046, #204619 ) ;
#254924 = AXIS2_PLACEMENT_3D ( 'NONE', #10185, #88397, #89692 ) ;
#254925 = VERTEX_POINT ( 'NONE', #238812 ) ;
#254926 = DIRECTION ( 'NONE',  ( -1.000000000000000000, 0.000000000000000000, -0.000000000000000000 ) ) ;
#254927 = CARTESIAN_POINT ( 'NONE',  ( 18.54999999999999716, 8.750000000011182166, -188.3499999999999659 ) ) ;
#254930 = EDGE_LOOP ( 'NONE', ( #124816, #148026, #232488, #189333 ) ) ;
#254929 = CARTESIAN_POINT ( 'NONE',  ( -20.93284271247462058, 11.75000000001115019, -59.98519422934605672 ) ) ;
#254928 =( BOUNDED_SURFACE ( )  B_SPLINE_SURFACE ( 3, 2, ( 
 ( #191066, #171507, #250988 ),
 ( #72394, #151939, #34553 ),
 ( #52795, #132340, #33290 ),
 ( #114053, #112789, #14987 ),
 ( #247144, #192327, #13679 ),
 ( #73689, #232751, #54089 ) ),
 .UNSPECIFIED., .F., .F., .F. ) 
 B_SPLINE_SURFACE_WITH_KNOTS ( ( 4, 2, 4 ),
 ( 3, 3 ),
 ( 0.0001792624049599850797, 0.0003686986002125220850, 0.0005581347954650591175 ),
 ( 0.000000000000000000, 1.000000000000000000 ),
 .UNSPECIFIED. ) 
 GEOMETRIC_REPRESENTATION_ITEM ( )  RATIONAL_B_SPLINE_SURFACE ( (
 ( 1.000000000000000000, 0.9238795325112888479, 1.000000000000000000),
 ( 1.000000000000000000, 0.9229318695235336767, 1.000000000000000000),
 ( 1.000000000000000000, 0.8926288119235017415, 1.000000000000000000),
 ( 1.000000000000000000, 0.8123777807266672202, 1.000000000000000000),
 ( 1.000000000000000000, 0.7629087100935024734, 1.000000000000000000),
 ( 1.000000000000000000, 0.7071067811865475727, 1.000000000000000000) ) ) 
 REPRESENTATION_ITEM ( '' )  SURFACE ( )  );
#254931 = FACE_OUTER_BOUND ( 'NONE', #35420, .T. ) ;
#254932 = CARTESIAN_POINT ( 'NONE',  ( 21.14999999999999503, -0.09999999998884338825, -122.3504291924552234 ) ) ;
#254933 = DIRECTION ( 'NONE',  ( 1.000000000000000000, 7.049440681616511973E-16, -1.911869773728117427E-16 ) ) ;
#254934 = CYLINDRICAL_SURFACE ( 'NONE', #118494, 0.1000000000000028644 ) ;
#254935 = DIRECTION ( 'NONE',  ( 1.000000000000000000, 0.000000000000000000, 0.000000000000000000 ) ) ;
#254936 = CARTESIAN_POINT ( 'NONE',  ( 21.05000000000000071, 36.65892442174472876, -249.5511627012454596 ) ) ;
#254937 = DIRECTION ( 'NONE',  ( 1.000000000000000000, 0.000000000000000000, 0.000000000000000000 ) ) ;
#254939 = ORIENTED_EDGE ( 'NONE', *, *, #71764, .T. ) ;
#254938 = CYLINDRICAL_SURFACE ( 'NONE', #73696, 0.09999999999999609201 ) ;
#254941 = ORIENTED_EDGE ( 'NONE', *, *, #111360, .T. ) ;
#254940 = FACE_OUTER_BOUND ( 'NONE', #168665, .T. ) ;
#254943 = CARTESIAN_POINT ( 'NONE',  ( -20.94999999999999929, 74.73821383144705521, -128.4366085209788366 ) ) ;
#254942 = CARTESIAN_POINT ( 'NONE',  ( -16.91256925476571737, 60.87407910423024049, -221.1459158692213691 ) ) ;
#254945 = ORIENTED_EDGE ( 'NONE', *, *, #234903, .F. ) ;
#254944 = DIRECTION ( 'NONE',  ( 0.000000000000000000, -6.982962677686266711E-15, 1.000000000000000000 ) ) ;
#254946 = ORIENTED_EDGE ( 'NONE', *, *, #81032, .T. ) ;
#254947 = CARTESIAN_POINT ( 'NONE',  ( -21.05000000000000071, 6.540656951712397138, -167.5999999999999659 ) ) ;
#254948 = AXIS2_PLACEMENT_3D ( 'NONE', #49284, #6297, #47996 ) ;
#254949 = CARTESIAN_POINT ( 'NONE',  ( -18.50000000000000000, 66.65000000001198543, -115.3731074845243683 ) ) ;
#254950 = LINE ( 'NONE', #98461, #96723 ) ;
#254951 = CARTESIAN_POINT ( 'NONE',  ( 20.94999999999999929, 5.000000000011153745, -189.0947339810868755 ) ) ;
#254952 = LINE ( 'NONE', #213312, #242856 ) ;
#254953 = CARTESIAN_POINT ( 'NONE',  ( 20.94999999999999929, 74.98773774893902555, -233.8732236541320333 ) ) ;
#254954 = CARTESIAN_POINT ( 'NONE',  ( -16.89021194854739605, 66.05000000001200533, -115.7805393529200302 ) ) ;
#254955 = ORIENTED_EDGE ( 'NONE', *, *, #207240, .T. ) ;
#254956 = EDGE_LOOP ( 'NONE', ( #212667, #6443, #90625, #188864 ) ) ;
#254957 = EDGE_CURVE ( 'NONE', #114552, #197574, #177819, .T. ) ;
#254958 = DIRECTION ( 'NONE',  ( -1.000000000000000000, 0.000000000000000000, -0.000000000000000000 ) ) ;
#254959 = ORIENTED_EDGE ( 'NONE', *, *, #176133, .F. ) ;
#254960 = CARTESIAN_POINT ( 'NONE',  ( -23.25000000000000000, 4.350000000011156054, -179.8499999999999943 ) ) ;
#254961 = FACE_OUTER_BOUND ( 'NONE', #82097, .T. ) ;
#254962 = CARTESIAN_POINT ( 'NONE',  ( -20.64999999999999858, 74.00000000001199396, -116.2477294072864140 ) ) ;
#254963 = CIRCLE ( 'NONE', #109276, 0.09999999999999939493 ) ;
#254964 = CARTESIAN_POINT ( 'NONE',  ( 18.59999999999999787, 77.25000000001165290, -61.72262673010922640 ) ) ;
#254965 = ORIENTED_EDGE ( 'NONE', *, *, #245354, .T. ) ;
#254966 = EDGE_CURVE ( 'NONE', #95156, #157348, #202727, .T. ) ;
#254967 = DIRECTION ( 'NONE',  ( -1.000000000000000000, -0.000000000000000000, -0.000000000000000000 ) ) ;
#254968 = EDGE_LOOP ( 'NONE', ( #173621, #133961, #110037, #230564 ) ) ;
#254969 = DIRECTION ( 'NONE',  ( 1.000000000000000000, 0.000000000000000000, 0.000000000000000000 ) ) ;
#254970 = VERTEX_POINT ( 'NONE', #117571 ) ;
#254971 = EDGE_CURVE ( 'NONE', #245888, #224306, #211119, .T. ) ;
#254972 = CARTESIAN_POINT ( 'NONE',  ( -16.89208623190940273, 9.951577948986638944, -87.85527220321831976 ) ) ;
#254973 = LINE ( 'NONE', #197626, #29963 ) ;
#254974 = DIRECTION ( 'NONE',  ( 1.000000000000000000, 0.000000000000000000, 0.000000000000000000 ) ) ;
#254975 = ORIENTED_EDGE ( 'NONE', *, *, #41038, .F. ) ;
#254976 = AXIS2_PLACEMENT_3D ( 'NONE', #257742, #19190, #80404 ) ;
#254978 = ORIENTED_EDGE ( 'NONE', *, *, #216324, .T. ) ;
#254977 = DIRECTION ( 'NONE',  ( 0.000000000000000000, -1.000000000000000000, -6.982962677686265922E-15 ) ) ;
#254979 = CARTESIAN_POINT ( 'NONE',  ( -12.25000000000000178, 9.850000000011133849, -150.7500000000000284 ) ) ;
#254980 = EDGE_LOOP ( 'NONE', ( #153725, #38516, #105666, #241324 ) ) ;
#254981 = AXIS2_PLACEMENT_3D ( 'NONE', #236066, #233523, #114839 ) ;
#254982 = ORIENTED_EDGE ( 'NONE', *, *, #199825, .T. ) ;
#254983 = EDGE_CURVE ( 'NONE', #113968, #143581, #19586, .T. ) ;
#254984 = DIRECTION ( 'NONE',  ( -1.000000000000000000, 0.000000000000000000, 0.000000000000000000 ) ) ;
#254985 = ADVANCED_FACE ( 'NONE', ( #18475 ), #135834, .T. ) ;
#254986 = EDGE_LOOP ( 'NONE', ( #27634, #171396 ) ) ;
#254987 = DIRECTION ( 'NONE',  ( 0.000000000000000000, 0.1575844902526727098, 0.9875055080513754913 ) ) ;
#254988 = CARTESIAN_POINT ( 'NONE',  ( 21.05000000000000426, 69.69981666374535223, -69.57443491686539971 ) ) ;
#254989 = CARTESIAN_POINT ( 'NONE',  ( -20.64999999999999858, -8.999999999988846255, -43.39396912265245021 ) ) ;
#254990 = LINE ( 'NONE', #154709, #176726 ) ;
#254991 = EDGE_CURVE ( 'NONE', #109178, #4633, #58855, .T. ) ;
#254992 = CARTESIAN_POINT ( 'NONE',  ( -21.13498764882296044, 0.001656394742485162381, -60.50438185652610912 ) ) ;
#254993 = CIRCLE ( 'NONE', #167601, 0.09999999999999939493 ) ;
#254994 = ORIENTED_EDGE ( 'NONE', *, *, #103197, .T. ) ;
#254995 = VECTOR ( 'NONE', #101387, 1000.000000000000000 ) ;
#254996 = DIRECTION ( 'NONE',  ( 1.000000000000000000, -0.000000000000000000, -0.000000000000000000 ) ) ;
#254997 = CARTESIAN_POINT ( 'NONE',  ( -20.54999999999999716, 54.14029358995846053, -238.9803212882090691 ) ) ;
#254998 = CARTESIAN_POINT ( 'NONE',  ( -20.96077737575314970, 11.62390063401601381, -160.6407919571068135 ) ) ;
#254999 = ORIENTED_EDGE ( 'NONE', *, *, #246071, .T. ) ;
#255000 = DIRECTION ( 'NONE',  ( -1.000000000000000000, -0.000000000000000000, 0.000000000000000000 ) ) ;
#255001 = ORIENTED_EDGE ( 'NONE', *, *, #104662, .F. ) ;
#255002 = LINE ( 'NONE', #37327, #164759 ) ;
#255003 = ORIENTED_EDGE ( 'NONE', *, *, #116010, .T. ) ;
#255004 = EDGE_CURVE ( 'NONE', #156136, #139303, #181, .T. ) ;
#255005 = DIRECTION ( 'NONE',  ( 1.000000000000000000, 0.000000000000000000, 0.000000000000000000 ) ) ;
#255006 = CARTESIAN_POINT ( 'NONE',  ( -18.50000000000000000, 1.340746217944851715, -90.22713749457885513 ) ) ;
#255007 = AXIS2_PLACEMENT_3D ( 'NONE', #205946, #87264, #108137 ) ;
#255010 = VERTEX_POINT ( 'NONE', #79708 ) ;
#255009 = B_SPLINE_CURVE_WITH_KNOTS ( 'NONE', 3,
 ( #173534, #253006, #71827, #230907 ),
 .UNSPECIFIED., .F., .F.,
 ( 4, 4 ),
 ( 0.000000000000000000, 7.713889350930119414E-05 ),
 .UNSPECIFIED. ) ;
#255008 = DIRECTION ( 'NONE',  ( 0.000000000000000000, 1.000000000000000000, 7.272083257015735086E-15 ) ) ;
#255011 = CARTESIAN_POINT ( 'NONE',  ( -18.60000000000000142, 9.105964803472817337, -245.3658845043482586 ) ) ;
#255012 = ORIENTED_EDGE ( 'NONE', *, *, #205887, .T. ) ;
#255013 = CYLINDRICAL_SURFACE ( 'NONE', #173401, 0.09999999999999892308 ) ;
#255014 = VECTOR ( 'NONE', #153282, 1000.000000000000000 ) ;
#255015 = AXIS2_PLACEMENT_3D ( 'NONE', #153733, #136659, #214928 ) ;
#255016 = AXIS2_PLACEMENT_3D ( 'NONE', #52246, #191813, #129245 ) ;
#255017 = DIRECTION ( 'NONE',  ( 0.000000000000000000, 0.1350103645451876666, 0.9908441862701600211 ) ) ;
#255019 = EDGE_CURVE ( 'NONE', #200905, #192753, #11205, .T. ) ;
#255018 = EDGE_LOOP ( 'NONE', ( #128107, #17822, #214004, #219945 ) ) ;
#255020 = CIRCLE ( 'NONE', #188626, 0.1999999999999987899 ) ;
#255021 = DIRECTION ( 'NONE',  ( 1.000000000000000000, 0.000000000000000000, 0.000000000000000000 ) ) ;
#255022 = CARTESIAN_POINT ( 'NONE',  ( -21.05000000000000071, 11.75000000001115197, -194.1583993101029080 ) ) ;
#255023 = ORIENTED_EDGE ( 'NONE', *, *, #192145, .T. ) ;
#255024 = CARTESIAN_POINT ( 'NONE',  ( 21.05000000000000071, 10.12438351139595127, -228.1852649075067063 ) ) ;
#255025 = ORIENTED_EDGE ( 'NONE', *, *, #235471, .T. ) ;
#255026 = DIRECTION ( 'NONE',  ( -1.000000000000000000, -0.000000000000000000, -0.000000000000000000 ) ) ;
#255027 = LINE ( 'NONE', #230398, #209549 ) ;
#255029 = ORIENTED_EDGE ( 'NONE', *, *, #181825, .F. ) ;
#255028 = LINE ( 'NONE', #136400, #168112 ) ;
#255030 = DIRECTION ( 'NONE',  ( 1.000000000000000000, 0.000000000000000000, 0.000000000000000000 ) ) ;
#255031 = PLANE ( 'NONE',  #40095 ) ;
#255032 = CARTESIAN_POINT ( 'NONE',  ( -16.93521499325732549, 9.994786119803523050, -20.90710854109355310 ) ) ;
#255034 = CARTESIAN_POINT ( 'NONE',  ( -22.46246831459151494, 75.97808783307303315, -181.6729720457343262 ) ) ;
#255033 = CARTESIAN_POINT ( 'NONE',  ( -20.00857864376270001, 13.63658454968486389, -219.6758818217417968 ) ) ;
#255035 = CARTESIAN_POINT ( 'NONE',  ( -23.25000000000000355, 70.35000000001201670, -115.6731074845243370 ) ) ;
#255036 = DIRECTION ( 'NONE',  ( 0.000000000000000000, -0.1022405907414166287, -0.9947597004326451664 ) ) ;
#255037 = AXIS2_PLACEMENT_3D ( 'NONE', #250820, #134716, #192165 ) ;
#255038 = CARTESIAN_POINT ( 'NONE',  ( 18.50000000000000711, 85.41907808086091336, -29.19318213431596121 ) ) ;
#255039 = AXIS2_PLACEMENT_3D ( 'NONE', #36451, #152552, #232075 ) ;
#255040 = CARTESIAN_POINT ( 'NONE',  ( -21.70464131381649509, 68.90464198104429272, -136.5231074845243313 ) ) ;
#255041 = ORIENTED_EDGE ( 'NONE', *, *, #113490, .F. ) ;
#255042 = VERTEX_POINT ( 'NONE', #40650 ) ;
#255043 = ADVANCED_FACE ( 'NONE', ( #240098 ), #80993, .F. ) ;
#255044 = CARTESIAN_POINT ( 'NONE',  ( 18.46858270002953972, 85.47420267472293176, -162.9210855498204182 ) ) ;
#255045 = ADVANCED_FACE ( 'NONE', ( #141004 ), #219469, .F. ) ;
#255047 = ORIENTED_EDGE ( 'NONE', *, *, #128, .F. ) ;
#255046 = CARTESIAN_POINT ( 'NONE',  ( -18.38204789744325396, 33.92563192663926941, -235.0642528789780101 ) ) ;
#255048 = VERTEX_POINT ( 'NONE', #236232 ) ;
#255050 = DIRECTION ( 'NONE',  ( 0.000000000000000000, -0.8814952561688476074, 0.4721928772777262417 ) ) ;
#255049 = CIRCLE ( 'NONE', #38644, 0.09999999999999939493 ) ;
#255051 = ORIENTED_EDGE ( 'NONE', *, *, #6940, .F. ) ;
#255052 = CARTESIAN_POINT ( 'NONE',  ( 20.95224633520496127, 8.900522166557230719, -8.493276447921262573 ) ) ;
#255053 = ADVANCED_FACE ( 'NONE', ( #15937 ), #254483, .T. ) ;
#255054 = ADVANCED_FACE ( 'NONE', ( #198393 ), #38061, .F. ) ;
#255055 = CIRCLE ( 'NONE', #71978, 0.9000000000000014655 ) ;
#255056 = ORIENTED_EDGE ( 'NONE', *, *, #100263, .T. ) ;
#255057 = AXIS2_PLACEMENT_3D ( 'NONE', #95008, #155018, #118443 ) ;
#255058 = EDGE_CURVE ( 'NONE', #238460, #52704, #99273, .T. ) ;
#255059 = CIRCLE ( 'NONE', #38650, 11.64999999999999503 ) ;
#255060 = FACE_OUTER_BOUND ( 'NONE', #189162, .T. ) ;
#255061 = VECTOR ( 'NONE', #206053, 999.9999999999998863 ) ;
#255062 = B_SPLINE_CURVE_WITH_KNOTS ( 'NONE', 3,
 ( #245916, #162542, #4706, #33320, #112818, #111532, #51520, #73716, #93241, #52824 ),
 .UNSPECIFIED., .F., .F.,
 ( 4, 2, 2, 2, 4 ),
 ( 0.000000000000000000, 3.990160268014099847E-05, 7.980320536028199694E-05, 0.0001596064107204895363, 0.0003192128214409881257 ),
 .UNSPECIFIED. ) ;
#255063 = EDGE_CURVE ( 'NONE', #48580, #224075, #132666, .T. ) ;
#255065 = ORIENTED_EDGE ( 'NONE', *, *, #61792, .T. ) ;
#255064 = ORIENTED_EDGE ( 'NONE', *, *, #255216, .F. ) ;
#255066 = ORIENTED_EDGE ( 'NONE', *, *, #112755, .F. ) ;
#255069 = EDGE_CURVE ( 'NONE', #97864, #64945, #66019, .T. ) ;
#255068 = EDGE_CURVE ( 'NONE', #4905, #123588, #95242, .T. ) ;
#255067 = AXIS2_PLACEMENT_3D ( 'NONE', #118313, #257755, #221232 ) ;
#255070 = ORIENTED_EDGE ( 'NONE', *, *, #218716, .F. ) ;
#255072 = ORIENTED_EDGE ( 'NONE', *, *, #54134, .T. ) ;
#255071 = CIRCLE ( 'NONE', #30298, 0.1000000000000035305 ) ;
#255073 = DIRECTION ( 'NONE',  ( 0.000000000000000000, -1.000000000000000000, 0.000000000000000000 ) ) ;
#255074 = CARTESIAN_POINT ( 'NONE',  ( -20.64999999999999858, 63.53703427598990316, -222.1606900896233583 ) ) ;
#255076 = ORIENTED_EDGE ( 'NONE', *, *, #229538, .T. ) ;
#255075 = CARTESIAN_POINT ( 'NONE',  ( -21.55000000000000071, 7.350000000011155166, -155.1500000000000057 ) ) ;
#255077 = B_SPLINE_CURVE_WITH_KNOTS ( 'NONE', 3,
 ( #45180, #3478, #24360, #163856, #124730, #243377, #144256 ),
 .UNSPECIFIED., .F., .F.,
 ( 4, 3, 4 ),
 ( 5.692061405548898279E-19, 3.357501770814694990E-05, 5.199112466349232217E-05 ),
 .UNSPECIFIED. ) ;
#255078 = DIRECTION ( 'NONE',  ( 1.000000000000000000, -0.000000000000000000, -0.000000000000000000 ) ) ;
#255079 = LINE ( 'NONE', #179473, #82555 ) ;
#255081 = VERTEX_POINT ( 'NONE', #62742 ) ;
#255080 = CARTESIAN_POINT ( 'NONE',  ( -18.40000000000000213, 62.49259387941005173, -209.4439336506227960 ) ) ;
#255082 = CARTESIAN_POINT ( 'NONE',  ( -18.59999999999999787, 74.65925378207876406, -180.2959699899455472 ) ) ;
#255083 = ORIENTED_EDGE ( 'NONE', *, *, #196998, .T. ) ;
#255084 = CIRCLE ( 'NONE', #117771, 0.09999999999999939493 ) ;
#255086 = ORIENTED_EDGE ( 'NONE', *, *, #71200, .T. ) ;
#255085 = DIRECTION ( 'NONE',  ( -0.000000000000000000, 0.8164390028469706850, -0.5774316882803059992 ) ) ;
#255087 = VECTOR ( 'NONE', #153291, 1000.000000000000000 ) ;
#255088 = DIRECTION ( 'NONE',  ( 0.000000000000000000, 0.000000000000000000, -1.000000000000000000 ) ) ;
#255090 = EDGE_CURVE ( 'NONE', #75688, #176861, #32932, .T. ) ;
#255089 = DIRECTION ( 'NONE',  ( 1.301042606982683734E-14, 0.8660254037844367092, -0.5000000000000037748 ) ) ;
#255091 = DIRECTION ( 'NONE',  ( 1.000000000000000000, 0.000000000000000000, 0.000000000000000000 ) ) ;
#255092 = ORIENTED_EDGE ( 'NONE', *, *, #124898, .F. ) ;
#255093 = TOROIDAL_SURFACE ( 'NONE', #138588, 0.2000000000000000111, 0.1000000000000000056 ) ;
#255095 = LINE ( 'NONE', #156089, #53982 ) ;
#255094 = CARTESIAN_POINT ( 'NONE',  ( -20.64999999999999858, 74.00000000001205080, -123.2984855617622060 ) ) ;
#255096 = ADVANCED_FACE ( 'NONE', ( #7916 ), #185253, .T. ) ;
#255097 = ADVANCED_FACE ( 'NONE', ( #66596 ), #3644, .T. ) ;
#255098 = CARTESIAN_POINT ( 'NONE',  ( -20.94999999999999929, 69.15387683765879956, -32.28538121767450519 ) ) ;
#255099 = CARTESIAN_POINT ( 'NONE',  ( 18.49999999999998934, 19.00443933019177223, -232.7770257915295531 ) ) ;
#255100 = LINE ( 'NONE', #76508, #238442 ) ;
#255102 = VERTEX_POINT ( 'NONE', #23647 ) ;
#255101 = AXIS2_PLACEMENT_3D ( 'NONE', #165620, #31269, #149909 ) ;
#255103 = ORIENTED_EDGE ( 'NONE', *, *, #75590, .T. ) ;
#255104 = AXIS2_PLACEMENT_3D ( 'NONE', #152994, #173856, #158139 ) ;
#255105 = EDGE_CURVE ( 'NONE', #153574, #111618, #186104, .T. ) ;
#255106 = CARTESIAN_POINT ( 'NONE',  ( -21.07928932188134041, 0.09889514566555070163, -127.6714833436066954 ) ) ;
#255107 = PLANE ( 'NONE',  #185838 ) ;
#255108 = ORIENTED_EDGE ( 'NONE', *, *, #52420, .T. ) ;
#255109 = DIRECTION ( 'NONE',  ( -0.000000000000000000, -0.000000000000000000, 1.000000000000000000 ) ) ;
#255110 = EDGE_LOOP ( 'NONE', ( #120, #129977, #152269, #113058 ) ) ;
#255111 = DIRECTION ( 'NONE',  ( 0.000000000000000000, 6.853228547068871147E-15, -1.000000000000000000 ) ) ;
#255112 = FACE_OUTER_BOUND ( 'NONE', #219338, .T. ) ;
#255113 = EDGE_CURVE ( 'NONE', #221772, #88021, #182701, .T. ) ;
#255114 = ORIENTED_EDGE ( 'NONE', *, *, #67121, .F. ) ;
#255115 = DIRECTION ( 'NONE',  ( 0.000000000000000000, -7.086529944415893080E-15, 1.000000000000000000 ) ) ;
#255116 = AXIS2_PLACEMENT_3D ( 'NONE', #596, #21491, #180553 ) ;
#255117 = AXIS2_PLACEMENT_3D ( 'NONE', #186048, #8692, #188602 ) ;
#255118 = ORIENTED_EDGE ( 'NONE', *, *, #23992, .T. ) ;
#255120 = ORIENTED_EDGE ( 'NONE', *, *, #4097, .T. ) ;
#255119 = VECTOR ( 'NONE', #141664, 1000.000000000000114 ) ;
#255121 = ORIENTED_EDGE ( 'NONE', *, *, #19651, .F. ) ;
#255122 = LINE ( 'NONE', #212223, #108558 ) ;
#255123 = CARTESIAN_POINT ( 'NONE',  ( 12.47034474403012183, 66.62446189796352769, -53.65323160353356968 ) ) ;
#255124 = DIRECTION ( 'NONE',  ( 0.000000000000000000, -6.308085367188367561E-15, 1.000000000000000000 ) ) ;
#255125 = CARTESIAN_POINT ( 'NONE',  ( -18.50000000000000000, 64.25000000001237765, -169.9231074845244507 ) ) ;
#255126 = CARTESIAN_POINT ( 'NONE',  ( -22.59999999999999787, 25.98655542988603173, -254.2226763854395983 ) ) ;
#255128 = DIRECTION ( 'NONE',  ( 0.000000000000000000, -0.1350103645451876944, 0.9908441862701601321 ) ) ;
#255127 = CARTESIAN_POINT ( 'NONE',  ( 21.07928932188134397, 0.09889514566578838650, -161.1714833436012668 ) ) ;
#255130 = ORIENTED_EDGE ( 'NONE', *, *, #241672, .F. ) ;
#255129 = PLANE ( 'NONE',  #231487 ) ;
#255131 = CARTESIAN_POINT ( 'NONE',  ( -18.50000000000000000, 9.150000000011157653, -122.2500000000000284 ) ) ;
#255132 = VERTEX_POINT ( 'NONE', #181421 ) ;
#255133 = FACE_OUTER_BOUND ( 'NONE', #193227, .T. ) ;
#255134 = VERTEX_POINT ( 'NONE', #126564 ) ;
#255135 = ORIENTED_EDGE ( 'NONE', *, *, #104664, .T. ) ;
#255136 = FACE_OUTER_BOUND ( 'NONE', #199379, .T. ) ;
#255137 = CARTESIAN_POINT ( 'NONE',  ( -21.05000000000000071, 6.258842723548820430, -133.9679863068126338 ) ) ;
#255138 = CARTESIAN_POINT ( 'NONE',  ( -20.85000000000000142, 1.115600667400684642E-11, -134.0000000000000284 ) ) ;
#255139 = ORIENTED_EDGE ( 'NONE', *, *, #149451, .F. ) ;
#255140 = CARTESIAN_POINT ( 'NONE',  ( 21.05000000000000071, 28.51339163295720525, -258.4040038037771865 ) ) ;
#255141 = CIRCLE ( 'NONE', #163626, 0.1000000000000028644 ) ;
#255142 = CARTESIAN_POINT ( 'NONE',  ( 20.94999999999999929, 18.34743685832669158, -236.8753540304231535 ) ) ;
#255143 = ORIENTED_EDGE ( 'NONE', *, *, #183432, .T. ) ;
#255144 = ORIENTED_EDGE ( 'NONE', *, *, #47644, .F. ) ;
#255145 = CIRCLE ( 'NONE', #88590, 0.1000000000000024342 ) ;
#255146 = FACE_OUTER_BOUND ( 'NONE', #116914, .T. ) ;
#255147 = ORIENTED_EDGE ( 'NONE', *, *, #112142, .T. ) ;
#255148 = CARTESIAN_POINT ( 'NONE',  ( -16.93658211146646408, 60.88257505944956449, -221.0825842276667856 ) ) ;
#255149 = ORIENTED_EDGE ( 'NONE', *, *, #31450, .F. ) ;
#255150 = SPHERICAL_SURFACE ( 'NONE', #103031, 0.1000000000000000056 ) ;
#255151 = CARTESIAN_POINT ( 'NONE',  ( -16.87683809663752754, 9.864913447291343118, -120.7242815513040455 ) ) ;
#255152 = CARTESIAN_POINT ( 'NONE',  ( 21.04116576186320486, 65.37533692126093854, -157.6945257158966740 ) ) ;
#255153 = ORIENTED_EDGE ( 'NONE', *, *, #226283, .F. ) ;
#255154 = DIRECTION ( 'NONE',  ( 0.000000000000000000, 0.8103668758649577031, -0.5859227990963212784 ) ) ;
#255155 = EDGE_CURVE ( 'NONE', #96147, #183416, #242645, .T. ) ;
#255156 = CARTESIAN_POINT ( 'NONE',  ( -22.43310005002225438, 26.02505119112246490, -254.3088301514316925 ) ) ;
#255157 = ADVANCED_FACE ( 'NONE', ( #223083 ), #57802, .F. ) ;
#255159 = VERTEX_POINT ( 'NONE', #84828 ) ;
#255158 = CIRCLE ( 'NONE', #63672, 0.09999999999999939493 ) ;
#255160 = ADVANCED_FACE ( 'NONE', ( #46998 ), #164412, .F. ) ;
#255161 = DIRECTION ( 'NONE',  ( 1.000000000000000000, -0.000000000000000000, 0.000000000000000000 ) ) ;
#255162 = EDGE_CURVE ( 'NONE', #55595, #201052, #103590, .T. ) ;
#255163 = VERTEX_POINT ( 'NONE', #105682 ) ;
#255164 = CARTESIAN_POINT ( 'NONE',  ( 20.95512820512820440, 67.12384868372393498, -124.3731074845243683 ) ) ;
#255165 = CARTESIAN_POINT ( 'NONE',  ( 20.94999999999999929, 76.00000000001216449, -139.4231074845243654 ) ) ;
#255166 = LINE ( 'NONE', #38756, #171381 ) ;
#255167 = CARTESIAN_POINT ( 'NONE',  ( 23.15000000000000213, 87.48912529308798014, -106.1231074845242262 ) ) ;
#255168 = CARTESIAN_POINT ( 'NONE',  ( -16.86445178670636835, 9.962211629127192936, -46.10922256188256085 ) ) ;
#255169 = CARTESIAN_POINT ( 'NONE',  ( 23.15000000000000213, 87.65000000001192859, -106.1231074845242262 ) ) ;
#255170 = ORIENTED_EDGE ( 'NONE', *, *, #204520, .T. ) ;
#255171 = CARTESIAN_POINT ( 'NONE',  ( -16.93970660449832621, 65.98715860837648961, -123.9708257487299079 ) ) ;
#255172 = DIRECTION ( 'NONE',  ( 1.000000000000000000, 0.000000000000000000, 0.000000000000000000 ) ) ;
#255173 = CARTESIAN_POINT ( 'NONE',  ( -21.65000000000000213, 66.05000000001207638, -123.7731074845243739 ) ) ;
#255174 = DIRECTION ( 'NONE',  ( -0.000000000000000000, -1.000000000000000000, -0.000000000000000000 ) ) ;
#255175 = CIRCLE ( 'NONE', #171892, 0.4000000000000114575 ) ;
#255177 = DIRECTION ( 'NONE',  ( 0.000000000000000000, 0.000000000000000000, -1.000000000000000000 ) ) ;
#255176 = AXIS2_PLACEMENT_3D ( 'NONE', #211069, #92389, #171982 ) ;
#255178 = EDGE_CURVE ( 'NONE', #17643, #92561, #178473, .T. ) ;
#255179 = ADVANCED_FACE ( 'NONE', ( #146117 ), #170306, .T. ) ;
#255180 = VERTEX_POINT ( 'NONE', #161862 ) ;
#255181 = VERTEX_POINT ( 'NONE', #246502 ) ;
#255182 = CARTESIAN_POINT ( 'NONE',  ( 23.24999999999999645, 40.29670989715187090, -235.0462836312595130 ) ) ;
#255184 = CARTESIAN_POINT ( 'NONE',  ( -18.59999999999999787, 12.87592094156238609, -205.3750039893633073 ) ) ;
#255183 = AXIS2_PLACEMENT_3D ( 'NONE', #106353, #175073, #254527 ) ;
#255185 = CARTESIAN_POINT ( 'NONE',  ( 18.59999999999999432, -9.480686695278969012, -40.44111516875785384 ) ) ;
#255186 = LINE ( 'NONE', #58306, #134709 ) ;
#255187 = DIRECTION ( 'NONE',  ( 0.000000000000000000, 0.000000000000000000, 1.000000000000000000 ) ) ;
#255188 = ORIENTED_EDGE ( 'NONE', *, *, #163016, .T. ) ;
#255189 = FACE_OUTER_BOUND ( 'NONE', #33795, .T. ) ;
#255190 = CONTEXT_DEPENDENT_SHAPE_REPRESENTATION ( #19241, #176591 ) ;
#255191 = B_SPLINE_CURVE_WITH_KNOTS ( 'NONE', 3,
 ( #153428, #171695, #75159, #252463, #73882, #33478, #112977 ),
 .UNSPECIFIED., .F., .F.,
 ( 4, 3, 4 ),
 ( 0.000000000000000000, 3.357501770812408679E-05, 5.199112466348557301E-05 ),
 .UNSPECIFIED. ) ;
#255192 = CARTESIAN_POINT ( 'NONE',  ( 23.24999999999999289, 69.35000000001151932, -48.17310748452437252 ) ) ;
#255193 = CIRCLE ( 'NONE', #84518, 0.1000000000000124678 ) ;
#255194 = ORIENTED_EDGE ( 'NONE', *, *, #156226, .T. ) ;
#255195 = CIRCLE ( 'NONE', #1161, 0.09999999999999609201 ) ;
#255196 = DIRECTION ( 'NONE',  ( 0.000000000000000000, -0.9126074666063771490, -0.4088369013363281623 ) ) ;
#255197 = EDGE_CURVE ( 'NONE', #237745, #224664, #20240, .T. ) ;
#255198 = FACE_OUTER_BOUND ( 'NONE', #229496, .T. ) ;
#255199 = EDGE_CURVE ( 'NONE', #148199, #126474, #11777, .T. ) ;
#255200 = ORIENTED_EDGE ( 'NONE', *, *, #190138, .T. ) ;
#255201 = CARTESIAN_POINT ( 'NONE',  ( 23.24999999999999289, 6.650000000011155876, -179.8499999999999943 ) ) ;
#255202 = AXIS2_PLACEMENT_3D ( 'NONE', #205756, #246181, #46673 ) ;
#255203 = EDGE_LOOP ( 'NONE', ( #241632, #42689, #196324, #219118 ) ) ;
#255204 = CARTESIAN_POINT ( 'NONE',  ( 20.94999999999999574, 2.859758780633683273, -208.6670499591424459 ) ) ;
#255205 = DIRECTION ( 'NONE',  ( 0.000000000000000000, -1.000000000000000000, -0.000000000000000000 ) ) ;
#255206 = DIRECTION ( 'NONE',  ( 1.000000000000000000, 0.000000000000000000, 0.000000000000000000 ) ) ;
#255207 = EDGE_CURVE ( 'NONE', #5675, #157096, #220147, .T. ) ;
#255208 = CARTESIAN_POINT ( 'NONE',  ( 21.12642695952774474, 75.90109671682306214, -176.3987674065595286 ) ) ;
#255210 = AXIS2_PLACEMENT_3D ( 'NONE', #95528, #116392, #235053 ) ;
#255209 = CARTESIAN_POINT ( 'NONE',  ( -21.05000000000000071, 87.65000000001163016, -66.62310748452424036 ) ) ;
#255211 = CARTESIAN_POINT ( 'NONE',  ( -21.05000000000000071, 11.75000000001115552, -193.9851942293460070 ) ) ;
#255213 = CARTESIAN_POINT ( 'NONE',  ( 21.00000000000000000, 9.750000000011153745, -88.15000000000004832 ) ) ;
#255212 = AXIS2_PLACEMENT_3D ( 'NONE', #196331, #195082, #35999 ) ;
#255214 = AXIS2_PLACEMENT_3D ( 'NONE', #255547, #174836, #75699 ) ;
#255215 = CYLINDRICAL_SURFACE ( 'NONE', #93354, 0.1000000000000028644 ) ;
#255216 = EDGE_CURVE ( 'NONE', #126709, #163726, #112010, .T. ) ;
#255218 = DIRECTION ( 'NONE',  ( 1.000000000000000000, 0.000000000000000000, -0.000000000000000000 ) ) ;
#255217 = AXIS2_PLACEMENT_3D ( 'NONE', #126200, #205738, #246162 ) ;
#255219 = DIRECTION ( 'NONE',  ( 0.000000000000000000, 0.000000000000000000, 1.000000000000000000 ) ) ;
#255220 = CARTESIAN_POINT ( 'NONE',  ( 21.13461538461538680, 22.21093039075207543, -231.7318303787630214 ) ) ;
#255221 = CARTESIAN_POINT ( 'NONE',  ( -16.87331047859649757, 30.20632856012693424, -234.8070450048000737 ) ) ;
#255222 = DIRECTION ( 'NONE',  ( 0.000000000000000000, 0.4088369013363279403, -0.9126074666063771490 ) ) ;
#255223 = ADVANCED_FACE ( 'NONE', ( #48305 ), #136937, .T. ) ;
#255224 = EDGE_LOOP ( 'NONE', ( #171031, #173232, #128938, #78409, #147227, #223690 ) ) ;
#255225 = DIRECTION ( 'NONE',  ( -6.938893903907222856E-15, -0.4088369013363280513, 0.9126074666063769270 ) ) ;
#255226 = CARTESIAN_POINT ( 'NONE',  ( -23.15000000000000213, 11.75000000001115552, -97.40000000000004832 ) ) ;
#255227 = ORIENTED_EDGE ( 'NONE', *, *, #182508, .T. ) ;
#255228 = CYLINDRICAL_SURFACE ( 'NONE', #18821, 0.1000000000000098310 ) ;
#255229 = DIRECTION ( 'NONE',  ( 0.000000000000000000, 0.8814952561688428334, -0.4721928772777350125 ) ) ;
#255230 = DIRECTION ( 'NONE',  ( -1.000000000000000000, -0.000000000000000000, 0.000000000000000000 ) ) ;
#255231 = EDGE_CURVE ( 'NONE', #116714, #253651, #195228, .T. ) ;
#255232 = VERTEX_POINT ( 'NONE', #247789 ) ;
#255233 = CARTESIAN_POINT ( 'NONE',  ( 21.04552871983375795, 6.223900101736508539, 12.00000000000000178 ) ) ;
#255234 = DIRECTION ( 'NONE',  ( 0.000000000000000000, 0.000000000000000000, -1.000000000000000000 ) ) ;
#255235 = ADVANCED_FACE ( 'NONE', ( #112157 ), #66200, .T. ) ;
#255236 = ORIENTED_EDGE ( 'NONE', *, *, #139976, .T. ) ;
#255237 = CARTESIAN_POINT ( 'NONE',  ( -21.06715728752538652, 38.25685495413522119, -235.9601135138701409 ) ) ;
#255238 = CYLINDRICAL_SURFACE ( 'NONE', #134926, 0.09999999999999063804 ) ;
#255239 = VECTOR ( 'NONE', #26506, 1000.000000000000114 ) ;
#255240 = EDGE_LOOP ( 'NONE', ( #84143, #204762, #75512, #153420, #1780, #173539 ) ) ;
#255242 = CYLINDRICAL_SURFACE ( 'NONE', #106117, 11.80000000000000426 ) ;
#255241 = TOROIDAL_SURFACE ( 'NONE', #92990, 0.2000000000000000111, 0.1000000000000000056 ) ;
#255243 = EDGE_CURVE ( 'NONE', #254308, #218145, #91143, .T. ) ;
#255244 = TOROIDAL_SURFACE ( 'NONE', #55347, 2.100000000000002309, 0.1000000000000000056 ) ;
#255245 = ORIENTED_EDGE ( 'NONE', *, *, #138172, .F. ) ;
#255246 = CARTESIAN_POINT ( 'NONE',  ( -21.05000000000000071, 36.65892442174935439, -249.5511627012433848 ) ) ;
#255247 = DIRECTION ( 'NONE',  ( 1.000000000000000000, 0.000000000000000000, 0.000000000000000000 ) ) ;
#255249 = AXIS2_PLACEMENT_3D ( 'NONE', #113476, #32709, #193032 ) ;
#255248 = CARTESIAN_POINT ( 'NONE',  ( -21.05000000000000071, 79.13126459505528487, -235.8705213229730191 ) ) ;
#255250 = DIRECTION ( 'NONE',  ( 2.952720810173289112E-16, -1.000000000000000000, 0.000000000000000000 ) ) ;
#255251 = LINE ( 'NONE', #237033, #34946 ) ;
#255252 = CARTESIAN_POINT ( 'NONE',  ( -13.88555196119802915, 46.48141361689234685, -234.7877205119061728 ) ) ;
#255253 = AXIS2_PLACEMENT_3D ( 'NONE', #20318, #99801, #239350 ) ;
#255254 = DIRECTION ( 'NONE',  ( 0.000000000000000000, 0.000000000000000000, 1.000000000000000000 ) ) ;
#255256 = DIRECTION ( 'NONE',  ( 0.000000000000000000, 0.000000000000000000, 1.000000000000000000 ) ) ;
#255255 = CIRCLE ( 'NONE', #167857, 0.1000000000000028644 ) ;
#255258 = ORIENTED_EDGE ( 'NONE', *, *, #63486, .F. ) ;
#255257 = CARTESIAN_POINT ( 'NONE',  ( -18.46856557590792747, -9.474215907775342060, -40.60198624088229735 ) ) ;
#255259 = VERTEX_POINT ( 'NONE', #189106 ) ;
#255261 = CARTESIAN_POINT ( 'NONE',  ( 21.97500000000000497, 66.25000000001253397, -182.2731074845244450 ) ) ;
#255260 = DIRECTION ( 'NONE',  ( 0.000000000000000000, 0.000000000000000000, -1.000000000000000000 ) ) ;
#255263 = EDGE_LOOP ( 'NONE', ( #50761, #222330, #173172, #192891 ) ) ;
#255262 = DIRECTION ( 'NONE',  ( 0.000000000000000000, 6.982962677686266711E-15, -1.000000000000000000 ) ) ;
#255264 = ORIENTED_EDGE ( 'NONE', *, *, #24392, .T. ) ;
#255265 = CARTESIAN_POINT ( 'NONE',  ( -16.94389599337535657, 66.00880201025550775, -149.1307522863228314 ) ) ;
#255266 = DIRECTION ( 'NONE',  ( -1.000000000000000000, 0.000000000000000000, 0.000000000000000000 ) ) ;
#255267 = TOROIDAL_SURFACE ( 'NONE', #192795, 0.2000000000000000111, 0.1000000000000000056 ) ;
#255268 = CARTESIAN_POINT ( 'NONE',  ( -20.00857864376270001, 66.65000000001187175, -90.67310748452437963 ) ) ;
#255269 = CARTESIAN_POINT ( 'NONE',  ( 21.15000000000005187, 76.00000000001119815, -40.07310748452479032 ) ) ;
#255270 = CARTESIAN_POINT ( 'NONE',  ( -23.25000000000000355, 64.25000000001199396, -112.2731074845243739 ) ) ;
#255271 = CARTESIAN_POINT ( 'NONE',  ( -16.27683809663751191, 9.350000000011132073, -180.0499999999999545 ) ) ;
#255272 = CARTESIAN_POINT ( 'NONE',  ( -23.25000000000000000, 76.00000000001190870, -103.0231074845243029 ) ) ;
#255273 = TOROIDAL_SURFACE ( 'NONE', #250653, 0.2000000000000000111, 0.1000000000000000056 ) ;
#255274 = DIRECTION ( 'NONE',  ( 0.000000000000000000, -0.6728388485993083146, 0.7397890806274158848 ) ) ;
#255275 = CIRCLE ( 'NONE', #42960, 0.1999999999999987899 ) ;
#255276 = VERTEX_POINT ( 'NONE', #172151 ) ;
#255277 = ORIENTED_EDGE ( 'NONE', *, *, #141336, .F. ) ;
#255278 = PLANE ( 'NONE',  #222804 ) ;
#255279 = ORIENTED_EDGE ( 'NONE', *, *, #26610, .T. ) ;
#255280 = CARTESIAN_POINT ( 'NONE',  ( -23.25000000000000000, 68.29137419664525055, -231.9463301769586394 ) ) ;
#255281 = VERTEX_POINT ( 'NONE', #229523 ) ;
#255283 = TOROIDAL_SURFACE ( 'NONE', #234484, 0.2000000000000000111, 0.1000000000000000056 ) ;
#255282 = CARTESIAN_POINT ( 'NONE',  ( -16.81744102076748959, 14.15900158805613884, -219.2550725561364118 ) ) ;
#255284 = TOROIDAL_SURFACE ( 'NONE', #68082, 4.149999999999999467, 0.1000000000000000056 ) ;
#255285 = CIRCLE ( 'NONE', #113883, 0.1000000000000124678 ) ;
#255286 = TOROIDAL_SURFACE ( 'NONE', #197066, 11.70000000000000639, 0.1000000000000000056 ) ;
#255287 = FACE_OUTER_BOUND ( 'NONE', #11987, .T. ) ;
#255288 = LINE ( 'NONE', #114555, #135135 ) ;
#255289 = EDGE_CURVE ( 'NONE', #240937, #90768, #236885, .T. ) ;
#255291 = ORIENTED_EDGE ( 'NONE', *, *, #254579, .T. ) ;
#255290 = CARTESIAN_POINT ( 'NONE',  ( -22.24259225415828567, 7.491937870576586889, -33.40093411654716959 ) ) ;
#255292 = CARTESIAN_POINT ( 'NONE',  ( 18.59999999999997655, -1.164121893230052995, -175.4148480855716059 ) ) ;
#255293 = ORIENTED_EDGE ( 'NONE', *, *, #23010, .F. ) ;
#255294 = ADVANCED_FACE ( 'NONE', ( #70481 ), #131696, .T. ) ;
#255295 = DIRECTION ( 'NONE',  ( -0.000000000000000000, -6.982962677686266711E-15, 1.000000000000000000 ) ) ;
#255296 = ADVANCED_FACE ( 'NONE', ( #93847 ), #110844, .F. ) ;
#255297 = CARTESIAN_POINT ( 'NONE',  ( -21.04999999999999716, 76.08574093704510233, -75.93693377333728733 ) ) ;
#255298 = DIRECTION ( 'NONE',  ( -0.000000000000000000, -0.1335171055202867274, -0.9910465087640865089 ) ) ;
#255299 = DIRECTION ( 'NONE',  ( 0.000000000000000000, 7.056502275159890043E-15, -1.000000000000000000 ) ) ;
#255300 = EDGE_LOOP ( 'NONE', ( #65636, #229484, #72707, #121981 ) ) ;
#255301 = LINE ( 'NONE', #55841, #219139 ) ;
#255302 = AXIS2_PLACEMENT_3D ( 'NONE', #133501, #98186, #197313 ) ;
#255303 = VERTEX_POINT ( 'NONE', #53446 ) ;
#255306 = VERTEX_POINT ( 'NONE', #73046 ) ;
#255305 = DIRECTION ( 'NONE',  ( -1.000000000000000000, -0.000000000000000000, -0.000000000000000000 ) ) ;
#255304 = CARTESIAN_POINT ( 'NONE',  ( 21.87500000000000355, 66.25000000001205080, -124.1731074845243654 ) ) ;
#255307 = VECTOR ( 'NONE', #166509, 1000.000000000000000 ) ;
#255308 = AXIS2_PLACEMENT_3D ( 'NONE', #58106, #235469, #252464 ) ;
#255309 = CARTESIAN_POINT ( 'NONE',  ( 18.59999999999999076, 66.34920340998563404, -213.7018660128499334 ) ) ;
#255310 = VECTOR ( 'NONE', #196710, 1000.000000000000000 ) ;
#255311 = CARTESIAN_POINT ( 'NONE',  ( -22.60000000000080789, -2.453694707889708226, -189.5089297331973626 ) ) ;
#255312 = ORIENTED_EDGE ( 'NONE', *, *, #229902, .F. ) ;
#255313 = DIRECTION ( 'NONE',  ( -0.000000000000000000, 0.1575546449569960317, 0.9875102702516440623 ) ) ;
#255314 = EDGE_CURVE ( 'NONE', #39881, #159476, #49455, .T. ) ;
#255315 = CYLINDRICAL_SURFACE ( 'NONE', #257035, 0.09999999999999520384 ) ;
#255316 = CYLINDRICAL_SURFACE ( 'NONE', #51085, 0.1000000000000028644 ) ;
#255317 = UNCERTAINTY_MEASURE_WITH_UNIT (LENGTH_MEASURE( 1.000000000000000082E-05 ), #124534, 'distance_accuracy_value', 'NONE');
#255319 = ORIENTED_EDGE ( 'NONE', *, *, #207088, .T. ) ;
#255318 = DIRECTION ( 'NONE',  ( 1.000000000000000000, -7.667232114526941871E-17, 1.711482807214921537E-16 ) ) ;
#255320 = CARTESIAN_POINT ( 'NONE',  ( -20.54999999999999716, 74.05981308412442843, -157.1939882734710352 ) ) ;
#255321 = ORIENTED_EDGE ( 'NONE', *, *, #44655, .F. ) ;
#255322 = CYLINDRICAL_SURFACE ( 'NONE', #166113, 0.09999999999999939493 ) ;
#255323 = CARTESIAN_POINT ( 'NONE',  ( 18.45036689428334853, -9.490184143317749843, -74.01269582748609821 ) ) ;
#255324 = DIRECTION ( 'NONE',  ( -0.000000000000000000, 1.000000000000000000, -0.000000000000000000 ) ) ;
#255325 = VERTEX_POINT ( 'NONE', #212537 ) ;
#255326 = CARTESIAN_POINT ( 'NONE',  ( -23.49999999999994316, 74.94272479589878344, -3.023107484524792277 ) ) ;
#255327 = ORIENTED_EDGE ( 'NONE', *, *, #146606, .T. ) ;
#255328 = LINE ( 'NONE', #151166, #6157 ) ;
#255329 = AXIS2_PLACEMENT_3D ( 'NONE', #246945, #87856, #108732 ) ;
#255330 = EDGE_CURVE ( 'NONE', #16439, #152113, #127857, .T. ) ;
#255331 = FACE_OUTER_BOUND ( 'NONE', #223033, .T. ) ;
#255332 = CARTESIAN_POINT ( 'NONE',  ( 22.39999999999999503, 31.80471377451587500, -238.9601694054147742 ) ) ;
#255333 = EDGE_CURVE ( 'NONE', #245440, #41988, #12063, .T. ) ;
#255334 = ORIENTED_EDGE ( 'NONE', *, *, #186698, .F. ) ;
#255335 = CARTESIAN_POINT ( 'NONE',  ( 21.05563370358598263, 22.93207528815513641, -230.0321118342242244 ) ) ;
#255336 = CARTESIAN_POINT ( 'NONE',  ( -19.89999999999999858, 4.513204987021263825, 22.10000000000000142 ) ) ;
#255338 = EDGE_CURVE ( 'NONE', #64966, #109860, #257671, .T. ) ;
#255337 = ORIENTED_EDGE ( 'NONE', *, *, #76449, .T. ) ;
#255339 = DIRECTION ( 'NONE',  ( 1.000000000000000000, 0.000000000000000000, 0.000000000000000000 ) ) ;
#255341 = CARTESIAN_POINT ( 'NONE',  ( 13.40000000000000036, -8.250000000000003553, 15.00000000000000355 ) ) ;
#255340 = AXIS2_PLACEMENT_3D ( 'NONE', #36318, #237067, #53300 ) ;
#255342 = CIRCLE ( 'NONE', #80393, 0.3999999999999975797 ) ;
#255343 = EDGE_LOOP ( 'NONE', ( #237785, #171662, #54927, #53069 ) ) ;
#255344 = CYLINDRICAL_SURFACE ( 'NONE', #79124, 0.09999999999999939493 ) ;
#255345 = ORIENTED_EDGE ( 'NONE', *, *, #28911, .T. ) ;
#255347 = ORIENTED_EDGE ( 'NONE', *, *, #78419, .T. ) ;
#255346 = DIRECTION ( 'NONE',  ( 0.000000000000000000, 0.8660254037844281605, -0.5000000000000185407 ) ) ;
#255351 = ADVANCED_FACE ( 'NONE', ( #169590 ), #69182, .F. ) ;
#255350 = ORIENTED_EDGE ( 'NONE', *, *, #40377, .F. ) ;
#255349 = ORIENTED_EDGE ( 'NONE', *, *, #14867, .F. ) ;
#255348 = CARTESIAN_POINT ( 'NONE',  ( -21.55000000000000426, 12.03275902784684703, -220.0251779199349187 ) ) ;
#255352 = DIRECTION ( 'NONE',  ( 0.000000000000000000, 0.000000000000000000, 1.000000000000000000 ) ) ;
#255353 = CARTESIAN_POINT ( 'NONE',  ( -21.08035267497491816, 0.08268862478717949049, -161.1682931602169049 ) ) ;
#255354 = CARTESIAN_POINT ( 'NONE',  ( 23.24999999999999645, 73.90000000001214175, -136.5231074845243882 ) ) ;
#255355 = AXIS2_PLACEMENT_3D ( 'NONE', #195028, #59308, #158481 ) ;
#255356 = DIRECTION ( 'NONE',  ( -1.000000000000000000, -0.000000000000000000, -0.000000000000000000 ) ) ;
#255357 = CARTESIAN_POINT ( 'NONE',  ( 18.59999999999999432, 4.158309866074138661, -211.9342015984041439 ) ) ;
#255358 = LINE ( 'NONE', #156353, #184772 ) ;
#255359 = TOROIDAL_SURFACE ( 'NONE', #201243, 7.800000000000000711, 0.1000000000000000056 ) ;
#255360 = LINE ( 'NONE', #52065, #218062 ) ;
#255361 = ORIENTED_EDGE ( 'NONE', *, *, #75920, .T. ) ;
#255362 = ORIENTED_EDGE ( 'NONE', *, *, #183752, .F. ) ;
#255363 = VERTEX_POINT ( 'NONE', #76848 ) ;
#255364 = AXIS2_PLACEMENT_3D ( 'NONE', #160173, #218815, #121049 ) ;
#255365 = EDGE_CURVE ( 'NONE', #236786, #89147, #198083, .T. ) ;
#255366 = CARTESIAN_POINT ( 'NONE',  ( 23.14999999999999858, 70.50000000001185185, -90.61784146561124942 ) ) ;
#255368 = ORIENTED_EDGE ( 'NONE', *, *, #192204, .T. ) ;
#255367 = CARTESIAN_POINT ( 'NONE',  ( -21.45000000000000284, 7.708578643773852157, -45.75000000000000000 ) ) ;
#255369 = CARTESIAN_POINT ( 'NONE',  ( 18.39999999999997371, 11.74999999999998224, -9.250000000000001776 ) ) ;
#255370 = ORIENTED_EDGE ( 'NONE', *, *, #27667, .F. ) ;
#255371 = CARTESIAN_POINT ( 'NONE',  ( -18.59999999999999787, 9.350000000011156942, -79.35000000000005116 ) ) ;
#255372 = ORIENTED_EDGE ( 'NONE', *, *, #35662, .T. ) ;
#255373 = EDGE_CURVE ( 'NONE', #1139, #172722, #199395, .T. ) ;
#255374 = EDGE_CURVE ( 'NONE', #1409, #192117, #256725, .T. ) ;
#255375 = CIRCLE ( 'NONE', #113956, 0.09999999999999939493 ) ;
#255376 = CIRCLE ( 'NONE', #113782, 0.1000000000000028644 ) ;
#255377 = ORIENTED_EDGE ( 'NONE', *, *, #11392, .F. ) ;
#255378 = CIRCLE ( 'NONE', #76350, 0.6000000000000033085 ) ;
#255379 = DIRECTION ( 'NONE',  ( 0.000000000000000000, -1.000000000000000000, 0.000000000000000000 ) ) ;
#255380 = CARTESIAN_POINT ( 'NONE',  ( 23.15000000000000213, -11.64999999998883595, -164.4000000000000057 ) ) ;
#255381 = EDGE_CURVE ( 'NONE', #102074, #176779, #53555, .T. ) ;
#255383 = ORIENTED_EDGE ( 'NONE', *, *, #112755, .T. ) ;
#255382 = ORIENTED_EDGE ( 'NONE', *, *, #242512, .T. ) ;
#255384 = VERTEX_POINT ( 'NONE', #20755 ) ;
#255386 = EDGE_CURVE ( 'NONE', #113546, #16833, #153556, .T. ) ;
#255385 = CARTESIAN_POINT ( 'NONE',  ( 19.75857864376268935, 11.65000000000000391, -24.75000000000000000 ) ) ;
#255387 = ORIENTED_EDGE ( 'NONE', *, *, #70619, .F. ) ;
#255388 = ORIENTED_EDGE ( 'NONE', *, *, #141163, .T. ) ;
#255390 = DIRECTION ( 'NONE',  ( -0.000000000000000000, -0.1298341882519737922, -0.9915357197604890427 ) ) ;
#255389 = VECTOR ( 'NONE', #224990, 1000.000000000000000 ) ;
#255392 = ORIENTED_EDGE ( 'NONE', *, *, #202062, .F. ) ;
#255391 = DIRECTION ( 'NONE',  ( 0.000000000000000000, -0.1480365673253065117, 0.9889818879709273425 ) ) ;
#255393 = ADVANCED_FACE ( 'NONE', ( #1146 ), #156434, .F. ) ;
#255394 = DIRECTION ( 'NONE',  ( 0.000000000000000000, 0.2128009952263601179, -0.9770955615653315052 ) ) ;
#255395 = FACE_OUTER_BOUND ( 'NONE', #6452, .T. ) ;
#255396 = CARTESIAN_POINT ( 'NONE',  ( -22.57848426163147693, 76.00426432929585019, -215.2731657914146410 ) ) ;
#255397 = DIRECTION ( 'NONE',  ( -1.000000000000000000, 0.000000000000000000, 0.000000000000000000 ) ) ;
#255398 = ORIENTED_EDGE ( 'NONE', *, *, #153479, .T. ) ;
#255399 = VECTOR ( 'NONE', #186642, 1000.000000000000227 ) ;
#255400 = CIRCLE ( 'NONE', #142997, 0.1000000000000028644 ) ;
#255401 = VECTOR ( 'NONE', #74796, 1000.000000000000000 ) ;
#255402 = ORIENTED_EDGE ( 'NONE', *, *, #130205, .T. ) ;
#255403 = CIRCLE ( 'NONE', #176369, 0.09999999999999892308 ) ;
#255404 = CARTESIAN_POINT ( 'NONE',  ( -20.85000000000000142, 68.97833521811233481, -166.3895420826271163 ) ) ;
#255406 = EDGE_CURVE ( 'NONE', #100484, #15467, #19459, .T. ) ;
#255405 = CARTESIAN_POINT ( 'NONE',  ( 21.05000000000000071, 70.15000000001221281, -146.6556047088023149 ) ) ;
#255407 = EDGE_LOOP ( 'NONE', ( #177902, #2835, #200656, #180725 ) ) ;
#255408 = CYLINDRICAL_SURFACE ( 'NONE', #77782, 4.000000000000000000 ) ;
#255409 = EDGE_CURVE ( 'NONE', #217454, #99384, #237222, .T. ) ;
#255410 = ADVANCED_FACE ( 'NONE', ( #213800 ), #255440, .T. ) ;
#255411 = CARTESIAN_POINT ( 'NONE',  ( 18.59999999999999076, -1.835859311432481045, -78.60443916879853532 ) ) ;
#255412 = DIRECTION ( 'NONE',  ( 0.000000000000000000, 0.000000000000000000, -1.000000000000000000 ) ) ;
#255413 = ORIENTED_EDGE ( 'NONE', *, *, #240014, .T. ) ;
#255414 = ORIENTED_EDGE ( 'NONE', *, *, #104047, .T. ) ;
#255415 = ADVANCED_FACE ( 'NONE', ( #177275 ), #184312, .T. ) ;
#255416 = DIRECTION ( 'NONE',  ( 0.000000000000000000, 0.000000000000000000, -1.000000000000000000 ) ) ;
#255417 = CARTESIAN_POINT ( 'NONE',  ( 23.14999999999999503, 6.650000000011155876, -54.75000000000000000 ) ) ;
#255418 = ORIENTED_EDGE ( 'NONE', *, *, #39115, .T. ) ;
#255419 = CARTESIAN_POINT ( 'NONE',  ( 18.49999999999999289, 67.85909929089923764, -227.8797997985275856 ) ) ;
#255420 = ORIENTED_EDGE ( 'NONE', *, *, #209295, .T. ) ;
#255421 = CARTESIAN_POINT ( 'NONE',  ( 22.39999999999999503, 11.75000000001116263, -133.9000000000000057 ) ) ;
#255422 = DIRECTION ( 'NONE',  ( 0.000000000000000000, -1.000000000000000000, -1.897661533703519897E-16 ) ) ;
#255424 = DIRECTION ( 'NONE',  ( 1.000000000000000000, 0.000000000000000000, 0.000000000000000000 ) ) ;
#255423 = CARTESIAN_POINT ( 'NONE',  ( -5.900000000000003020, -11.75000000000000000, 10.00000000000000178 ) ) ;
#255425 = EDGE_CURVE ( 'NONE', #152513, #179560, #55983, .T. ) ;
#255427 = ADVANCED_FACE ( 'NONE', ( #179828, #37755, #233392 ), #54721, .T. ) ;
#255426 = CARTESIAN_POINT ( 'NONE',  ( -23.15000000000000213, 54.82645269529697885, -239.3027372265576957 ) ) ;
#255428 = DIRECTION ( 'NONE',  ( -1.000000000000000000, -2.986185139342071370E-16, 6.665775143889693760E-16 ) ) ;
#255429 = TOROIDAL_SURFACE ( 'NONE', #130566, 0.6000000000000004219, 0.1000000000000000056 ) ;
#255430 = EDGE_CURVE ( 'NONE', #208529, #2024, #151021, .T. ) ;
#255431 = VECTOR ( 'NONE', #60168, 1000.000000000000000 ) ;
#255432 = CARTESIAN_POINT ( 'NONE',  ( 21.05000000000000071, 11.60000000001116227, -160.5717967697245285 ) ) ;
#255434 = VERTEX_POINT ( 'NONE', #18166 ) ;
#255433 = ORIENTED_EDGE ( 'NONE', *, *, #62671, .T. ) ;
#255435 = EDGE_LOOP ( 'NONE', ( #76920, #164311, #157955, #165217 ) ) ;
#255436 = AXIS2_PLACEMENT_3D ( 'NONE', #71025, #139939, #179123 ) ;
#255437 = DIRECTION ( 'NONE',  ( -1.000000000000000000, 2.952720810173289112E-16, 2.061873921506763405E-30 ) ) ;
#255438 = PLANE ( 'NONE',  #253002 ) ;
#255439 = CARTESIAN_POINT ( 'NONE',  ( -21.05000000000000071, 5.900000000011162093, -123.7809002353436654 ) ) ;
#255440 = CYLINDRICAL_SURFACE ( 'NONE', #238292, 0.09999999999998898659 ) ;
#255441 = EDGE_CURVE ( 'NONE', #2430, #16782, #195153, .T. ) ;
#255443 = CARTESIAN_POINT ( 'NONE',  ( -12.47155713865592297, 66.62433047358608462, -87.15531747513844607 ) ) ;
#255442 = DIRECTION ( 'NONE',  ( 1.000000000000000000, 0.000000000000000000, 0.000000000000000000 ) ) ;
#255444 = CARTESIAN_POINT ( 'NONE',  ( -0.8999999999999430678, 63.75000000001118394, -10.02310748452479139 ) ) ;
#255445 = ORIENTED_EDGE ( 'NONE', *, *, #29671, .F. ) ;
#255446 = VECTOR ( 'NONE', #213546, 1000.000000000000000 ) ;
#255447 = CARTESIAN_POINT ( 'NONE',  ( 20.85000000000000142, -1.362429037182151470, -175.3888812479212334 ) ) ;
#255448 = VERTEX_POINT ( 'NONE', #195548 ) ;
#255449 = ORIENTED_EDGE ( 'NONE', *, *, #235771, .F. ) ;
#255450 = VECTOR ( 'NONE', #203768, 1000.000000000000000 ) ;
#255451 = DIRECTION ( 'NONE',  ( 1.000000000000000000, -0.000000000000000000, -0.000000000000000000 ) ) ;
#255452 = DIRECTION ( 'NONE',  ( -1.000000000000000000, 9.012599976028471648E-15, 6.882867235861662930E-14 ) ) ;
#255453 = AXIS2_PLACEMENT_3D ( 'NONE', #58824, #117541, #161834 ) ;
#255454 = AXIS2_PLACEMENT_3D ( 'NONE', #16829, #32562, #91220 ) ;
#255455 = CARTESIAN_POINT ( 'NONE',  ( -18.59999999999999787, 6.933893972137497030, -171.2856458343736108 ) ) ;
#255456 = AXIS2_PLACEMENT_3D ( 'NONE', #190712, #86407, #225913 ) ;
#255457 = AXIS2_PLACEMENT_3D ( 'NONE', #228135, #43385, #49489 ) ;
#255458 = CARTESIAN_POINT ( 'NONE',  ( -23.15000000000000213, 73.50000000001223555, -149.7477294072864709 ) ) ;
#255459 = ORIENTED_EDGE ( 'NONE', *, *, #17679, .F. ) ;
#255460 = VERTEX_POINT ( 'NONE', #225326 ) ;
#255461 = DIRECTION ( 'NONE',  ( 2.710505431213777355E-16, 1.000000000000000000, 6.982962677686266711E-15 ) ) ;
#255462 = DIRECTION ( 'NONE',  ( -3.265361837132813093E-16, 1.000000000000000000, 0.000000000000000000 ) ) ;
#255463 = ORIENTED_EDGE ( 'NONE', *, *, #63762, .T. ) ;
#255464 = CARTESIAN_POINT ( 'NONE',  ( 20.90000000000000213, 6.841561409100513025, 9.675512259591560138 ) ) ;
#255466 = AXIS2_PLACEMENT_3D ( 'NONE', #160327, #138144, #2489 ) ;
#255465 = FACE_OUTER_BOUND ( 'NONE', #167564, .T. ) ;
#255467 = CARTESIAN_POINT ( 'NONE',  ( 20.94999999999999929, -9.399999999988844834, -57.10603087734755690 ) ) ;
#255468 = CARTESIAN_POINT ( 'NONE',  ( 18.39999999999999503, 11.47316190337363828, -79.65000000000004832 ) ) ;
#255470 = LINE ( 'NONE', #234679, #253869 ) ;
#255469 = DIRECTION ( 'NONE',  ( 0.000000000000000000, 6.982962677686266711E-15, -1.000000000000000000 ) ) ;
#255471 = DIRECTION ( 'NONE',  ( 0.000000000000000000, 0.4930308989875575865, 0.8700118002898125091 ) ) ;
#255472 = LINE ( 'NONE', #73081, #87468 ) ;
#255473 = VECTOR ( 'NONE', #92486, 1000.000000000000000 ) ;
#255474 = ADVANCED_FACE ( 'NONE', ( #221478 ), #46700, .F. ) ;
#255475 = DIRECTION ( 'NONE',  ( -1.000000000000000000, -0.000000000000000000, 0.000000000000000000 ) ) ;
#255476 = FACE_OUTER_BOUND ( 'NONE', #48409, .T. ) ;
#255478 = ORIENTED_EDGE ( 'NONE', *, *, #241856, .F. ) ;
#255477 = DIRECTION ( 'NONE',  ( 0.000000000000000000, 0.000000000000000000, -1.000000000000000000 ) ) ;
#255479 = EDGE_CURVE ( 'NONE', #164247, #46606, #67618, .T. ) ;
#255480 = AXIS2_PLACEMENT_3D ( 'NONE', #107565, #142821, #223653 ) ;
#255481 = CIRCLE ( 'NONE', #143076, 0.1000000000000028644 ) ;
#255482 = PRESENTATION_LAYER_ASSIGNMENT (  '', '', ( #184605 ) ) ;
#255483 = DIRECTION ( 'NONE',  ( -1.000000000000000000, 0.000000000000000000, 0.000000000000000000 ) ) ;
#255484 = ORIENTED_EDGE ( 'NONE', *, *, #209680, .T. ) ;
#255485 = CARTESIAN_POINT ( 'NONE',  ( -22.14074124539699895, 0.09905289585522827900, -93.10992214895625807 ) ) ;
#255486 = DIRECTION ( 'NONE',  ( -0.000000000000000000, 1.000000000000000000, 6.982962677686266711E-15 ) ) ;
#255487 = ORIENTED_EDGE ( 'NONE', *, *, #113708, .T. ) ;
#255488 = CARTESIAN_POINT ( 'NONE',  ( 11.60000000000000142, -11.75000000000000000, 17.70000000000000284 ) ) ;
#255489 = EDGE_CURVE ( 'NONE', #36888, #86236, #22035, .T. ) ;
#255490 = DIRECTION ( 'NONE',  ( 1.000000000000000000, 0.000000000000000000, 0.000000000000000000 ) ) ;
#255491 = CARTESIAN_POINT ( 'NONE',  ( 22.47809213839789066, 0.03753706763967752658, -21.85002666521219794 ) ) ;
#255492 = CIRCLE ( 'NONE', #113513, 11.80000000000001670 ) ;
#255493 = AXIS2_PLACEMENT_3D ( 'NONE', #41164, #690, #200214 ) ;
#255495 = CARTESIAN_POINT ( 'NONE',  ( -23.15000000000000213, 64.35000000001198828, -115.1731074845243938 ) ) ;
#255494 = CIRCLE ( 'NONE', #89136, 7.900000000000000355 ) ;
#255496 = CARTESIAN_POINT ( 'NONE',  ( 18.59999999999999432, 10.49142135623730887, -24.75000000000000000 ) ) ;
#255497 = DIRECTION ( 'NONE',  ( 0.000000000000000000, 0.000000000000000000, -1.000000000000000000 ) ) ;
#255498 = ORIENTED_EDGE ( 'NONE', *, *, #255694, .F. ) ;
#255499 = DIRECTION ( 'NONE',  ( 0.000000000000000000, -6.938893903907222067E-15, 1.000000000000000000 ) ) ;
#255501 = ORIENTED_EDGE ( 'NONE', *, *, #123269, .F. ) ;
#255500 = DIRECTION ( 'NONE',  ( -0.000000000000000000, 0.9651348961777157509, -0.2617529984165031243 ) ) ;
#255502 = DIRECTION ( 'NONE',  ( -0.7071067811865127117, -0.7071067811865821007, 0.000000000000000000 ) ) ;
#255503 = CARTESIAN_POINT ( 'NONE',  ( 22.39999999999999858, 75.90000000001273861, -211.3138870828977360 ) ) ;
#255504 = SPHERICAL_SURFACE ( 'NONE', #158779, 0.1000000000000000056 ) ;
#255505 = ORIENTED_EDGE ( 'NONE', *, *, #176363, .T. ) ;
#255506 = CARTESIAN_POINT ( 'NONE',  ( -22.94999999999999929, -1.467286812112899463, 28.00000000000000000 ) ) ;
#255507 = APPLICATION_PROTOCOL_DEFINITION ( 'draft international standard', 'automotive_design', 1998, #77473 ) ;
#255508 = SPHERICAL_SURFACE ( 'NONE', #143931, 0.1000000000000000056 ) ;
#255509 = CARTESIAN_POINT ( 'NONE',  ( 22.49999999999999645, -2.401771312552908100, -189.4980873520050011 ) ) ;
#255510 = EDGE_LOOP ( 'NONE', ( #251306, #81911, #176604, #66096, #163603, #232985, #101524, #148268, #21497, #23602 ) ) ;
#255511 = CARTESIAN_POINT ( 'NONE',  ( 21.05000000000000071, 76.00000000001170974, -69.52310748452431710 ) ) ;
#255512 = DIRECTION ( 'NONE',  ( -1.000000000000000000, 3.265361837132813093E-16, 2.280189983783949500E-30 ) ) ;
#255513 = AXIS2_PLACEMENT_3D ( 'NONE', #164562, #242791, #61598 ) ;
#255514 = CARTESIAN_POINT ( 'NONE',  ( -16.80939487329394666, 9.950000000011138823, -121.3500000000009180 ) ) ;
#255515 = ORIENTED_EDGE ( 'NONE', *, *, #8496, .T. ) ;
#255516 = ORIENTED_EDGE ( 'NONE', *, *, #100024, .F. ) ;
#255517 = DIRECTION ( 'NONE',  ( 0.000000000000000000, 0.000000000000000000, -1.000000000000000000 ) ) ;
#255518 = CARTESIAN_POINT ( 'NONE',  ( 21.05095171578076574, 8.776179878782192745, -45.66587327663788187 ) ) ;
#255519 = EDGE_CURVE ( 'NONE', #143815, #11889, #250939, .T. ) ;
#255520 = CARTESIAN_POINT ( 'NONE',  ( -22.47071067811865319, 1.115600667400684642E-11, -33.50000000000000000 ) ) ;
#255521 = DIRECTION ( 'NONE',  ( 0.000000000000000000, 0.2617529984165028467, 0.9651348961777158619 ) ) ;
#255522 = CARTESIAN_POINT ( 'NONE',  ( -17.04295772865385672, 30.24169553524738419, -234.7410215167427054 ) ) ;
#255523 = ADVANCED_FACE ( 'NONE', ( #239791 ), #106664, .T. ) ;
#255525 = DIRECTION ( 'NONE',  ( 0.000000000000000000, -0.8814952561688438326, 0.4721928772777332917 ) ) ;
#255524 = CARTESIAN_POINT ( 'NONE',  ( 18.55857864376268296, 65.63284271248636514, -78.27310748452438816 ) ) ;
#255526 = DIRECTION ( 'NONE',  ( 0.000000000000000000, -1.411300455031978166E-14, 1.000000000000000000 ) ) ;
#255527 = CARTESIAN_POINT ( 'NONE',  ( -16.93658623642901873, 9.980381671668284937, -113.1119027291292269 ) ) ;
#255528 = CARTESIAN_POINT ( 'NONE',  ( 18.54148534481893762, 65.67467670974366456, -30.45317318268843465 ) ) ;
#255530 = CARTESIAN_POINT ( 'NONE',  ( 21.14999999999999858, 11.75000000000000711, -0.1000000000000028644 ) ) ;
#255529 = AXIS2_PLACEMENT_3D ( 'NONE', #220070, #60983, #166228 ) ;
#255531 = ORIENTED_EDGE ( 'NONE', *, *, #23806, .F. ) ;
#255532 = AXIS2_PLACEMENT_3D ( 'NONE', #166811, #230611, #6410 ) ;
#255533 = VERTEX_POINT ( 'NONE', #104095 ) ;
#255534 = DIRECTION ( 'NONE',  ( -0.7071067811865475727, 0.7071067811865475727, 4.937700262164531476E-15 ) ) ;
#255535 = CARTESIAN_POINT ( 'NONE',  ( -5.899999999999938183, 64.25000000001119815, -22.12310748452479103 ) ) ;
#255538 = DIRECTION ( 'NONE',  ( -0.7071067811865474617, 0.7071067811865474617, 4.937700262164531476E-15 ) ) ;
#255537 = CARTESIAN_POINT ( 'NONE',  ( 21.09316766718127667, 69.62984668753723838, -69.56237088683906222 ) ) ;
#255536 = CIRCLE ( 'NONE', #201413, 0.09999999999998898659 ) ;
#255539 = EDGE_CURVE ( 'NONE', #88951, #169154, #109298, .T. ) ;
#255540 = CARTESIAN_POINT ( 'NONE',  ( 18.39999999999999503, 53.98582189624753624, -228.9137301112145622 ) ) ;
#255541 = CARTESIAN_POINT ( 'NONE',  ( -23.25000000000000000, 64.35000000001258513, -191.3731074845244393 ) ) ;
#255542 = CYLINDRICAL_SURFACE ( 'NONE', #173214, 0.9000000000000014655 ) ;
#255543 = EDGE_CURVE ( 'NONE', #26647, #88045, #200888, .T. ) ;
#255544 = VERTEX_POINT ( 'NONE', #205783 ) ;
#255545 = EDGE_CURVE ( 'NONE', #226085, #136324, #113416, .T. ) ;
#255546 = ORIENTED_EDGE ( 'NONE', *, *, #193896, .T. ) ;
#255548 = VECTOR ( 'NONE', #241833, 1000.000000000000000 ) ;
#255547 = CARTESIAN_POINT ( 'NONE',  ( 23.14999999999999858, 76.00000000001142553, -36.02310748452432421 ) ) ;
#255549 = EDGE_CURVE ( 'NONE', #60383, #138609, #221712, .T. ) ;
#255550 = ORIENTED_EDGE ( 'NONE', *, *, #69771, .T. ) ;
#255551 = FACE_OUTER_BOUND ( 'NONE', #143838, .T. ) ;
#255552 = CIRCLE ( 'NONE', #139035, 0.5000000000000004441 ) ;
#255554 = FACE_OUTER_BOUND ( 'NONE', #62221, .T. ) ;
#255553 = TOROIDAL_SURFACE ( 'NONE', #239041, 11.65000000000000036, 0.1000000000000000056 ) ;
#255555 = VECTOR ( 'NONE', #175883, 1000.000000000000000 ) ;
#255556 = EDGE_LOOP ( 'NONE', ( #112599, #127514, #20996, #154637, #85993 ) ) ;
#255557 = CARTESIAN_POINT ( 'NONE',  ( -16.93388492042258164, 66.01145817749670641, -190.9236526077106078 ) ) ;
#255558 = ADVANCED_FACE ( 'NONE', ( #143236 ), #164105, .T. ) ;
#255559 = ORIENTED_EDGE ( 'NONE', *, *, #145568, .F. ) ;
#255560 = FACE_OUTER_BOUND ( 'NONE', #92903, .T. ) ;
#255561 = CARTESIAN_POINT ( 'NONE',  ( 20.94999999999999929, 76.00000000001213607, -136.5231074845243313 ) ) ;
#255562 = CARTESIAN_POINT ( 'NONE',  ( -16.92925196614874750, 66.02766820360193378, -123.9063626368075859 ) ) ;
#255563 = AXIS2_PLACEMENT_3D ( 'NONE', #194897, #174074, #56606 ) ;
#255565 = FACE_OUTER_BOUND ( 'NONE', #145876, .T. ) ;
#255564 = CIRCLE ( 'NONE', #80622, 0.1000000000000052097 ) ;
#255566 = CARTESIAN_POINT ( 'NONE',  ( -16.94225986326250322, 9.949999999999981526, -12.94671937560788599 ) ) ;
#255569 = FACE_OUTER_BOUND ( 'NONE', #109516, .T. ) ;
#255568 = AXIS2_PLACEMENT_3D ( 'NONE', #200801, #102960, #59978 ) ;
#255567 = CARTESIAN_POINT ( 'NONE',  ( 23.24999999999999289, 8.980461154494404852, -187.0187154576991304 ) ) ;
#255570 = DIRECTION ( 'NONE',  ( 0.000000000000000000, 0.2617529984165065660, 0.9651348961777146407 ) ) ;
#255571 = EDGE_LOOP ( 'NONE', ( #97829, #143141, #243590, #81704 ) ) ;
#255573 = CARTESIAN_POINT ( 'NONE',  ( 21.00000000000000000, 9.750000000011153745, -179.8499999999999943 ) ) ;
#255572 = DIRECTION ( 'NONE',  ( 0.000000000000000000, 1.000000000000000000, 0.000000000000000000 ) ) ;
#255574 = ORIENTED_EDGE ( 'NONE', *, *, #50288, .T. ) ;
#255576 = ORIENTED_EDGE ( 'NONE', *, *, #185816, .T. ) ;
#255575 = DIRECTION ( 'NONE',  ( -1.000000000000000000, -0.000000000000000000, -0.000000000000000000 ) ) ;
#255577 = EDGE_LOOP ( 'NONE', ( #201888, #3579, #73338, #210989 ) ) ;
#255578 = CYLINDRICAL_SURFACE ( 'NONE', #36804, 0.09999999999999939493 ) ;
#255579 = CARTESIAN_POINT ( 'NONE',  ( 21.05000000000000071, 0.000000000000000000, -33.50000000000000000 ) ) ;
#255580 = DIRECTION ( 'NONE',  ( -1.000000000000000000, 0.000000000000000000, 0.000000000000000000 ) ) ;
#255581 = AXIS2_PLACEMENT_3D ( 'NONE', #79606, #139575, #255648 ) ;
#255582 = DIRECTION ( 'NONE',  ( 0.000000000000000000, 1.224646799142185182E-16, 1.000000000000000000 ) ) ;
#255583 = VERTEX_POINT ( 'NONE', #126241 ) ;
#255584 = CARTESIAN_POINT ( 'NONE',  ( -18.69999999999999929, 1.250000000000000000, 21.90000000000000213 ) ) ;
#255585 = FILL_AREA_STYLE_COLOUR ( '', #180739 ) ;
#255586 = DIRECTION ( 'NONE',  ( 0.000000000000000000, 0.2617529984165032908, 0.9651348961777156399 ) ) ;
#255587 = AXIS2_PLACEMENT_3D ( 'NONE', #10366, #50728, #66473 ) ;
#255588 = ORIENTED_EDGE ( 'NONE', *, *, #134574, .F. ) ;
#255589 = VECTOR ( 'NONE', #151433, 1000.000000000000000 ) ;
#255590 = DIRECTION ( 'NONE',  ( 1.000000000000000000, -7.304098846218134667E-16, -4.217023435051626718E-16 ) ) ;
#255591 = CIRCLE ( 'NONE', #226388, 4.150000000000001243 ) ;
#255592 = CARTESIAN_POINT ( 'NONE',  ( 23.15000000000000213, -11.74999999998883737, -79.25000000000004263 ) ) ;
#255593 = ORIENTED_EDGE ( 'NONE', *, *, #212823, .T. ) ;
#255594 = ORIENTED_EDGE ( 'NONE', *, *, #39115, .F. ) ;
#255595 = CARTESIAN_POINT ( 'NONE',  ( -20.64999999999999858, 7.250000000011155521, -88.15000000000004832 ) ) ;
#255596 = EDGE_CURVE ( 'NONE', #59508, #12728, #161550, .T. ) ;
#255597 = VERTEX_POINT ( 'NONE', #160277 ) ;
#255598 = CARTESIAN_POINT ( 'NONE',  ( -18.59999999999999787, 74.83729825007408465, -128.4231074845243086 ) ) ;
#255599 = ORIENTED_EDGE ( 'NONE', *, *, #182778, .T. ) ;
#255600 = CARTESIAN_POINT ( 'NONE',  ( 21.07928932188134397, 75.90110485435802445, -176.3516241409176644 ) ) ;
#255601 = CARTESIAN_POINT ( 'NONE',  ( -20.94999999999999929, 76.00000000001222134, -148.3231074845243427 ) ) ;
#255602 = DIRECTION ( 'NONE',  ( 1.296989514748957922E-15, 0.2677755899090746849, -0.9634813093406884299 ) ) ;
#255603 = EDGE_CURVE ( 'NONE', #149981, #185072, #121799, .T. ) ;
#255604 = CARTESIAN_POINT ( 'NONE',  ( 20.95512820512820440, 60.90483797576754910, -225.2715357783924333 ) ) ;
#255605 = AXIS2_PLACEMENT_3D ( 'NONE', #218400, #256192, #21525 ) ;
#255606 = ADVANCED_FACE ( 'NONE', ( #224054 ), #243628, .T. ) ;
#255607 = ADVANCED_FACE ( 'NONE', ( #63704 ), #45432, .F. ) ;
#255608 = VECTOR ( 'NONE', #223568, 1000.000000000000000 ) ;
#255609 = CARTESIAN_POINT ( 'NONE',  ( -23.25000000000000000, 66.26558728512915764, -222.7970849955717938 ) ) ;
#255610 = CARTESIAN_POINT ( 'NONE',  ( 18.41815437325349691, -9.498709853130264946, -73.60394583880211883 ) ) ;
#255611 = CARTESIAN_POINT ( 'NONE',  ( -22.19999999999999929, -1.467286812112899463, 32.89999999999999858 ) ) ;
#255612 = CIRCLE ( 'NONE', #238927, 4.100000000000011191 ) ;
#255613 = ORIENTED_EDGE ( 'NONE', *, *, #47798, .F. ) ;
#255615 = CARTESIAN_POINT ( 'NONE',  ( -14.00000000000000178, 47.91805600923872532, -233.7139610577891631 ) ) ;
#255614 = CYLINDRICAL_SURFACE ( 'NONE', #237272, 0.09999999999999939493 ) ;
#255616 = ORIENTED_EDGE ( 'NONE', *, *, #195398, .F. ) ;
#255619 = ORIENTED_EDGE ( 'NONE', *, *, #143676, .T. ) ;
#255618 = CARTESIAN_POINT ( 'NONE',  ( -18.50000000000000711, 85.41920341803825067, -62.27532167409560060 ) ) ;
#255617 = DIRECTION ( 'NONE',  ( 1.000000000000000000, 3.265361837132813093E-16, -0.000000000000000000 ) ) ;
#255620 = EDGE_LOOP ( 'NONE', ( #256303, #61400, #148100, #94813 ) ) ;
#255621 = CARTESIAN_POINT ( 'NONE',  ( -23.25000000000000355, 8.212522512469059066, -212.1579332307740344 ) ) ;
#255622 = CARTESIAN_POINT ( 'NONE',  ( 13.54556439290363556, 66.54940788787858708, -154.9669191657160638 ) ) ;
#255623 = AXIS2_PLACEMENT_3D ( 'NONE', #147578, #42083, #43353 ) ;
#255624 = PLANE ( 'NONE',  #156904 ) ;
#255625 = DIRECTION ( 'NONE',  ( 0.000000000000000000, 0.2617529984165055668, 0.9651348961777149738 ) ) ;
#255626 = AXIS2_PLACEMENT_3D ( 'NONE', #83220, #141935, #24589 ) ;
#255627 = ORIENTED_EDGE ( 'NONE', *, *, #106783, .F. ) ;
#255628 = LINE ( 'NONE', #53633, #188537 ) ;
#255629 = EDGE_CURVE ( 'NONE', #110700, #12767, #41608, .T. ) ;
#255630 = PLANE ( 'NONE',  #202723 ) ;
#255631 = CIRCLE ( 'NONE', #109920, 0.5000000000000014433 ) ;
#255632 = EDGE_CURVE ( 'NONE', #210105, #148669, #101513, .T. ) ;
#255634 = CARTESIAN_POINT ( 'NONE',  ( -18.40000000000000213, 11.48667500175767131, -24.25000000000000000 ) ) ;
#255633 = CARTESIAN_POINT ( 'NONE',  ( 20.04142135623730070, 11.65000000001115943, -155.3500000000000227 ) ) ;
#255635 = ORIENTED_EDGE ( 'NONE', *, *, #146400, .T. ) ;
#255636 = AXIS2_PLACEMENT_3D ( 'NONE', #252687, #152354, #156201 ) ;
#255637 = PRODUCT_RELATED_PRODUCT_CATEGORY ( 'part', '', ( #74532 ) ) ;
#255638 = AXIS2_PLACEMENT_3D ( 'NONE', #178863, #217920, #127510 ) ;
#255639 = PRODUCT_DEFINITION_SHAPE ( 'NONE', 'NONE',  #258115 ) ;
#255640 = ORIENTED_EDGE ( 'NONE', *, *, #88190, .T. ) ;
#255641 = VECTOR ( 'NONE', #122297, 1000.000000000000000 ) ;
#255642 = CARTESIAN_POINT ( 'NONE',  ( 20.95545211741311320, 11.95827706127094103, -206.1595911373138676 ) ) ;
#255643 = PLANE ( 'NONE',  #14056 ) ;
#255644 = ORIENTED_EDGE ( 'NONE', *, *, #183013, .F. ) ;
#255645 = PLANE ( 'NONE',  #39529 ) ;
#255646 = EDGE_LOOP ( 'NONE', ( #24303, #146001, #48516, #164664 ) ) ;
#255647 = ADVANCED_FACE ( 'NONE', ( #110531 ), #10163, .T. ) ;
#255648 = DIRECTION ( 'NONE',  ( 0.000000000000000000, 0.000000000000000000, -1.000000000000000000 ) ) ;
#255650 = EDGE_CURVE ( 'NONE', #24665, #219149, #212227, .T. ) ;
#255649 = CARTESIAN_POINT ( 'NONE',  ( 21.98333005346336577, 29.92928821712973786, -252.5659568089976403 ) ) ;
#255651 = DIRECTION ( 'NONE',  ( -0.000000000000000000, 1.000000000000000000, 0.000000000000000000 ) ) ;
#255652 = EDGE_CURVE ( 'NONE', #253844, #231239, #38385, .T. ) ;
#255653 = AXIS2_PLACEMENT_3D ( 'NONE', #224760, #61856, #121837 ) ;
#255654 = ORIENTED_EDGE ( 'NONE', *, *, #146766, .F. ) ;
#255655 = FACE_OUTER_BOUND ( 'NONE', #166635, .T. ) ;
#255656 = CIRCLE ( 'NONE', #30874, 0.1000000000000214190 ) ;
#255657 = CARTESIAN_POINT ( 'NONE',  ( -21.05000000000000071, 11.62071067812980907, -73.86841665234109655 ) ) ;
#255658 = AXIS2_PLACEMENT_3D ( 'NONE', #170833, #245187, #30012 ) ;
#255659 = CIRCLE ( 'NONE', #130805, 0.1000000000000057648 ) ;
#255660 = ORIENTED_EDGE ( 'NONE', *, *, #71531, .T. ) ;
#255661 = ORIENTED_EDGE ( 'NONE', *, *, #98241, .F. ) ;
#255662 = CARTESIAN_POINT ( 'NONE',  ( -16.96982749440684657, 44.56876802688330486, -235.1048246731278084 ) ) ;
#255663 = VERTEX_POINT ( 'NONE', #167982 ) ;
#255664 = VERTEX_POINT ( 'NONE', #190082 ) ;
#255666 = ORIENTED_EDGE ( 'NONE', *, *, #78423, .F. ) ;
#255665 = CARTESIAN_POINT ( 'NONE',  ( 20.85000000000000142, 7.120270961708750512, -204.6595630418393057 ) ) ;
#255667 = APPLICATION_CONTEXT ( 'automotive_design' ) ;
#255668 = ORIENTED_EDGE ( 'NONE', *, *, #216381, .F. ) ;
#255669 = DIRECTION ( 'NONE',  ( 0.000000000000000000, 0.000000000000000000, -1.000000000000000000 ) ) ;
#255673 = ADVANCED_FACE ( 'NONE', ( #109242 ), #231785, .F. ) ;
#255672 = EDGE_LOOP ( 'NONE', ( #19433, #182602, #116370, #152324, #43288 ) ) ;
#255671 = ORIENTED_EDGE ( 'NONE', *, *, #109787, .T. ) ;
#255670 = CARTESIAN_POINT ( 'NONE',  ( -23.25000000000000000, 7.128833340094563376, -233.7327013124401276 ) ) ;
#255674 = ORIENTED_EDGE ( 'NONE', *, *, #68831, .F. ) ;
#255675 = CIRCLE ( 'NONE', #80737, 0.1000000000000000472 ) ;
#255676 = FACE_OUTER_BOUND ( 'NONE', #63753, .T. ) ;
#255677 = AXIS2_PLACEMENT_3D ( 'NONE', #150776, #214588, #92077 ) ;
#255678 = TOROIDAL_SURFACE ( 'NONE', #251448, 0.2000000000000000111, 0.1000000000000000056 ) ;
#255679 = FACE_OUTER_BOUND ( 'NONE', #135626, .T. ) ;
#255680 = DIRECTION ( 'NONE',  ( 0.000000000000000000, -2.862293735361729181E-14, -1.000000000000000000 ) ) ;
#255681 = ORIENTED_EDGE ( 'NONE', *, *, #140030, .F. ) ;
#255682 = EDGE_CURVE ( 'NONE', #28076, #236193, #100886, .T. ) ;
#255683 = DIRECTION ( 'NONE',  ( -0.000000000000000000, 1.000000000000000000, -0.000000000000000000 ) ) ;
#255684 =( BOUNDED_CURVE ( )  B_SPLINE_CURVE ( 3, ( #244238, #46046, #121763, #201268 ),
 .UNSPECIFIED., .F., .F. ) 
 B_SPLINE_CURVE_WITH_KNOTS ( ( 4, 4 ),
 ( 3.141592653589816653, 4.712388980384673687 ),
 .UNSPECIFIED. ) 
 CURVE ( )  GEOMETRIC_REPRESENTATION_ITEM ( )  RATIONAL_B_SPLINE_CURVE ( ( 1.000000000000000000, 0.8047378541243743744, 0.8047378541243743744, 1.000000000000000000 ) ) 
 REPRESENTATION_ITEM ( '' )  );
#255686 = ORIENTED_EDGE ( 'NONE', *, *, #113563, .T. ) ;
#255685 = CARTESIAN_POINT ( 'NONE',  ( 23.50000000000005684, 84.00000000001119815, -37.18565239344504647 ) ) ;
#255687 = DIRECTION ( 'NONE',  ( -1.000000000000000000, 7.304098846218133681E-16, -4.217023435051677994E-16 ) ) ;
#255689 = ORIENTED_EDGE ( 'NONE', *, *, #166432, .T. ) ;
#255688 = FACE_OUTER_BOUND ( 'NONE', #203345, .T. ) ;
#255690 = VERTEX_POINT ( 'NONE', #169270 ) ;
#255691 = ADVANCED_FACE ( 'NONE', ( #147081 ), #191394, .T. ) ;
#255692 = CARTESIAN_POINT ( 'NONE',  ( 21.53752568622134334, 0.09897446127763709356, -160.7131921254513998 ) ) ;
#255693 = DIRECTION ( 'NONE',  ( 0.000000000000000000, 0.000000000000000000, -1.000000000000000000 ) ) ;
#255694 = EDGE_CURVE ( 'NONE', #171180, #70632, #63502, .T. ) ;
#255695 = VERTEX_POINT ( 'NONE', #68865 ) ;
#255696 = VERTEX_POINT ( 'NONE', #171837 ) ;
#255697 = CARTESIAN_POINT ( 'NONE',  ( -16.94107738177415712, 10.01423928514777728, -180.0499999999999545 ) ) ;
#255698 = CARTESIAN_POINT ( 'NONE',  ( -21.52071067811865746, 7.779289321892505882, -54.75000000000000000 ) ) ;
#255699 = ADVANCED_FACE ( 'NONE', ( #187534 ), #207081, .T. ) ;
#255701 = ORIENTED_EDGE ( 'NONE', *, *, #211360, .T. ) ;
#255700 = VERTEX_POINT ( 'NONE', #53128 ) ;
#255702 = CIRCLE ( 'NONE', #138995, 0.09999999999999939493 ) ;
#255703 = VERTEX_POINT ( 'NONE', #166697 ) ;
#255705 = EDGE_CURVE ( 'NONE', #88402, #187424, #254231, .T. ) ;
#255704 = CARTESIAN_POINT ( 'NONE',  ( 18.59999999999999432, 77.13501884592203339, -95.30613060109196510 ) ) ;
#255706 = ORIENTED_EDGE ( 'NONE', *, *, #243383, .F. ) ;
#255707 = ORIENTED_EDGE ( 'NONE', *, *, #72415, .F. ) ;
#255708 = CARTESIAN_POINT ( 'NONE',  ( 5.899999999999995914, -11.75000000000000000, 9.900000000000002132 ) ) ;
#255709 = ORIENTED_EDGE ( 'NONE', *, *, #219565, .F. ) ;
#255710 = CARTESIAN_POINT ( 'NONE',  ( -16.93226657140833069, 12.44727255555560319, -211.1626918736521361 ) ) ;
#255712 = CARTESIAN_POINT ( 'NONE',  ( -22.50000000000000000, 64.35023708198076520, -203.6119174609113713 ) ) ;
#255711 = CARTESIAN_POINT ( 'NONE',  ( 20.04999999999999716, 8.750000000011173285, -109.7500000000000426 ) ) ;
#255713 = ORIENTED_EDGE ( 'NONE', *, *, #82862, .F. ) ;
#255714 = EDGE_LOOP ( 'NONE', ( #39303, #1371, #112657, #29830 ) ) ;
#255715 = CARTESIAN_POINT ( 'NONE',  ( -21.05000000000000071, -4.914013037343267776, -233.1828366659746905 ) ) ;
#255716 = AXIS2_PLACEMENT_3D ( 'NONE', #69376, #90181, #169782 ) ;
#255717 = ORIENTED_EDGE ( 'NONE', *, *, #215082, .F. ) ;
#255718 = ADVANCED_FACE ( 'NONE', ( #148389 ), #38578, .T. ) ;
#255719 = VECTOR ( 'NONE', #119650, 1000.000000000000000 ) ;
#255720 = EDGE_CURVE ( 'NONE', #186535, #55330, #11456, .T. ) ;
#255721 = AXIS2_PLACEMENT_3D ( 'NONE', #224377, #87428, #208699 ) ;
#255722 = CIRCLE ( 'NONE', #155833, 0.1000000000000070832 ) ;
#255723 = DIRECTION ( 'NONE',  ( -1.000000000000000000, 0.000000000000000000, -0.000000000000000000 ) ) ;
#255724 = ORIENTED_EDGE ( 'NONE', *, *, #17216, .T. ) ;
#255725 = VERTEX_POINT ( 'NONE', #150955 ) ;
#255726 = EDGE_CURVE ( 'NONE', #39812, #36453, #171703, .T. ) ;
#255727 = CYLINDRICAL_SURFACE ( 'NONE', #191810, 0.09999999999998898659 ) ;
#255729 = ORIENTED_EDGE ( 'NONE', *, *, #151876, .T. ) ;
#255728 = DIRECTION ( 'NONE',  ( 0.000000000000000000, 0.000000000000000000, 1.000000000000000000 ) ) ;
#255730 = FACE_OUTER_BOUND ( 'NONE', #157577, .T. ) ;
#255731 = PLANE ( 'NONE',  #201934 ) ;
#255732 = ORIENTED_EDGE ( 'NONE', *, *, #133247, .T. ) ;
#255733 = CARTESIAN_POINT ( 'NONE',  ( -2.995603634470891112E-16, 69.35000000001254250, -182.2731074845244166 ) ) ;
#255734 = DIRECTION ( 'NONE',  ( -1.000000000000000000, 0.000000000000000000, 0.000000000000000000 ) ) ;
#255735 = DIRECTION ( 'NONE',  ( 0.000000000000000000, -0.5868805631290325842, -0.8096735173027148624 ) ) ;
#255736 = FACE_OUTER_BOUND ( 'NONE', #222097, .T. ) ;
#255737 = CARTESIAN_POINT ( 'NONE',  ( -18.59999999999999787, 64.35000000001234355, -163.0083017138704236 ) ) ;
#255738 = DIRECTION ( 'NONE',  ( -1.000000000000000000, 0.000000000000000000, 0.000000000000000000 ) ) ;
#255740 = EDGE_CURVE ( 'NONE', #20388, #99952, #116959, .T. ) ;
#255739 = CARTESIAN_POINT ( 'NONE',  ( -16.83794479845801462, 66.07364258066074569, -149.3266627803021152 ) ) ;
#255741 = AXIS2_PLACEMENT_3D ( 'NONE', #249250, #232269, #10637 ) ;
#255742 = CARTESIAN_POINT ( 'NONE',  ( 21.05000000000000071, 4.436385504674529301, -245.3241086753762659 ) ) ;
#255743 = CYLINDRICAL_SURFACE ( 'NONE', #197241, 0.09999999999999939493 ) ;
#255744 = EDGE_CURVE ( 'NONE', #200983, #143659, #130153, .T. ) ;
#255745 = AXIS2_PLACEMENT_3D ( 'NONE', #91260, #14312, #190372 ) ;
#255746 = ORIENTED_EDGE ( 'NONE', *, *, #192555, .T. ) ;
#255747 = AXIS2_PLACEMENT_3D ( 'NONE', #186751, #249291, #8105 ) ;
#255748 = CIRCLE ( 'NONE', #55849, 0.1000000000000052097 ) ;
#255749 = EDGE_CURVE ( 'NONE', #193233, #182596, #174417, .T. ) ;
#255751 = ORIENTED_EDGE ( 'NONE', *, *, #99099, .F. ) ;
#255750 = ORIENTED_EDGE ( 'NONE', *, *, #116568, .T. ) ;
#255753 = ORIENTED_EDGE ( 'NONE', *, *, #91534, .F. ) ;
#255752 = AXIS2_PLACEMENT_3D ( 'NONE', #175136, #128576, #90716 ) ;
#255754 = CARTESIAN_POINT ( 'NONE',  ( -21.04999999999994387, 84.00000000001119815, -34.86056257560453986 ) ) ;
#255755 = CARTESIAN_POINT ( 'NONE',  ( 20.04142135623730070, 64.35000000001180354, -81.67310748452439384 ) ) ;
#255756 = ADVANCED_FACE ( 'NONE', ( #97354 ), #230107, .F. ) ;
#255758 = CARTESIAN_POINT ( 'NONE',  ( 18.49999999999999645, 74.98773774893902555, -233.8732236541320333 ) ) ;
#255757 = DIRECTION ( 'NONE',  ( 1.000000000000000000, 0.000000000000000000, 0.000000000000000000 ) ) ;
#255759 = EDGE_CURVE ( 'NONE', #21635, #139646, #55657, .T. ) ;
#255760 = ORIENTED_EDGE ( 'NONE', *, *, #48208, .F. ) ;
#255761 = AXIS2_PLACEMENT_3D ( 'NONE', #123053, #184291, #202582 ) ;
#255762 = DIRECTION ( 'NONE',  ( 0.000000000000000000, 0.2617529984165033463, 0.9651348961777157509 ) ) ;
#255764 = CIRCLE ( 'NONE', #85078, 0.1000000000000028644 ) ;
#255763 = DIRECTION ( 'NONE',  ( 0.000000000000000000, 0.3738317757009345654, 0.9274965247785492695 ) ) ;
#255765 = CARTESIAN_POINT ( 'NONE',  ( -22.57320508075687115, 64.25000000001195133, -103.0231074845244024 ) ) ;
#255766 = CARTESIAN_POINT ( 'NONE',  ( -16.97683809663752186, 9.950000000011138823, -176.7499999999999716 ) ) ;
#255768 = ORIENTED_EDGE ( 'NONE', *, *, #19474, .F. ) ;
#255767 = CIRCLE ( 'NONE', #18299, 12.87499999999999822 ) ;
#255769 = DIRECTION ( 'NONE',  ( -0.000000000000000000, -0.01283462868040327436, 0.9999176327611370985 ) ) ;
#255770 = VECTOR ( 'NONE', #55860, 1000.000000000000114 ) ;
#255771 = ORIENTED_EDGE ( 'NONE', *, *, #168600, .F. ) ;
#255772 = DIRECTION ( 'NONE',  ( 0.000000000000000000, 0.2617529984165034018, 0.9651348961777157509 ) ) ;
#255773 = DIRECTION ( 'NONE',  ( 0.000000000000000000, 0.000000000000000000, 1.000000000000000000 ) ) ;
#255774 = LINE ( 'NONE', #77172, #157011 ) ;
#255775 = CARTESIAN_POINT ( 'NONE',  ( 21.14999999999999858, 76.00000000001267608, -203.4231074845243654 ) ) ;
#255776 = CARTESIAN_POINT ( 'NONE',  ( 21.14999999999999503, -11.64999999999999147, 11.75000000000000000 ) ) ;
#255777 = CIRCLE ( 'NONE', #22802, 0.1000000000000028644 ) ;
#255778 = LINE ( 'NONE', #15960, #116799 ) ;
#255780 = VERTEX_POINT ( 'NONE', #75293 ) ;
#255779 = AXIS2_PLACEMENT_3D ( 'NONE', #226780, #37587, #117113 ) ;
#255781 = FACE_OUTER_BOUND ( 'NONE', #110601, .T. ) ;
#255782 = CARTESIAN_POINT ( 'NONE',  ( -16.27683809663750480, 66.65000000001161595, -60.27310748452439526 ) ) ;
#255783 = CIRCLE ( 'NONE', #10125, 0.09999999999998898659 ) ;
#255785 = DIRECTION ( 'NONE',  ( 0.000000000000000000, -7.056502275159890043E-15, 1.000000000000000000 ) ) ;
#255784 = CARTESIAN_POINT ( 'NONE',  ( -16.85939591225059075, 66.09477352162421937, -123.5630392380553531 ) ) ;
#255786 = DIRECTION ( 'NONE',  ( 0.000000000000000000, 6.982962677686266711E-15, -1.000000000000000000 ) ) ;
#255787 = CARTESIAN_POINT ( 'NONE',  ( 21.09610168723073187, 0.03358950690264995292, -27.12104428477520912 ) ) ;
#255788 = CARTESIAN_POINT ( 'NONE',  ( 18.47149038651512143, 85.67145715801912331, -163.3503211497859127 ) ) ;
#255789 = CARTESIAN_POINT ( 'NONE',  ( 22.49436431346199683, 75.93309647028976883, -114.6730584321777684 ) ) ;
#255790 = EDGE_LOOP ( 'NONE', ( #157904, #185859, #49222, #38422 ) ) ;
#255791 = EDGE_CURVE ( 'NONE', #86923, #221912, #56946, .T. ) ;
#255792 =( BOUNDED_SURFACE ( )  B_SPLINE_SURFACE ( 3, 2, ( 
 ( #142591, #82599, #64369 ),
 ( #241714, #181743, #223416 ),
 ( #100868, #22694, #164751 ),
 ( #26535, #203862, #25254 ),
 ( #222117, #240433, #141330 ),
 ( #220857, #43525, #104731 ) ),
 .UNSPECIFIED., .F., .F., .F. ) 
 B_SPLINE_SURFACE_WITH_KNOTS ( ( 4, 2, 4 ),
 ( 3, 3 ),
 ( 1.570796326794897668, 2.356194490192346169, 3.141592653589794448 ),
 ( 0.000000000000000000, 1.000000000000000000 ),
 .UNSPECIFIED. ) 
 GEOMETRIC_REPRESENTATION_ITEM ( )  RATIONAL_B_SPLINE_SURFACE ( (
 ( 1.000000000000000000, 0.7071067811865536790, 1.000000000000000000),
 ( 1.000000000000000000, 0.6611148371784283384, 1.000000000000000000),
 ( 1.000000000000000000, 0.6092287576688637518, 1.000000000000000000),
 ( 1.000000000000000000, 0.5278258667065212073, 1.000000000000000000),
 ( 1.000000000000000000, 0.4993418825328512778, 1.000000000000000000),
 ( 1.000000000000000000, 0.4999999999999970024, 1.000000000000000000) ) ) 
 REPRESENTATION_ITEM ( '' )  SURFACE ( )  );
#255793 = ORIENTED_EDGE ( 'NONE', *, *, #8930, .T. ) ;
#255794 = DIRECTION ( 'NONE',  ( 0.000000000000000000, -0.000000000000000000, 1.000000000000000000 ) ) ;
#255795 = ORIENTED_EDGE ( 'NONE', *, *, #122054, .T. ) ;
#255796 = DIRECTION ( 'NONE',  ( -0.000000000000000000, -1.000000000000000000, -0.000000000000000000 ) ) ;
#255797 = TOROIDAL_SURFACE ( 'NONE', #43458, 7.800000000000000711, 0.1000000000000000056 ) ;
#255798 = AXIS2_PLACEMENT_3D ( 'NONE', #253093, #54888, #111028 ) ;
#255799 = EDGE_CURVE ( 'NONE', #131374, #69570, #92553, .T. ) ;
#255800 = AXIS2_PLACEMENT_3D ( 'NONE', #150767, #186044, #67378 ) ;
#255801 = VERTEX_POINT ( 'NONE', #178244 ) ;
#255802 = DIRECTION ( 'NONE',  ( 0.000000000000000000, 0.000000000000000000, 1.000000000000000000 ) ) ;
#255803 = DIRECTION ( 'NONE',  ( 0.000000000000000000, 0.000000000000000000, 1.000000000000000000 ) ) ;
#255804 = FACE_OUTER_BOUND ( 'NONE', #247398, .T. ) ;
#255805 = VECTOR ( 'NONE', #230673, 1000.000000000000114 ) ;
#255806 = AXIS2_PLACEMENT_3D ( 'NONE', #131052, #170239, #248443 ) ;
#255807 = LINE ( 'NONE', #138445, #149602 ) ;
#255809 = ORIENTED_EDGE ( 'NONE', *, *, #166259, .F. ) ;
#255808 = CARTESIAN_POINT ( 'NONE',  ( -16.97683809663752186, 9.950000000011137047, -187.5976359818036485 ) ) ;
#255811 = CARTESIAN_POINT ( 'NONE',  ( -20.64999999999999858, 1.940186915887853303, -12.82911921105332631 ) ) ;
#255810 = LINE ( 'NONE', #214168, #80145 ) ;
#255812 = DIRECTION ( 'NONE',  ( -1.000000000000000000, 0.000000000000000000, 0.000000000000000000 ) ) ;
#255813 = DIRECTION ( 'NONE',  ( 1.000000000000000000, 0.000000000000000000, 0.000000000000000000 ) ) ;
#255814 = AXIS2_PLACEMENT_3D ( 'NONE', #111285, #92992, #55120 ) ;
#255815 = DIRECTION ( 'NONE',  ( -1.000000000000000000, 0.000000000000000000, 0.000000000000000000 ) ) ;
#255816 = ORIENTED_EDGE ( 'NONE', *, *, #72632, .F. ) ;
#255817 = CIRCLE ( 'NONE', #126870, 0.09999999999999939493 ) ;
#255818 = DIRECTION ( 'NONE',  ( 0.000000000000000000, 0.000000000000000000, 1.000000000000000000 ) ) ;
#255819 = CARTESIAN_POINT ( 'NONE',  ( 23.25000000000000355, 98.45632476063454419, -62.72920903679256099 ) ) ;
#255820 = VECTOR ( 'NONE', #218061, 1000.000000000000000 ) ;
#255821 = AXIS2_PLACEMENT_3D ( 'NONE', #50208, #90619, #73672 ) ;
#255822 = ORIENTED_EDGE ( 'NONE', *, *, #43221, .F. ) ;
#255823 = LINE ( 'NONE', #78500, #227772 ) ;
#255824 = ORIENTED_EDGE ( 'NONE', *, *, #14568, .T. ) ;
#255825 = DIRECTION ( 'NONE',  ( 1.000000000000000000, 0.000000000000000000, -0.000000000000000000 ) ) ;
#255826 = SPHERICAL_SURFACE ( 'NONE', #28446, 0.1000000000000000056 ) ;
#255827 = LINE ( 'NONE', #57656, #245178 ) ;
#255828 = ORIENTED_EDGE ( 'NONE', *, *, #183164, .T. ) ;
#255829 = AXIS2_PLACEMENT_3D ( 'NONE', #13141, #92657, #245328 ) ;
#255830 = ORIENTED_EDGE ( 'NONE', *, *, #138600, .T. ) ;
#255831 = CARTESIAN_POINT ( 'NONE',  ( 18.39999999999997371, 62.50563584222673796, -209.4474707446456421 ) ) ;
#255832 = VECTOR ( 'NONE', #101111, 1000.000000000000000 ) ;
#255833 = CARTESIAN_POINT ( 'NONE',  ( -16.82542659449979539, 63.07592089668835911, -213.2230149068291212 ) ) ;
#255834 = CARTESIAN_POINT ( 'NONE',  ( -16.94107738177415712, 65.98576071487524075, -90.47310748452439100 ) ) ;
#255835 = EDGE_CURVE ( 'NONE', #46965, #132176, #159221, .T. ) ;
#255837 = DIRECTION ( 'NONE',  ( 0.000000000000000000, -0.2128009952263603677, 0.9770955615653313941 ) ) ;
#255836 = DIRECTION ( 'NONE',  ( 1.000000000000000000, 0.000000000000000000, 0.000000000000000000 ) ) ;
#255838 = CARTESIAN_POINT ( 'NONE',  ( 23.14999999999999858, 1.115600667400684642E-11, -100.5000000000000426 ) ) ;
#255839 = DIRECTION ( 'NONE',  ( 0.000000000000000000, 0.1575546449569757979, 0.9875102702516471709 ) ) ;
#255840 = VECTOR ( 'NONE', #188740, 1000.000000000000000 ) ;
#255841 = VERTEX_POINT ( 'NONE', #38712 ) ;
#255842 = CARTESIAN_POINT ( 'NONE',  ( -17.22361732159831504, 10.34515565861358866, -189.6292154741328204 ) ) ;
#255843 = CIRCLE ( 'NONE', #139343, 0.3999999999999975797 ) ;
#255845 = EDGE_LOOP ( 'NONE', ( #154103, #188687, #138244, #175611 ) ) ;
#255844 = CARTESIAN_POINT ( 'NONE',  ( -23.25000000000000000, 64.35000000001187459, -90.87310748452438247 ) ) ;
#255846 = AXIS2_PLACEMENT_3D ( 'NONE', #96811, #95557, #116421 ) ;
#255847 = CARTESIAN_POINT ( 'NONE',  ( 23.25000000000000000, 11.75000000001116263, -54.85000000000000142 ) ) ;
#255848 = DIRECTION ( 'NONE',  ( 0.000000000000000000, 1.810617628050740656E-13, 1.000000000000000000 ) ) ;
#255850 = DIRECTION ( 'NONE',  ( 1.000000000000000000, 0.000000000000000000, 0.000000000000000000 ) ) ;
#255849 = SPHERICAL_SURFACE ( 'NONE', #221026, 0.1000000000000000056 ) ;
#255851 = ADVANCED_FACE ( 'NONE', ( #193941 ), #221899, .T. ) ;
#255852 = ORIENTED_EDGE ( 'NONE', *, *, #157063, .T. ) ;
#255854 = LINE ( 'NONE', #92972, #167626 ) ;
#255853 = DIRECTION ( 'NONE',  ( 0.000000000000000000, 0.9770955615653315052, 0.2128009952263603954 ) ) ;
#255855 = CARTESIAN_POINT ( 'NONE',  ( -23.25000000000000000, 4.250000000011156409, -188.6499999999999488 ) ) ;
#255856 = LINE ( 'NONE', #156838, #242684 ) ;
#255857 = CARTESIAN_POINT ( 'NONE',  ( -20.90000000000000213, 11.49641995933507843, -1.885425182446133885 ) ) ;
#255858 = CARTESIAN_POINT ( 'NONE',  ( -18.57399277249657032, 10.33112638556969465, -139.5901228926975080 ) ) ;
#255859 = EDGE_CURVE ( 'NONE', #55681, #119280, #229323, .T. ) ;
#255860 = ORIENTED_EDGE ( 'NONE', *, *, #106544, .F. ) ;
#255861 = FACE_OUTER_BOUND ( 'NONE', #114259, .T. ) ;
#255862 = ORIENTED_EDGE ( 'NONE', *, *, #194523, .F. ) ;
#255863 = CARTESIAN_POINT ( 'NONE',  ( -20.94999999999999929, 10.29270135741298731, -206.4573618871519045 ) ) ;
#255864 = ADVANCED_FACE ( 'NONE', ( #179520 ), #62127, .F. ) ;
#255865 = ORIENTED_EDGE ( 'NONE', *, *, #113348, .T. ) ;
#255866 = DIRECTION ( 'NONE',  ( -1.000000000000000000, 0.000000000000000000, 0.000000000000000000 ) ) ;
#255867 = TOROIDAL_SURFACE ( 'NONE', #205843, 6.258578643762700899, 0.1000000000000000056 ) ;
#255868 = VERTEX_POINT ( 'NONE', #165069 ) ;
#255869 = CARTESIAN_POINT ( 'NONE',  ( -23.49999999999994316, 85.52235250936193722, -34.45408804175119144 ) ) ;
#255870 = AXIS2_PLACEMENT_3D ( 'NONE', #138182, #61235, #202035 ) ;
#255871 = CARTESIAN_POINT ( 'NONE',  ( 18.59999999999999076, 64.35000000001221565, -148.2731074845243882 ) ) ;
#255872 = ORIENTED_EDGE ( 'NONE', *, *, #126501, .T. ) ;
#255873 = EDGE_CURVE ( 'NONE', #3432, #62026, #141650, .T. ) ;
#255874 = DIRECTION ( 'NONE',  ( 0.000000000000000000, 0.000000000000000000, -1.000000000000000000 ) ) ;
#255875 = CARTESIAN_POINT ( 'NONE',  ( -20.64999999999999858, 68.85000000001222986, -148.8731074845244109 ) ) ;
#255876 = DIRECTION ( 'NONE',  ( -0.000000000000000000, 0.9126074666063771490, 0.4088369013363281623 ) ) ;
#255877 = DIRECTION ( 'NONE',  ( -0.000000000000000000, -0.4721928772777341798, -0.8814952561688433885 ) ) ;
#255878 = CARTESIAN_POINT ( 'NONE',  ( 21.15000000000005187, 64.35000000001120668, -5.923107484524795296 ) ) ;
#255879 = EDGE_LOOP ( 'NONE', ( #128299, #26414, #51662, #93430, #103918, #159172, #168190, #19601, #227304, #64958, #39423, #87127 ) ) ;
#255880 = CARTESIAN_POINT ( 'NONE',  ( -18.47130263965444996, 85.47115558597597840, -129.8397027190475512 ) ) ;
#255881 = ORIENTED_EDGE ( 'NONE', *, *, #173357, .F. ) ;
#255883 = ORIENTED_EDGE ( 'NONE', *, *, #81399, .F. ) ;
#255882 = CARTESIAN_POINT ( 'NONE',  ( 21.14999999999999858, 67.21339244341174890, -90.77310748452437394 ) ) ;
#255884 = VECTOR ( 'NONE', #99773, 1000.000000000000000 ) ;
#255885 = ORIENTED_EDGE ( 'NONE', *, *, #210239, .T. ) ;
#255886 = STYLED_ITEM ( 'NONE', ( #218746 ), #197609 ) ;
#255887 = CARTESIAN_POINT ( 'NONE',  ( -22.39999999999999858, 75.90000000001273861, -211.3138870828977645 ) ) ;
#255888 = CARTESIAN_POINT ( 'NONE',  ( 14.22821877134047064, 66.54397173950468414, -188.5119094494587557 ) ) ;
#255889 = CYLINDRICAL_SURFACE ( 'NONE', #26501, 0.09999999999998898659 ) ;
#255890 = CYLINDRICAL_SURFACE ( 'NONE', #8301, 0.09999999999999939493 ) ;
#255891 = VERTEX_POINT ( 'NONE', #99928 ) ;
#255892 = CYLINDRICAL_SURFACE ( 'NONE', #64032, 0.1000000000000000472 ) ;
#255893 = LINE ( 'NONE', #35655, #231249 ) ;
#255894 = VERTEX_POINT ( 'NONE', #81641 ) ;
#255895 = EDGE_CURVE ( 'NONE', #256630, #28814, #46386, .T. ) ;
#255897 = VERTEX_POINT ( 'NONE', #25571 ) ;
#255896 = DIRECTION ( 'NONE',  ( -1.000000000000000000, 0.000000000000000000, 0.000000000000000000 ) ) ;
#255898 = CARTESIAN_POINT ( 'NONE',  ( 23.24999999999999289, 69.55000000001228955, -157.6731074845243938 ) ) ;
#255900 = AXIS2_PLACEMENT_3D ( 'NONE', #255332, #156324, #178448 ) ;
#255899 = CARTESIAN_POINT ( 'NONE',  ( 22.16821283564876666, 7.558973340791918183, -100.5000000000000284 ) ) ;
#255901 = ORIENTED_EDGE ( 'NONE', *, *, #210526, .F. ) ;
#255902 = CIRCLE ( 'NONE', #105894, 0.1000000000000028644 ) ;
#255903 = AXIS2_PLACEMENT_3D ( 'NONE', #232866, #212013, #34666 ) ;
#255904 = EDGE_CURVE ( 'NONE', #203005, #207677, #76161, .T. ) ;
#255905 = LINE ( 'NONE', #119029, #788 ) ;
#255906 = ORIENTED_EDGE ( 'NONE', *, *, #147158, .T. ) ;
#255907 = DIRECTION ( 'NONE',  ( 1.000000000000000000, -0.000000000000000000, -0.000000000000000000 ) ) ;
#255908 = COLOUR_RGB ( '', 0.72549020, 0.75294118, 0.79215686) ;
#255909 = DIRECTION ( 'NONE',  ( 0.000000000000000000, 6.982962677686266711E-15, -1.000000000000000000 ) ) ;
#255910 = CARTESIAN_POINT ( 'NONE',  ( 20.96077737575317457, 64.37609936600755134, -176.8823155274176315 ) ) ;
#255911 = EDGE_CURVE ( 'NONE', #92509, #201984, #162525, .T. ) ;
#255912 = FACE_OUTER_BOUND ( 'NONE', #137015, .T. ) ;
#255913 = EDGE_CURVE ( 'NONE', #45497, #219313, #223740, .T. ) ;
#255914 = CIRCLE ( 'NONE', #31159, 11.64999999999999325 ) ;
#255915 = CIRCLE ( 'NONE', #164405, 0.1000000000000052097 ) ;
#255916 = ORIENTED_EDGE ( 'NONE', *, *, #171910, .F. ) ;
#255917 = DIRECTION ( 'NONE',  ( 0.000000000000000000, -0.3738317757008748909, -0.9274965247785733613 ) ) ;
#255918 = AXIS2_PLACEMENT_3D ( 'NONE', #245174, #163087, #241332 ) ;
#255919 = CIRCLE ( 'NONE', #143545, 0.1000000000000028644 ) ;
#255920 = ORIENTED_EDGE ( 'NONE', *, *, #135086, .F. ) ;
#255921 = CARTESIAN_POINT ( 'NONE',  ( -17.11825945287481687, 9.950000000011167245, -188.3499999999999375 ) ) ;
#255922 = DIRECTION ( 'NONE',  ( 0.000000000000000000, 0.000000000000000000, 1.000000000000000000 ) ) ;
#255925 = ADVANCED_FACE ( 'NONE', ( #64678 ), #130329, .T. ) ;
#255924 = ORIENTED_EDGE ( 'NONE', *, *, #29301, .F. ) ;
#255923 = DIRECTION ( 'NONE',  ( -1.000000000000000000, 0.000000000000000000, 0.000000000000000000 ) ) ;
#255926 = CARTESIAN_POINT ( 'NONE',  ( -18.59999999999999787, 9.350000000000001421, -21.15000000000000213 ) ) ;
#255927 = LINE ( 'NONE', #77329, #40868 ) ;
#255928 = DIRECTION ( 'NONE',  ( -1.000000000000000000, -7.136802563874199107E-16, -1.554319503706929991E-16 ) ) ;
#255929 = CARTESIAN_POINT ( 'NONE',  ( -18.40000000000000213, 70.35000000001181775, -82.17310748452435121 ) ) ;
#255930 = CARTESIAN_POINT ( 'NONE',  ( 15.48841904831874849, 8.561580951681223794, -12.64999999999999858 ) ) ;
#255931 = VECTOR ( 'NONE', #135324, 1000.000000000000000 ) ;
#255932 = EDGE_CURVE ( 'NONE', #208712, #217297, #21716, .T. ) ;
#255933 = DIRECTION ( 'NONE',  ( 0.000000000000000000, 0.000000000000000000, 1.000000000000000000 ) ) ;
#255934 = VECTOR ( 'NONE', #72848, 1000.000000000000000 ) ;
#255935 = ADVANCED_FACE ( 'NONE', ( #180792 ), #242759, .F. ) ;
#255936 = CARTESIAN_POINT ( 'NONE',  ( -18.46946985241234529, 85.50931722872354612, -129.5364449190244045 ) ) ;
#255938 = ORIENTED_EDGE ( 'NONE', *, *, #234855, .F. ) ;
#255937 = DIRECTION ( 'NONE',  ( 0.000000000000000000, 0.000000000000000000, -1.000000000000000000 ) ) ;
#255939 = AXIS2_PLACEMENT_3D ( 'NONE', #199877, #44642, #203712 ) ;
#255940 = VECTOR ( 'NONE', #206296, 999.9999999999998863 ) ;
#255942 = EDGE_CURVE ( 'NONE', #209999, #198367, #102491, .T. ) ;
#255941 = CYLINDRICAL_SURFACE ( 'NONE', #68378, 0.09999999999998898659 ) ;
#255943 = AXIS2_PLACEMENT_3D ( 'NONE', #157273, #94696, #38584 ) ;
#255945 = ADVANCED_FACE ( 'NONE', ( #45121 ), #242031, .T. ) ;
#255944 = FACE_OUTER_BOUND ( 'NONE', #173275, .T. ) ;
#255946 = CARTESIAN_POINT ( 'NONE',  ( 22.39999999999999147, 68.20922040163857503, -103.0231074845243597 ) ) ;
#255947 = ADVANCED_FACE ( 'NONE', ( #183360 ), #204181, .F. ) ;
#255948 = AXIS2_PLACEMENT_3D ( 'NONE', #156659, #154104, #159210 ) ;
#255950 = EDGE_LOOP ( 'NONE', ( #148091, #28091, #253417, #230114 ) ) ;
#255949 = AXIS2_PLACEMENT_3D ( 'NONE', #140499, #223885, #124812 ) ;
#255951 = CARTESIAN_POINT ( 'NONE',  ( -21.07928932188134041, 1.115600667400684642E-11, -167.4999999999999716 ) ) ;
#255952 = CARTESIAN_POINT ( 'NONE',  ( -18.59999999999999787, 9.150000000011157653, -188.6499999999999488 ) ) ;
#255953 = ORIENTED_EDGE ( 'NONE', *, *, #69411, .T. ) ;
#255954 = DIRECTION ( 'NONE',  ( 0.000000000000000000, 0.2128009952263604510, -0.9770955615653315052 ) ) ;
#255955 = CARTESIAN_POINT ( 'NONE',  ( -23.25000000000000355, 10.04999999999998295, -20.75000000000000000 ) ) ;
#255956 = ORIENTED_EDGE ( 'NONE', *, *, #19152, .F. ) ;
#255957 = CARTESIAN_POINT ( 'NONE',  ( -18.38817693311004575, 11.48149151591092476, -124.7500000000000284 ) ) ;
#255958 = ADVANCED_FACE ( 'NONE', ( #63384 ), #65969, .T. ) ;
#255959 = ORIENTED_EDGE ( 'NONE', *, *, #34130, .F. ) ;
#255960 = EDGE_CURVE ( 'NONE', #55997, #239916, #101055, .T. ) ;
#255961 = CARTESIAN_POINT ( 'NONE',  ( -21.98333005346336932, 76.00000000001243450, -177.3971828135810256 ) ) ;
#255963 = ORIENTED_EDGE ( 'NONE', *, *, #46683, .F. ) ;
#255962 = CARTESIAN_POINT ( 'NONE',  ( 21.14999999999999858, 6.540656951712402467, -134.0000000000000284 ) ) ;
#255964 = CARTESIAN_POINT ( 'NONE',  ( -20.00857864376270001, 66.65000000001187175, -90.77310748452437394 ) ) ;
#255965 = ORIENTED_EDGE ( 'NONE', *, *, #198863, .F. ) ;
#255966 = CIRCLE ( 'NONE', #147698, 1.749999999999999778 ) ;
#255967 = VERTEX_POINT ( 'NONE', #825 ) ;
#255968 = AXIS2_PLACEMENT_3D ( 'NONE', #191572, #151147, #12937 ) ;
#255971 = EDGE_CURVE ( 'NONE', #144465, #167927, #80364, .T. ) ;
#255970 = ORIENTED_EDGE ( 'NONE', *, *, #214153, .T. ) ;
#255969 = ORIENTED_EDGE ( 'NONE', *, *, #98558, .T. ) ;
#255972 = CARTESIAN_POINT ( 'NONE',  ( 18.45036689428336274, 85.49018414334089755, -129.5104116570378778 ) ) ;
#255973 = ORIENTED_EDGE ( 'NONE', *, *, #230944, .T. ) ;
#255974 = VECTOR ( 'NONE', #1646, 1000.000000000000000 ) ;
#255975 = DIRECTION ( 'NONE',  ( 0.000000000000000000, 0.4999999999999689138, -0.8660254037844565822 ) ) ;
#255976 = ORIENTED_EDGE ( 'NONE', *, *, #83849, .T. ) ;
#255977 = AXIS2_PLACEMENT_3D ( 'NONE', #155661, #93072, #10980 ) ;
#255978 = CIRCLE ( 'NONE', #176960, 0.5000000000000004441 ) ;
#255979 = ORIENTED_EDGE ( 'NONE', *, *, #210839, .T. ) ;
#255980 = DIRECTION ( 'NONE',  ( -1.000000000000000000, 2.952720810173289112E-16, 2.061873921506763405E-30 ) ) ;
#255981 = CARTESIAN_POINT ( 'NONE',  ( -20.90000000000000213, -11.65000000000000036, -15.00000000000000000 ) ) ;
#255982 = DIRECTION ( 'NONE',  ( 0.000000000000000000, 0.000000000000000000, -1.000000000000000000 ) ) ;
#255983 = DIRECTION ( 'NONE',  ( 0.000000000000000000, 0.000000000000000000, -1.000000000000000000 ) ) ;
#255984 = VERTEX_POINT ( 'NONE', #140357 ) ;
#255985 = DIRECTION ( 'NONE',  ( 0.000000000000000000, 0.000000000000000000, -1.000000000000000000 ) ) ;
#255986 = CARTESIAN_POINT ( 'NONE',  ( -18.49719636458545224, -9.446365359216978064, -74.07161386988313723 ) ) ;
#255987 = CARTESIAN_POINT ( 'NONE',  ( 20.94999999999999929, 36.65892442174935439, -249.5511627012433848 ) ) ;
#255988 = CIRCLE ( 'NONE', #72925, 0.09999999999999971412 ) ;
#255990 = ORIENTED_EDGE ( 'NONE', *, *, #208584, .F. ) ;
#255989 = EDGE_CURVE ( 'NONE', #189995, #133767, #196972, .T. ) ;
#255991 = LINE ( 'NONE', #137368, #87866 ) ;
#255992 = CARTESIAN_POINT ( 'NONE',  ( -20.94999999999999929, 87.48912529308842068, -166.9231074845242802 ) ) ;
#255993 = CARTESIAN_POINT ( 'NONE',  ( -13.40000000000000213, -11.65000000000000036, 17.70000000000000284 ) ) ;
#255994 = AXIS2_PLACEMENT_3D ( 'NONE', #210298, #31681, #186889 ) ;
#255995 = EDGE_CURVE ( 'NONE', #205943, #79099, #109478, .T. ) ;
#255996 = EDGE_LOOP ( 'NONE', ( #247808, #249570, #106921, #167118 ) ) ;
#255997 = ORIENTED_EDGE ( 'NONE', *, *, #215082, .T. ) ;
#255998 = ORIENTED_EDGE ( 'NONE', *, *, #222824, .T. ) ;
#255999 = CYLINDRICAL_SURFACE ( 'NONE', #68048, 0.09999999999999939493 ) ;
#256000 = ORIENTED_EDGE ( 'NONE', *, *, #226458, .T. ) ;
#256001 = ORIENTED_EDGE ( 'NONE', *, *, #23461, .T. ) ;
#256002 = ADVANCED_FACE ( 'NONE', ( #187220 ), #163662, .T. ) ;
#256003 = CARTESIAN_POINT ( 'NONE',  ( -16.87036670365548474, 9.989418819312801290, -154.9795601173020714 ) ) ;
#256004 = ORIENTED_EDGE ( 'NONE', *, *, #229667, .F. ) ;
#256005 = AXIS2_PLACEMENT_3D ( 'NONE', #109646, #69267, #146207 ) ;
#256006 = EDGE_LOOP ( 'NONE', ( #246727, #131051, #236492, #141144 ) ) ;
#256007 = CARTESIAN_POINT ( 'NONE',  ( -18.59999999999999787, 11.64999999999999680, -12.14999999999999680 ) ) ;
#256008 = ADVANCED_FACE ( 'NONE', ( #185912 ), #146755, .F. ) ;
#256009 = LINE ( 'NONE', #59110, #98221 ) ;
#256010 = ORIENTED_EDGE ( 'NONE', *, *, #136528, .F. ) ;
#256011 = ORIENTED_EDGE ( 'NONE', *, *, #42712, .T. ) ;
#256012 = ORIENTED_EDGE ( 'NONE', *, *, #149128, .F. ) ;
#256013 = TOROIDAL_SURFACE ( 'NONE', #6451, 12.77499999999999858, 0.1000000000000000056 ) ;
#256014 = ADVANCED_FACE ( 'NONE', ( #253260 ), #201080, .F. ) ;
#256015 = VECTOR ( 'NONE', #169051, 1000.000000000000000 ) ;
#256017 = EDGE_CURVE ( 'NONE', #39426, #101907, #234385, .T. ) ;
#256016 = CARTESIAN_POINT ( 'NONE',  ( 20.94999999999999574, 74.75000000001261924, -195.5231074845243597 ) ) ;
#256018 = CARTESIAN_POINT ( 'NONE',  ( 22.10000000000000853, 3.461118860469513336, 28.84309995045515507 ) ) ;
#256019 = EDGE_CURVE ( 'NONE', #94806, #218203, #151202, .T. ) ;
#256020 = CARTESIAN_POINT ( 'NONE',  ( -21.14999999999999858, 6.540656951712397138, -67.00000000000004263 ) ) ;
#256021 = LINE ( 'NONE', #157002, #163976 ) ;
#256022 = CARTESIAN_POINT ( 'NONE',  ( -18.39999999999999858, 11.47316190337362762, -109.8259460668080152 ) ) ;
#256023 = DIRECTION ( 'NONE',  ( -0.000000000000000000, -0.8660254037844420383, 0.4999999999999943379 ) ) ;
#256024 = FACE_OUTER_BOUND ( 'NONE', #210422, .T. ) ;
#256026 = LINE ( 'NONE', #54030, #32827 ) ;
#256025 = CARTESIAN_POINT ( 'NONE',  ( 21.14999999999999503, 76.00000000001169553, -76.06376443622556849 ) ) ;
#256027 = CARTESIAN_POINT ( 'NONE',  ( -20.94999999999999929, 70.22659352830977753, -197.9852579278363578 ) ) ;
#256028 = LINE ( 'NONE', #159565, #190303 ) ;
#256029 = DIRECTION ( 'NONE',  ( -1.000000000000000000, 0.000000000000000000, 0.000000000000000000 ) ) ;
#256030 = DIRECTION ( 'NONE',  ( -0.7071067811865475727, 0.2890913453342130457, -0.6453109281988448354 ) ) ;
#256031 = EDGE_CURVE ( 'NONE', #99810, #50561, #184488, .T. ) ;
#256032 = AXIS2_PLACEMENT_3D ( 'NONE', #114982, #194551, #175007 ) ;
#256033 = EDGE_CURVE ( 'NONE', #91448, #52101, #167781, .T. ) ;
#256034 = ORIENTED_EDGE ( 'NONE', *, *, #93278, .T. ) ;
#256035 = B_SPLINE_CURVE_WITH_KNOTS ( 'NONE', 3,
 ( #240392, #61747, #46027, #141286, #121742, #181701 ),
 .UNSPECIFIED., .F., .F.,
 ( 4, 2, 4 ),
 ( 0.000000000000000000, 0.0002113392456166019308, 0.0004226784912332038615 ),
 .UNSPECIFIED. ) ;
#256036 = EDGE_CURVE ( 'NONE', #121164, #65499, #88621, .T. ) ;
#256037 = CIRCLE ( 'NONE', #51888, 0.09999999999999939493 ) ;
#256039 = ORIENTED_EDGE ( 'NONE', *, *, #198169, .F. ) ;
#256038 = DIRECTION ( 'NONE',  ( 0.000000000000000000, 1.776356839400277286E-15, -1.000000000000000000 ) ) ;
#256040 = ADVANCED_FACE ( 'NONE', ( #74680 ), #211590, .T. ) ;
#256041 = CARTESIAN_POINT ( 'NONE',  ( 21.05000000000000071, 70.15000000001252545, -180.1556047088023149 ) ) ;
#256042 = CYLINDRICAL_SURFACE ( 'NONE', #144587, 0.09999999999999881206 ) ;
#256043 = EDGE_CURVE ( 'NONE', #125, #57260, #63697, .T. ) ;
#256044 = EDGE_LOOP ( 'NONE', ( #21971, #36100, #85762, #218909 ) ) ;
#256045 = CARTESIAN_POINT ( 'NONE',  ( 20.27550659511088682, 10.97336462231075416, -208.0769506682813130 ) ) ;
#256046 = CARTESIAN_POINT ( 'NONE',  ( -16.92570016628985385, 66.04121104227242256, -157.4024568144854470 ) ) ;
#256047 = EDGE_LOOP ( 'NONE', ( #202357, #150136, #20293, #168266 ) ) ;
#256049 = CARTESIAN_POINT ( 'NONE',  ( -18.53317502108577486, 10.32263460347359363, -206.5605957968671760 ) ) ;
#256048 = CONICAL_SURFACE ( 'NONE', #181126, 4.049999999999998046, 0.7853981633974604915 ) ;
#256050 = VECTOR ( 'NONE', #86304, 1000.000000000000000 ) ;
#256051 = DIRECTION ( 'NONE',  ( -0.7071067811865389130, 0.1504730267678074940, -0.6909108974501321221 ) ) ;
#256052 = ADVANCED_FACE ( 'NONE', ( #134586 ), #112495, .F. ) ;
#256053 = DIRECTION ( 'NONE',  ( 0.000000000000000000, 0.000000000000000000, 1.000000000000000000 ) ) ;
#256055 = EDGE_LOOP ( 'NONE', ( #24800, #174889, #139065, #95287 ) ) ;
#256054 = DIRECTION ( 'NONE',  ( 1.000000000000000000, -2.952720810173289112E-16, -2.061873921506763405E-30 ) ) ;
#256057 = ORIENTED_EDGE ( 'NONE', *, *, #27910, .F. ) ;
#256056 = DIRECTION ( 'NONE',  ( 1.000000000000000000, -1.145314911736513911E-16, 3.106193895438251633E-17 ) ) ;
#256058 = CARTESIAN_POINT ( 'NONE',  ( -21.05000000000000426, 10.15197506655037429, -228.1685576039200498 ) ) ;
#256059 = DIRECTION ( 'NONE',  ( -1.646408749285562691E-14, 1.000000000000000000, 0.000000000000000000 ) ) ;
#256060 = CARTESIAN_POINT ( 'NONE',  ( -15.75000000000000711, 9.350000000011142731, -184.0215193718251214 ) ) ;
#256061 = EDGE_CURVE ( 'NONE', #8721, #66884, #105358, .T. ) ;
#256063 = CARTESIAN_POINT ( 'NONE',  ( -20.94999999999999929, 72.91131461869652242, -214.9116992594219369 ) ) ;
#256062 = DIRECTION ( 'NONE',  ( 0.000000000000000000, 0.000000000000000000, 1.000000000000000000 ) ) ;
#256064 = DIRECTION ( 'NONE',  ( 0.000000000000000000, 0.000000000000000000, -1.000000000000000000 ) ) ;
#256065 = CIRCLE ( 'NONE', #139409, 0.09999999999999939493 ) ;
#256066 = FACE_OUTER_BOUND ( 'NONE', #176365, .T. ) ;
#256067 = VECTOR ( 'NONE', #41761, 1000.000000000000000 ) ;
#256068 = DIRECTION ( 'NONE',  ( 0.000000000000000000, 0.2128009952263604232, -0.9770955615653316162 ) ) ;
#256069 = ORIENTED_EDGE ( 'NONE', *, *, #170782, .F. ) ;
#256070 = VECTOR ( 'NONE', #104420, 1000.000000000000000 ) ;
#256071 = CYLINDRICAL_SURFACE ( 'NONE', #43076, 11.80000000000000426 ) ;
#256072 = ORIENTED_EDGE ( 'NONE', *, *, #100825, .F. ) ;
#256073 = VERTEX_POINT ( 'NONE', #47666 ) ;
#256074 = EDGE_CURVE ( 'NONE', #73136, #83407, #86793, .T. ) ;
#256075 = DIRECTION ( 'NONE',  ( 1.000000000000000000, -0.000000000000000000, -0.000000000000000000 ) ) ;
#256076 = DIRECTION ( 'NONE',  ( 0.000000000000000000, -1.000000000000000000, 0.000000000000000000 ) ) ;
#256077 = ORIENTED_EDGE ( 'NONE', *, *, #209196, .F. ) ;
#256078 = ORIENTED_EDGE ( 'NONE', *, *, #123917, .F. ) ;
#256079 = EDGE_CURVE ( 'NONE', #168532, #211446, #138675, .T. ) ;
#256080 = ORIENTED_EDGE ( 'NONE', *, *, #249901, .F. ) ;
#256081 = AXIS2_PLACEMENT_3D ( 'NONE', #30926, #55548, #50427 ) ;
#256082 = ORIENTED_EDGE ( 'NONE', *, *, #131545, .T. ) ;
#256083 = VECTOR ( 'NONE', #191652, 1000.000000000000000 ) ;
#256084 = DIRECTION ( 'NONE',  ( -1.000000000000000000, -0.000000000000000000, 0.000000000000000000 ) ) ;
#256085 = CARTESIAN_POINT ( 'NONE',  ( 21.05000000000000071, 10.47338541492405817, -41.07865446424855094 ) ) ;
#256086 = DIRECTION ( 'NONE',  ( 0.000000000000000000, -0.9999631594459056361, -0.008583690987124413183 ) ) ;
#256087 = VECTOR ( 'NONE', #145590, 1000.000000000000000 ) ;
#256088 = CARTESIAN_POINT ( 'NONE',  ( -20.94999999999999929, 7.128833340093095217, -233.7327013124392749 ) ) ;
#256089 = DIRECTION ( 'NONE',  ( -1.000000000000000000, -0.000000000000000000, -0.000000000000000000 ) ) ;
#256090 = DIRECTION ( 'NONE',  ( 0.000000000000000000, 0.2617529984165033463, 0.9651348961777156399 ) ) ;
#256091 = DIRECTION ( 'NONE',  ( 1.000000000000000000, 0.000000000000000000, 0.000000000000000000 ) ) ;
#256093 = ORIENTED_EDGE ( 'NONE', *, *, #239539, .T. ) ;
#256092 = DIRECTION ( 'NONE',  ( 1.000000000000000000, 0.000000000000000000, 0.000000000000000000 ) ) ;
#256095 = DIRECTION ( 'NONE',  ( 0.000000000000000000, 1.000000000000000000, 0.000000000000000000 ) ) ;
#256094 = CARTESIAN_POINT ( 'NONE',  ( -22.57848426163147693, -0.004264329283117146777, 11.75005830689033282 ) ) ;
#256096 = CARTESIAN_POINT ( 'NONE',  ( -18.50000000000000000, 64.35000000001238618, -169.9231074845244507 ) ) ;
#256097 = ORIENTED_EDGE ( 'NONE', *, *, #2277, .T. ) ;
#256098 = CARTESIAN_POINT ( 'NONE',  ( 23.15000000000000213, 69.16514130714681130, -247.7543978865853660 ) ) ;
#256099 = CARTESIAN_POINT ( 'NONE',  ( -23.25000000000000355, 5.650000000011139001, -54.35000000000000142 ) ) ;
#256100 = VECTOR ( 'NONE', #21239, 1000.000000000000000 ) ;
#256102 = VERTEX_POINT ( 'NONE', #75928 ) ;
#256101 = VECTOR ( 'NONE', #133548, 1000.000000000000000 ) ;
#256104 = CARTESIAN_POINT ( 'NONE',  ( -21.37071067811865532, 62.64842427125413593, -221.9196913089517125 ) ) ;
#256103 = LINE ( 'NONE', #237889, #145338 ) ;
#256105 = CARTESIAN_POINT ( 'NONE',  ( -20.94999999999999929, 74.83729825007408465, -128.4231074845243086 ) ) ;
#256106 = DIRECTION ( 'NONE',  ( 0.000000000000000000, -7.086529944415886769E-15, 1.000000000000000000 ) ) ;
#256107 = EDGE_LOOP ( 'NONE', ( #65455, #208530, #27390, #138908 ) ) ;
#256108 = VERTEX_POINT ( 'NONE', #7266 ) ;
#256109 = VECTOR ( 'NONE', #201495, 1000.000000000000000 ) ;
#256110 = CARTESIAN_POINT ( 'NONE',  ( -21.10000000000000142, 0.000000000000000000, 4.100000000000000533 ) ) ;
#256111 = CIRCLE ( 'NONE', #75652, 12.77500000000000036 ) ;
#256112 = CARTESIAN_POINT ( 'NONE',  ( -15.75000000000000355, 62.10905854918435409, -217.1108499610990918 ) ) ;
#256113 = CARTESIAN_POINT ( 'NONE',  ( 20.85000000000000142, 87.65000000001172964, -72.42310748452422331 ) ) ;
#256114 = LINE ( 'NONE', #56659, #192776 ) ;
#256115 = VERTEX_POINT ( 'NONE', #245898 ) ;
#256116 = AXIS2_PLACEMENT_3D ( 'NONE', #124759, #144282, #162607 ) ;
#256117 = VECTOR ( 'NONE', #201459, 1000.000000000000000 ) ;
#256118 = DIRECTION ( 'NONE',  ( 1.000000000000000000, 0.000000000000000000, 0.000000000000000000 ) ) ;
#256119 = EDGE_CURVE ( 'NONE', #162201, #174581, #209436, .T. ) ;
#256120 = DIRECTION ( 'NONE',  ( 0.000000000000000000, 0.2617529984165031243, 0.9651348961777157509 ) ) ;
#256121 = CARTESIAN_POINT ( 'NONE',  ( -21.05000000000000071, 76.00000000001213607, -136.5231074845243313 ) ) ;
#256122 = DIRECTION ( 'NONE',  ( 1.000000000000000000, 0.000000000000000000, 0.000000000000000000 ) ) ;
#256124 = ORIENTED_EDGE ( 'NONE', *, *, #58664, .T. ) ;
#256123 = DIRECTION ( 'NONE',  ( 0.000000000000000000, 0.000000000000000000, -1.000000000000000000 ) ) ;
#256125 = CARTESIAN_POINT ( 'NONE',  ( 21.14999999999999858, 64.25000000001185185, -90.87310748452438247 ) ) ;
#256126 = DIRECTION ( 'NONE',  ( -0.000000000000000000, -0.1332476588733589318, -0.9910827722268049644 ) ) ;
#256127 = FACE_OUTER_BOUND ( 'NONE', #72501, .T. ) ;
#256128 = CARTESIAN_POINT ( 'NONE',  ( -23.25000000000000355, 64.25000000001153921, -48.67310748452440805 ) ) ;
#256129 = EDGE_CURVE ( 'NONE', #158360, #46992, #236274, .T. ) ;
#256130 = LINE ( 'NONE', #65703, #112980 ) ;
#256132 = VERTEX_POINT ( 'NONE', #60195 ) ;
#256131 = CARTESIAN_POINT ( 'NONE',  ( -20.00857864376270001, 66.85000000001186038, -90.67310748452436542 ) ) ;
#256133 = DIRECTION ( 'NONE',  ( -1.000000000000000000, 0.000000000000000000, 0.000000000000000000 ) ) ;
#256134 = DIRECTION ( 'NONE',  ( 0.000000000000000000, 6.982962677686266711E-15, -1.000000000000000000 ) ) ;
#256135 = ADVANCED_FACE ( 'NONE', ( #77196 ), #219275, .T. ) ;
#256136 = ORIENTED_EDGE ( 'NONE', *, *, #201811, .T. ) ;
#256137 = CARTESIAN_POINT ( 'NONE',  ( 18.54999999999999716, 8.750000000011182166, -154.8500000000000227 ) ) ;
#256138 = AXIS2_PLACEMENT_3D ( 'NONE', #222581, #180921, #240896 ) ;
#256139 = CARTESIAN_POINT ( 'NONE',  ( 21.14999999999999147, 76.00000000001242029, -176.5637644362255969 ) ) ;
#256140 = CARTESIAN_POINT ( 'NONE',  ( -20.54999999999999716, 7.150000000011155876, -45.85000000000000142 ) ) ;
#256142 = CIRCLE ( 'NONE', #185479, 0.5000000000000014433 ) ;
#256141 = CARTESIAN_POINT ( 'NONE',  ( -20.64999999999999858, 2.000000000011154189, -187.7753780772378889 ) ) ;
#256143 = AXIS2_PLACEMENT_3D ( 'NONE', #236420, #216850, #38236 ) ;
#256144 = CARTESIAN_POINT ( 'NONE',  ( 5.900000000000059863, 64.65000000001120384, -26.02310748452479316 ) ) ;
#256145 = EDGE_CURVE ( 'NONE', #133216, #80211, #118919, .T. ) ;
#256146 = DIRECTION ( 'NONE',  ( 0.000000000000000000, 0.000000000000000000, 1.000000000000000000 ) ) ;
#256147 = VERTEX_POINT ( 'NONE', #17250 ) ;
#256148 = ORIENTED_EDGE ( 'NONE', *, *, #75208, .T. ) ;
#256149 = EDGE_CURVE ( 'NONE', #133700, #150237, #36834, .T. ) ;
#256150 = DIRECTION ( 'NONE',  ( 0.000000000000000000, 0.000000000000000000, 1.000000000000000000 ) ) ;
#256151 = AXIS2_PLACEMENT_3D ( 'NONE', #48011, #109262, #28507 ) ;
#256152 = CARTESIAN_POINT ( 'NONE',  ( -18.39999999999999858, 46.96039402156217335, -255.3459641718773128 ) ) ;
#256153 = ADVANCED_FACE ( 'NONE', ( #40690 ), #159334, .T. ) ;
#256154 = DIRECTION ( 'NONE',  ( 0.000000000000000000, 0.000000000000000000, -1.000000000000000000 ) ) ;
#256155 = FACE_OUTER_BOUND ( 'NONE', #160317, .T. ) ;
#256156 = ORIENTED_EDGE ( 'NONE', *, *, #152678, .F. ) ;
#256157 = EDGE_CURVE ( 'NONE', #243786, #5738, #80224, .T. ) ;
#256159 = AXIS2_PLACEMENT_3D ( 'NONE', #150958, #148393, #149697 ) ;
#256158 = DIRECTION ( 'NONE',  ( 1.000000000000000000, 0.000000000000000000, 0.000000000000000000 ) ) ;
#256160 = DIRECTION ( 'NONE',  ( 0.000000000000000000, -0.9976611540403004241, -0.06835365183350541884 ) ) ;
#256161 = EDGE_CURVE ( 'NONE', #108178, #139621, #178911, .T. ) ;
#256162 = VECTOR ( 'NONE', #28532, 1000.000000000000000 ) ;
#256163 = CARTESIAN_POINT ( 'NONE',  ( -23.15000000000000213, 76.00000000001213607, -136.5231074845243313 ) ) ;
#256164 = LINE ( 'NONE', #93302, #240130 ) ;
#256165 = EDGE_LOOP ( 'NONE', ( #188206, #47567, #148380, #227194 ) ) ;
#256166 = CARTESIAN_POINT ( 'NONE',  ( -23.25000000000000000, 1.115600667400684642E-11, -208.8999999999999488 ) ) ;
#256167 = ORIENTED_EDGE ( 'NONE', *, *, #135861, .T. ) ;
#256168 = ORIENTED_EDGE ( 'NONE', *, *, #119328, .F. ) ;
#256169 = CARTESIAN_POINT ( 'NONE',  ( -21.14999999999999858, 1.115527483754041871E-11, -26.95934304829875927 ) ) ;
#256170 = CARTESIAN_POINT ( 'NONE',  ( -16.98495255085918032, 65.99443563401710833, -90.38849027830387683 ) ) ;
#256171 = CARTESIAN_POINT ( 'NONE',  ( 20.95000000000005258, 64.35000000001119247, -6.023107484524794941 ) ) ;
#256172 = ORIENTED_EDGE ( 'NONE', *, *, #83722, .T. ) ;
#256173 = LINE ( 'NONE', #253660, #232227 ) ;
#256174 = CARTESIAN_POINT ( 'NONE',  ( -22.50000000000000000, 76.00000000001203659, -114.6726782920691221 ) ) ;
#256175 = CARTESIAN_POINT ( 'NONE',  ( -23.25000000000000000, 11.75000000001115552, -122.2500000000000284 ) ) ;
#256176 = VERTEX_POINT ( 'NONE', #1506 ) ;
#256177 = EDGE_CURVE ( 'NONE', #60099, #84586, #213727, .T. ) ;
#256178 = DIRECTION ( 'NONE',  ( -1.000000000000000000, 0.000000000000000000, 0.000000000000000000 ) ) ;
#256180 = ORIENTED_EDGE ( 'NONE', *, *, #68692, .F. ) ;
#256179 = CARTESIAN_POINT ( 'NONE',  ( 18.49999999999999289, 65.58283456529579780, -145.1731074851066410 ) ) ;
#256181 = CARTESIAN_POINT ( 'NONE',  ( 21.05000000000000071, 88.41227409416113403, -39.02310748452423894 ) ) ;
#256182 = CYLINDRICAL_SURFACE ( 'NONE', #39811, 0.09999999999999939493 ) ;
#256183 = AXIS2_PLACEMENT_3D ( 'NONE', #250340, #69161, #194250 ) ;
#256184 = CIRCLE ( 'NONE', #68836, 0.2000000000000057288 ) ;
#256185 = ORIENTED_EDGE ( 'NONE', *, *, #16035, .F. ) ;
#256186 = CARTESIAN_POINT ( 'NONE',  ( -16.77902162784673834, 9.946419257218996890, -79.66199124406939802 ) ) ;
#256188 = EDGE_CURVE ( 'NONE', #177428, #34297, #199744, .T. ) ;
#256187 = CARTESIAN_POINT ( 'NONE',  ( -16.81930730667006557, 66.06300193113784758, -90.29633975398620294 ) ) ;
#256189 = FACE_OUTER_BOUND ( 'NONE', #47188, .T. ) ;
#256190 = ORIENTED_EDGE ( 'NONE', *, *, #201565, .T. ) ;
#256191 = CARTESIAN_POINT ( 'NONE',  ( 18.59999999999999076, 6.450000000011156587, -110.5170271704400591 ) ) ;
#256192 = DIRECTION ( 'NONE',  ( 0.000000000000000000, 1.000000000000000000, 6.982962677686266711E-15 ) ) ;
#256193 = LINE ( 'NONE', #118037, #184852 ) ;
#256194 = ORIENTED_EDGE ( 'NONE', *, *, #64657, .T. ) ;
#256195 = ORIENTED_EDGE ( 'NONE', *, *, #185926, .F. ) ;
#256196 = EDGE_CURVE ( 'NONE', #142241, #221915, #67986, .T. ) ;
#256197 = VECTOR ( 'NONE', #145891, 1000.000000000000000 ) ;
#256198 = ORIENTED_EDGE ( 'NONE', *, *, #189882, .F. ) ;
#256199 = DIRECTION ( 'NONE',  ( -1.000000000000000000, 0.000000000000000000, 0.000000000000000000 ) ) ;
#256200 = CARTESIAN_POINT ( 'NONE',  ( 18.49999999999999289, 11.65000000001115588, -167.5000000000000284 ) ) ;
#256203 = ADVANCED_FACE ( 'NONE', ( #141041 ), #215427, .F. ) ;
#256202 = ORIENTED_EDGE ( 'NONE', *, *, #200290, .T. ) ;
#256201 = CARTESIAN_POINT ( 'NONE',  ( -20.94999999999999929, 10.71906255309368383, -222.4921384173655383 ) ) ;
#256204 = CARTESIAN_POINT ( 'NONE',  ( 18.50000000000000000, 85.50000000001222134, -148.2731074845242460 ) ) ;
#256205 = DIRECTION ( 'NONE',  ( -0.000000000000000000, 1.000000000000000000, 8.717686153663073805E-15 ) ) ;
#256206 = CYLINDRICAL_SURFACE ( 'NONE', #212934, 0.1000000000000028644 ) ;
#256207 = CARTESIAN_POINT ( 'NONE',  ( -18.50000000000000000, 85.41908450282495835, -62.69319967749883915 ) ) ;
#256208 = CARTESIAN_POINT ( 'NONE',  ( -20.64999999999999858, 67.23127455305835554, -235.8551265064784559 ) ) ;
#256209 = EDGE_CURVE ( 'NONE', #77135, #26148, #9709, .T. ) ;
#256210 = FACE_OUTER_BOUND ( 'NONE', #111411, .T. ) ;
#256211 = EDGE_CURVE ( 'NONE', #155242, #219674, #156773, .T. ) ;
#256213 = ORIENTED_EDGE ( 'NONE', *, *, #102321, .F. ) ;
#256212 = DIRECTION ( 'NONE',  ( 0.000000000000000000, 0.9908441862701605762, 0.1350103645451835310 ) ) ;
#256215 = ORIENTED_EDGE ( 'NONE', *, *, #157523, .F. ) ;
#256214 = CARTESIAN_POINT ( 'NONE',  ( 20.94999999999999929, 5.000000000011153745, -188.5947339810868755 ) ) ;
#256217 = CARTESIAN_POINT ( 'NONE',  ( -16.89935556175725395, 51.17198062720201790, -232.1466667825101808 ) ) ;
#256216 = FACE_OUTER_BOUND ( 'NONE', #106978, .T. ) ;
#256219 = ORIENTED_EDGE ( 'NONE', *, *, #89948, .F. ) ;
#256218 = CARTESIAN_POINT ( 'NONE',  ( 18.59999999999999787, -8.350000000000004974, 10.52591260281975138 ) ) ;
#256220 = EDGE_LOOP ( 'NONE', ( #82889, #207313, #142958, #217783 ) ) ;
#256221 = FACE_OUTER_BOUND ( 'NONE', #161421, .T. ) ;
#256222 = CARTESIAN_POINT ( 'NONE',  ( 21.14999999999999858, 6.540656951701244282, -0.09999999999999939493 ) ) ;
#256223 = AXIS2_PLACEMENT_3D ( 'NONE', #189675, #253486, #231381 ) ;
#256224 = AXIS2_PLACEMENT_3D ( 'NONE', #5036, #162886, #48038 ) ;
#256226 = EDGE_CURVE ( 'NONE', #255048, #50561, #117618, .T. ) ;
#256225 = CARTESIAN_POINT ( 'NONE',  ( -23.25000000000000000, -0.09999999998884338825, -155.8504291924551808 ) ) ;
#256227 = CYLINDRICAL_SURFACE ( 'NONE', #197055, 0.09999999999998898659 ) ;
#256228 = DIRECTION ( 'NONE',  ( 1.000000000000000000, -0.000000000000000000, -0.000000000000000000 ) ) ;
#256229 = CARTESIAN_POINT ( 'NONE',  ( -16.84419801905645997, 66.05000000001201954, -115.6925973307464091 ) ) ;
#256230 = ORIENTED_EDGE ( 'NONE', *, *, #75532, .F. ) ;
#256231 = ORIENTED_EDGE ( 'NONE', *, *, #10075, .F. ) ;
#256232 = CARTESIAN_POINT ( 'NONE',  ( -23.15000000000000213, 64.35000000001249987, -177.0379132551784096 ) ) ;
#256233 = AXIS2_PLACEMENT_3D ( 'NONE', #9732, #129687, #8468 ) ;
#256234 = AXIS2_PLACEMENT_3D ( 'NONE', #149534, #226449, #165218 ) ;
#256235 = VERTEX_POINT ( 'NONE', #18520 ) ;
#256236 = DIRECTION ( 'NONE',  ( 0.000000000000000000, 0.000000000000000000, 1.000000000000000000 ) ) ;
#256237 = CARTESIAN_POINT ( 'NONE',  ( 18.50000324121758055, 68.00468331834500191, -224.2298952291171474 ) ) ;
#256238 = AXIS2_PLACEMENT_3D ( 'NONE', #86485, #6975, #241738 ) ;
#256239 = AXIS2_PLACEMENT_3D ( 'NONE', #138317, #39275, #118796 ) ;
#256240 = CARTESIAN_POINT ( 'NONE',  ( -18.59999999999999787, 79.15532900748003442, -196.2806010913881778 ) ) ;
#256241 = DIRECTION ( 'NONE',  ( 0.000000000000000000, 0.000000000000000000, -1.000000000000000000 ) ) ;
#256242 = EDGE_LOOP ( 'NONE', ( #75973, #97891, #12932, #180384 ) ) ;
#256243 = CARTESIAN_POINT ( 'NONE',  ( -15.31895204843005232, 66.60346600605809897, -118.6171677053510933 ) ) ;
#256244 = EDGE_CURVE ( 'NONE', #21519, #131079, #226, .T. ) ;
#256245 = VERTEX_POINT ( 'NONE', #75499 ) ;
#256246 = EDGE_CURVE ( 'NONE', #205206, #203901, #176339, .T. ) ;
#256247 = DIRECTION ( 'NONE',  ( -0.7071067811865474617, 0.6824534298470372740, -0.1850873201762209819 ) ) ;
#256248 = ORIENTED_EDGE ( 'NONE', *, *, #217692, .F. ) ;
#256249 = PLANE ( 'NONE',  #218779 ) ;
#256250 = B_SPLINE_CURVE_WITH_KNOTS ( 'NONE', 3,
 ( #115155, #194717, #95583, #218082, #235111, #116447, #197255, #58997, #17347, #238964 ),
 .UNSPECIFIED., .F., .F.,
 ( 4, 2, 2, 2, 4 ),
 ( 0.000000000000000000, 0.0003916577441626726262, 0.0005874866162440096169, 0.0006854010522846797114, 0.0007833154883253498060 ),
 .UNSPECIFIED. ) ;
#256251 = CYLINDRICAL_SURFACE ( 'NONE', #109024, 0.09999999999998898659 ) ;
#256252 = DIRECTION ( 'NONE',  ( 0.000000000000000000, 0.000000000000000000, -1.000000000000000000 ) ) ;
#256253 = ORIENTED_EDGE ( 'NONE', *, *, #90199, .T. ) ;
#256254 = ADVANCED_FACE ( 'NONE', ( #153781 ), #5595, .T. ) ;
#256255 = FACE_OUTER_BOUND ( 'NONE', #210390, .T. ) ;
#256256 = VERTEX_POINT ( 'NONE', #15527 ) ;
#256257 = DIRECTION ( 'NONE',  ( 0.000000000000000000, 7.086529944415894657E-15, -1.000000000000000000 ) ) ;
#256259 = ORIENTED_EDGE ( 'NONE', *, *, #249066, .F. ) ;
#256258 = CIRCLE ( 'NONE', #227289, 0.09999999999999939493 ) ;
#256260 = COLOUR_RGB ( '', 0.66274510, 0.83137255, 0.94901961) ;
#256261 = CIRCLE ( 'NONE', #148179, 0.2000000000000057288 ) ;
#256262 = DIRECTION ( 'NONE',  ( 0.000000000000000000, 0.9126074666063660468, 0.4088369013363524762 ) ) ;
#256263 = ORIENTED_EDGE ( 'NONE', *, *, #235806, .F. ) ;
#256264 = AXIS2_PLACEMENT_3D ( 'NONE', #225773, #144958, #5435 ) ;
#256265 = DIRECTION ( 'NONE',  ( -0.000000000000000000, 6.982962677686266711E-15, -1.000000000000000000 ) ) ;
#256266 = CARTESIAN_POINT ( 'NONE',  ( 22.47809213839789066, 64.14563076733692526, -247.0890968714184055 ) ) ;
#256267 = CYLINDRICAL_SURFACE ( 'NONE', #245132, 1.749999999999999778 ) ;
#256268 = CARTESIAN_POINT ( 'NONE',  ( -16.87786941232800686, 9.958154714156124854, -121.3771857997940486 ) ) ;
#256269 = AXIS2_PLACEMENT_3D ( 'NONE', #28636, #37582, #93687 ) ;
#256270 = VECTOR ( 'NONE', #54868, 1000.000000000000000 ) ;
#256271 = AXIS2_PLACEMENT_3D ( 'NONE', #178826, #256986, #217888 ) ;
#256272 = CARTESIAN_POINT ( 'NONE',  ( 20.94999999999999574, 1.162701749949165642, -175.5999999999999659 ) ) ;
#256273 = ORIENTED_EDGE ( 'NONE', *, *, #62321, .T. ) ;
#256274 = DIRECTION ( 'NONE',  ( 0.000000000000000000, 6.997203936713167125E-15, -1.000000000000000000 ) ) ;
#256275 = CARTESIAN_POINT ( 'NONE',  ( 22.47071067811865319, 33.41224047107334627, -242.5462774987836667 ) ) ;
#256276 = CARTESIAN_POINT ( 'NONE',  ( 20.94999999999999574, 77.85102823015243700, -57.86919421510181394 ) ) ;
#256277 = EDGE_CURVE ( 'NONE', #85165, #150222, #201245, .T. ) ;
#256278 = EDGE_LOOP ( 'NONE', ( #21891, #35050, #223342, #68218 ) ) ;
#256279 = CARTESIAN_POINT ( 'NONE',  ( 18.59999999999999076, 43.16354019706792400, -239.5695141926698284 ) ) ;
#256280 = ORIENTED_EDGE ( 'NONE', *, *, #57314, .F. ) ;
#256281 = DIRECTION ( 'NONE',  ( 0.000000000000000000, -6.982962677686266711E-15, 1.000000000000000000 ) ) ;
#256282 = ORIENTED_EDGE ( 'NONE', *, *, #94230, .T. ) ;
#256283 = AXIS2_PLACEMENT_3D ( 'NONE', #186798, #86360, #107239 ) ;
#256284 = AXIS2_PLACEMENT_3D ( 'NONE', #137360, #239048, #240344 ) ;
#256285 = CARTESIAN_POINT ( 'NONE',  ( -23.15000000000000213, 74.00000000001180922, -82.14772940728641970 ) ) ;
#256286 = CARTESIAN_POINT ( 'NONE',  ( 18.59999999999996945, 7.021664781911246322, -70.83356540189728889 ) ) ;
#256289 = ORIENTED_EDGE ( 'NONE', *, *, #243354, .T. ) ;
#256288 = EDGE_CURVE ( 'NONE', #67154, #58501, #115890, .T. ) ;
#256287 = DIRECTION ( 'NONE',  ( 0.000000000000000000, 1.214306433183772287E-13, 1.000000000000000000 ) ) ;
#256290 = DIRECTION ( 'NONE',  ( -0.000000000000000000, -1.000000000000000000, -6.982962677686266711E-15 ) ) ;
#256291 = ORIENTED_EDGE ( 'NONE', *, *, #7114, .T. ) ;
#256292 = AXIS2_PLACEMENT_3D ( 'NONE', #164215, #226730, #50648 ) ;
#256293 = DIRECTION ( 'NONE',  ( 0.000000000000000000, 0.000000000000000000, 1.000000000000000000 ) ) ;
#256294 = EDGE_CURVE ( 'NONE', #42831, #185781, #155508, .T. ) ;
#256295 = CYLINDRICAL_SURFACE ( 'NONE', #23089, 4.049999999999998046 ) ;
#256296 = VERTEX_POINT ( 'NONE', #71640 ) ;
#256297 = ORIENTED_EDGE ( 'NONE', *, *, #43716, .F. ) ;
#256298 = CYLINDRICAL_SURFACE ( 'NONE', #122533, 0.09999999999999939493 ) ;
#256300 = EDGE_CURVE ( 'NONE', #116221, #42831, #252814, .T. ) ;
#256299 = CARTESIAN_POINT ( 'NONE',  ( -22.59999970745345976, -3.233606324747438254, -228.1924402736483444 ) ) ;
#256301 = EDGE_LOOP ( 'NONE', ( #231625, #220740, #143399, #40900 ) ) ;
#256302 = CARTESIAN_POINT ( 'NONE',  ( -18.50000000000000000, 64.35000000001208775, -129.5083017138703667 ) ) ;
#256303 = ORIENTED_EDGE ( 'NONE', *, *, #256353, .F. ) ;
#256304 = ORIENTED_EDGE ( 'NONE', *, *, #28727, .F. ) ;
#256305 = EDGE_CURVE ( 'NONE', #84823, #254080, #226154, .T. ) ;
#256306 = CARTESIAN_POINT ( 'NONE',  ( 22.60000000000000142, 25.89494711235935043, -254.2627752153468350 ) ) ;
#256309 = ADVANCED_FACE ( 'NONE', ( #214976 ), #112049, .T. ) ;
#256308 = EDGE_CURVE ( 'NONE', #67031, #215026, #192866, .T. ) ;
#256307 = CARTESIAN_POINT ( 'NONE',  ( 21.04999999999998650, 6.649999999999999467, -12.25000000000000000 ) ) ;
#256311 = ORIENTED_EDGE ( 'NONE', *, *, #69256, .T. ) ;
#256310 = FACE_BOUND ( 'NONE', #148154, .T. ) ;
#256312 = CIRCLE ( 'NONE', #177324, 4.049999999999998046 ) ;
#256313 = DIRECTION ( 'NONE',  ( -1.000000000000000000, 0.000000000000000000, 0.000000000000000000 ) ) ;
#256314 = CARTESIAN_POINT ( 'NONE',  ( -20.54999999999999716, 73.50000000001151079, -49.24772940728643533 ) ) ;
#256315 = AXIS2_PLACEMENT_3D ( 'NONE', #137345, #17418, #406 ) ;
#256316 = DIRECTION ( 'NONE',  ( 1.000000000000000000, 0.000000000000000000, 0.000000000000000000 ) ) ;
#256318 = DIRECTION ( 'NONE',  ( 0.000000000000000000, 0.000000000000000000, -1.000000000000000000 ) ) ;
#256317 = DIRECTION ( 'NONE',  ( 0.000000000000000000, -0.8103668758649578141, 0.5859227990963212784 ) ) ;
#256319 = AXIS2_PLACEMENT_3D ( 'NONE', #205629, #150805, #106518 ) ;
#256320 = DIRECTION ( 'NONE',  ( 1.000000000000000000, 0.000000000000000000, 0.000000000000000000 ) ) ;
#256321 = DIRECTION ( 'NONE',  ( 0.000000000000000000, -6.467318590049456648E-15, 1.000000000000000000 ) ) ;
#256322 = CARTESIAN_POINT ( 'NONE',  ( 22.45380639572256953, -3.229117443981163849, -228.1842304705649553 ) ) ;
#256323 = EDGE_CURVE ( 'NONE', #147150, #111234, #76748, .T. ) ;
#256324 = EDGE_CURVE ( 'NONE', #37705, #138239, #72943, .T. ) ;
#256325 = ORIENTED_EDGE ( 'NONE', *, *, #135902, .T. ) ;
#256327 = ORIENTED_EDGE ( 'NONE', *, *, #190658, .T. ) ;
#256326 = CIRCLE ( 'NONE', #143965, 11.90000000000000746 ) ;
#256328 = DIRECTION ( 'NONE',  ( 1.000000000000000000, 2.885090398161910739E-16, 6.283419270304611573E-17 ) ) ;
#256330 = ORIENTED_EDGE ( 'NONE', *, *, #36968, .F. ) ;
#256329 = DIRECTION ( 'NONE',  ( 0.000000000000000000, 0.000000000000000000, -1.000000000000000000 ) ) ;
#256331 = ORIENTED_EDGE ( 'NONE', *, *, #201517, .T. ) ;
#256332 = EDGE_CURVE ( 'NONE', #74117, #111464, #191604, .T. ) ;
#256333 = CARTESIAN_POINT ( 'NONE',  ( 20.94999999999999929, 63.58084468663284383, -237.4904741118237723 ) ) ;
#256334 = VERTEX_POINT ( 'NONE', #235819 ) ;
#256335 = CIRCLE ( 'NONE', #143971, 2.000000000000003109 ) ;
#256336 = TOROIDAL_SURFACE ( 'NONE', #52386, 0.6000000000000013101, 0.1000000000000000056 ) ;
#256337 = EDGE_CURVE ( 'NONE', #130320, #43656, #59761, .T. ) ;
#256338 = ORIENTED_EDGE ( 'NONE', *, *, #213326, .T. ) ;
#256339 = AXIS2_PLACEMENT_3D ( 'NONE', #125658, #190810, #155536 ) ;
#256340 = LINE ( 'NONE', #157344, #128150 ) ;
#256341 = EDGE_CURVE ( 'NONE', #99076, #19990, #55463, .T. ) ;
#256343 = ORIENTED_EDGE ( 'NONE', *, *, #138721, .T. ) ;
#256342 = ORIENTED_EDGE ( 'NONE', *, *, #139836, .T. ) ;
#256344 = ORIENTED_EDGE ( 'NONE', *, *, #103926, .T. ) ;
#256345 = ORIENTED_EDGE ( 'NONE', *, *, #122991, .F. ) ;
#256346 = ORIENTED_EDGE ( 'NONE', *, *, #197992, .F. ) ;
#256347 = CYLINDRICAL_SURFACE ( 'NONE', #67066, 0.09999999999999939493 ) ;
#256348 = CARTESIAN_POINT ( 'NONE',  ( -18.43569575749026512, -9.519327731092442235, -6.972976376559330447 ) ) ;
#256350 = ORIENTED_EDGE ( 'NONE', *, *, #57035, .T. ) ;
#256349 = LINE ( 'NONE', #774, #71018 ) ;
#256351 = AXIS2_PLACEMENT_3D ( 'NONE', #136735, #232021, #91213 ) ;
#256352 = LINE ( 'NONE', #234278, #7655 ) ;
#256353 = EDGE_CURVE ( 'NONE', #42158, #84512, #167977, .T. ) ;
#256354 = CARTESIAN_POINT ( 'NONE',  ( 14.56326696814969957, 12.44126776692609582, -213.7332981774226539 ) ) ;
#256356 = EDGE_LOOP ( 'NONE', ( #1211, #238904, #156231, #222981 ) ) ;
#256355 = CARTESIAN_POINT ( 'NONE',  ( 20.12500000000000000, 66.25000000001185185, -81.87310748452438247 ) ) ;
#256357 = DIRECTION ( 'NONE',  ( 0.000000000000000000, -0.9908441862701791170, 0.1350103645450472789 ) ) ;
#256358 = ORIENTED_EDGE ( 'NONE', *, *, #206780, .F. ) ;
#256359 = DIRECTION ( 'NONE',  ( 1.000000000000000000, 0.000000000000000000, 0.000000000000000000 ) ) ;
#256361 = EDGE_LOOP ( 'NONE', ( #243820, #88958, #104021, #13760 ) ) ;
#256360 = CYLINDRICAL_SURFACE ( 'NONE', #247716, 0.09999999999999939493 ) ;
#256362 = FACE_OUTER_BOUND ( 'NONE', #120518, .T. ) ;
#256363 = CARTESIAN_POINT ( 'NONE',  ( 20.94999999999999929, 5.000000000011153745, -54.59473398108690390 ) ) ;
#256364 = FACE_OUTER_BOUND ( 'NONE', #203038, .T. ) ;
#256366 = ADVANCED_FACE ( 'NONE', ( #152472 ), #84699, .F. ) ;
#256365 = ORIENTED_EDGE ( 'NONE', *, *, #137292, .F. ) ;
#256368 = CARTESIAN_POINT ( 'NONE',  ( 18.49999999999999645, 76.00000000001165290, -69.52310748452431710 ) ) ;
#256367 = DIRECTION ( 'NONE',  ( 0.000000000000000000, -0.1332476588733448597, -0.9910827722268067408 ) ) ;
#256369 = CARTESIAN_POINT ( 'NONE',  ( 20.94999999999999574, 14.00000000001115730, -172.9270925303825095 ) ) ;
#256370 = DIRECTION ( 'NONE',  ( 9.044546369203339308E-15, 0.9165223833629894123, -0.3999834006488590110 ) ) ;
#256371 = AXIS2_PLACEMENT_3D ( 'NONE', #153897, #211249, #33947 ) ;
#256372 = VECTOR ( 'NONE', #74000, 1000.000000000000000 ) ;
#256373 = DIRECTION ( 'NONE',  ( 0.000000000000000000, 8.770518838402102073E-15, -1.000000000000000000 ) ) ;
#256375 = DIRECTION ( 'NONE',  ( 0.000000000000000000, 0.000000000000000000, 1.000000000000000000 ) ) ;
#256374 = AXIS2_PLACEMENT_3D ( 'NONE', #62426, #118563, #58545 ) ;
#256376 = EDGE_LOOP ( 'NONE', ( #45955, #233752, #117835, #214759 ) ) ;
#256377 = VERTEX_POINT ( 'NONE', #54615 ) ;
#256378 = ORIENTED_EDGE ( 'NONE', *, *, #24993, .F. ) ;
#256379 = CARTESIAN_POINT ( 'NONE',  ( 18.59999999999999432, -1.162701749926855266, -175.5999999999999659 ) ) ;
#256380 = DIRECTION ( 'NONE',  ( -4.408576920032448588E-17, -0.1350103645451807832, -0.9908441862701610203 ) ) ;
#256381 = VERTEX_POINT ( 'NONE', #14241 ) ;
#256382 = DIRECTION ( 'NONE',  ( 0.000000000000000000, 0.9654727137038715545, -0.2605042016806676242 ) ) ;
#256383 = VERTEX_POINT ( 'NONE', #134149 ) ;
#256384 = ADVANCED_FACE ( 'NONE', ( #194159 ), #237117, .F. ) ;
#256385 = CARTESIAN_POINT ( 'NONE',  ( -21.65000000000000213, 9.052352027203962592, -208.4953267290897543 ) ) ;
#256386 = DIRECTION ( 'NONE',  ( 0.000000000000000000, -1.000000000000000000, 0.000000000000000000 ) ) ;
#256387 = VERTEX_POINT ( 'NONE', #59729 ) ;
#256388 = CARTESIAN_POINT ( 'NONE',  ( -21.14999999999999858, -11.64999999998884483, -134.0000000000000000 ) ) ;
#256389 = CIRCLE ( 'NONE', #60619, 7.800000000000001599 ) ;
#256390 = ORIENTED_EDGE ( 'NONE', *, *, #163858, .F. ) ;
#256391 = ORIENTED_EDGE ( 'NONE', *, *, #202355, .F. ) ;
#256392 = VERTEX_POINT ( 'NONE', #118467 ) ;
#256393 = CARTESIAN_POINT ( 'NONE',  ( -22.39999999999999858, 31.94635157770351341, -238.7871412784868994 ) ) ;
#256394 = AXIS2_PLACEMENT_3D ( 'NONE', #20538, #217412, #63477 ) ;
#256395 = DIRECTION ( 'NONE',  ( 1.000000000000000000, -1.476360405086644309E-16, 0.000000000000000000 ) ) ;
#256396 = CARTESIAN_POINT ( 'NONE',  ( -20.64999999999999858, -9.399999999988846611, -157.6060308773475924 ) ) ;
#256397 = CARTESIAN_POINT ( 'NONE',  ( 13.88638282980484284, 66.54257354752311926, -118.0230656161243701 ) ) ;
#256399 = DIRECTION ( 'NONE',  ( 0.000000000000000000, 0.000000000000000000, -1.000000000000000000 ) ) ;
#256398 = SPHERICAL_SURFACE ( 'NONE', #245349, 0.1000000000000000056 ) ;
#256400 = DIRECTION ( 'NONE',  ( 0.000000000000000000, 0.000000000000000000, -1.000000000000000000 ) ) ;
#256402 = EDGE_LOOP ( 'NONE', ( #185469, #198643, #121131 ) ) ;
#256401 = DIRECTION ( 'NONE',  ( 1.000000000000000000, -0.000000000000000000, -0.000000000000000000 ) ) ;
#256403 = CARTESIAN_POINT ( 'NONE',  ( -16.87036670365549895, 9.989418819312803066, -79.52043988269799968 ) ) ;
#256404 = ORIENTED_EDGE ( 'NONE', *, *, #113141, .T. ) ;
#256405 = CYLINDRICAL_SURFACE ( 'NONE', #177963, 0.09999999999999939493 ) ;
#256406 = VERTEX_POINT ( 'NONE', #122303 ) ;
#256407 = ORIENTED_EDGE ( 'NONE', *, *, #247076, .F. ) ;
#256408 = DIRECTION ( 'NONE',  ( -0.000000000000000000, -0.9651348961777157509, 0.2617529984165031243 ) ) ;
#256409 = FACE_OUTER_BOUND ( 'NONE', #132250, .T. ) ;
#256410 = CARTESIAN_POINT ( 'NONE',  ( -21.14999999999994174, 83.90000000001120384, -34.86056257560453986 ) ) ;
#256411 = ORIENTED_EDGE ( 'NONE', *, *, #173785, .T. ) ;
#256412 = CIRCLE ( 'NONE', #73355, 4.150000000000001243 ) ;
#256413 = DIRECTION ( 'NONE',  ( 0.000000000000000000, -0.9126074666069882158, -0.4088369013349636427 ) ) ;
#256414 = EDGE_LOOP ( 'NONE', ( #88693, #128792, #15869, #84135 ) ) ;
#256415 = EDGE_LOOP ( 'NONE', ( #78268, #158257, #160018, #190971 ) ) ;
#256416 = CARTESIAN_POINT ( 'NONE',  ( -21.05000000000000071, 38.08698097766499302, -236.1457910985472779 ) ) ;
#256417 = ORIENTED_EDGE ( 'NONE', *, *, #112404, .F. ) ;
#256418 = LINE ( 'NONE', #140379, #136220 ) ;
#256419 = DIRECTION ( 'NONE',  ( 0.000000000000000000, -0.2128009952263650861, 0.9770955615653305060 ) ) ;
#256420 = VERTEX_POINT ( 'NONE', #238392 ) ;
#256421 = CARTESIAN_POINT ( 'NONE',  ( 20.94999999999999929, 36.65892442174935439, -249.5511627012433848 ) ) ;
#256422 = CARTESIAN_POINT ( 'NONE',  ( -16.83199318825828783, 9.930646127992318384, -121.2275851882092184 ) ) ;
#256423 = DIRECTION ( 'NONE',  ( -1.000000000000000000, 0.000000000000000000, 0.000000000000000000 ) ) ;
#256424 = ORIENTED_EDGE ( 'NONE', *, *, #213328, .T. ) ;
#256425 = CARTESIAN_POINT ( 'NONE',  ( -18.59999999999999787, 3.912899247244609580, -44.98182297301097066 ) ) ;
#256427 = EDGE_CURVE ( 'NONE', #186212, #223374, #88810, .T. ) ;
#256426 = CARTESIAN_POINT ( 'NONE',  ( 20.85000000000000142, -1.835859311432481045, -145.5044391687985694 ) ) ;
#256428 = AXIS2_PLACEMENT_3D ( 'NONE', #255838, #117660, #158120 ) ;
#256429 = CARTESIAN_POINT ( 'NONE',  ( 20.85000000000000142, 67.65998959290219261, -227.8609496483021530 ) ) ;
#256430 = AXIS2_PLACEMENT_3D ( 'NONE', #157239, #254958, #155955 ) ;
#256431 = AXIS2_PLACEMENT_3D ( 'NONE', #49330, #85857, #149746 ) ;
#256432 = CIRCLE ( 'NONE', #135868, 0.1000000000000000749 ) ;
#256433 = ORIENTED_EDGE ( 'NONE', *, *, #9065, .T. ) ;
#256434 = PRESENTATION_LAYER_ASSIGNMENT (  '', '', ( #89896 ) ) ;
#256435 = DIRECTION ( 'NONE',  ( 0.000000000000000000, -0.1568667991644714932, 0.9876197685951274563 ) ) ;
#256436 = VERTEX_POINT ( 'NONE', #80573 ) ;
#256437 = CARTESIAN_POINT ( 'NONE',  ( 21.14999999999999503, 25.97741635855165754, -254.4468634167653249 ) ) ;
#256438 = DIRECTION ( 'NONE',  ( 0.000000000000000000, -1.000000000000000000, -6.982962677686265922E-15 ) ) ;
#256439 = FACE_OUTER_BOUND ( 'NONE', #208236, .T. ) ;
#256440 = FACE_OUTER_BOUND ( 'NONE', #18114, .T. ) ;
#256441 = CARTESIAN_POINT ( 'NONE',  ( -18.40000000000000213, 11.33174054712516110, -12.65000000000000213 ) ) ;
#256442 = EDGE_CURVE ( 'NONE', #201117, #252116, #81846, .T. ) ;
#256443 = EDGE_CURVE ( 'NONE', #138337, #137060, #205525, .T. ) ;
#256444 = ORIENTED_EDGE ( 'NONE', *, *, #257077, .T. ) ;
#256445 = CARTESIAN_POINT ( 'NONE',  ( -23.25000000000000000, 11.65000000000000036, 11.75000000000000000 ) ) ;
#256446 = CARTESIAN_POINT ( 'NONE',  ( 21.10710606213542206, 67.22310597611885896, -124.2821109581249317 ) ) ;
#256447 = CARTESIAN_POINT ( 'NONE',  ( -18.54260524012568823, 77.31769039854688685, -241.8823842174727474 ) ) ;
#256448 = DIRECTION ( 'NONE',  ( -1.000000000000000000, 0.000000000000000000, 0.000000000000000000 ) ) ;
#256449 = B_SPLINE_CURVE_WITH_KNOTS ( 'NONE', 3,
 ( #175793, #132814, #135345, #212355, #74141, #231917, #235734, #94940, #173261, #213605, #251455, #117090, #214895, #252727 ),
 .UNSPECIFIED., .F., .F.,
 ( 4, 2, 2, 2, 2, 2, 4 ),
 ( 0.000000000000000000, 2.389617747642649214E-05, 4.779235495285298429E-05, 9.558470990571555021E-05, 0.0001911694198114329165, 0.0003823388396228745065, 0.0007646776792457625656 ),
 .UNSPECIFIED. ) ;
#256450 = AXIS2_PLACEMENT_3D ( 'NONE', #143666, #127969, #224485 ) ;
#256451 = CARTESIAN_POINT ( 'NONE',  ( 20.96937028524355284, 65.37553062838493645, -62.03168138335477977 ) ) ;
#256452 = CIRCLE ( 'NONE', #239976, 0.09999999999999438505 ) ;
#256453 = ORIENTED_EDGE ( 'NONE', *, *, #79738, .T. ) ;
#256454 = ORIENTED_EDGE ( 'NONE', *, *, #103416, .T. ) ;
#256455 = DIRECTION ( 'NONE',  ( 0.000000000000000000, 0.1350103645451945777, -0.9908441862701589109 ) ) ;
#256456 = DIRECTION ( 'NONE',  ( 0.000000000000000000, 0.000000000000000000, -1.000000000000000000 ) ) ;
#256458 = EDGE_CURVE ( 'NONE', #75854, #202553, #238861, .T. ) ;
#256457 = CARTESIAN_POINT ( 'NONE',  ( -16.87331047859651179, 66.05000000001261640, -190.8731074845244393 ) ) ;
#256459 = CARTESIAN_POINT ( 'NONE',  ( 21.00000000000000000, 66.25000000001229239, -157.7731074845244166 ) ) ;
#256460 = CARTESIAN_POINT ( 'NONE',  ( -21.64999999999999858, 10.05000000001113847, -154.8500000000000227 ) ) ;
#256461 = EDGE_CURVE ( 'NONE', #85452, #98329, #238680, .T. ) ;
#256462 = AXIS2_PLACEMENT_3D ( 'NONE', #174863, #155282, #215219 ) ;
#256463 =( BOUNDED_CURVE ( )  B_SPLINE_CURVE ( 3, ( #111522, #191082, #106359, #185919 ),
 .UNSPECIFIED., .F., .F. ) 
 B_SPLINE_CURVE_WITH_KNOTS ( ( 4, 4 ),
 ( -9.769962616701377556E-15, 1.570796326794793529 ),
 .UNSPECIFIED. ) 
 CURVE ( )  GEOMETRIC_REPRESENTATION_ITEM ( )  RATIONAL_B_SPLINE_CURVE ( ( 1.000000000000000000, 0.8047378541243870309, 0.8047378541243870309, 1.000000000000000000 ) ) 
 REPRESENTATION_ITEM ( '' )  );
#256464 = EDGE_LOOP ( 'NONE', ( #106368, #141960, #79915, #205983 ) ) ;
#256465 = FACE_OUTER_BOUND ( 'NONE', #35675, .T. ) ;
#256466 = AXIS2_PLACEMENT_3D ( 'NONE', #231936, #235753, #16736 ) ;
#256467 = ADVANCED_FACE ( 'NONE', ( #182285 ), #97149, .F. ) ;
#256468 = AXIS2_PLACEMENT_3D ( 'NONE', #122691, #26149, #164371 ) ;
#256469 = DIRECTION ( 'NONE',  ( 1.000000000000000000, 0.000000000000000000, 0.000000000000000000 ) ) ;
#256470 = ORIENTED_EDGE ( 'NONE', *, *, #248577, .F. ) ;
#256471 = SPHERICAL_SURFACE ( 'NONE', #175647, 0.1000000000000000056 ) ;
#256472 = EDGE_CURVE ( 'NONE', #198296, #252068, #119752, .T. ) ;
#256473 = LINE ( 'NONE', #20519, #28834 ) ;
#256474 = AXIS2_PLACEMENT_3D ( 'NONE', #164986, #226205, #205378 ) ;
#256475 = ADVANCED_FACE ( 'NONE', ( #181005, #78027 ), #177173, .T. ) ;
#256476 = ORIENTED_EDGE ( 'NONE', *, *, #256933, .T. ) ;
#256479 =( BOUNDED_SURFACE ( )  B_SPLINE_SURFACE ( 3, 2, ( 
 ( #103007, #142145, #196976 ),
 ( #219103, #43060, #163019 ),
 ( #157917, #202130, #239980 ),
 ( #161743, #237405, #200848 ),
 ( #238684, #178754, #62624 ),
 ( #23527, #140875, #118756 ) ),
 .UNSPECIFIED., .F., .F., .T. ) 
 B_SPLINE_SURFACE_WITH_KNOTS ( ( 4, 2, 4 ),
 ( 3, 3 ),
 ( 4.712388980384689674, 5.497787143782137953, 6.283185307179586232 ),
 ( 0.000000000000000000, 1.000000000000000000 ),
 .UNSPECIFIED. ) 
 GEOMETRIC_REPRESENTATION_ITEM ( )  RATIONAL_B_SPLINE_SURFACE ( (
 ( 1.000000000000000000, 0.7071067811865408004, 1.000000000000000000),
 ( 1.000000000000000000, 0.7727932973489139989, 1.000000000000000000),
 ( 1.000000000000000000, 0.8282379607651187969, 1.000000000000000000),
 ( 1.000000000000000000, 0.9038128468037410768, 1.000000000000000000),
 ( 1.000000000000000000, 0.9240297172245056645, 1.000000000000000000),
 ( 1.000000000000000000, 0.9238795325112937329, 1.000000000000000000) ) ) 
 REPRESENTATION_ITEM ( '' )  SURFACE ( )  );
#256478 = CIRCLE ( 'NONE', #144092, 0.1999999999999987899 ) ;
#256477 = CARTESIAN_POINT ( 'NONE',  ( -18.35235881385853318, 64.52658099229972777, -194.2731074845244450 ) ) ;
#256480 = ORIENTED_EDGE ( 'NONE', *, *, #59317, .F. ) ;
#256481 = DIRECTION ( 'NONE',  ( 1.000000000000000000, 0.000000000000000000, 0.000000000000000000 ) ) ;
#256482 = FACE_OUTER_BOUND ( 'NONE', #48157, .T. ) ;
#256483 = DIRECTION ( 'NONE',  ( 0.000000000000000000, 0.9999631594459056361, -0.008583690987128059571 ) ) ;
#256484 = AXIS2_PLACEMENT_3D ( 'NONE', #257584, #120736, #256293 ) ;
#256485 = LINE ( 'NONE', #34980, #182248 ) ;
#256486 = DIRECTION ( 'NONE',  ( 1.000000000000000000, 0.000000000000000000, 0.000000000000000000 ) ) ;
#256487 = DIRECTION ( 'NONE',  ( 1.000000000000000000, -0.000000000000000000, -0.000000000000000000 ) ) ;
#256488 = CARTESIAN_POINT ( 'NONE',  ( 15.48841904831874849, 22.32246587424956985, -232.1589482157900761 ) ) ;
#256489 = CARTESIAN_POINT ( 'NONE',  ( -23.25000000000000355, 40.29670989715187090, -235.0462836312595130 ) ) ;
#256490 = EDGE_CURVE ( 'NONE', #173016, #185405, #13812, .T. ) ;
#256491 = CARTESIAN_POINT ( 'NONE',  ( -20.94999999999999929, 43.48442877397276618, -245.2193771921251084 ) ) ;
#256492 = DIRECTION ( 'NONE',  ( -3.469446951953995998E-14, 0.000000000000000000, -1.000000000000000000 ) ) ;
#256493 = CARTESIAN_POINT ( 'NONE',  ( -21.65000000000000213, 66.05000000001207638, -123.8731074845243683 ) ) ;
#256494 = AXIS2_PLACEMENT_3D ( 'NONE', #19714, #61391, #200900 ) ;
#256495 = CARTESIAN_POINT ( 'NONE',  ( -20.54999999999999716, 74.07476635515247665, -157.2928639513982318 ) ) ;
#256496 = DIRECTION ( 'NONE',  ( 0.000000000000000000, 0.8689845192018014197, -0.4948392722769828778 ) ) ;
#256497 = CARTESIAN_POINT ( 'NONE',  ( 21.13461538461538325, 10.61458296203669427, -79.35000000000006537 ) ) ;
#256498 = CARTESIAN_POINT ( 'NONE',  ( -20.85000000000000142, 43.18640298906419162, -245.2812653309023574 ) ) ;
#256499 =( BOUNDED_CURVE ( )  B_SPLINE_CURVE ( 3, ( #124665, #106350, #166387, #8567 ),
 .UNSPECIFIED., .F., .F. ) 
 B_SPLINE_CURVE_WITH_KNOTS ( ( 4, 4 ),
 ( 3.141592653589778461, 4.712388980384686121 ),
 .UNSPECIFIED. ) 
 CURVE ( )  GEOMETRIC_REPRESENTATION_ITEM ( )  RATIONAL_B_SPLINE_CURVE ( ( 1.000000000000000000, 0.8047378541243622729, 0.8047378541243622729, 1.000000000000000000 ) ) 
 REPRESENTATION_ITEM ( '' )  );
#256500 = ORIENTED_EDGE ( 'NONE', *, *, #76820, .F. ) ;
#256501 = LINE ( 'NONE', #197868, #139606 ) ;
#256502 = CARTESIAN_POINT ( 'NONE',  ( 21.05000000000000071, 71.00000000001180922, -81.52837350343745015 ) ) ;
#256503 = CARTESIAN_POINT ( 'NONE',  ( 20.94999999999999929, 44.15903683684981473, -236.5744930507153185 ) ) ;
#256504 = ORIENTED_EDGE ( 'NONE', *, *, #3338, .F. ) ;
#256505 = CARTESIAN_POINT ( 'NONE',  ( 21.10000000000000142, 6.223900101154155706, 12.00000000000000178 ) ) ;
#256506 = CIRCLE ( 'NONE', #89973, 0.1000000000000014488 ) ;
#256507 = CIRCLE ( 'NONE', #248382, 0.09999999999999982514 ) ;
#256508 = CARTESIAN_POINT ( 'NONE',  ( -16.27683809663750480, 30.01116235937717391, -235.3831614462291384 ) ) ;
#256509 = ORIENTED_EDGE ( 'NONE', *, *, #67024, .F. ) ;
#256511 = CIRCLE ( 'NONE', #223246, 0.09999999999999344136 ) ;
#256510 = CARTESIAN_POINT ( 'NONE',  ( -21.14999999999999503, 38.16955627025379982, -235.9992222486930302 ) ) ;
#256512 = CARTESIAN_POINT ( 'NONE',  ( -20.94999999999999929, 70.65782965956557859, -228.4198064469268559 ) ) ;
#256513 = CIRCLE ( 'NONE', #40133, 0.1000000000000028644 ) ;
#256514 = ORIENTED_EDGE ( 'NONE', *, *, #192865, .F. ) ;
#256515 = AXIS2_PLACEMENT_3D ( 'NONE', #40231, #257907, #95035 ) ;
#256516 = EDGE_CURVE ( 'NONE', #20400, #18191, #159571, .T. ) ;
#256517 = ADVANCED_FACE ( 'NONE', ( #19352 ), #2332, .F. ) ;
#256518 = VERTEX_POINT ( 'NONE', #240967 ) ;
#256519 = DIRECTION ( 'NONE',  ( 0.000000000000000000, 0.01562499999998609446, -0.9998779222360101304 ) ) ;
#256520 = ORIENTED_EDGE ( 'NONE', *, *, #32473, .F. ) ;
#256521 = EDGE_CURVE ( 'NONE', #210246, #237621, #172273, .T. ) ;
#256524 = ADVANCED_FACE ( 'NONE', ( #40225 ), #196691, .F. ) ;
#256523 = CIRCLE ( 'NONE', #219164, 0.6000000000000033085 ) ;
#256522 = CARTESIAN_POINT ( 'NONE',  ( -17.11825945287482753, 10.05000000001113847, -113.1500000000000341 ) ) ;
#256525 = CARTESIAN_POINT ( 'NONE',  ( -20.94999999999999929, 1.835341550224411922, -11.55515129256298046 ) ) ;
#256527 = DIRECTION ( 'NONE',  ( 1.000000000000000000, 0.000000000000000000, 0.000000000000000000 ) ) ;
#256526 = UNCERTAINTY_MEASURE_WITH_UNIT (LENGTH_MEASURE( 1.000000000000000082E-05 ), #102480, 'distance_accuracy_value', 'NONE');
#256528 = DIRECTION ( 'NONE',  ( -1.000000000000000000, 0.000000000000000000, 0.000000000000000000 ) ) ;
#256529 = CIRCLE ( 'NONE', #69362, 0.09999999999998898659 ) ;
#256530 = DIRECTION ( 'NONE',  ( -1.000000000000000000, 0.000000000000000000, 0.000000000000000000 ) ) ;
#256531 = CARTESIAN_POINT ( 'NONE',  ( -12.60206096961792355, 47.12322829752087472, -234.5744283691289240 ) ) ;
#256532 = AXIS2_PLACEMENT_3D ( 'NONE', #151364, #74413, #229600 ) ;
#256533 = ADVANCED_FACE ( 'NONE', ( #3620 ), #217528, .T. ) ;
#256534 = DIRECTION ( 'NONE',  ( 0.000000000000000000, 6.982962677686266711E-15, -1.000000000000000000 ) ) ;
#256535 = CARTESIAN_POINT ( 'NONE',  ( 23.14999999999999503, 69.35000000001222986, -148.7731074845244166 ) ) ;
#256537 = EDGE_LOOP ( 'NONE', ( #87837, #108757, #228505, #9027 ) ) ;
#256536 = CARTESIAN_POINT ( 'NONE',  ( 21.09096482362058467, 69.63645563460745791, -103.0625557632984339 ) ) ;
#256538 = ORIENTED_EDGE ( 'NONE', *, *, #93029, .T. ) ;
#256540 = CARTESIAN_POINT ( 'NONE',  ( -21.14999999999999858, 64.25000000001161027, -62.73924182154625129 ) ) ;
#256539 = CARTESIAN_POINT ( 'NONE',  ( 18.52351027002947959, 38.02524580842611357, -261.2214809015557080 ) ) ;
#256542 = VERTEX_POINT ( 'NONE', #97570 ) ;
#256541 = DIRECTION ( 'NONE',  ( 0.000000000000000000, 0.000000000000000000, 1.000000000000000000 ) ) ;
#256543 = EDGE_CURVE ( 'NONE', #172709, #88008, #206004, .T. ) ;
#256544 = ORIENTED_EDGE ( 'NONE', *, *, #190468, .F. ) ;
#256545 = DIRECTION ( 'NONE',  ( 0.000000000000000000, 0.2128009952263601456, -0.9770955615653316162 ) ) ;
#256546 = ADVANCED_FACE ( 'NONE', ( #86018 ), #34881, .F. ) ;
#256547 = CARTESIAN_POINT ( 'NONE',  ( 20.94999999999999929, 69.55000000001261640, -193.5060803140843859 ) ) ;
#256549 = EDGE_CURVE ( 'NONE', #168114, #105990, #14217, .T. ) ;
#256548 = DIRECTION ( 'NONE',  ( 0.000000000000000000, 0.8814952561688436106, -0.4721928772777334027 ) ) ;
#256550 = CARTESIAN_POINT ( 'NONE',  ( -18.50000000000000000, 11.74999999999999645, -0.1000000000000028644 ) ) ;
#256552 = DIRECTION ( 'NONE',  ( -2.915501640297154283E-16, 1.000000000000000000, 0.000000000000000000 ) ) ;
#256551 = AXIS2_PLACEMENT_3D ( 'NONE', #34805, #11364, #249973 ) ;
#256553 = CARTESIAN_POINT ( 'NONE',  ( -18.59999999999999787, 29.37215541956148002, -237.4231786350947857 ) ) ;
#256554 = CYLINDRICAL_SURFACE ( 'NONE', #19741, 0.5000000000000004441 ) ;
#256555 = B_SPLINE_CURVE_WITH_KNOTS ( 'NONE', 3,
 ( #137702, #197684, #135136, #116878, #252522, #214685, #36072, #19058, #98550, #158599 ),
 .UNSPECIFIED., .F., .F.,
 ( 4, 3, 3, 4 ),
 ( 0.000000000000000000, 3.394313611810755905E-05, 6.779740500699793829E-05, 0.0001049857339142623287 ),
 .UNSPECIFIED. ) ;
#256556 = EDGE_CURVE ( 'NONE', #171323, #139155, #9899, .T. ) ;
#256557 = DIRECTION ( 'NONE',  ( 1.000000000000000000, 0.000000000000000000, 0.000000000000000000 ) ) ;
#256558 = EDGE_LOOP ( 'NONE', ( #21940, #77630, #51552, #5800 ) ) ;
#256559 = ORIENTED_EDGE ( 'NONE', *, *, #188614, .T. ) ;
#256560 = DIRECTION ( 'NONE',  ( 4.239556034732057360E-17, 0.1298341882519953860, 0.9915357197604862671 ) ) ;
#256561 = EDGE_CURVE ( 'NONE', #234077, #27940, #147308, .T. ) ;
#256562 = EDGE_CURVE ( 'NONE', #34543, #159519, #43232, .T. ) ;
#256563 = AXIS2_PLACEMENT_3D ( 'NONE', #52806, #119227, #20128 ) ;
#256564 = TOROIDAL_SURFACE ( 'NONE', #2712, 0.6000000000000004219, 0.1000000000000000056 ) ;
#256565 = ORIENTED_EDGE ( 'NONE', *, *, #144182, .T. ) ;
#256566 = CIRCLE ( 'NONE', #2534, 0.09999999999999967248 ) ;
#256567 = CARTESIAN_POINT ( 'NONE',  ( -22.94999999999999929, 1.885425182446134107, -11.59641995933507808 ) ) ;
#256568 = VERTEX_POINT ( 'NONE', #66496 ) ;
#256569 = CARTESIAN_POINT ( 'NONE',  ( -23.25000000000000000, 74.83412143252222393, -233.7087995678629966 ) ) ;
#256570 = EDGE_CURVE ( 'NONE', #150942, #68194, #184865, .T. ) ;
#256571 = CARTESIAN_POINT ( 'NONE',  ( -12.68215100488889924, 49.15934945732310268, -233.6546618023459985 ) ) ;
#256572 = FACE_OUTER_BOUND ( 'NONE', #210492, .T. ) ;
#256574 = ORIENTED_EDGE ( 'NONE', *, *, #128452, .F. ) ;
#256573 = CARTESIAN_POINT ( 'NONE',  ( -21.40925344232282512, 6.658518859401606704, -33.40104981138036067 ) ) ;
#256575 = ADVANCED_FACE ( 'NONE', ( #31260 ), #28698, .T. ) ;
#256576 = CARTESIAN_POINT ( 'NONE',  ( 20.94999999999999929, -9.000000000000000000, -23.60603087734755690 ) ) ;
#256577 = VERTEX_POINT ( 'NONE', #7814 ) ;
#256578 = EDGE_CURVE ( 'NONE', #70322, #50778, #247694, .T. ) ;
#256579 = CARTESIAN_POINT ( 'NONE',  ( 21.30000000000002558, 1.115600667400684642E-11, -33.50000000000000000 ) ) ;
#256580 = DIRECTION ( 'NONE',  ( -1.000000000000000000, 0.000000000000000000, 0.000000000000000000 ) ) ;
#256581 = CARTESIAN_POINT ( 'NONE',  ( -23.25000000000000000, 67.23127455305835554, -235.8551265064784559 ) ) ;
#256582 = FACE_OUTER_BOUND ( 'NONE', #97934, .T. ) ;
#256583 = AXIS2_PLACEMENT_3D ( 'NONE', #134280, #170913, #169624 ) ;
#256584 = CARTESIAN_POINT ( 'NONE',  ( -21.05000000000000071, 76.00000000001190870, -103.0231074845243029 ) ) ;
#256585 = VERTEX_POINT ( 'NONE', #50750 ) ;
#256586 = AXIS2_PLACEMENT_3D ( 'NONE', #7933, #130429, #151303 ) ;
#256587 = CARTESIAN_POINT ( 'NONE',  ( -18.31331870001086060, 85.53629471919219895, -29.15452879353895099 ) ) ;
#256588 = ORIENTED_EDGE ( 'NONE', *, *, #212284, .F. ) ;
#256591 = EDGE_LOOP ( 'NONE', ( #103738, #109760, #53686 ) ) ;
#256590 = CARTESIAN_POINT ( 'NONE',  ( -21.64999999999999858, 65.95000000001181206, -82.17310748452439384 ) ) ;
#256589 = DIRECTION ( 'NONE',  ( -1.000000000000000000, -0.000000000000000000, -0.000000000000000000 ) ) ;
#256592 = PLANE ( 'NONE',  #14632 ) ;
#256593 = CARTESIAN_POINT ( 'NONE',  ( -22.50485643085240284, -2.577349838974356100, -189.5360933269992358 ) ) ;
#256594 = VECTOR ( 'NONE', #103573, 1000.000000000000000 ) ;
#256595 = ORIENTED_EDGE ( 'NONE', *, *, #213904, .F. ) ;
#256596 = CARTESIAN_POINT ( 'NONE',  ( 18.46932045258642674, 85.67068520027788736, -129.8492471115277169 ) ) ;
#256597 = DIRECTION ( 'NONE',  ( 1.073024830501117725E-15, 6.982962677686266711E-15, -1.000000000000000000 ) ) ;
#256599 = ORIENTED_EDGE ( 'NONE', *, *, #233858, .T. ) ;
#256598 = DIRECTION ( 'NONE',  ( 0.000000000000000000, -1.000000000000000000, -6.982962677686265922E-15 ) ) ;
#256600 = CARTESIAN_POINT ( 'NONE',  ( 20.94999999999999929, 64.58471289989986985, -237.0407535203538316 ) ) ;
#256601 = ORIENTED_EDGE ( 'NONE', *, *, #165020, .T. ) ;
#256602 = CARTESIAN_POINT ( 'NONE',  ( -16.87036670365549895, 9.989418819312803066, -180.0204398826979286 ) ) ;
#256603 = CARTESIAN_POINT ( 'NONE',  ( 18.51565452909393983, -9.352859338825888713, -74.19490932123386528 ) ) ;
#256604 = DIRECTION ( 'NONE',  ( 0.000000000000000000, 0.1568667991644863147, 0.9876197685951252359 ) ) ;
#256605 = VECTOR ( 'NONE', #61411, 1000.000000000000000 ) ;
#256606 = ORIENTED_EDGE ( 'NONE', *, *, #22098, .F. ) ;
#256607 = CARTESIAN_POINT ( 'NONE',  ( -16.89268316805466341, 66.04827818677011919, -157.3788599630699707 ) ) ;
#256608 = VERTEX_POINT ( 'NONE', #148610 ) ;
#256609 = DIRECTION ( 'NONE',  ( 2.659396599871503240E-15, -0.3850724248243104775, 0.9228863568391969530 ) ) ;
#256610 = DIRECTION ( 'NONE',  ( 1.186688945009009831E-16, -1.000000000000000000, 0.000000000000000000 ) ) ;
#256611 = CARTESIAN_POINT ( 'NONE',  ( 22.59999999999999076, 11.46682355977092804, -198.4356847424421062 ) ) ;
#256612 = ORIENTED_EDGE ( 'NONE', *, *, #236306, .T. ) ;
#256613 = FACE_OUTER_BOUND ( 'NONE', #45595, .T. ) ;
#256614 = DIRECTION ( 'NONE',  ( 0.000000000000000000, -1.000000000000000000, 0.000000000000000000 ) ) ;
#256615 = EDGE_CURVE ( 'NONE', #33086, #90057, #228143, .T. ) ;
#256616 = FACE_OUTER_BOUND ( 'NONE', #108953, .T. ) ;
#256617 = ORIENTED_EDGE ( 'NONE', *, *, #193789, .T. ) ;
#256618 = CIRCLE ( 'NONE', #144231, 11.80000000000000426 ) ;
#256619 = FACE_OUTER_BOUND ( 'NONE', #250432, .T. ) ;
#256621 = EDGE_CURVE ( 'NONE', #104983, #222021, #213913, .T. ) ;
#256620 = DIRECTION ( 'NONE',  ( 0.000000000000000000, 0.000000000000000000, 1.000000000000000000 ) ) ;
#256622 = DIRECTION ( 'NONE',  ( 0.000000000000000000, 0.000000000000000000, -1.000000000000000000 ) ) ;
#256623 = AXIS2_PLACEMENT_3D ( 'NONE', #69895, #169015, #189825 ) ;
#256624 = VERTEX_POINT ( 'NONE', #89888 ) ;
#256625 = STYLED_ITEM ( 'NONE', ( #174091 ), #29580 ) ;
#256626 = ADVANCED_FACE ( 'NONE', ( #250265 ), #169489, .T. ) ;
#256627 = FACE_OUTER_BOUND ( 'NONE', #47931, .T. ) ;
#256628 = EDGE_LOOP ( 'NONE', ( #45102, #99189, #104646, #115672 ) ) ;
#256631 = EDGE_CURVE ( 'NONE', #237980, #43295, #126614, .T. ) ;
#256630 = VERTEX_POINT ( 'NONE', #151175 ) ;
#256629 = DIRECTION ( 'NONE',  ( 0.000000000000000000, -0.9126074666063660468, -0.4088369013363524762 ) ) ;
#256634 = ORIENTED_EDGE ( 'NONE', *, *, #25261, .T. ) ;
#256633 = ORIENTED_EDGE ( 'NONE', *, *, #215235, .F. ) ;
#256632 = DIRECTION ( 'NONE',  ( 0.000000000000000000, 0.000000000000000000, -1.000000000000000000 ) ) ;
#256635 = CARTESIAN_POINT ( 'NONE',  ( 21.05000000000000071, 65.37127968600755423, -95.35819391543677170 ) ) ;
#256636 = FACE_OUTER_BOUND ( 'NONE', #177372, .T. ) ;
#256637 = CARTESIAN_POINT ( 'NONE',  ( 21.05000000000000071, 87.75000000001246292, -172.9231074845242802 ) ) ;
#256638 = CARTESIAN_POINT ( 'NONE',  ( -16.87683809663752399, 12.47642768288814707, -211.9993005936845805 ) ) ;
#256639 = DIRECTION ( 'NONE',  ( 0.000000000000000000, 0.9061079809440786281, 0.4230464831072883181 ) ) ;
#256640 = AXIS2_PLACEMENT_3D ( 'NONE', #198470, #135914, #177662 ) ;
#256641 = CARTESIAN_POINT ( 'NONE',  ( 21.05000000000000071, 65.27628289530510131, -195.8581939154368285 ) ) ;
#256642 = LINE ( 'NONE', #181035, #55539 ) ;
#256644 = DIRECTION ( 'NONE',  ( -1.000000000000000000, -0.000000000000000000, -0.000000000000000000 ) ) ;
#256643 = DIRECTION ( 'NONE',  ( 0.000000000000000000, 0.000000000000000000, -1.000000000000000000 ) ) ;
#256647 = EDGE_CURVE ( 'NONE', #204435, #143126, #97349, .T. ) ;
#256646 = VERTEX_POINT ( 'NONE', #11673 ) ;
#256645 = VECTOR ( 'NONE', #156941, 1000.000000000000114 ) ;
#256649 = ORIENTED_EDGE ( 'NONE', *, *, #252897, .T. ) ;
#256648 = AXIS2_PLACEMENT_3D ( 'NONE', #49107, #27018, #189914 ) ;
#256650 = ORIENTED_EDGE ( 'NONE', *, *, #234868, .F. ) ;
#256651 = LINE ( 'NONE', #165313, #124776 ) ;
#256653 = ORIENTED_EDGE ( 'NONE', *, *, #11399, .T. ) ;
#256652 = CARTESIAN_POINT ( 'NONE',  ( -18.50000000000000000, 85.50000000001203659, -114.7731074845242460 ) ) ;
#256655 = DIRECTION ( 'NONE',  ( 1.000000000000000000, 8.623019343401618085E-17, 8.389849937938898203E-16 ) ) ;
#256654 = TOROIDAL_SURFACE ( 'NONE', #144258, 0.2000000000000000111, 0.1000000000000000056 ) ;
#256656 = ORIENTED_EDGE ( 'NONE', *, *, #93731, .F. ) ;
#256657 = CARTESIAN_POINT ( 'NONE',  ( -37.88850191057539973, -10.80884033489985363, 6.100000000000002309 ) ) ;
#256658 = VERTEX_POINT ( 'NONE', #131594 ) ;
#256659 = FACE_OUTER_BOUND ( 'NONE', #133212, .T. ) ;
#256660 = CIRCLE ( 'NONE', #161046, 0.1000000000000009492 ) ;
#256661 = VECTOR ( 'NONE', #104984, 1000.000000000000000 ) ;
#256662 = ADVANCED_FACE ( 'NONE', ( #186450 ), #22401, .T. ) ;
#256663 = VERTEX_POINT ( 'NONE', #191608 ) ;
#256664 = DIRECTION ( 'NONE',  ( 0.000000000000000000, -0.8103668758649578141, 0.5859227990963212784 ) ) ;
#256665 = DIRECTION ( 'NONE',  ( 1.000000000000000000, -0.000000000000000000, 0.000000000000000000 ) ) ;
#256666 = EDGE_CURVE ( 'NONE', #10085, #120362, #84877, .T. ) ;
#256669 = ORIENTED_EDGE ( 'NONE', *, *, #240472, .T. ) ;
#256668 = VERTEX_POINT ( 'NONE', #38930 ) ;
#256667 = AXIS2_PLACEMENT_3D ( 'NONE', #117844, #219508, #177850 ) ;
#256670 = ORIENTED_EDGE ( 'NONE', *, *, #44948, .F. ) ;
#256671 = DIRECTION ( 'NONE',  ( 0.000000000000000000, 0.9126074666063769270, 0.4088369013363282733 ) ) ;
#256672 = AXIS2_PLACEMENT_3D ( 'NONE', #196467, #96075, #240747 ) ;
#256673 = ORIENTED_EDGE ( 'NONE', *, *, #164993, .T. ) ;
#256674 = CIRCLE ( 'NONE', #85824, 11.75000000000000533 ) ;
#256675 = ORIENTED_EDGE ( 'NONE', *, *, #76645, .F. ) ;
#256676 = DIRECTION ( 'NONE',  ( 0.000000000000000000, 0.9126074666063844765, 0.4088369013363114535 ) ) ;
#256678 = VERTEX_POINT ( 'NONE', #36378 ) ;
#256677 = LINE ( 'NONE', #252871, #72770 ) ;
#256679 = AXIS2_PLACEMENT_3D ( 'NONE', #78690, #120445, #119130 ) ;
#256681 = CARTESIAN_POINT ( 'NONE',  ( 21.05000000000000071, 76.00000000001213607, -136.5231074845242745 ) ) ;
#256680 = CARTESIAN_POINT ( 'NONE',  ( 23.15000000000000213, 82.67551891922275331, -215.5849511313000164 ) ) ;
#256682 = ADVANCED_FACE ( 'NONE', ( #137996 ), #194162, .T. ) ;
#256683 = FACE_OUTER_BOUND ( 'NONE', #5269, .T. ) ;
#256684 = DIRECTION ( 'NONE',  ( 0.000000000000000000, 1.000000000000000000, 6.982962677686266711E-15 ) ) ;
#256685 = CARTESIAN_POINT ( 'NONE',  ( 20.94999999999999929, 2.449293598294709866E-16, -31.50000000000000000 ) ) ;
#256686 = VERTEX_POINT ( 'NONE', #192869 ) ;
#256687 = ADVANCED_FACE ( 'NONE', ( #256619 ), #117178, .T. ) ;
#256688 = EDGE_LOOP ( 'NONE', ( #77923, #77754, #213893, #78060 ) ) ;
#256689 = DIRECTION ( 'NONE',  ( 0.000000000000000000, 0.9126074666063660468, 0.4088369013363524762 ) ) ;
#256690 = CARTESIAN_POINT ( 'NONE',  ( -16.86337532320261090, 66.02003279578788408, -149.0741830155416210 ) ) ;
#256691 = CARTESIAN_POINT ( 'NONE',  ( -20.64999999999999858, 36.65892442174935439, -249.5511627012433848 ) ) ;
#256692 = CIRCLE ( 'NONE', #6939, 0.1999999999999981515 ) ;
#256694 = ADVANCED_FACE ( 'NONE', ( #234544, #254097 ), #157624, .T. ) ;
#256693 = ORIENTED_EDGE ( 'NONE', *, *, #48590, .F. ) ;
#256695 = DIRECTION ( 'NONE',  ( 1.000000000000000000, -1.207181226542539700E-16, 2.694675058168174199E-16 ) ) ;
#256696 = CARTESIAN_POINT ( 'NONE',  ( -16.93415306273742260, 51.65501928279542199, -231.8802803063003353 ) ) ;
#256697 = CARTESIAN_POINT ( 'NONE',  ( -15.75000000000001066, 12.65163926562330765, -215.1534139431610413 ) ) ;
#256698 = ORIENTED_EDGE ( 'NONE', *, *, #103185, .T. ) ;
#256699 = ORIENTED_EDGE ( 'NONE', *, *, #112993, .F. ) ;
#256700 = DIRECTION ( 'NONE',  ( 1.000000000000000000, 7.304098846218133681E-16, -4.217023435051677501E-16 ) ) ;
#256701 = DIRECTION ( 'NONE',  ( -0.000000000000000000, 1.000000000000000000, -0.000000000000000000 ) ) ;
#256702 = ORIENTED_EDGE ( 'NONE', *, *, #107805, .F. ) ;
#256703 = CARTESIAN_POINT ( 'NONE',  ( -23.15000000000000213, -9.000000000000003553, -9.893969122652444881 ) ) ;
#256704 = ORIENTED_EDGE ( 'NONE', *, *, #211019, .F. ) ;
#256705 = EDGE_CURVE ( 'NONE', #40935, #153112, #51562, .T. ) ;
#256706 = DIRECTION ( 'NONE',  ( -1.000000000000000000, -0.000000000000000000, -0.000000000000000000 ) ) ;
#256707 = DIRECTION ( 'NONE',  ( 0.000000000000000000, -1.000000000000000000, 0.000000000000000000 ) ) ;
#256709 = CARTESIAN_POINT ( 'NONE',  ( -20.94999999999999929, 68.00366762990589109, -224.2307594727497815 ) ) ;
#256708 = FACE_OUTER_BOUND ( 'NONE', #161487, .T. ) ;
#256710 = VECTOR ( 'NONE', #172985, 1000.000000000000000 ) ;
#256711 = DIRECTION ( 'NONE',  ( 0.000000000000000000, -0.8660254037844383745, 0.5000000000000003331 ) ) ;
#256712 = VECTOR ( 'NONE', #67134, 1000.000000000000000 ) ;
#256714 = ADVANCED_FACE ( 'NONE', ( #53346 ), #113947, .T. ) ;
#256713 = LINE ( 'NONE', #78114, #137009 ) ;
#256715 = CIRCLE ( 'NONE', #181751, 0.09999999999999971412 ) ;
#256716 = VECTOR ( 'NONE', #160805, 1000.000000000000000 ) ;
#256717 = CARTESIAN_POINT ( 'NONE',  ( -18.59999999999999787, 8.980461154494397746, -187.0187154576991304 ) ) ;
#256718 = AXIS2_PLACEMENT_3D ( 'NONE', #12026, #131945, #250602 ) ;
#256720 = EDGE_LOOP ( 'NONE', ( #253218, #199465, #75303, #183610 ) ) ;
#256719 = VERTEX_POINT ( 'NONE', #37656 ) ;
#256721 = ORIENTED_EDGE ( 'NONE', *, *, #67626, .F. ) ;
#256722 = DIRECTION ( 'NONE',  ( -0.000000000000000000, 1.000000000000000000, -0.000000000000000000 ) ) ;
#256723 = DIRECTION ( 'NONE',  ( -0.7071067811865388020, 0.7071067811865561215, 0.000000000000000000 ) ) ;
#256724 = DIRECTION ( 'NONE',  ( -1.000000000000000000, 0.000000000000000000, -0.000000000000000000 ) ) ;
#256725 = LINE ( 'NONE', #40340, #166008 ) ;
#256726 = AXIS2_PLACEMENT_3D ( 'NONE', #115321, #93191, #172782 ) ;
#256727 = CARTESIAN_POINT ( 'NONE',  ( -15.70407651835961005, 66.64419340838171024, -86.73200495297821533 ) ) ;
#256728 = CARTESIAN_POINT ( 'NONE',  ( -18.40000000000000213, 5.650000000011139001, -79.65000000000004832 ) ) ;
#256729 = ORIENTED_EDGE ( 'NONE', *, *, #50299, .T. ) ;
#256730 = CARTESIAN_POINT ( 'NONE',  ( 21.00023020733438273, 69.60913075474394418, -69.52310748452435973 ) ) ;
#256731 = AXIS2_PLACEMENT_3D ( 'NONE', #251604, #131655, #112116 ) ;
#256732 = ORIENTED_EDGE ( 'NONE', *, *, #152364, .F. ) ;
#256733 = ORIENTED_EDGE ( 'NONE', *, *, #225891, .F. ) ;
#256734 = DIRECTION ( 'NONE',  ( -1.000000000000000000, 0.000000000000000000, 0.000000000000000000 ) ) ;
#256735 = CIRCLE ( 'NONE', #127797, 4.300000000000024691 ) ;
#256736 = DIRECTION ( 'NONE',  ( -3.469446951953635015E-14, 1.000000000000000000, 0.000000000000000000 ) ) ;
#256737 = CARTESIAN_POINT ( 'NONE',  ( -16.89268316805466341, 9.951721813253341153, -180.1442475214544174 ) ) ;
#256738 = CARTESIAN_POINT ( 'NONE',  ( 12.60053434924910043, 9.389534562357859215, -82.67480930438998143 ) ) ;
#256739 = FACE_OUTER_BOUND ( 'NONE', #142891, .T. ) ;
#256740 = EDGE_LOOP ( 'NONE', ( #120094, #131175, #26807, #176536 ) ) ;
#256741 = ORIENTED_EDGE ( 'NONE', *, *, #103038, .F. ) ;
#256742 = DIRECTION ( 'NONE',  ( 0.000000000000000000, 0.8660254037844352659, -0.5000000000000058842 ) ) ;
#256743 = AXIS2_PLACEMENT_3D ( 'NONE', #62053, #219820, #196404 ) ;
#256744 = DIRECTION ( 'NONE',  ( 0.000000000000000000, -0.4721928772777346239, -0.8814952561688430555 ) ) ;
#256745 = ORIENTED_EDGE ( 'NONE', *, *, #48816, .F. ) ;
#256746 = CARTESIAN_POINT ( 'NONE',  ( -17.04295772865662073, 23.01343443466265271, -230.8690399230656851 ) ) ;
#256747 = CARTESIAN_POINT ( 'NONE',  ( 21.05000000000000071, -8.999999999988844479, -143.8939691226524644 ) ) ;
#256748 = CARTESIAN_POINT ( 'NONE',  ( 19.99999999999998934, 64.35000000001198828, -115.2731074845243739 ) ) ;
#256749 = DIRECTION ( 'NONE',  ( 0.000000000000000000, 0.000000000000000000, -1.000000000000000000 ) ) ;
#256750 = SPHERICAL_SURFACE ( 'NONE', #129193, 0.1000000000000000056 ) ;
#256752 = PLANE ( 'NONE',  #137335 ) ;
#256751 = FACE_OUTER_BOUND ( 'NONE', #211937, .T. ) ;
#256753 = DIRECTION ( 'NONE',  ( 0.000000000000000000, 0.000000000000000000, 1.000000000000000000 ) ) ;
#256754 = CARTESIAN_POINT ( 'NONE',  ( -21.44999999999999929, 68.85000000001186038, -90.77310748452435973 ) ) ;
#256756 = ADVANCED_FACE ( 'NONE', ( #251539 ), #213697, .T. ) ;
#256755 = CARTESIAN_POINT ( 'NONE',  ( 18.49999999999999289, 10.80300742114540391, -220.2930047078982625 ) ) ;
#256757 = DIRECTION ( 'NONE',  ( 0.000000000000000000, 0.2128009952263605342, -0.9770955615653316162 ) ) ;
#256760 = VERTEX_POINT ( 'NONE', #195449 ) ;
#256759 = AXIS2_PLACEMENT_3D ( 'NONE', #152921, #154220, #226647 ) ;
#256758 = CARTESIAN_POINT ( 'NONE',  ( -16.94107738177414291, 10.01423928514777373, -54.44999999999999574 ) ) ;
#256761 = AXIS2_PLACEMENT_3D ( 'NONE', #158671, #136485, #2115 ) ;
#256762 = DIRECTION ( 'NONE',  ( 0.000000000000000000, 1.000000000000000000, 0.000000000000000000 ) ) ;
#256763 = EDGE_CURVE ( 'NONE', #159614, #121293, #193084, .T. ) ;
#256764 = ORIENTED_EDGE ( 'NONE', *, *, #47858, .F. ) ;
#256765 = DIRECTION ( 'NONE',  ( -1.000000000000000000, 0.000000000000000000, 0.000000000000000000 ) ) ;
#256767 = EDGE_CURVE ( 'NONE', #205939, #242970, #247223, .T. ) ;
#256766 = FACE_OUTER_BOUND ( 'NONE', #144008, .T. ) ;
#256768 = EDGE_CURVE ( 'NONE', #2493, #201172, #55652, .T. ) ;
#256769 = ORIENTED_EDGE ( 'NONE', *, *, #242076, .T. ) ;
#256770 = DIRECTION ( 'NONE',  ( -1.000000000000000000, 0.000000000000000000, 0.000000000000000000 ) ) ;
#256771 = CARTESIAN_POINT ( 'NONE',  ( -20.85000000000000142, -1.249999999988843369, -108.3004807544151333 ) ) ;
#256772 = DIRECTION ( 'NONE',  ( 1.000000000000000000, 0.000000000000000000, 0.000000000000000000 ) ) ;
#256773 = DIRECTION ( 'NONE',  ( 0.000000000000000000, -0.9908441862701596881, 0.1350103645451904977 ) ) ;
#256774 = CARTESIAN_POINT ( 'NONE',  ( 18.43709777086140278, 85.68240343348807642, -62.86626410711147628 ) ) ;
#256775 = CARTESIAN_POINT ( 'NONE',  ( -23.25000000000000000, 77.26488334054519669, -241.9697969554615611 ) ) ;
#256776 = AXIS2_PLACEMENT_3D ( 'NONE', #10936, #55150, #214264 ) ;
#256777 = VERTEX_POINT ( 'NONE', #97574 ) ;
#256778 = FACE_OUTER_BOUND ( 'NONE', #228885, .T. ) ;
#256780 = ORIENTED_EDGE ( 'NONE', *, *, #53486, .F. ) ;
#256779 = CARTESIAN_POINT ( 'NONE',  ( -21.05000000000000071, 14.00000000001115374, -61.57290746961752603 ) ) ;
#256781 = EDGE_CURVE ( 'NONE', #143932, #244869, #55882, .T. ) ;
#256782 = DIRECTION ( 'NONE',  ( 1.000000000000000000, 0.000000000000000000, -0.000000000000000000 ) ) ;
#256783 = CARTESIAN_POINT ( 'NONE',  ( 23.14999999999998437, 1.115650265596050101E-11, -62.95000000000004547 ) ) ;
#256784 = ORIENTED_EDGE ( 'NONE', *, *, #56548, .F. ) ;
#256785 = CARTESIAN_POINT ( 'NONE',  ( 18.54999999999999716, 9.950000000011153034, -146.6499999999999773 ) ) ;
#256786 = APPLICATION_PROTOCOL_DEFINITION ( 'draft international standard', 'automotive_design', 1998, #12422 ) ;
#256787 = CARTESIAN_POINT ( 'NONE',  ( -18.51555513499573635, 85.35265705451607232, -95.82793758882698398 ) ) ;
#256788 = ORIENTED_EDGE ( 'NONE', *, *, #222745, .F. ) ;
#256789 = DIRECTION ( 'NONE',  ( 0.000000000000000000, -0.9651348961777157509, 0.2617529984165031243 ) ) ;
#256790 = CARTESIAN_POINT ( 'NONE',  ( 12.25000000000000000, 13.18880795147152618, -215.2702608532411830 ) ) ;
#256791 = AXIS2_PLACEMENT_3D ( 'NONE', #20711, #140629, #239746 ) ;
#256792 = CARTESIAN_POINT ( 'NONE',  ( 20.85000000000000142, 77.14957036958705316, -28.20719500002235236 ) ) ;
#256793 = EDGE_CURVE ( 'NONE', #51386, #160519, #30782, .T. ) ;
#256794 = ORIENTED_EDGE ( 'NONE', *, *, #124347, .T. ) ;
#256795 = ADVANCED_FACE ( 'NONE', ( #214979 ), #234764, .F. ) ;
#256796 = ORIENTED_EDGE ( 'NONE', *, *, #146236, .T. ) ;
#256797 = DIRECTION ( 'NONE',  ( -0.000000000000000000, 1.000000000000000000, -0.000000000000000000 ) ) ;
#256798 = AXIS2_PLACEMENT_3D ( 'NONE', #195907, #156790, #217988 ) ;
#256799 = FACE_OUTER_BOUND ( 'NONE', #57522, .T. ) ;
#256800 = DIRECTION ( 'NONE',  ( 0.000000000000000000, -5.551115123125777653E-14, 1.000000000000000000 ) ) ;
#256801 = DIRECTION ( 'NONE',  ( 1.000000000000000000, 0.000000000000000000, 0.000000000000000000 ) ) ;
#256802 = EDGE_CURVE ( 'NONE', #95681, #124743, #122337, .T. ) ;
#256805 = FACE_OUTER_BOUND ( 'NONE', #163029, .T. ) ;
#256804 = VECTOR ( 'NONE', #137550, 1000.000000000000114 ) ;
#256803 = FACE_OUTER_BOUND ( 'NONE', #124998, .T. ) ;
#256806 = CARTESIAN_POINT ( 'NONE',  ( 20.86777300164945004, 65.66799936921481162, -30.42993998886010587 ) ) ;
#256807 = CARTESIAN_POINT ( 'NONE',  ( -16.27683809663751191, 66.65000000001234071, -160.7731074845244450 ) ) ;
#256808 = CARTESIAN_POINT ( 'NONE',  ( 18.59117750673696179, 65.66751761918619934, -30.42826094061123854 ) ) ;
#256809 = CARTESIAN_POINT ( 'NONE',  ( 18.50000000000000000, -10.35479209691423996, -60.75654098307376216 ) ) ;
#256810 = CIRCLE ( 'NONE', #15280, 4.049999999999990941 ) ;
#256811 = ORIENTED_EDGE ( 'NONE', *, *, #220741, .T. ) ;
#256812 = CIRCLE ( 'NONE', #123594, 0.1000000000000028644 ) ;
#256813 = ORIENTED_EDGE ( 'NONE', *, *, #99644, .F. ) ;
#256814 = DIRECTION ( 'NONE',  ( 1.000000000000000000, 0.000000000000000000, 0.000000000000000000 ) ) ;
#256815 = CARTESIAN_POINT ( 'NONE',  ( -21.44999999999999929, 68.65000000001205649, -124.2731074845243455 ) ) ;
#256817 = CARTESIAN_POINT ( 'NONE',  ( 21.05995757104869881, 67.22461075529132302, -191.3282023615332150 ) ) ;
#256816 = DIRECTION ( 'NONE',  ( 0.000000000000000000, 0.000000000000000000, -1.000000000000000000 ) ) ;
#256818 =( GEOMETRIC_REPRESENTATION_CONTEXT ( 3 ) GLOBAL_UNCERTAINTY_ASSIGNED_CONTEXT ( ( #53263 ) ) GLOBAL_UNIT_ASSIGNED_CONTEXT ( ( #55069, #151665, #75952 ) ) REPRESENTATION_CONTEXT ( 'NONE', 'WORKASPACE' ) );
#256819 = CARTESIAN_POINT ( 'NONE',  ( -18.40000000000000213, 64.25000000001151079, -45.27310748452440947 ) ) ;
#256820 = CARTESIAN_POINT ( 'NONE',  ( 20.94999999999999929, 6.450000000011156587, -144.0170271704400307 ) ) ;
#256821 = CIRCLE ( 'NONE', #169632, 0.09999999999999839573 ) ;
#256822 = CARTESIAN_POINT ( 'NONE',  ( 14.22916352759893321, 13.17759476088265380, -217.0636392655389670 ) ) ;
#256823 = VERTEX_POINT ( 'NONE', #212437 ) ;
#256824 = ORIENTED_EDGE ( 'NONE', *, *, #126217, .F. ) ;
#256825 = CARTESIAN_POINT ( 'NONE',  ( 23.24999999999999645, 5.600000000011153389, -188.5947339810868755 ) ) ;
#256826 = VERTEX_POINT ( 'NONE', #58452 ) ;
#256827 = CARTESIAN_POINT ( 'NONE',  ( 23.15000000000000213, -9.000000000000000000, -23.60603087734755690 ) ) ;
#256828 = AXIS2_PLACEMENT_3D ( 'NONE', #202323, #143628, #104477 ) ;
#256829 = AXIS2_PLACEMENT_3D ( 'NONE', #90193, #188043, #129338 ) ;
#256830 = DIRECTION ( 'NONE',  ( 0.000000000000000000, 0.2617529984164564949, 0.9651348961777284075 ) ) ;
#256831 = EDGE_CURVE ( 'NONE', #54825, #137582, #35110, .T. ) ;
#256832 = AXIS2_PLACEMENT_3D ( 'NONE', #92884, #169916, #73366 ) ;
#256833 = EDGE_CURVE ( 'NONE', #56467, #243852, #163991, .T. ) ;
#256835 = ORIENTED_EDGE ( 'NONE', *, *, #128489, .F. ) ;
#256834 = TOROIDAL_SURFACE ( 'NONE', #186166, 11.70000000000000462, 0.1000000000000000056 ) ;
#256836 = CARTESIAN_POINT ( 'NONE',  ( -16.92209698673626050, 66.05000000001263061, -190.8124719174703614 ) ) ;
#256837 = ORIENTED_EDGE ( 'NONE', *, *, #938, .T. ) ;
#256838 = CIRCLE ( 'NONE', #36350, 3.900000000000000799 ) ;
#256839 = EDGE_CURVE ( 'NONE', #44305, #89936, #172447, .T. ) ;
#256841 = EDGE_CURVE ( 'NONE', #207248, #35313, #130699, .T. ) ;
#256840 = FACE_OUTER_BOUND ( 'NONE', #23277, .T. ) ;
#256842 = AXIS2_PLACEMENT_3D ( 'NONE', #201251, #181706, #57877 ) ;
#256843 = CARTESIAN_POINT ( 'NONE',  ( -23.15000000000000213, -11.75000000000000000, 3.469446951953614189E-15 ) ) ;
#256844 = DIRECTION ( 'NONE',  ( 1.000000000000000000, 0.000000000000000000, 0.000000000000000000 ) ) ;
#256845 = CARTESIAN_POINT ( 'NONE',  ( -23.15000000000000213, 64.35000000001146248, -43.03791325517834565 ) ) ;
#256846 = CARTESIAN_POINT ( 'NONE',  ( 21.05000000000000071, 65.60157203287515415, -241.9458622313809144 ) ) ;
#256848 = DIRECTION ( 'NONE',  ( -1.000000000000000000, 0.000000000000000000, -0.000000000000000000 ) ) ;
#256847 = CARTESIAN_POINT ( 'NONE',  ( -20.94999999999999929, 61.95000000001248708, -175.5368025552853624 ) ) ;
#256849 = DIRECTION ( 'NONE',  ( 0.000000000000000000, 1.000000000000000000, -0.000000000000000000 ) ) ;
#256850 = EDGE_LOOP ( 'NONE', ( #135520, #57214, #155409, #172350 ) ) ;
#256852 = CARTESIAN_POINT ( 'NONE',  ( -11.59999999999994458, 64.25000000001119815, -18.32310748452479388 ) ) ;
#256851 = CARTESIAN_POINT ( 'NONE',  ( -23.15000000000000213, -11.64999999998884483, -164.5000000000000000 ) ) ;
#256853 = ORIENTED_EDGE ( 'NONE', *, *, #14460, .T. ) ;
#256855 = ORIENTED_EDGE ( 'NONE', *, *, #138757, .T. ) ;
#256854 = LINE ( 'NONE', #22175, #185788 ) ;
#256856 = EDGE_CURVE ( 'NONE', #45497, #157258, #243530, .T. ) ;
#256857 = CIRCLE ( 'NONE', #32077, 0.1000000000000028644 ) ;
#256858 = VERTEX_POINT ( 'NONE', #24508 ) ;
#256859 = PLANE ( 'NONE',  #161690 ) ;
#256861 = EDGE_CURVE ( 'NONE', #240778, #135871, #251506, .T. ) ;
#256860 = EDGE_CURVE ( 'NONE', #209659, #100827, #141856, .T. ) ;
#256862 = AXIS2_PLACEMENT_3D ( 'NONE', #111196, #73385, #89049 ) ;
#256863 = DIRECTION ( 'NONE',  ( -1.186688945009010077E-16, -0.9651348961777157509, 0.2617529984165031243 ) ) ;
#256864 = AXIS2_PLACEMENT_3D ( 'NONE', #226372, #28236, #228978 ) ;
#256865 = DIRECTION ( 'NONE',  ( 0.000000000000000000, 0.000000000000000000, 1.000000000000000000 ) ) ;
#256866 = CARTESIAN_POINT ( 'NONE',  ( -21.05000000000000071, 43.52285900727589762, -245.0935880436369985 ) ) ;
#256867 = ORIENTED_EDGE ( 'NONE', *, *, #104417, .F. ) ;
#256868 = DIRECTION ( 'NONE',  ( 0.000000000000000000, 0.000000000000000000, -1.000000000000000000 ) ) ;
#256869 = DIRECTION ( 'NONE',  ( -1.000000000000000000, -0.000000000000000000, -0.000000000000000000 ) ) ;
#256871 = EDGE_CURVE ( 'NONE', #220201, #146363, #26677, .T. ) ;
#256870 = DIRECTION ( 'NONE',  ( 0.000000000000000000, 0.000000000000000000, -1.000000000000000000 ) ) ;
#256872 = ORIENTED_EDGE ( 'NONE', *, *, #151809, .F. ) ;
#256873 = EDGE_CURVE ( 'NONE', #124743, #256334, #62334, .T. ) ;
#256874 = AXIS2_PLACEMENT_3D ( 'NONE', #146389, #142545, #202533 ) ;
#256875 = CARTESIAN_POINT ( 'NONE',  ( 18.49999999999998934, 56.14960075277857499, -134.2428044267230689 ) ) ;
#256876 = ORIENTED_EDGE ( 'NONE', *, *, #35886, .F. ) ;
#256877 = ORIENTED_EDGE ( 'NONE', *, *, #212490, .F. ) ;
#256878 = CARTESIAN_POINT ( 'NONE',  ( -16.86445178670582479, 9.962211629127164514, -188.3907774381173112 ) ) ;
#256879 = EDGE_CURVE ( 'NONE', #127472, #222808, #93288, .T. ) ;
#256880 = EDGE_CURVE ( 'NONE', #7765, #144828, #14016, .T. ) ;
#256881 = ORIENTED_EDGE ( 'NONE', *, *, #154410, .T. ) ;
#256882 = CARTESIAN_POINT ( 'NONE',  ( -18.41431012584568805, 11.48747202920816868, -9.226763986898326664 ) ) ;
#256883 = VERTEX_POINT ( 'NONE', #203119 ) ;
#256884 = CARTESIAN_POINT ( 'NONE',  ( -11.60000000000000320, -11.65000000000000036, 12.40000000000000391 ) ) ;
#256885 = ADVANCED_FACE ( 'NONE', ( #182291 ), #40230, .F. ) ;
#256886 = CARTESIAN_POINT ( 'NONE',  ( -18.39999999999999858, 85.50000000001161027, -62.52382180668540457 ) ) ;
#256887 = CARTESIAN_POINT ( 'NONE',  ( 21.70464131381650219, 68.90464198104483273, -203.5231074845243882 ) ) ;
#256888 = DIRECTION ( 'NONE',  ( 3.616040088954497272E-32, -1.224646799147352961E-16, 1.000000000000000000 ) ) ;
#256889 = ADVANCED_FACE ( 'NONE', ( #45331 ), #83132, .T. ) ;
#256890 = AXIS2_PLACEMENT_3D ( 'NONE', #244462, #21583, #80218 ) ;
#256891 = AXIS2_PLACEMENT_3D ( 'NONE', #51083, #207650, #10719 ) ;
#256892 = AXIS2_PLACEMENT_3D ( 'NONE', #163154, #47021, #242666 ) ;
#256893 = VECTOR ( 'NONE', #203217, 1000.000000000000114 ) ;
#256894 = EDGE_CURVE ( 'NONE', #158009, #1224, #18468, .T. ) ;
#256895 = DIRECTION ( 'NONE',  ( 1.000000000000000000, -3.265361837132813093E-16, -2.280189983783949500E-30 ) ) ;
#256896 = CARTESIAN_POINT ( 'NONE',  ( -21.08376601933334271, 0.06377601094103470258, -27.15805272872427523 ) ) ;
#256897 = DIRECTION ( 'NONE',  ( 0.000000000000000000, 0.8814952561688437216, -0.4721928772777334582 ) ) ;
#256898 = VERTEX_POINT ( 'NONE', #199281 ) ;
#256900 = CARTESIAN_POINT ( 'NONE',  ( -23.15000000000000213, 42.98415524044399660, -233.9519173640447889 ) ) ;
#256899 = CARTESIAN_POINT ( 'NONE',  ( -23.25000000000000000, 69.01799029515568407, -132.8269553662681233 ) ) ;
#256901 = ORIENTED_EDGE ( 'NONE', *, *, #243569, .F. ) ;
#256904 = VERTEX_POINT ( 'NONE', #103991 ) ;
#256903 = FACE_OUTER_BOUND ( 'NONE', #117309, .T. ) ;
#256902 = CARTESIAN_POINT ( 'NONE',  ( -21.05000000000000071, 1.115600667400684642E-11, -167.4999999999999716 ) ) ;
#256905 = AXIS2_PLACEMENT_3D ( 'NONE', #143493, #44415, #206045 ) ;
#256906 = ORIENTED_EDGE ( 'NONE', *, *, #88429, .F. ) ;
#256907 = DIRECTION ( 'NONE',  ( 1.000000000000000000, 0.000000000000000000, 0.000000000000000000 ) ) ;
#256908 = CARTESIAN_POINT ( 'NONE',  ( 21.09107601085565165, 0.03930716472848838627, -60.63612202464012313 ) ) ;
#256909 = CARTESIAN_POINT ( 'NONE',  ( 18.59999999999999076, 64.35000000001245724, -181.7731074845244450 ) ) ;
#256910 = LINE ( 'NONE', #156619, #187551 ) ;
#256911 = ORIENTED_EDGE ( 'NONE', *, *, #65647, .T. ) ;
#256912 = CYLINDRICAL_SURFACE ( 'NONE', #213668, 14.30833333333333357 ) ;
#256913 = ADVANCED_FACE ( 'NONE', ( #144402 ), #164006, .F. ) ;
#256914 = PLANE ( 'NONE',  #186170 ) ;
#256916 = DIRECTION ( 'NONE',  ( 0.000000000000000000, -6.352154140967427193E-15, 1.000000000000000000 ) ) ;
#256915 = CARTESIAN_POINT ( 'NONE',  ( -20.64999999999999858, 7.250000000011155521, -146.2500000000000284 ) ) ;
#256917 = VECTOR ( 'NONE', #179784, 1000.000000000000000 ) ;
#256919 = ORIENTED_EDGE ( 'NONE', *, *, #108550, .T. ) ;
#256918 = LINE ( 'NONE', #216554, #84906 ) ;
#256920 = AXIS2_PLACEMENT_3D ( 'NONE', #137867, #216128, #120922 ) ;
#256921 = VERTEX_POINT ( 'NONE', #122306 ) ;
#256922 = B_SPLINE_CURVE_WITH_KNOTS ( 'NONE', 3,
 ( #34839, #50494, #190038, #10116, #114350, #191349 ),
 .UNSPECIFIED., .F., .F.,
 ( 4, 2, 4 ),
 ( 0.000000000000000000, 0.0002113392456165961845, 0.0004226784912331923690 ),
 .UNSPECIFIED. ) ;
#256923 = TOROIDAL_SURFACE ( 'NONE', #144532, 11.90000000000000213, 0.1000000000000000056 ) ;
#256924 = DIRECTION ( 'NONE',  ( -4.408576920032448588E-17, -0.1350103645451807555, -0.9908441862701609093 ) ) ;
#256925 = ORIENTED_EDGE ( 'NONE', *, *, #36961, .T. ) ;
#256926 = DIRECTION ( 'NONE',  ( 1.000000000000000000, 0.000000000000000000, 0.000000000000000000 ) ) ;
#256927 = ORIENTED_EDGE ( 'NONE', *, *, #83032, .T. ) ;
#256928 = CARTESIAN_POINT ( 'NONE',  ( -16.27683809663750480, 66.65000000001191438, -93.77310748452437394 ) ) ;
#256929 = DIRECTION ( 'NONE',  ( -1.000000000000000000, 0.000000000000000000, 0.000000000000000000 ) ) ;
#256930 = DIRECTION ( 'NONE',  ( 0.000000000000000000, -0.9651348961777155289, 0.2617529984165036794 ) ) ;
#256931 = ORIENTED_EDGE ( 'NONE', *, *, #257421, .F. ) ;
#256932 = LINE ( 'NONE', #78335, #237551 ) ;
#256933 = EDGE_CURVE ( 'NONE', #6309, #213361, #164226, .T. ) ;
#256934 = AXIS2_PLACEMENT_3D ( 'NONE', #93901, #13104, #211291 ) ;
#256935 = CIRCLE ( 'NONE', #256759, 0.09999999999999949207 ) ;
#256937 = EDGE_CURVE ( 'NONE', #76326, #96909, #51752, .T. ) ;
#256936 = CARTESIAN_POINT ( 'NONE',  ( 21.14999999999999858, 64.35000000001237197, -169.9231074845244507 ) ) ;
#256938 = CIRCLE ( 'NONE', #148678, 0.09999999999999062417 ) ;
#256939 = AXIS2_PLACEMENT_3D ( 'NONE', #28141, #163783, #24286 ) ;
#256940 = ORIENTED_EDGE ( 'NONE', *, *, #127575, .T. ) ;
#256941 = ORIENTED_EDGE ( 'NONE', *, *, #35369, .T. ) ;
#256942 = ORIENTED_EDGE ( 'NONE', *, *, #184069, .T. ) ;
#256943 = ADVANCED_FACE ( 'NONE', ( #170468 ), #226509, .F. ) ;
#256944 = CARTESIAN_POINT ( 'NONE',  ( -23.15000000000000213, 70.60814576644823148, -215.7631455941064189 ) ) ;
#256945 = EDGE_LOOP ( 'NONE', ( #32854, #5404, #75334, #176954 ) ) ;
#256948 = ADVANCED_FACE ( 'NONE', ( #145700 ), #127437, .F. ) ;
#256947 = VERTEX_POINT ( 'NONE', #189982 ) ;
#256946 = CARTESIAN_POINT ( 'NONE',  ( 22.01447462590973458, 75.90096299995246909, -110.2869076857542154 ) ) ;
#256949 = ORIENTED_EDGE ( 'NONE', *, *, #96111, .T. ) ;
#256952 = ORIENTED_EDGE ( 'NONE', *, *, #152722, .T. ) ;
#256951 = ORIENTED_EDGE ( 'NONE', *, *, #47512, .F. ) ;
#256950 = FACE_OUTER_BOUND ( 'NONE', #168957, .T. ) ;
#256953 = CIRCLE ( 'NONE', #136344, 12.77499999999998970 ) ;
#256954 = TOROIDAL_SURFACE ( 'NONE', #206937, 0.2000000000000000111, 0.1000000000000000056 ) ;
#256955 = AXIS2_PLACEMENT_3D ( 'NONE', #245620, #185646, #66974 ) ;
#256956 = ORIENTED_EDGE ( 'NONE', *, *, #143253, .T. ) ;
#256957 = FACE_OUTER_BOUND ( 'NONE', #159399, .T. ) ;
#256958 = DIRECTION ( 'NONE',  ( 0.000000000000000000, 0.000000000000000000, -1.000000000000000000 ) ) ;
#256959 = ADVANCED_FACE ( 'NONE', ( #124875 ), #225226, .F. ) ;
#256960 = AXIS2_PLACEMENT_3D ( 'NONE', #114210, #95912, #175489 ) ;
#256961 = LINE ( 'NONE', #181349, #67497 ) ;
#256962 = ORIENTED_EDGE ( 'NONE', *, *, #91028, .T. ) ;
#256963 = DIRECTION ( 'NONE',  ( 1.000000000000000000, 0.000000000000000000, 0.000000000000000000 ) ) ;
#256965 = ORIENTED_EDGE ( 'NONE', *, *, #120353, .T. ) ;
#256964 = CARTESIAN_POINT ( 'NONE',  ( -21.64999999999999858, 11.60596396992029433, -220.2204734678737168 ) ) ;
#256966 = DIRECTION ( 'NONE',  ( 1.000000000000000000, 0.000000000000000000, 0.000000000000000000 ) ) ;
#256968 = ORIENTED_EDGE ( 'NONE', *, *, #252973, .F. ) ;
#256967 = CARTESIAN_POINT ( 'NONE',  ( -20.64999999999999858, 4.350000000011156054, -121.7500000000000426 ) ) ;
#256969 = VERTEX_POINT ( 'NONE', #247370 ) ;
#256970 = LINE ( 'NONE', #191952, #15142 ) ;
#256971 = CARTESIAN_POINT ( 'NONE',  ( 18.43565242384933711, 85.51932773110434027, -96.05013110796494402 ) ) ;
#256972 = ORIENTED_EDGE ( 'NONE', *, *, #157717, .F. ) ;
#256973 = ORIENTED_EDGE ( 'NONE', *, *, #148055, .T. ) ;
#256974 = DIRECTION ( 'NONE',  ( 3.469446951953515108E-14, 0.000000000000000000, 1.000000000000000000 ) ) ;
#256975 = CARTESIAN_POINT ( 'NONE',  ( -23.25000000000000000, -0.1008583690875562017, -122.2504328765106294 ) ) ;
#256976 = VECTOR ( 'NONE', #145123, 1000.000000000000000 ) ;
#256977 = EDGE_CURVE ( 'NONE', #47498, #24511, #105919, .T. ) ;
#256979 = VERTEX_POINT ( 'NONE', #150851 ) ;
#256978 = ORIENTED_EDGE ( 'NONE', *, *, #12817, .F. ) ;
#256980 = ORIENTED_EDGE ( 'NONE', *, *, #33969, .T. ) ;
#256981 = CARTESIAN_POINT ( 'NONE',  ( 21.05000000000000071, 76.00000000001243450, -168.1231074845243540 ) ) ;
#256982 = ORIENTED_EDGE ( 'NONE', *, *, #117250, .F. ) ;
#256983 = ORIENTED_EDGE ( 'NONE', *, *, #34764, .F. ) ;
#256984 = PLANE ( 'NONE',  #34225 ) ;
#256985 = ORIENTED_EDGE ( 'NONE', *, *, #98015, .F. ) ;
#256986 = DIRECTION ( 'NONE',  ( -1.000000000000000000, 0.000000000000000000, -0.000000000000000000 ) ) ;
#256987 = CIRCLE ( 'NONE', #144593, 1.500000000000001332 ) ;
#256989 = CYLINDRICAL_SURFACE ( 'NONE', #190024, 7.900000000000000355 ) ;
#256988 = DIRECTION ( 'NONE',  ( 0.000000000000000000, 0.9893560106964510714, -0.1455152366551481502 ) ) ;
#256990 = EDGE_CURVE ( 'NONE', #166894, #6267, #186128, .T. ) ;
#256991 = ORIENTED_EDGE ( 'NONE', *, *, #69886, .T. ) ;
#256992 = EDGE_CURVE ( 'NONE', #171429, #162828, #43408, .T. ) ;
#256994 = VERTEX_POINT ( 'NONE', #85699 ) ;
#256993 = ORIENTED_EDGE ( 'NONE', *, *, #131843, .F. ) ;
#256995 = CIRCLE ( 'NONE', #148739, 0.09999999999999939493 ) ;
#256996 = DIRECTION ( 'NONE',  ( 0.000000000000000000, 0.000000000000000000, -1.000000000000000000 ) ) ;
#256997 = DIRECTION ( 'NONE',  ( -1.000000000000000000, -8.673617379884087537E-15, 0.000000000000000000 ) ) ;
#256998 = ORIENTED_EDGE ( 'NONE', *, *, #163797, .F. ) ;
#256999 = VECTOR ( 'NONE', #66113, 1000.000000000000000 ) ;
#257000 = PRODUCT_DEFINITION_FORMATION_WITH_SPECIFIED_SOURCE ( 'ANY', '', #203297, .NOT_KNOWN. ) ;
#257001 = ADVANCED_FACE ( 'NONE', ( #165278 ), #101629, .T. ) ;
#257002 = DIRECTION ( 'NONE',  ( -1.000000000000000000, 0.000000000000000000, 0.000000000000000000 ) ) ;
#257003 = CIRCLE ( 'NONE', #32221, 3.900000000000000799 ) ;
#257004 = ORIENTED_EDGE ( 'NONE', *, *, #76568, .F. ) ;
#257005 = ORIENTED_EDGE ( 'NONE', *, *, #150699, .F. ) ;
#257006 = DIRECTION ( 'NONE',  ( 0.000000000000000000, -1.000000000000000000, -6.982962677686265922E-15 ) ) ;
#257007 = AXIS2_PLACEMENT_3D ( 'NONE', #247166, #108942, #142919 ) ;
#257009 = ADVANCED_FACE ( 'NONE', ( #30939 ), #99558, .F. ) ;
#257008 = ORIENTED_EDGE ( 'NONE', *, *, #205688, .F. ) ;
#257010 = DIRECTION ( 'NONE',  ( 1.000000000000000000, -0.000000000000000000, -0.000000000000000000 ) ) ;
#257011 = CARTESIAN_POINT ( 'NONE',  ( -20.85000000000000142, 77.13501884592203339, -95.30613060109196510 ) ) ;
#257012 = ORIENTED_EDGE ( 'NONE', *, *, #168683, .F. ) ;
#257013 = EDGE_CURVE ( 'NONE', #39027, #206635, #218353, .T. ) ;
#257014 = CARTESIAN_POINT ( 'NONE',  ( -17.22767730082740556, 10.34924421247841408, -44.85757130942987914 ) ) ;
#257016 = DIRECTION ( 'NONE',  ( 0.000000000000000000, 2.168404344971003346E-15, -1.000000000000000000 ) ) ;
#257015 = DIRECTION ( 'NONE',  ( 0.000000000000000000, -1.000000000000000000, -6.982962677686266711E-15 ) ) ;
#257017 = DIRECTION ( 'NONE',  ( 1.000000000000000000, 0.000000000000000000, 0.000000000000000000 ) ) ;
#257018 = CARTESIAN_POINT ( 'NONE',  ( -16.89021194854741026, 63.05761173939616526, -213.2313078320790396 ) ) ;
#257019 = CARTESIAN_POINT ( 'NONE',  ( -16.83199318825828072, 66.06935387203108689, -149.2955222963152266 ) ) ;
#257021 = EDGE_CURVE ( 'NONE', #108503, #199040, #6195, .T. ) ;
#257020 = DIRECTION ( 'NONE',  ( 0.000000000000000000, -1.000000000000000000, -0.000000000000000000 ) ) ;
#257022 = CYLINDRICAL_SURFACE ( 'NONE', #188867, 0.1000000000000002554 ) ;
#257023 = AXIS2_PLACEMENT_3D ( 'NONE', #110929, #127933, #52222 ) ;
#257024 = ORIENTED_EDGE ( 'NONE', *, *, #252511, .F. ) ;
#257025 = VECTOR ( 'NONE', #201515, 1000.000000000000000 ) ;
#257028 = ORIENTED_EDGE ( 'NONE', *, *, #160425, .T. ) ;
#257027 = ORIENTED_EDGE ( 'NONE', *, *, #243459, .T. ) ;
#257026 = AXIS2_PLACEMENT_3D ( 'NONE', #121422, #200920, #241346 ) ;
#257029 = ORIENTED_EDGE ( 'NONE', *, *, #60971, .T. ) ;
#257030 = VERTEX_POINT ( 'NONE', #29654 ) ;
#257031 = AXIS2_PLACEMENT_3D ( 'NONE', #87585, #207574, #69346 ) ;
#257033 = EDGE_CURVE ( 'NONE', #233341, #146715, #205674, .T. ) ;
#257032 = LINE ( 'NONE', #17208, #215410 ) ;
#257034 = DIRECTION ( 'NONE',  ( -1.000000000000000000, -0.000000000000000000, -0.000000000000000000 ) ) ;
#257035 = AXIS2_PLACEMENT_3D ( 'NONE', #172029, #196667, #97545 ) ;
#257037 = DIRECTION ( 'NONE',  ( -1.000000000000000000, -0.000000000000000000, -0.000000000000000000 ) ) ;
#257036 = CARTESIAN_POINT ( 'NONE',  ( -12.25000000000000178, 66.65000000001228386, -153.2731074845244166 ) ) ;
#257038 = ORIENTED_EDGE ( 'NONE', *, *, #24989, .F. ) ;
#257039 = CYLINDRICAL_SURFACE ( 'NONE', #250546, 0.09999999999999939493 ) ;
#257040 = DIRECTION ( 'NONE',  ( 0.000000000000000000, -0.9770955615653313941, -0.2128009952263603677 ) ) ;
#257041 = LINE ( 'NONE', #191, #22386 ) ;
#257042 = DIRECTION ( 'NONE',  ( 0.000000000000000000, 0.000000000000000000, -1.000000000000000000 ) ) ;
#257043 = ORIENTED_EDGE ( 'NONE', *, *, #92860, .T. ) ;
#257044 = AXIS2_PLACEMENT_3D ( 'NONE', #154160, #54986, #255735 ) ;
#257045 = TOROIDAL_SURFACE ( 'NONE', #223759, 0.6000000000000013101, 0.1000000000000000056 ) ;
#257046 = AXIS2_PLACEMENT_3D ( 'NONE', #94185, #217648, #239823 ) ;
#257047 = CARTESIAN_POINT ( 'NONE',  ( 21.14999999999999858, 11.65000000001115943, -100.6000000000000369 ) ) ;
#257048 = ORIENTED_EDGE ( 'NONE', *, *, #216702, .T. ) ;
#257049 = CARTESIAN_POINT ( 'NONE',  ( -18.50000000000000000, 18.81339837015603322, -226.7756228984618190 ) ) ;
#257050 = DIRECTION ( 'NONE',  ( 1.000000000000000000, 0.000000000000000000, 0.000000000000000000 ) ) ;
#257051 = LINE ( 'NONE', #173774, #198198 ) ;
#257052 = DIRECTION ( 'NONE',  ( 1.000000000000000000, 0.000000000000000000, -0.000000000000000000 ) ) ;
#257053 = VERTEX_POINT ( 'NONE', #248668 ) ;
#257054 = CARTESIAN_POINT ( 'NONE',  ( -23.25000000000000000, 1.115600667400684642E-11, -46.27499999999999858 ) ) ;
#257055 = DIRECTION ( 'NONE',  ( 0.000000000000000000, -0.9126074666063773710, -0.4088369013363274962 ) ) ;
#257056 = CARTESIAN_POINT ( 'NONE',  ( -15.55912972643740488, 67.50912972644894694, -48.57310748452438531 ) ) ;
#257057 = VECTOR ( 'NONE', #199704, 1000.000000000000000 ) ;
#257059 = DIRECTION ( 'NONE',  ( -1.000000000000000000, -2.952720810173289112E-16, 0.000000000000000000 ) ) ;
#257058 = DIRECTION ( 'NONE',  ( -1.000000000000000000, 0.000000000000000000, 0.000000000000000000 ) ) ;
#257060 = CARTESIAN_POINT ( 'NONE',  ( 21.13461538461538325, 10.61458296203669249, -45.85000000000000142 ) ) ;
#257061 = AXIS2_PLACEMENT_3D ( 'NONE', #137130, #197083, #234947 ) ;
#257062 = CARTESIAN_POINT ( 'NONE',  ( 21.05000000000000071, 84.73084112150721126, -93.42503276553991043 ) ) ;
#257063 = DIRECTION ( 'NONE',  ( 1.000000000000000000, 0.000000000000000000, 0.000000000000000000 ) ) ;
#257064 = CARTESIAN_POINT ( 'NONE',  ( -23.15000000000000213, -8.663551401858001100, -57.47589888193270014 ) ) ;
#257065 = ORIENTED_EDGE ( 'NONE', *, *, #7283, .T. ) ;
#257066 = ADVANCED_FACE ( 'NONE', ( #70058 ), #149594, .F. ) ;
#257067 = AXIS2_PLACEMENT_3D ( 'NONE', #159881, #221102, #42470 ) ;
#257068 = ORIENTED_EDGE ( 'NONE', *, *, #3372, .T. ) ;
#257069 = CARTESIAN_POINT ( 'NONE',  ( 18.50000000000000000, 78.13562659007693867, -231.5603498355943373 ) ) ;
#257070 = ORIENTED_EDGE ( 'NONE', *, *, #108273, .T. ) ;
#257071 = ADVANCED_FACE ( 'NONE', ( #175570 ), #256298, .F. ) ;
#257072 = CARTESIAN_POINT ( 'NONE',  ( -23.15000000000000213, -11.74999999998884448, -55.25000000000004974 ) ) ;
#257073 = AXIS2_PLACEMENT_3D ( 'NONE', #174635, #254098, #167234 ) ;
#257074 = CIRCLE ( 'NONE', #256494, 12.87499999999999822 ) ;
#257075 = ADVANCED_FACE ( 'NONE', ( #235513 ), #231690, .F. ) ;
#257077 = EDGE_CURVE ( 'NONE', #83539, #120381, #93460, .T. ) ;
#257076 = TOROIDAL_SURFACE ( 'NONE', #65588, 7.800000000000000711, 0.1000000000000000056 ) ;
#257078 = DIRECTION ( 'NONE',  ( 0.000000000000000000, 0.9550021345545507412, -0.2965989261549202838 ) ) ;
#257079 = AXIS2_PLACEMENT_3D ( 'NONE', #215847, #39832, #237989 ) ;
#257080 = LINE ( 'NONE', #137178, #13014 ) ;
#257081 = ORIENTED_EDGE ( 'NONE', *, *, #21133, .T. ) ;
#257082 = CIRCLE ( 'NONE', #211356, 0.5000000000000051070 ) ;
#257083 = CARTESIAN_POINT ( 'NONE',  ( -21.65000000000000213, 68.75000000001209344, -127.2731074845243597 ) ) ;
#257084 = DIRECTION ( 'NONE',  ( 0.000000000000000000, 0.000000000000000000, -1.000000000000000000 ) ) ;
#257085 = CARTESIAN_POINT ( 'NONE',  ( -21.53699400384203599, 75.99999999999828049, -109.8108192777691414 ) ) ;
#257086 = CARTESIAN_POINT ( 'NONE',  ( 21.05000000000000071, 1.115600667400684642E-11, -179.6499999999999773 ) ) ;
#257088 = EDGE_LOOP ( 'NONE', ( #15351, #3660, #82940 ) ) ;
#257087 = FACE_OUTER_BOUND ( 'NONE', #164221, .T. ) ;
#257090 = DIRECTION ( 'NONE',  ( -0.7071067811865475727, 0.7071067811865475727, 4.937700262164531476E-15 ) ) ;
#257089 = DIRECTION ( 'NONE',  ( -1.000000000000000000, 0.000000000000000000, 0.000000000000000000 ) ) ;
#257091 = EDGE_CURVE ( 'NONE', #239961, #5222, #47659, .T. ) ;
#257092 = FACE_OUTER_BOUND ( 'NONE', #174648, .T. ) ;
#257093 = CARTESIAN_POINT ( 'NONE',  ( -23.39999999999994529, 83.80000000001119531, -34.77310748452479316 ) ) ;
#257094 = DIRECTION ( 'NONE',  ( -1.000000000000000000, 0.000000000000000000, 0.000000000000000000 ) ) ;
#257096 = EDGE_CURVE ( 'NONE', #51404, #159889, #16496, .T. ) ;
#257095 = CARTESIAN_POINT ( 'NONE',  ( -20.94999999999999929, 11.75000000001115552, -40.51480577065400013 ) ) ;
#257097 = VERTEX_POINT ( 'NONE', #156011 ) ;
#257098 = CIRCLE ( 'NONE', #165591, 11.75000000000000000 ) ;
#257099 = CARTESIAN_POINT ( 'NONE',  ( -20.54999999999999716, 1.925233644870967487, -54.26975646687386501 ) ) ;
#257100 = ORIENTED_EDGE ( 'NONE', *, *, #216233, .F. ) ;
#257101 = DIRECTION ( 'NONE',  ( -1.000000000000000000, -0.000000000000000000, -0.000000000000000000 ) ) ;
#257102 = ORIENTED_EDGE ( 'NONE', *, *, #175511, .F. ) ;
#257103 = CARTESIAN_POINT ( 'NONE',  ( -23.25000000000000000, 77.83585931145526615, -58.01866831572577610 ) ) ;
#257104 = ADVANCED_FACE ( 'NONE', ( #92159 ), #155861, .F. ) ;
#257105 = DIRECTION ( 'NONE',  ( 0.000000000000000000, -0.2617529984165024026, -0.9651348961777158619 ) ) ;
#257106 = CARTESIAN_POINT ( 'NONE',  ( -23.15000000000000213, 11.75000000000000000, -21.34999999999999787 ) ) ;
#257107 = EDGE_CURVE ( 'NONE', #9105, #232658, #180785, .T. ) ;
#257108 = VERTEX_POINT ( 'NONE', #157298 ) ;
#257109 = ADVANCED_FACE ( 'NONE', ( #132580 ), #91699, .F. ) ;
#257110 = EDGE_LOOP ( 'NONE', ( #34067, #145070, #132160, #226067, #107600 ) ) ;
#257111 = CARTESIAN_POINT ( 'NONE',  ( 22.47071067811865319, 7.720074744509199505, -167.4009075452973434 ) ) ;
#257112 = DIRECTION ( 'NONE',  ( 1.000000000000000000, -1.335000415235278971E-16, 2.979993593738921214E-16 ) ) ;
#257113 = FACE_OUTER_BOUND ( 'NONE', #245165, .T. ) ;
#257114 = DIRECTION ( 'NONE',  ( 0.000000000000000000, 0.000000000000000000, -1.000000000000000000 ) ) ;
#257115 = EDGE_CURVE ( 'NONE', #139103, #39149, #247400, .T. ) ;
#257117 = CARTESIAN_POINT ( 'NONE',  ( 21.03670563405601968, 10.62482368932824173, -12.32554688620915151 ) ) ;
#257116 = CARTESIAN_POINT ( 'NONE',  ( 18.49999999999998934, 69.45000000001181206, -81.77310748452434552 ) ) ;
#257118 = CIRCLE ( 'NONE', #82349, 0.1000000000000002831 ) ;
#257119 = AXIS2_PLACEMENT_3D ( 'NONE', #37464, #17870, #58273 ) ;
#257120 = CYLINDRICAL_SURFACE ( 'NONE', #2591, 0.09999999999999939493 ) ;
#257121 = CARTESIAN_POINT ( 'NONE',  ( -20.54999999999999716, 4.350000000011156054, -155.2500000000000284 ) ) ;
#257122 = AXIS2_PLACEMENT_3D ( 'NONE', #247828, #70515, #24954 ) ;
#257123 = CARTESIAN_POINT ( 'NONE',  ( -16.98495255085916611, 65.99443563401723623, -115.6577246907448853 ) ) ;
#257124 = VERTEX_POINT ( 'NONE', #195143 ) ;
#257125 = CARTESIAN_POINT ( 'NONE',  ( 19.92426406871192412, 34.58225676390223668, -235.1091250528070304 ) ) ;
#257127 = ORIENTED_EDGE ( 'NONE', *, *, #23221, .T. ) ;
#257126 = DIRECTION ( 'NONE',  ( 1.000000000000000000, 0.000000000000000000, 0.000000000000000000 ) ) ;
#257128 = DIRECTION ( 'NONE',  ( 0.000000000000000000, 0.000000000000000000, -1.000000000000000000 ) ) ;
#257129 = CARTESIAN_POINT ( 'NONE',  ( 22.48660254037844197, 11.37252324248628987, -198.4720136275361426 ) ) ;
#257131 = CARTESIAN_POINT ( 'NONE',  ( 15.74999999999999645, 66.15000000001228386, -153.2731074845244450 ) ) ;
#257130 = DIRECTION ( 'NONE',  ( 1.000000000000000000, 0.000000000000000000, 0.000000000000000000 ) ) ;
#257132 = EDGE_LOOP ( 'NONE', ( #66306, #138836, #43695, #234402, #72466, #40446, #59800, #138641, #243299, #46939 ) ) ;
#257134 = LINE ( 'NONE', #53857, #38427 ) ;
#257133 = CYLINDRICAL_SURFACE ( 'NONE', #246749, 0.1000000000000024342 ) ;
#257135 = DIRECTION ( 'NONE',  ( -0.000000000000000000, 0.9770955615653313941, 0.2128009952263603954 ) ) ;
#257136 = DIRECTION ( 'NONE',  ( 0.000000000000000000, -6.308085367188367561E-15, 1.000000000000000000 ) ) ;
#257137 = CARTESIAN_POINT ( 'NONE',  ( -18.53317502108577131, 10.32263460347359540, -139.5605957968672328 ) ) ;
#257138 = ORIENTED_EDGE ( 'NONE', *, *, #122490, .T. ) ;
#257139 = CARTESIAN_POINT ( 'NONE',  ( -21.05000000000000071, 77.36087058720413268, -128.4501095574333362 ) ) ;
#257140 = ORIENTED_EDGE ( 'NONE', *, *, #16983, .T. ) ;
#257141 = EDGE_CURVE ( 'NONE', #1463, #95344, #5966, .T. ) ;
#257142 = AXIS2_PLACEMENT_3D ( 'NONE', #103955, #223908, #120558 ) ;
#257143 = CARTESIAN_POINT ( 'NONE',  ( -18.49513951962167013, -9.437725026677698636, -40.27807257502914240 ) ) ;
#257144 = ORIENTED_EDGE ( 'NONE', *, *, #93600, .F. ) ;
#257145 = CARTESIAN_POINT ( 'NONE',  ( 20.99999999999999645, 9.749999999999982236, -9.250000000000001776 ) ) ;
#257146 = ORIENTED_EDGE ( 'NONE', *, *, #157099, .F. ) ;
#257147 = VECTOR ( 'NONE', #239002, 1000.000000000000000 ) ;
#257148 = EDGE_CURVE ( 'NONE', #22668, #38886, #22572, .T. ) ;
#257149 = DIRECTION ( 'NONE',  ( 0.000000000000000000, -0.9770955615653551529, -0.2128009952262517601 ) ) ;
#257150 = ORIENTED_EDGE ( 'NONE', *, *, #157575, .F. ) ;
#257151 = EDGE_CURVE ( 'NONE', #216000, #243879, #13920, .T. ) ;
#257152 = SPHERICAL_SURFACE ( 'NONE', #138375, 0.1000000000000000056 ) ;
#257153 = SPHERICAL_SURFACE ( 'NONE', #24222, 0.1000000000000000056 ) ;
#257154 = CARTESIAN_POINT ( 'NONE',  ( -20.64999999999999858, 85.50000000001159606, -59.62913836187181005 ) ) ;
#257155 = DIRECTION ( 'NONE',  ( 0.000000000000000000, -0.1568667991644355497, 0.9876197685951332295 ) ) ;
#257156 = FACE_OUTER_BOUND ( 'NONE', #56087, .T. ) ;
#257157 = CARTESIAN_POINT ( 'NONE',  ( 23.24999999999999645, 5.650000000011139001, -79.65000000000004832 ) ) ;
#257158 = VECTOR ( 'NONE', #6609, 1000.000000000000000 ) ;
#257159 = VERTEX_POINT ( 'NONE', #154732 ) ;
#257160 = CARTESIAN_POINT ( 'NONE',  ( -18.59999999999999787, 1.851028230152016674, -78.65391326942254580 ) ) ;
#257162 = ORIENTED_EDGE ( 'NONE', *, *, #23221, .F. ) ;
#257161 = AXIS2_PLACEMENT_3D ( 'NONE', #168845, #227472, #48842 ) ;
#257164 = ORIENTED_EDGE ( 'NONE', *, *, #139933, .F. ) ;
#257163 = CARTESIAN_POINT ( 'NONE',  ( -20.54999999999999716, 84.66355140188112216, -112.5472086025915388 ) ) ;
#257165 = EDGE_CURVE ( 'NONE', #234233, #147787, #255748, .T. ) ;
#257166 = ORIENTED_EDGE ( 'NONE', *, *, #32987, .T. ) ;
#257167 = CARTESIAN_POINT ( 'NONE',  ( -18.59999999999999787, 76.00000000001126921, -203.5231074845248997 ) ) ;
#257168 = ADVANCED_FACE ( 'NONE', ( #251217 ), #201616, .T. ) ;
#257169 = DIRECTION ( 'NONE',  ( 0.000000000000000000, 0.000000000000000000, 1.000000000000000000 ) ) ;
#257170 = CARTESIAN_POINT ( 'NONE',  ( -18.59999999999999787, 77.83585931145526615, -58.01866831572577610 ) ) ;
#257171 = CYLINDRICAL_SURFACE ( 'NONE', #154084, 11.75000000000001066 ) ;
#257172 = ORIENTED_EDGE ( 'NONE', *, *, #222878, .T. ) ;
#257173 = DIRECTION ( 'NONE',  ( 1.000000000000000000, -7.304098846218135653E-16, -2.111765289898286048E-31 ) ) ;
#257174 = CIRCLE ( 'NONE', #186503, 0.1000000000000124678 ) ;
#257175 = DIRECTION ( 'NONE',  ( 0.000000000000000000, 0.000000000000000000, -1.000000000000000000 ) ) ;
#257176 = ORIENTED_EDGE ( 'NONE', *, *, #33450, .F. ) ;
#257178 = EDGE_LOOP ( 'NONE', ( #239152, #23472, #250031, #99682 ) ) ;
#257177 = DIRECTION ( 'NONE',  ( 0.000000000000000000, -1.000000000000000000, -7.272083257015735086E-15 ) ) ;
#257179 = FACE_OUTER_BOUND ( 'NONE', #85591, .T. ) ;
#257180 = VECTOR ( 'NONE', #40469, 1000.000000000000000 ) ;
#257181 = EDGE_CURVE ( 'NONE', #170251, #60665, #55563, .T. ) ;
#257182 = CARTESIAN_POINT ( 'NONE',  ( -16.87683809663752399, 9.850000000011123191, -80.40236401819653622 ) ) ;
#257183 = VECTOR ( 'NONE', #50086, 1000.000000000000000 ) ;
#257184 = ORIENTED_EDGE ( 'NONE', *, *, #207320, .F. ) ;
#257185 = CIRCLE ( 'NONE', #153216, 0.09999999999998898659 ) ;
#257186 = ADVANCED_FACE ( 'NONE', ( #200251 ), #161131, .F. ) ;
#257187 = AXIS2_PLACEMENT_3D ( 'NONE', #191202, #92062, #18941 ) ;
#257188 = DIRECTION ( 'NONE',  ( -1.000000000000000000, 0.000000000000000000, 0.000000000000000000 ) ) ;
#257190 = EDGE_LOOP ( 'NONE', ( #230264, #79666, #226278, #218184 ) ) ;
#257189 = AXIS2_PLACEMENT_3D ( 'NONE', #83830, #180417, #5596 ) ;
#257191 = CARTESIAN_POINT ( 'NONE',  ( 18.49999999999999645, 5.699452464332751767, -54.45772604343021328 ) ) ;
#257192 = EDGE_CURVE ( 'NONE', #256420, #13934, #151766, .T. ) ;
#257193 = CIRCLE ( 'NONE', #90245, 11.80000000000000426 ) ;
#257194 = DIRECTION ( 'NONE',  ( 1.000000000000000000, 6.834672213024256725E-16, -4.941700349840507066E-16 ) ) ;
#257195 = CARTESIAN_POINT ( 'NONE',  ( 12.84435279558019438, 66.58929125296442919, -51.45389907868029411 ) ) ;
#257196 = DIRECTION ( 'NONE',  ( 1.000000000000000000, 0.000000000000000000, 0.000000000000000000 ) ) ;
#257197 = EDGE_CURVE ( 'NONE', #117705, #137344, #181977, .T. ) ;
#257198 = ADVANCED_FACE ( 'NONE', ( #4598, #123287 ), #239380, .F. ) ;
#257199 = VECTOR ( 'NONE', #76623, 1000.000000000000000 ) ;
#257200 = TOROIDAL_SURFACE ( 'NONE', #52850, 11.70000000000000107, 0.1000000000000000056 ) ;
#257201 = EDGE_LOOP ( 'NONE', ( #147850, #178308, #36296, #63122 ) ) ;
#257202 = CARTESIAN_POINT ( 'NONE',  ( 21.05000000000000071, 67.12872031401595052, -60.96447848938343128 ) ) ;
#257203 = CIRCLE ( 'NONE', #119927, 0.5000000000000004441 ) ;
#257204 = AXIS2_PLACEMENT_3D ( 'NONE', #62981, #163378, #107242 ) ;
#257205 = ORIENTED_EDGE ( 'NONE', *, *, #99747, .F. ) ;
#257206 = TOROIDAL_SURFACE ( 'NONE', #144820, 11.65000000000000036, 0.1000000000000000056 ) ;
#257207 = CARTESIAN_POINT ( 'NONE',  ( -22.50000000000000000, 76.00000000001195133, -103.0231074845243171 ) ) ;
#257208 = CARTESIAN_POINT ( 'NONE',  ( -23.25000000000000000, 76.00000000001126921, -203.5231074845248997 ) ) ;
#257211 = ORIENTED_EDGE ( 'NONE', *, *, #73878, .F. ) ;
#257210 = DIRECTION ( 'NONE',  ( 0.000000000000000000, -1.000000000000000000, 0.000000000000000000 ) ) ;
#257209 =( BOUNDED_SURFACE ( )  B_SPLINE_SURFACE ( 3, 2, ( 
 ( #11409, #53082, #49233 ),
 ( #8833, #32271, #150907 ),
 ( #73970, #33574, #251275 ),
 ( #92204, #212180, #173089 ) ),
 .UNSPECIFIED., .F., .F., .F. ) 
 B_SPLINE_SURFACE_WITH_KNOTS ( ( 4, 4 ),
 ( 3, 3 ),
 ( 0.04058434257139475337, 0.04256401539001600232 ),
 ( 0.000000000000000000, 1.000000000000000000 ),
 .UNSPECIFIED. ) 
 GEOMETRIC_REPRESENTATION_ITEM ( )  RATIONAL_B_SPLINE_SURFACE ( (
 ( 1.000000000000000000, 0.7103081912007809251, 1.000000000000000000),
 ( 1.000000000000000000, 0.7104998333556865608, 1.000000000000000000),
 ( 1.000000000000000000, 0.7107238315753950930, 1.000000000000000000),
 ( 1.000000000000000000, 0.7110073749539780330, 1.000000000000000000) ) ) 
 REPRESENTATION_ITEM ( '' )  SURFACE ( )  );
#257212 = EDGE_CURVE ( 'NONE', #90455, #249596, #144985, .T. ) ;
#257214 = CIRCLE ( 'NONE', #82450, 0.2000000000000048683 ) ;
#257213 = DIRECTION ( 'NONE',  ( 0.000000000000000000, 0.000000000000000000, -1.000000000000000000 ) ) ;
#257215 = CARTESIAN_POINT ( 'NONE',  ( 22.48970261584622321, 64.35000000001195986, -103.0784769727417967 ) ) ;
#257216 = CARTESIAN_POINT ( 'NONE',  ( -20.85000000000000142, 64.25000000001148237, -42.80697314750250371 ) ) ;
#257217 = CARTESIAN_POINT ( 'NONE',  ( -16.85312841634287651, 9.913606177331358182, -79.89717313329258275 ) ) ;
#257218 = ADVANCED_FACE ( 'NONE', ( #21623 ), #39922, .T. ) ;
#257219 = DIRECTION ( 'NONE',  ( 0.000000000000000000, 0.1335171055202864221, 0.9910465087640865089 ) ) ;
#257220 = CARTESIAN_POINT ( 'NONE',  ( 20.95512820512820440, 8.876151316299271343, -45.65000000000000568 ) ) ;
#257222 = ORIENTED_EDGE ( 'NONE', *, *, #36768, .T. ) ;
#257221 = FACE_OUTER_BOUND ( 'NONE', #79365, .T. ) ;
#257223 = VECTOR ( 'NONE', #232085, 1000.000000000000000 ) ;
#257224 = COLOUR_RGB ( '', 0.31764706, 0.68627451, 0.89019608) ;
#257225 = AXIS2_PLACEMENT_3D ( 'NONE', #140062, #95801, #115378 ) ;
#257226 = LINE ( 'NONE', #17390, #72478 ) ;
#257227 = ORIENTED_EDGE ( 'NONE', *, *, #125960, .T. ) ;
#257228 = VERTEX_POINT ( 'NONE', #38615 ) ;
#257229 = DIRECTION ( 'NONE',  ( 0.000000000000000000, -1.000000000000000000, -0.000000000000000000 ) ) ;
#257230 = CARTESIAN_POINT ( 'NONE',  ( -1.820710678118657944, -9.929289321881341834, -24.75000000000000000 ) ) ;
#257231 = ORIENTED_EDGE ( 'NONE', *, *, #256079, .T. ) ;
#257232 = DIRECTION ( 'NONE',  ( 0.000000000000000000, 0.2128009952263485993, -0.9770955615653341697 ) ) ;
#257233 = CONICAL_SURFACE ( 'NONE', #7302, 4.299999999999956302, 0.7853981633974466137 ) ;
#257234 = AXIS2_PLACEMENT_3D ( 'NONE', #6273, #229201, #187519 ) ;
#257235 = CARTESIAN_POINT ( 'NONE',  ( 22.47071067811865319, 0.09909245470260570621, 7.720074744498046648 ) ) ;
#257237 = ORIENTED_EDGE ( 'NONE', *, *, #70675, .F. ) ;
#257236 = AXIS2_PLACEMENT_3D ( 'NONE', #92965, #74737, #249493 ) ;
#257239 = ADVANCED_FACE ( 'NONE', ( #43745 ), #202812, .T. ) ;
#257238 = CARTESIAN_POINT ( 'NONE',  ( -23.15000000000000213, 74.00000000001199396, -116.2477294072864140 ) ) ;
#257241 = CARTESIAN_POINT ( 'NONE',  ( 21.05000000000000071, 76.00000000001267608, -203.5231074845243597 ) ) ;
#257240 = AXIS2_PLACEMENT_3D ( 'NONE', #46018, #23926, #227226 ) ;
#257242 = VERTEX_POINT ( 'NONE', #140251 ) ;
#257243 = DIRECTION ( 'NONE',  ( 0.000000000000000000, 0.1350103645451876666, -0.9908441862701600211 ) ) ;
#257244 = EDGE_LOOP ( 'NONE', ( #64280, #148609, #221046 ) ) ;
#257245 = DIRECTION ( 'NONE',  ( 0.000000000000000000, -7.086529944415894657E-15, 1.000000000000000000 ) ) ;
#257247 = ORIENTED_EDGE ( 'NONE', *, *, #90753, .T. ) ;
#257246 = CARTESIAN_POINT ( 'NONE',  ( -23.25000000000000000, 77.83585931145570669, -125.0186683157258329 ) ) ;
#257248 = CIRCLE ( 'NONE', #32494, 0.1000000000000055844 ) ;
#257249 = DIRECTION ( 'NONE',  ( 0.000000000000000000, -0.8814952561688430555, 0.4721928772777346239 ) ) ;
#257250 = ORIENTED_EDGE ( 'NONE', *, *, #56475, .F. ) ;
#257251 = DIRECTION ( 'NONE',  ( -0.000000000000000000, 0.8660254037844383745, -0.5000000000000003331 ) ) ;
#257252 = AXIS2_PLACEMENT_3D ( 'NONE', #38734, #96110, #214789 ) ;
#257253 = AXIS2_PLACEMENT_3D ( 'NONE', #90345, #168667, #13403 ) ;
#257254 = ORIENTED_EDGE ( 'NONE', *, *, #192639, .T. ) ;
#257256 = ORIENTED_EDGE ( 'NONE', *, *, #46866, .T. ) ;
#257255 = EDGE_LOOP ( 'NONE', ( #100904, #80632, #56024 ) ) ;
#257257 = CARTESIAN_POINT ( 'NONE',  ( 18.41789779300686192, 85.50000000001209344, -129.4910378181635622 ) ) ;
#257258 = VECTOR ( 'NONE', #167484, 1000.000000000000000 ) ;
#257259 = ORIENTED_EDGE ( 'NONE', *, *, #94608, .F. ) ;
#257260 = ADVANCED_FACE ( 'NONE', ( #197669 ), #147460, .T. ) ;
#257261 = DIRECTION ( 'NONE',  ( 1.000000000000000000, 0.000000000000000000, -0.000000000000000000 ) ) ;
#257262 = ORIENTED_EDGE ( 'NONE', *, *, #117445, .F. ) ;
#257263 = CIRCLE ( 'NONE', #157398, 12.87499999999999467 ) ;
#257264 = ORIENTED_EDGE ( 'NONE', *, *, #256244, .F. ) ;
#257265 = PLANE ( 'NONE',  #128693 ) ;
#257266 = CARTESIAN_POINT ( 'NONE',  ( -18.40000000000000213, 70.35000000001222986, -145.7731074845243882 ) ) ;
#257268 = VERTEX_POINT ( 'NONE', #122002 ) ;
#257267 = DIRECTION ( 'NONE',  ( -1.000000000000000000, 0.000000000000000000, 0.000000000000000000 ) ) ;
#257269 = FACE_OUTER_BOUND ( 'NONE', #114676, .T. ) ;
#257270 = ORIENTED_EDGE ( 'NONE', *, *, #86762, .T. ) ;
#257271 = DIRECTION ( 'NONE',  ( 0.000000000000000000, 0.2617529984163859957, 0.9651348961777475033 ) ) ;
#257272 = DIRECTION ( 'NONE',  ( 0.000000000000000000, 0.2617529984165152257, 0.9651348961777124202 ) ) ;
#257273 = DIRECTION ( 'NONE',  ( 0.000000000000000000, 0.000000000000000000, -1.000000000000000000 ) ) ;
#257274 = VECTOR ( 'NONE', #239920, 1000.000000000000227 ) ;
#257275 = EDGE_LOOP ( 'NONE', ( #8386, #125288, #208022, #169387, #175284, #78412 ) ) ;
#257276 = CARTESIAN_POINT ( 'NONE',  ( -20.00857864376270001, 61.43991280424057777, -221.4883200034892923 ) ) ;
#257277 = DIRECTION ( 'NONE',  ( 1.000000000000000000, 0.000000000000000000, 0.000000000000000000 ) ) ;
#257278 = ORIENTED_EDGE ( 'NONE', *, *, #114913, .T. ) ;
#257279 = DIRECTION ( 'NONE',  ( 0.000000000000000000, 1.000000000000000000, 2.891205793294679805E-16 ) ) ;
#257280 = ORIENTED_EDGE ( 'NONE', *, *, #127451, .F. ) ;
#257282 = VERTEX_POINT ( 'NONE', #20353 ) ;
#257281 = AXIS2_PLACEMENT_3D ( 'NONE', #168135, #3877, #65127 ) ;
#257283 = DIRECTION ( 'NONE',  ( -1.000000000000000000, 0.000000000000000000, 0.000000000000000000 ) ) ;
#257284 = VERTEX_POINT ( 'NONE', #19040 ) ;
#257285 = EDGE_LOOP ( 'NONE', ( #36828, #115125, #31304, #12593 ) ) ;
#257286 = CARTESIAN_POINT ( 'NONE',  ( 18.59999999999999787, 77.83534155023670564, -158.4679561919613491 ) ) ;
#257287 = CARTESIAN_POINT ( 'NONE',  ( -18.34374000495059676, 11.47316190337362940, -158.2500000000000284 ) ) ;
#257288 = ORIENTED_EDGE ( 'NONE', *, *, #2174, .T. ) ;
#257289 = ORIENTED_EDGE ( 'NONE', *, *, #104343, .F. ) ;
#257290 = FACE_OUTER_BOUND ( 'NONE', #40558, .T. ) ;
#257291 = CARTESIAN_POINT ( 'NONE',  ( 22.39999999999999503, 76.10085836911147794, -215.2726746080137445 ) ) ;
#257292 = ORIENTED_EDGE ( 'NONE', *, *, #12563, .F. ) ;
#257293 = EDGE_CURVE ( 'NONE', #52704, #109, #214101, .T. ) ;
#257294 = ORIENTED_EDGE ( 'NONE', *, *, #172491, .F. ) ;
#257295 = AXIS2_PLACEMENT_3D ( 'NONE', #205521, #26929, #106407 ) ;
#257296 = VECTOR ( 'NONE', #195265, 1000.000000000000000 ) ;
#257297 = VECTOR ( 'NONE', #190125, 1000.000000000000114 ) ;
#257298 = EDGE_LOOP ( 'NONE', ( #81961, #54625, #226857, #20004 ) ) ;
#257299 =( BOUNDED_SURFACE ( )  B_SPLINE_SURFACE ( 3, 2, ( 
 ( #232243, #75725, #130542 ),
 ( #213939, #172295, #54845 ),
 ( #52276, #35343, #91432 ),
 ( #11914, #53586, #13182 ) ),
 .UNSPECIFIED., .F., .F., .F. ) 
 B_SPLINE_SURFACE_WITH_KNOTS ( ( 4, 4 ),
 ( 3, 3 ),
 ( 0.0008258556059633777964, 0.0009616864997632713560 ),
 ( 0.000000000000000000, 1.000000000000000000 ),
 .UNSPECIFIED. ) 
 GEOMETRIC_REPRESENTATION_ITEM ( )  RATIONAL_B_SPLINE_SURFACE ( (
 ( 1.000000000000000000, 0.9152888060719425178, 1.000000000000000000),
 ( 1.000000000000000000, 0.9327727094137988617, 1.000000000000000000),
 ( 1.000000000000000000, 0.9369023509258489479, 1.000000000000000000),
 ( 1.000000000000000000, 0.9246339933864502481, 1.000000000000000000) ) ) 
 REPRESENTATION_ITEM ( '' )  SURFACE ( )  );
#257300 = ADVANCED_FACE ( 'NONE', ( #78982 ), #72845, .T. ) ;
#257301 = CARTESIAN_POINT ( 'NONE',  ( 21.05000000000000071, 69.45934304831145312, -203.5231074845243882 ) ) ;
#257302 = EDGE_CURVE ( 'NONE', #113635, #181798, #210199, .T. ) ;
#257303 = CARTESIAN_POINT ( 'NONE',  ( -20.85000000000000142, 11.65000000001115232, -93.71613433702194129 ) ) ;
#257304 = CARTESIAN_POINT ( 'NONE',  ( -23.25000000000000000, 11.75000000001115552, -179.6499999999999773 ) ) ;
#257305 = CARTESIAN_POINT ( 'NONE',  ( 22.39999999999999503, 1.666707276765596379, -230.6933463038365630 ) ) ;
#257306 = DIRECTION ( 'NONE',  ( 1.000000000000000000, 0.000000000000000000, 0.000000000000000000 ) ) ;
#257307 = CARTESIAN_POINT ( 'NONE',  ( -21.55000000000000071, 68.65000000001187175, -90.77310748452435973 ) ) ;
#257310 = LINE ( 'NONE', #34497, #3734 ) ;
#257309 = CIRCLE ( 'NONE', #3466, 0.1000000000000055844 ) ;
#257308 = CARTESIAN_POINT ( 'NONE',  ( -16.86757978335471719, 9.965650379034281414, -12.59800465316751250 ) ) ;
#257311 = CARTESIAN_POINT ( 'NONE',  ( -20.85000000000000142, 65.66751761918618513, -30.42826094061123499 ) ) ;
#257312 = CARTESIAN_POINT ( 'NONE',  ( -16.92280123533723213, 23.15492389264284867, -231.0298005607855032 ) ) ;
#257313 = AXIS2_PLACEMENT_3D ( 'NONE', #130846, #85267, #164849 ) ;
#257314 = ADVANCED_FACE ( 'NONE', ( #179419, #731, #80265 ), #159859, .T. ) ;
#257315 = DIRECTION ( 'NONE',  ( 0.000000000000000000, 0.000000000000000000, 1.000000000000000000 ) ) ;
#257316 = CARTESIAN_POINT ( 'NONE',  ( 18.57071067811864040, 51.98142472962693716, -231.5327994178193762 ) ) ;
#257317 = ORIENTED_EDGE ( 'NONE', *, *, #8142, .T. ) ;
#257318 = CIRCLE ( 'NONE', #203211, 0.09999999999999767408 ) ;
#257320 = EDGE_LOOP ( 'NONE', ( #156109, #176423, #172613, #185829 ) ) ;
#257319 = CARTESIAN_POINT ( 'NONE',  ( -18.69999999999999929, -1.885425182446132997, -11.49641995933507843 ) ) ;
#257321 = EDGE_CURVE ( 'NONE', #201551, #40973, #5882, .T. ) ;
#257322 = CARTESIAN_POINT ( 'NONE',  ( -15.55912972643740488, 64.49398937010923305, -213.5095531679024532 ) ) ;
#257323 = FACE_OUTER_BOUND ( 'NONE', #25795, .T. ) ;
#257324 = ORIENTED_EDGE ( 'NONE', *, *, #92959, .F. ) ;
#257325 = DIRECTION ( 'NONE',  ( 1.000000000000000000, 0.000000000000000000, 0.000000000000000000 ) ) ;
#257326 = AXIS2_PLACEMENT_3D ( 'NONE', #15313, #94821, #174420 ) ;
#257327 = CARTESIAN_POINT ( 'NONE',  ( -16.93388492042257809, 9.988541822527059466, -54.40054512318618407 ) ) ;
#257328 = VERTEX_POINT ( 'NONE', #46295 ) ;
#257329 = CIRCLE ( 'NONE', #86674, 0.09999999999999939493 ) ;
#257330 = VECTOR ( 'NONE', #65073, 999.9999999999998863 ) ;
#257331 = CARTESIAN_POINT ( 'NONE',  ( -18.50000000000000000, 85.50000000001277556, -215.2731074845243029 ) ) ;
#257332 = CARTESIAN_POINT ( 'NONE',  ( -20.94999999999999929, 4.252251777740764460, -211.8999245327126744 ) ) ;
#257333 = DIRECTION ( 'NONE',  ( 0.000000000000000000, 0.000000000000000000, -1.000000000000000000 ) ) ;
#257334 = PLANE ( 'NONE',  #61930 ) ;
#257336 = ORIENTED_EDGE ( 'NONE', *, *, #206507, .F. ) ;
#257335 = CARTESIAN_POINT ( 'NONE',  ( 21.05000000000000071, 76.00000000001270450, -207.8231074845243711 ) ) ;
#257337 = AXIS2_PLACEMENT_3D ( 'NONE', #64128, #127955, #165817 ) ;
#257339 = ORIENTED_EDGE ( 'NONE', *, *, #150518, .T. ) ;
#257338 = CARTESIAN_POINT ( 'NONE',  ( -18.48408745364680428, 85.66432225867497152, -96.34002895119586185 ) ) ;
#257340 = CARTESIAN_POINT ( 'NONE',  ( 23.25000000000000355, -22.45632476061176774, -174.2938984477315785 ) ) ;
#257341 = CARTESIAN_POINT ( 'NONE',  ( 18.39999999999999503, 64.25000000001256240, -182.6731074845244507 ) ) ;
#257342 = CYLINDRICAL_SURFACE ( 'NONE', #52683, 0.09999999999999976963 ) ;
#257343 = LINE ( 'NONE', #81301, #119407 ) ;
#257344 = DIRECTION ( 'NONE',  ( 0.000000000000000000, 0.000000000000000000, 1.000000000000000000 ) ) ;
#257345 = CARTESIAN_POINT ( 'NONE',  ( -23.25000000000000355, 11.75000000001113953, -91.25000000000005684 ) ) ;
#257346 = DIRECTION ( 'NONE',  ( 0.000000000000000000, -0.6728971962617102953, 0.7397360091702507301 ) ) ;
#257347 = CARTESIAN_POINT ( 'NONE',  ( -18.40000000000000213, 85.50000000001242029, -163.1009576351939074 ) ) ;
#257348 = AXIS2_PLACEMENT_3D ( 'NONE', #85030, #125480, #108482 ) ;
#257349 = CIRCLE ( 'NONE', #32609, 0.5000000000000014433 ) ;
#257350 = DIRECTION ( 'NONE',  ( 0.000000000000000000, -1.000000000000000000, -6.982962677686265922E-15 ) ) ;
#257351 = VECTOR ( 'NONE', #206582, 1000.000000000000000 ) ;
#257352 = EDGE_LOOP ( 'NONE', ( #17521, #32258, #139615, #241518 ) ) ;
#257353 = EDGE_CURVE ( 'NONE', #34960, #172291, #97725, .T. ) ;
#257354 = CARTESIAN_POINT ( 'NONE',  ( -21.52071067811865746, 7.779289321881349473, -21.15000000000000213 ) ) ;
#257355 = AXIS2_PLACEMENT_3D ( 'NONE', #105770, #203613, #4125 ) ;
#257356 = ORIENTED_EDGE ( 'NONE', *, *, #120089, .T. ) ;
#257357 = EDGE_LOOP ( 'NONE', ( #74013, #209766, #239934, #34126 ) ) ;
#257358 = CARTESIAN_POINT ( 'NONE',  ( 23.14999999999999147, 71.23658437219593509, -236.9414014499068912 ) ) ;
#257359 = DIRECTION ( 'NONE',  ( 0.000000000000000000, 0.000000000000000000, -1.000000000000000000 ) ) ;
#257360 = ORIENTED_EDGE ( 'NONE', *, *, #51566, .F. ) ;
#257361 = ADVANCED_FACE ( 'NONE', ( #145401 ), #26778, .F. ) ;
#257362 = VERTEX_POINT ( 'NONE', #45028 ) ;
#257363 = EDGE_CURVE ( 'NONE', #155936, #78065, #85395, .T. ) ;
#257364 = EDGE_CURVE ( 'NONE', #195237, #203031, #151945, .T. ) ;
#257365 = ORIENTED_EDGE ( 'NONE', *, *, #229369, .F. ) ;
#257366 = AXIS2_PLACEMENT_3D ( 'NONE', #166961, #226890, #7867 ) ;
#257367 = ORIENTED_EDGE ( 'NONE', *, *, #165695, .F. ) ;
#257369 = CARTESIAN_POINT ( 'NONE',  ( -16.89268316805465986, 66.04827818677036078, -182.6673550059788909 ) ) ;
#257368 = AXIS2_PLACEMENT_3D ( 'NONE', #134546, #135835, #2746 ) ;
#257370 = DIRECTION ( 'NONE',  ( 0.000000000000000000, 0.000000000000000000, 1.000000000000000000 ) ) ;
#257371 = VECTOR ( 'NONE', #192200, 1000.000000000000114 ) ;
#257372 = CIRCLE ( 'NONE', #40990, 0.1000000000000028644 ) ;
#257373 = DIRECTION ( 'NONE',  ( -0.000000000000000000, -6.982962677686266711E-15, 1.000000000000000000 ) ) ;
#257374 = CARTESIAN_POINT ( 'NONE',  ( 23.15000000000000213, -11.48912529306489994, -64.00000000000000000 ) ) ;
#257375 = AXIS2_PLACEMENT_3D ( 'NONE', #175846, #14212, #72910 ) ;
#257376 = EDGE_CURVE ( 'NONE', #186482, #64319, #147984, .T. ) ;
#257377 = CARTESIAN_POINT ( 'NONE',  ( 20.94999999999999929, 49.57218508014540959, -254.1759139559835035 ) ) ;
#257378 = CARTESIAN_POINT ( 'NONE',  ( 21.05000000000000071, 76.08559286337410299, -142.9367702193934804 ) ) ;
#257380 = ORIENTED_EDGE ( 'NONE', *, *, #223329, .F. ) ;
#257379 = CARTESIAN_POINT ( 'NONE',  ( -21.05000000000000071, 76.00000000001190870, -103.0231074845243029 ) ) ;
#257382 = CARTESIAN_POINT ( 'NONE',  ( -21.05000000000000071, 1.115600667400684642E-11, -134.0000000000000000 ) ) ;
#257381 = LINE ( 'NONE', #35852, #237833 ) ;
#257383 = ADVANCED_FACE ( 'NONE', ( #223643 ), #124578, .F. ) ;
#257384 = VECTOR ( 'NONE', #247080, 1000.000000000000000 ) ;
#257385 = CARTESIAN_POINT ( 'NONE',  ( -20.94999999999994600, 66.15000000001120384, -4.623107484524796362 ) ) ;
#257386 = ORIENTED_EDGE ( 'NONE', *, *, #247209, .F. ) ;
#257387 = CARTESIAN_POINT ( 'NONE',  ( -16.94333152882356686, 63.05779874932826345, -213.0764958470617785 ) ) ;
#257389 = ADVANCED_FACE ( 'NONE', ( #209232 ), #163702, .T. ) ;
#257388 = CARTESIAN_POINT ( 'NONE',  ( 20.90000000000000213, 7.800000000000000711, 1.212568896937007867 ) ) ;
#257390 = ORIENTED_EDGE ( 'NONE', *, *, #100027, .F. ) ;
#257392 = CARTESIAN_POINT ( 'NONE',  ( -18.59999999999999787, 77.16270174995010223, -128.4231074845242802 ) ) ;
#257391 = DIRECTION ( 'NONE',  ( 0.000000000000000000, -1.000000000000000000, -6.982962677686266711E-15 ) ) ;
#257393 = FACE_OUTER_BOUND ( 'NONE', #140375, .T. ) ;
#257394 = LINE ( 'NONE', #115373, #251068 ) ;
#257395 = AXIS2_PLACEMENT_3D ( 'NONE', #12948, #173332, #237104 ) ;
#257397 = ORIENTED_EDGE ( 'NONE', *, *, #1373, .T. ) ;
#257396 = VECTOR ( 'NONE', #198764, 1000.000000000000114 ) ;
#257398 = ADVANCED_FACE ( 'NONE', ( #86693 ), #39532, .F. ) ;
#257399 = FACE_OUTER_BOUND ( 'NONE', #81183, .T. ) ;
#257400 = EDGE_CURVE ( 'NONE', #95061, #212130, #168541, .T. ) ;
#257401 = PLANE ( 'NONE',  #44971 ) ;
#257402 = CARTESIAN_POINT ( 'NONE',  ( 23.04999999999999716, 8.822561741677553471, -42.75000000000000000 ) ) ;
#257404 = EDGE_CURVE ( 'NONE', #181531, #182718, #193451, .T. ) ;
#257403 = DIRECTION ( 'NONE',  ( -1.000000000000000000, 0.000000000000000000, 0.000000000000000000 ) ) ;
#257405 = ORIENTED_EDGE ( 'NONE', *, *, #19582, .F. ) ;
#257406 = EDGE_CURVE ( 'NONE', #143756, #53148, #226196, .T. ) ;
#257407 = CARTESIAN_POINT ( 'NONE',  ( 20.95512820512820795, 8.876151316299273120, -179.7001728591287133 ) ) ;
#257408 = CIRCLE ( 'NONE', #165918, 0.8750000000000007772 ) ;
#257409 = VECTOR ( 'NONE', #7798, 1000.000000000000114 ) ;
#257410 = CYLINDRICAL_SURFACE ( 'NONE', #60877, 7.899999999999990585 ) ;
#257411 = CARTESIAN_POINT ( 'NONE',  ( -22.39999999999999858, 7.612336166715881092, -199.3421143478784359 ) ) ;
#257412 = DIRECTION ( 'NONE',  ( 0.000000000000000000, 0.000000000000000000, 1.000000000000000000 ) ) ;
#257413 = CARTESIAN_POINT ( 'NONE',  ( -18.42554971533678199, 85.49715966945009882, -162.9832805709756371 ) ) ;
#257414 = AXIS2_PLACEMENT_3D ( 'NONE', #222060, #205079, #128142 ) ;
#257416 = ORIENTED_EDGE ( 'NONE', *, *, #204189, .T. ) ;
#257415 = DIRECTION ( 'NONE',  ( 0.000000000000000000, -0.9126074666063660468, -0.4088369013363524762 ) ) ;
#257417 = CARTESIAN_POINT ( 'NONE',  ( -20.54999999999999716, -11.74999999998884448, -155.1500000000000057 ) ) ;
#257419 = EDGE_CURVE ( 'NONE', #134584, #77128, #184527, .T. ) ;
#257418 = CARTESIAN_POINT ( 'NONE',  ( -16.83233564386414116, 66.06977820342717678, -90.24762814800000399 ) ) ;
#257420 = DIRECTION ( 'NONE',  ( -1.000000000000000000, -0.000000000000000000, -0.000000000000000000 ) ) ;
#257421 = EDGE_CURVE ( 'NONE', #56541, #44902, #51939, .T. ) ;
#257422 = DIRECTION ( 'NONE',  ( 0.000000000000000000, 0.000000000000000000, 1.000000000000000000 ) ) ;
#257424 = ORIENTED_EDGE ( 'NONE', *, *, #102978, .T. ) ;
#257423 = CARTESIAN_POINT ( 'NONE',  ( 20.94999999999999929, 85.40000000001178648, -79.41707660717668205 ) ) ;
#257425 = DIRECTION ( 'NONE',  ( 0.000000000000000000, 0.000000000000000000, -1.000000000000000000 ) ) ;
#257426 = AXIS2_PLACEMENT_3D ( 'NONE', #91591, #72037, #151592 ) ;
#257427 = DIRECTION ( 'NONE',  ( 0.000000000000000000, 0.000000000000000000, -1.000000000000000000 ) ) ;
#257428 = CARTESIAN_POINT ( 'NONE',  ( 20.89192007715128341, 67.49241595948059569, -195.4314365843280541 ) ) ;
#257429 = VERTEX_POINT ( 'NONE', #68454 ) ;
#257430 = CARTESIAN_POINT ( 'NONE',  ( -23.15000000000000213, 71.65000000001180069, -81.67310748452435121 ) ) ;
#257431 = CARTESIAN_POINT ( 'NONE',  ( 20.73486653747088226, 68.75000000001155342, -56.87310748452436826 ) ) ;
#257432 = CARTESIAN_POINT ( 'NONE',  ( 20.94999999999999929, -11.39257802169451317, -164.4260504201680817 ) ) ;
#257433 = CIRCLE ( 'NONE', #253397, 0.1000000000000002554 ) ;
#257434 = TOROIDAL_SURFACE ( 'NONE', #228287, 11.65000000000000036, 0.1000000000000000056 ) ;
#257435 = CARTESIAN_POINT ( 'NONE',  ( -18.39999999999999858, 87.08727414655710675, -199.6327537731849873 ) ) ;
#257436 = EDGE_CURVE ( 'NONE', #127785, #187652, #56035, .T. ) ;
#257437 = VECTOR ( 'NONE', #181943, 1000.000000000000000 ) ;
#257438 = CARTESIAN_POINT ( 'NONE',  ( -18.51991288638553002, 78.16601445863898334, -231.4194093194572588 ) ) ;
#257439 = VECTOR ( 'NONE', #66207, 1000.000000000000000 ) ;
#257440 = DIRECTION ( 'NONE',  ( 0.000000000000000000, -0.7203564749500950271, 0.6936040289657154911 ) ) ;
#257441 = ORIENTED_EDGE ( 'NONE', *, *, #113563, .F. ) ;
#257442 = ORIENTED_EDGE ( 'NONE', *, *, #222094, .T. ) ;
#257443 = LINE ( 'NONE', #140105, #5887 ) ;
#257444 = FACE_OUTER_BOUND ( 'NONE', #14900, .T. ) ;
#257445 = LINE ( 'NONE', #215793, #66479 ) ;
#257446 = FACE_OUTER_BOUND ( 'NONE', #138986, .T. ) ;
#257447 = ORIENTED_EDGE ( 'NONE', *, *, #82679, .T. ) ;
#257448 = CARTESIAN_POINT ( 'NONE',  ( 20.95520789717937404, 10.57693059939611224, -175.0802329738748142 ) ) ;
#257449 = CIRCLE ( 'NONE', #186616, 0.09999999999999939493 ) ;
#257450 = EDGE_CURVE ( 'NONE', #113714, #225825, #188387, .T. ) ;
#257451 = CARTESIAN_POINT ( 'NONE',  ( 20.12518398540832365, 11.44831387781778353, -206.6908002495722769 ) ) ;
#257452 = CARTESIAN_POINT ( 'NONE',  ( 21.05000000000000071, 85.00000000001149658, -45.91707660717670336 ) ) ;
#257453 = EDGE_CURVE ( 'NONE', #228499, #113219, #168874, .T. ) ;
#257454 = FACE_OUTER_BOUND ( 'NONE', #82282, .T. ) ;
#257455 = VERTEX_POINT ( 'NONE', #159235 ) ;
#257456 = LINE ( 'NONE', #118005, #15333 ) ;
#257457 = EDGE_CURVE ( 'NONE', #146336, #28760, #171232, .T. ) ;
#257458 = VERTEX_POINT ( 'NONE', #56241 ) ;
#257459 = LINE ( 'NONE', #161001, #165405 ) ;
#257460 = EDGE_CURVE ( 'NONE', #257702, #16882, #15884, .T. ) ;
#257461 = ORIENTED_EDGE ( 'NONE', *, *, #3637, .T. ) ;
#257462 = CARTESIAN_POINT ( 'NONE',  ( -21.05000000000000071, -0.08579911626297659355, -27.08602111851157090 ) ) ;
#257463 = CARTESIAN_POINT ( 'NONE',  ( 21.05000000000000071, 71.00000000001180922, -81.92837350343744163 ) ) ;
#257464 = CARTESIAN_POINT ( 'NONE',  ( -20.54999999999999716, 2.000000000011154189, -180.7246219227620543 ) ) ;
#257465 = ORIENTED_EDGE ( 'NONE', *, *, #183512, .F. ) ;
#257466 = DIRECTION ( 'NONE',  ( 0.000000000000000000, 0.000000000000000000, 1.000000000000000000 ) ) ;
#257468 = EDGE_CURVE ( 'NONE', #131237, #83073, #1871, .T. ) ;
#257467 = CARTESIAN_POINT ( 'NONE',  ( -23.15000000000000213, 11.75000000001115552, -54.84999999999999432 ) ) ;
#257469 = ORIENTED_EDGE ( 'NONE', *, *, #165116, .T. ) ;
#257470 = DIRECTION ( 'NONE',  ( 0.000000000000000000, 0.000000000000000000, -1.000000000000000000 ) ) ;
#257472 = ORIENTED_EDGE ( 'NONE', *, *, #170993, .F. ) ;
#257471 = DIRECTION ( 'NONE',  ( -0.000000000000000000, 1.000000000000000000, -1.224646799147352961E-16 ) ) ;
#257473 = DIRECTION ( 'NONE',  ( -1.000000000000000000, 0.000000000000000000, 0.000000000000000000 ) ) ;
#257474 = FACE_OUTER_BOUND ( 'NONE', #88624, .T. ) ;
#257475 = AXIS2_PLACEMENT_3D ( 'NONE', #23742, #241477, #4136 ) ;
#257476 = AXIS2_PLACEMENT_3D ( 'NONE', #48887, #9759, #167582 ) ;
#257477 = VECTOR ( 'NONE', #57964, 1000.000000000000000 ) ;
#257478 = ADVANCED_FACE ( 'NONE', ( #155400 ), #195800, .T. ) ;
#257479 = EDGE_CURVE ( 'NONE', #257956, #134738, #206901, .T. ) ;
#257480 = VERTEX_POINT ( 'NONE', #170159 ) ;
#257481 = CARTESIAN_POINT ( 'NONE',  ( -18.40000000000000213, 64.25000000001224976, -149.1731074845244507 ) ) ;
#257482 = CARTESIAN_POINT ( 'NONE',  ( -16.77683809663752257, 66.05416425680770942, -90.35915846542016538 ) ) ;
#257483 = DIRECTION ( 'NONE',  ( 4.239556034732056743E-17, 0.1298341882519953860, 0.9915357197604862671 ) ) ;
#257484 = VERTEX_POINT ( 'NONE', #199648 ) ;
#257485 = CARTESIAN_POINT ( 'NONE',  ( 21.08376601933332495, 6.341947271286813681, -133.9362239890700153 ) ) ;
#257486 = EDGE_CURVE ( 'NONE', #200735, #75516, #18416, .T. ) ;
#257487 = CARTESIAN_POINT ( 'NONE',  ( 15.73863059295127798, 48.33137198101099585, -234.0751437313343786 ) ) ;
#257488 = EDGE_LOOP ( 'NONE', ( #160414, #128982, #235964, #120250 ) ) ;
#257489 = CIRCLE ( 'NONE', #232454, 0.1000000000000021844 ) ;
#257490 = AXIS2_PLACEMENT_3D ( 'NONE', #1599, #141133, #2876 ) ;
#257491 = ORIENTED_EDGE ( 'NONE', *, *, #43565, .T. ) ;
#257492 = EDGE_CURVE ( 'NONE', #47066, #39469, #106107, .T. ) ;
#257493 = VECTOR ( 'NONE', #133899, 1000.000000000000227 ) ;
#257494 = EDGE_CURVE ( 'NONE', #243821, #109956, #80987, .T. ) ;
#257495 = ORIENTED_EDGE ( 'NONE', *, *, #184169, .F. ) ;
#257496 = CARTESIAN_POINT ( 'NONE',  ( -20.64999999999999858, 7.150000000011155876, -146.2500000000000284 ) ) ;
#257497 = CARTESIAN_POINT ( 'NONE',  ( 20.95512828230152280, 8.876151312336450161, -45.70243026550310361 ) ) ;
#257499 = EDGE_LOOP ( 'NONE', ( #166086, #194493, #87180, #129276 ) ) ;
#257498 = DIRECTION ( 'NONE',  ( 1.000000000000000000, 0.000000000000000000, 0.000000000000000000 ) ) ;
#257500 = EDGE_CURVE ( 'NONE', #161732, #20544, #201800, .T. ) ;
#257501 = CARTESIAN_POINT ( 'NONE',  ( 18.59999999999999432, -1.235880796157547756, -222.7862885752216471 ) ) ;
#257502 = SPHERICAL_SURFACE ( 'NONE', #144688, 0.1000000000000000056 ) ;
#257503 = DIRECTION ( 'NONE',  ( 1.000000000000000000, 0.000000000000000000, 0.000000000000000000 ) ) ;
#257504 = CARTESIAN_POINT ( 'NONE',  ( -20.64999999999999858, 23.68770167995059595, -252.8127582590406348 ) ) ;
#257505 = EDGE_CURVE ( 'NONE', #13648, #38706, #160331, .T. ) ;
#257506 = DIRECTION ( 'NONE',  ( 0.000000000000000000, -1.000000000000000000, 0.000000000000000000 ) ) ;
#257507 = CARTESIAN_POINT ( 'NONE',  ( -17.78043020864321022, 15.53411659463512429, -221.3228573289305245 ) ) ;
#257509 = ORIENTED_EDGE ( 'NONE', *, *, #238385, .T. ) ;
#257508 = DIRECTION ( 'NONE',  ( 0.000000000000000000, -8.338584948901395817E-15, 1.000000000000000000 ) ) ;
#257511 = ORIENTED_EDGE ( 'NONE', *, *, #103803, .T. ) ;
#257510 = DIRECTION ( 'NONE',  ( 0.000000000000000000, -7.272083257015735086E-15, 1.000000000000000000 ) ) ;
#257512 = DIRECTION ( 'NONE',  ( 0.000000000000000000, -0.2617529984165035128, -0.9651348961777155289 ) ) ;
#257513 = ORIENTED_EDGE ( 'NONE', *, *, #217302, .F. ) ;
#257514 = ORIENTED_EDGE ( 'NONE', *, *, #146304, .T. ) ;
#257515 = CYLINDRICAL_SURFACE ( 'NONE', #126669, 0.09999999999998898659 ) ;
#257517 = DIRECTION ( 'NONE',  ( -1.000000000000000000, -1.116774769942150098E-16, -0.000000000000000000 ) ) ;
#257516 = CIRCLE ( 'NONE', #78502, 12.87499999999999822 ) ;
#257518 = VECTOR ( 'NONE', #164541, 1000.000000000000114 ) ;
#257519 = CARTESIAN_POINT ( 'NONE',  ( -6.000000000000003553, -11.34999999999999964, 10.10000000000000142 ) ) ;
#257520 = CARTESIAN_POINT ( 'NONE',  ( 23.14999999999999503, 11.65000000001116298, -160.4851942293460638 ) ) ;
#257521 = EDGE_CURVE ( 'NONE', #114655, #111692, #174977, .T. ) ;
#257523 = CARTESIAN_POINT ( 'NONE',  ( 21.72449340488910607, 10.28395627750227703, -42.75000000000000000 ) ) ;
#257522 = VECTOR ( 'NONE', #67974, 1000.000000000000000 ) ;
#257524 = CARTESIAN_POINT ( 'NONE',  ( 20.94999999999999929, 7.021664781911246322, -171.3335654018973173 ) ) ;
#257525 = CARTESIAN_POINT ( 'NONE',  ( 21.05000000000001847, 10.52493806863740389, -207.3780514093641614 ) ) ;
#257526 = ORIENTED_EDGE ( 'NONE', *, *, #16633, .F. ) ;
#257527 = ORIENTED_EDGE ( 'NONE', *, *, #59661, .F. ) ;
#257528 = FILL_AREA_STYLE ('',( #41140 ) ) ;
#257529 = CIRCLE ( 'NONE', #220193, 0.09999999999999939493 ) ;
#257530 = AXIS2_PLACEMENT_3D ( 'NONE', #106371, #98980, #184640 ) ;
#257531 = ORIENTED_EDGE ( 'NONE', *, *, #58034, .F. ) ;
#257532 = DIRECTION ( 'NONE',  ( -3.265361837132813093E-16, 1.000000000000000000, 0.000000000000000000 ) ) ;
#257534 = DIRECTION ( 'NONE',  ( 0.000000000000000000, -0.4930308989875170078, -0.8700118002898356018 ) ) ;
#257533 = CIRCLE ( 'NONE', #195274, 0.09999999999999986677 ) ;
#257535 = CARTESIAN_POINT ( 'NONE',  ( -12.60206096961792355, 66.61031399435590572, -53.85026397817309629 ) ) ;
#257536 = VECTOR ( 'NONE', #52224, 1000.000000000000227 ) ;
#257537 = CARTESIAN_POINT ( 'NONE',  ( -21.53752568622134689, -1.347531963291977330, -194.3475782847241931 ) ) ;
#257538 = VERTEX_POINT ( 'NONE', #54952 ) ;
#257539 = EDGE_CURVE ( 'NONE', #150112, #37076, #114319, .T. ) ;
#257540 = DIRECTION ( 'NONE',  ( 1.000000000000000000, -0.000000000000000000, -0.000000000000000000 ) ) ;
#257541 = ORIENTED_EDGE ( 'NONE', *, *, #207044, .F. ) ;
#257542 = DIRECTION ( 'NONE',  ( 1.000000000000000000, 0.000000000000000000, 0.000000000000000000 ) ) ;
#257543 = ORIENTED_EDGE ( 'NONE', *, *, #151196, .F. ) ;
#257544 = CIRCLE ( 'NONE', #145167, 0.09999999999998898659 ) ;
#257545 = CARTESIAN_POINT ( 'NONE',  ( 23.04999999999999716, 8.822561741677553471, -46.15000000000001279 ) ) ;
#257546 = DIRECTION ( 'NONE',  ( 0.000000000000000000, 3.469446951953635015E-14, 1.000000000000000000 ) ) ;
#257547 = DIRECTION ( 'NONE',  ( -1.000000000000000000, 0.000000000000000000, 0.000000000000000000 ) ) ;
#257548 = ORIENTED_EDGE ( 'NONE', *, *, #211785, .F. ) ;
#257549 = CARTESIAN_POINT ( 'NONE',  ( 21.05000000000000071, 1.115600667400684642E-11, -167.5000000000000284 ) ) ;
#257550 = CIRCLE ( 'NONE', #16050, 0.1000000000000001860 ) ;
#257552 = ORIENTED_EDGE ( 'NONE', *, *, #228523, .T. ) ;
#257551 = DIRECTION ( 'NONE',  ( 0.000000000000000000, 0.4088369013363281068, -0.9126074666063770380 ) ) ;
#257553 = EDGE_CURVE ( 'NONE', #222451, #86057, #180971, .T. ) ;
#257554 = SPHERICAL_SURFACE ( 'NONE', #210441, 0.1000000000000000056 ) ;
#257555 = VERTEX_POINT ( 'NONE', #160526 ) ;
#257556 = TOROIDAL_SURFACE ( 'NONE', #57870, 3.899999999999999467, 0.1000000000000000056 ) ;
#257557 = AXIS2_PLACEMENT_3D ( 'NONE', #129221, #108377, #191789 ) ;
#257558 = AXIS2_PLACEMENT_3D ( 'NONE', #172136, #74312, #16886 ) ;
#257559 = CARTESIAN_POINT ( 'NONE',  ( 21.30000000000002558, 0.000000000000000000, 0.000000000000000000 ) ) ;
#257560 = ORIENTED_EDGE ( 'NONE', *, *, #22427, .F. ) ;
#257562 = AXIS2_PLACEMENT_3D ( 'NONE', #157009, #233952, #56564 ) ;
#257561 = DIRECTION ( 'NONE',  ( -0.000000000000000000, 0.4721928772777345684, 0.8814952561688429444 ) ) ;
#257563 = CARTESIAN_POINT ( 'NONE',  ( 22.47809213839789066, 26.01172523223769417, -254.2798450918986646 ) ) ;
#257564 = CARTESIAN_POINT ( 'NONE',  ( -20.64999999999999858, 8.772386841380839684, -220.8375963540301257 ) ) ;
#257565 = DIRECTION ( 'NONE',  ( 0.000000000000000000, -2.775557561563196798E-13, -1.000000000000000000 ) ) ;
#257566 = CYLINDRICAL_SURFACE ( 'NONE', #27074, 0.09999999999999939493 ) ;
#257567 = EDGE_LOOP ( 'NONE', ( #15728, #240720, #85035, #228259 ) ) ;
#257568 = CYLINDRICAL_SURFACE ( 'NONE', #240215, 0.1000000000000028644 ) ;
#257569 = CARTESIAN_POINT ( 'NONE',  ( 21.05000000000000071, 6.477552182504600964, -100.5999999652995882 ) ) ;
#257570 = DIRECTION ( 'NONE',  ( 0.000000000000000000, -1.000000000000000000, 3.469446951953614189E-14 ) ) ;
#257571 = VERTEX_POINT ( 'NONE', #123950 ) ;
#257572 = DIRECTION ( 'NONE',  ( 1.000000000000000000, 0.000000000000000000, 0.000000000000000000 ) ) ;
#257574 = EDGE_LOOP ( 'NONE', ( #8581, #45116, #22936, #175687 ) ) ;
#257573 = AXIS2_PLACEMENT_3D ( 'NONE', #223620, #24175, #29337 ) ;
#257576 = AXIS2_PLACEMENT_3D ( 'NONE', #13119, #32718, #9253 ) ;
#257575 = DIRECTION ( 'NONE',  ( 1.000000000000000000, 0.000000000000000000, 0.000000000000000000 ) ) ;
#257577 = ORIENTED_EDGE ( 'NONE', *, *, #200506, .T. ) ;
#257578 = CARTESIAN_POINT ( 'NONE',  ( 20.85000000000000142, 14.70949956575304185, -235.9560995168023112 ) ) ;
#257579 = DIRECTION ( 'NONE',  ( 0.000000000000000000, 0.1180230956474139226, -0.9930108503404186937 ) ) ;
#257581 = EDGE_LOOP ( 'NONE', ( #249683, #21017, #97257, #230578 ) ) ;
#257580 = FACE_OUTER_BOUND ( 'NONE', #82165, .T. ) ;
#257582 = CARTESIAN_POINT ( 'NONE',  ( -18.40000000000000213, 8.780520186313282238, -245.4165333277509831 ) ) ;
#257583 = ORIENTED_EDGE ( 'NONE', *, *, #169635, .T. ) ;
#257584 = CARTESIAN_POINT ( 'NONE',  ( 21.05000000000005400, 76.00000000001119815, -36.02310748452479316 ) ) ;
#257585 = AXIS2_PLACEMENT_3D ( 'NONE', #34558, #14995, #12433 ) ;
#257586 = ADVANCED_FACE ( 'NONE', ( #221725 ), #104347, .F. ) ;
#257587 = DIRECTION ( 'NONE',  ( 0.000000000000000000, -0.9209589331071864615, 0.3896596508878908960 ) ) ;
#257588 = VERTEX_POINT ( 'NONE', #183910 ) ;
#257589 = ORIENTED_EDGE ( 'NONE', *, *, #148901, .F. ) ;
#257590 = DIRECTION ( 'NONE',  ( 0.000000000000000000, 0.8700118002898356018, -0.4930308989875170078 ) ) ;
#257591 = CARTESIAN_POINT ( 'NONE',  ( 20.95512820512820440, 67.12384868372377866, -94.46447848938342418 ) ) ;
#257592 = AXIS2_PLACEMENT_3D ( 'NONE', #176086, #198181, #240310 ) ;
#257593 = ORIENTED_EDGE ( 'NONE', *, *, #200637, .T. ) ;
#257594 = CARTESIAN_POINT ( 'NONE',  ( 20.90000000000000213, 1.885425182446133885, -11.49641995933507843 ) ) ;
#257595 = ORIENTED_EDGE ( 'NONE', *, *, #42908, .F. ) ;
#257596 = ORIENTED_EDGE ( 'NONE', *, *, #209772, .F. ) ;
#257597 = CIRCLE ( 'NONE', #228459, 0.09999999999999939493 ) ;
#257598 = DIRECTION ( 'NONE',  ( 0.000000000000000000, 0.000000000000000000, 1.000000000000000000 ) ) ;
#257599 = EDGE_CURVE ( 'NONE', #101496, #106082, #27056, .T. ) ;
#257600 = ADVANCED_FACE ( 'NONE', ( #126507 ), #122676, .T. ) ;
#257602 = VERTEX_POINT ( 'NONE', #86059 ) ;
#257601 = LINE ( 'NONE', #96009, #1460 ) ;
#257603 = DIRECTION ( 'NONE',  ( 1.000000000000000000, 0.000000000000000000, 0.000000000000000000 ) ) ;
#257604 = CARTESIAN_POINT ( 'NONE',  ( -20.54999999999999716, 7.150000000011155876, -45.75000000000000000 ) ) ;
#257605 = AXIS2_PLACEMENT_3D ( 'NONE', #12473, #55391, #151995 ) ;
#257606 = DIRECTION ( 'NONE',  ( -1.000000000000000000, -0.000000000000000000, -0.000000000000000000 ) ) ;
#257607 = AXIS2_PLACEMENT_3D ( 'NONE', #245478, #244161, #88937 ) ;
#257609 = DIRECTION ( 'NONE',  ( -7.304098846217948299E-16, -1.000000000000000000, 0.000000000000000000 ) ) ;
#257608 = FACE_OUTER_BOUND ( 'NONE', #21305, .T. ) ;
#257610 = DIRECTION ( 'NONE',  ( 6.938893903906840889E-14, -0.2128009952263485993, 0.9770955615653341697 ) ) ;
#257611 = DIRECTION ( 'NONE',  ( 0.000000000000000000, 0.2617529984165152257, 0.9651348961777124202 ) ) ;
#257612 = EDGE_CURVE ( 'NONE', #214318, #93424, #76902, .T. ) ;
#257613 = PLANE ( 'NONE',  #135051 ) ;
#257614 = LINE ( 'NONE', #79009, #96634 ) ;
#257615 = ORIENTED_EDGE ( 'NONE', *, *, #84884, .T. ) ;
#257617 = ORIENTED_EDGE ( 'NONE', *, *, #45849, .F. ) ;
#257616 = DIRECTION ( 'NONE',  ( 0.000000000000000000, 0.000000000000000000, -1.000000000000000000 ) ) ;
#257618 = VERTEX_POINT ( 'NONE', #185195 ) ;
#257619 = CARTESIAN_POINT ( 'NONE',  ( -18.35668295345803713, 64.52683809665005299, -179.2731074845244450 ) ) ;
#257620 = VERTEX_POINT ( 'NONE', #146056 ) ;
#257621 = CARTESIAN_POINT ( 'NONE',  ( 20.95346350065193519, 8.887177249174493809, -8.511731947035384493 ) ) ;
#257622 = EDGE_CURVE ( 'NONE', #22332, #53093, #223027, .T. ) ;
#257623 = CIRCLE ( 'NONE', #149395, 11.74999999999999645 ) ;
#257624 = VERTEX_POINT ( 'NONE', #165651 ) ;
#257625 = EDGE_CURVE ( 'NONE', #191619, #28459, #176886, .T. ) ;
#257626 = CARTESIAN_POINT ( 'NONE',  ( -20.90000000000000213, 7.800000000000000711, -1.300000000000000044 ) ) ;
#257628 = EDGE_LOOP ( 'NONE', ( #136268, #104985, #220187, #23907 ) ) ;
#257627 = ORIENTED_EDGE ( 'NONE', *, *, #67365, .T. ) ;
#257629 = VERTEX_POINT ( 'NONE', #224317 ) ;
#257630 = ORIENTED_EDGE ( 'NONE', *, *, #231597, .F. ) ;
#257631 = DIRECTION ( 'NONE',  ( -1.000000000000000000, 0.000000000000000000, 0.000000000000000000 ) ) ;
#257632 = CARTESIAN_POINT ( 'NONE',  ( -16.86578989773640913, 30.32384205394743404, -234.8305042728591161 ) ) ;
#257634 = EDGE_LOOP ( 'NONE', ( #48563, #40835, #61375 ) ) ;
#257633 = DIRECTION ( 'NONE',  ( 1.000000000000000000, 0.000000000000000000, 0.000000000000000000 ) ) ;
#257635 = CARTESIAN_POINT ( 'NONE',  ( 20.77526135991786660, 40.73566841623622281, -237.9374812591170780 ) ) ;
#257637 = ORIENTED_EDGE ( 'NONE', *, *, #236214, .T. ) ;
#257636 = DIRECTION ( 'NONE',  ( -1.000000000000000000, 0.000000000000000000, 0.000000000000000000 ) ) ;
#257638 = CARTESIAN_POINT ( 'NONE',  ( -21.76363531954647357, 0.09900187431060442078, -59.98706345212830371 ) ) ;
#257639 = ORIENTED_EDGE ( 'NONE', *, *, #221203, .T. ) ;
#257640 = CARTESIAN_POINT ( 'NONE',  ( -20.64999999999999858, 84.73084112150731073, -112.6211822035085675 ) ) ;
#257643 = ADVANCED_FACE ( 'NONE', ( #181369 ), #18648, .T. ) ;
#257642 = VERTEX_POINT ( 'NONE', #100488 ) ;
#257641 = DIRECTION ( 'NONE',  ( 0.000000000000000000, 0.4999999999999929501, 0.8660254037844427044 ) ) ;
#257644 = DIRECTION ( 'NONE',  ( 0.000000000000000000, 6.982962677686266711E-15, -1.000000000000000000 ) ) ;
#257645 = LINE ( 'NONE', #118206, #99921 ) ;
#257646 = CARTESIAN_POINT ( 'NONE',  ( 21.05000000000000071, 10.72371710471867701, -74.66491356908764487 ) ) ;
#257647 = ORIENTED_EDGE ( 'NONE', *, *, #198379, .T. ) ;
#257648 = VECTOR ( 'NONE', #169376, 1000.000000000000114 ) ;
#257651 = CARTESIAN_POINT ( 'NONE',  ( 20.94999999999999574, 65.37642973952908676, -95.53116228129383103 ) ) ;
#257650 = CIRCLE ( 'NONE', #241171, 0.5000000000000004441 ) ;
#257649 = CARTESIAN_POINT ( 'NONE',  ( -16.93710578446435733, 9.950000000011137047, -46.41880398379915817 ) ) ;
#257652 = CARTESIAN_POINT ( 'NONE',  ( -12.42749937872396515, 66.62931007840923314, -85.49664235786333677 ) ) ;
#257653 = AXIS2_PLACEMENT_3D ( 'NONE', #186953, #244314, #65686 ) ;
#257654 = CIRCLE ( 'NONE', #149994, 0.09999999999998898659 ) ;
#257655 = CARTESIAN_POINT ( 'NONE',  ( 18.36493879433276177, 85.50000080620296217, -163.1009588241743984 ) ) ;
#257656 = DIRECTION ( 'NONE',  ( -1.000000000000000000, 0.000000000000000000, -0.000000000000000000 ) ) ;
#257657 = CARTESIAN_POINT ( 'NONE',  ( 18.39999999999998082, 13.17878477875124865, -207.5966336730521391 ) ) ;
#257658 = ORIENTED_EDGE ( 'NONE', *, *, #72392, .F. ) ;
#257659 = EDGE_LOOP ( 'NONE', ( #12377, #152059, #118615, #217931, #204708 ) ) ;
#257660 = EDGE_LOOP ( 'NONE', ( #185991, #196593, #242916, #199962 ) ) ;
#257661 = EDGE_CURVE ( 'NONE', #241341, #45688, #110401, .T. ) ;
#257662 = DIRECTION ( 'NONE',  ( 0.000000000000000000, -1.000000000000000000, 0.000000000000000000 ) ) ;
#257663 = CIRCLE ( 'NONE', #103582, 0.09999999999999939493 ) ;
#257664 = VERTEX_POINT ( 'NONE', #3985 ) ;
#257665 = DIRECTION ( 'NONE',  ( 0.000000000000000000, 0.000000000000000000, -1.000000000000000000 ) ) ;
#257666 = EDGE_LOOP ( 'NONE', ( #192133, #171949, #122798, #51103 ) ) ;
#257667 = FACE_OUTER_BOUND ( 'NONE', #52756, .T. ) ;
#257668 = CARTESIAN_POINT ( 'NONE',  ( 21.04999999999998650, 64.01960172407876826, -222.2915665888316141 ) ) ;
#257669 = EDGE_CURVE ( 'NONE', #171719, #251940, #21014, .T. ) ;
#257670 = AXIS2_PLACEMENT_3D ( 'NONE', #8151, #168553, #6856 ) ;
#257671 = CIRCLE ( 'NONE', #191133, 0.09999999999999939493 ) ;
#257672 = EDGE_LOOP ( 'NONE', ( #194655, #178091, #164964, #22394 ) ) ;
#257673 = CIRCLE ( 'NONE', #207691, 3.899999999999987033 ) ;
#257674 = LINE ( 'NONE', #140344, #227577 ) ;
#257675 = SURFACE_STYLE_FILL_AREA ( #176950 ) ;
#257676 = ADVANCED_FACE ( 'NONE', ( #242587 ), #65242, .F. ) ;
#257677 = ADVANCED_FACE ( 'NONE', ( #225576 ), #197832, .F. ) ;
#257678 = EDGE_LOOP ( 'NONE', ( #216834, #42239, #230432, #55308, #34568 ) ) ;
#257679 = AXIS2_PLACEMENT_3D ( 'NONE', #56591, #176599, #194878 ) ;
#257680 = ORIENTED_EDGE ( 'NONE', *, *, #719, .T. ) ;
#257681 = ORIENTED_EDGE ( 'NONE', *, *, #39522, .T. ) ;
#257682 = LINE ( 'NONE', #3403, #142056 ) ;
#257683 = CARTESIAN_POINT ( 'NONE',  ( -20.64999999999999858, 2.000000000011154189, -187.7753780772378889 ) ) ;
#257684 = DIRECTION ( 'NONE',  ( 0.000000000000000000, 0.2128009952263403282, -0.9770955615653358350 ) ) ;
#257685 = DIRECTION ( 'NONE',  ( 1.000000000000000000, 0.000000000000000000, 0.000000000000000000 ) ) ;
#257686 = DIRECTION ( 'NONE',  ( 0.000000000000000000, 0.000000000000000000, 1.000000000000000000 ) ) ;
#257687 = EDGE_CURVE ( 'NONE', #11381, #38071, #89933, .T. ) ;
#257689 = CYLINDRICAL_SURFACE ( 'NONE', #228183, 0.1000000000000000472 ) ;
#257688 = DIRECTION ( 'NONE',  ( 1.000000000000000000, 0.000000000000000000, 0.000000000000000000 ) ) ;
#257690 = DIRECTION ( 'NONE',  ( 0.000000000000000000, -7.086529944415894657E-15, 1.000000000000000000 ) ) ;
#257692 = ORIENTED_EDGE ( 'NONE', *, *, #150360, .F. ) ;
#257691 = SPHERICAL_SURFACE ( 'NONE', #202255, 0.1000000000000000056 ) ;
#257693 = DIRECTION ( 'NONE',  ( 0.000000000000000000, -6.352154140967427193E-15, 1.000000000000000000 ) ) ;
#257694 = EDGE_LOOP ( 'NONE', ( #55881, #6406, #45492, #120158 ) ) ;
#257695 = CARTESIAN_POINT ( 'NONE',  ( -18.49346865148318386, -9.443073798513808015, -141.1851962553153328 ) ) ;
#257696 = VERTEX_POINT ( 'NONE', #172093 ) ;
#257697 = EDGE_LOOP ( 'NONE', ( #170329, #244464, #209211, #126751 ) ) ;
#257698 = DIRECTION ( 'NONE',  ( 0.000000000000000000, 0.2617529984165031243, 0.9651348961777157509 ) ) ;
#257699 = CYLINDRICAL_SURFACE ( 'NONE', #10444, 0.5000000000000004441 ) ;
#257701 = EDGE_CURVE ( 'NONE', #189246, #25147, #13003, .T. ) ;
#257700 = CARTESIAN_POINT ( 'NONE',  ( -23.15000000000000213, 47.91013932883114990, -242.3192343197862044 ) ) ;
#257703 = EDGE_CURVE ( 'NONE', #64997, #175552, #222827, .T. ) ;
#257702 = VERTEX_POINT ( 'NONE', #149942 ) ;
#257704 = VECTOR ( 'NONE', #174663, 999.9999999999998863 ) ;
#257705 = TOROIDAL_SURFACE ( 'NONE', #249402, 0.6000000000000017542, 0.1000000000000000056 ) ;
#257706 = DIRECTION ( 'NONE',  ( 0.000000000000000000, 6.982962677686266711E-15, -1.000000000000000000 ) ) ;
#257707 = ORIENTED_EDGE ( 'NONE', *, *, #109709, .T. ) ;
#257708 = ORIENTED_EDGE ( 'NONE', *, *, #247649, .F. ) ;
#257709 = ADVANCED_FACE ( 'NONE', ( #127800 ), #30001, .T. ) ;
#257710 = FACE_OUTER_BOUND ( 'NONE', #40705, .T. ) ;
#257711 = ORIENTED_EDGE ( 'NONE', *, *, #204957, .F. ) ;
#257712 = CARTESIAN_POINT ( 'NONE',  ( -16.94037747912386394, 60.85215442253927165, -221.1205180743122298 ) ) ;
#257713 = CARTESIAN_POINT ( 'NONE',  ( -18.40000000000000213, 11.33174054713633261, -188.3499999999999659 ) ) ;
#257714 = EDGE_LOOP ( 'NONE', ( #4935, #5766, #190637 ) ) ;
#257716 = DIRECTION ( 'NONE',  ( -2.978066053179066272E-16, -1.000000000000000000, -7.147358527629759053E-15 ) ) ;
#257715 = CIRCLE ( 'NONE', #141254, 2.100000000000004530 ) ;
#257717 = CARTESIAN_POINT ( 'NONE',  ( -16.87036670365549895, 22.88247411645692253, -230.8391385443351282 ) ) ;
#257718 = CARTESIAN_POINT ( 'NONE',  ( 18.49999999999998934, 21.15538238767524604, -233.7023398932965108 ) ) ;
#257719 = EDGE_LOOP ( 'NONE', ( #199041, #130561, #183501, #225966 ) ) ;
#257720 = ADVANCED_FACE ( 'NONE', ( #148653 ), #224488, .T. ) ;
#257721 = DIRECTION ( 'NONE',  ( 0.000000000000000000, 7.056502275159890832E-15, -1.000000000000000000 ) ) ;
#257722 = CARTESIAN_POINT ( 'NONE',  ( -20.94999999999999929, 1.115600667400684642E-11, -134.0000000000000284 ) ) ;
#257723 = CARTESIAN_POINT ( 'NONE',  ( -22.49072729836730389, 26.00394800917974436, -254.2625701408315990 ) ) ;
#257724 = AXIS2_PLACEMENT_3D ( 'NONE', #20142, #59209, #99632 ) ;
#257725 = AXIS2_PLACEMENT_3D ( 'NONE', #149412, #210643, #172854 ) ;
#257726 = ORIENTED_EDGE ( 'NONE', *, *, #155913, .T. ) ;
#257727 = VECTOR ( 'NONE', #72177, 1000.000000000000000 ) ;
#257729 = VERTEX_POINT ( 'NONE', #130342 ) ;
#257728 = CARTESIAN_POINT ( 'NONE',  ( -21.05000000000000071, 0.5663372425336981042, -209.0641885820623997 ) ) ;
#257730 = ORIENTED_EDGE ( 'NONE', *, *, #157365, .T. ) ;
#257731 = EDGE_CURVE ( 'NONE', #207618, #62655, #28740, .T. ) ;
#257732 = DIRECTION ( 'NONE',  ( 0.000000000000000000, -0.3427706569149635563, 0.9394191166662964054 ) ) ;
#257733 = EDGE_CURVE ( 'NONE', #111921, #69129, #52082, .T. ) ;
#257734 = CARTESIAN_POINT ( 'NONE',  ( -22.49231231312463208, 12.57605540120662901, -223.4344661467465301 ) ) ;
#257735 = FACE_OUTER_BOUND ( 'NONE', #170409, .T. ) ;
#257737 = AXIS2_PLACEMENT_3D ( 'NONE', #44500, #238836, #61485 ) ;
#257736 = CARTESIAN_POINT ( 'NONE',  ( 21.14999999999999858, 8.882751598337874199, -187.0399955572217721 ) ) ;
#257738 = CARTESIAN_POINT ( 'NONE',  ( 18.39999999999999503, 64.25000000001222134, -145.7731074845244450 ) ) ;
#257739 = DIRECTION ( 'NONE',  ( 0.000000000000000000, -7.147358527629766941E-15, 1.000000000000000000 ) ) ;
#257740 = AXIS2_PLACEMENT_3D ( 'NONE', #127626, #207172, #28577 ) ;
#257741 = EDGE_LOOP ( 'NONE', ( #65209, #200820, #93750, #205789 ) ) ;
#257742 = CARTESIAN_POINT ( 'NONE',  ( -23.39999999999994529, 84.00000000001119815, -34.86056257560453986 ) ) ;
#257743 = FACE_OUTER_BOUND ( 'NONE', #275, .T. ) ;
#257744 = CARTESIAN_POINT ( 'NONE',  ( -18.46154800491015990, 77.18277205392021756, -241.7850219657576076 ) ) ;
#257745 = CARTESIAN_POINT ( 'NONE',  ( 22.39999999999999503, 26.02743912001966464, -254.3139371321002216 ) ) ;
#257746 = ADVANCED_FACE ( 'NONE', ( #152521 ), #53385, .T. ) ;
#257747 = CARTESIAN_POINT ( 'NONE',  ( 20.97107704358301916, 67.12452184799030874, -60.96413425513512863 ) ) ;
#257748 = AXIS2_PLACEMENT_3D ( 'NONE', #173134, #54413, #34889 ) ;
#257749 = AXIS2_PLACEMENT_3D ( 'NONE', #173225, #14119, #93632 ) ;
#257751 = VERTEX_POINT ( 'NONE', #87358 ) ;
#257750 = CIRCLE ( 'NONE', #3726, 11.70000000000000284 ) ;
#257752 = ORIENTED_EDGE ( 'NONE', *, *, #32853, .F. ) ;
#257753 = CARTESIAN_POINT ( 'NONE',  ( -5.999999999999938716, 64.35000000001120668, -25.92310748452479174 ) ) ;
#257754 = AXIS2_PLACEMENT_3D ( 'NONE', #110808, #190373, #10440 ) ;
#257755 = DIRECTION ( 'NONE',  ( 1.000000000000000000, 0.000000000000000000, 0.000000000000000000 ) ) ;
#257756 = DIRECTION ( 'NONE',  ( 1.000000000000000000, 0.000000000000000000, 0.000000000000000000 ) ) ;
#257757 = CARTESIAN_POINT ( 'NONE',  ( 21.14999999999999503, -2.576749817950531707, -189.6385361693310756 ) ) ;
#257758 = CARTESIAN_POINT ( 'NONE',  ( 21.14999999999999503, -11.64999999998883595, -122.2500000000000284 ) ) ;
#257759 = AXIS2_PLACEMENT_3D ( 'NONE', #187501, #88348, #85769 ) ;
#257760 = ORIENTED_EDGE ( 'NONE', *, *, #198917, .T. ) ;
#257761 = CARTESIAN_POINT ( 'NONE',  ( 20.94999999999999929, 76.00000000001189449, -101.0231074845243029 ) ) ;
#257762 = ITEM_DEFINED_TRANSFORMATION ( 'NONE', 'NONE', #165285,  #2425 ) ;
#257763 = CARTESIAN_POINT ( 'NONE',  ( 21.14999999999999503, 76.10000000001276987, -215.1726782920691505 ) ) ;
#257764 = EDGE_CURVE ( 'NONE', #44201, #49525, #201999, .T. ) ;
#257765 = DIRECTION ( 'NONE',  ( -1.000000000000000000, 0.000000000000000000, 0.000000000000000000 ) ) ;
#257766 = PRODUCT ( 'Snap Open Cable Crossbars 3', 'Snap Open Cable Crossbars 3', '', ( #123763 ) ) ;
#257767 = DIRECTION ( 'NONE',  ( 0.000000000000000000, -6.982962677686266711E-15, 1.000000000000000000 ) ) ;
#257768 = EDGE_CURVE ( 'NONE', #143460, #128093, #193803, .T. ) ;
#257769 =( GEOMETRIC_REPRESENTATION_CONTEXT ( 3 ) GLOBAL_UNCERTAINTY_ASSIGNED_CONTEXT ( ( #239665 ) ) GLOBAL_UNIT_ASSIGNED_CONTEXT ( ( #198158, #6373, #242411 ) ) REPRESENTATION_CONTEXT ( 'NONE', 'WORKASPACE' ) );
#257770 = ORIENTED_EDGE ( 'NONE', *, *, #215678, .T. ) ;
#257771 = CARTESIAN_POINT ( 'NONE',  ( -21.05000000000000071, 12.82677665681127976, -205.1493534351658354 ) ) ;
#257772 = EDGE_CURVE ( 'NONE', #168498, #228584, #96339, .T. ) ;
#257773 = EDGE_LOOP ( 'NONE', ( #158027, #120442, #32988, #97530 ) ) ;
#257774 = CARTESIAN_POINT ( 'NONE',  ( 21.05000000000000071, 69.52244781751889491, -169.9231075192253115 ) ) ;
#257775 = DIRECTION ( 'NONE',  ( 0.000000000000000000, -0.8814952561688437216, 0.4721928772777334582 ) ) ;
#257776 = CARTESIAN_POINT ( 'NONE',  ( -20.54999999999999716, 2.000000000011154189, -113.7246219227621395 ) ) ;
#257777 = DIRECTION ( 'NONE',  ( 0.000000000000000000, 0.9126074666063777041, 0.4088369013363267190 ) ) ;
#257779 = EDGE_CURVE ( 'NONE', #161574, #253517, #93784, .T. ) ;
#257778 = CARTESIAN_POINT ( 'NONE',  ( 21.05000000000000071, 18.80860808352057134, -227.8685889463688454 ) ) ;
#257780 = LINE ( 'NONE', #59604, #58042 ) ;
#257781 = DIRECTION ( 'NONE',  ( 0.000000000000000000, -0.9887567792719351711, 0.1495327102803594987 ) ) ;
#257782 = DIRECTION ( 'NONE',  ( 0.000000000000000000, -0.9910465087640865089, -0.1335171055202864221 ) ) ;
#257783 = DIRECTION ( 'NONE',  ( 0.000000000000000000, 0.000000000000000000, -1.000000000000000000 ) ) ;
#257784 = EDGE_CURVE ( 'NONE', #110056, #43771, #127161, .T. ) ;
#257785 = AXIS2_PLACEMENT_3D ( 'NONE', #19234, #93641, #134038 ) ;
#257786 = CARTESIAN_POINT ( 'NONE',  ( -21.05000000000000071, 76.00000000001237765, -170.0231074845243597 ) ) ;
#257787 = CARTESIAN_POINT ( 'NONE',  ( -23.15000000000000213, 64.25000000001253397, -182.1731074845244507 ) ) ;
#257788 = CARTESIAN_POINT ( 'NONE',  ( -18.50000000000000000, 7.021664781911246322, -204.8335654018972605 ) ) ;
#257789 = LINE ( 'NONE', #41391, #112188 ) ;
#257790 = VECTOR ( 'NONE', #210584, 1000.000000000000227 ) ;
#257791 = ADVANCED_FACE ( 'NONE', ( #158930 ), #55925, .F. ) ;
#257793 = ADVANCED_FACE ( 'NONE', ( #38975 ), #234586, .F. ) ;
#257792 = EDGE_CURVE ( 'NONE', #197017, #25429, #52136, .T. ) ;
#257794 = ORIENTED_EDGE ( 'NONE', *, *, #176048, .F. ) ;
#257795 = LINE ( 'NONE', #81740, #143725 ) ;
#257796 = DIRECTION ( 'NONE',  ( 0.000000000000000000, 0.000000000000000000, 1.000000000000000000 ) ) ;
#257797 = CARTESIAN_POINT ( 'NONE',  ( 20.87631937322882081, 10.47149503677605509, -41.07974587458117099 ) ) ;
#257798 = EDGE_LOOP ( 'NONE', ( #79399, #92292, #66733 ) ) ;
#257799 = DIRECTION ( 'NONE',  ( 6.484947573744954877E-15, -0.9274965247785555977, 0.3738317757009190223 ) ) ;
#257800 = VECTOR ( 'NONE', #230563, 1000.000000000000000 ) ;
#257801 = DIRECTION ( 'NONE',  ( -0.000000000000000000, 0.4721928772777345684, 0.8814952561688429444 ) ) ;
#257802 = AXIS2_PLACEMENT_3D ( 'NONE', #99202, #161795, #181353 ) ;
#257803 = ORIENTED_EDGE ( 'NONE', *, *, #48142, .F. ) ;
#257804 = CARTESIAN_POINT ( 'NONE',  ( -23.15000000000000213, 1.115600667400684642E-11, -67.00000000000000000 ) ) ;
#257805 = CARTESIAN_POINT ( 'NONE',  ( -23.15000000000000213, 2.000000000011154189, -188.3753780772378548 ) ) ;
#257806 = ORIENTED_EDGE ( 'NONE', *, *, #175210, .T. ) ;
#257807 = EDGE_CURVE ( 'NONE', #183877, #165216, #143724, .T. ) ;
#257809 = EDGE_CURVE ( 'NONE', #160946, #216004, #131251, .T. ) ;
#257808 = CIRCLE ( 'NONE', #245406, 0.4999999999999944489 ) ;
#257810 = ORIENTED_EDGE ( 'NONE', *, *, #70681, .F. ) ;
#257811 = DIRECTION ( 'NONE',  ( -0.000000000000000000, 0.9651348961777158619, -0.2617529984165031243 ) ) ;
#257812 = EDGE_CURVE ( 'NONE', #163992, #114614, #48050, .T. ) ;
#257813 = ORIENTED_EDGE ( 'NONE', *, *, #138665, .F. ) ;
#257814 = CARTESIAN_POINT ( 'NONE',  ( 18.59999999999999076, 74.16465844978765176, -124.9679561919613207 ) ) ;
#257815 = DIRECTION ( 'NONE',  ( 0.000000000000000000, 0.000000000000000000, -1.000000000000000000 ) ) ;
#257816 = PLANE ( 'NONE',  #53509 ) ;
#257817 = LINE ( 'NONE', #17968, #250164 ) ;
#257818 = DIRECTION ( 'NONE',  ( 1.000000000000000000, 0.000000000000000000, -0.000000000000000000 ) ) ;
#257819 = EDGE_CURVE ( 'NONE', #121672, #70695, #235294, .T. ) ;
#257820 = CARTESIAN_POINT ( 'NONE',  ( -15.52965525596987995, 47.30882569885145017, -234.5067857460875302 ) ) ;
#257821 = DIRECTION ( 'NONE',  ( 0.000000000000000000, 0.000000000000000000, 1.000000000000000000 ) ) ;
#257822 = DIRECTION ( 'NONE',  ( 0.000000000000000000, 0.4088369013363281623, -0.9126074666063771490 ) ) ;
#257824 = ORIENTED_EDGE ( 'NONE', *, *, #25510, .T. ) ;
#257823 = CARTESIAN_POINT ( 'NONE',  ( -18.42609945526390902, -9.499999710479542614, -40.49936249024798229 ) ) ;
#257825 = ORIENTED_EDGE ( 'NONE', *, *, #157983, .T. ) ;
#257828 = DIRECTION ( 'NONE',  ( 0.000000000000000000, 0.000000000000000000, 1.000000000000000000 ) ) ;
#257827 = CARTESIAN_POINT ( 'NONE',  ( -20.64999999999999858, -8.999999999988844479, -57.50603087734755547 ) ) ;
#257826 = CIRCLE ( 'NONE', #53885, 0.1000000000000028644 ) ;
#257831 = VERTEX_POINT ( 'NONE', #14287 ) ;
#257830 = DIRECTION ( 'NONE',  ( 0.000000000000000000, 0.4088369013363345461, -0.9126074666063741514 ) ) ;
#257829 = DIRECTION ( 'NONE',  ( 1.000000000000000000, -0.000000000000000000, -0.000000000000000000 ) ) ;
#257832 = ORIENTED_EDGE ( 'NONE', *, *, #228064, .T. ) ;
#257833 = CARTESIAN_POINT ( 'NONE',  ( -16.90987985657660886, 66.04219248183250102, -149.1538203956407926 ) ) ;
#257834 = DIRECTION ( 'NONE',  ( 0.000000000000000000, 0.8814952561688431665, -0.4721928772777346794 ) ) ;
#257835 = CARTESIAN_POINT ( 'NONE',  ( 20.87155475150661132, 62.85241404162280077, -207.1112001314805582 ) ) ;
#257837 = B_SPLINE_CURVE_WITH_KNOTS ( 'NONE', 3,
 ( #203647, #25037, #131806, #146227 ),
 .UNSPECIFIED., .F., .F.,
 ( 4, 4 ),
 ( 0.000000000000000000, 7.713889350928753320E-05 ),
 .UNSPECIFIED. ) ;
#257836 = CARTESIAN_POINT ( 'NONE',  ( -21.05000000000000071, -11.48912529306489994, -130.9000000000000341 ) ) ;
#257838 = DIRECTION ( 'NONE',  ( 0.000000000000000000, 0.000000000000000000, 1.000000000000000000 ) ) ;
#257839 = EDGE_CURVE ( 'NONE', #126571, #120029, #98894, .T. ) ;
#257840 = CARTESIAN_POINT ( 'NONE',  ( -21.05000000000000071, 70.10000000001267040, -193.3040077198679967 ) ) ;
#257841 = CARTESIAN_POINT ( 'NONE',  ( 21.05000000000000071, 36.65892442174935439, -249.5511627012433848 ) ) ;
#257842 = B_SPLINE_CURVE_WITH_KNOTS ( 'NONE', 3,
 ( #194550, #116283, #191980, #150273, #130686, #94127, #13322, #210247 ),
 .UNSPECIFIED., .F., .F.,
 ( 4, 2, 2, 4 ),
 ( 0.000000000000000000, 0.0001306511400391254711, 0.0001959767100586882202, 0.0002613022800782509422 ),
 .UNSPECIFIED. ) ;
#257843 = DIRECTION ( 'NONE',  ( 0.000000000000000000, 1.265107689135680095E-16, -1.000000000000000000 ) ) ;
#257844 = EDGE_CURVE ( 'NONE', #188280, #22343, #196738, .T. ) ;
#257845 = AXIS2_PLACEMENT_3D ( 'NONE', #85566, #167744, #226376 ) ;
#257846 = ORIENTED_EDGE ( 'NONE', *, *, #36486, .T. ) ;
#257847 = ORIENTED_EDGE ( 'NONE', *, *, #194937, .T. ) ;
#257848 = VECTOR ( 'NONE', #31334, 1000.000000000000114 ) ;
#257849 = LINE ( 'NONE', #216191, #218886 ) ;
#257850 = AXIS2_PLACEMENT_3D ( 'NONE', #16357, #231544, #73771 ) ;
#257851 = CIRCLE ( 'NONE', #66376, 11.75000000000000178 ) ;
#257852 = ORIENTED_EDGE ( 'NONE', *, *, #216949, .T. ) ;
#257853 = DIRECTION ( 'NONE',  ( 1.000000000000000000, 0.000000000000000000, 0.000000000000000000 ) ) ;
#257854 = ORIENTED_EDGE ( 'NONE', *, *, #96490, .T. ) ;
#257855 = DIRECTION ( 'NONE',  ( -1.000000000000000000, -1.394253735153569469E-16, -2.602809386958778209E-16 ) ) ;
#257856 = CIRCLE ( 'NONE', #228715, 0.09999999999999939493 ) ;
#257857 = CARTESIAN_POINT ( 'NONE',  ( -14.11361717019516249, 49.67565583792541162, -233.3567449137543974 ) ) ;
#257858 = FACE_OUTER_BOUND ( 'NONE', #231175, .T. ) ;
#257859 = EDGE_CURVE ( 'NONE', #156337, #253401, #177216, .T. ) ;
#257860 = DIRECTION ( 'NONE',  ( 0.000000000000000000, 1.776356839400303713E-15, 1.000000000000000000 ) ) ;
#257861 = CARTESIAN_POINT ( 'NONE',  ( 21.05000000000000071, 6.350000000011161383, -177.3438220896831012 ) ) ;
#257862 = ORIENTED_EDGE ( 'NONE', *, *, #50616, .T. ) ;
#257863 = CARTESIAN_POINT ( 'NONE',  ( 23.14999999999999858, 74.00000000001170974, -69.52310748452431710 ) ) ;
#257865 = CARTESIAN_POINT ( 'NONE',  ( 22.45301702632625762, 0.01521087972134078925, -122.3502077757396336 ) ) ;
#257864 = AXIS2_PLACEMENT_3D ( 'NONE', #145716, #46608, #126151 ) ;
#257866 = CIRCLE ( 'NONE', #20429, 11.65000000000000036 ) ;
#257867 = FACE_OUTER_BOUND ( 'NONE', #43527, .T. ) ;
#257869 = VECTOR ( 'NONE', #55484, 1000.000000000000000 ) ;
#257868 = CARTESIAN_POINT ( 'NONE',  ( -23.25000000000000000, -11.74999999998884448, -197.8999999999999773 ) ) ;
#257870 = CARTESIAN_POINT ( 'NONE',  ( -18.59999999999999787, 74.83729825007360148, -61.42310748452432989 ) ) ;
#257871 = EDGE_LOOP ( 'NONE', ( #139086, #71382, #128413, #233631 ) ) ;
#257872 = CARTESIAN_POINT ( 'NONE',  ( -18.46919391072065153, 85.67072438828911629, -29.34930395272471415 ) ) ;
#257873 = EDGE_LOOP ( 'NONE', ( #76737, #52615, #146035, #169915 ) ) ;
#257876 = VERTEX_POINT ( 'NONE', #35149 ) ;
#257875 = DIRECTION ( 'NONE',  ( 0.000000000000000000, -0.1495327102803283015, 0.9887567792719397231 ) ) ;
#257874 = CARTESIAN_POINT ( 'NONE',  ( 20.94999999999999929, 76.00000000001188027, -99.02310748452428868 ) ) ;
#257877 = CIRCLE ( 'NONE', #28849, 0.4000000000000114575 ) ;
#257878 = SPHERICAL_SURFACE ( 'NONE', #110273, 0.1000000000000000056 ) ;
#257879 = CARTESIAN_POINT ( 'NONE',  ( -22.50000000000000000, 64.35012909624745703, -69.60562737539738976 ) ) ;
#257880 = ORIENTED_EDGE ( 'NONE', *, *, #229332, .T. ) ;
#257881 = CARTESIAN_POINT ( 'NONE',  ( 18.43466021071410310, 85.49419069046865616, -129.9060459243966932 ) ) ;
#257882 = CARTESIAN_POINT ( 'NONE',  ( -21.14999999999999858, 11.75000000001115552, -140.7261306360592243 ) ) ;
#257883 = CARTESIAN_POINT ( 'NONE',  ( 20.99999999999999645, 66.25000000001159606, -56.87310748452438958 ) ) ;
#257884 = UNCERTAINTY_MEASURE_WITH_UNIT (LENGTH_MEASURE( 1.000000000000000082E-05 ), #223454, 'distance_accuracy_value', 'NONE');
#257886 = ORIENTED_EDGE ( 'NONE', *, *, #35056, .T. ) ;
#257885 = DIRECTION ( 'NONE',  ( -0.000000000000000000, 0.4721928772777345684, 0.8814952561688429444 ) ) ;
#257887 = DIRECTION ( 'NONE',  ( -1.000000000000000000, 0.000000000000000000, 0.000000000000000000 ) ) ;
#257888 = EDGE_LOOP ( 'NONE', ( #149998, #18218, #78654, #18763 ) ) ;
#257889 = CARTESIAN_POINT ( 'NONE',  ( -20.54999999999999716, 74.00000000001229239, -157.2984855617622770 ) ) ;
#257890 = CARTESIAN_POINT ( 'NONE',  ( 18.59999999999999076, 5.950000000011100632, -144.3057023050348846 ) ) ;
#257891 = DIRECTION ( 'NONE',  ( -1.000000000000000000, -0.000000000000000000, -0.000000000000000000 ) ) ;
#257892 = VECTOR ( 'NONE', #142075, 1000.000000000000000 ) ;
#257893 = ORIENTED_EDGE ( 'NONE', *, *, #154338, .F. ) ;
#257894 = CARTESIAN_POINT ( 'NONE',  ( 20.95512820512820440, 18.90192396791320562, -227.9871466877642661 ) ) ;
#257895 = VERTEX_POINT ( 'NONE', #213740 ) ;
#257896 = CARTESIAN_POINT ( 'NONE',  ( 18.59999999999999076, 42.15997144203495139, -239.2817429668763793 ) ) ;
#257897 = DIRECTION ( 'NONE',  ( 0.000000000000000000, 0.000000000000000000, 1.000000000000000000 ) ) ;
#257898 = DIRECTION ( 'NONE',  ( 0.000000000000000000, -1.000000000000000000, 0.000000000000000000 ) ) ;
#257899 = AXIS2_PLACEMENT_3D ( 'NONE', #163434, #242954, #64333 ) ;
#257900 = ORIENTED_EDGE ( 'NONE', *, *, #177419, .T. ) ;
#257901 = CARTESIAN_POINT ( 'NONE',  ( -21.05000000000000071, 87.29603075034673054, -39.07100664418810965 ) ) ;
#257902 = DIRECTION ( 'NONE',  ( 0.000000000000000000, 0.000000000000000000, -1.000000000000000000 ) ) ;
#257903 = EDGE_CURVE ( 'NONE', #157610, #242842, #218715, .T. ) ;
#257904 = DIRECTION ( 'NONE',  ( 0.000000000000000000, 6.467318590049456648E-15, -1.000000000000000000 ) ) ;
#257905 = ORIENTED_EDGE ( 'NONE', *, *, #224996, .F. ) ;
#257906 = DIRECTION ( 'NONE',  ( 0.000000000000000000, 0.000000000000000000, -1.000000000000000000 ) ) ;
#257907 = DIRECTION ( 'NONE',  ( 0.000000000000000000, -0.9126074666063771490, -0.4088369013363281623 ) ) ;
#257908 = DIRECTION ( 'NONE',  ( 0.000000000000000000, 0.000000000000000000, -1.000000000000000000 ) ) ;
#257909 = CIRCLE ( 'NONE', #20660, 2.000000000000001776 ) ;
#257910 = ORIENTED_EDGE ( 'NONE', *, *, #115659, .F. ) ;
#257911 = CIRCLE ( 'NONE', #37414, 0.1000000000000055844 ) ;
#257912 = CARTESIAN_POINT ( 'NONE',  ( 21.05000000000000071, 11.65000000001116298, -45.65000000000000568 ) ) ;
#257913 = EDGE_LOOP ( 'NONE', ( #13356, #1090, #218673, #178467 ) ) ;
#257915 = ORIENTED_EDGE ( 'NONE', *, *, #144006, .T. ) ;
#257914 = DIRECTION ( 'NONE',  ( 1.000000000000000000, 7.304098846218134667E-16, 0.000000000000000000 ) ) ;
#257916 = EDGE_CURVE ( 'NONE', #100189, #113855, #215023, .T. ) ;
#257917 = VECTOR ( 'NONE', #76875, 1000.000000000000000 ) ;
#257918 = AXIS2_PLACEMENT_3D ( 'NONE', #93313, #232852, #90734 ) ;
#257919 = ADVANCED_FACE ( 'NONE', ( #117214 ), #174672, .T. ) ;
#257922 = VERTEX_POINT ( 'NONE', #257952 ) ;
#257921 = ORIENTED_EDGE ( 'NONE', *, *, #135947, .T. ) ;
#257920 = CARTESIAN_POINT ( 'NONE',  ( -21.07928932188134041, 0.09889514565439468108, 6.328516656393293083 ) ) ;
#257923 = PLANE ( 'NONE',  #216209 ) ;
#257924 = CARTESIAN_POINT ( 'NONE',  ( 18.49999999999999289, 65.79142135624951493, -145.3731074845244109 ) ) ;
#257925 = LINE ( 'NONE', #208292, #152409 ) ;
#257926 = CARTESIAN_POINT ( 'NONE',  ( 18.49999999999999645, -1.162701749926855266, -142.1000000000000227 ) ) ;
#257927 = DIRECTION ( 'NONE',  ( 0.000000000000000000, -0.9126074666063770380, -0.4088369013363281068 ) ) ;
#257928 = DIRECTION ( 'NONE',  ( -1.000000000000000000, -0.000000000000000000, -0.000000000000000000 ) ) ;
#257929 = AXIS2_PLACEMENT_3D ( 'NONE', #4689, #45123, #2129 ) ;
#257930 = DIRECTION ( 'NONE',  ( 0.000000000000000000, 1.000000000000000000, 0.000000000000000000 ) ) ;
#257932 = DIRECTION ( 'NONE',  ( 0.000000000000000000, 0.2617529984165432588, 0.9651348961777048707 ) ) ;
#257931 = CARTESIAN_POINT ( 'NONE',  ( -21.05000000000000071, -11.64999999998884306, -131.1000000000000227 ) ) ;
#257933 = AXIS2_PLACEMENT_3D ( 'NONE', #180878, #81729, #243403 ) ;
#257934 = AXIS2_PLACEMENT_3D ( 'NONE', #175339, #254790, #235270 ) ;
#257935 = VERTEX_POINT ( 'NONE', #75541 ) ;
#257936 = AXIS2_PLACEMENT_3D ( 'NONE', #165350, #160240, #225289 ) ;
#257937 = ORIENTED_EDGE ( 'NONE', *, *, #106095, .T. ) ;
#257938 = EDGE_CURVE ( 'NONE', #104231, #57195, #85421, .T. ) ;
#257939 = DIRECTION ( 'NONE',  ( 1.000000000000000000, -0.000000000000000000, -0.000000000000000000 ) ) ;
#257942 = ORIENTED_EDGE ( 'NONE', *, *, #205044, .T. ) ;
#257941 = EDGE_CURVE ( 'NONE', #32344, #194844, #31346, .T. ) ;
#257940 = CARTESIAN_POINT ( 'NONE',  ( -18.59999999999999787, -9.499999999988849808, -142.1000000000000227 ) ) ;
#257943 = DIRECTION ( 'NONE',  ( -1.000000000000000000, 0.000000000000000000, 0.000000000000000000 ) ) ;
#257944 = ORIENTED_EDGE ( 'NONE', *, *, #163467, .T. ) ;
#257945 = VECTOR ( 'NONE', #156720, 1000.000000000000000 ) ;
#257946 = CARTESIAN_POINT ( 'NONE',  ( -23.25000000000000000, 76.00000000001190870, -103.0231074845243029 ) ) ;
#257947 = ORIENTED_EDGE ( 'NONE', *, *, #12690, .T. ) ;
#257948 = FACE_OUTER_BOUND ( 'NONE', #208087, .T. ) ;
#257949 = ADVANCED_FACE ( 'NONE', ( #105304 ), #206276, .T. ) ;
#257950 = ORIENTED_EDGE ( 'NONE', *, *, #154004, .T. ) ;
#257951 = ADVANCED_FACE ( 'NONE', ( #124921 ), #100182, .F. ) ;
#257952 = CARTESIAN_POINT ( 'NONE',  ( 19.75857864376268935, 11.75000000001115907, -91.85000000000003695 ) ) ;
#257953 = CARTESIAN_POINT ( 'NONE',  ( 21.05000000000000071, 76.00000000001145395, -40.02310748452431710 ) ) ;
#257954 = AXIS2_PLACEMENT_3D ( 'NONE', #254178, #93832, #53428 ) ;
#257956 = VERTEX_POINT ( 'NONE', #184878 ) ;
#257955 = ORIENTED_EDGE ( 'NONE', *, *, #199523, .T. ) ;
#257957 = VERTEX_POINT ( 'NONE', #143175 ) ;
#257958 = CARTESIAN_POINT ( 'NONE',  ( -20.54999999999999716, 87.75000000001253397, -182.3731074845242972 ) ) ;
#257960 = EDGE_LOOP ( 'NONE', ( #98467, #4075, #145702, #5121 ) ) ;
#257959 = ADVANCED_FACE ( 'NONE', ( #121096 ), #241016, .F. ) ;
#257961 = ORIENTED_EDGE ( 'NONE', *, *, #248109, .F. ) ;
#257962 = CARTESIAN_POINT ( 'NONE',  ( 18.59999999999999076, 69.45000000001149942, -48.37310748452436826 ) ) ;
#257964 = VERTEX_POINT ( 'NONE', #160218 ) ;
#257963 = CARTESIAN_POINT ( 'NONE',  ( 18.59999999999999076, 76.00000000001213607, -136.5231074845243313 ) ) ;
#257966 = FACE_OUTER_BOUND ( 'NONE', #249725, .T. ) ;
#257965 = DIRECTION ( 'NONE',  ( 0.000000000000000000, -6.982962677686266711E-15, 1.000000000000000000 ) ) ;
#257967 = CARTESIAN_POINT ( 'NONE',  ( 23.14999999999999503, 56.06656052939784729, -228.0911609752645290 ) ) ;
#257968 = DIRECTION ( 'NONE',  ( 1.000000000000000000, 0.000000000000000000, 0.000000000000000000 ) ) ;
#257969 = DIRECTION ( 'NONE',  ( 0.000000000000000000, 0.9910465087640866200, -0.1335171055202867274 ) ) ;
#257970 = ORIENTED_EDGE ( 'NONE', *, *, #141713, .T. ) ;
#257971 = AXIS2_PLACEMENT_3D ( 'NONE', #37604, #237071, #77982 ) ;
#257973 = ADVANCED_FACE ( 'NONE', ( #181055 ), #185429, .F. ) ;
#257972 = ORIENTED_EDGE ( 'NONE', *, *, #166456, .F. ) ;
#257974 = FACE_OUTER_BOUND ( 'NONE', #166071, .T. ) ;
#257975 = CARTESIAN_POINT ( 'NONE',  ( -20.85000000000000142, 79.37986612816742138, -196.2658927859692142 ) ) ;
#257976 = AXIS2_PLACEMENT_3D ( 'NONE', #168627, #128166, #70785 ) ;
#257977 = ORIENTED_EDGE ( 'NONE', *, *, #254736, .F. ) ;
#257978 = CARTESIAN_POINT ( 'NONE',  ( -23.25000000000000000, -1.249999999988843369, -208.8004807544150481 ) ) ;
#257979 = CIRCLE ( 'NONE', #183033, 3.900000000000000799 ) ;
#257980 = CARTESIAN_POINT ( 'NONE',  ( -23.15000000000000213, 70.02906482874161043, -215.6060937950565233 ) ) ;
#257981 = DIRECTION ( 'NONE',  ( 0.000000000000000000, -0.9893560106964500722, 0.1455152366551550613 ) ) ;
#257982 = VERTEX_POINT ( 'NONE', #239732 ) ;
#257983 = VERTEX_POINT ( 'NONE', #41551 ) ;
#257984 = CARTESIAN_POINT ( 'NONE',  ( 20.85000000000000142, -1.835859311432481045, -212.5044391687984842 ) ) ;
#257985 = ORIENTED_EDGE ( 'NONE', *, *, #67359, .T. ) ;
#257986 = CARTESIAN_POINT ( 'NONE',  ( -18.59999999999999787, 66.75000000001260503, -191.2731074845244166 ) ) ;
#257987 = ORIENTED_EDGE ( 'NONE', *, *, #179077, .F. ) ;
#257988 = CARTESIAN_POINT ( 'NONE',  ( 21.05000000000000071, 76.00000000001213607, -136.5231074845242745 ) ) ;
#257989 = DIRECTION ( 'NONE',  ( 0.000000000000000000, -1.000000000000000000, 6.938893903907030216E-14 ) ) ;
#257991 = SURFACE_STYLE_FILL_AREA ( #178539 ) ;
#257990 = CARTESIAN_POINT ( 'NONE',  ( -18.50000000000000000, 9.250000000011157297, -121.7500000000000426 ) ) ;
#257992 = CIRCLE ( 'NONE', #87332, 11.65000000000000213 ) ;
#257993 = CARTESIAN_POINT ( 'NONE',  ( 18.49999999999999289, 11.75000000001115907, -21.75000000000000355 ) ) ;
#257994 = DIRECTION ( 'NONE',  ( 1.000000000000000000, 0.000000000000000000, 0.000000000000000000 ) ) ;
#257995 = AXIS2_PLACEMENT_3D ( 'NONE', #226870, #26122, #48235 ) ;
#257996 = LINE ( 'NONE', #157716, #173293 ) ;
#257997 = VECTOR ( 'NONE', #81913, 1000.000000000000227 ) ;
#257998 = EDGE_CURVE ( 'NONE', #140176, #208557, #114506, .T. ) ;
#258000 = VERTEX_POINT ( 'NONE', #243574 ) ;
#257999 = ORIENTED_EDGE ( 'NONE', *, *, #217178, .T. ) ;
#258001 = EDGE_LOOP ( 'NONE', ( #201164, #175389, #206900, #127808 ) ) ;
#258002 = DIRECTION ( 'NONE',  ( 0.000000000000000000, 0.000000000000000000, -1.000000000000000000 ) ) ;
#258003 = CARTESIAN_POINT ( 'NONE',  ( -18.50000000000000000, -7.631834139421013852, -210.1304494778855769 ) ) ;
#258004 = CARTESIAN_POINT ( 'NONE',  ( -20.94999999999999929, -11.41227409413852811, -97.60000000000005116 ) ) ;
#258005 = DIRECTION ( 'NONE',  ( 1.000000000000000000, -0.000000000000000000, -0.000000000000000000 ) ) ;
#258006 = ADVANCED_FACE ( 'NONE', ( #183607 ), #152127, .F. ) ;
#258008 = ADVANCED_FACE ( 'NONE', ( #42810 ), #147845, .T. ) ;
#258007 =( BOUNDED_CURVE ( )  B_SPLINE_CURVE ( 3, ( #191562, #69038, #12926, #76703 ),
 .UNSPECIFIED., .F., .F. ) 
 B_SPLINE_CURVE_WITH_KNOTS ( ( 4, 4 ),
 ( 1.570796326794908992, 2.617993877991549034 ),
 .UNSPECIFIED. ) 
 CURVE ( )  GEOMETRIC_REPRESENTATION_ITEM ( )  RATIONAL_B_SPLINE_CURVE ( ( 1.000000000000000000, 0.9106836025229521070, 0.9106836025229521070, 1.000000000000000000 ) ) 
 REPRESENTATION_ITEM ( '' )  );
#258010 = DIRECTION ( 'NONE',  ( 0.000000000000000000, 0.6728971962617388280, 0.7397360091702248619 ) ) ;
#258009 = CARTESIAN_POINT ( 'NONE',  ( 20.54374330479337374, 10.50501031422304798, -7.725683634888938833 ) ) ;
#258011 = ORIENTED_EDGE ( 'NONE', *, *, #116126, .F. ) ;
#258012 = FACE_OUTER_BOUND ( 'NONE', #141656, .T. ) ;
#258013 = ORIENTED_EDGE ( 'NONE', *, *, #52609, .F. ) ;
#258014 = CARTESIAN_POINT ( 'NONE',  ( -22.57320508075687115, 11.75000000001115552, -67.00000000000007105 ) ) ;
#258015 = VERTEX_POINT ( 'NONE', #102751 ) ;
#258016 = ORIENTED_EDGE ( 'NONE', *, *, #203726, .F. ) ;
#258017 = CARTESIAN_POINT ( 'NONE',  ( -20.54999999999999716, 76.00000000001213607, -136.5231074845242745 ) ) ;
#258018 = CARTESIAN_POINT ( 'NONE',  ( 21.05000000000000071, 6.540656951701244282, -0.09999999999999939493 ) ) ;
#258020 = ADVANCED_FACE ( 'NONE', ( #24550 ), #162772, .F. ) ;
#258019 = DIRECTION ( 'NONE',  ( -1.000000000000000000, 0.000000000000000000, 0.000000000000000000 ) ) ;
#258021 = ADVANCED_FACE ( 'NONE', ( #140614 ), #104035, .T. ) ;
#258022 = CARTESIAN_POINT ( 'NONE',  ( 21.46681500598285197, 76.00000000001273293, -210.3806186439483099 ) ) ;
#258023 = CIRCLE ( 'NONE', #70845, 0.1000000000000028644 ) ;
#258024 = AXIS2_PLACEMENT_3D ( 'NONE', #64204, #2925, #25101 ) ;
#258025 = EDGE_CURVE ( 'NONE', #148732, #153574, #191511, .T. ) ;
#258026 = EDGE_CURVE ( 'NONE', #76104, #130997, #66225, .T. ) ;
#258027 = DIRECTION ( 'NONE',  ( -2.978066053179064300E-16, 0.4721928772777334582, 0.8814952561688436106 ) ) ;
#258028 = ORIENTED_EDGE ( 'NONE', *, *, #48100, .T. ) ;
#258029 = ORIENTED_EDGE ( 'NONE', *, *, #74926, .F. ) ;
#258030 =( BOUNDED_CURVE ( )  B_SPLINE_CURVE ( 3, ( #10916, #206534, #29226, #46166 ),
 .UNSPECIFIED., .F., .F. ) 
 B_SPLINE_CURVE_WITH_KNOTS ( ( 4, 4 ),
 ( 4.712388980384689674, 6.283185307179586232 ),
 .UNSPECIFIED. ) 
 CURVE ( )  GEOMETRIC_REPRESENTATION_ITEM ( )  RATIONAL_B_SPLINE_CURVE ( ( 1.000000000000000000, 0.8047378541243649375, 0.8047378541243649375, 1.000000000000000000 ) ) 
 REPRESENTATION_ITEM ( '' )  );
#258031 = CARTESIAN_POINT ( 'NONE',  ( -16.81744102076748959, 66.05000000001153637, -48.67310748452439384 ) ) ;
#258032 = EDGE_CURVE ( 'NONE', #160493, #232467, #230428, .T. ) ;
#258033 = DIRECTION ( 'NONE',  ( -0.5932847527679310229, -0.8049926720990042694, -4.984624513800578906E-15 ) ) ;
#258034 = VERTEX_POINT ( 'NONE', #88316 ) ;
#258035 = DIRECTION ( 'NONE',  ( 0.000000000000000000, -0.2617529984165152257, -0.9651348961777124202 ) ) ;
#258036 = DIRECTION ( 'NONE',  ( -1.000000000000000000, 0.000000000000000000, 0.000000000000000000 ) ) ;
#258037 = CARTESIAN_POINT ( 'NONE',  ( -23.15000000000000213, 73.40000000001253966, -183.2477294072864709 ) ) ;
#258038 = DIRECTION ( 'NONE',  ( 0.000000000000000000, 0.000000000000000000, 1.000000000000000000 ) ) ;
#258039 = CARTESIAN_POINT ( 'NONE',  ( 21.05000000000000071, 11.65000000000000746, -26.48519422934605316 ) ) ;
#258040 = LINE ( 'NONE', #39065, #116708 ) ;
#258042 = CARTESIAN_POINT ( 'NONE',  ( -21.14999999999994174, 77.16254490893143725, -44.02310748452479316 ) ) ;
#258041 = DIRECTION ( 'NONE',  ( 0.000000000000000000, 0.8490545835447252943, 0.5283051335749948674 ) ) ;
#258043 = CARTESIAN_POINT ( 'NONE',  ( 18.59999999999999787, 86.35479209693734504, -109.2665665014504697 ) ) ;
#258044 = DIRECTION ( 'NONE',  ( -1.000000000000000000, 0.000000000000000000, 0.000000000000000000 ) ) ;
#258045 = AXIS2_PLACEMENT_3D ( 'NONE', #89449, #170333, #249826 ) ;
#258046 = CIRCLE ( 'NONE', #120743, 4.299999999999956302 ) ;
#258047 = CARTESIAN_POINT ( 'NONE',  ( 23.15000000000000213, -9.599999999988842347, -57.10603087734755690 ) ) ;
#258048 = CIRCLE ( 'NONE', #187190, 0.1000000000000072220 ) ;
#258049 = CIRCLE ( 'NONE', #53909, 3.999999999999994671 ) ;
#258050 = CARTESIAN_POINT ( 'NONE',  ( -18.44085059012131822, 11.51401249349495970, -57.74030531912154629 ) ) ;
#258051 =( BOUNDED_CURVE ( )  B_SPLINE_CURVE ( 3, ( #181269, #183812, #44316, #63867 ),
 .UNSPECIFIED., .F., .F. ) 
 B_SPLINE_CURVE_WITH_KNOTS ( ( 4, 4 ),
 ( 1.570796326794893893, 3.141592653589793116 ),
 .UNSPECIFIED. ) 
 CURVE ( )  GEOMETRIC_REPRESENTATION_ITEM ( )  RATIONAL_B_SPLINE_CURVE ( ( 1.000000000000000000, 0.8047378541243643824, 0.8047378541243643824, 1.000000000000000000 ) ) 
 REPRESENTATION_ITEM ( '' )  );
#258052 = EDGE_CURVE ( 'NONE', #176995, #74814, #2235, .T. ) ;
#258053 = VERTEX_POINT ( 'NONE', #145742 ) ;
#258054 = VECTOR ( 'NONE', #210022, 1000.000000000000000 ) ;
#258055 = CARTESIAN_POINT ( 'NONE',  ( -16.88328101497759448, 30.20753490274668351, -234.8072909416581524 ) ) ;
#258056 = ORIENTED_EDGE ( 'NONE', *, *, #123303, .T. ) ;
#258057 = EDGE_CURVE ( 'NONE', #20141, #205, #19647, .T. ) ;
#258058 = EDGE_CURVE ( 'NONE', #90910, #155920, #160705, .T. ) ;
#258059 = DIRECTION ( 'NONE',  ( -0.000000000000000000, 1.000000000000000000, 0.000000000000000000 ) ) ;
#258060 = CYLINDRICAL_SURFACE ( 'NONE', #140995, 0.1000000000000028644 ) ;
#258061 = DIRECTION ( 'NONE',  ( 0.000000000000000000, 0.000000000000000000, -1.000000000000000000 ) ) ;
#258062 = AXIS2_PLACEMENT_3D ( 'NONE', #205822, #87146, #187573 ) ;
#258063 = VERTEX_POINT ( 'NONE', #166642 ) ;
#258065 = TOROIDAL_SURFACE ( 'NONE', #179041, 0.2000000000000000111, 0.1000000000000000056 ) ;
#258064 = SPHERICAL_SURFACE ( 'NONE', #159041, 0.1000000000000000056 ) ;
#258066 = LINE ( 'NONE', #19515, #72991 ) ;
#258067 = AXIS2_PLACEMENT_3D ( 'NONE', #125302, #86134, #106999 ) ;
#258068 = CARTESIAN_POINT ( 'NONE',  ( 18.49999999999999289, 10.41716543471636136, -24.84999999941982551 ) ) ;
#258069 = DIRECTION ( 'NONE',  ( 0.000000000000000000, 1.000000000000000000, 0.000000000000000000 ) ) ;
#258070 = ORIENTED_EDGE ( 'NONE', *, *, #169557, .F. ) ;
#258071 = CARTESIAN_POINT ( 'NONE',  ( 23.25000000000000000, -11.74999999998883560, -45.65000000000000568 ) ) ;
#258073 = ORIENTED_EDGE ( 'NONE', *, *, #254559, .T. ) ;
#258072 = CARTESIAN_POINT ( 'NONE',  ( -20.85000000000000142, 67.23127455305835554, -235.8551265064784559 ) ) ;
#258074 = CARTESIAN_POINT ( 'NONE',  ( -20.85000000000000142, 77.16412189325258453, -28.10825939895270764 ) ) ;
#258075 = CARTESIAN_POINT ( 'NONE',  ( -16.77828822459933633, 9.946229375067616729, -188.3373717490810293 ) ) ;
#258076 = DIRECTION ( 'NONE',  ( 0.000000000000000000, -0.9126074666063660468, -0.4088369013363524762 ) ) ;
#258077 = ORIENTED_EDGE ( 'NONE', *, *, #179060, .F. ) ;
#258078 = CARTESIAN_POINT ( 'NONE',  ( -23.15000000000000213, 26.42645436459467589, -241.9028176822583589 ) ) ;
#258079 = SHAPE_DEFINITION_REPRESENTATION ( #191023, #135069 ) ;
#258080 = CARTESIAN_POINT ( 'NONE',  ( 22.40000000000010516, -2.479040261794990485, -189.6172560698083487 ) ) ;
#258081 = EDGE_LOOP ( 'NONE', ( #27715, #30260, #3320, #84804 ) ) ;
#258082 = LINE ( 'NONE', #80757, #4553 ) ;
#258083 = CARTESIAN_POINT ( 'NONE',  ( 18.39999999999999858, 85.60000000001186038, -96.32291809330219223 ) ) ;
#258084 = VECTOR ( 'NONE', #34685, 1000.000000000000114 ) ;
#258085 = CARTESIAN_POINT ( 'NONE',  ( -16.81744102076748959, 9.950000000011138823, -121.3500000000000369 ) ) ;
#258086 = VERTEX_POINT ( 'NONE', #208320 ) ;
#258087 = AXIS2_PLACEMENT_3D ( 'NONE', #165403, #109255, #87124 ) ;
#258088 = ORIENTED_EDGE ( 'NONE', *, *, #176456, .T. ) ;
#258089 = DIRECTION ( 'NONE',  ( 0.000000000000000000, -7.116814260417693756E-15, 1.000000000000000000 ) ) ;
#258090 = AXIS2_PLACEMENT_3D ( 'NONE', #62262, #141786, #162657 ) ;
#258091 = DIRECTION ( 'NONE',  ( -1.000000000000000000, -2.952720810173289112E-16, 0.000000000000000000 ) ) ;
#258092 = CARTESIAN_POINT ( 'NONE',  ( 21.05000000000000071, 5.850000000011156942, -123.8675027757221159 ) ) ;
#258093 = CARTESIAN_POINT ( 'NONE',  ( -20.64999999999999858, 46.19206980365409265, -240.6234452366647076 ) ) ;
#258094 = ADVANCED_FACE ( 'NONE', ( #29692 ), #210866, .T. ) ;
#258095 = DIRECTION ( 'NONE',  ( 1.000000000000000000, -0.000000000000000000, -0.000000000000000000 ) ) ;
#258096 = DIRECTION ( 'NONE',  ( 0.000000000000000000, 0.000000000000000000, -1.000000000000000000 ) ) ;
#258098 = CYLINDRICAL_SURFACE ( 'NONE', #199583, 0.09999999999999939493 ) ;
#258097 = DIRECTION ( 'NONE',  ( 1.000000000000000000, 0.000000000000000000, 0.000000000000000000 ) ) ;
#258099 = CARTESIAN_POINT ( 'NONE',  ( 23.24999999999999645, 58.31215475832291162, -223.8520309854405923 ) ) ;
#258100 = EDGE_CURVE ( 'NONE', #134468, #178236, #64789, .T. ) ;
#258101 = CARTESIAN_POINT ( 'NONE',  ( -23.15000000000000213, 73.40000000001205649, -123.2984855617622202 ) ) ;
#258102 = CARTESIAN_POINT ( 'NONE',  ( 18.49999999999998934, 65.70711192142313450, -30.56510546851223609 ) ) ;
#258103 = FACE_OUTER_BOUND ( 'NONE', #121688, .T. ) ;
#258104 = AXIS2_PLACEMENT_3D ( 'NONE', #205885, #42978, #83344 ) ;
#258105 = VERTEX_POINT ( 'NONE', #148325 ) ;
#258106 = DIRECTION ( 'NONE',  ( 0.000000000000000000, -0.1350103645451974088, 0.9908441862701587999 ) ) ;
#258107 = NEXT_ASSEMBLY_USAGE_OCCURRENCE ( 'NAUO1', ' ', ' ', #42271, #99334, $ ) ;
#258108 = NEXT_ASSEMBLY_USAGE_OCCURRENCE ( 'NAUO2', ' ', ' ', #42271, #171249, $ ) ;
#258109 = NEXT_ASSEMBLY_USAGE_OCCURRENCE ( 'NAUO3', ' ', ' ', #42271, #70844, $ ) ;
#258110 = NEXT_ASSEMBLY_USAGE_OCCURRENCE ( 'NAUO4', ' ', ' ', #42271, #62861, $ ) ;
#258111 = NEXT_ASSEMBLY_USAGE_OCCURRENCE ( 'NAUO5', ' ', ' ', #42271, #155341, $ ) ;
#258112 = NEXT_ASSEMBLY_USAGE_OCCURRENCE ( 'NAUO6', ' ', ' ', #42271, #222081, $ ) ;
#258113 = NEXT_ASSEMBLY_USAGE_OCCURRENCE ( 'NAUO7', ' ', ' ', #42271, #195054, $ ) ;
#258114 = NEXT_ASSEMBLY_USAGE_OCCURRENCE ( 'NAUO8', ' ', ' ', #42271, #163264, $ ) ;
#258115 = NEXT_ASSEMBLY_USAGE_OCCURRENCE ( 'NAUO9', ' ', ' ', #42271, #148835, $ ) ;
#258116 = NEXT_ASSEMBLY_USAGE_OCCURRENCE ( 'NAUO10', ' ', ' ', #42271, #121752, $ ) ;
#258117 = NEXT_ASSEMBLY_USAGE_OCCURRENCE ( 'NAUO11', ' ', ' ', #42271, #152080, $ ) ;
#258118 = NEXT_ASSEMBLY_USAGE_OCCURRENCE ( 'NAUO12', ' ', ' ', #42271, #168000, $ ) ;
#258119 = NEXT_ASSEMBLY_USAGE_OCCURRENCE ( 'NAUO13', ' ', ' ', #42271, #252419, $ ) ;
#258120 = NEXT_ASSEMBLY_USAGE_OCCURRENCE ( 'NAUO14', ' ', ' ', #42271, #2194, $ ) ;
#258121 = NEXT_ASSEMBLY_USAGE_OCCURRENCE ( 'NAUO15', ' ', ' ', #42271, #32578, $ ) ;
#258122 = NEXT_ASSEMBLY_USAGE_OCCURRENCE ( 'NAUO16', ' ', ' ', #42271, #198277, $ ) ;
#258123 = NEXT_ASSEMBLY_USAGE_OCCURRENCE ( 'NAUO17', ' ', ' ', #42271, #5427, $ ) ;
#258124 = NEXT_ASSEMBLY_USAGE_OCCURRENCE ( 'NAUO18', ' ', ' ', #42271, #40537, $ ) ;
#258125 = NEXT_ASSEMBLY_USAGE_OCCURRENCE ( 'NAUO19', ' ', ' ', #42271, #97863, $ ) ;
#258126 = NEXT_ASSEMBLY_USAGE_OCCURRENCE ( 'NAUO20', ' ', ' ', #42271, #94639, $ ) ;
#258127 = NEXT_ASSEMBLY_USAGE_OCCURRENCE ( 'NAUO21', ' ', ' ', #42271, #160032, $ ) ;
#258128 = NEXT_ASSEMBLY_USAGE_OCCURRENCE ( 'NAUO22', ' ', ' ', #42271, #144083, $ ) ;
#258129 = NEXT_ASSEMBLY_USAGE_OCCURRENCE ( 'NAUO23', ' ', ' ', #42271, #75539, $ ) ;
#258130 = NEXT_ASSEMBLY_USAGE_OCCURRENCE ( 'NAUO24', ' ', ' ', #42271, #29336, $ ) ;
#258131 = NEXT_ASSEMBLY_USAGE_OCCURRENCE ( 'NAUO25', ' ', ' ', #42271, #206229, $ ) ;
#258132 = NEXT_ASSEMBLY_USAGE_OCCURRENCE ( 'NAUO26', ' ', ' ', #42271, #86666, $ ) ;
#258133 = NEXT_ASSEMBLY_USAGE_OCCURRENCE ( 'NAUO27', ' ', ' ', #42271, #236527, $ ) ;
#258134 = NEXT_ASSEMBLY_USAGE_OCCURRENCE ( 'NAUO28', ' ', ' ', #42271, #132936, $ ) ;
#258135 = NEXT_ASSEMBLY_USAGE_OCCURRENCE ( 'NAUO29', ' ', ' ', #42271, #228620, $ ) ;
#258136 = NEXT_ASSEMBLY_USAGE_OCCURRENCE ( 'NAUO30', ' ', ' ', #42271, #21371, $ ) ;
#258137 = NEXT_ASSEMBLY_USAGE_OCCURRENCE ( 'NAUO31', ' ', ' ', #42271, #190348, $ ) ;
#258138 = NEXT_ASSEMBLY_USAGE_OCCURRENCE ( 'NAUO32', ' ', ' ', #42271, #179166, $ ) ;
#258139 = NEXT_ASSEMBLY_USAGE_OCCURRENCE ( 'NAUO33', ' ', ' ', #42271, #182404, $ ) ;
ENDSEC;
END-ISO-10303-21;
